#51279=EDGE_CURVE('',#39831,#39832,#25096,.T.);
#51280=EDGE_CURVE('',#39566,#39830,#21091,.T.);
#51281=EDGE_CURVE('',#39832,#39830,#21092,.T.);
#51282=EDGE_CURVE('',#39567,#39832,#21093,.T.);
#51283=EDGE_CURVE('',#39565,#39829,#21094,.T.);
#51284=EDGE_CURVE('',#39825,#39564,#21095,.T.);
#51285=EDGE_CURVE('',#39826,#38907,#21096,.T.);
#51286=EDGE_CURVE('',#39827,#38906,#21097,.T.);
#51287=EDGE_CURVE('',#39821,#38905,#21098,.T.);
#51288=EDGE_CURVE('',#39822,#38904,#21099,.T.);
#51289=EDGE_CURVE('',#39569,#39823,#21100,.T.);
#51290=EDGE_CURVE('',#39568,#39824,#21101,.T.);
#51291=EDGE_CURVE('',#39833,#39834,#29412,.T.);
#51292=EDGE_CURVE('',#39834,#39835,#25097,.T.);
#51293=EDGE_CURVE('',#39835,#39836,#744,.T.);
#51294=EDGE_CURVE('',#39836,#39837,#29413,.T.);
#51295=EDGE_CURVE('',#39837,#39833,#25098,.T.);
#51296=EDGE_CURVE('',#39838,#39839,#745,.T.);
#51297=EDGE_CURVE('',#39839,#39840,#25099,.T.);
#51298=EDGE_CURVE('',#39841,#39840,#29414,.T.);
#51299=EDGE_CURVE('',#39841,#39842,#25100,.T.);
#51300=EDGE_CURVE('',#39842,#39838,#29415,.T.);
#51301=EDGE_CURVE('',#39840,#39834,#25101,.T.);
#51302=EDGE_CURVE('',#39833,#39841,#21102,.T.);
#51303=EDGE_CURVE('',#39842,#39843,#25102,.T.);
#51304=EDGE_CURVE('',#39844,#39841,#746,.T.);
#51305=EDGE_CURVE('',#39843,#39844,#25103,.T.);
#51306=EDGE_CURVE('',#39844,#39833,#747,.T.);
#51307=EDGE_CURVE('',#39845,#39837,#25104,.T.);
#51308=EDGE_CURVE('',#39844,#39845,#25105,.T.);
#51309=EDGE_CURVE('',#39572,#39843,#21103,.T.);
#51310=EDGE_CURVE('',#39845,#39843,#21104,.T.);
#51311=EDGE_CURVE('',#39573,#39845,#21105,.T.);
#51312=EDGE_CURVE('',#39571,#39842,#21106,.T.);
#51313=EDGE_CURVE('',#39838,#39570,#21107,.T.);
#51314=EDGE_CURVE('',#39839,#38903,#21108,.T.);
#51315=EDGE_CURVE('',#39840,#38902,#21109,.T.);
#51316=EDGE_CURVE('',#39834,#38901,#21110,.T.);
#51317=EDGE_CURVE('',#39835,#38900,#21111,.T.);
#51318=EDGE_CURVE('',#39575,#39836,#21112,.T.);
#51319=EDGE_CURVE('',#39574,#39837,#21113,.T.);
#51320=EDGE_CURVE('',#39846,#39847,#29416,.T.);
#51321=EDGE_CURVE('',#39847,#39848,#25106,.T.);
#51322=EDGE_CURVE('',#39848,#39849,#748,.T.);
#51323=EDGE_CURVE('',#39849,#39850,#29417,.T.);
#51324=EDGE_CURVE('',#39850,#39846,#25107,.T.);
#51325=EDGE_CURVE('',#39851,#39852,#749,.T.);
#51326=EDGE_CURVE('',#39852,#39853,#25108,.T.);
#51327=EDGE_CURVE('',#39854,#39853,#29418,.T.);
#51328=EDGE_CURVE('',#39854,#39855,#25109,.T.);
#51329=EDGE_CURVE('',#39855,#39851,#29419,.T.);
#51330=EDGE_CURVE('',#39853,#39847,#25110,.T.);
#51331=EDGE_CURVE('',#39846,#39854,#21114,.T.);
#51332=EDGE_CURVE('',#39855,#39856,#25111,.T.);
#51333=EDGE_CURVE('',#39857,#39854,#750,.T.);
#51334=EDGE_CURVE('',#39856,#39857,#25112,.T.);
#51335=EDGE_CURVE('',#39857,#39846,#751,.T.);
#51336=EDGE_CURVE('',#39858,#39850,#25113,.T.);
#51337=EDGE_CURVE('',#39857,#39858,#25114,.T.);
#51338=EDGE_CURVE('',#39578,#39856,#21115,.T.);
#51339=EDGE_CURVE('',#39858,#39856,#21116,.T.);
#51340=EDGE_CURVE('',#39579,#39858,#21117,.T.);
#51341=EDGE_CURVE('',#39577,#39855,#21118,.T.);
#51342=EDGE_CURVE('',#39851,#39576,#21119,.T.);
#51343=EDGE_CURVE('',#39852,#38899,#21120,.T.);
#51344=EDGE_CURVE('',#39853,#38898,#21121,.T.);
#51345=EDGE_CURVE('',#39847,#38897,#21122,.T.);
#51346=EDGE_CURVE('',#39848,#38896,#21123,.T.);
#51347=EDGE_CURVE('',#39581,#39849,#21124,.T.);
#51348=EDGE_CURVE('',#39580,#39850,#21125,.T.);
#51349=EDGE_CURVE('',#39859,#39860,#29420,.T.);
#51350=EDGE_CURVE('',#39860,#39861,#25115,.T.);
#51351=EDGE_CURVE('',#39861,#39862,#752,.T.);
#51352=EDGE_CURVE('',#39862,#39863,#29421,.T.);
#51353=EDGE_CURVE('',#39863,#39859,#25116,.T.);
#51354=EDGE_CURVE('',#39864,#39865,#753,.T.);
#51355=EDGE_CURVE('',#39865,#39866,#25117,.T.);
#51356=EDGE_CURVE('',#39867,#39866,#29422,.T.);
#51357=EDGE_CURVE('',#39867,#39868,#25118,.T.);
#51358=EDGE_CURVE('',#39868,#39864,#29423,.T.);
#51359=EDGE_CURVE('',#39866,#39860,#25119,.T.);
#51360=EDGE_CURVE('',#39859,#39867,#21126,.T.);
#51361=EDGE_CURVE('',#39868,#39869,#25120,.T.);
#51362=EDGE_CURVE('',#39870,#39867,#754,.T.);
#51363=EDGE_CURVE('',#39869,#39870,#25121,.T.);
#51364=EDGE_CURVE('',#39870,#39859,#755,.T.);
#51365=EDGE_CURVE('',#39871,#39863,#25122,.T.);
#51366=EDGE_CURVE('',#39870,#39871,#25123,.T.);
#51367=EDGE_CURVE('',#39584,#39869,#21127,.T.);
#51368=EDGE_CURVE('',#39871,#39869,#21128,.T.);
#51369=EDGE_CURVE('',#39585,#39871,#21129,.T.);
#51370=EDGE_CURVE('',#39583,#39868,#21130,.T.);
#51371=EDGE_CURVE('',#39864,#39582,#21131,.T.);
#51372=EDGE_CURVE('',#39865,#38895,#21132,.T.);
#51373=EDGE_CURVE('',#39866,#38894,#21133,.T.);
#51374=EDGE_CURVE('',#39860,#38893,#21134,.T.);
#51375=EDGE_CURVE('',#39861,#38892,#21135,.T.);
#51376=EDGE_CURVE('',#39587,#39862,#21136,.T.);
#51377=EDGE_CURVE('',#39586,#39863,#21137,.T.);
#51378=EDGE_CURVE('',#39872,#39873,#29424,.T.);
#51379=EDGE_CURVE('',#39873,#39874,#25124,.T.);
#51380=EDGE_CURVE('',#39874,#39875,#756,.T.);
#51381=EDGE_CURVE('',#39875,#39876,#29425,.T.);
#51382=EDGE_CURVE('',#39876,#39872,#25125,.T.);
#51383=EDGE_CURVE('',#39877,#39878,#757,.T.);
#51384=EDGE_CURVE('',#39878,#39879,#25126,.T.);
#51385=EDGE_CURVE('',#39880,#39879,#29426,.T.);
#51386=EDGE_CURVE('',#39880,#39881,#25127,.T.);
#51387=EDGE_CURVE('',#39881,#39877,#29427,.T.);
#51388=EDGE_CURVE('',#39879,#39873,#25128,.T.);
#51389=EDGE_CURVE('',#39872,#39880,#21138,.T.);
#51390=EDGE_CURVE('',#39881,#39882,#25129,.T.);
#51391=EDGE_CURVE('',#39883,#39880,#758,.T.);
#51392=EDGE_CURVE('',#39882,#39883,#25130,.T.);
#51393=EDGE_CURVE('',#39883,#39872,#759,.T.);
#51394=EDGE_CURVE('',#39884,#39876,#25131,.T.);
#51395=EDGE_CURVE('',#39883,#39884,#25132,.T.);
#51396=EDGE_CURVE('',#39590,#39882,#21139,.T.);
#51397=EDGE_CURVE('',#39884,#39882,#21140,.T.);
#51398=EDGE_CURVE('',#39591,#39884,#21141,.T.);
#51399=EDGE_CURVE('',#39589,#39881,#21142,.T.);
#51400=EDGE_CURVE('',#39877,#39588,#21143,.T.);
#51401=EDGE_CURVE('',#39878,#38891,#21144,.T.);
#51402=EDGE_CURVE('',#39879,#38890,#21145,.T.);
#51403=EDGE_CURVE('',#39873,#38889,#21146,.T.);
#51404=EDGE_CURVE('',#39874,#38888,#21147,.T.);
#51405=EDGE_CURVE('',#39593,#39875,#21148,.T.);
#51406=EDGE_CURVE('',#39592,#39876,#21149,.T.);
#51407=EDGE_CURVE('',#39885,#39886,#29428,.T.);
#51408=EDGE_CURVE('',#39886,#39887,#25133,.T.);
#51409=EDGE_CURVE('',#39887,#39888,#760,.T.);
#51410=EDGE_CURVE('',#39888,#39889,#29429,.T.);
#51411=EDGE_CURVE('',#39889,#39885,#25134,.T.);
#51412=EDGE_CURVE('',#39890,#39891,#761,.T.);
#51413=EDGE_CURVE('',#39891,#39892,#25135,.T.);
#51414=EDGE_CURVE('',#39893,#39892,#29430,.T.);
#51415=EDGE_CURVE('',#39893,#39894,#25136,.T.);
#51416=EDGE_CURVE('',#39894,#39890,#29431,.T.);
#51417=EDGE_CURVE('',#39892,#39886,#25137,.T.);
#51418=EDGE_CURVE('',#39885,#39893,#21150,.T.);
#51419=EDGE_CURVE('',#39894,#39895,#25138,.T.);
#51420=EDGE_CURVE('',#39896,#39893,#762,.T.);
#51421=EDGE_CURVE('',#39895,#39896,#25139,.T.);
#51422=EDGE_CURVE('',#39896,#39885,#763,.T.);
#51423=EDGE_CURVE('',#39897,#39889,#25140,.T.);
#51424=EDGE_CURVE('',#39896,#39897,#25141,.T.);
#51425=EDGE_CURVE('',#39596,#39895,#21151,.T.);
#51426=EDGE_CURVE('',#39897,#39895,#21152,.T.);
#51427=EDGE_CURVE('',#39597,#39897,#21153,.T.);
#51428=EDGE_CURVE('',#39595,#39894,#21154,.T.);
#51429=EDGE_CURVE('',#39890,#39594,#21155,.T.);
#51430=EDGE_CURVE('',#39891,#38887,#21156,.T.);
#51431=EDGE_CURVE('',#39892,#38886,#21157,.T.);
#51432=EDGE_CURVE('',#39886,#38885,#21158,.T.);
#51433=EDGE_CURVE('',#39887,#38884,#21159,.T.);
#51434=EDGE_CURVE('',#39599,#39888,#21160,.T.);
#51435=EDGE_CURVE('',#39598,#39889,#21161,.T.);
#51436=EDGE_CURVE('',#39898,#39899,#29432,.T.);
#51437=EDGE_CURVE('',#39899,#39900,#25142,.T.);
#51438=EDGE_CURVE('',#39900,#39901,#764,.T.);
#51439=EDGE_CURVE('',#39901,#39902,#29433,.T.);
#51440=EDGE_CURVE('',#39902,#39898,#25143,.T.);
#51441=EDGE_CURVE('',#39903,#39904,#765,.T.);
#51442=EDGE_CURVE('',#39904,#39905,#25144,.T.);
#51443=EDGE_CURVE('',#39906,#39905,#29434,.T.);
#51444=EDGE_CURVE('',#39906,#39907,#25145,.T.);
#51445=EDGE_CURVE('',#39907,#39903,#29435,.T.);
#51446=EDGE_CURVE('',#39905,#39899,#25146,.T.);
#51447=EDGE_CURVE('',#39898,#39906,#21162,.T.);
#51448=EDGE_CURVE('',#39907,#39908,#25147,.T.);
#51449=EDGE_CURVE('',#39909,#39906,#766,.T.);
#51450=EDGE_CURVE('',#39908,#39909,#25148,.T.);
#51451=EDGE_CURVE('',#39909,#39898,#767,.T.);
#51452=EDGE_CURVE('',#39910,#39902,#25149,.T.);
#51453=EDGE_CURVE('',#39909,#39910,#25150,.T.);
#51454=EDGE_CURVE('',#39602,#39908,#21163,.T.);
#51455=EDGE_CURVE('',#39910,#39908,#21164,.T.);
#51456=EDGE_CURVE('',#39603,#39910,#21165,.T.);
#51457=EDGE_CURVE('',#39601,#39907,#21166,.T.);
#51458=EDGE_CURVE('',#39903,#39600,#21167,.T.);
#51459=EDGE_CURVE('',#39904,#38883,#21168,.T.);
#51460=EDGE_CURVE('',#39905,#38882,#21169,.T.);
#51461=EDGE_CURVE('',#39899,#38881,#21170,.T.);
#51462=EDGE_CURVE('',#39900,#38880,#21171,.T.);
#51463=EDGE_CURVE('',#39605,#39901,#21172,.T.);
#51464=EDGE_CURVE('',#39604,#39902,#21173,.T.);
#51465=EDGE_CURVE('',#39911,#39912,#29436,.T.);
#51466=EDGE_CURVE('',#39912,#39913,#25151,.T.);
#51467=EDGE_CURVE('',#39913,#39914,#768,.T.);
#51468=EDGE_CURVE('',#39914,#39915,#29437,.T.);
#51469=EDGE_CURVE('',#39915,#39911,#25152,.T.);
#51470=EDGE_CURVE('',#39916,#39917,#769,.T.);
#51471=EDGE_CURVE('',#39917,#39918,#25153,.T.);
#51472=EDGE_CURVE('',#39919,#39918,#29438,.T.);
#51473=EDGE_CURVE('',#39919,#39920,#25154,.T.);
#51474=EDGE_CURVE('',#39920,#39916,#29439,.T.);
#51475=EDGE_CURVE('',#39918,#39912,#25155,.T.);
#51476=EDGE_CURVE('',#39911,#39919,#21174,.T.);
#51477=EDGE_CURVE('',#39920,#39921,#25156,.T.);
#51478=EDGE_CURVE('',#39922,#39919,#770,.T.);
#51479=EDGE_CURVE('',#39921,#39922,#25157,.T.);
#51480=EDGE_CURVE('',#39922,#39911,#771,.T.);
#51481=EDGE_CURVE('',#39923,#39915,#25158,.T.);
#51482=EDGE_CURVE('',#39922,#39923,#25159,.T.);
#51483=EDGE_CURVE('',#39608,#39921,#21175,.T.);
#51484=EDGE_CURVE('',#39923,#39921,#21176,.T.);
#51485=EDGE_CURVE('',#39609,#39923,#21177,.T.);
#51486=EDGE_CURVE('',#39607,#39920,#21178,.T.);
#51487=EDGE_CURVE('',#39916,#39606,#21179,.T.);
#51488=EDGE_CURVE('',#39917,#38879,#21180,.T.);
#51489=EDGE_CURVE('',#39918,#38878,#21181,.T.);
#51490=EDGE_CURVE('',#39912,#38877,#21182,.T.);
#51491=EDGE_CURVE('',#39913,#38876,#21183,.T.);
#51492=EDGE_CURVE('',#39611,#39914,#21184,.T.);
#51493=EDGE_CURVE('',#39610,#39915,#21185,.T.);
#51494=EDGE_CURVE('',#39924,#39925,#29440,.T.);
#51495=EDGE_CURVE('',#39925,#39926,#25160,.T.);
#51496=EDGE_CURVE('',#39926,#39927,#772,.T.);
#51497=EDGE_CURVE('',#39927,#39928,#29441,.T.);
#51498=EDGE_CURVE('',#39928,#39924,#25161,.T.);
#51499=EDGE_CURVE('',#39929,#39930,#773,.T.);
#51500=EDGE_CURVE('',#39930,#39931,#25162,.T.);
#51501=EDGE_CURVE('',#39932,#39931,#29442,.T.);
#51502=EDGE_CURVE('',#39932,#39933,#25163,.T.);
#51503=EDGE_CURVE('',#39933,#39929,#29443,.T.);
#51504=EDGE_CURVE('',#39931,#39925,#25164,.T.);
#51505=EDGE_CURVE('',#39924,#39932,#21186,.T.);
#51506=EDGE_CURVE('',#39933,#39934,#25165,.T.);
#51507=EDGE_CURVE('',#39935,#39932,#774,.T.);
#51508=EDGE_CURVE('',#39934,#39935,#25166,.T.);
#51509=EDGE_CURVE('',#39935,#39924,#775,.T.);
#51510=EDGE_CURVE('',#39936,#39928,#25167,.T.);
#51511=EDGE_CURVE('',#39935,#39936,#25168,.T.);
#51512=EDGE_CURVE('',#39614,#39934,#21187,.T.);
#51513=EDGE_CURVE('',#39936,#39934,#21188,.T.);
#51514=EDGE_CURVE('',#39615,#39936,#21189,.T.);
#51515=EDGE_CURVE('',#39613,#39933,#21190,.T.);
#51516=EDGE_CURVE('',#39929,#39612,#21191,.T.);
#51517=EDGE_CURVE('',#39930,#38875,#21192,.T.);
#51518=EDGE_CURVE('',#39931,#38874,#21193,.T.);
#51519=EDGE_CURVE('',#39925,#38873,#21194,.T.);
#51520=EDGE_CURVE('',#39926,#38872,#21195,.T.);
#51521=EDGE_CURVE('',#39617,#39927,#21196,.T.);
#51522=EDGE_CURVE('',#39616,#39928,#21197,.T.);
#51523=EDGE_CURVE('',#39937,#39938,#29444,.T.);
#51524=EDGE_CURVE('',#39938,#39939,#25169,.T.);
#51525=EDGE_CURVE('',#39939,#39940,#776,.T.);
#51526=EDGE_CURVE('',#39940,#39941,#29445,.T.);
#51527=EDGE_CURVE('',#39941,#39937,#25170,.T.);
#51528=EDGE_CURVE('',#39942,#39943,#777,.T.);
#51529=EDGE_CURVE('',#39943,#39944,#25171,.T.);
#51530=EDGE_CURVE('',#39945,#39944,#29446,.T.);
#51531=EDGE_CURVE('',#39945,#39946,#25172,.T.);
#51532=EDGE_CURVE('',#39946,#39942,#29447,.T.);
#51533=EDGE_CURVE('',#39944,#39938,#25173,.T.);
#51534=EDGE_CURVE('',#39937,#39945,#21198,.T.);
#51535=EDGE_CURVE('',#39946,#39947,#25174,.T.);
#51536=EDGE_CURVE('',#39948,#39945,#778,.T.);
#51537=EDGE_CURVE('',#39947,#39948,#25175,.T.);
#51538=EDGE_CURVE('',#39948,#39937,#779,.T.);
#51539=EDGE_CURVE('',#39949,#39941,#25176,.T.);
#51540=EDGE_CURVE('',#39948,#39949,#25177,.T.);
#51541=EDGE_CURVE('',#39620,#39947,#21199,.T.);
#51542=EDGE_CURVE('',#39949,#39947,#21200,.T.);
#51543=EDGE_CURVE('',#39621,#39949,#21201,.T.);
#51544=EDGE_CURVE('',#39619,#39946,#21202,.T.);
#51545=EDGE_CURVE('',#39942,#39618,#21203,.T.);
#51546=EDGE_CURVE('',#39943,#38871,#21204,.T.);
#51547=EDGE_CURVE('',#39944,#38870,#21205,.T.);
#51548=EDGE_CURVE('',#39938,#38869,#21206,.T.);
#51549=EDGE_CURVE('',#39939,#38868,#21207,.T.);
#51550=EDGE_CURVE('',#39623,#39940,#21208,.T.);
#51551=EDGE_CURVE('',#39622,#39941,#21209,.T.);
#51552=EDGE_CURVE('',#39950,#39951,#29448,.T.);
#51553=EDGE_CURVE('',#39951,#39952,#25178,.T.);
#51554=EDGE_CURVE('',#39952,#39953,#780,.T.);
#51555=EDGE_CURVE('',#39953,#39954,#29449,.T.);
#51556=EDGE_CURVE('',#39954,#39950,#25179,.T.);
#51557=EDGE_CURVE('',#39955,#39956,#781,.T.);
#51558=EDGE_CURVE('',#39956,#39957,#25180,.T.);
#51559=EDGE_CURVE('',#39958,#39957,#29450,.T.);
#51560=EDGE_CURVE('',#39958,#39959,#25181,.T.);
#51561=EDGE_CURVE('',#39959,#39955,#29451,.T.);
#51562=EDGE_CURVE('',#39957,#39951,#25182,.T.);
#51563=EDGE_CURVE('',#39950,#39958,#21210,.T.);
#51564=EDGE_CURVE('',#39959,#39960,#25183,.T.);
#51565=EDGE_CURVE('',#39961,#39958,#782,.T.);
#51566=EDGE_CURVE('',#39960,#39961,#25184,.T.);
#51567=EDGE_CURVE('',#39961,#39950,#783,.T.);
#51568=EDGE_CURVE('',#39962,#39954,#25185,.T.);
#51569=EDGE_CURVE('',#39961,#39962,#25186,.T.);
#51570=EDGE_CURVE('',#39626,#39960,#21211,.T.);
#51571=EDGE_CURVE('',#39962,#39960,#21212,.T.);
#51572=EDGE_CURVE('',#39627,#39962,#21213,.T.);
#51573=EDGE_CURVE('',#39625,#39959,#21214,.T.);
#51574=EDGE_CURVE('',#39955,#39624,#21215,.T.);
#51575=EDGE_CURVE('',#39956,#38867,#21216,.T.);
#51576=EDGE_CURVE('',#39957,#38866,#21217,.T.);
#51577=EDGE_CURVE('',#39951,#38865,#21218,.T.);
#51578=EDGE_CURVE('',#39952,#38864,#21219,.T.);
#51579=EDGE_CURVE('',#39629,#39953,#21220,.T.);
#51580=EDGE_CURVE('',#39628,#39954,#21221,.T.);
#51581=EDGE_CURVE('',#39963,#39964,#29452,.T.);
#51582=EDGE_CURVE('',#39964,#39965,#25187,.T.);
#51583=EDGE_CURVE('',#39965,#39966,#784,.T.);
#51584=EDGE_CURVE('',#39966,#39967,#29453,.T.);
#51585=EDGE_CURVE('',#39967,#39963,#25188,.T.);
#51586=EDGE_CURVE('',#39968,#39969,#785,.T.);
#51587=EDGE_CURVE('',#39969,#39970,#25189,.T.);
#51588=EDGE_CURVE('',#39971,#39970,#29454,.T.);
#51589=EDGE_CURVE('',#39971,#39972,#25190,.T.);
#51590=EDGE_CURVE('',#39972,#39968,#29455,.T.);
#51591=EDGE_CURVE('',#39970,#39964,#25191,.T.);
#51592=EDGE_CURVE('',#39963,#39971,#21222,.T.);
#51593=EDGE_CURVE('',#39972,#39973,#25192,.T.);
#51594=EDGE_CURVE('',#39974,#39971,#786,.T.);
#51595=EDGE_CURVE('',#39973,#39974,#25193,.T.);
#51596=EDGE_CURVE('',#39974,#39963,#787,.T.);
#51597=EDGE_CURVE('',#39975,#39967,#25194,.T.);
#51598=EDGE_CURVE('',#39974,#39975,#25195,.T.);
#51599=EDGE_CURVE('',#39632,#39973,#21223,.T.);
#51600=EDGE_CURVE('',#39975,#39973,#21224,.T.);
#51601=EDGE_CURVE('',#39633,#39975,#21225,.T.);
#51602=EDGE_CURVE('',#39631,#39972,#21226,.T.);
#51603=EDGE_CURVE('',#39968,#39630,#21227,.T.);
#51604=EDGE_CURVE('',#39969,#38863,#21228,.T.);
#51605=EDGE_CURVE('',#39970,#38862,#21229,.T.);
#51606=EDGE_CURVE('',#39964,#38861,#21230,.T.);
#51607=EDGE_CURVE('',#39965,#38860,#21231,.T.);
#51608=EDGE_CURVE('',#39635,#39966,#21232,.T.);
#51609=EDGE_CURVE('',#39634,#39967,#21233,.T.);
#51610=EDGE_CURVE('',#39976,#39977,#29456,.T.);
#51611=EDGE_CURVE('',#39977,#39978,#25196,.T.);
#51612=EDGE_CURVE('',#39978,#39979,#788,.T.);
#51613=EDGE_CURVE('',#39979,#39980,#29457,.T.);
#51614=EDGE_CURVE('',#39980,#39976,#25197,.T.);
#51615=EDGE_CURVE('',#39981,#39982,#789,.T.);
#51616=EDGE_CURVE('',#39982,#39983,#25198,.T.);
#51617=EDGE_CURVE('',#39984,#39983,#29458,.T.);
#51618=EDGE_CURVE('',#39984,#39985,#25199,.T.);
#51619=EDGE_CURVE('',#39985,#39981,#29459,.T.);
#51620=EDGE_CURVE('',#39983,#39977,#25200,.T.);
#51621=EDGE_CURVE('',#39976,#39984,#21234,.T.);
#51622=EDGE_CURVE('',#39985,#39986,#25201,.T.);
#51623=EDGE_CURVE('',#39987,#39984,#790,.T.);
#51624=EDGE_CURVE('',#39986,#39987,#25202,.T.);
#51625=EDGE_CURVE('',#39987,#39976,#791,.T.);
#51626=EDGE_CURVE('',#39988,#39980,#25203,.T.);
#51627=EDGE_CURVE('',#39987,#39988,#25204,.T.);
#51628=EDGE_CURVE('',#39638,#39986,#21235,.T.);
#51629=EDGE_CURVE('',#39988,#39986,#21236,.T.);
#51630=EDGE_CURVE('',#39639,#39988,#21237,.T.);
#51631=EDGE_CURVE('',#39637,#39985,#21238,.T.);
#51632=EDGE_CURVE('',#39981,#39636,#21239,.T.);
#51633=EDGE_CURVE('',#39982,#38859,#21240,.T.);
#51634=EDGE_CURVE('',#39983,#38858,#21241,.T.);
#51635=EDGE_CURVE('',#39977,#38857,#21242,.T.);
#51636=EDGE_CURVE('',#39978,#38856,#21243,.T.);
#51637=EDGE_CURVE('',#39053,#39979,#21244,.T.);
#51638=EDGE_CURVE('',#39640,#39980,#21245,.T.);
#51639=EDGE_CURVE('',#39989,#39990,#29460,.T.);
#51640=EDGE_CURVE('',#39990,#39991,#25205,.T.);
#51641=EDGE_CURVE('',#39991,#39992,#792,.T.);
#51642=EDGE_CURVE('',#39992,#39993,#29461,.T.);
#51643=EDGE_CURVE('',#39993,#39989,#25206,.T.);
#51644=EDGE_CURVE('',#39994,#39995,#793,.T.);
#51645=EDGE_CURVE('',#39995,#39996,#25207,.T.);
#51646=EDGE_CURVE('',#39997,#39996,#29462,.T.);
#51647=EDGE_CURVE('',#39997,#39998,#25208,.T.);
#51648=EDGE_CURVE('',#39998,#39994,#29463,.T.);
#51649=EDGE_CURVE('',#39996,#39990,#25209,.T.);
#51650=EDGE_CURVE('',#39989,#39997,#21246,.T.);
#51651=EDGE_CURVE('',#39998,#39999,#25210,.T.);
#51652=EDGE_CURVE('',#40000,#39997,#794,.T.);
#51653=EDGE_CURVE('',#39999,#40000,#25211,.T.);
#51654=EDGE_CURVE('',#40000,#39989,#795,.T.);
#51655=EDGE_CURVE('',#40001,#39993,#25212,.T.);
#51656=EDGE_CURVE('',#40000,#40001,#25213,.T.);
#51657=EDGE_CURVE('',#39055,#39999,#21247,.T.);
#51658=EDGE_CURVE('',#40001,#39999,#21248,.T.);
#51659=EDGE_CURVE('',#39056,#40001,#21249,.T.);
#51660=EDGE_CURVE('',#39054,#39998,#21250,.T.);
#51661=EDGE_CURVE('',#39994,#39052,#21251,.T.);
#51662=EDGE_CURVE('',#39995,#38852,#21252,.T.);
#51663=EDGE_CURVE('',#39996,#38851,#21253,.T.);
#51664=EDGE_CURVE('',#39990,#38850,#21254,.T.);
#51665=EDGE_CURVE('',#39991,#38849,#21255,.T.);
#51666=EDGE_CURVE('',#39058,#39992,#21256,.T.);
#51667=EDGE_CURVE('',#39057,#39993,#21257,.T.);
#51668=EDGE_CURVE('',#40002,#40003,#29464,.T.);
#51669=EDGE_CURVE('',#40003,#40004,#25214,.T.);
#51670=EDGE_CURVE('',#40004,#40005,#796,.T.);
#51671=EDGE_CURVE('',#40005,#40006,#29465,.T.);
#51672=EDGE_CURVE('',#40006,#40002,#25215,.T.);
#51673=EDGE_CURVE('',#40007,#40008,#797,.T.);
#51674=EDGE_CURVE('',#40008,#40009,#25216,.T.);
#51675=EDGE_CURVE('',#40010,#40009,#29466,.T.);
#51676=EDGE_CURVE('',#40010,#40011,#25217,.T.);
#51677=EDGE_CURVE('',#40011,#40007,#29467,.T.);
#51678=EDGE_CURVE('',#40009,#40003,#25218,.T.);
#51679=EDGE_CURVE('',#40002,#40010,#21258,.T.);
#51680=EDGE_CURVE('',#40011,#40012,#25219,.T.);
#51681=EDGE_CURVE('',#40013,#40010,#798,.T.);
#51682=EDGE_CURVE('',#40012,#40013,#25220,.T.);
#51683=EDGE_CURVE('',#40013,#40002,#799,.T.);
#51684=EDGE_CURVE('',#40014,#40006,#25221,.T.);
#51685=EDGE_CURVE('',#40013,#40014,#25222,.T.);
#51686=EDGE_CURVE('',#39061,#40012,#21259,.T.);
#51687=EDGE_CURVE('',#40014,#40012,#21260,.T.);
#51688=EDGE_CURVE('',#39062,#40014,#21261,.T.);
#51689=EDGE_CURVE('',#39060,#40011,#21262,.T.);
#51690=EDGE_CURVE('',#40007,#39059,#21263,.T.);
#51691=EDGE_CURVE('',#40008,#38848,#21264,.T.);
#51692=EDGE_CURVE('',#40009,#38847,#21265,.T.);
#51693=EDGE_CURVE('',#40003,#38846,#21266,.T.);
#51694=EDGE_CURVE('',#40004,#38845,#21267,.T.);
#51695=EDGE_CURVE('',#39064,#40005,#21268,.T.);
#51696=EDGE_CURVE('',#39063,#40006,#21269,.T.);
#51697=EDGE_CURVE('',#40015,#40016,#29468,.T.);
#51698=EDGE_CURVE('',#40016,#40017,#25223,.T.);
#51699=EDGE_CURVE('',#40017,#40018,#800,.T.);
#51700=EDGE_CURVE('',#40018,#40019,#29469,.T.);
#51701=EDGE_CURVE('',#40019,#40015,#25224,.T.);
#51702=EDGE_CURVE('',#40020,#40021,#801,.T.);
#51703=EDGE_CURVE('',#40021,#40022,#25225,.T.);
#51704=EDGE_CURVE('',#40023,#40022,#29470,.T.);
#51705=EDGE_CURVE('',#40023,#40024,#25226,.T.);
#51706=EDGE_CURVE('',#40024,#40020,#29471,.T.);
#51707=EDGE_CURVE('',#40022,#40016,#25227,.T.);
#51708=EDGE_CURVE('',#40015,#40023,#21270,.T.);
#51709=EDGE_CURVE('',#40024,#40025,#25228,.T.);
#51710=EDGE_CURVE('',#40026,#40023,#802,.T.);
#51711=EDGE_CURVE('',#40025,#40026,#25229,.T.);
#51712=EDGE_CURVE('',#40026,#40015,#803,.T.);
#51713=EDGE_CURVE('',#40027,#40019,#25230,.T.);
#51714=EDGE_CURVE('',#40026,#40027,#25231,.T.);
#51715=EDGE_CURVE('',#39067,#40025,#21271,.T.);
#51716=EDGE_CURVE('',#40027,#40025,#21272,.T.);
#51717=EDGE_CURVE('',#39068,#40027,#21273,.T.);
#51718=EDGE_CURVE('',#39066,#40024,#21274,.T.);
#51719=EDGE_CURVE('',#40020,#39065,#21275,.T.);
#51720=EDGE_CURVE('',#40021,#38844,#21276,.T.);
#51721=EDGE_CURVE('',#40022,#38843,#21277,.T.);
#51722=EDGE_CURVE('',#40016,#38842,#21278,.T.);
#51723=EDGE_CURVE('',#40017,#38841,#21279,.T.);
#51724=EDGE_CURVE('',#39070,#40018,#21280,.T.);
#51725=EDGE_CURVE('',#39069,#40019,#21281,.T.);
#51726=EDGE_CURVE('',#40028,#40029,#29472,.T.);
#51727=EDGE_CURVE('',#40029,#40030,#25232,.T.);
#51728=EDGE_CURVE('',#40030,#40031,#804,.T.);
#51729=EDGE_CURVE('',#40031,#40032,#29473,.T.);
#51730=EDGE_CURVE('',#40032,#40028,#25233,.T.);
#51731=EDGE_CURVE('',#40033,#40034,#805,.T.);
#51732=EDGE_CURVE('',#40034,#40035,#25234,.T.);
#51733=EDGE_CURVE('',#40036,#40035,#29474,.T.);
#51734=EDGE_CURVE('',#40036,#40037,#25235,.T.);
#51735=EDGE_CURVE('',#40037,#40033,#29475,.T.);
#51736=EDGE_CURVE('',#40035,#40029,#25236,.T.);
#51737=EDGE_CURVE('',#40028,#40036,#21282,.T.);
#51738=EDGE_CURVE('',#40037,#40038,#25237,.T.);
#51739=EDGE_CURVE('',#40039,#40036,#806,.T.);
#51740=EDGE_CURVE('',#40038,#40039,#25238,.T.);
#51741=EDGE_CURVE('',#40039,#40028,#807,.T.);
#51742=EDGE_CURVE('',#40040,#40032,#25239,.T.);
#51743=EDGE_CURVE('',#40039,#40040,#25240,.T.);
#51744=EDGE_CURVE('',#39073,#40038,#21283,.T.);
#51745=EDGE_CURVE('',#40040,#40038,#21284,.T.);
#51746=EDGE_CURVE('',#39074,#40040,#21285,.T.);
#51747=EDGE_CURVE('',#39072,#40037,#21286,.T.);
#51748=EDGE_CURVE('',#40033,#39071,#21287,.T.);
#51749=EDGE_CURVE('',#40034,#38840,#21288,.T.);
#51750=EDGE_CURVE('',#40035,#38839,#21289,.T.);
#51751=EDGE_CURVE('',#40029,#38838,#21290,.T.);
#51752=EDGE_CURVE('',#40030,#38837,#21291,.T.);
#51753=EDGE_CURVE('',#39076,#40031,#21292,.T.);
#51754=EDGE_CURVE('',#39075,#40032,#21293,.T.);
#51755=EDGE_CURVE('',#40041,#40042,#29476,.T.);
#51756=EDGE_CURVE('',#40042,#40043,#25241,.T.);
#51757=EDGE_CURVE('',#40043,#40044,#808,.T.);
#51758=EDGE_CURVE('',#40044,#40045,#29477,.T.);
#51759=EDGE_CURVE('',#40045,#40041,#25242,.T.);
#51760=EDGE_CURVE('',#40046,#40047,#809,.T.);
#51761=EDGE_CURVE('',#40047,#40048,#25243,.T.);
#51762=EDGE_CURVE('',#40049,#40048,#29478,.T.);
#51763=EDGE_CURVE('',#40049,#40050,#25244,.T.);
#51764=EDGE_CURVE('',#40050,#40046,#29479,.T.);
#51765=EDGE_CURVE('',#40048,#40042,#25245,.T.);
#51766=EDGE_CURVE('',#40041,#40049,#21294,.T.);
#51767=EDGE_CURVE('',#40050,#40051,#25246,.T.);
#51768=EDGE_CURVE('',#40052,#40049,#810,.T.);
#51769=EDGE_CURVE('',#40051,#40052,#25247,.T.);
#51770=EDGE_CURVE('',#40052,#40041,#811,.T.);
#51771=EDGE_CURVE('',#40053,#40045,#25248,.T.);
#51772=EDGE_CURVE('',#40052,#40053,#25249,.T.);
#51773=EDGE_CURVE('',#39079,#40051,#21295,.T.);
#51774=EDGE_CURVE('',#40053,#40051,#21296,.T.);
#51775=EDGE_CURVE('',#39080,#40053,#21297,.T.);
#51776=EDGE_CURVE('',#39078,#40050,#21298,.T.);
#51777=EDGE_CURVE('',#40046,#39077,#21299,.T.);
#51778=EDGE_CURVE('',#40047,#38836,#21300,.T.);
#51779=EDGE_CURVE('',#40048,#38835,#21301,.T.);
#51780=EDGE_CURVE('',#40042,#38834,#21302,.T.);
#51781=EDGE_CURVE('',#40043,#38833,#21303,.T.);
#51782=EDGE_CURVE('',#39082,#40044,#21304,.T.);
#51783=EDGE_CURVE('',#39081,#40045,#21305,.T.);
#51784=EDGE_CURVE('',#40054,#40055,#29480,.T.);
#51785=EDGE_CURVE('',#40055,#40056,#25250,.T.);
#51786=EDGE_CURVE('',#40056,#40057,#812,.T.);
#51787=EDGE_CURVE('',#40057,#40058,#29481,.T.);
#51788=EDGE_CURVE('',#40058,#40054,#25251,.T.);
#51789=EDGE_CURVE('',#40059,#40060,#813,.T.);
#51790=EDGE_CURVE('',#40060,#40061,#25252,.T.);
#51791=EDGE_CURVE('',#40062,#40061,#29482,.T.);
#51792=EDGE_CURVE('',#40062,#40063,#25253,.T.);
#51793=EDGE_CURVE('',#40063,#40059,#29483,.T.);
#51794=EDGE_CURVE('',#40061,#40055,#25254,.T.);
#51795=EDGE_CURVE('',#40054,#40062,#21306,.T.);
#51796=EDGE_CURVE('',#40063,#40064,#25255,.T.);
#51797=EDGE_CURVE('',#40065,#40062,#814,.T.);
#51798=EDGE_CURVE('',#40064,#40065,#25256,.T.);
#51799=EDGE_CURVE('',#40065,#40054,#815,.T.);
#51800=EDGE_CURVE('',#40066,#40058,#25257,.T.);
#51801=EDGE_CURVE('',#40065,#40066,#25258,.T.);
#51802=EDGE_CURVE('',#39085,#40064,#21307,.T.);
#51803=EDGE_CURVE('',#40066,#40064,#21308,.T.);
#51804=EDGE_CURVE('',#39086,#40066,#21309,.T.);
#51805=EDGE_CURVE('',#39084,#40063,#21310,.T.);
#51806=EDGE_CURVE('',#40059,#39083,#21311,.T.);
#51807=EDGE_CURVE('',#40060,#38832,#21312,.T.);
#51808=EDGE_CURVE('',#40061,#38831,#21313,.T.);
#51809=EDGE_CURVE('',#40055,#38830,#21314,.T.);
#51810=EDGE_CURVE('',#40056,#38829,#21315,.T.);
#51811=EDGE_CURVE('',#39088,#40057,#21316,.T.);
#51812=EDGE_CURVE('',#39087,#40058,#21317,.T.);
#51813=EDGE_CURVE('',#40067,#40068,#29484,.T.);
#51814=EDGE_CURVE('',#40068,#40069,#25259,.T.);
#51815=EDGE_CURVE('',#40069,#40070,#816,.T.);
#51816=EDGE_CURVE('',#40070,#40071,#29485,.T.);
#51817=EDGE_CURVE('',#40071,#40067,#25260,.T.);
#51818=EDGE_CURVE('',#40072,#40073,#817,.T.);
#51819=EDGE_CURVE('',#40073,#40074,#25261,.T.);
#51820=EDGE_CURVE('',#40075,#40074,#29486,.T.);
#51821=EDGE_CURVE('',#40075,#40076,#25262,.T.);
#51822=EDGE_CURVE('',#40076,#40072,#29487,.T.);
#51823=EDGE_CURVE('',#40074,#40068,#25263,.T.);
#51824=EDGE_CURVE('',#40067,#40075,#21318,.T.);
#51825=EDGE_CURVE('',#40076,#40077,#25264,.T.);
#51826=EDGE_CURVE('',#40078,#40075,#818,.T.);
#51827=EDGE_CURVE('',#40077,#40078,#25265,.T.);
#51828=EDGE_CURVE('',#40078,#40067,#819,.T.);
#51829=EDGE_CURVE('',#40079,#40071,#25266,.T.);
#51830=EDGE_CURVE('',#40078,#40079,#25267,.T.);
#51831=EDGE_CURVE('',#39091,#40077,#21319,.T.);
#51832=EDGE_CURVE('',#40079,#40077,#21320,.T.);
#51833=EDGE_CURVE('',#39092,#40079,#21321,.T.);
#51834=EDGE_CURVE('',#39090,#40076,#21322,.T.);
#51835=EDGE_CURVE('',#40072,#39089,#21323,.T.);
#51836=EDGE_CURVE('',#40073,#38828,#21324,.T.);
#51837=EDGE_CURVE('',#40074,#38827,#21325,.T.);
#51838=EDGE_CURVE('',#40068,#38826,#21326,.T.);
#51839=EDGE_CURVE('',#40069,#38825,#21327,.T.);
#51840=EDGE_CURVE('',#39094,#40070,#21328,.T.);
#51841=EDGE_CURVE('',#39093,#40071,#21329,.T.);
#51842=EDGE_CURVE('',#40080,#40081,#29488,.T.);
#51843=EDGE_CURVE('',#40081,#40082,#25268,.T.);
#51844=EDGE_CURVE('',#40082,#40083,#820,.T.);
#51845=EDGE_CURVE('',#40083,#40084,#29489,.T.);
#51846=EDGE_CURVE('',#40084,#40080,#25269,.T.);
#51847=EDGE_CURVE('',#40085,#40086,#821,.T.);
#51848=EDGE_CURVE('',#40086,#40087,#25270,.T.);
#51849=EDGE_CURVE('',#40088,#40087,#29490,.T.);
#51850=EDGE_CURVE('',#40088,#40089,#25271,.T.);
#51851=EDGE_CURVE('',#40089,#40085,#29491,.T.);
#51852=EDGE_CURVE('',#40087,#40081,#25272,.T.);
#51853=EDGE_CURVE('',#40080,#40088,#21330,.T.);
#51854=EDGE_CURVE('',#40089,#40090,#25273,.T.);
#51855=EDGE_CURVE('',#40091,#40088,#822,.T.);
#51856=EDGE_CURVE('',#40090,#40091,#25274,.T.);
#51857=EDGE_CURVE('',#40091,#40080,#823,.T.);
#51858=EDGE_CURVE('',#40092,#40084,#25275,.T.);
#51859=EDGE_CURVE('',#40091,#40092,#25276,.T.);
#51860=EDGE_CURVE('',#39097,#40090,#21331,.T.);
#51861=EDGE_CURVE('',#40092,#40090,#21332,.T.);
#51862=EDGE_CURVE('',#39098,#40092,#21333,.T.);
#51863=EDGE_CURVE('',#39096,#40089,#21334,.T.);
#51864=EDGE_CURVE('',#40085,#39095,#21335,.T.);
#51865=EDGE_CURVE('',#40086,#38824,#21336,.T.);
#51866=EDGE_CURVE('',#40087,#38823,#21337,.T.);
#51867=EDGE_CURVE('',#40081,#38822,#21338,.T.);
#51868=EDGE_CURVE('',#40082,#38821,#21339,.T.);
#51869=EDGE_CURVE('',#39100,#40083,#21340,.T.);
#51870=EDGE_CURVE('',#39099,#40084,#21341,.T.);
#51871=EDGE_CURVE('',#40093,#40094,#29492,.T.);
#51872=EDGE_CURVE('',#40094,#40095,#25277,.T.);
#51873=EDGE_CURVE('',#40095,#40096,#824,.T.);
#51874=EDGE_CURVE('',#40096,#40097,#29493,.T.);
#51875=EDGE_CURVE('',#40097,#40093,#25278,.T.);
#51876=EDGE_CURVE('',#40098,#40099,#825,.T.);
#51877=EDGE_CURVE('',#40099,#40100,#25279,.T.);
#51878=EDGE_CURVE('',#40101,#40100,#29494,.T.);
#51879=EDGE_CURVE('',#40101,#40102,#25280,.T.);
#51880=EDGE_CURVE('',#40102,#40098,#29495,.T.);
#51881=EDGE_CURVE('',#40100,#40094,#25281,.T.);
#51882=EDGE_CURVE('',#40093,#40101,#21342,.T.);
#51883=EDGE_CURVE('',#40102,#40103,#25282,.T.);
#51884=EDGE_CURVE('',#40104,#40101,#826,.T.);
#51885=EDGE_CURVE('',#40103,#40104,#25283,.T.);
#51886=EDGE_CURVE('',#40104,#40093,#827,.T.);
#51887=EDGE_CURVE('',#40105,#40097,#25284,.T.);
#51888=EDGE_CURVE('',#40104,#40105,#25285,.T.);
#51889=EDGE_CURVE('',#39482,#40103,#21343,.T.);
#51890=EDGE_CURVE('',#40105,#40103,#21344,.T.);
#51891=EDGE_CURVE('',#39483,#40105,#21345,.T.);
#51892=EDGE_CURVE('',#39481,#40102,#21346,.T.);
#51893=EDGE_CURVE('',#40098,#39480,#21347,.T.);
#51894=EDGE_CURVE('',#40099,#38963,#21348,.T.);
#51895=EDGE_CURVE('',#40100,#38962,#21349,.T.);
#51896=EDGE_CURVE('',#40094,#38961,#21350,.T.);
#51897=EDGE_CURVE('',#40095,#38960,#21351,.T.);
#51898=EDGE_CURVE('',#39485,#40096,#21352,.T.);
#51899=EDGE_CURVE('',#39484,#40097,#21353,.T.);
#51900=EDGE_CURVE('',#40106,#40107,#29496,.T.);
#51901=EDGE_CURVE('',#40107,#40108,#25286,.T.);
#51902=EDGE_CURVE('',#40108,#40109,#828,.T.);
#51903=EDGE_CURVE('',#40109,#40110,#29497,.T.);
#51904=EDGE_CURVE('',#40110,#40106,#25287,.T.);
#51905=EDGE_CURVE('',#40111,#40112,#829,.T.);
#51906=EDGE_CURVE('',#40112,#40113,#25288,.T.);
#51907=EDGE_CURVE('',#40114,#40113,#29498,.T.);
#51908=EDGE_CURVE('',#40114,#40115,#25289,.T.);
#51909=EDGE_CURVE('',#40115,#40111,#29499,.T.);
#51910=EDGE_CURVE('',#40113,#40107,#25290,.T.);
#51911=EDGE_CURVE('',#40106,#40114,#21354,.T.);
#51912=EDGE_CURVE('',#40115,#40116,#25291,.T.);
#51913=EDGE_CURVE('',#40117,#40114,#830,.T.);
#51914=EDGE_CURVE('',#40116,#40117,#25292,.T.);
#51915=EDGE_CURVE('',#40117,#40106,#831,.T.);
#51916=EDGE_CURVE('',#40118,#40110,#25293,.T.);
#51917=EDGE_CURVE('',#40117,#40118,#25294,.T.);
#51918=EDGE_CURVE('',#39476,#40116,#21355,.T.);
#51919=EDGE_CURVE('',#40118,#40116,#21356,.T.);
#51920=EDGE_CURVE('',#39477,#40118,#21357,.T.);
#51921=EDGE_CURVE('',#39475,#40115,#21358,.T.);
#51922=EDGE_CURVE('',#40111,#39474,#21359,.T.);
#51923=EDGE_CURVE('',#40112,#38967,#21360,.T.);
#51924=EDGE_CURVE('',#40113,#38966,#21361,.T.);
#51925=EDGE_CURVE('',#40107,#38965,#21362,.T.);
#51926=EDGE_CURVE('',#40108,#38964,#21363,.T.);
#51927=EDGE_CURVE('',#39479,#40109,#21364,.T.);
#51928=EDGE_CURVE('',#39478,#40110,#21365,.T.);
#51929=EDGE_CURVE('',#40119,#40120,#29500,.T.);
#51930=EDGE_CURVE('',#40120,#40121,#25295,.T.);
#51931=EDGE_CURVE('',#40121,#40122,#832,.T.);
#51932=EDGE_CURVE('',#40122,#40123,#29501,.T.);
#51933=EDGE_CURVE('',#40123,#40119,#25296,.T.);
#51934=EDGE_CURVE('',#40124,#40125,#833,.T.);
#51935=EDGE_CURVE('',#40125,#40126,#25297,.T.);
#51936=EDGE_CURVE('',#40127,#40126,#29502,.T.);
#51937=EDGE_CURVE('',#40127,#40128,#25298,.T.);
#51938=EDGE_CURVE('',#40128,#40124,#29503,.T.);
#51939=EDGE_CURVE('',#40126,#40120,#25299,.T.);
#51940=EDGE_CURVE('',#40119,#40127,#21366,.T.);
#51941=EDGE_CURVE('',#40128,#40129,#25300,.T.);
#51942=EDGE_CURVE('',#40130,#40127,#834,.T.);
#51943=EDGE_CURVE('',#40129,#40130,#25301,.T.);
#51944=EDGE_CURVE('',#40130,#40119,#835,.T.);
#51945=EDGE_CURVE('',#40131,#40123,#25302,.T.);
#51946=EDGE_CURVE('',#40130,#40131,#25303,.T.);
#51947=EDGE_CURVE('',#39470,#40129,#21367,.T.);
#51948=EDGE_CURVE('',#40131,#40129,#21368,.T.);
#51949=EDGE_CURVE('',#39471,#40131,#21369,.T.);
#51950=EDGE_CURVE('',#39469,#40128,#21370,.T.);
#51951=EDGE_CURVE('',#40124,#39468,#21371,.T.);
#51952=EDGE_CURVE('',#40125,#38971,#21372,.T.);
#51953=EDGE_CURVE('',#40126,#38970,#21373,.T.);
#51954=EDGE_CURVE('',#40120,#38969,#21374,.T.);
#51955=EDGE_CURVE('',#40121,#38968,#21375,.T.);
#51956=EDGE_CURVE('',#39473,#40122,#21376,.T.);
#51957=EDGE_CURVE('',#39472,#40123,#21377,.T.);
#51958=EDGE_CURVE('',#40132,#40133,#29504,.T.);
#51959=EDGE_CURVE('',#40133,#40134,#25304,.T.);
#51960=EDGE_CURVE('',#40134,#40135,#836,.T.);
#51961=EDGE_CURVE('',#40135,#40136,#29505,.T.);
#51962=EDGE_CURVE('',#40136,#40132,#25305,.T.);
#51963=EDGE_CURVE('',#40137,#40138,#837,.T.);
#51964=EDGE_CURVE('',#40138,#40139,#25306,.T.);
#51965=EDGE_CURVE('',#40140,#40139,#29506,.T.);
#51966=EDGE_CURVE('',#40140,#40141,#25307,.T.);
#51967=EDGE_CURVE('',#40141,#40137,#29507,.T.);
#51968=EDGE_CURVE('',#40139,#40133,#25308,.T.);
#51969=EDGE_CURVE('',#40132,#40140,#21378,.T.);
#51970=EDGE_CURVE('',#40141,#40142,#25309,.T.);
#51971=EDGE_CURVE('',#40143,#40140,#838,.T.);
#51972=EDGE_CURVE('',#40142,#40143,#25310,.T.);
#51973=EDGE_CURVE('',#40143,#40132,#839,.T.);
#51974=EDGE_CURVE('',#40144,#40136,#25311,.T.);
#51975=EDGE_CURVE('',#40143,#40144,#25312,.T.);
#51976=EDGE_CURVE('',#39464,#40142,#21379,.T.);
#51977=EDGE_CURVE('',#40144,#40142,#21380,.T.);
#51978=EDGE_CURVE('',#39465,#40144,#21381,.T.);
#51979=EDGE_CURVE('',#39463,#40141,#21382,.T.);
#51980=EDGE_CURVE('',#40137,#39462,#21383,.T.);
#51981=EDGE_CURVE('',#40138,#38975,#21384,.T.);
#51982=EDGE_CURVE('',#40139,#38974,#21385,.T.);
#51983=EDGE_CURVE('',#40133,#38973,#21386,.T.);
#51984=EDGE_CURVE('',#40134,#38972,#21387,.T.);
#51985=EDGE_CURVE('',#39467,#40135,#21388,.T.);
#51986=EDGE_CURVE('',#39466,#40136,#21389,.T.);
#51987=EDGE_CURVE('',#40145,#40146,#29508,.T.);
#51988=EDGE_CURVE('',#40146,#40147,#25313,.T.);
#51989=EDGE_CURVE('',#40147,#40148,#840,.T.);
#51990=EDGE_CURVE('',#40148,#40149,#29509,.T.);
#51991=EDGE_CURVE('',#40149,#40145,#25314,.T.);
#51992=EDGE_CURVE('',#40150,#40151,#841,.T.);
#51993=EDGE_CURVE('',#40151,#40152,#25315,.T.);
#51994=EDGE_CURVE('',#40153,#40152,#29510,.T.);
#51995=EDGE_CURVE('',#40153,#40154,#25316,.T.);
#51996=EDGE_CURVE('',#40154,#40150,#29511,.T.);
#51997=EDGE_CURVE('',#40152,#40146,#25317,.T.);
#51998=EDGE_CURVE('',#40145,#40153,#21390,.T.);
#51999=EDGE_CURVE('',#40154,#40155,#25318,.T.);
#52000=EDGE_CURVE('',#40156,#40153,#842,.T.);
#52001=EDGE_CURVE('',#40155,#40156,#25319,.T.);
#52002=EDGE_CURVE('',#40156,#40145,#843,.T.);
#52003=EDGE_CURVE('',#40157,#40149,#25320,.T.);
#52004=EDGE_CURVE('',#40156,#40157,#25321,.T.);
#52005=EDGE_CURVE('',#39458,#40155,#21391,.T.);
#52006=EDGE_CURVE('',#40157,#40155,#21392,.T.);
#52007=EDGE_CURVE('',#39459,#40157,#21393,.T.);
#52008=EDGE_CURVE('',#39457,#40154,#21394,.T.);
#52009=EDGE_CURVE('',#40150,#39456,#21395,.T.);
#52010=EDGE_CURVE('',#40151,#38979,#21396,.T.);
#52011=EDGE_CURVE('',#40152,#38978,#21397,.T.);
#52012=EDGE_CURVE('',#40146,#38977,#21398,.T.);
#52013=EDGE_CURVE('',#40147,#38976,#21399,.T.);
#52014=EDGE_CURVE('',#39461,#40148,#21400,.T.);
#52015=EDGE_CURVE('',#39460,#40149,#21401,.T.);
#52016=EDGE_CURVE('',#40158,#40159,#29512,.T.);
#52017=EDGE_CURVE('',#40159,#40160,#25322,.T.);
#52018=EDGE_CURVE('',#40160,#40161,#844,.T.);
#52019=EDGE_CURVE('',#40161,#40162,#29513,.T.);
#52020=EDGE_CURVE('',#40162,#40158,#25323,.T.);
#52021=EDGE_CURVE('',#40163,#40164,#845,.T.);
#52022=EDGE_CURVE('',#40164,#40165,#25324,.T.);
#52023=EDGE_CURVE('',#40166,#40165,#29514,.T.);
#52024=EDGE_CURVE('',#40166,#40167,#25325,.T.);
#52025=EDGE_CURVE('',#40167,#40163,#29515,.T.);
#52026=EDGE_CURVE('',#40165,#40159,#25326,.T.);
#52027=EDGE_CURVE('',#40158,#40166,#21402,.T.);
#52028=EDGE_CURVE('',#40167,#40168,#25327,.T.);
#52029=EDGE_CURVE('',#40169,#40166,#846,.T.);
#52030=EDGE_CURVE('',#40168,#40169,#25328,.T.);
#52031=EDGE_CURVE('',#40169,#40158,#847,.T.);
#52032=EDGE_CURVE('',#40170,#40162,#25329,.T.);
#52033=EDGE_CURVE('',#40169,#40170,#25330,.T.);
#52034=EDGE_CURVE('',#39452,#40168,#21403,.T.);
#52035=EDGE_CURVE('',#40170,#40168,#21404,.T.);
#52036=EDGE_CURVE('',#39453,#40170,#21405,.T.);
#52037=EDGE_CURVE('',#39451,#40167,#21406,.T.);
#52038=EDGE_CURVE('',#40163,#39450,#21407,.T.);
#52039=EDGE_CURVE('',#40164,#38983,#21408,.T.);
#52040=EDGE_CURVE('',#40165,#38982,#21409,.T.);
#52041=EDGE_CURVE('',#40159,#38981,#21410,.T.);
#52042=EDGE_CURVE('',#40160,#38980,#21411,.T.);
#52043=EDGE_CURVE('',#39455,#40161,#21412,.T.);
#52044=EDGE_CURVE('',#39454,#40162,#21413,.T.);
#52045=EDGE_CURVE('',#40171,#40172,#29516,.T.);
#52046=EDGE_CURVE('',#40172,#40173,#25331,.T.);
#52047=EDGE_CURVE('',#40173,#40174,#848,.T.);
#52048=EDGE_CURVE('',#40174,#40175,#29517,.T.);
#52049=EDGE_CURVE('',#40175,#40171,#25332,.T.);
#52050=EDGE_CURVE('',#40176,#40177,#849,.T.);
#52051=EDGE_CURVE('',#40177,#40178,#25333,.T.);
#52052=EDGE_CURVE('',#40179,#40178,#29518,.T.);
#52053=EDGE_CURVE('',#40179,#40180,#25334,.T.);
#52054=EDGE_CURVE('',#40180,#40176,#29519,.T.);
#52055=EDGE_CURVE('',#40178,#40172,#25335,.T.);
#52056=EDGE_CURVE('',#40171,#40179,#21414,.T.);
#52057=EDGE_CURVE('',#40180,#40181,#25336,.T.);
#52058=EDGE_CURVE('',#40182,#40179,#850,.T.);
#52059=EDGE_CURVE('',#40181,#40182,#25337,.T.);
#52060=EDGE_CURVE('',#40182,#40171,#851,.T.);
#52061=EDGE_CURVE('',#40183,#40175,#25338,.T.);
#52062=EDGE_CURVE('',#40182,#40183,#25339,.T.);
#52063=EDGE_CURVE('',#39446,#40181,#21415,.T.);
#52064=EDGE_CURVE('',#40183,#40181,#21416,.T.);
#52065=EDGE_CURVE('',#39447,#40183,#21417,.T.);
#52066=EDGE_CURVE('',#39445,#40180,#21418,.T.);
#52067=EDGE_CURVE('',#40176,#39444,#21419,.T.);
#52068=EDGE_CURVE('',#40177,#38987,#21420,.T.);
#52069=EDGE_CURVE('',#40178,#38986,#21421,.T.);
#52070=EDGE_CURVE('',#40172,#38985,#21422,.T.);
#52071=EDGE_CURVE('',#40173,#38984,#21423,.T.);
#52072=EDGE_CURVE('',#39449,#40174,#21424,.T.);
#52073=EDGE_CURVE('',#39448,#40175,#21425,.T.);
#52074=EDGE_CURVE('',#40184,#40185,#29520,.T.);
#52075=EDGE_CURVE('',#40185,#40186,#25340,.T.);
#52076=EDGE_CURVE('',#40186,#40187,#852,.T.);
#52077=EDGE_CURVE('',#40187,#40188,#29521,.T.);
#52078=EDGE_CURVE('',#40188,#40184,#25341,.T.);
#52079=EDGE_CURVE('',#40189,#40190,#853,.T.);
#52080=EDGE_CURVE('',#40190,#40191,#25342,.T.);
#52081=EDGE_CURVE('',#40192,#40191,#29522,.T.);
#52082=EDGE_CURVE('',#40192,#40193,#25343,.T.);
#52083=EDGE_CURVE('',#40193,#40189,#29523,.T.);
#52084=EDGE_CURVE('',#40191,#40185,#25344,.T.);
#52085=EDGE_CURVE('',#40184,#40192,#21426,.T.);
#52086=EDGE_CURVE('',#40193,#40194,#25345,.T.);
#52087=EDGE_CURVE('',#40195,#40192,#854,.T.);
#52088=EDGE_CURVE('',#40194,#40195,#25346,.T.);
#52089=EDGE_CURVE('',#40195,#40184,#855,.T.);
#52090=EDGE_CURVE('',#40196,#40188,#25347,.T.);
#52091=EDGE_CURVE('',#40195,#40196,#25348,.T.);
#52092=EDGE_CURVE('',#39440,#40194,#21427,.T.);
#52093=EDGE_CURVE('',#40196,#40194,#21428,.T.);
#52094=EDGE_CURVE('',#39441,#40196,#21429,.T.);
#52095=EDGE_CURVE('',#39439,#40193,#21430,.T.);
#52096=EDGE_CURVE('',#40189,#39438,#21431,.T.);
#52097=EDGE_CURVE('',#40190,#38991,#21432,.T.);
#52098=EDGE_CURVE('',#40191,#38990,#21433,.T.);
#52099=EDGE_CURVE('',#40185,#38989,#21434,.T.);
#52100=EDGE_CURVE('',#40186,#38988,#21435,.T.);
#52101=EDGE_CURVE('',#39443,#40187,#21436,.T.);
#52102=EDGE_CURVE('',#39442,#40188,#21437,.T.);
#52103=EDGE_CURVE('',#40197,#40198,#29524,.T.);
#52104=EDGE_CURVE('',#40198,#40199,#25349,.T.);
#52105=EDGE_CURVE('',#40199,#40200,#856,.T.);
#52106=EDGE_CURVE('',#40200,#40201,#29525,.T.);
#52107=EDGE_CURVE('',#40201,#40197,#25350,.T.);
#52108=EDGE_CURVE('',#40202,#40203,#857,.T.);
#52109=EDGE_CURVE('',#40203,#40204,#25351,.T.);
#52110=EDGE_CURVE('',#40205,#40204,#29526,.T.);
#52111=EDGE_CURVE('',#40205,#40206,#25352,.T.);
#52112=EDGE_CURVE('',#40206,#40202,#29527,.T.);
#52113=EDGE_CURVE('',#40204,#40198,#25353,.T.);
#52114=EDGE_CURVE('',#40197,#40205,#21438,.T.);
#52115=EDGE_CURVE('',#40206,#40207,#25354,.T.);
#52116=EDGE_CURVE('',#40208,#40205,#858,.T.);
#52117=EDGE_CURVE('',#40207,#40208,#25355,.T.);
#52118=EDGE_CURVE('',#40208,#40197,#859,.T.);
#52119=EDGE_CURVE('',#40209,#40201,#25356,.T.);
#52120=EDGE_CURVE('',#40208,#40209,#25357,.T.);
#52121=EDGE_CURVE('',#39434,#40207,#21439,.T.);
#52122=EDGE_CURVE('',#40209,#40207,#21440,.T.);
#52123=EDGE_CURVE('',#39435,#40209,#21441,.T.);
#52124=EDGE_CURVE('',#39433,#40206,#21442,.T.);
#52125=EDGE_CURVE('',#40202,#39432,#21443,.T.);
#52126=EDGE_CURVE('',#40203,#38995,#21444,.T.);
#52127=EDGE_CURVE('',#40204,#38994,#21445,.T.);
#52128=EDGE_CURVE('',#40198,#38993,#21446,.T.);
#52129=EDGE_CURVE('',#40199,#38992,#21447,.T.);
#52130=EDGE_CURVE('',#39437,#40200,#21448,.T.);
#52131=EDGE_CURVE('',#39436,#40201,#21449,.T.);
#52132=EDGE_CURVE('',#40210,#40211,#29528,.T.);
#52133=EDGE_CURVE('',#40211,#40212,#25358,.T.);
#52134=EDGE_CURVE('',#40212,#40213,#860,.T.);
#52135=EDGE_CURVE('',#40213,#40214,#29529,.T.);
#52136=EDGE_CURVE('',#40214,#40210,#25359,.T.);
#52137=EDGE_CURVE('',#40215,#40216,#861,.T.);
#52138=EDGE_CURVE('',#40216,#40217,#25360,.T.);
#52139=EDGE_CURVE('',#40218,#40217,#29530,.T.);
#52140=EDGE_CURVE('',#40218,#40219,#25361,.T.);
#52141=EDGE_CURVE('',#40219,#40215,#29531,.T.);
#52142=EDGE_CURVE('',#40217,#40211,#25362,.T.);
#52143=EDGE_CURVE('',#40210,#40218,#21450,.T.);
#52144=EDGE_CURVE('',#40219,#40220,#25363,.T.);
#52145=EDGE_CURVE('',#40221,#40218,#862,.T.);
#52146=EDGE_CURVE('',#40220,#40221,#25364,.T.);
#52147=EDGE_CURVE('',#40221,#40210,#863,.T.);
#52148=EDGE_CURVE('',#40222,#40214,#25365,.T.);
#52149=EDGE_CURVE('',#40221,#40222,#25366,.T.);
#52150=EDGE_CURVE('',#39428,#40220,#21451,.T.);
#52151=EDGE_CURVE('',#40222,#40220,#21452,.T.);
#52152=EDGE_CURVE('',#39429,#40222,#21453,.T.);
#52153=EDGE_CURVE('',#39427,#40219,#21454,.T.);
#52154=EDGE_CURVE('',#40215,#39426,#21455,.T.);
#52155=EDGE_CURVE('',#40216,#38999,#21456,.T.);
#52156=EDGE_CURVE('',#40217,#38998,#21457,.T.);
#52157=EDGE_CURVE('',#40211,#38997,#21458,.T.);
#52158=EDGE_CURVE('',#40212,#38996,#21459,.T.);
#52159=EDGE_CURVE('',#39431,#40213,#21460,.T.);
#52160=EDGE_CURVE('',#39430,#40214,#21461,.T.);
#52161=EDGE_CURVE('',#40223,#40224,#29532,.T.);
#52162=EDGE_CURVE('',#40224,#40225,#25367,.T.);
#52163=EDGE_CURVE('',#40225,#40226,#864,.T.);
#52164=EDGE_CURVE('',#40226,#40227,#29533,.T.);
#52165=EDGE_CURVE('',#40227,#40223,#25368,.T.);
#52166=EDGE_CURVE('',#40228,#40229,#865,.T.);
#52167=EDGE_CURVE('',#40229,#40230,#25369,.T.);
#52168=EDGE_CURVE('',#40231,#40230,#29534,.T.);
#52169=EDGE_CURVE('',#40231,#40232,#25370,.T.);
#52170=EDGE_CURVE('',#40232,#40228,#29535,.T.);
#52171=EDGE_CURVE('',#40230,#40224,#25371,.T.);
#52172=EDGE_CURVE('',#40223,#40231,#21462,.T.);
#52173=EDGE_CURVE('',#40232,#40233,#25372,.T.);
#52174=EDGE_CURVE('',#40234,#40231,#866,.T.);
#52175=EDGE_CURVE('',#40233,#40234,#25373,.T.);
#52176=EDGE_CURVE('',#40234,#40223,#867,.T.);
#52177=EDGE_CURVE('',#40235,#40227,#25374,.T.);
#52178=EDGE_CURVE('',#40234,#40235,#25375,.T.);
#52179=EDGE_CURVE('',#39422,#40233,#21463,.T.);
#52180=EDGE_CURVE('',#40235,#40233,#21464,.T.);
#52181=EDGE_CURVE('',#39423,#40235,#21465,.T.);
#52182=EDGE_CURVE('',#39421,#40232,#21466,.T.);
#52183=EDGE_CURVE('',#40228,#39420,#21467,.T.);
#52184=EDGE_CURVE('',#40229,#39003,#21468,.T.);
#52185=EDGE_CURVE('',#40230,#39002,#21469,.T.);
#52186=EDGE_CURVE('',#40224,#39001,#21470,.T.);
#52187=EDGE_CURVE('',#40225,#39000,#21471,.T.);
#52188=EDGE_CURVE('',#39425,#40226,#21472,.T.);
#52189=EDGE_CURVE('',#39424,#40227,#21473,.T.);
#52190=EDGE_CURVE('',#40236,#40237,#29536,.T.);
#52191=EDGE_CURVE('',#40237,#40238,#25376,.T.);
#52192=EDGE_CURVE('',#40238,#40239,#868,.T.);
#52193=EDGE_CURVE('',#40239,#40240,#29537,.T.);
#52194=EDGE_CURVE('',#40240,#40236,#25377,.T.);
#52195=EDGE_CURVE('',#40241,#40242,#869,.T.);
#52196=EDGE_CURVE('',#40242,#40243,#25378,.T.);
#52197=EDGE_CURVE('',#40244,#40243,#29538,.T.);
#52198=EDGE_CURVE('',#40244,#40245,#25379,.T.);
#52199=EDGE_CURVE('',#40245,#40241,#29539,.T.);
#52200=EDGE_CURVE('',#40243,#40237,#25380,.T.);
#52201=EDGE_CURVE('',#40236,#40244,#21474,.T.);
#52202=EDGE_CURVE('',#40245,#40246,#25381,.T.);
#52203=EDGE_CURVE('',#40247,#40244,#870,.T.);
#52204=EDGE_CURVE('',#40246,#40247,#25382,.T.);
#52205=EDGE_CURVE('',#40247,#40236,#871,.T.);
#52206=EDGE_CURVE('',#40248,#40240,#25383,.T.);
#52207=EDGE_CURVE('',#40247,#40248,#25384,.T.);
#52208=EDGE_CURVE('',#39416,#40246,#21475,.T.);
#52209=EDGE_CURVE('',#40248,#40246,#21476,.T.);
#52210=EDGE_CURVE('',#39417,#40248,#21477,.T.);
#52211=EDGE_CURVE('',#39415,#40245,#21478,.T.);
#52212=EDGE_CURVE('',#40241,#39414,#21479,.T.);
#52213=EDGE_CURVE('',#40242,#39007,#21480,.T.);
#52214=EDGE_CURVE('',#40243,#39006,#21481,.T.);
#52215=EDGE_CURVE('',#40237,#39005,#21482,.T.);
#52216=EDGE_CURVE('',#40238,#39004,#21483,.T.);
#52217=EDGE_CURVE('',#39419,#40239,#21484,.T.);
#52218=EDGE_CURVE('',#39418,#40240,#21485,.T.);
#52219=EDGE_CURVE('',#40249,#40250,#29540,.T.);
#52220=EDGE_CURVE('',#40250,#40251,#25385,.T.);
#52221=EDGE_CURVE('',#40251,#40252,#872,.T.);
#52222=EDGE_CURVE('',#40252,#40253,#29541,.T.);
#52223=EDGE_CURVE('',#40253,#40249,#25386,.T.);
#52224=EDGE_CURVE('',#40254,#40255,#873,.T.);
#52225=EDGE_CURVE('',#40255,#40256,#25387,.T.);
#52226=EDGE_CURVE('',#40257,#40256,#29542,.T.);
#52227=EDGE_CURVE('',#40257,#40258,#25388,.T.);
#52228=EDGE_CURVE('',#40258,#40254,#29543,.T.);
#52229=EDGE_CURVE('',#40256,#40250,#25389,.T.);
#52230=EDGE_CURVE('',#40249,#40257,#21486,.T.);
#52231=EDGE_CURVE('',#40258,#40259,#25390,.T.);
#52232=EDGE_CURVE('',#40260,#40257,#874,.T.);
#52233=EDGE_CURVE('',#40259,#40260,#25391,.T.);
#52234=EDGE_CURVE('',#40260,#40249,#875,.T.);
#52235=EDGE_CURVE('',#40261,#40253,#25392,.T.);
#52236=EDGE_CURVE('',#40260,#40261,#25393,.T.);
#52237=EDGE_CURVE('',#39410,#40259,#21487,.T.);
#52238=EDGE_CURVE('',#40261,#40259,#21488,.T.);
#52239=EDGE_CURVE('',#39411,#40261,#21489,.T.);
#52240=EDGE_CURVE('',#39409,#40258,#21490,.T.);
#52241=EDGE_CURVE('',#40254,#39408,#21491,.T.);
#52242=EDGE_CURVE('',#40255,#39011,#21492,.T.);
#52243=EDGE_CURVE('',#40256,#39010,#21493,.T.);
#52244=EDGE_CURVE('',#40250,#39009,#21494,.T.);
#52245=EDGE_CURVE('',#40251,#39008,#21495,.T.);
#52246=EDGE_CURVE('',#39413,#40252,#21496,.T.);
#52247=EDGE_CURVE('',#39412,#40253,#21497,.T.);
#52248=EDGE_CURVE('',#40262,#40263,#29544,.T.);
#52249=EDGE_CURVE('',#40263,#40264,#25394,.T.);
#52250=EDGE_CURVE('',#40264,#40265,#876,.T.);
#52251=EDGE_CURVE('',#40265,#40266,#29545,.T.);
#52252=EDGE_CURVE('',#40266,#40262,#25395,.T.);
#52253=EDGE_CURVE('',#40267,#40268,#877,.T.);
#52254=EDGE_CURVE('',#40268,#40269,#25396,.T.);
#52255=EDGE_CURVE('',#40270,#40269,#29546,.T.);
#52256=EDGE_CURVE('',#40270,#40271,#25397,.T.);
#52257=EDGE_CURVE('',#40271,#40267,#29547,.T.);
#52258=EDGE_CURVE('',#40269,#40263,#25398,.T.);
#52259=EDGE_CURVE('',#40262,#40270,#21498,.T.);
#52260=EDGE_CURVE('',#40271,#40272,#25399,.T.);
#52261=EDGE_CURVE('',#40273,#40270,#878,.T.);
#52262=EDGE_CURVE('',#40272,#40273,#25400,.T.);
#52263=EDGE_CURVE('',#40273,#40262,#879,.T.);
#52264=EDGE_CURVE('',#40274,#40266,#25401,.T.);
#52265=EDGE_CURVE('',#40273,#40274,#25402,.T.);
#52266=EDGE_CURVE('',#39404,#40272,#21499,.T.);
#52267=EDGE_CURVE('',#40274,#40272,#21500,.T.);
#52268=EDGE_CURVE('',#39405,#40274,#21501,.T.);
#52269=EDGE_CURVE('',#39403,#40271,#21502,.T.);
#52270=EDGE_CURVE('',#40267,#39402,#21503,.T.);
#52271=EDGE_CURVE('',#40268,#39015,#21504,.T.);
#52272=EDGE_CURVE('',#40269,#39014,#21505,.T.);
#52273=EDGE_CURVE('',#40263,#39013,#21506,.T.);
#52274=EDGE_CURVE('',#40264,#39012,#21507,.T.);
#52275=EDGE_CURVE('',#39407,#40265,#21508,.T.);
#52276=EDGE_CURVE('',#39406,#40266,#21509,.T.);
#52277=EDGE_CURVE('',#40275,#40276,#29548,.T.);
#52278=EDGE_CURVE('',#40276,#40277,#25403,.T.);
#52279=EDGE_CURVE('',#40277,#40278,#880,.T.);
#52280=EDGE_CURVE('',#40278,#40279,#29549,.T.);
#52281=EDGE_CURVE('',#40279,#40275,#25404,.T.);
#52282=EDGE_CURVE('',#40280,#40281,#881,.T.);
#52283=EDGE_CURVE('',#40281,#40282,#25405,.T.);
#52284=EDGE_CURVE('',#40283,#40282,#29550,.T.);
#52285=EDGE_CURVE('',#40283,#40284,#25406,.T.);
#52286=EDGE_CURVE('',#40284,#40280,#29551,.T.);
#52287=EDGE_CURVE('',#40282,#40276,#25407,.T.);
#52288=EDGE_CURVE('',#40275,#40283,#21510,.T.);
#52289=EDGE_CURVE('',#40284,#40285,#25408,.T.);
#52290=EDGE_CURVE('',#40286,#40283,#882,.T.);
#52291=EDGE_CURVE('',#40285,#40286,#25409,.T.);
#52292=EDGE_CURVE('',#40286,#40275,#883,.T.);
#52293=EDGE_CURVE('',#40287,#40279,#25410,.T.);
#52294=EDGE_CURVE('',#40286,#40287,#25411,.T.);
#52295=EDGE_CURVE('',#39398,#40285,#21511,.T.);
#52296=EDGE_CURVE('',#40287,#40285,#21512,.T.);
#52297=EDGE_CURVE('',#39399,#40287,#21513,.T.);
#52298=EDGE_CURVE('',#39397,#40284,#21514,.T.);
#52299=EDGE_CURVE('',#40280,#39396,#21515,.T.);
#52300=EDGE_CURVE('',#40281,#39019,#21516,.T.);
#52301=EDGE_CURVE('',#40282,#39018,#21517,.T.);
#52302=EDGE_CURVE('',#40276,#39017,#21518,.T.);
#52303=EDGE_CURVE('',#40277,#39016,#21519,.T.);
#52304=EDGE_CURVE('',#39401,#40278,#21520,.T.);
#52305=EDGE_CURVE('',#39400,#40279,#21521,.T.);
#52306=EDGE_CURVE('',#40288,#40289,#29552,.T.);
#52307=EDGE_CURVE('',#40289,#40290,#25412,.T.);
#52308=EDGE_CURVE('',#40290,#40291,#884,.T.);
#52309=EDGE_CURVE('',#40291,#40292,#29553,.T.);
#52310=EDGE_CURVE('',#40292,#40288,#25413,.T.);
#52311=EDGE_CURVE('',#40293,#40294,#885,.T.);
#52312=EDGE_CURVE('',#40294,#40295,#25414,.T.);
#52313=EDGE_CURVE('',#40296,#40295,#29554,.T.);
#52314=EDGE_CURVE('',#40296,#40297,#25415,.T.);
#52315=EDGE_CURVE('',#40297,#40293,#29555,.T.);
#52316=EDGE_CURVE('',#40295,#40289,#25416,.T.);
#52317=EDGE_CURVE('',#40288,#40296,#21522,.T.);
#52318=EDGE_CURVE('',#40297,#40298,#25417,.T.);
#52319=EDGE_CURVE('',#40299,#40296,#886,.T.);
#52320=EDGE_CURVE('',#40298,#40299,#25418,.T.);
#52321=EDGE_CURVE('',#40299,#40288,#887,.T.);
#52322=EDGE_CURVE('',#40300,#40292,#25419,.T.);
#52323=EDGE_CURVE('',#40299,#40300,#25420,.T.);
#52324=EDGE_CURVE('',#39392,#40298,#21523,.T.);
#52325=EDGE_CURVE('',#40300,#40298,#21524,.T.);
#52326=EDGE_CURVE('',#39393,#40300,#21525,.T.);
#52327=EDGE_CURVE('',#39391,#40297,#21526,.T.);
#52328=EDGE_CURVE('',#40293,#39390,#21527,.T.);
#52329=EDGE_CURVE('',#40294,#39023,#21528,.T.);
#52330=EDGE_CURVE('',#40295,#39022,#21529,.T.);
#52331=EDGE_CURVE('',#40289,#39021,#21530,.T.);
#52332=EDGE_CURVE('',#40290,#39020,#21531,.T.);
#52333=EDGE_CURVE('',#39395,#40291,#21532,.T.);
#52334=EDGE_CURVE('',#39394,#40292,#21533,.T.);
#52335=EDGE_CURVE('',#40301,#40302,#29556,.T.);
#52336=EDGE_CURVE('',#40302,#40303,#25421,.T.);
#52337=EDGE_CURVE('',#40303,#40304,#888,.T.);
#52338=EDGE_CURVE('',#40304,#40305,#29557,.T.);
#52339=EDGE_CURVE('',#40305,#40301,#25422,.T.);
#52340=EDGE_CURVE('',#40306,#40307,#889,.T.);
#52341=EDGE_CURVE('',#40307,#40308,#25423,.T.);
#52342=EDGE_CURVE('',#40309,#40308,#29558,.T.);
#52343=EDGE_CURVE('',#40309,#40310,#25424,.T.);
#52344=EDGE_CURVE('',#40310,#40306,#29559,.T.);
#52345=EDGE_CURVE('',#40308,#40302,#25425,.T.);
#52346=EDGE_CURVE('',#40301,#40309,#21534,.T.);
#52347=EDGE_CURVE('',#40310,#40311,#25426,.T.);
#52348=EDGE_CURVE('',#40312,#40309,#890,.T.);
#52349=EDGE_CURVE('',#40311,#40312,#25427,.T.);
#52350=EDGE_CURVE('',#40312,#40301,#891,.T.);
#52351=EDGE_CURVE('',#40313,#40305,#25428,.T.);
#52352=EDGE_CURVE('',#40312,#40313,#25429,.T.);
#52353=EDGE_CURVE('',#39386,#40311,#21535,.T.);
#52354=EDGE_CURVE('',#40313,#40311,#21536,.T.);
#52355=EDGE_CURVE('',#39387,#40313,#21537,.T.);
#52356=EDGE_CURVE('',#39385,#40310,#21538,.T.);
#52357=EDGE_CURVE('',#40306,#39384,#21539,.T.);
#52358=EDGE_CURVE('',#40307,#39027,#21540,.T.);
#52359=EDGE_CURVE('',#40308,#39026,#21541,.T.);
#52360=EDGE_CURVE('',#40302,#39025,#21542,.T.);
#52361=EDGE_CURVE('',#40303,#39024,#21543,.T.);
#52362=EDGE_CURVE('',#39389,#40304,#21544,.T.);
#52363=EDGE_CURVE('',#39388,#40305,#21545,.T.);
#52364=EDGE_CURVE('',#40314,#40315,#29560,.T.);
#52365=EDGE_CURVE('',#40315,#40316,#25430,.T.);
#52366=EDGE_CURVE('',#40316,#40317,#892,.T.);
#52367=EDGE_CURVE('',#40317,#40318,#29561,.T.);
#52368=EDGE_CURVE('',#40318,#40314,#25431,.T.);
#52369=EDGE_CURVE('',#40319,#40320,#893,.T.);
#52370=EDGE_CURVE('',#40320,#40321,#25432,.T.);
#52371=EDGE_CURVE('',#40322,#40321,#29562,.T.);
#52372=EDGE_CURVE('',#40322,#40323,#25433,.T.);
#52373=EDGE_CURVE('',#40323,#40319,#29563,.T.);
#52374=EDGE_CURVE('',#40321,#40315,#25434,.T.);
#52375=EDGE_CURVE('',#40314,#40322,#21546,.T.);
#52376=EDGE_CURVE('',#40323,#40324,#25435,.T.);
#52377=EDGE_CURVE('',#40325,#40322,#894,.T.);
#52378=EDGE_CURVE('',#40324,#40325,#25436,.T.);
#52379=EDGE_CURVE('',#40325,#40314,#895,.T.);
#52380=EDGE_CURVE('',#40326,#40318,#25437,.T.);
#52381=EDGE_CURVE('',#40325,#40326,#25438,.T.);
#52382=EDGE_CURVE('',#39380,#40324,#21547,.T.);
#52383=EDGE_CURVE('',#40326,#40324,#21548,.T.);
#52384=EDGE_CURVE('',#39381,#40326,#21549,.T.);
#52385=EDGE_CURVE('',#39379,#40323,#21550,.T.);
#52386=EDGE_CURVE('',#40319,#39378,#21551,.T.);
#52387=EDGE_CURVE('',#40320,#39031,#21552,.T.);
#52388=EDGE_CURVE('',#40321,#39030,#21553,.T.);
#52389=EDGE_CURVE('',#40315,#39029,#21554,.T.);
#52390=EDGE_CURVE('',#40316,#39028,#21555,.T.);
#52391=EDGE_CURVE('',#39383,#40317,#21556,.T.);
#52392=EDGE_CURVE('',#39382,#40318,#21557,.T.);
#52393=EDGE_CURVE('',#40327,#40328,#29564,.T.);
#52394=EDGE_CURVE('',#40328,#40329,#25439,.T.);
#52395=EDGE_CURVE('',#40329,#40330,#896,.T.);
#52396=EDGE_CURVE('',#40330,#40331,#29565,.T.);
#52397=EDGE_CURVE('',#40331,#40327,#25440,.T.);
#52398=EDGE_CURVE('',#40332,#40333,#897,.T.);
#52399=EDGE_CURVE('',#40333,#40334,#25441,.T.);
#52400=EDGE_CURVE('',#40335,#40334,#29566,.T.);
#52401=EDGE_CURVE('',#40335,#40336,#25442,.T.);
#52402=EDGE_CURVE('',#40336,#40332,#29567,.T.);
#52403=EDGE_CURVE('',#40334,#40328,#25443,.T.);
#52404=EDGE_CURVE('',#40327,#40335,#21558,.T.);
#52405=EDGE_CURVE('',#40336,#40337,#25444,.T.);
#52406=EDGE_CURVE('',#40338,#40335,#898,.T.);
#52407=EDGE_CURVE('',#40337,#40338,#25445,.T.);
#52408=EDGE_CURVE('',#40338,#40327,#899,.T.);
#52409=EDGE_CURVE('',#40339,#40331,#25446,.T.);
#52410=EDGE_CURVE('',#40338,#40339,#25447,.T.);
#52411=EDGE_CURVE('',#39374,#40337,#21559,.T.);
#52412=EDGE_CURVE('',#40339,#40337,#21560,.T.);
#52413=EDGE_CURVE('',#39375,#40339,#21561,.T.);
#52414=EDGE_CURVE('',#39373,#40336,#21562,.T.);
#52415=EDGE_CURVE('',#40332,#39372,#21563,.T.);
#52416=EDGE_CURVE('',#40333,#39035,#21564,.T.);
#52417=EDGE_CURVE('',#40334,#39034,#21565,.T.);
#52418=EDGE_CURVE('',#40328,#39033,#21566,.T.);
#52419=EDGE_CURVE('',#40329,#39032,#21567,.T.);
#52420=EDGE_CURVE('',#39377,#40330,#21568,.T.);
#52421=EDGE_CURVE('',#39376,#40331,#21569,.T.);
#52422=EDGE_CURVE('',#40340,#40341,#29568,.T.);
#52423=EDGE_CURVE('',#40341,#40342,#25448,.T.);
#52424=EDGE_CURVE('',#40342,#40343,#900,.T.);
#52425=EDGE_CURVE('',#40343,#40344,#29569,.T.);
#52426=EDGE_CURVE('',#40344,#40340,#25449,.T.);
#52427=EDGE_CURVE('',#40345,#40346,#901,.T.);
#52428=EDGE_CURVE('',#40346,#40347,#25450,.T.);
#52429=EDGE_CURVE('',#40348,#40347,#29570,.T.);
#52430=EDGE_CURVE('',#40348,#40349,#25451,.T.);
#52431=EDGE_CURVE('',#40349,#40345,#29571,.T.);
#52432=EDGE_CURVE('',#40347,#40341,#25452,.T.);
#52433=EDGE_CURVE('',#40340,#40348,#21570,.T.);
#52434=EDGE_CURVE('',#40349,#40350,#25453,.T.);
#52435=EDGE_CURVE('',#40351,#40348,#902,.T.);
#52436=EDGE_CURVE('',#40350,#40351,#25454,.T.);
#52437=EDGE_CURVE('',#40351,#40340,#903,.T.);
#52438=EDGE_CURVE('',#40352,#40344,#25455,.T.);
#52439=EDGE_CURVE('',#40351,#40352,#25456,.T.);
#52440=EDGE_CURVE('',#39368,#40350,#21571,.T.);
#52441=EDGE_CURVE('',#40352,#40350,#21572,.T.);
#52442=EDGE_CURVE('',#39369,#40352,#21573,.T.);
#52443=EDGE_CURVE('',#39367,#40349,#21574,.T.);
#52444=EDGE_CURVE('',#40345,#39366,#21575,.T.);
#52445=EDGE_CURVE('',#40346,#39039,#21576,.T.);
#52446=EDGE_CURVE('',#40347,#39038,#21577,.T.);
#52447=EDGE_CURVE('',#40341,#39037,#21578,.T.);
#52448=EDGE_CURVE('',#40342,#39036,#21579,.T.);
#52449=EDGE_CURVE('',#39371,#40343,#21580,.T.);
#52450=EDGE_CURVE('',#39370,#40344,#21581,.T.);
#52451=EDGE_CURVE('',#40353,#40354,#29572,.T.);
#52452=EDGE_CURVE('',#40354,#40355,#25457,.T.);
#52453=EDGE_CURVE('',#40355,#40356,#904,.T.);
#52454=EDGE_CURVE('',#40356,#40357,#29573,.T.);
#52455=EDGE_CURVE('',#40357,#40353,#25458,.T.);
#52456=EDGE_CURVE('',#40358,#40359,#905,.T.);
#52457=EDGE_CURVE('',#40359,#40360,#25459,.T.);
#52458=EDGE_CURVE('',#40361,#40360,#29574,.T.);
#52459=EDGE_CURVE('',#40361,#40362,#25460,.T.);
#52460=EDGE_CURVE('',#40362,#40358,#29575,.T.);
#52461=EDGE_CURVE('',#40360,#40354,#25461,.T.);
#52462=EDGE_CURVE('',#40353,#40361,#21582,.T.);
#52463=EDGE_CURVE('',#40362,#40363,#25462,.T.);
#52464=EDGE_CURVE('',#40364,#40361,#906,.T.);
#52465=EDGE_CURVE('',#40363,#40364,#25463,.T.);
#52466=EDGE_CURVE('',#40364,#40353,#907,.T.);
#52467=EDGE_CURVE('',#40365,#40357,#25464,.T.);
#52468=EDGE_CURVE('',#40364,#40365,#25465,.T.);
#52469=EDGE_CURVE('',#39362,#40363,#21583,.T.);
#52470=EDGE_CURVE('',#40365,#40363,#21584,.T.);
#52471=EDGE_CURVE('',#39363,#40365,#21585,.T.);
#52472=EDGE_CURVE('',#39361,#40362,#21586,.T.);
#52473=EDGE_CURVE('',#40358,#39360,#21587,.T.);
#52474=EDGE_CURVE('',#40359,#39043,#21588,.T.);
#52475=EDGE_CURVE('',#40360,#39042,#21589,.T.);
#52476=EDGE_CURVE('',#40354,#39041,#21590,.T.);
#52477=EDGE_CURVE('',#40355,#39040,#21591,.T.);
#52478=EDGE_CURVE('',#39365,#40356,#21592,.T.);
#52479=EDGE_CURVE('',#39364,#40357,#21593,.T.);
#52480=EDGE_CURVE('',#40366,#40367,#29576,.T.);
#52481=EDGE_CURVE('',#40367,#40368,#25466,.T.);
#52482=EDGE_CURVE('',#40368,#40369,#908,.T.);
#52483=EDGE_CURVE('',#40369,#40370,#29577,.T.);
#52484=EDGE_CURVE('',#40370,#40366,#25467,.T.);
#52485=EDGE_CURVE('',#40371,#40372,#909,.T.);
#52486=EDGE_CURVE('',#40372,#40373,#25468,.T.);
#52487=EDGE_CURVE('',#40374,#40373,#29578,.T.);
#52488=EDGE_CURVE('',#40374,#40375,#25469,.T.);
#52489=EDGE_CURVE('',#40375,#40371,#29579,.T.);
#52490=EDGE_CURVE('',#40373,#40367,#25470,.T.);
#52491=EDGE_CURVE('',#40366,#40374,#21594,.T.);
#52492=EDGE_CURVE('',#40375,#40376,#25471,.T.);
#52493=EDGE_CURVE('',#40377,#40374,#910,.T.);
#52494=EDGE_CURVE('',#40376,#40377,#25472,.T.);
#52495=EDGE_CURVE('',#40377,#40366,#911,.T.);
#52496=EDGE_CURVE('',#40378,#40370,#25473,.T.);
#52497=EDGE_CURVE('',#40377,#40378,#25474,.T.);
#52498=EDGE_CURVE('',#39356,#40376,#21595,.T.);
#52499=EDGE_CURVE('',#40378,#40376,#21596,.T.);
#52500=EDGE_CURVE('',#39357,#40378,#21597,.T.);
#52501=EDGE_CURVE('',#39355,#40375,#21598,.T.);
#52502=EDGE_CURVE('',#40371,#39354,#21599,.T.);
#52503=EDGE_CURVE('',#40372,#39047,#21600,.T.);
#52504=EDGE_CURVE('',#40373,#39046,#21601,.T.);
#52505=EDGE_CURVE('',#40367,#39045,#21602,.T.);
#52506=EDGE_CURVE('',#40368,#39044,#21603,.T.);
#52507=EDGE_CURVE('',#39359,#40369,#21604,.T.);
#52508=EDGE_CURVE('',#39358,#40370,#21605,.T.);
#52509=EDGE_CURVE('',#40379,#40380,#29580,.T.);
#52510=EDGE_CURVE('',#40380,#40381,#25475,.T.);
#52511=EDGE_CURVE('',#40381,#40382,#912,.T.);
#52512=EDGE_CURVE('',#40382,#40383,#29581,.T.);
#52513=EDGE_CURVE('',#40383,#40379,#25476,.T.);
#52514=EDGE_CURVE('',#40384,#40385,#913,.T.);
#52515=EDGE_CURVE('',#40385,#40386,#25477,.T.);
#52516=EDGE_CURVE('',#40387,#40386,#29582,.T.);
#52517=EDGE_CURVE('',#40387,#40388,#25478,.T.);
#52518=EDGE_CURVE('',#40388,#40384,#29583,.T.);
#52519=EDGE_CURVE('',#40386,#40380,#25479,.T.);
#52520=EDGE_CURVE('',#40379,#40387,#21606,.T.);
#52521=EDGE_CURVE('',#40388,#40389,#25480,.T.);
#52522=EDGE_CURVE('',#40390,#40387,#914,.T.);
#52523=EDGE_CURVE('',#40389,#40390,#25481,.T.);
#52524=EDGE_CURVE('',#40390,#40379,#915,.T.);
#52525=EDGE_CURVE('',#40391,#40383,#25482,.T.);
#52526=EDGE_CURVE('',#40390,#40391,#25483,.T.);
#52527=EDGE_CURVE('',#39350,#40389,#21607,.T.);
#52528=EDGE_CURVE('',#40391,#40389,#21608,.T.);
#52529=EDGE_CURVE('',#39351,#40391,#21609,.T.);
#52530=EDGE_CURVE('',#39349,#40388,#21610,.T.);
#52531=EDGE_CURVE('',#40384,#39348,#21611,.T.);
#52532=EDGE_CURVE('',#40385,#38656,#21612,.T.);
#52533=EDGE_CURVE('',#40386,#39050,#21613,.T.);
#52534=EDGE_CURVE('',#40380,#39049,#21614,.T.);
#52535=EDGE_CURVE('',#40381,#39048,#21615,.T.);
#52536=EDGE_CURVE('',#39353,#40382,#21616,.T.);
#52537=EDGE_CURVE('',#39352,#40383,#21617,.T.);
#52538=EDGE_CURVE('',#40392,#40393,#29584,.T.);
#52539=EDGE_CURVE('',#40393,#40394,#25484,.T.);
#52540=EDGE_CURVE('',#40394,#40395,#916,.T.);
#52541=EDGE_CURVE('',#40395,#40396,#29585,.T.);
#52542=EDGE_CURVE('',#40396,#40392,#25485,.T.);
#52543=EDGE_CURVE('',#40397,#40398,#917,.T.);
#52544=EDGE_CURVE('',#40398,#40399,#25486,.T.);
#52545=EDGE_CURVE('',#40400,#40399,#29586,.T.);
#52546=EDGE_CURVE('',#40400,#40401,#25487,.T.);
#52547=EDGE_CURVE('',#40401,#40397,#29587,.T.);
#52548=EDGE_CURVE('',#40399,#40393,#25488,.T.);
#52549=EDGE_CURVE('',#40392,#40400,#21618,.T.);
#52550=EDGE_CURVE('',#40401,#40402,#25489,.T.);
#52551=EDGE_CURVE('',#40403,#40400,#918,.T.);
#52552=EDGE_CURVE('',#40402,#40403,#25490,.T.);
#52553=EDGE_CURVE('',#40403,#40392,#919,.T.);
#52554=EDGE_CURVE('',#40404,#40396,#25491,.T.);
#52555=EDGE_CURVE('',#40403,#40404,#25492,.T.);
#52556=EDGE_CURVE('',#39343,#40402,#21619,.T.);
#52557=EDGE_CURVE('',#40404,#40402,#21620,.T.);
#52558=EDGE_CURVE('',#39344,#40404,#21621,.T.);
#52559=EDGE_CURVE('',#39342,#40401,#21622,.T.);
#52560=EDGE_CURVE('',#40397,#39341,#21623,.T.);
#52561=EDGE_CURVE('',#40398,#38660,#21624,.T.);
#52562=EDGE_CURVE('',#40399,#38659,#21625,.T.);
#52563=EDGE_CURVE('',#40393,#38658,#21626,.T.);
#52564=EDGE_CURVE('',#40394,#38657,#21627,.T.);
#52565=EDGE_CURVE('',#39346,#40395,#21628,.T.);
#52566=EDGE_CURVE('',#39345,#40396,#21629,.T.);
#52567=EDGE_CURVE('',#40405,#40406,#29588,.T.);
#52568=EDGE_CURVE('',#40406,#40407,#25493,.T.);
#52569=EDGE_CURVE('',#40407,#40408,#920,.T.);
#52570=EDGE_CURVE('',#40408,#40409,#29589,.T.);
#52571=EDGE_CURVE('',#40409,#40405,#25494,.T.);
#52572=EDGE_CURVE('',#40410,#40411,#921,.T.);
#52573=EDGE_CURVE('',#40411,#40412,#25495,.T.);
#52574=EDGE_CURVE('',#40413,#40412,#29590,.T.);
#52575=EDGE_CURVE('',#40413,#40414,#25496,.T.);
#52576=EDGE_CURVE('',#40414,#40410,#29591,.T.);
#52577=EDGE_CURVE('',#40412,#40406,#25497,.T.);
#52578=EDGE_CURVE('',#40405,#40413,#21630,.T.);
#52579=EDGE_CURVE('',#40414,#40415,#25498,.T.);
#52580=EDGE_CURVE('',#40416,#40413,#922,.T.);
#52581=EDGE_CURVE('',#40415,#40416,#25499,.T.);
#52582=EDGE_CURVE('',#40416,#40405,#923,.T.);
#52583=EDGE_CURVE('',#40417,#40409,#25500,.T.);
#52584=EDGE_CURVE('',#40416,#40417,#25501,.T.);
#52585=EDGE_CURVE('',#39337,#40415,#21631,.T.);
#52586=EDGE_CURVE('',#40417,#40415,#21632,.T.);
#52587=EDGE_CURVE('',#39338,#40417,#21633,.T.);
#52588=EDGE_CURVE('',#39336,#40414,#21634,.T.);
#52589=EDGE_CURVE('',#40410,#39335,#21635,.T.);
#52590=EDGE_CURVE('',#40411,#38664,#21636,.T.);
#52591=EDGE_CURVE('',#40412,#38663,#21637,.T.);
#52592=EDGE_CURVE('',#40406,#38662,#21638,.T.);
#52593=EDGE_CURVE('',#40407,#38661,#21639,.T.);
#52594=EDGE_CURVE('',#39340,#40408,#21640,.T.);
#52595=EDGE_CURVE('',#39339,#40409,#21641,.T.);
#52596=EDGE_CURVE('',#40418,#40419,#29592,.T.);
#52597=EDGE_CURVE('',#40419,#40420,#25502,.T.);
#52598=EDGE_CURVE('',#40420,#40421,#924,.T.);
#52599=EDGE_CURVE('',#40421,#40422,#29593,.T.);
#52600=EDGE_CURVE('',#40422,#40418,#25503,.T.);
#52601=EDGE_CURVE('',#40423,#40424,#925,.T.);
#52602=EDGE_CURVE('',#40424,#40425,#25504,.T.);
#52603=EDGE_CURVE('',#40426,#40425,#29594,.T.);
#52604=EDGE_CURVE('',#40426,#40427,#25505,.T.);
#52605=EDGE_CURVE('',#40427,#40423,#29595,.T.);
#52606=EDGE_CURVE('',#40425,#40419,#25506,.T.);
#52607=EDGE_CURVE('',#40418,#40426,#21642,.T.);
#52608=EDGE_CURVE('',#40427,#40428,#25507,.T.);
#52609=EDGE_CURVE('',#40429,#40426,#926,.T.);
#52610=EDGE_CURVE('',#40428,#40429,#25508,.T.);
#52611=EDGE_CURVE('',#40429,#40418,#927,.T.);
#52612=EDGE_CURVE('',#40430,#40422,#25509,.T.);
#52613=EDGE_CURVE('',#40429,#40430,#25510,.T.);
#52614=EDGE_CURVE('',#39331,#40428,#21643,.T.);
#52615=EDGE_CURVE('',#40430,#40428,#21644,.T.);
#52616=EDGE_CURVE('',#39332,#40430,#21645,.T.);
#52617=EDGE_CURVE('',#39330,#40427,#21646,.T.);
#52618=EDGE_CURVE('',#40423,#39329,#21647,.T.);
#52619=EDGE_CURVE('',#40424,#38668,#21648,.T.);
#52620=EDGE_CURVE('',#40425,#38667,#21649,.T.);
#52621=EDGE_CURVE('',#40419,#38666,#21650,.T.);
#52622=EDGE_CURVE('',#40420,#38665,#21651,.T.);
#52623=EDGE_CURVE('',#39334,#40421,#21652,.T.);
#52624=EDGE_CURVE('',#39333,#40422,#21653,.T.);
#52625=EDGE_CURVE('',#40431,#40432,#29596,.T.);
#52626=EDGE_CURVE('',#40432,#40433,#25511,.T.);
#52627=EDGE_CURVE('',#40433,#40434,#928,.T.);
#52628=EDGE_CURVE('',#40434,#40435,#29597,.T.);
#52629=EDGE_CURVE('',#40435,#40431,#25512,.T.);
#52630=EDGE_CURVE('',#40436,#40437,#929,.T.);
#52631=EDGE_CURVE('',#40437,#40438,#25513,.T.);
#52632=EDGE_CURVE('',#40439,#40438,#29598,.T.);
#52633=EDGE_CURVE('',#40439,#40440,#25514,.T.);
#52634=EDGE_CURVE('',#40440,#40436,#29599,.T.);
#52635=EDGE_CURVE('',#40438,#40432,#25515,.T.);
#52636=EDGE_CURVE('',#40431,#40439,#21654,.T.);
#52637=EDGE_CURVE('',#40440,#40441,#25516,.T.);
#52638=EDGE_CURVE('',#40442,#40439,#930,.T.);
#52639=EDGE_CURVE('',#40441,#40442,#25517,.T.);
#52640=EDGE_CURVE('',#40442,#40431,#931,.T.);
#52641=EDGE_CURVE('',#40443,#40435,#25518,.T.);
#52642=EDGE_CURVE('',#40442,#40443,#25519,.T.);
#52643=EDGE_CURVE('',#39325,#40441,#21655,.T.);
#52644=EDGE_CURVE('',#40443,#40441,#21656,.T.);
#52645=EDGE_CURVE('',#39326,#40443,#21657,.T.);
#52646=EDGE_CURVE('',#39324,#40440,#21658,.T.);
#52647=EDGE_CURVE('',#40436,#39323,#21659,.T.);
#52648=EDGE_CURVE('',#40437,#38672,#21660,.T.);
#52649=EDGE_CURVE('',#40438,#38671,#21661,.T.);
#52650=EDGE_CURVE('',#40432,#38670,#21662,.T.);
#52651=EDGE_CURVE('',#40433,#38669,#21663,.T.);
#52652=EDGE_CURVE('',#39328,#40434,#21664,.T.);
#52653=EDGE_CURVE('',#39327,#40435,#21665,.T.);
#52654=EDGE_CURVE('',#40444,#40445,#29600,.T.);
#52655=EDGE_CURVE('',#40445,#40446,#25520,.T.);
#52656=EDGE_CURVE('',#40446,#40447,#932,.T.);
#52657=EDGE_CURVE('',#40447,#40448,#29601,.T.);
#52658=EDGE_CURVE('',#40448,#40444,#25521,.T.);
#52659=EDGE_CURVE('',#40449,#40450,#933,.T.);
#52660=EDGE_CURVE('',#40450,#40451,#25522,.T.);
#52661=EDGE_CURVE('',#40452,#40451,#29602,.T.);
#52662=EDGE_CURVE('',#40452,#40453,#25523,.T.);
#52663=EDGE_CURVE('',#40453,#40449,#29603,.T.);
#52664=EDGE_CURVE('',#40451,#40445,#25524,.T.);
#52665=EDGE_CURVE('',#40444,#40452,#21666,.T.);
#52666=EDGE_CURVE('',#40453,#40454,#25525,.T.);
#52667=EDGE_CURVE('',#40455,#40452,#934,.T.);
#52668=EDGE_CURVE('',#40454,#40455,#25526,.T.);
#52669=EDGE_CURVE('',#40455,#40444,#935,.T.);
#52670=EDGE_CURVE('',#40456,#40448,#25527,.T.);
#52671=EDGE_CURVE('',#40455,#40456,#25528,.T.);
#52672=EDGE_CURVE('',#39319,#40454,#21667,.T.);
#52673=EDGE_CURVE('',#40456,#40454,#21668,.T.);
#52674=EDGE_CURVE('',#39320,#40456,#21669,.T.);
#52675=EDGE_CURVE('',#39318,#40453,#21670,.T.);
#52676=EDGE_CURVE('',#40449,#39317,#21671,.T.);
#52677=EDGE_CURVE('',#40450,#38676,#21672,.T.);
#52678=EDGE_CURVE('',#40451,#38675,#21673,.T.);
#52679=EDGE_CURVE('',#40445,#38674,#21674,.T.);
#52680=EDGE_CURVE('',#40446,#38673,#21675,.T.);
#52681=EDGE_CURVE('',#39322,#40447,#21676,.T.);
#52682=EDGE_CURVE('',#39321,#40448,#21677,.T.);
#52683=EDGE_CURVE('',#40457,#40458,#29604,.T.);
#52684=EDGE_CURVE('',#40458,#40459,#25529,.T.);
#52685=EDGE_CURVE('',#40459,#40460,#936,.T.);
#52686=EDGE_CURVE('',#40460,#40461,#29605,.T.);
#52687=EDGE_CURVE('',#40461,#40457,#25530,.T.);
#52688=EDGE_CURVE('',#40462,#40463,#937,.T.);
#52689=EDGE_CURVE('',#40463,#40464,#25531,.T.);
#52690=EDGE_CURVE('',#40465,#40464,#29606,.T.);
#52691=EDGE_CURVE('',#40465,#40466,#25532,.T.);
#52692=EDGE_CURVE('',#40466,#40462,#29607,.T.);
#52693=EDGE_CURVE('',#40464,#40458,#25533,.T.);
#52694=EDGE_CURVE('',#40457,#40465,#21678,.T.);
#52695=EDGE_CURVE('',#40466,#40467,#25534,.T.);
#52696=EDGE_CURVE('',#40468,#40465,#938,.T.);
#52697=EDGE_CURVE('',#40467,#40468,#25535,.T.);
#52698=EDGE_CURVE('',#40468,#40457,#939,.T.);
#52699=EDGE_CURVE('',#40469,#40461,#25536,.T.);
#52700=EDGE_CURVE('',#40468,#40469,#25537,.T.);
#52701=EDGE_CURVE('',#39313,#40467,#21679,.T.);
#52702=EDGE_CURVE('',#40469,#40467,#21680,.T.);
#52703=EDGE_CURVE('',#39314,#40469,#21681,.T.);
#52704=EDGE_CURVE('',#39312,#40466,#21682,.T.);
#52705=EDGE_CURVE('',#40462,#39311,#21683,.T.);
#52706=EDGE_CURVE('',#40463,#38680,#21684,.T.);
#52707=EDGE_CURVE('',#40464,#38679,#21685,.T.);
#52708=EDGE_CURVE('',#40458,#38678,#21686,.T.);
#52709=EDGE_CURVE('',#40459,#38677,#21687,.T.);
#52710=EDGE_CURVE('',#39316,#40460,#21688,.T.);
#52711=EDGE_CURVE('',#39315,#40461,#21689,.T.);
#52712=EDGE_CURVE('',#40470,#40471,#29608,.T.);
#52713=EDGE_CURVE('',#40471,#40472,#25538,.T.);
#52714=EDGE_CURVE('',#40472,#40473,#940,.T.);
#52715=EDGE_CURVE('',#40473,#40474,#29609,.T.);
#52716=EDGE_CURVE('',#40474,#40470,#25539,.T.);
#52717=EDGE_CURVE('',#40475,#40476,#941,.T.);
#52718=EDGE_CURVE('',#40476,#40477,#25540,.T.);
#52719=EDGE_CURVE('',#40478,#40477,#29610,.T.);
#52720=EDGE_CURVE('',#40478,#40479,#25541,.T.);
#52721=EDGE_CURVE('',#40479,#40475,#29611,.T.);
#52722=EDGE_CURVE('',#40477,#40471,#25542,.T.);
#52723=EDGE_CURVE('',#40470,#40478,#21690,.T.);
#52724=EDGE_CURVE('',#40479,#40480,#25543,.T.);
#52725=EDGE_CURVE('',#40481,#40478,#942,.T.);
#52726=EDGE_CURVE('',#40480,#40481,#25544,.T.);
#52727=EDGE_CURVE('',#40481,#40470,#943,.T.);
#52728=EDGE_CURVE('',#40482,#40474,#25545,.T.);
#52729=EDGE_CURVE('',#40481,#40482,#25546,.T.);
#52730=EDGE_CURVE('',#39307,#40480,#21691,.T.);
#52731=EDGE_CURVE('',#40482,#40480,#21692,.T.);
#52732=EDGE_CURVE('',#39308,#40482,#21693,.T.);
#52733=EDGE_CURVE('',#39306,#40479,#21694,.T.);
#52734=EDGE_CURVE('',#40475,#39305,#21695,.T.);
#52735=EDGE_CURVE('',#40476,#38684,#21696,.T.);
#52736=EDGE_CURVE('',#40477,#38683,#21697,.T.);
#52737=EDGE_CURVE('',#40471,#38682,#21698,.T.);
#52738=EDGE_CURVE('',#40472,#38681,#21699,.T.);
#52739=EDGE_CURVE('',#39310,#40473,#21700,.T.);
#52740=EDGE_CURVE('',#39309,#40474,#21701,.T.);
#52741=EDGE_CURVE('',#40483,#40484,#29612,.T.);
#52742=EDGE_CURVE('',#40484,#40485,#25547,.T.);
#52743=EDGE_CURVE('',#40485,#40486,#944,.T.);
#52744=EDGE_CURVE('',#40486,#40487,#29613,.T.);
#52745=EDGE_CURVE('',#40487,#40483,#25548,.T.);
#52746=EDGE_CURVE('',#40488,#40489,#945,.T.);
#52747=EDGE_CURVE('',#40489,#40490,#25549,.T.);
#52748=EDGE_CURVE('',#40491,#40490,#29614,.T.);
#52749=EDGE_CURVE('',#40491,#40492,#25550,.T.);
#52750=EDGE_CURVE('',#40492,#40488,#29615,.T.);
#52751=EDGE_CURVE('',#40490,#40484,#25551,.T.);
#52752=EDGE_CURVE('',#40483,#40491,#21702,.T.);
#52753=EDGE_CURVE('',#40492,#40493,#25552,.T.);
#52754=EDGE_CURVE('',#40494,#40491,#946,.T.);
#52755=EDGE_CURVE('',#40493,#40494,#25553,.T.);
#52756=EDGE_CURVE('',#40494,#40483,#947,.T.);
#52757=EDGE_CURVE('',#40495,#40487,#25554,.T.);
#52758=EDGE_CURVE('',#40494,#40495,#25555,.T.);
#52759=EDGE_CURVE('',#39301,#40493,#21703,.T.);
#52760=EDGE_CURVE('',#40495,#40493,#21704,.T.);
#52761=EDGE_CURVE('',#39302,#40495,#21705,.T.);
#52762=EDGE_CURVE('',#39300,#40492,#21706,.T.);
#52763=EDGE_CURVE('',#40488,#39299,#21707,.T.);
#52764=EDGE_CURVE('',#40489,#38688,#21708,.T.);
#52765=EDGE_CURVE('',#40490,#38687,#21709,.T.);
#52766=EDGE_CURVE('',#40484,#38686,#21710,.T.);
#52767=EDGE_CURVE('',#40485,#38685,#21711,.T.);
#52768=EDGE_CURVE('',#39304,#40486,#21712,.T.);
#52769=EDGE_CURVE('',#39303,#40487,#21713,.T.);
#52770=EDGE_CURVE('',#40496,#40497,#29616,.T.);
#52771=EDGE_CURVE('',#40497,#40498,#25556,.T.);
#52772=EDGE_CURVE('',#40498,#40499,#948,.T.);
#52773=EDGE_CURVE('',#40499,#40500,#29617,.T.);
#52774=EDGE_CURVE('',#40500,#40496,#25557,.T.);
#52775=EDGE_CURVE('',#40501,#40502,#949,.T.);
#52776=EDGE_CURVE('',#40502,#40503,#25558,.T.);
#52777=EDGE_CURVE('',#40504,#40503,#29618,.T.);
#52778=EDGE_CURVE('',#40504,#40505,#25559,.T.);
#52779=EDGE_CURVE('',#40505,#40501,#29619,.T.);
#52780=EDGE_CURVE('',#40503,#40497,#25560,.T.);
#52781=EDGE_CURVE('',#40496,#40504,#21714,.T.);
#52782=EDGE_CURVE('',#40505,#40506,#25561,.T.);
#52783=EDGE_CURVE('',#40507,#40504,#950,.T.);
#52784=EDGE_CURVE('',#40506,#40507,#25562,.T.);
#52785=EDGE_CURVE('',#40507,#40496,#951,.T.);
#52786=EDGE_CURVE('',#40508,#40500,#25563,.T.);
#52787=EDGE_CURVE('',#40507,#40508,#25564,.T.);
#52788=EDGE_CURVE('',#39295,#40506,#21715,.T.);
#52789=EDGE_CURVE('',#40508,#40506,#21716,.T.);
#52790=EDGE_CURVE('',#39296,#40508,#21717,.T.);
#52791=EDGE_CURVE('',#39294,#40505,#21718,.T.);
#52792=EDGE_CURVE('',#40501,#39293,#21719,.T.);
#52793=EDGE_CURVE('',#40502,#38692,#21720,.T.);
#52794=EDGE_CURVE('',#40503,#38691,#21721,.T.);
#52795=EDGE_CURVE('',#40497,#38690,#21722,.T.);
#52796=EDGE_CURVE('',#40498,#38689,#21723,.T.);
#52797=EDGE_CURVE('',#39298,#40499,#21724,.T.);
#52798=EDGE_CURVE('',#39297,#40500,#21725,.T.);
#52799=EDGE_CURVE('',#40509,#40510,#29620,.T.);
#52800=EDGE_CURVE('',#40510,#40511,#25565,.T.);
#52801=EDGE_CURVE('',#40511,#40512,#952,.T.);
#52802=EDGE_CURVE('',#40512,#40513,#29621,.T.);
#52803=EDGE_CURVE('',#40513,#40509,#25566,.T.);
#52804=EDGE_CURVE('',#40514,#40515,#953,.T.);
#52805=EDGE_CURVE('',#40515,#40516,#25567,.T.);
#52806=EDGE_CURVE('',#40517,#40516,#29622,.T.);
#52807=EDGE_CURVE('',#40517,#40518,#25568,.T.);
#52808=EDGE_CURVE('',#40518,#40514,#29623,.T.);
#52809=EDGE_CURVE('',#40516,#40510,#25569,.T.);
#52810=EDGE_CURVE('',#40509,#40517,#21726,.T.);
#52811=EDGE_CURVE('',#40518,#40519,#25570,.T.);
#52812=EDGE_CURVE('',#40520,#40517,#954,.T.);
#52813=EDGE_CURVE('',#40519,#40520,#25571,.T.);
#52814=EDGE_CURVE('',#40520,#40509,#955,.T.);
#52815=EDGE_CURVE('',#40521,#40513,#25572,.T.);
#52816=EDGE_CURVE('',#40520,#40521,#25573,.T.);
#52817=EDGE_CURVE('',#39289,#40519,#21727,.T.);
#52818=EDGE_CURVE('',#40521,#40519,#21728,.T.);
#52819=EDGE_CURVE('',#39290,#40521,#21729,.T.);
#52820=EDGE_CURVE('',#39288,#40518,#21730,.T.);
#52821=EDGE_CURVE('',#40514,#39287,#21731,.T.);
#52822=EDGE_CURVE('',#40515,#38696,#21732,.T.);
#52823=EDGE_CURVE('',#40516,#38695,#21733,.T.);
#52824=EDGE_CURVE('',#40510,#38694,#21734,.T.);
#52825=EDGE_CURVE('',#40511,#38693,#21735,.T.);
#52826=EDGE_CURVE('',#39292,#40512,#21736,.T.);
#52827=EDGE_CURVE('',#39291,#40513,#21737,.T.);
#52828=EDGE_CURVE('',#40522,#40523,#29624,.T.);
#52829=EDGE_CURVE('',#40523,#40524,#25574,.T.);
#52830=EDGE_CURVE('',#40524,#40525,#956,.T.);
#52831=EDGE_CURVE('',#40525,#40526,#29625,.T.);
#52832=EDGE_CURVE('',#40526,#40522,#25575,.T.);
#52833=EDGE_CURVE('',#40527,#40528,#957,.T.);
#52834=EDGE_CURVE('',#40528,#40529,#25576,.T.);
#52835=EDGE_CURVE('',#40530,#40529,#29626,.T.);
#52836=EDGE_CURVE('',#40530,#40531,#25577,.T.);
#52837=EDGE_CURVE('',#40531,#40527,#29627,.T.);
#52838=EDGE_CURVE('',#40529,#40523,#25578,.T.);
#52839=EDGE_CURVE('',#40522,#40530,#21738,.T.);
#52840=EDGE_CURVE('',#40531,#40532,#25579,.T.);
#52841=EDGE_CURVE('',#40533,#40530,#958,.T.);
#52842=EDGE_CURVE('',#40532,#40533,#25580,.T.);
#52843=EDGE_CURVE('',#40533,#40522,#959,.T.);
#52844=EDGE_CURVE('',#40534,#40526,#25581,.T.);
#52845=EDGE_CURVE('',#40533,#40534,#25582,.T.);
#52846=EDGE_CURVE('',#39283,#40532,#21739,.T.);
#52847=EDGE_CURVE('',#40534,#40532,#21740,.T.);
#52848=EDGE_CURVE('',#39284,#40534,#21741,.T.);
#52849=EDGE_CURVE('',#39282,#40531,#21742,.T.);
#52850=EDGE_CURVE('',#40527,#39281,#21743,.T.);
#52851=EDGE_CURVE('',#40528,#38700,#21744,.T.);
#52852=EDGE_CURVE('',#40529,#38699,#21745,.T.);
#52853=EDGE_CURVE('',#40523,#38698,#21746,.T.);
#52854=EDGE_CURVE('',#40524,#38697,#21747,.T.);
#52855=EDGE_CURVE('',#39286,#40525,#21748,.T.);
#52856=EDGE_CURVE('',#39285,#40526,#21749,.T.);
#52857=EDGE_CURVE('',#40535,#40536,#29628,.T.);
#52858=EDGE_CURVE('',#40536,#40537,#25583,.T.);
#52859=EDGE_CURVE('',#40537,#40538,#960,.T.);
#52860=EDGE_CURVE('',#40538,#40539,#29629,.T.);
#52861=EDGE_CURVE('',#40539,#40535,#25584,.T.);
#52862=EDGE_CURVE('',#40540,#40541,#961,.T.);
#52863=EDGE_CURVE('',#40541,#40542,#25585,.T.);
#52864=EDGE_CURVE('',#40543,#40542,#29630,.T.);
#52865=EDGE_CURVE('',#40543,#40544,#25586,.T.);
#52866=EDGE_CURVE('',#40544,#40540,#29631,.T.);
#52867=EDGE_CURVE('',#40542,#40536,#25587,.T.);
#52868=EDGE_CURVE('',#40535,#40543,#21750,.T.);
#52869=EDGE_CURVE('',#40544,#40545,#25588,.T.);
#52870=EDGE_CURVE('',#40546,#40543,#962,.T.);
#52871=EDGE_CURVE('',#40545,#40546,#25589,.T.);
#52872=EDGE_CURVE('',#40546,#40535,#963,.T.);
#52873=EDGE_CURVE('',#40547,#40539,#25590,.T.);
#52874=EDGE_CURVE('',#40546,#40547,#25591,.T.);
#52875=EDGE_CURVE('',#39277,#40545,#21751,.T.);
#52876=EDGE_CURVE('',#40547,#40545,#21752,.T.);
#52877=EDGE_CURVE('',#39278,#40547,#21753,.T.);
#52878=EDGE_CURVE('',#39276,#40544,#21754,.T.);
#52879=EDGE_CURVE('',#40540,#39275,#21755,.T.);
#52880=EDGE_CURVE('',#40541,#38704,#21756,.T.);
#52881=EDGE_CURVE('',#40542,#38703,#21757,.T.);
#52882=EDGE_CURVE('',#40536,#38702,#21758,.T.);
#52883=EDGE_CURVE('',#40537,#38701,#21759,.T.);
#52884=EDGE_CURVE('',#39280,#40538,#21760,.T.);
#52885=EDGE_CURVE('',#39279,#40539,#21761,.T.);
#52886=EDGE_CURVE('',#40548,#40549,#29632,.T.);
#52887=EDGE_CURVE('',#40549,#40550,#25592,.T.);
#52888=EDGE_CURVE('',#40550,#40551,#964,.T.);
#52889=EDGE_CURVE('',#40551,#40552,#29633,.T.);
#52890=EDGE_CURVE('',#40552,#40548,#25593,.T.);
#52891=EDGE_CURVE('',#40553,#40554,#965,.T.);
#52892=EDGE_CURVE('',#40554,#40555,#25594,.T.);
#52893=EDGE_CURVE('',#40556,#40555,#29634,.T.);
#52894=EDGE_CURVE('',#40556,#40557,#25595,.T.);
#52895=EDGE_CURVE('',#40557,#40553,#29635,.T.);
#52896=EDGE_CURVE('',#40555,#40549,#25596,.T.);
#52897=EDGE_CURVE('',#40548,#40556,#21762,.T.);
#52898=EDGE_CURVE('',#40557,#40558,#25597,.T.);
#52899=EDGE_CURVE('',#40559,#40556,#966,.T.);
#52900=EDGE_CURVE('',#40558,#40559,#25598,.T.);
#52901=EDGE_CURVE('',#40559,#40548,#967,.T.);
#52902=EDGE_CURVE('',#40560,#40552,#25599,.T.);
#52903=EDGE_CURVE('',#40559,#40560,#25600,.T.);
#52904=EDGE_CURVE('',#39271,#40558,#21763,.T.);
#52905=EDGE_CURVE('',#40560,#40558,#21764,.T.);
#52906=EDGE_CURVE('',#39272,#40560,#21765,.T.);
#52907=EDGE_CURVE('',#39270,#40557,#21766,.T.);
#52908=EDGE_CURVE('',#40553,#39269,#21767,.T.);
#52909=EDGE_CURVE('',#40554,#38708,#21768,.T.);
#52910=EDGE_CURVE('',#40555,#38707,#21769,.T.);
#52911=EDGE_CURVE('',#40549,#38706,#21770,.T.);
#52912=EDGE_CURVE('',#40550,#38705,#21771,.T.);
#52913=EDGE_CURVE('',#39274,#40551,#21772,.T.);
#52914=EDGE_CURVE('',#39273,#40552,#21773,.T.);
#52915=EDGE_CURVE('',#40561,#40562,#29636,.T.);
#52916=EDGE_CURVE('',#40562,#40563,#25601,.T.);
#52917=EDGE_CURVE('',#40563,#40564,#968,.T.);
#52918=EDGE_CURVE('',#40564,#40565,#29637,.T.);
#52919=EDGE_CURVE('',#40565,#40561,#25602,.T.);
#52920=EDGE_CURVE('',#40566,#40567,#969,.T.);
#52921=EDGE_CURVE('',#40567,#40568,#25603,.T.);
#52922=EDGE_CURVE('',#40569,#40568,#29638,.T.);
#52923=EDGE_CURVE('',#40569,#40570,#25604,.T.);
#52924=EDGE_CURVE('',#40570,#40566,#29639,.T.);
#52925=EDGE_CURVE('',#40568,#40562,#25605,.T.);
#52926=EDGE_CURVE('',#40561,#40569,#21774,.T.);
#52927=EDGE_CURVE('',#40570,#40571,#25606,.T.);
#52928=EDGE_CURVE('',#40572,#40569,#970,.T.);
#52929=EDGE_CURVE('',#40571,#40572,#25607,.T.);
#52930=EDGE_CURVE('',#40572,#40561,#971,.T.);
#52931=EDGE_CURVE('',#40573,#40565,#25608,.T.);
#52932=EDGE_CURVE('',#40572,#40573,#25609,.T.);
#52933=EDGE_CURVE('',#39265,#40571,#21775,.T.);
#52934=EDGE_CURVE('',#40573,#40571,#21776,.T.);
#52935=EDGE_CURVE('',#39266,#40573,#21777,.T.);
#52936=EDGE_CURVE('',#39264,#40570,#21778,.T.);
#52937=EDGE_CURVE('',#40566,#39263,#21779,.T.);
#52938=EDGE_CURVE('',#40567,#38712,#21780,.T.);
#52939=EDGE_CURVE('',#40568,#38711,#21781,.T.);
#52940=EDGE_CURVE('',#40562,#38710,#21782,.T.);
#52941=EDGE_CURVE('',#40563,#38709,#21783,.T.);
#52942=EDGE_CURVE('',#39268,#40564,#21784,.T.);
#52943=EDGE_CURVE('',#39267,#40565,#21785,.T.);
#52944=EDGE_CURVE('',#40574,#40575,#29640,.T.);
#52945=EDGE_CURVE('',#40575,#40576,#25610,.T.);
#52946=EDGE_CURVE('',#40576,#40577,#972,.T.);
#52947=EDGE_CURVE('',#40577,#40578,#29641,.T.);
#52948=EDGE_CURVE('',#40578,#40574,#25611,.T.);
#52949=EDGE_CURVE('',#40579,#40580,#973,.T.);
#52950=EDGE_CURVE('',#40580,#40581,#25612,.T.);
#52951=EDGE_CURVE('',#40582,#40581,#29642,.T.);
#52952=EDGE_CURVE('',#40582,#40583,#25613,.T.);
#52953=EDGE_CURVE('',#40583,#40579,#29643,.T.);
#52954=EDGE_CURVE('',#40581,#40575,#25614,.T.);
#52955=EDGE_CURVE('',#40574,#40582,#21786,.T.);
#52956=EDGE_CURVE('',#40583,#40584,#25615,.T.);
#52957=EDGE_CURVE('',#40585,#40582,#974,.T.);
#52958=EDGE_CURVE('',#40584,#40585,#25616,.T.);
#52959=EDGE_CURVE('',#40585,#40574,#975,.T.);
#52960=EDGE_CURVE('',#40586,#40578,#25617,.T.);
#52961=EDGE_CURVE('',#40585,#40586,#25618,.T.);
#52962=EDGE_CURVE('',#39259,#40584,#21787,.T.);
#52963=EDGE_CURVE('',#40586,#40584,#21788,.T.);
#52964=EDGE_CURVE('',#39260,#40586,#21789,.T.);
#52965=EDGE_CURVE('',#39258,#40583,#21790,.T.);
#52966=EDGE_CURVE('',#40579,#39257,#21791,.T.);
#52967=EDGE_CURVE('',#40580,#38716,#21792,.T.);
#52968=EDGE_CURVE('',#40581,#38715,#21793,.T.);
#52969=EDGE_CURVE('',#40575,#38714,#21794,.T.);
#52970=EDGE_CURVE('',#40576,#38713,#21795,.T.);
#52971=EDGE_CURVE('',#39262,#40577,#21796,.T.);
#52972=EDGE_CURVE('',#39261,#40578,#21797,.T.);
#52973=EDGE_CURVE('',#40587,#40588,#29644,.T.);
#52974=EDGE_CURVE('',#40588,#40589,#25619,.T.);
#52975=EDGE_CURVE('',#40589,#40590,#976,.T.);
#52976=EDGE_CURVE('',#40590,#40591,#29645,.T.);
#52977=EDGE_CURVE('',#40591,#40587,#25620,.T.);
#52978=EDGE_CURVE('',#40592,#40593,#977,.T.);
#52979=EDGE_CURVE('',#40593,#40594,#25621,.T.);
#52980=EDGE_CURVE('',#40595,#40594,#29646,.T.);
#52981=EDGE_CURVE('',#40595,#40596,#25622,.T.);
#52982=EDGE_CURVE('',#40596,#40592,#29647,.T.);
#52983=EDGE_CURVE('',#40594,#40588,#25623,.T.);
#52984=EDGE_CURVE('',#40587,#40595,#21798,.T.);
#52985=EDGE_CURVE('',#40596,#40597,#25624,.T.);
#52986=EDGE_CURVE('',#40598,#40595,#978,.T.);
#52987=EDGE_CURVE('',#40597,#40598,#25625,.T.);
#52988=EDGE_CURVE('',#40598,#40587,#979,.T.);
#52989=EDGE_CURVE('',#40599,#40591,#25626,.T.);
#52990=EDGE_CURVE('',#40598,#40599,#25627,.T.);
#52991=EDGE_CURVE('',#39253,#40597,#21799,.T.);
#52992=EDGE_CURVE('',#40599,#40597,#21800,.T.);
#52993=EDGE_CURVE('',#39254,#40599,#21801,.T.);
#52994=EDGE_CURVE('',#39252,#40596,#21802,.T.);
#52995=EDGE_CURVE('',#40592,#39251,#21803,.T.);
#52996=EDGE_CURVE('',#40593,#38720,#21804,.T.);
#52997=EDGE_CURVE('',#40594,#38719,#21805,.T.);
#52998=EDGE_CURVE('',#40588,#38718,#21806,.T.);
#52999=EDGE_CURVE('',#40589,#38717,#21807,.T.);
#53000=EDGE_CURVE('',#39256,#40590,#21808,.T.);
#53001=EDGE_CURVE('',#39255,#40591,#21809,.T.);
#53002=EDGE_CURVE('',#40600,#40601,#29648,.T.);
#53003=EDGE_CURVE('',#40601,#40602,#25628,.T.);
#53004=EDGE_CURVE('',#40602,#40603,#980,.T.);
#53005=EDGE_CURVE('',#40603,#40604,#29649,.T.);
#53006=EDGE_CURVE('',#40604,#40600,#25629,.T.);
#53007=EDGE_CURVE('',#40605,#40606,#981,.T.);
#53008=EDGE_CURVE('',#40606,#40607,#25630,.T.);
#53009=EDGE_CURVE('',#40608,#40607,#29650,.T.);
#53010=EDGE_CURVE('',#40608,#40609,#25631,.T.);
#53011=EDGE_CURVE('',#40609,#40605,#29651,.T.);
#53012=EDGE_CURVE('',#40607,#40601,#25632,.T.);
#53013=EDGE_CURVE('',#40600,#40608,#21810,.T.);
#53014=EDGE_CURVE('',#40609,#40610,#25633,.T.);
#53015=EDGE_CURVE('',#40611,#40608,#982,.T.);
#53016=EDGE_CURVE('',#40610,#40611,#25634,.T.);
#53017=EDGE_CURVE('',#40611,#40600,#983,.T.);
#53018=EDGE_CURVE('',#40612,#40604,#25635,.T.);
#53019=EDGE_CURVE('',#40611,#40612,#25636,.T.);
#53020=EDGE_CURVE('',#39247,#40610,#21811,.T.);
#53021=EDGE_CURVE('',#40612,#40610,#21812,.T.);
#53022=EDGE_CURVE('',#39248,#40612,#21813,.T.);
#53023=EDGE_CURVE('',#39246,#40609,#21814,.T.);
#53024=EDGE_CURVE('',#40605,#39245,#21815,.T.);
#53025=EDGE_CURVE('',#40606,#38724,#21816,.T.);
#53026=EDGE_CURVE('',#40607,#38723,#21817,.T.);
#53027=EDGE_CURVE('',#40601,#38722,#21818,.T.);
#53028=EDGE_CURVE('',#40602,#38721,#21819,.T.);
#53029=EDGE_CURVE('',#39250,#40603,#21820,.T.);
#53030=EDGE_CURVE('',#39249,#40604,#21821,.T.);
#53031=EDGE_CURVE('',#40613,#40614,#29652,.T.);
#53032=EDGE_CURVE('',#40614,#40615,#25637,.T.);
#53033=EDGE_CURVE('',#40615,#40616,#984,.T.);
#53034=EDGE_CURVE('',#40616,#40617,#29653,.T.);
#53035=EDGE_CURVE('',#40617,#40613,#25638,.T.);
#53036=EDGE_CURVE('',#40618,#40619,#985,.T.);
#53037=EDGE_CURVE('',#40619,#40620,#25639,.T.);
#53038=EDGE_CURVE('',#40621,#40620,#29654,.T.);
#53039=EDGE_CURVE('',#40621,#40622,#25640,.T.);
#53040=EDGE_CURVE('',#40622,#40618,#29655,.T.);
#53041=EDGE_CURVE('',#40620,#40614,#25641,.T.);
#53042=EDGE_CURVE('',#40613,#40621,#21822,.T.);
#53043=EDGE_CURVE('',#40622,#40623,#25642,.T.);
#53044=EDGE_CURVE('',#40624,#40621,#986,.T.);
#53045=EDGE_CURVE('',#40623,#40624,#25643,.T.);
#53046=EDGE_CURVE('',#40624,#40613,#987,.T.);
#53047=EDGE_CURVE('',#40625,#40617,#25644,.T.);
#53048=EDGE_CURVE('',#40624,#40625,#25645,.T.);
#53049=EDGE_CURVE('',#39241,#40623,#21823,.T.);
#53050=EDGE_CURVE('',#40625,#40623,#21824,.T.);
#53051=EDGE_CURVE('',#39242,#40625,#21825,.T.);
#53052=EDGE_CURVE('',#39240,#40622,#21826,.T.);
#53053=EDGE_CURVE('',#40618,#39239,#21827,.T.);
#53054=EDGE_CURVE('',#40619,#38728,#21828,.T.);
#53055=EDGE_CURVE('',#40620,#38727,#21829,.T.);
#53056=EDGE_CURVE('',#40614,#38726,#21830,.T.);
#53057=EDGE_CURVE('',#40615,#38725,#21831,.T.);
#53058=EDGE_CURVE('',#39244,#40616,#21832,.T.);
#53059=EDGE_CURVE('',#39243,#40617,#21833,.T.);
#53060=EDGE_CURVE('',#40626,#40627,#29656,.T.);
#53061=EDGE_CURVE('',#40627,#40628,#25646,.T.);
#53062=EDGE_CURVE('',#40628,#40629,#988,.T.);
#53063=EDGE_CURVE('',#40629,#40630,#29657,.T.);
#53064=EDGE_CURVE('',#40630,#40626,#25647,.T.);
#53065=EDGE_CURVE('',#40631,#40632,#989,.T.);
#53066=EDGE_CURVE('',#40632,#40633,#25648,.T.);
#53067=EDGE_CURVE('',#40634,#40633,#29658,.T.);
#53068=EDGE_CURVE('',#40634,#40635,#25649,.T.);
#53069=EDGE_CURVE('',#40635,#40631,#29659,.T.);
#53070=EDGE_CURVE('',#40633,#40627,#25650,.T.);
#53071=EDGE_CURVE('',#40626,#40634,#21834,.T.);
#53072=EDGE_CURVE('',#40635,#40636,#25651,.T.);
#53073=EDGE_CURVE('',#40637,#40634,#990,.T.);
#53074=EDGE_CURVE('',#40636,#40637,#25652,.T.);
#53075=EDGE_CURVE('',#40637,#40626,#991,.T.);
#53076=EDGE_CURVE('',#40638,#40630,#25653,.T.);
#53077=EDGE_CURVE('',#40637,#40638,#25654,.T.);
#53078=EDGE_CURVE('',#39235,#40636,#21835,.T.);
#53079=EDGE_CURVE('',#40638,#40636,#21836,.T.);
#53080=EDGE_CURVE('',#39236,#40638,#21837,.T.);
#53081=EDGE_CURVE('',#39234,#40635,#21838,.T.);
#53082=EDGE_CURVE('',#40631,#39233,#21839,.T.);
#53083=EDGE_CURVE('',#40632,#38732,#21840,.T.);
#53084=EDGE_CURVE('',#40633,#38731,#21841,.T.);
#53085=EDGE_CURVE('',#40627,#38730,#21842,.T.);
#53086=EDGE_CURVE('',#40628,#38729,#21843,.T.);
#53087=EDGE_CURVE('',#39238,#40629,#21844,.T.);
#53088=EDGE_CURVE('',#39237,#40630,#21845,.T.);
#53089=EDGE_CURVE('',#40639,#40640,#29660,.T.);
#53090=EDGE_CURVE('',#40640,#40641,#25655,.T.);
#53091=EDGE_CURVE('',#40641,#40642,#992,.T.);
#53092=EDGE_CURVE('',#40642,#40643,#29661,.T.);
#53093=EDGE_CURVE('',#40643,#40639,#25656,.T.);
#53094=EDGE_CURVE('',#40644,#40645,#993,.T.);
#53095=EDGE_CURVE('',#40645,#40646,#25657,.T.);
#53096=EDGE_CURVE('',#40647,#40646,#29662,.T.);
#53097=EDGE_CURVE('',#40647,#40648,#25658,.T.);
#53098=EDGE_CURVE('',#40648,#40644,#29663,.T.);
#53099=EDGE_CURVE('',#40646,#40640,#25659,.T.);
#53100=EDGE_CURVE('',#40639,#40647,#21846,.T.);
#53101=EDGE_CURVE('',#40648,#40649,#25660,.T.);
#53102=EDGE_CURVE('',#40650,#40647,#994,.T.);
#53103=EDGE_CURVE('',#40649,#40650,#25661,.T.);
#53104=EDGE_CURVE('',#40650,#40639,#995,.T.);
#53105=EDGE_CURVE('',#40651,#40643,#25662,.T.);
#53106=EDGE_CURVE('',#40650,#40651,#25663,.T.);
#53107=EDGE_CURVE('',#39229,#40649,#21847,.T.);
#53108=EDGE_CURVE('',#40651,#40649,#21848,.T.);
#53109=EDGE_CURVE('',#39230,#40651,#21849,.T.);
#53110=EDGE_CURVE('',#39228,#40648,#21850,.T.);
#53111=EDGE_CURVE('',#40644,#39227,#21851,.T.);
#53112=EDGE_CURVE('',#40645,#38736,#21852,.T.);
#53113=EDGE_CURVE('',#40646,#38735,#21853,.T.);
#53114=EDGE_CURVE('',#40640,#38734,#21854,.T.);
#53115=EDGE_CURVE('',#40641,#38733,#21855,.T.);
#53116=EDGE_CURVE('',#39232,#40642,#21856,.T.);
#53117=EDGE_CURVE('',#39231,#40643,#21857,.T.);
#53118=EDGE_CURVE('',#40652,#40653,#29664,.T.);
#53119=EDGE_CURVE('',#40653,#40654,#25664,.T.);
#53120=EDGE_CURVE('',#40654,#40655,#996,.T.);
#53121=EDGE_CURVE('',#40655,#40656,#29665,.T.);
#53122=EDGE_CURVE('',#40656,#40652,#25665,.T.);
#53123=EDGE_CURVE('',#40657,#40658,#997,.T.);
#53124=EDGE_CURVE('',#40658,#40659,#25666,.T.);
#53125=EDGE_CURVE('',#40660,#40659,#29666,.T.);
#53126=EDGE_CURVE('',#40660,#40661,#25667,.T.);
#53127=EDGE_CURVE('',#40661,#40657,#29667,.T.);
#53128=EDGE_CURVE('',#40659,#40653,#25668,.T.);
#53129=EDGE_CURVE('',#40652,#40660,#21858,.T.);
#53130=EDGE_CURVE('',#40661,#40662,#25669,.T.);
#53131=EDGE_CURVE('',#40663,#40660,#998,.T.);
#53132=EDGE_CURVE('',#40662,#40663,#25670,.T.);
#53133=EDGE_CURVE('',#40663,#40652,#999,.T.);
#53134=EDGE_CURVE('',#40664,#40656,#25671,.T.);
#53135=EDGE_CURVE('',#40663,#40664,#25672,.T.);
#53136=EDGE_CURVE('',#39223,#40662,#21859,.T.);
#53137=EDGE_CURVE('',#40664,#40662,#21860,.T.);
#53138=EDGE_CURVE('',#39224,#40664,#21861,.T.);
#53139=EDGE_CURVE('',#39222,#40661,#21862,.T.);
#53140=EDGE_CURVE('',#40657,#39221,#21863,.T.);
#53141=EDGE_CURVE('',#40658,#38740,#21864,.T.);
#53142=EDGE_CURVE('',#40659,#38739,#21865,.T.);
#53143=EDGE_CURVE('',#40653,#38738,#21866,.T.);
#53144=EDGE_CURVE('',#40654,#38737,#21867,.T.);
#53145=EDGE_CURVE('',#39226,#40655,#21868,.T.);
#53146=EDGE_CURVE('',#39225,#40656,#21869,.T.);
#53147=EDGE_CURVE('',#40665,#40666,#29668,.T.);
#53148=EDGE_CURVE('',#40666,#40667,#25673,.T.);
#53149=EDGE_CURVE('',#40667,#40668,#1000,.T.);
#53150=EDGE_CURVE('',#40668,#40669,#29669,.T.);
#53151=EDGE_CURVE('',#40669,#40665,#25674,.T.);
#53152=EDGE_CURVE('',#40670,#40671,#1001,.T.);
#53153=EDGE_CURVE('',#40671,#40672,#25675,.T.);
#53154=EDGE_CURVE('',#40673,#40672,#29670,.T.);
#53155=EDGE_CURVE('',#40673,#40674,#25676,.T.);
#53156=EDGE_CURVE('',#40674,#40670,#29671,.T.);
#53157=EDGE_CURVE('',#40672,#40666,#25677,.T.);
#53158=EDGE_CURVE('',#40665,#40673,#21870,.T.);
#53159=EDGE_CURVE('',#40674,#40675,#25678,.T.);
#53160=EDGE_CURVE('',#40676,#40673,#1002,.T.);
#53161=EDGE_CURVE('',#40675,#40676,#25679,.T.);
#53162=EDGE_CURVE('',#40676,#40665,#1003,.T.);
#53163=EDGE_CURVE('',#40677,#40669,#25680,.T.);
#53164=EDGE_CURVE('',#40676,#40677,#25681,.T.);
#53165=EDGE_CURVE('',#39217,#40675,#21871,.T.);
#53166=EDGE_CURVE('',#40677,#40675,#21872,.T.);
#53167=EDGE_CURVE('',#39218,#40677,#21873,.T.);
#53168=EDGE_CURVE('',#39216,#40674,#21874,.T.);
#53169=EDGE_CURVE('',#40670,#39215,#21875,.T.);
#53170=EDGE_CURVE('',#40671,#38744,#21876,.T.);
#53171=EDGE_CURVE('',#40672,#38743,#21877,.T.);
#53172=EDGE_CURVE('',#40666,#38742,#21878,.T.);
#53173=EDGE_CURVE('',#40667,#38741,#21879,.T.);
#53174=EDGE_CURVE('',#39220,#40668,#21880,.T.);
#53175=EDGE_CURVE('',#39219,#40669,#21881,.T.);
#53176=EDGE_CURVE('',#40678,#40679,#29672,.T.);
#53177=EDGE_CURVE('',#40679,#40680,#25682,.T.);
#53178=EDGE_CURVE('',#40680,#40681,#1004,.T.);
#53179=EDGE_CURVE('',#40681,#40682,#29673,.T.);
#53180=EDGE_CURVE('',#40682,#40678,#25683,.T.);
#53181=EDGE_CURVE('',#40683,#40684,#1005,.T.);
#53182=EDGE_CURVE('',#40684,#40685,#25684,.T.);
#53183=EDGE_CURVE('',#40686,#40685,#29674,.T.);
#53184=EDGE_CURVE('',#40686,#40687,#25685,.T.);
#53185=EDGE_CURVE('',#40687,#40683,#29675,.T.);
#53186=EDGE_CURVE('',#40685,#40679,#25686,.T.);
#53187=EDGE_CURVE('',#40678,#40686,#21882,.T.);
#53188=EDGE_CURVE('',#40687,#40688,#25687,.T.);
#53189=EDGE_CURVE('',#40689,#40686,#1006,.T.);
#53190=EDGE_CURVE('',#40688,#40689,#25688,.T.);
#53191=EDGE_CURVE('',#40689,#40678,#1007,.T.);
#53192=EDGE_CURVE('',#40690,#40682,#25689,.T.);
#53193=EDGE_CURVE('',#40689,#40690,#25690,.T.);
#53194=EDGE_CURVE('',#39211,#40688,#21883,.T.);
#53195=EDGE_CURVE('',#40690,#40688,#21884,.T.);
#53196=EDGE_CURVE('',#39212,#40690,#21885,.T.);
#53197=EDGE_CURVE('',#39210,#40687,#21886,.T.);
#53198=EDGE_CURVE('',#40683,#39209,#21887,.T.);
#53199=EDGE_CURVE('',#40684,#38748,#21888,.T.);
#53200=EDGE_CURVE('',#40685,#38747,#21889,.T.);
#53201=EDGE_CURVE('',#40679,#38746,#21890,.T.);
#53202=EDGE_CURVE('',#40680,#38745,#21891,.T.);
#53203=EDGE_CURVE('',#39214,#40681,#21892,.T.);
#53204=EDGE_CURVE('',#39213,#40682,#21893,.T.);
#53205=EDGE_CURVE('',#40691,#40692,#29676,.T.);
#53206=EDGE_CURVE('',#40692,#40693,#25691,.T.);
#53207=EDGE_CURVE('',#40693,#40694,#1008,.T.);
#53208=EDGE_CURVE('',#40694,#40695,#29677,.T.);
#53209=EDGE_CURVE('',#40695,#40691,#25692,.T.);
#53210=EDGE_CURVE('',#40696,#40697,#1009,.T.);
#53211=EDGE_CURVE('',#40697,#40698,#25693,.T.);
#53212=EDGE_CURVE('',#40699,#40698,#29678,.T.);
#53213=EDGE_CURVE('',#40699,#40700,#25694,.T.);
#53214=EDGE_CURVE('',#40700,#40696,#29679,.T.);
#53215=EDGE_CURVE('',#40698,#40692,#25695,.T.);
#53216=EDGE_CURVE('',#40691,#40699,#21894,.T.);
#53217=EDGE_CURVE('',#40700,#40701,#25696,.T.);
#53218=EDGE_CURVE('',#40702,#40699,#1010,.T.);
#53219=EDGE_CURVE('',#40701,#40702,#25697,.T.);
#53220=EDGE_CURVE('',#40702,#40691,#1011,.T.);
#53221=EDGE_CURVE('',#40703,#40695,#25698,.T.);
#53222=EDGE_CURVE('',#40702,#40703,#25699,.T.);
#53223=EDGE_CURVE('',#39205,#40701,#21895,.T.);
#53224=EDGE_CURVE('',#40703,#40701,#21896,.T.);
#53225=EDGE_CURVE('',#39206,#40703,#21897,.T.);
#53226=EDGE_CURVE('',#39204,#40700,#21898,.T.);
#53227=EDGE_CURVE('',#40696,#39203,#21899,.T.);
#53228=EDGE_CURVE('',#40697,#38752,#21900,.T.);
#53229=EDGE_CURVE('',#40698,#38751,#21901,.T.);
#53230=EDGE_CURVE('',#40692,#38750,#21902,.T.);
#53231=EDGE_CURVE('',#40693,#38749,#21903,.T.);
#53232=EDGE_CURVE('',#39208,#40694,#21904,.T.);
#53233=EDGE_CURVE('',#39207,#40695,#21905,.T.);
#53234=EDGE_CURVE('',#40704,#40705,#29680,.T.);
#53235=EDGE_CURVE('',#40705,#40706,#25700,.T.);
#53236=EDGE_CURVE('',#40706,#40707,#1012,.T.);
#53237=EDGE_CURVE('',#40707,#40708,#29681,.T.);
#53238=EDGE_CURVE('',#40708,#40704,#25701,.T.);
#53239=EDGE_CURVE('',#40709,#40710,#1013,.T.);
#53240=EDGE_CURVE('',#40710,#40711,#25702,.T.);
#53241=EDGE_CURVE('',#40712,#40711,#29682,.T.);
#53242=EDGE_CURVE('',#40712,#40713,#25703,.T.);
#53243=EDGE_CURVE('',#40713,#40709,#29683,.T.);
#53244=EDGE_CURVE('',#40711,#40705,#25704,.T.);
#53245=EDGE_CURVE('',#40704,#40712,#21906,.T.);
#53246=EDGE_CURVE('',#40713,#40714,#25705,.T.);
#53247=EDGE_CURVE('',#40715,#40712,#1014,.T.);
#53248=EDGE_CURVE('',#40714,#40715,#25706,.T.);
#53249=EDGE_CURVE('',#40715,#40704,#1015,.T.);
#53250=EDGE_CURVE('',#40716,#40708,#25707,.T.);
#53251=EDGE_CURVE('',#40715,#40716,#25708,.T.);
#53252=EDGE_CURVE('',#39199,#40714,#21907,.T.);
#53253=EDGE_CURVE('',#40716,#40714,#21908,.T.);
#53254=EDGE_CURVE('',#39200,#40716,#21909,.T.);
#53255=EDGE_CURVE('',#39198,#40713,#21910,.T.);
#53256=EDGE_CURVE('',#40709,#39197,#21911,.T.);
#53257=EDGE_CURVE('',#40710,#38756,#21912,.T.);
#53258=EDGE_CURVE('',#40711,#38755,#21913,.T.);
#53259=EDGE_CURVE('',#40705,#38754,#21914,.T.);
#53260=EDGE_CURVE('',#40706,#38753,#21915,.T.);
#53261=EDGE_CURVE('',#39202,#40707,#21916,.T.);
#53262=EDGE_CURVE('',#39201,#40708,#21917,.T.);
#53263=EDGE_CURVE('',#40717,#40718,#29684,.T.);
#53264=EDGE_CURVE('',#40718,#40719,#25709,.T.);
#53265=EDGE_CURVE('',#40719,#40720,#1016,.T.);
#53266=EDGE_CURVE('',#40720,#40721,#29685,.T.);
#53267=EDGE_CURVE('',#40721,#40717,#25710,.T.);
#53268=EDGE_CURVE('',#40722,#40723,#1017,.T.);
#53269=EDGE_CURVE('',#40723,#40724,#25711,.T.);
#53270=EDGE_CURVE('',#40725,#40724,#29686,.T.);
#53271=EDGE_CURVE('',#40725,#40726,#25712,.T.);
#53272=EDGE_CURVE('',#40726,#40722,#29687,.T.);
#53273=EDGE_CURVE('',#40724,#40718,#25713,.T.);
#53274=EDGE_CURVE('',#40717,#40725,#21918,.T.);
#53275=EDGE_CURVE('',#40726,#40727,#25714,.T.);
#53276=EDGE_CURVE('',#40728,#40725,#1018,.T.);
#53277=EDGE_CURVE('',#40727,#40728,#25715,.T.);
#53278=EDGE_CURVE('',#40728,#40717,#1019,.T.);
#53279=EDGE_CURVE('',#40729,#40721,#25716,.T.);
#53280=EDGE_CURVE('',#40728,#40729,#25717,.T.);
#53281=EDGE_CURVE('',#39193,#40727,#21919,.T.);
#53282=EDGE_CURVE('',#40729,#40727,#21920,.T.);
#53283=EDGE_CURVE('',#39194,#40729,#21921,.T.);
#53284=EDGE_CURVE('',#39192,#40726,#21922,.T.);
#53285=EDGE_CURVE('',#40722,#39191,#21923,.T.);
#53286=EDGE_CURVE('',#40723,#38760,#21924,.T.);
#53287=EDGE_CURVE('',#40724,#38759,#21925,.T.);
#53288=EDGE_CURVE('',#40718,#38758,#21926,.T.);
#53289=EDGE_CURVE('',#40719,#38757,#21927,.T.);
#53290=EDGE_CURVE('',#39196,#40720,#21928,.T.);
#53291=EDGE_CURVE('',#39195,#40721,#21929,.T.);
#53292=EDGE_CURVE('',#40730,#40731,#29688,.T.);
#53293=EDGE_CURVE('',#40731,#40732,#25718,.T.);
#53294=EDGE_CURVE('',#40732,#40733,#1020,.T.);
#53295=EDGE_CURVE('',#40733,#40734,#29689,.T.);
#53296=EDGE_CURVE('',#40734,#40730,#25719,.T.);
#53297=EDGE_CURVE('',#40735,#40736,#1021,.T.);
#53298=EDGE_CURVE('',#40736,#40737,#25720,.T.);
#53299=EDGE_CURVE('',#40738,#40737,#29690,.T.);
#53300=EDGE_CURVE('',#40738,#40739,#25721,.T.);
#53301=EDGE_CURVE('',#40739,#40735,#29691,.T.);
#53302=EDGE_CURVE('',#40737,#40731,#25722,.T.);
#53303=EDGE_CURVE('',#40730,#40738,#21930,.T.);
#53304=EDGE_CURVE('',#40739,#40740,#25723,.T.);
#53305=EDGE_CURVE('',#40741,#40738,#1022,.T.);
#53306=EDGE_CURVE('',#40740,#40741,#25724,.T.);
#53307=EDGE_CURVE('',#40741,#40730,#1023,.T.);
#53308=EDGE_CURVE('',#40742,#40734,#25725,.T.);
#53309=EDGE_CURVE('',#40741,#40742,#25726,.T.);
#53310=EDGE_CURVE('',#39187,#40740,#21931,.T.);
#53311=EDGE_CURVE('',#40742,#40740,#21932,.T.);
#53312=EDGE_CURVE('',#39188,#40742,#21933,.T.);
#53313=EDGE_CURVE('',#39186,#40739,#21934,.T.);
#53314=EDGE_CURVE('',#40735,#39185,#21935,.T.);
#53315=EDGE_CURVE('',#40736,#38764,#21936,.T.);
#53316=EDGE_CURVE('',#40737,#38763,#21937,.T.);
#53317=EDGE_CURVE('',#40731,#38762,#21938,.T.);
#53318=EDGE_CURVE('',#40732,#38761,#21939,.T.);
#53319=EDGE_CURVE('',#39190,#40733,#21940,.T.);
#53320=EDGE_CURVE('',#39189,#40734,#21941,.T.);
#53321=EDGE_CURVE('',#40743,#40744,#29692,.T.);
#53322=EDGE_CURVE('',#40744,#40745,#25727,.T.);
#53323=EDGE_CURVE('',#40745,#40746,#1024,.T.);
#53324=EDGE_CURVE('',#40746,#40747,#29693,.T.);
#53325=EDGE_CURVE('',#40747,#40743,#25728,.T.);
#53326=EDGE_CURVE('',#40748,#40749,#1025,.T.);
#53327=EDGE_CURVE('',#40749,#40750,#25729,.T.);
#53328=EDGE_CURVE('',#40751,#40750,#29694,.T.);
#53329=EDGE_CURVE('',#40751,#40752,#25730,.T.);
#53330=EDGE_CURVE('',#40752,#40748,#29695,.T.);
#53331=EDGE_CURVE('',#40750,#40744,#25731,.T.);
#53332=EDGE_CURVE('',#40743,#40751,#21942,.T.);
#53333=EDGE_CURVE('',#40752,#40753,#25732,.T.);
#53334=EDGE_CURVE('',#40754,#40751,#1026,.T.);
#53335=EDGE_CURVE('',#40753,#40754,#25733,.T.);
#53336=EDGE_CURVE('',#40754,#40743,#1027,.T.);
#53337=EDGE_CURVE('',#40755,#40747,#25734,.T.);
#53338=EDGE_CURVE('',#40754,#40755,#25735,.T.);
#53339=EDGE_CURVE('',#39181,#40753,#21943,.T.);
#53340=EDGE_CURVE('',#40755,#40753,#21944,.T.);
#53341=EDGE_CURVE('',#39182,#40755,#21945,.T.);
#53342=EDGE_CURVE('',#39180,#40752,#21946,.T.);
#53343=EDGE_CURVE('',#40748,#39179,#21947,.T.);
#53344=EDGE_CURVE('',#40749,#38768,#21948,.T.);
#53345=EDGE_CURVE('',#40750,#38767,#21949,.T.);
#53346=EDGE_CURVE('',#40744,#38766,#21950,.T.);
#53347=EDGE_CURVE('',#40745,#38765,#21951,.T.);
#53348=EDGE_CURVE('',#39184,#40746,#21952,.T.);
#53349=EDGE_CURVE('',#39183,#40747,#21953,.T.);
#53350=EDGE_CURVE('',#40756,#40757,#29696,.T.);
#53351=EDGE_CURVE('',#40757,#40758,#25736,.T.);
#53352=EDGE_CURVE('',#40758,#40759,#1028,.T.);
#53353=EDGE_CURVE('',#40759,#40760,#29697,.T.);
#53354=EDGE_CURVE('',#40760,#40756,#25737,.T.);
#53355=EDGE_CURVE('',#40761,#40762,#1029,.T.);
#53356=EDGE_CURVE('',#40762,#40763,#25738,.T.);
#53357=EDGE_CURVE('',#40764,#40763,#29698,.T.);
#53358=EDGE_CURVE('',#40764,#40765,#25739,.T.);
#53359=EDGE_CURVE('',#40765,#40761,#29699,.T.);
#53360=EDGE_CURVE('',#40763,#40757,#25740,.T.);
#53361=EDGE_CURVE('',#40756,#40764,#21954,.T.);
#53362=EDGE_CURVE('',#40765,#40766,#25741,.T.);
#53363=EDGE_CURVE('',#40767,#40764,#1030,.T.);
#53364=EDGE_CURVE('',#40766,#40767,#25742,.T.);
#53365=EDGE_CURVE('',#40767,#40756,#1031,.T.);
#53366=EDGE_CURVE('',#40768,#40760,#25743,.T.);
#53367=EDGE_CURVE('',#40767,#40768,#25744,.T.);
#53368=EDGE_CURVE('',#39175,#40766,#21955,.T.);
#53369=EDGE_CURVE('',#40768,#40766,#21956,.T.);
#53370=EDGE_CURVE('',#39176,#40768,#21957,.T.);
#53371=EDGE_CURVE('',#39174,#40765,#21958,.T.);
#53372=EDGE_CURVE('',#40761,#39173,#21959,.T.);
#53373=EDGE_CURVE('',#40762,#38772,#21960,.T.);
#53374=EDGE_CURVE('',#40763,#38771,#21961,.T.);
#53375=EDGE_CURVE('',#40757,#38770,#21962,.T.);
#53376=EDGE_CURVE('',#40758,#38769,#21963,.T.);
#53377=EDGE_CURVE('',#39178,#40759,#21964,.T.);
#53378=EDGE_CURVE('',#39177,#40760,#21965,.T.);
#53379=EDGE_CURVE('',#40769,#40770,#29700,.T.);
#53380=EDGE_CURVE('',#40770,#40771,#25745,.T.);
#53381=EDGE_CURVE('',#40771,#40772,#1032,.T.);
#53382=EDGE_CURVE('',#40772,#40773,#29701,.T.);
#53383=EDGE_CURVE('',#40773,#40769,#25746,.T.);
#53384=EDGE_CURVE('',#40774,#40775,#1033,.T.);
#53385=EDGE_CURVE('',#40775,#40776,#25747,.T.);
#53386=EDGE_CURVE('',#40777,#40776,#29702,.T.);
#53387=EDGE_CURVE('',#40777,#40778,#25748,.T.);
#53388=EDGE_CURVE('',#40778,#40774,#29703,.T.);
#53389=EDGE_CURVE('',#40776,#40770,#25749,.T.);
#53390=EDGE_CURVE('',#40769,#40777,#21966,.T.);
#53391=EDGE_CURVE('',#40778,#40779,#25750,.T.);
#53392=EDGE_CURVE('',#40780,#40777,#1034,.T.);
#53393=EDGE_CURVE('',#40779,#40780,#25751,.T.);
#53394=EDGE_CURVE('',#40780,#40769,#1035,.T.);
#53395=EDGE_CURVE('',#40781,#40773,#25752,.T.);
#53396=EDGE_CURVE('',#40780,#40781,#25753,.T.);
#53397=EDGE_CURVE('',#39169,#40779,#21967,.T.);
#53398=EDGE_CURVE('',#40781,#40779,#21968,.T.);
#53399=EDGE_CURVE('',#39170,#40781,#21969,.T.);
#53400=EDGE_CURVE('',#39168,#40778,#21970,.T.);
#53401=EDGE_CURVE('',#40774,#39167,#21971,.T.);
#53402=EDGE_CURVE('',#40775,#38776,#21972,.T.);
#53403=EDGE_CURVE('',#40776,#38775,#21973,.T.);
#53404=EDGE_CURVE('',#40770,#38774,#21974,.T.);
#53405=EDGE_CURVE('',#40771,#38773,#21975,.T.);
#53406=EDGE_CURVE('',#39172,#40772,#21976,.T.);
#53407=EDGE_CURVE('',#39171,#40773,#21977,.T.);
#53408=EDGE_CURVE('',#40782,#40783,#29704,.T.);
#53409=EDGE_CURVE('',#40783,#40784,#25754,.T.);
#53410=EDGE_CURVE('',#40784,#40785,#1036,.T.);
#53411=EDGE_CURVE('',#40785,#40786,#29705,.T.);
#53412=EDGE_CURVE('',#40786,#40782,#25755,.T.);
#53413=EDGE_CURVE('',#40787,#40788,#1037,.T.);
#53414=EDGE_CURVE('',#40788,#40789,#25756,.T.);
#53415=EDGE_CURVE('',#40790,#40789,#29706,.T.);
#53416=EDGE_CURVE('',#40790,#40791,#25757,.T.);
#53417=EDGE_CURVE('',#40791,#40787,#29707,.T.);
#53418=EDGE_CURVE('',#40789,#40783,#25758,.T.);
#53419=EDGE_CURVE('',#40782,#40790,#21978,.T.);
#53420=EDGE_CURVE('',#40791,#40792,#25759,.T.);
#53421=EDGE_CURVE('',#40793,#40790,#1038,.T.);
#53422=EDGE_CURVE('',#40792,#40793,#25760,.T.);
#53423=EDGE_CURVE('',#40793,#40782,#1039,.T.);
#53424=EDGE_CURVE('',#40794,#40786,#25761,.T.);
#53425=EDGE_CURVE('',#40793,#40794,#25762,.T.);
#53426=EDGE_CURVE('',#39163,#40792,#21979,.T.);
#53427=EDGE_CURVE('',#40794,#40792,#21980,.T.);
#53428=EDGE_CURVE('',#39164,#40794,#21981,.T.);
#53429=EDGE_CURVE('',#39162,#40791,#21982,.T.);
#53430=EDGE_CURVE('',#40787,#39161,#21983,.T.);
#53431=EDGE_CURVE('',#40788,#38780,#21984,.T.);
#53432=EDGE_CURVE('',#40789,#38779,#21985,.T.);
#53433=EDGE_CURVE('',#40783,#38778,#21986,.T.);
#53434=EDGE_CURVE('',#40784,#38777,#21987,.T.);
#53435=EDGE_CURVE('',#39166,#40785,#21988,.T.);
#53436=EDGE_CURVE('',#39165,#40786,#21989,.T.);
#53437=EDGE_CURVE('',#40795,#40796,#29708,.T.);
#53438=EDGE_CURVE('',#40796,#40797,#25763,.T.);
#53439=EDGE_CURVE('',#40797,#40798,#1040,.T.);
#53440=EDGE_CURVE('',#40798,#40799,#29709,.T.);
#53441=EDGE_CURVE('',#40799,#40795,#25764,.T.);
#53442=EDGE_CURVE('',#40800,#40801,#1041,.T.);
#53443=EDGE_CURVE('',#40801,#40802,#25765,.T.);
#53444=EDGE_CURVE('',#40803,#40802,#29710,.T.);
#53445=EDGE_CURVE('',#40803,#40804,#25766,.T.);
#53446=EDGE_CURVE('',#40804,#40800,#29711,.T.);
#53447=EDGE_CURVE('',#40802,#40796,#25767,.T.);
#53448=EDGE_CURVE('',#40795,#40803,#21990,.T.);
#53449=EDGE_CURVE('',#40804,#40805,#25768,.T.);
#53450=EDGE_CURVE('',#40806,#40803,#1042,.T.);
#53451=EDGE_CURVE('',#40805,#40806,#25769,.T.);
#53452=EDGE_CURVE('',#40806,#40795,#1043,.T.);
#53453=EDGE_CURVE('',#40807,#40799,#25770,.T.);
#53454=EDGE_CURVE('',#40806,#40807,#25771,.T.);
#53455=EDGE_CURVE('',#39157,#40805,#21991,.T.);
#53456=EDGE_CURVE('',#40807,#40805,#21992,.T.);
#53457=EDGE_CURVE('',#39158,#40807,#21993,.T.);
#53458=EDGE_CURVE('',#39156,#40804,#21994,.T.);
#53459=EDGE_CURVE('',#40800,#39155,#21995,.T.);
#53460=EDGE_CURVE('',#40801,#38784,#21996,.T.);
#53461=EDGE_CURVE('',#40802,#38783,#21997,.T.);
#53462=EDGE_CURVE('',#40796,#38782,#21998,.T.);
#53463=EDGE_CURVE('',#40797,#38781,#21999,.T.);
#53464=EDGE_CURVE('',#39160,#40798,#22000,.T.);
#53465=EDGE_CURVE('',#39159,#40799,#22001,.T.);
#53466=EDGE_CURVE('',#40808,#40809,#29712,.T.);
#53467=EDGE_CURVE('',#40809,#40810,#25772,.T.);
#53468=EDGE_CURVE('',#40810,#40811,#1044,.T.);
#53469=EDGE_CURVE('',#40811,#40812,#29713,.T.);
#53470=EDGE_CURVE('',#40812,#40808,#25773,.T.);
#53471=EDGE_CURVE('',#40813,#40814,#1045,.T.);
#53472=EDGE_CURVE('',#40814,#40815,#25774,.T.);
#53473=EDGE_CURVE('',#40816,#40815,#29714,.T.);
#53474=EDGE_CURVE('',#40816,#40817,#25775,.T.);
#53475=EDGE_CURVE('',#40817,#40813,#29715,.T.);
#53476=EDGE_CURVE('',#40815,#40809,#25776,.T.);
#53477=EDGE_CURVE('',#40808,#40816,#22002,.T.);
#53478=EDGE_CURVE('',#40817,#40818,#25777,.T.);
#53479=EDGE_CURVE('',#40819,#40816,#1046,.T.);
#53480=EDGE_CURVE('',#40818,#40819,#25778,.T.);
#53481=EDGE_CURVE('',#40819,#40808,#1047,.T.);
#53482=EDGE_CURVE('',#40820,#40812,#25779,.T.);
#53483=EDGE_CURVE('',#40819,#40820,#25780,.T.);
#53484=EDGE_CURVE('',#39151,#40818,#22003,.T.);
#53485=EDGE_CURVE('',#40820,#40818,#22004,.T.);
#53486=EDGE_CURVE('',#39152,#40820,#22005,.T.);
#53487=EDGE_CURVE('',#39150,#40817,#22006,.T.);
#53488=EDGE_CURVE('',#40813,#39149,#22007,.T.);
#53489=EDGE_CURVE('',#40814,#38788,#22008,.T.);
#53490=EDGE_CURVE('',#40815,#38787,#22009,.T.);
#53491=EDGE_CURVE('',#40809,#38786,#22010,.T.);
#53492=EDGE_CURVE('',#40810,#38785,#22011,.T.);
#53493=EDGE_CURVE('',#39154,#40811,#22012,.T.);
#53494=EDGE_CURVE('',#39153,#40812,#22013,.T.);
#53495=EDGE_CURVE('',#40821,#40822,#29716,.T.);
#53496=EDGE_CURVE('',#40822,#40823,#25781,.T.);
#53497=EDGE_CURVE('',#40823,#40824,#1048,.T.);
#53498=EDGE_CURVE('',#40824,#40825,#29717,.T.);
#53499=EDGE_CURVE('',#40825,#40821,#25782,.T.);
#53500=EDGE_CURVE('',#40826,#40827,#1049,.T.);
#53501=EDGE_CURVE('',#40827,#40828,#25783,.T.);
#53502=EDGE_CURVE('',#40829,#40828,#29718,.T.);
#53503=EDGE_CURVE('',#40829,#40830,#25784,.T.);
#53504=EDGE_CURVE('',#40830,#40826,#29719,.T.);
#53505=EDGE_CURVE('',#40828,#40822,#25785,.T.);
#53506=EDGE_CURVE('',#40821,#40829,#22014,.T.);
#53507=EDGE_CURVE('',#40830,#40831,#25786,.T.);
#53508=EDGE_CURVE('',#40832,#40829,#1050,.T.);
#53509=EDGE_CURVE('',#40831,#40832,#25787,.T.);
#53510=EDGE_CURVE('',#40832,#40821,#1051,.T.);
#53511=EDGE_CURVE('',#40833,#40825,#25788,.T.);
#53512=EDGE_CURVE('',#40832,#40833,#25789,.T.);
#53513=EDGE_CURVE('',#39145,#40831,#22015,.T.);
#53514=EDGE_CURVE('',#40833,#40831,#22016,.T.);
#53515=EDGE_CURVE('',#39146,#40833,#22017,.T.);
#53516=EDGE_CURVE('',#39144,#40830,#22018,.T.);
#53517=EDGE_CURVE('',#40826,#39143,#22019,.T.);
#53518=EDGE_CURVE('',#40827,#38792,#22020,.T.);
#53519=EDGE_CURVE('',#40828,#38791,#22021,.T.);
#53520=EDGE_CURVE('',#40822,#38790,#22022,.T.);
#53521=EDGE_CURVE('',#40823,#38789,#22023,.T.);
#53522=EDGE_CURVE('',#39148,#40824,#22024,.T.);
#53523=EDGE_CURVE('',#39147,#40825,#22025,.T.);
#53524=EDGE_CURVE('',#40834,#40835,#29720,.T.);
#53525=EDGE_CURVE('',#40835,#40836,#25790,.T.);
#53526=EDGE_CURVE('',#40836,#40837,#1052,.T.);
#53527=EDGE_CURVE('',#40837,#40838,#29721,.T.);
#53528=EDGE_CURVE('',#40838,#40834,#25791,.T.);
#53529=EDGE_CURVE('',#40839,#40840,#1053,.T.);
#53530=EDGE_CURVE('',#40840,#40841,#25792,.T.);
#53531=EDGE_CURVE('',#40842,#40841,#29722,.T.);
#53532=EDGE_CURVE('',#40842,#40843,#25793,.T.);
#53533=EDGE_CURVE('',#40843,#40839,#29723,.T.);
#53534=EDGE_CURVE('',#40841,#40835,#25794,.T.);
#53535=EDGE_CURVE('',#40834,#40842,#22026,.T.);
#53536=EDGE_CURVE('',#40843,#40844,#25795,.T.);
#53537=EDGE_CURVE('',#40845,#40842,#1054,.T.);
#53538=EDGE_CURVE('',#40844,#40845,#25796,.T.);
#53539=EDGE_CURVE('',#40845,#40834,#1055,.T.);
#53540=EDGE_CURVE('',#40846,#40838,#25797,.T.);
#53541=EDGE_CURVE('',#40845,#40846,#25798,.T.);
#53542=EDGE_CURVE('',#39139,#40844,#22027,.T.);
#53543=EDGE_CURVE('',#40846,#40844,#22028,.T.);
#53544=EDGE_CURVE('',#39140,#40846,#22029,.T.);
#53545=EDGE_CURVE('',#39138,#40843,#22030,.T.);
#53546=EDGE_CURVE('',#40839,#39137,#22031,.T.);
#53547=EDGE_CURVE('',#40840,#38796,#22032,.T.);
#53548=EDGE_CURVE('',#40841,#38795,#22033,.T.);
#53549=EDGE_CURVE('',#40835,#38794,#22034,.T.);
#53550=EDGE_CURVE('',#40836,#38793,#22035,.T.);
#53551=EDGE_CURVE('',#39142,#40837,#22036,.T.);
#53552=EDGE_CURVE('',#39141,#40838,#22037,.T.);
#53553=EDGE_CURVE('',#40847,#40848,#29724,.T.);
#53554=EDGE_CURVE('',#40848,#40849,#25799,.T.);
#53555=EDGE_CURVE('',#40849,#40850,#1056,.T.);
#53556=EDGE_CURVE('',#40850,#40851,#29725,.T.);
#53557=EDGE_CURVE('',#40851,#40847,#25800,.T.);
#53558=EDGE_CURVE('',#40852,#40853,#1057,.T.);
#53559=EDGE_CURVE('',#40853,#40854,#25801,.T.);
#53560=EDGE_CURVE('',#40855,#40854,#29726,.T.);
#53561=EDGE_CURVE('',#40855,#40856,#25802,.T.);
#53562=EDGE_CURVE('',#40856,#40852,#29727,.T.);
#53563=EDGE_CURVE('',#40854,#40848,#25803,.T.);
#53564=EDGE_CURVE('',#40847,#40855,#22038,.T.);
#53565=EDGE_CURVE('',#40856,#40857,#25804,.T.);
#53566=EDGE_CURVE('',#40858,#40855,#1058,.T.);
#53567=EDGE_CURVE('',#40857,#40858,#25805,.T.);
#53568=EDGE_CURVE('',#40858,#40847,#1059,.T.);
#53569=EDGE_CURVE('',#40859,#40851,#25806,.T.);
#53570=EDGE_CURVE('',#40858,#40859,#25807,.T.);
#53571=EDGE_CURVE('',#39133,#40857,#22039,.T.);
#53572=EDGE_CURVE('',#40859,#40857,#22040,.T.);
#53573=EDGE_CURVE('',#39134,#40859,#22041,.T.);
#53574=EDGE_CURVE('',#39132,#40856,#22042,.T.);
#53575=EDGE_CURVE('',#40852,#39131,#22043,.T.);
#53576=EDGE_CURVE('',#40853,#38800,#22044,.T.);
#53577=EDGE_CURVE('',#40854,#38799,#22045,.T.);
#53578=EDGE_CURVE('',#40848,#38798,#22046,.T.);
#53579=EDGE_CURVE('',#40849,#38797,#22047,.T.);
#53580=EDGE_CURVE('',#39136,#40850,#22048,.T.);
#53581=EDGE_CURVE('',#39135,#40851,#22049,.T.);
#53582=EDGE_CURVE('',#40860,#40861,#29728,.T.);
#53583=EDGE_CURVE('',#40861,#40862,#25808,.T.);
#53584=EDGE_CURVE('',#40862,#40863,#1060,.T.);
#53585=EDGE_CURVE('',#40863,#40864,#29729,.T.);
#53586=EDGE_CURVE('',#40864,#40860,#25809,.T.);
#53587=EDGE_CURVE('',#40865,#40866,#1061,.T.);
#53588=EDGE_CURVE('',#40866,#40867,#25810,.T.);
#53589=EDGE_CURVE('',#40868,#40867,#29730,.T.);
#53590=EDGE_CURVE('',#40868,#40869,#25811,.T.);
#53591=EDGE_CURVE('',#40869,#40865,#29731,.T.);
#53592=EDGE_CURVE('',#40867,#40861,#25812,.T.);
#53593=EDGE_CURVE('',#40860,#40868,#22050,.T.);
#53594=EDGE_CURVE('',#40869,#40870,#25813,.T.);
#53595=EDGE_CURVE('',#40871,#40868,#1062,.T.);
#53596=EDGE_CURVE('',#40870,#40871,#25814,.T.);
#53597=EDGE_CURVE('',#40871,#40860,#1063,.T.);
#53598=EDGE_CURVE('',#40872,#40864,#25815,.T.);
#53599=EDGE_CURVE('',#40871,#40872,#25816,.T.);
#53600=EDGE_CURVE('',#39127,#40870,#22051,.T.);
#53601=EDGE_CURVE('',#40872,#40870,#22052,.T.);
#53602=EDGE_CURVE('',#39128,#40872,#22053,.T.);
#53603=EDGE_CURVE('',#39126,#40869,#22054,.T.);
#53604=EDGE_CURVE('',#40865,#39125,#22055,.T.);
#53605=EDGE_CURVE('',#40866,#38804,#22056,.T.);
#53606=EDGE_CURVE('',#40867,#38803,#22057,.T.);
#53607=EDGE_CURVE('',#40861,#38802,#22058,.T.);
#53608=EDGE_CURVE('',#40862,#38801,#22059,.T.);
#53609=EDGE_CURVE('',#39130,#40863,#22060,.T.);
#53610=EDGE_CURVE('',#39129,#40864,#22061,.T.);
#53611=EDGE_CURVE('',#40873,#40874,#29732,.T.);
#53612=EDGE_CURVE('',#40874,#40875,#25817,.T.);
#53613=EDGE_CURVE('',#40875,#40876,#1064,.T.);
#53614=EDGE_CURVE('',#40876,#40877,#29733,.T.);
#53615=EDGE_CURVE('',#40877,#40873,#25818,.T.);
#53616=EDGE_CURVE('',#40878,#40879,#1065,.T.);
#53617=EDGE_CURVE('',#40879,#40880,#25819,.T.);
#53618=EDGE_CURVE('',#40881,#40880,#29734,.T.);
#53619=EDGE_CURVE('',#40881,#40882,#25820,.T.);
#53620=EDGE_CURVE('',#40882,#40878,#29735,.T.);
#53621=EDGE_CURVE('',#40880,#40874,#25821,.T.);
#53622=EDGE_CURVE('',#40873,#40881,#22062,.T.);
#53623=EDGE_CURVE('',#40882,#40883,#25822,.T.);
#53624=EDGE_CURVE('',#40884,#40881,#1066,.T.);
#53625=EDGE_CURVE('',#40883,#40884,#25823,.T.);
#53626=EDGE_CURVE('',#40884,#40873,#1067,.T.);
#53627=EDGE_CURVE('',#40885,#40877,#25824,.T.);
#53628=EDGE_CURVE('',#40884,#40885,#25825,.T.);
#53629=EDGE_CURVE('',#39121,#40883,#22063,.T.);
#53630=EDGE_CURVE('',#40885,#40883,#22064,.T.);
#53631=EDGE_CURVE('',#39122,#40885,#22065,.T.);
#53632=EDGE_CURVE('',#39120,#40882,#22066,.T.);
#53633=EDGE_CURVE('',#40878,#39119,#22067,.T.);
#53634=EDGE_CURVE('',#40879,#38808,#22068,.T.);
#53635=EDGE_CURVE('',#40880,#38807,#22069,.T.);
#53636=EDGE_CURVE('',#40874,#38806,#22070,.T.);
#53637=EDGE_CURVE('',#40875,#38805,#22071,.T.);
#53638=EDGE_CURVE('',#39124,#40876,#22072,.T.);
#53639=EDGE_CURVE('',#39123,#40877,#22073,.T.);
#53640=EDGE_CURVE('',#40886,#40887,#29736,.T.);
#53641=EDGE_CURVE('',#40887,#40888,#25826,.T.);
#53642=EDGE_CURVE('',#40888,#40889,#1068,.T.);
#53643=EDGE_CURVE('',#40889,#40890,#29737,.T.);
#53644=EDGE_CURVE('',#40890,#40886,#25827,.T.);
#53645=EDGE_CURVE('',#40891,#40892,#1069,.T.);
#53646=EDGE_CURVE('',#40892,#40893,#25828,.T.);
#53647=EDGE_CURVE('',#40894,#40893,#29738,.T.);
#53648=EDGE_CURVE('',#40894,#40895,#25829,.T.);
#53649=EDGE_CURVE('',#40895,#40891,#29739,.T.);
#53650=EDGE_CURVE('',#40893,#40887,#25830,.T.);
#53651=EDGE_CURVE('',#40886,#40894,#22074,.T.);
#53652=EDGE_CURVE('',#40895,#40896,#25831,.T.);
#53653=EDGE_CURVE('',#40897,#40894,#1070,.T.);
#53654=EDGE_CURVE('',#40896,#40897,#25832,.T.);
#53655=EDGE_CURVE('',#40897,#40886,#1071,.T.);
#53656=EDGE_CURVE('',#40898,#40890,#25833,.T.);
#53657=EDGE_CURVE('',#40897,#40898,#25834,.T.);
#53658=EDGE_CURVE('',#39115,#40896,#22075,.T.);
#53659=EDGE_CURVE('',#40898,#40896,#22076,.T.);
#53660=EDGE_CURVE('',#39116,#40898,#22077,.T.);
#53661=EDGE_CURVE('',#39114,#40895,#22078,.T.);
#53662=EDGE_CURVE('',#40891,#39113,#22079,.T.);
#53663=EDGE_CURVE('',#40892,#38812,#22080,.T.);
#53664=EDGE_CURVE('',#40893,#38811,#22081,.T.);
#53665=EDGE_CURVE('',#40887,#38810,#22082,.T.);
#53666=EDGE_CURVE('',#40888,#38809,#22083,.T.);
#53667=EDGE_CURVE('',#39118,#40889,#22084,.T.);
#53668=EDGE_CURVE('',#39117,#40890,#22085,.T.);
#53669=EDGE_CURVE('',#40899,#40900,#29740,.T.);
#53670=EDGE_CURVE('',#40900,#40901,#25835,.T.);
#53671=EDGE_CURVE('',#40901,#40902,#1072,.T.);
#53672=EDGE_CURVE('',#40902,#40903,#29741,.T.);
#53673=EDGE_CURVE('',#40903,#40899,#25836,.T.);
#53674=EDGE_CURVE('',#40904,#40905,#1073,.T.);
#53675=EDGE_CURVE('',#40905,#40906,#25837,.T.);
#53676=EDGE_CURVE('',#40907,#40906,#29742,.T.);
#53677=EDGE_CURVE('',#40907,#40908,#25838,.T.);
#53678=EDGE_CURVE('',#40908,#40904,#29743,.T.);
#53679=EDGE_CURVE('',#40906,#40900,#25839,.T.);
#53680=EDGE_CURVE('',#40899,#40907,#22086,.T.);
#53681=EDGE_CURVE('',#40908,#40909,#25840,.T.);
#53682=EDGE_CURVE('',#40910,#40907,#1074,.T.);
#53683=EDGE_CURVE('',#40909,#40910,#25841,.T.);
#53684=EDGE_CURVE('',#40910,#40899,#1075,.T.);
#53685=EDGE_CURVE('',#40911,#40903,#25842,.T.);
#53686=EDGE_CURVE('',#40910,#40911,#25843,.T.);
#53687=EDGE_CURVE('',#39109,#40909,#22087,.T.);
#53688=EDGE_CURVE('',#40911,#40909,#22088,.T.);
#53689=EDGE_CURVE('',#39110,#40911,#22089,.T.);
#53690=EDGE_CURVE('',#39108,#40908,#22090,.T.);
#53691=EDGE_CURVE('',#40904,#39107,#22091,.T.);
#53692=EDGE_CURVE('',#40905,#38816,#22092,.T.);
#53693=EDGE_CURVE('',#40906,#38815,#22093,.T.);
#53694=EDGE_CURVE('',#40900,#38814,#22094,.T.);
#53695=EDGE_CURVE('',#40901,#38813,#22095,.T.);
#53696=EDGE_CURVE('',#39112,#40902,#22096,.T.);
#53697=EDGE_CURVE('',#39111,#40903,#22097,.T.);
#53698=EDGE_CURVE('',#40912,#40913,#29744,.T.);
#53699=EDGE_CURVE('',#40913,#40914,#25844,.T.);
#53700=EDGE_CURVE('',#40914,#40915,#1076,.T.);
#53701=EDGE_CURVE('',#40915,#40916,#29745,.T.);
#53702=EDGE_CURVE('',#40916,#40912,#25845,.T.);
#53703=EDGE_CURVE('',#40917,#40918,#1077,.T.);
#53704=EDGE_CURVE('',#40918,#40919,#25846,.T.);
#53705=EDGE_CURVE('',#40920,#40919,#29746,.T.);
#53706=EDGE_CURVE('',#40920,#40921,#25847,.T.);
#53707=EDGE_CURVE('',#40921,#40917,#29747,.T.);
#53708=EDGE_CURVE('',#40919,#40913,#25848,.T.);
#53709=EDGE_CURVE('',#40912,#40920,#22098,.T.);
#53710=EDGE_CURVE('',#40921,#40922,#25849,.T.);
#53711=EDGE_CURVE('',#40923,#40920,#1078,.T.);
#53712=EDGE_CURVE('',#40922,#40923,#25850,.T.);
#53713=EDGE_CURVE('',#40923,#40912,#1079,.T.);
#53714=EDGE_CURVE('',#40924,#40916,#25851,.T.);
#53715=EDGE_CURVE('',#40923,#40924,#25852,.T.);
#53716=EDGE_CURVE('',#39103,#40922,#22099,.T.);
#53717=EDGE_CURVE('',#40924,#40922,#22100,.T.);
#53718=EDGE_CURVE('',#39104,#40924,#22101,.T.);
#53719=EDGE_CURVE('',#39102,#40921,#22102,.T.);
#53720=EDGE_CURVE('',#40917,#39101,#22103,.T.);
#53721=EDGE_CURVE('',#40918,#38820,#22104,.T.);
#53722=EDGE_CURVE('',#40919,#38819,#22105,.T.);
#53723=EDGE_CURVE('',#40913,#38818,#22106,.T.);
#53724=EDGE_CURVE('',#40914,#38817,#22107,.T.);
#53725=EDGE_CURVE('',#39106,#40915,#22108,.T.);
#53726=EDGE_CURVE('',#39105,#40916,#22109,.T.);
#53727=EDGE_CURVE('',#40925,#40926,#29748,.T.);
#53728=EDGE_CURVE('',#40927,#40925,#4326,.T.);
#53729=EDGE_CURVE('',#40927,#40926,#22110,.T.);
#53730=EDGE_CURVE('',#40928,#40929,#29749,.T.);
#53731=EDGE_CURVE('',#40925,#40928,#4327,.T.);
#53732=EDGE_CURVE('',#40926,#40929,#4328,.T.);
#53733=EDGE_CURVE('',#40930,#40931,#29750,.T.);
#53734=EDGE_CURVE('',#40928,#40930,#4329,.T.);
#53735=EDGE_CURVE('',#40929,#40931,#4330,.T.);
#53736=EDGE_CURVE('',#40932,#40933,#29751,.T.);
#53737=EDGE_CURVE('',#40930,#40932,#4331,.T.);
#53738=EDGE_CURVE('',#40931,#40933,#4332,.T.);
#53739=EDGE_CURVE('',#40934,#40935,#29752,.T.);
#53740=EDGE_CURVE('',#40932,#40934,#4333,.T.);
#53741=EDGE_CURVE('',#40933,#40935,#4334,.T.);
#53742=EDGE_CURVE('',#40936,#40937,#29753,.T.);
#53743=EDGE_CURVE('',#40934,#40936,#4335,.T.);
#53744=EDGE_CURVE('',#40935,#40937,#4336,.T.);
#53745=EDGE_CURVE('',#40938,#40939,#29754,.T.);
#53746=EDGE_CURVE('',#40936,#40938,#4337,.T.);
#53747=EDGE_CURVE('',#40937,#40939,#4338,.T.);
#53748=EDGE_CURVE('',#40940,#40941,#29755,.T.);
#53749=EDGE_CURVE('',#40938,#40940,#4339,.T.);
#53750=EDGE_CURVE('',#40939,#40941,#4340,.T.);
#53751=EDGE_CURVE('',#40942,#40943,#29756,.T.);
#53752=EDGE_CURVE('',#40940,#40942,#4341,.T.);
#53753=EDGE_CURVE('',#40941,#40943,#4342,.T.);
#53754=EDGE_CURVE('',#40944,#40945,#29757,.T.);
#53755=EDGE_CURVE('',#40942,#40944,#4343,.T.);
#53756=EDGE_CURVE('',#40943,#40945,#4344,.T.);
#53757=EDGE_CURVE('',#40946,#40947,#29758,.T.);
#53758=EDGE_CURVE('',#40944,#40946,#4345,.T.);
#53759=EDGE_CURVE('',#40945,#40947,#4346,.T.);
#53760=EDGE_CURVE('',#40948,#40949,#29759,.T.);
#53761=EDGE_CURVE('',#40946,#40948,#4347,.T.);
#53762=EDGE_CURVE('',#40947,#40949,#4348,.T.);
#53763=EDGE_CURVE('',#40950,#40951,#29760,.T.);
#53764=EDGE_CURVE('',#40948,#40950,#4349,.T.);
#53765=EDGE_CURVE('',#40949,#40951,#4350,.T.);
#53766=EDGE_CURVE('',#40952,#40953,#29761,.T.);
#53767=EDGE_CURVE('',#40950,#40952,#4351,.T.);
#53768=EDGE_CURVE('',#40951,#40953,#4352,.T.);
#53769=EDGE_CURVE('',#40954,#40955,#29762,.T.);
#53770=EDGE_CURVE('',#40952,#40954,#4353,.T.);
#53771=EDGE_CURVE('',#40953,#40955,#4354,.T.);
#53772=EDGE_CURVE('',#40956,#40957,#29763,.T.);
#53773=EDGE_CURVE('',#40954,#40956,#4355,.T.);
#53774=EDGE_CURVE('',#40955,#40957,#4356,.T.);
#53775=EDGE_CURVE('',#40958,#40959,#29764,.T.);
#53776=EDGE_CURVE('',#40956,#40958,#4357,.T.);
#53777=EDGE_CURVE('',#40957,#40959,#4358,.T.);
#53778=EDGE_CURVE('',#40960,#40961,#29765,.T.);
#53779=EDGE_CURVE('',#40958,#40960,#4359,.T.);
#53780=EDGE_CURVE('',#40959,#40961,#4360,.T.);
#53781=EDGE_CURVE('',#40962,#40963,#29766,.T.);
#53782=EDGE_CURVE('',#40960,#40962,#4361,.T.);
#53783=EDGE_CURVE('',#40961,#40963,#4362,.T.);
#53784=EDGE_CURVE('',#40964,#40965,#29767,.T.);
#53785=EDGE_CURVE('',#40962,#40964,#4363,.T.);
#53786=EDGE_CURVE('',#40963,#40965,#4364,.T.);
#53787=EDGE_CURVE('',#40966,#40967,#29768,.T.);
#53788=EDGE_CURVE('',#40964,#40966,#4365,.T.);
#53789=EDGE_CURVE('',#40965,#40967,#4366,.T.);
#53790=EDGE_CURVE('',#40968,#40969,#29769,.T.);
#53791=EDGE_CURVE('',#40966,#40968,#4367,.T.);
#53792=EDGE_CURVE('',#40967,#40969,#4368,.T.);
#53793=EDGE_CURVE('',#40970,#40971,#29770,.T.);
#53794=EDGE_CURVE('',#40968,#40970,#4369,.T.);
#53795=EDGE_CURVE('',#40969,#40971,#4370,.T.);
#53796=EDGE_CURVE('',#40972,#40973,#29771,.T.);
#53797=EDGE_CURVE('',#40970,#40972,#4371,.T.);
#53798=EDGE_CURVE('',#40971,#40973,#4372,.T.);
#53799=EDGE_CURVE('',#40974,#40975,#29772,.T.);
#53800=EDGE_CURVE('',#40972,#40974,#4373,.T.);
#53801=EDGE_CURVE('',#40973,#40975,#4374,.T.);
#53802=EDGE_CURVE('',#40976,#40977,#29773,.T.);
#53803=EDGE_CURVE('',#40974,#40976,#4375,.T.);
#53804=EDGE_CURVE('',#40975,#40977,#4376,.T.);
#53805=EDGE_CURVE('',#40978,#40979,#29774,.T.);
#53806=EDGE_CURVE('',#40976,#40978,#4377,.T.);
#53807=EDGE_CURVE('',#40977,#40979,#4378,.T.);
#53808=EDGE_CURVE('',#40980,#40981,#29775,.T.);
#53809=EDGE_CURVE('',#40978,#40980,#4379,.T.);
#53810=EDGE_CURVE('',#40979,#40981,#4380,.T.);
#53811=EDGE_CURVE('',#40982,#40983,#29776,.T.);
#53812=EDGE_CURVE('',#40980,#40982,#4381,.T.);
#53813=EDGE_CURVE('',#40981,#40983,#4382,.T.);
#53814=EDGE_CURVE('',#40984,#40985,#29777,.T.);
#53815=EDGE_CURVE('',#40982,#40984,#4383,.T.);
#53816=EDGE_CURVE('',#40983,#40985,#4384,.T.);
#53817=EDGE_CURVE('',#40986,#40987,#29778,.T.);
#53818=EDGE_CURVE('',#40984,#40986,#4385,.T.);
#53819=EDGE_CURVE('',#40985,#40987,#4386,.T.);
#53820=EDGE_CURVE('',#40988,#40989,#29779,.T.);
#53821=EDGE_CURVE('',#40986,#40988,#4387,.T.);
#53822=EDGE_CURVE('',#40987,#40989,#4388,.T.);
#53823=EDGE_CURVE('',#40990,#40991,#29780,.T.);
#53824=EDGE_CURVE('',#40988,#40990,#4389,.T.);
#53825=EDGE_CURVE('',#40989,#40991,#4390,.T.);
#53826=EDGE_CURVE('',#40992,#40993,#29781,.T.);
#53827=EDGE_CURVE('',#40990,#40992,#4391,.T.);
#53828=EDGE_CURVE('',#40991,#40993,#4392,.T.);
#53829=EDGE_CURVE('',#40994,#40995,#29782,.T.);
#53830=EDGE_CURVE('',#40992,#40994,#4393,.T.);
#53831=EDGE_CURVE('',#40993,#40995,#4394,.T.);
#53832=EDGE_CURVE('',#40996,#40997,#29783,.T.);
#53833=EDGE_CURVE('',#40994,#40996,#4395,.T.);
#53834=EDGE_CURVE('',#40995,#40997,#4396,.T.);
#53835=EDGE_CURVE('',#40998,#40999,#29784,.T.);
#53836=EDGE_CURVE('',#40998,#41000,#25853,.T.);
#53837=EDGE_CURVE('',#41000,#41001,#22111,.T.);
#53838=EDGE_CURVE('',#41001,#40999,#25854,.T.);
#53839=EDGE_CURVE('',#41002,#41003,#29785,.T.);
#53840=EDGE_CURVE('',#40926,#41002,#25855,.F.);
#53841=EDGE_CURVE('',#40926,#41003,#22112,.T.);
#53842=EDGE_CURVE('',#41004,#41005,#29786,.T.);
#53843=EDGE_CURVE('',#41006,#41004,#25856,.F.);
#53844=EDGE_CURVE('',#41006,#41007,#22113,.T.);
#53845=EDGE_CURVE('',#41005,#41007,#25857,.F.);
#53846=EDGE_CURVE('',#41008,#41009,#29787,.T.);
#53847=EDGE_CURVE('',#41004,#41008,#25858,.F.);
#53848=EDGE_CURVE('',#41009,#41005,#25859,.F.);
#53849=EDGE_CURVE('',#41010,#41011,#29788,.T.);
#53850=EDGE_CURVE('',#41008,#41010,#25860,.F.);
#53851=EDGE_CURVE('',#41011,#41009,#25861,.F.);
#53852=EDGE_CURVE('',#41012,#41013,#29789,.T.);
#53853=EDGE_CURVE('',#41010,#41012,#25862,.F.);
#53854=EDGE_CURVE('',#41013,#41011,#25863,.F.);
#53855=EDGE_CURVE('',#41014,#41015,#29790,.T.);
#53856=EDGE_CURVE('',#41012,#41014,#25864,.F.);
#53857=EDGE_CURVE('',#41015,#41013,#25865,.F.);
#53858=EDGE_CURVE('',#41016,#41017,#29791,.T.);
#53859=EDGE_CURVE('',#41014,#41016,#25866,.F.);
#53860=EDGE_CURVE('',#41017,#41015,#25867,.F.);
#53861=EDGE_CURVE('',#41018,#41019,#29792,.T.);
#53862=EDGE_CURVE('',#41016,#41018,#25868,.F.);
#53863=EDGE_CURVE('',#41019,#41017,#25869,.F.);
#53864=EDGE_CURVE('',#41020,#41021,#29793,.T.);
#53865=EDGE_CURVE('',#41018,#41020,#25870,.F.);
#53866=EDGE_CURVE('',#41021,#41019,#25871,.F.);
#53867=EDGE_CURVE('',#41022,#41023,#29794,.T.);
#53868=EDGE_CURVE('',#41020,#41022,#25872,.F.);
#53869=EDGE_CURVE('',#41023,#41021,#25873,.F.);
#53870=EDGE_CURVE('',#41024,#41025,#29795,.T.);
#53871=EDGE_CURVE('',#41022,#41024,#25874,.F.);
#53872=EDGE_CURVE('',#41025,#41023,#25875,.F.);
#53873=EDGE_CURVE('',#41026,#41027,#29796,.T.);
#53874=EDGE_CURVE('',#41024,#41026,#25876,.F.);
#53875=EDGE_CURVE('',#41027,#41025,#25877,.F.);
#53876=EDGE_CURVE('',#41028,#41029,#29797,.T.);
#53877=EDGE_CURVE('',#41026,#41028,#25878,.F.);
#53878=EDGE_CURVE('',#41029,#41027,#25879,.F.);
#53879=EDGE_CURVE('',#41030,#41031,#29798,.T.);
#53880=EDGE_CURVE('',#41028,#41030,#25880,.F.);
#53881=EDGE_CURVE('',#41031,#41029,#25881,.F.);
#53882=EDGE_CURVE('',#41032,#41033,#29799,.T.);
#53883=EDGE_CURVE('',#41030,#41032,#25882,.F.);
#53884=EDGE_CURVE('',#41033,#41031,#25883,.F.);
#53885=EDGE_CURVE('',#41034,#41035,#29800,.T.);
#53886=EDGE_CURVE('',#41032,#41034,#25884,.F.);
#53887=EDGE_CURVE('',#41035,#41033,#25885,.F.);
#53888=EDGE_CURVE('',#41036,#41037,#29801,.T.);
#53889=EDGE_CURVE('',#41034,#41036,#25886,.F.);
#53890=EDGE_CURVE('',#41037,#41035,#25887,.F.);
#53891=EDGE_CURVE('',#41038,#41039,#29802,.T.);
#53892=EDGE_CURVE('',#41036,#41038,#25888,.F.);
#53893=EDGE_CURVE('',#41039,#41037,#25889,.F.);
#53894=EDGE_CURVE('',#41040,#41041,#29803,.T.);
#53895=EDGE_CURVE('',#41038,#41040,#25890,.F.);
#53896=EDGE_CURVE('',#41041,#41039,#25891,.F.);
#53897=EDGE_CURVE('',#41042,#41043,#29804,.T.);
#53898=EDGE_CURVE('',#41040,#41042,#25892,.F.);
#53899=EDGE_CURVE('',#41043,#41041,#25893,.F.);
#53900=EDGE_CURVE('',#41044,#41045,#29805,.T.);
#53901=EDGE_CURVE('',#41042,#41044,#25894,.F.);
#53902=EDGE_CURVE('',#41045,#41043,#25895,.F.);
#53903=EDGE_CURVE('',#41046,#41047,#29806,.T.);
#53904=EDGE_CURVE('',#41044,#41046,#25896,.F.);
#53905=EDGE_CURVE('',#41047,#41045,#25897,.F.);
#53906=EDGE_CURVE('',#41048,#41049,#29807,.T.);
#53907=EDGE_CURVE('',#41046,#41048,#25898,.F.);
#53908=EDGE_CURVE('',#41049,#41047,#25899,.F.);
#53909=EDGE_CURVE('',#41050,#41051,#29808,.T.);
#53910=EDGE_CURVE('',#41048,#41050,#25900,.F.);
#53911=EDGE_CURVE('',#41051,#41049,#25901,.F.);
#53912=EDGE_CURVE('',#41052,#41053,#29809,.T.);
#53913=EDGE_CURVE('',#41050,#41052,#25902,.F.);
#53914=EDGE_CURVE('',#41053,#41051,#25903,.F.);
#53915=EDGE_CURVE('',#41054,#41055,#29810,.T.);
#53916=EDGE_CURVE('',#41052,#41054,#25904,.F.);
#53917=EDGE_CURVE('',#41055,#41053,#25905,.F.);
#53918=EDGE_CURVE('',#41056,#41057,#29811,.T.);
#53919=EDGE_CURVE('',#41054,#41056,#25906,.F.);
#53920=EDGE_CURVE('',#41057,#41055,#25907,.F.);
#53921=EDGE_CURVE('',#41058,#41059,#29812,.T.);
#53922=EDGE_CURVE('',#41056,#41058,#25908,.F.);
#53923=EDGE_CURVE('',#41059,#41057,#25909,.F.);
#53924=EDGE_CURVE('',#41060,#41061,#29813,.T.);
#53925=EDGE_CURVE('',#41058,#41060,#25910,.F.);
#53926=EDGE_CURVE('',#41061,#41059,#25911,.F.);
#53927=EDGE_CURVE('',#41062,#41063,#29814,.T.);
#53928=EDGE_CURVE('',#41060,#41062,#25912,.F.);
#53929=EDGE_CURVE('',#41063,#41061,#25913,.F.);
#53930=EDGE_CURVE('',#41064,#41065,#29815,.T.);
#53931=EDGE_CURVE('',#41062,#41064,#25914,.F.);
#53932=EDGE_CURVE('',#41065,#41063,#25915,.F.);
#53933=EDGE_CURVE('',#41066,#41067,#29816,.T.);
#53934=EDGE_CURVE('',#41064,#41066,#25916,.F.);
#53935=EDGE_CURVE('',#41067,#41065,#25917,.F.);
#53936=EDGE_CURVE('',#41068,#41069,#29817,.T.);
#53937=EDGE_CURVE('',#41066,#41068,#25918,.F.);
#53938=EDGE_CURVE('',#41070,#41067,#25919,.F.);
#53939=EDGE_CURVE('',#41069,#41070,#25920,.F.);
#53940=EDGE_CURVE('',#41071,#41072,#29818,.T.);
#53941=EDGE_CURVE('',#41068,#41071,#25921,.F.);
#53942=EDGE_CURVE('',#41072,#41069,#25922,.F.);
#53943=EDGE_CURVE('',#41073,#41074,#29819,.T.);
#53944=EDGE_CURVE('',#41071,#41073,#25923,.F.);
#53945=EDGE_CURVE('',#41074,#41072,#25924,.F.);
#53946=EDGE_CURVE('',#41075,#41075,#22114,.T.);
#53947=EDGE_CURVE('',#41075,#40998,#29820,.T.);
#53948=EDGE_CURVE('',#41076,#40998,#22115,.T.);
#53949=EDGE_CURVE('',#41077,#41076,#25925,.F.);
#53950=EDGE_CURVE('',#41077,#41078,#29821,.T.);
#53951=EDGE_CURVE('',#40998,#41078,#25926,.F.);
#53952=EDGE_CURVE('',#41079,#41080,#22116,.T.);
#53953=EDGE_CURVE('',#41081,#41079,#22117,.T.);
#53954=EDGE_CURVE('',#41082,#41081,#22118,.T.);
#53955=EDGE_CURVE('',#41082,#41080,#22119,.T.);
#53956=EDGE_CURVE('',#41083,#41084,#22120,.T.);
#53957=EDGE_CURVE('',#41085,#41083,#22121,.T.);
#53958=EDGE_CURVE('',#41086,#41085,#22122,.T.);
#53959=EDGE_CURVE('',#41086,#41084,#22123,.T.);
#53960=EDGE_CURVE('',#41087,#41088,#22124,.T.);
#53961=EDGE_CURVE('',#41089,#41087,#22125,.T.);
#53962=EDGE_CURVE('',#41090,#41089,#22126,.T.);
#53963=EDGE_CURVE('',#41090,#41088,#22127,.T.);
#53964=EDGE_CURVE('',#41091,#41092,#22128,.T.);
#53965=EDGE_CURVE('',#41093,#41091,#22129,.T.);
#53966=EDGE_CURVE('',#41094,#41093,#22130,.T.);
#53967=EDGE_CURVE('',#41094,#41092,#22131,.T.);
#53968=EDGE_CURVE('',#41095,#41096,#22132,.T.);
#53969=EDGE_CURVE('',#41097,#41095,#22133,.T.);
#53970=EDGE_CURVE('',#41098,#41097,#22134,.T.);
#53971=EDGE_CURVE('',#41098,#41096,#22135,.T.);
#53972=EDGE_CURVE('',#41099,#41100,#22136,.T.);
#53973=EDGE_CURVE('',#41101,#41099,#22137,.T.);
#53974=EDGE_CURVE('',#41102,#41101,#22138,.T.);
#53975=EDGE_CURVE('',#41102,#41100,#22139,.T.);
#53976=EDGE_CURVE('',#41103,#41104,#22140,.T.);
#53977=EDGE_CURVE('',#41105,#41103,#22141,.T.);
#53978=EDGE_CURVE('',#41106,#41105,#22142,.T.);
#53979=EDGE_CURVE('',#41106,#41104,#22143,.T.);
#53980=EDGE_CURVE('',#41107,#41108,#22144,.T.);
#53981=EDGE_CURVE('',#41109,#41107,#22145,.T.);
#53982=EDGE_CURVE('',#41110,#41109,#22146,.T.);
#53983=EDGE_CURVE('',#41110,#41108,#22147,.T.);
#53984=EDGE_CURVE('',#41111,#41112,#22148,.T.);
#53985=EDGE_CURVE('',#41113,#41111,#22149,.T.);
#53986=EDGE_CURVE('',#41114,#41113,#22150,.T.);
#53987=EDGE_CURVE('',#41114,#41112,#22151,.T.);
#53988=EDGE_CURVE('',#41115,#41116,#22152,.T.);
#53989=EDGE_CURVE('',#41117,#41115,#22153,.T.);
#53990=EDGE_CURVE('',#41118,#41117,#22154,.T.);
#53991=EDGE_CURVE('',#41118,#41116,#22155,.T.);
#53992=EDGE_CURVE('',#41119,#41120,#22156,.T.);
#53993=EDGE_CURVE('',#41121,#41119,#22157,.T.);
#53994=EDGE_CURVE('',#41122,#41121,#22158,.T.);
#53995=EDGE_CURVE('',#41122,#41120,#22159,.T.);
#53996=EDGE_CURVE('',#41123,#41124,#22160,.T.);
#53997=EDGE_CURVE('',#41125,#41123,#22161,.T.);
#53998=EDGE_CURVE('',#41126,#41125,#22162,.T.);
#53999=EDGE_CURVE('',#41126,#41124,#22163,.T.);
#54000=EDGE_CURVE('',#41127,#41128,#22164,.T.);
#54001=EDGE_CURVE('',#41129,#41127,#22165,.T.);
#54002=EDGE_CURVE('',#41130,#41129,#22166,.T.);
#54003=EDGE_CURVE('',#41130,#41128,#22167,.T.);
#54004=EDGE_CURVE('',#41131,#41132,#22168,.T.);
#54005=EDGE_CURVE('',#41133,#41131,#22169,.T.);
#54006=EDGE_CURVE('',#41134,#41133,#22170,.T.);
#54007=EDGE_CURVE('',#41134,#41132,#22171,.T.);
#54008=EDGE_CURVE('',#41135,#41136,#22172,.T.);
#54009=EDGE_CURVE('',#41137,#41135,#22173,.T.);
#54010=EDGE_CURVE('',#41138,#41137,#22174,.T.);
#54011=EDGE_CURVE('',#41138,#41136,#22175,.T.);
#54012=EDGE_CURVE('',#41139,#41140,#22176,.T.);
#54013=EDGE_CURVE('',#41141,#41139,#22177,.T.);
#54014=EDGE_CURVE('',#41142,#41141,#22178,.T.);
#54015=EDGE_CURVE('',#41142,#41140,#22179,.T.);
#54016=EDGE_CURVE('',#41143,#41144,#22180,.T.);
#54017=EDGE_CURVE('',#41145,#41143,#22181,.T.);
#54018=EDGE_CURVE('',#41146,#41145,#22182,.T.);
#54019=EDGE_CURVE('',#41146,#41144,#22183,.T.);
#54020=EDGE_CURVE('',#41147,#41148,#22184,.T.);
#54021=EDGE_CURVE('',#41149,#41147,#22185,.T.);
#54022=EDGE_CURVE('',#41150,#41149,#22186,.T.);
#54023=EDGE_CURVE('',#41150,#41148,#22187,.T.);
#54024=EDGE_CURVE('',#41151,#41152,#22188,.T.);
#54025=EDGE_CURVE('',#41153,#41151,#22189,.T.);
#54026=EDGE_CURVE('',#41154,#41153,#22190,.T.);
#54027=EDGE_CURVE('',#41154,#41152,#22191,.T.);
#54028=EDGE_CURVE('',#41155,#41156,#22192,.T.);
#54029=EDGE_CURVE('',#41157,#41155,#22193,.T.);
#54030=EDGE_CURVE('',#41158,#41157,#22194,.T.);
#54031=EDGE_CURVE('',#41158,#41156,#22195,.T.);
#54032=EDGE_CURVE('',#41159,#41160,#22196,.T.);
#54033=EDGE_CURVE('',#41161,#41159,#22197,.T.);
#54034=EDGE_CURVE('',#41162,#41161,#22198,.T.);
#54035=EDGE_CURVE('',#41162,#41160,#22199,.T.);
#54036=EDGE_CURVE('',#41163,#41164,#22200,.T.);
#54037=EDGE_CURVE('',#41165,#41163,#22201,.T.);
#54038=EDGE_CURVE('',#41166,#41165,#22202,.T.);
#54039=EDGE_CURVE('',#41166,#41164,#22203,.T.);
#54040=EDGE_CURVE('',#41167,#41168,#22204,.T.);
#54041=EDGE_CURVE('',#41169,#41167,#22205,.T.);
#54042=EDGE_CURVE('',#41170,#41169,#22206,.T.);
#54043=EDGE_CURVE('',#41170,#41168,#22207,.T.);
#54044=EDGE_CURVE('',#41171,#41172,#22208,.T.);
#54045=EDGE_CURVE('',#41173,#41171,#22209,.T.);
#54046=EDGE_CURVE('',#41174,#41173,#22210,.T.);
#54047=EDGE_CURVE('',#41174,#41172,#22211,.T.);
#54048=EDGE_CURVE('',#41175,#41176,#22212,.T.);
#54049=EDGE_CURVE('',#41177,#41175,#22213,.T.);
#54050=EDGE_CURVE('',#41178,#41177,#22214,.T.);
#54051=EDGE_CURVE('',#41178,#41176,#22215,.T.);
#54052=EDGE_CURVE('',#41179,#41180,#22216,.T.);
#54053=EDGE_CURVE('',#41181,#41179,#22217,.T.);
#54054=EDGE_CURVE('',#41182,#41181,#22218,.T.);
#54055=EDGE_CURVE('',#41182,#41180,#22219,.T.);
#54056=EDGE_CURVE('',#41183,#41184,#22220,.T.);
#54057=EDGE_CURVE('',#41185,#41183,#22221,.T.);
#54058=EDGE_CURVE('',#41186,#41185,#22222,.T.);
#54059=EDGE_CURVE('',#41186,#41184,#22223,.T.);
#54060=EDGE_CURVE('',#41187,#41188,#22224,.T.);
#54061=EDGE_CURVE('',#41189,#41187,#22225,.T.);
#54062=EDGE_CURVE('',#41190,#41189,#22226,.T.);
#54063=EDGE_CURVE('',#41190,#41188,#22227,.T.);
#54064=EDGE_CURVE('',#41191,#41192,#22228,.T.);
#54065=EDGE_CURVE('',#41193,#41191,#22229,.T.);
#54066=EDGE_CURVE('',#41194,#41193,#22230,.T.);
#54067=EDGE_CURVE('',#41194,#41192,#22231,.T.);
#54068=EDGE_CURVE('',#41195,#41196,#22232,.T.);
#54069=EDGE_CURVE('',#41197,#41195,#22233,.T.);
#54070=EDGE_CURVE('',#41198,#41197,#22234,.T.);
#54071=EDGE_CURVE('',#41198,#41196,#22235,.T.);
#54072=EDGE_CURVE('',#41199,#41200,#22236,.T.);
#54073=EDGE_CURVE('',#41201,#41199,#22237,.T.);
#54074=EDGE_CURVE('',#41202,#41201,#22238,.T.);
#54075=EDGE_CURVE('',#41202,#41200,#22239,.T.);
#54076=EDGE_CURVE('',#41203,#41204,#22240,.T.);
#54077=EDGE_CURVE('',#41205,#41203,#22241,.T.);
#54078=EDGE_CURVE('',#41206,#41205,#22242,.T.);
#54079=EDGE_CURVE('',#41206,#41204,#22243,.T.);
#54080=EDGE_CURVE('',#41207,#41208,#22244,.T.);
#54081=EDGE_CURVE('',#41209,#41207,#22245,.T.);
#54082=EDGE_CURVE('',#41210,#41209,#22246,.T.);
#54083=EDGE_CURVE('',#41210,#41208,#22247,.T.);
#54084=EDGE_CURVE('',#41211,#41212,#22248,.T.);
#54085=EDGE_CURVE('',#41213,#41211,#22249,.T.);
#54086=EDGE_CURVE('',#41214,#41213,#22250,.T.);
#54087=EDGE_CURVE('',#41214,#41212,#22251,.T.);
#54088=EDGE_CURVE('',#41215,#41216,#22252,.T.);
#54089=EDGE_CURVE('',#41217,#41215,#22253,.T.);
#54090=EDGE_CURVE('',#41218,#41217,#22254,.T.);
#54091=EDGE_CURVE('',#41218,#41216,#22255,.T.);
#54092=EDGE_CURVE('',#41219,#41220,#22256,.T.);
#54093=EDGE_CURVE('',#41221,#41219,#22257,.T.);
#54094=EDGE_CURVE('',#41222,#41221,#22258,.T.);
#54095=EDGE_CURVE('',#41222,#41220,#22259,.T.);
#54096=EDGE_CURVE('',#41223,#41224,#22260,.T.);
#54097=EDGE_CURVE('',#41225,#41223,#22261,.T.);
#54098=EDGE_CURVE('',#41226,#41225,#22262,.T.);
#54099=EDGE_CURVE('',#41226,#41224,#22263,.T.);
#54100=EDGE_CURVE('',#41227,#41228,#22264,.T.);
#54101=EDGE_CURVE('',#41229,#41227,#22265,.T.);
#54102=EDGE_CURVE('',#41230,#41229,#22266,.T.);
#54103=EDGE_CURVE('',#41230,#41228,#22267,.T.);
#54104=EDGE_CURVE('',#41231,#41232,#22268,.T.);
#54105=EDGE_CURVE('',#41233,#41231,#22269,.T.);
#54106=EDGE_CURVE('',#41234,#41233,#22270,.T.);
#54107=EDGE_CURVE('',#41234,#41232,#22271,.T.);
#54108=EDGE_CURVE('',#41235,#41236,#22272,.T.);
#54109=EDGE_CURVE('',#41237,#41235,#22273,.T.);
#54110=EDGE_CURVE('',#41238,#41237,#22274,.T.);
#54111=EDGE_CURVE('',#41238,#41236,#22275,.T.);
#54112=EDGE_CURVE('',#41239,#41240,#22276,.T.);
#54113=EDGE_CURVE('',#41241,#41239,#22277,.T.);
#54114=EDGE_CURVE('',#41242,#41241,#22278,.T.);
#54115=EDGE_CURVE('',#41242,#41240,#22279,.T.);
#54116=EDGE_CURVE('',#41243,#41244,#22280,.T.);
#54117=EDGE_CURVE('',#41245,#41243,#22281,.T.);
#54118=EDGE_CURVE('',#41246,#41245,#22282,.T.);
#54119=EDGE_CURVE('',#41246,#41244,#22283,.T.);
#54120=EDGE_CURVE('',#41247,#41248,#22284,.T.);
#54121=EDGE_CURVE('',#41249,#41247,#22285,.T.);
#54122=EDGE_CURVE('',#41250,#41249,#22286,.T.);
#54123=EDGE_CURVE('',#41250,#41248,#22287,.T.);
#54124=EDGE_CURVE('',#41251,#41252,#22288,.T.);
#54125=EDGE_CURVE('',#41253,#41251,#22289,.T.);
#54126=EDGE_CURVE('',#41254,#41253,#22290,.T.);
#54127=EDGE_CURVE('',#41254,#41252,#22291,.T.);
#54128=EDGE_CURVE('',#41255,#41256,#22292,.T.);
#54129=EDGE_CURVE('',#41257,#41255,#22293,.T.);
#54130=EDGE_CURVE('',#41258,#41257,#22294,.T.);
#54131=EDGE_CURVE('',#41258,#41256,#22295,.T.);
#54132=EDGE_CURVE('',#41259,#41260,#22296,.T.);
#54133=EDGE_CURVE('',#41261,#41259,#22297,.T.);
#54134=EDGE_CURVE('',#41262,#41261,#22298,.T.);
#54135=EDGE_CURVE('',#41262,#41260,#22299,.T.);
#54136=EDGE_CURVE('',#41263,#41264,#22300,.T.);
#54137=EDGE_CURVE('',#41265,#41263,#22301,.T.);
#54138=EDGE_CURVE('',#41266,#41265,#22302,.T.);
#54139=EDGE_CURVE('',#41266,#41264,#22303,.T.);
#54140=EDGE_CURVE('',#41267,#41268,#22304,.T.);
#54141=EDGE_CURVE('',#41269,#41267,#22305,.T.);
#54142=EDGE_CURVE('',#41270,#41269,#22306,.T.);
#54143=EDGE_CURVE('',#41270,#41268,#22307,.T.);
#54144=EDGE_CURVE('',#41271,#41272,#22308,.T.);
#54145=EDGE_CURVE('',#41273,#41271,#22309,.T.);
#54146=EDGE_CURVE('',#41274,#41273,#22310,.T.);
#54147=EDGE_CURVE('',#41274,#41272,#22311,.T.);
#54148=EDGE_CURVE('',#41275,#41276,#22312,.T.);
#54149=EDGE_CURVE('',#41277,#41275,#22313,.T.);
#54150=EDGE_CURVE('',#41278,#41277,#22314,.T.);
#54151=EDGE_CURVE('',#41278,#41276,#22315,.T.);
#54152=EDGE_CURVE('',#41279,#41280,#22316,.T.);
#54153=EDGE_CURVE('',#41281,#41279,#22317,.T.);
#54154=EDGE_CURVE('',#41282,#41281,#22318,.T.);
#54155=EDGE_CURVE('',#41282,#41280,#22319,.T.);
#54156=EDGE_CURVE('',#41283,#41284,#22320,.T.);
#54157=EDGE_CURVE('',#41285,#41283,#22321,.T.);
#54158=EDGE_CURVE('',#41286,#41285,#22322,.T.);
#54159=EDGE_CURVE('',#41286,#41284,#22323,.T.);
#54160=EDGE_CURVE('',#41287,#41288,#22324,.T.);
#54161=EDGE_CURVE('',#41289,#41287,#22325,.T.);
#54162=EDGE_CURVE('',#41290,#41289,#22326,.T.);
#54163=EDGE_CURVE('',#41290,#41288,#22327,.T.);
#54164=EDGE_CURVE('',#41291,#41292,#22328,.T.);
#54165=EDGE_CURVE('',#41293,#41291,#22329,.T.);
#54166=EDGE_CURVE('',#41294,#41293,#22330,.T.);
#54167=EDGE_CURVE('',#41294,#41292,#22331,.T.);
#54168=EDGE_CURVE('',#41295,#41296,#22332,.T.);
#54169=EDGE_CURVE('',#41297,#41295,#22333,.T.);
#54170=EDGE_CURVE('',#41298,#41297,#22334,.T.);
#54171=EDGE_CURVE('',#41298,#41296,#22335,.T.);
#54172=EDGE_CURVE('',#41299,#41300,#22336,.T.);
#54173=EDGE_CURVE('',#41301,#41299,#22337,.T.);
#54174=EDGE_CURVE('',#41302,#41301,#22338,.T.);
#54175=EDGE_CURVE('',#41302,#41300,#22339,.T.);
#54176=EDGE_CURVE('',#41303,#41304,#22340,.T.);
#54177=EDGE_CURVE('',#41305,#41303,#22341,.T.);
#54178=EDGE_CURVE('',#41306,#41305,#22342,.T.);
#54179=EDGE_CURVE('',#41306,#41304,#22343,.T.);
#54180=EDGE_CURVE('',#41307,#41308,#22344,.T.);
#54181=EDGE_CURVE('',#41309,#41307,#22345,.T.);
#54182=EDGE_CURVE('',#41310,#41309,#22346,.T.);
#54183=EDGE_CURVE('',#41310,#41308,#22347,.T.);
#54184=EDGE_CURVE('',#41311,#41312,#22348,.T.);
#54185=EDGE_CURVE('',#41313,#41311,#22349,.T.);
#54186=EDGE_CURVE('',#41314,#41313,#22350,.T.);
#54187=EDGE_CURVE('',#41314,#41312,#22351,.T.);
#54188=EDGE_CURVE('',#41315,#41316,#22352,.T.);
#54189=EDGE_CURVE('',#41317,#41315,#22353,.T.);
#54190=EDGE_CURVE('',#41318,#41317,#22354,.T.);
#54191=EDGE_CURVE('',#41318,#41316,#22355,.T.);
#54192=EDGE_CURVE('',#41319,#41320,#22356,.T.);
#54193=EDGE_CURVE('',#41321,#41319,#22357,.T.);
#54194=EDGE_CURVE('',#41322,#41321,#22358,.T.);
#54195=EDGE_CURVE('',#41322,#41320,#22359,.T.);
#54196=EDGE_CURVE('',#41323,#41324,#22360,.T.);
#54197=EDGE_CURVE('',#41325,#41323,#22361,.T.);
#54198=EDGE_CURVE('',#41326,#41325,#22362,.T.);
#54199=EDGE_CURVE('',#41326,#41324,#22363,.T.);
#54200=EDGE_CURVE('',#41327,#41328,#22364,.T.);
#54201=EDGE_CURVE('',#41329,#41327,#22365,.T.);
#54202=EDGE_CURVE('',#41330,#41329,#22366,.T.);
#54203=EDGE_CURVE('',#41330,#41328,#22367,.T.);
#54204=EDGE_CURVE('',#41331,#41332,#22368,.T.);
#54205=EDGE_CURVE('',#41333,#41331,#22369,.T.);
#54206=EDGE_CURVE('',#41334,#41333,#22370,.T.);
#54207=EDGE_CURVE('',#41334,#41332,#22371,.T.);
#54208=EDGE_CURVE('',#41335,#41336,#22372,.T.);
#54209=EDGE_CURVE('',#41337,#41335,#22373,.T.);
#54210=EDGE_CURVE('',#41338,#41337,#22374,.T.);
#54211=EDGE_CURVE('',#41338,#41336,#22375,.T.);
#54212=EDGE_CURVE('',#41339,#41340,#22376,.T.);
#54213=EDGE_CURVE('',#41341,#41339,#22377,.T.);
#54214=EDGE_CURVE('',#41342,#41341,#22378,.T.);
#54215=EDGE_CURVE('',#41342,#41340,#22379,.T.);
#54216=EDGE_CURVE('',#41343,#41344,#22380,.T.);
#54217=EDGE_CURVE('',#41345,#41343,#22381,.T.);
#54218=EDGE_CURVE('',#41346,#41345,#22382,.T.);
#54219=EDGE_CURVE('',#41346,#41344,#22383,.T.);
#54220=EDGE_CURVE('',#41347,#41348,#22384,.T.);
#54221=EDGE_CURVE('',#41349,#41347,#22385,.T.);
#54222=EDGE_CURVE('',#41350,#41349,#22386,.T.);
#54223=EDGE_CURVE('',#41350,#41348,#22387,.T.);
#54224=EDGE_CURVE('',#41351,#41352,#22388,.T.);
#54225=EDGE_CURVE('',#41353,#41351,#22389,.T.);
#54226=EDGE_CURVE('',#41354,#41353,#22390,.T.);
#54227=EDGE_CURVE('',#41354,#41352,#22391,.T.);
#54228=EDGE_CURVE('',#41355,#41356,#22392,.T.);
#54229=EDGE_CURVE('',#41357,#41355,#22393,.T.);
#54230=EDGE_CURVE('',#41358,#41357,#22394,.T.);
#54231=EDGE_CURVE('',#41358,#41356,#22395,.T.);
#54232=EDGE_CURVE('',#41359,#41360,#22396,.T.);
#54233=EDGE_CURVE('',#41361,#41359,#22397,.T.);
#54234=EDGE_CURVE('',#41362,#41361,#22398,.T.);
#54235=EDGE_CURVE('',#41362,#41360,#22399,.T.);
#54236=EDGE_CURVE('',#41363,#41364,#22400,.T.);
#54237=EDGE_CURVE('',#41365,#41363,#22401,.T.);
#54238=EDGE_CURVE('',#41366,#41365,#22402,.T.);
#54239=EDGE_CURVE('',#41366,#41364,#22403,.T.);
#54240=EDGE_CURVE('',#41367,#41368,#22404,.T.);
#54241=EDGE_CURVE('',#41369,#41367,#22405,.T.);
#54242=EDGE_CURVE('',#41370,#41369,#22406,.T.);
#54243=EDGE_CURVE('',#41370,#41368,#22407,.T.);
#54244=EDGE_CURVE('',#41371,#41372,#22408,.T.);
#54245=EDGE_CURVE('',#41373,#41371,#22409,.T.);
#54246=EDGE_CURVE('',#41374,#41373,#22410,.T.);
#54247=EDGE_CURVE('',#41374,#41372,#22411,.T.);
#54248=EDGE_CURVE('',#41375,#41376,#22412,.T.);
#54249=EDGE_CURVE('',#41377,#41375,#22413,.T.);
#54250=EDGE_CURVE('',#41378,#41377,#22414,.T.);
#54251=EDGE_CURVE('',#41378,#41376,#22415,.T.);
#54252=EDGE_CURVE('',#41379,#41380,#22416,.T.);
#54253=EDGE_CURVE('',#41381,#41379,#22417,.T.);
#54254=EDGE_CURVE('',#41382,#41381,#22418,.T.);
#54255=EDGE_CURVE('',#41382,#41380,#22419,.T.);
#54256=EDGE_CURVE('',#41383,#41384,#22420,.T.);
#54257=EDGE_CURVE('',#41385,#41383,#22421,.T.);
#54258=EDGE_CURVE('',#41386,#41385,#22422,.T.);
#54259=EDGE_CURVE('',#41387,#41386,#22423,.T.);
#54260=EDGE_CURVE('',#41387,#41384,#22424,.T.);
#54261=EDGE_CURVE('',#41073,#41077,#25927,.F.);
#54262=EDGE_CURVE('',#41078,#41074,#25928,.F.);
#54263=EDGE_CURVE('',#41003,#40927,#22425,.T.);
#54264=EDGE_CURVE('',#41007,#40927,#25929,.F.);
#54265=EDGE_CURVE('',#41002,#41006,#25930,.F.);
#54266=EDGE_CURVE('',#41388,#41388,#22426,.T.);
#54267=EDGE_CURVE('',#41388,#41075,#29822,.T.);
#54268=EDGE_CURVE('',#40999,#41076,#25931,.T.);
#54269=EDGE_CURVE('',#41389,#41390,#29823,.T.);
#54270=EDGE_CURVE('',#41391,#41390,#22427,.T.);
#54271=EDGE_CURVE('',#41392,#41391,#22428,.T.);
#54272=EDGE_CURVE('',#41393,#41392,#22429,.T.);
#54273=EDGE_CURVE('',#41393,#41394,#22430,.T.);
#54274=EDGE_CURVE('',#41395,#41394,#22431,.T.);
#54275=EDGE_CURVE('',#41390,#41395,#22432,.T.);
#54276=EDGE_CURVE('',#41396,#41397,#4397,.T.);
#54277=EDGE_CURVE('',#41397,#41396,#22433,.T.);
#54278=EDGE_CURVE('',#41398,#41398,#22434,.T.);
#54279=EDGE_CURVE('',#41398,#41399,#22435,.T.);
#54280=EDGE_CURVE('',#41399,#41399,#22436,.T.);
#54281=EDGE_CURVE('',#41400,#41400,#22437,.T.);
#54282=EDGE_CURVE('',#41400,#41398,#29824,.T.);
#54283=EDGE_CURVE('',#41401,#41401,#22438,.T.);
#54284=EDGE_CURVE('',#41401,#41400,#22439,.T.);
#54285=EDGE_CURVE('',#41402,#41403,#25932,.T.);
#54286=EDGE_CURVE('',#41403,#41404,#29825,.T.);
#54287=EDGE_CURVE('',#41404,#41405,#22440,.T.);
#54288=EDGE_CURVE('',#41405,#41406,#29826,.T.);
#54289=EDGE_CURVE('',#41406,#41407,#25933,.T.);
#54290=EDGE_CURVE('',#41407,#41408,#29827,.T.);
#54291=EDGE_CURVE('',#41408,#41409,#22441,.T.);
#54292=EDGE_CURVE('',#41409,#41410,#29828,.T.);
#54293=EDGE_CURVE('',#41410,#41411,#25934,.T.);
#54294=EDGE_CURVE('',#41411,#41412,#29829,.T.);
#54295=EDGE_CURVE('',#41412,#41413,#22442,.T.);
#54296=EDGE_CURVE('',#41413,#41414,#29830,.T.);
#54297=EDGE_CURVE('',#41414,#41415,#25935,.T.);
#54298=EDGE_CURVE('',#41415,#41416,#29831,.T.);
#54299=EDGE_CURVE('',#41416,#41417,#22443,.T.);
#54300=EDGE_CURVE('',#41417,#41418,#29832,.T.);
#54301=EDGE_CURVE('',#41418,#41419,#25936,.T.);
#54302=EDGE_CURVE('',#41419,#41420,#29833,.T.);
#54303=EDGE_CURVE('',#41420,#41421,#22444,.T.);
#54304=EDGE_CURVE('',#41421,#41422,#29834,.T.);
#54305=EDGE_CURVE('',#41422,#41423,#25937,.T.);
#54306=EDGE_CURVE('',#41423,#41424,#29835,.T.);
#54307=EDGE_CURVE('',#41424,#41425,#22445,.T.);
#54308=EDGE_CURVE('',#41425,#41426,#29836,.T.);
#54309=EDGE_CURVE('',#41426,#41427,#25938,.T.);
#54310=EDGE_CURVE('',#41427,#41428,#29837,.T.);
#54311=EDGE_CURVE('',#41428,#41429,#22446,.T.);
#54312=EDGE_CURVE('',#41429,#41430,#29838,.T.);
#54313=EDGE_CURVE('',#41430,#41431,#25939,.T.);
#54314=EDGE_CURVE('',#41431,#41432,#29839,.T.);
#54315=EDGE_CURVE('',#41432,#41433,#22447,.T.);
#54316=EDGE_CURVE('',#41433,#41434,#29840,.T.);
#54317=EDGE_CURVE('',#41434,#41435,#25940,.T.);
#54318=EDGE_CURVE('',#41435,#41436,#29841,.T.);
#54319=EDGE_CURVE('',#41436,#41437,#22448,.T.);
#54320=EDGE_CURVE('',#41437,#41438,#29842,.T.);
#54321=EDGE_CURVE('',#41438,#41439,#25941,.T.);
#54322=EDGE_CURVE('',#41439,#41440,#29843,.T.);
#54323=EDGE_CURVE('',#41440,#41441,#22449,.T.);
#54324=EDGE_CURVE('',#41441,#41442,#29844,.T.);
#54325=EDGE_CURVE('',#41442,#41443,#25942,.T.);
#54326=EDGE_CURVE('',#41443,#41444,#29845,.T.);
#54327=EDGE_CURVE('',#41444,#41445,#22450,.T.);
#54328=EDGE_CURVE('',#41445,#41446,#29846,.T.);
#54329=EDGE_CURVE('',#41446,#41447,#25943,.T.);
#54330=EDGE_CURVE('',#41447,#41448,#29847,.T.);
#54331=EDGE_CURVE('',#41448,#41449,#22451,.T.);
#54332=EDGE_CURVE('',#41449,#41450,#29848,.T.);
#54333=EDGE_CURVE('',#41450,#41451,#25944,.T.);
#54334=EDGE_CURVE('',#41451,#41452,#29849,.T.);
#54335=EDGE_CURVE('',#41452,#41453,#22452,.T.);
#54336=EDGE_CURVE('',#41453,#41454,#29850,.T.);
#54337=EDGE_CURVE('',#41454,#41455,#25945,.T.);
#54338=EDGE_CURVE('',#41455,#41456,#29851,.T.);
#54339=EDGE_CURVE('',#41456,#41457,#22453,.T.);
#54340=EDGE_CURVE('',#41457,#41458,#29852,.T.);
#54341=EDGE_CURVE('',#41458,#41459,#25946,.T.);
#54342=EDGE_CURVE('',#41459,#41460,#29853,.T.);
#54343=EDGE_CURVE('',#41460,#41461,#22454,.T.);
#54344=EDGE_CURVE('',#41461,#41462,#29854,.T.);
#54345=EDGE_CURVE('',#41462,#41463,#25947,.T.);
#54346=EDGE_CURVE('',#41463,#41464,#29855,.T.);
#54347=EDGE_CURVE('',#41464,#41465,#22455,.T.);
#54348=EDGE_CURVE('',#41465,#41466,#29856,.T.);
#54349=EDGE_CURVE('',#41466,#41467,#25948,.T.);
#54350=EDGE_CURVE('',#41467,#41468,#29857,.T.);
#54351=EDGE_CURVE('',#41468,#41469,#22456,.T.);
#54352=EDGE_CURVE('',#41469,#41470,#29858,.T.);
#54353=EDGE_CURVE('',#41470,#41471,#25949,.T.);
#54354=EDGE_CURVE('',#41471,#41472,#29859,.T.);
#54355=EDGE_CURVE('',#41472,#41473,#22457,.T.);
#54356=EDGE_CURVE('',#41473,#41474,#29860,.T.);
#54357=EDGE_CURVE('',#41474,#41475,#25950,.T.);
#54358=EDGE_CURVE('',#41475,#41476,#29861,.T.);
#54359=EDGE_CURVE('',#41476,#41477,#22458,.T.);
#54360=EDGE_CURVE('',#41477,#41478,#29862,.T.);
#54361=EDGE_CURVE('',#41478,#41479,#25951,.T.);
#54362=EDGE_CURVE('',#41479,#41480,#29863,.T.);
#54363=EDGE_CURVE('',#41480,#41481,#22459,.T.);
#54364=EDGE_CURVE('',#41481,#41482,#29864,.T.);
#54365=EDGE_CURVE('',#41482,#41483,#25952,.T.);
#54366=EDGE_CURVE('',#41483,#41484,#29865,.T.);
#54367=EDGE_CURVE('',#41484,#41485,#22460,.T.);
#54368=EDGE_CURVE('',#41485,#41486,#29866,.T.);
#54369=EDGE_CURVE('',#41486,#41487,#25953,.T.);
#54370=EDGE_CURVE('',#41487,#41488,#29867,.T.);
#54371=EDGE_CURVE('',#41488,#41489,#22461,.T.);
#54372=EDGE_CURVE('',#41489,#41490,#29868,.T.);
#54373=EDGE_CURVE('',#41490,#41491,#25954,.T.);
#54374=EDGE_CURVE('',#41491,#41492,#29869,.T.);
#54375=EDGE_CURVE('',#41492,#41493,#22462,.T.);
#54376=EDGE_CURVE('',#41493,#41494,#29870,.T.);
#54377=EDGE_CURVE('',#41494,#41495,#25955,.T.);
#54378=EDGE_CURVE('',#41495,#41496,#29871,.T.);
#54379=EDGE_CURVE('',#41496,#41497,#22463,.T.);
#54380=EDGE_CURVE('',#41497,#41498,#29872,.T.);
#54381=EDGE_CURVE('',#41498,#41499,#25956,.T.);
#54382=EDGE_CURVE('',#41499,#41500,#29873,.T.);
#54383=EDGE_CURVE('',#41500,#41501,#22464,.T.);
#54384=EDGE_CURVE('',#41501,#41502,#29874,.T.);
#54385=EDGE_CURVE('',#41502,#41503,#25957,.T.);
#54386=EDGE_CURVE('',#41503,#41504,#29875,.T.);
#54387=EDGE_CURVE('',#41504,#41505,#22465,.T.);
#54388=EDGE_CURVE('',#41505,#41506,#29876,.T.);
#54389=EDGE_CURVE('',#41506,#41507,#25958,.T.);
#54390=EDGE_CURVE('',#41507,#41508,#29877,.T.);
#54391=EDGE_CURVE('',#41508,#41509,#22466,.T.);
#54392=EDGE_CURVE('',#41509,#41510,#29878,.T.);
#54393=EDGE_CURVE('',#41510,#41511,#25959,.T.);
#54394=EDGE_CURVE('',#41511,#41512,#29879,.T.);
#54395=EDGE_CURVE('',#41512,#41513,#22467,.T.);
#54396=EDGE_CURVE('',#41513,#41514,#29880,.T.);
#54397=EDGE_CURVE('',#41514,#41515,#25960,.T.);
#54398=EDGE_CURVE('',#41515,#41516,#29881,.T.);
#54399=EDGE_CURVE('',#41516,#41517,#22468,.T.);
#54400=EDGE_CURVE('',#41517,#41518,#29882,.T.);
#54401=EDGE_CURVE('',#41518,#41519,#25961,.T.);
#54402=EDGE_CURVE('',#41519,#41520,#29883,.T.);
#54403=EDGE_CURVE('',#41520,#41521,#22469,.T.);
#54404=EDGE_CURVE('',#41521,#41522,#29884,.T.);
#54405=EDGE_CURVE('',#41522,#41523,#25962,.T.);
#54406=EDGE_CURVE('',#41523,#41524,#29885,.T.);
#54407=EDGE_CURVE('',#41524,#41525,#22470,.T.);
#54408=EDGE_CURVE('',#41525,#41526,#29886,.T.);
#54409=EDGE_CURVE('',#41526,#41527,#25963,.T.);
#54410=EDGE_CURVE('',#41527,#41528,#29887,.T.);
#54411=EDGE_CURVE('',#41528,#41529,#22471,.T.);
#54412=EDGE_CURVE('',#41529,#41530,#29888,.T.);
#54413=EDGE_CURVE('',#41530,#41531,#25964,.T.);
#54414=EDGE_CURVE('',#41531,#41532,#29889,.T.);
#54415=EDGE_CURVE('',#41532,#41533,#22472,.T.);
#54416=EDGE_CURVE('',#41533,#41534,#29890,.T.);
#54417=EDGE_CURVE('',#41534,#41535,#25965,.T.);
#54418=EDGE_CURVE('',#41535,#41536,#29891,.T.);
#54419=EDGE_CURVE('',#41536,#41537,#22473,.T.);
#54420=EDGE_CURVE('',#41537,#41538,#29892,.T.);
#54421=EDGE_CURVE('',#41538,#41539,#25966,.T.);
#54422=EDGE_CURVE('',#41539,#41540,#29893,.T.);
#54423=EDGE_CURVE('',#41540,#41541,#22474,.T.);
#54424=EDGE_CURVE('',#41541,#41542,#29894,.T.);
#54425=EDGE_CURVE('',#41542,#41543,#25967,.T.);
#54426=EDGE_CURVE('',#41543,#41544,#29895,.T.);
#54427=EDGE_CURVE('',#41544,#41545,#22475,.T.);
#54428=EDGE_CURVE('',#41545,#41546,#29896,.T.);
#54429=EDGE_CURVE('',#41546,#41547,#25968,.T.);
#54430=EDGE_CURVE('',#41547,#41548,#29897,.T.);
#54431=EDGE_CURVE('',#41548,#41549,#22476,.T.);
#54432=EDGE_CURVE('',#41549,#41550,#29898,.T.);
#54433=EDGE_CURVE('',#41550,#41551,#25969,.T.);
#54434=EDGE_CURVE('',#41551,#41552,#29899,.T.);
#54435=EDGE_CURVE('',#41552,#41553,#22477,.T.);
#54436=EDGE_CURVE('',#41553,#41554,#29900,.T.);
#54437=EDGE_CURVE('',#41554,#41555,#25970,.T.);
#54438=EDGE_CURVE('',#41555,#41556,#29901,.T.);
#54439=EDGE_CURVE('',#41556,#41557,#22478,.T.);
#54440=EDGE_CURVE('',#41557,#41558,#29902,.T.);
#54441=EDGE_CURVE('',#41559,#41558,#22479,.T.);
#54442=EDGE_CURVE('',#41558,#41559,#22480,.T.);
#54443=EDGE_CURVE('',#41557,#41560,#22481,.T.);
#54444=EDGE_CURVE('',#41560,#41561,#29903,.T.);
#54445=EDGE_CURVE('',#41561,#41562,#25971,.T.);
#54446=EDGE_CURVE('',#41562,#41563,#29904,.T.);
#54447=EDGE_CURVE('',#41563,#41564,#22482,.T.);
#54448=EDGE_CURVE('',#41564,#41565,#29905,.T.);
#54449=EDGE_CURVE('',#41565,#41566,#25972,.T.);
#54450=EDGE_CURVE('',#41566,#41567,#29906,.T.);
#54451=EDGE_CURVE('',#41567,#41568,#22483,.T.);
#54452=EDGE_CURVE('',#41568,#41569,#29907,.T.);
#54453=EDGE_CURVE('',#41569,#41570,#25973,.T.);
#54454=EDGE_CURVE('',#41570,#41571,#29908,.T.);
#54455=EDGE_CURVE('',#41571,#41572,#22484,.T.);
#54456=EDGE_CURVE('',#41572,#41573,#29909,.T.);
#54457=EDGE_CURVE('',#41573,#41574,#25974,.T.);
#54458=EDGE_CURVE('',#41574,#41575,#29910,.T.);
#54459=EDGE_CURVE('',#41575,#41576,#22485,.T.);
#54460=EDGE_CURVE('',#41576,#41577,#29911,.T.);
#54461=EDGE_CURVE('',#41577,#41578,#25975,.T.);
#54462=EDGE_CURVE('',#41578,#41579,#29912,.T.);
#54463=EDGE_CURVE('',#41579,#41580,#22486,.T.);
#54464=EDGE_CURVE('',#41580,#41581,#29913,.T.);
#54465=EDGE_CURVE('',#41581,#41582,#25976,.T.);
#54466=EDGE_CURVE('',#41582,#41583,#29914,.T.);
#54467=EDGE_CURVE('',#41583,#41584,#22487,.T.);
#54468=EDGE_CURVE('',#41584,#41585,#29915,.T.);
#54469=EDGE_CURVE('',#41585,#41586,#25977,.T.);
#54470=EDGE_CURVE('',#41586,#41587,#29916,.T.);
#54471=EDGE_CURVE('',#41587,#41588,#22488,.T.);
#54472=EDGE_CURVE('',#41588,#41589,#29917,.T.);
#54473=EDGE_CURVE('',#41589,#41590,#25978,.T.);
#54474=EDGE_CURVE('',#41590,#41591,#29918,.T.);
#54475=EDGE_CURVE('',#41591,#41592,#22489,.T.);
#54476=EDGE_CURVE('',#41592,#41593,#29919,.T.);
#54477=EDGE_CURVE('',#41593,#41594,#25979,.T.);
#54478=EDGE_CURVE('',#41594,#41595,#29920,.T.);
#54479=EDGE_CURVE('',#41595,#41596,#22490,.T.);
#54480=EDGE_CURVE('',#41596,#41597,#29921,.T.);
#54481=EDGE_CURVE('',#41597,#41598,#25980,.T.);
#54482=EDGE_CURVE('',#41598,#41599,#29922,.T.);
#54483=EDGE_CURVE('',#41599,#41600,#22491,.T.);
#54484=EDGE_CURVE('',#41600,#41601,#29923,.T.);
#54485=EDGE_CURVE('',#41601,#41602,#25981,.T.);
#54486=EDGE_CURVE('',#41602,#41603,#29924,.T.);
#54487=EDGE_CURVE('',#41603,#41604,#22492,.T.);
#54488=EDGE_CURVE('',#41604,#41605,#29925,.T.);
#54489=EDGE_CURVE('',#41605,#41606,#25982,.T.);
#54490=EDGE_CURVE('',#41606,#41607,#29926,.T.);
#54491=EDGE_CURVE('',#41607,#41608,#22493,.T.);
#54492=EDGE_CURVE('',#41608,#41609,#29927,.T.);
#54493=EDGE_CURVE('',#41609,#41610,#25983,.T.);
#54494=EDGE_CURVE('',#41610,#41611,#29928,.T.);
#54495=EDGE_CURVE('',#41611,#41612,#22494,.T.);
#54496=EDGE_CURVE('',#41612,#41613,#29929,.T.);
#54497=EDGE_CURVE('',#41613,#41614,#25984,.T.);
#54498=EDGE_CURVE('',#41614,#41615,#29930,.T.);
#54499=EDGE_CURVE('',#41615,#41616,#22495,.T.);
#54500=EDGE_CURVE('',#41616,#41617,#29931,.T.);
#54501=EDGE_CURVE('',#41617,#41618,#25985,.T.);
#54502=EDGE_CURVE('',#41618,#41619,#29932,.T.);
#54503=EDGE_CURVE('',#41619,#41620,#22496,.T.);
#54504=EDGE_CURVE('',#41620,#41621,#29933,.T.);
#54505=EDGE_CURVE('',#41621,#41622,#25986,.T.);
#54506=EDGE_CURVE('',#41622,#41623,#29934,.T.);
#54507=EDGE_CURVE('',#41623,#41624,#22497,.T.);
#54508=EDGE_CURVE('',#41624,#41625,#29935,.T.);
#54509=EDGE_CURVE('',#41625,#41626,#25987,.T.);
#54510=EDGE_CURVE('',#41626,#41627,#29936,.T.);
#54511=EDGE_CURVE('',#41627,#41628,#22498,.T.);
#54512=EDGE_CURVE('',#41628,#41629,#29937,.T.);
#54513=EDGE_CURVE('',#41629,#41630,#25988,.T.);
#54514=EDGE_CURVE('',#41630,#41631,#29938,.T.);
#54515=EDGE_CURVE('',#41631,#41632,#22499,.T.);
#54516=EDGE_CURVE('',#41632,#41633,#29939,.T.);
#54517=EDGE_CURVE('',#41633,#41634,#25989,.T.);
#54518=EDGE_CURVE('',#41634,#41635,#29940,.T.);
#54519=EDGE_CURVE('',#41635,#41636,#22500,.T.);
#54520=EDGE_CURVE('',#41636,#41637,#29941,.T.);
#54521=EDGE_CURVE('',#41637,#41638,#25990,.T.);
#54522=EDGE_CURVE('',#41638,#41639,#29942,.T.);
#54523=EDGE_CURVE('',#41639,#41640,#22501,.T.);
#54524=EDGE_CURVE('',#41640,#41641,#29943,.T.);
#54525=EDGE_CURVE('',#41641,#41642,#25991,.T.);
#54526=EDGE_CURVE('',#41642,#41643,#29944,.T.);
#54527=EDGE_CURVE('',#41643,#41644,#22502,.T.);
#54528=EDGE_CURVE('',#41644,#41645,#29945,.T.);
#54529=EDGE_CURVE('',#41645,#41646,#25992,.T.);
#54530=EDGE_CURVE('',#41646,#41647,#29946,.T.);
#54531=EDGE_CURVE('',#41647,#41648,#22503,.T.);
#54532=EDGE_CURVE('',#41648,#41649,#29947,.T.);
#54533=EDGE_CURVE('',#41649,#41650,#25993,.T.);
#54534=EDGE_CURVE('',#41650,#41651,#29948,.T.);
#54535=EDGE_CURVE('',#41651,#41652,#22504,.T.);
#54536=EDGE_CURVE('',#41652,#41653,#29949,.T.);
#54537=EDGE_CURVE('',#41653,#41654,#25994,.T.);
#54538=EDGE_CURVE('',#41654,#41655,#29950,.T.);
#54539=EDGE_CURVE('',#41655,#41656,#22505,.T.);
#54540=EDGE_CURVE('',#41656,#41657,#29951,.T.);
#54541=EDGE_CURVE('',#41657,#41658,#25995,.T.);
#54542=EDGE_CURVE('',#41658,#41659,#29952,.T.);
#54543=EDGE_CURVE('',#41659,#41660,#22506,.T.);
#54544=EDGE_CURVE('',#41660,#41661,#29953,.T.);
#54545=EDGE_CURVE('',#41661,#41662,#25996,.T.);
#54546=EDGE_CURVE('',#41662,#41663,#29954,.T.);
#54547=EDGE_CURVE('',#41663,#41664,#22507,.T.);
#54548=EDGE_CURVE('',#41664,#41665,#29955,.T.);
#54549=EDGE_CURVE('',#41665,#41666,#25997,.T.);
#54550=EDGE_CURVE('',#41666,#41667,#29956,.T.);
#54551=EDGE_CURVE('',#41667,#41668,#22508,.T.);
#54552=EDGE_CURVE('',#41668,#41669,#29957,.T.);
#54553=EDGE_CURVE('',#41669,#41670,#25998,.T.);
#54554=EDGE_CURVE('',#41670,#41671,#29958,.T.);
#54555=EDGE_CURVE('',#41671,#41672,#22509,.T.);
#54556=EDGE_CURVE('',#41672,#41673,#29959,.T.);
#54557=EDGE_CURVE('',#41673,#41674,#25999,.T.);
#54558=EDGE_CURVE('',#41674,#41675,#29960,.T.);
#54559=EDGE_CURVE('',#41675,#41676,#22510,.T.);
#54560=EDGE_CURVE('',#41676,#41677,#29961,.T.);
#54561=EDGE_CURVE('',#41677,#41678,#26000,.T.);
#54562=EDGE_CURVE('',#41678,#41679,#29962,.T.);
#54563=EDGE_CURVE('',#41679,#41680,#22511,.T.);
#54564=EDGE_CURVE('',#41680,#41681,#29963,.T.);
#54565=EDGE_CURVE('',#41681,#41682,#26001,.T.);
#54566=EDGE_CURVE('',#41682,#41683,#29964,.T.);
#54567=EDGE_CURVE('',#41683,#41684,#22512,.T.);
#54568=EDGE_CURVE('',#41684,#41685,#29965,.T.);
#54569=EDGE_CURVE('',#41685,#41686,#26002,.T.);
#54570=EDGE_CURVE('',#41686,#41687,#29966,.T.);
#54571=EDGE_CURVE('',#41687,#41688,#22513,.T.);
#54572=EDGE_CURVE('',#41688,#41689,#29967,.T.);
#54573=EDGE_CURVE('',#41689,#41690,#26003,.T.);
#54574=EDGE_CURVE('',#41690,#41691,#29968,.T.);
#54575=EDGE_CURVE('',#41691,#41692,#22514,.T.);
#54576=EDGE_CURVE('',#41692,#41693,#29969,.T.);
#54577=EDGE_CURVE('',#41693,#41694,#26004,.T.);
#54578=EDGE_CURVE('',#41694,#41695,#29970,.T.);
#54579=EDGE_CURVE('',#41695,#41696,#22515,.T.);
#54580=EDGE_CURVE('',#41696,#41697,#29971,.T.);
#54581=EDGE_CURVE('',#41697,#41698,#26005,.T.);
#54582=EDGE_CURVE('',#41698,#41699,#29972,.T.);
#54583=EDGE_CURVE('',#41699,#41700,#22516,.T.);
#54584=EDGE_CURVE('',#41700,#41701,#29973,.T.);
#54585=EDGE_CURVE('',#41701,#41702,#26006,.T.);
#54586=EDGE_CURVE('',#41702,#41703,#29974,.T.);
#54587=EDGE_CURVE('',#41703,#41704,#22517,.T.);
#54588=EDGE_CURVE('',#41704,#41705,#29975,.T.);
#54589=EDGE_CURVE('',#41705,#41706,#26007,.T.);
#54590=EDGE_CURVE('',#41706,#41707,#29976,.T.);
#54591=EDGE_CURVE('',#41707,#41708,#22518,.T.);
#54592=EDGE_CURVE('',#41708,#41709,#29977,.T.);
#54593=EDGE_CURVE('',#41709,#41710,#26008,.T.);
#54594=EDGE_CURVE('',#41710,#41711,#29978,.T.);
#54595=EDGE_CURVE('',#41711,#41712,#22519,.T.);
#54596=EDGE_CURVE('',#41712,#41713,#29979,.T.);
#54597=EDGE_CURVE('',#41713,#41402,#26009,.T.);
#54598=EDGE_CURVE('',#41714,#41714,#22520,.T.);
#54599=EDGE_CURVE('',#41714,#41559,#22521,.T.);
#54600=EDGE_CURVE('',#41715,#41716,#22522,.T.);
#54601=EDGE_CURVE('',#41715,#41717,#29980,.T.);
#54602=EDGE_CURVE('',#41190,#41717,#26010,.T.);
#54603=EDGE_CURVE('',#41718,#41189,#26011,.T.);
#54604=EDGE_CURVE('',#41718,#41719,#29981,.T.);
#54605=EDGE_CURVE('',#41720,#41719,#22523,.T.);
#54606=EDGE_CURVE('',#41720,#41721,#29982,.T.);
#54607=EDGE_CURVE('',#41194,#41721,#26012,.T.);
#54608=EDGE_CURVE('',#41722,#41193,#26013,.T.);
#54609=EDGE_CURVE('',#41722,#41723,#29983,.T.);
#54610=EDGE_CURVE('',#41724,#41723,#22524,.T.);
#54611=EDGE_CURVE('',#41724,#41725,#29984,.T.);
#54612=EDGE_CURVE('',#41198,#41725,#26014,.T.);
#54613=EDGE_CURVE('',#41726,#41197,#26015,.T.);
#54614=EDGE_CURVE('',#41726,#41727,#29985,.T.);
#54615=EDGE_CURVE('',#41728,#41727,#22525,.T.);
#54616=EDGE_CURVE('',#41728,#41729,#29986,.T.);
#54617=EDGE_CURVE('',#41202,#41729,#26016,.T.);
#54618=EDGE_CURVE('',#41730,#41201,#26017,.T.);
#54619=EDGE_CURVE('',#41730,#41731,#29987,.T.);
#54620=EDGE_CURVE('',#41732,#41731,#22526,.T.);
#54621=EDGE_CURVE('',#41732,#41733,#29988,.T.);
#54622=EDGE_CURVE('',#41206,#41733,#26018,.T.);
#54623=EDGE_CURVE('',#41734,#41205,#26019,.T.);
#54624=EDGE_CURVE('',#41734,#41735,#29989,.T.);
#54625=EDGE_CURVE('',#41736,#41735,#22527,.T.);
#54626=EDGE_CURVE('',#41736,#41737,#29990,.T.);
#54627=EDGE_CURVE('',#41210,#41737,#26020,.T.);
#54628=EDGE_CURVE('',#41738,#41209,#26021,.T.);
#54629=EDGE_CURVE('',#41738,#41739,#29991,.T.);
#54630=EDGE_CURVE('',#41740,#41739,#22528,.T.);
#54631=EDGE_CURVE('',#41740,#41741,#29992,.T.);
#54632=EDGE_CURVE('',#41214,#41741,#26022,.T.);
#54633=EDGE_CURVE('',#41742,#41213,#26023,.T.);
#54634=EDGE_CURVE('',#41742,#41743,#29993,.T.);
#54635=EDGE_CURVE('',#41744,#41743,#22529,.T.);
#54636=EDGE_CURVE('',#41744,#41745,#29994,.T.);
#54637=EDGE_CURVE('',#41218,#41745,#26024,.T.);
#54638=EDGE_CURVE('',#41746,#41217,#26025,.T.);
#54639=EDGE_CURVE('',#41746,#41747,#29995,.T.);
#54640=EDGE_CURVE('',#41748,#41747,#22530,.T.);
#54641=EDGE_CURVE('',#41748,#41749,#29996,.T.);
#54642=EDGE_CURVE('',#41222,#41749,#26026,.T.);
#54643=EDGE_CURVE('',#41750,#41221,#26027,.T.);
#54644=EDGE_CURVE('',#41750,#41751,#29997,.T.);
#54645=EDGE_CURVE('',#41752,#41751,#22531,.T.);
#54646=EDGE_CURVE('',#41752,#41753,#29998,.T.);
#54647=EDGE_CURVE('',#41226,#41753,#26028,.T.);
#54648=EDGE_CURVE('',#41754,#41225,#26029,.T.);
#54649=EDGE_CURVE('',#41754,#41755,#29999,.T.);
#54650=EDGE_CURVE('',#41756,#41755,#22532,.T.);
#54651=EDGE_CURVE('',#41756,#41757,#30000,.T.);
#54652=EDGE_CURVE('',#41230,#41757,#26030,.T.);
#54653=EDGE_CURVE('',#41758,#41229,#26031,.T.);
#54654=EDGE_CURVE('',#41758,#41759,#30001,.T.);
#54655=EDGE_CURVE('',#41760,#41759,#22533,.T.);
#54656=EDGE_CURVE('',#41760,#41761,#30002,.T.);
#54657=EDGE_CURVE('',#41234,#41761,#26032,.T.);
#54658=EDGE_CURVE('',#41762,#41233,#26033,.T.);
#54659=EDGE_CURVE('',#41762,#41763,#30003,.T.);
#54660=EDGE_CURVE('',#41764,#41763,#22534,.T.);
#54661=EDGE_CURVE('',#41764,#41765,#30004,.T.);
#54662=EDGE_CURVE('',#41238,#41765,#26034,.T.);
#54663=EDGE_CURVE('',#41766,#41237,#26035,.T.);
#54664=EDGE_CURVE('',#41766,#41767,#30005,.T.);
#54665=EDGE_CURVE('',#41768,#41767,#22535,.T.);
#54666=EDGE_CURVE('',#41768,#41769,#30006,.T.);
#54667=EDGE_CURVE('',#41242,#41769,#26036,.T.);
#54668=EDGE_CURVE('',#41770,#41241,#26037,.T.);
#54669=EDGE_CURVE('',#41770,#41771,#30007,.T.);
#54670=EDGE_CURVE('',#41772,#41771,#22536,.T.);
#54671=EDGE_CURVE('',#41772,#41773,#30008,.T.);
#54672=EDGE_CURVE('',#41246,#41773,#26038,.T.);
#54673=EDGE_CURVE('',#41774,#41245,#26039,.T.);
#54674=EDGE_CURVE('',#41774,#41775,#30009,.T.);
#54675=EDGE_CURVE('',#41776,#41775,#22537,.T.);
#54676=EDGE_CURVE('',#41776,#41777,#30010,.T.);
#54677=EDGE_CURVE('',#41250,#41777,#26040,.T.);
#54678=EDGE_CURVE('',#41778,#41249,#26041,.T.);
#54679=EDGE_CURVE('',#41778,#41779,#30011,.T.);
#54680=EDGE_CURVE('',#41780,#41779,#22538,.T.);
#54681=EDGE_CURVE('',#41780,#41781,#30012,.T.);
#54682=EDGE_CURVE('',#41254,#41781,#26042,.T.);
#54683=EDGE_CURVE('',#41782,#41253,#26043,.T.);
#54684=EDGE_CURVE('',#41782,#41783,#30013,.T.);
#54685=EDGE_CURVE('',#41784,#41783,#22539,.T.);
#54686=EDGE_CURVE('',#41784,#41785,#30014,.T.);
#54687=EDGE_CURVE('',#41258,#41785,#26044,.T.);
#54688=EDGE_CURVE('',#41786,#41257,#26045,.T.);
#54689=EDGE_CURVE('',#41786,#41787,#30015,.T.);
#54690=EDGE_CURVE('',#41788,#41787,#22540,.T.);
#54691=EDGE_CURVE('',#41788,#41789,#30016,.T.);
#54692=EDGE_CURVE('',#41262,#41789,#26046,.T.);
#54693=EDGE_CURVE('',#41790,#41261,#26047,.T.);
#54694=EDGE_CURVE('',#41790,#41791,#30017,.T.);
#54695=EDGE_CURVE('',#41792,#41791,#22541,.T.);
#54696=EDGE_CURVE('',#41792,#41793,#30018,.T.);
#54697=EDGE_CURVE('',#41266,#41793,#26048,.T.);
#54698=EDGE_CURVE('',#41794,#41265,#26049,.T.);
#54699=EDGE_CURVE('',#41794,#41795,#30019,.T.);
#54700=EDGE_CURVE('',#41796,#41795,#22542,.T.);
#54701=EDGE_CURVE('',#41796,#41797,#30020,.T.);
#54702=EDGE_CURVE('',#41270,#41797,#26050,.T.);
#54703=EDGE_CURVE('',#41798,#41269,#26051,.T.);
#54704=EDGE_CURVE('',#41798,#41799,#30021,.T.);
#54705=EDGE_CURVE('',#41800,#41799,#22543,.T.);
#54706=EDGE_CURVE('',#41800,#41801,#30022,.T.);
#54707=EDGE_CURVE('',#41274,#41801,#26052,.T.);
#54708=EDGE_CURVE('',#41802,#41273,#26053,.T.);
#54709=EDGE_CURVE('',#41802,#41803,#30023,.T.);
#54710=EDGE_CURVE('',#41804,#41803,#22544,.T.);
#54711=EDGE_CURVE('',#41804,#41805,#30024,.T.);
#54712=EDGE_CURVE('',#41278,#41805,#26054,.T.);
#54713=EDGE_CURVE('',#41806,#41277,#26055,.T.);
#54714=EDGE_CURVE('',#41806,#41807,#30025,.T.);
#54715=EDGE_CURVE('',#41808,#41807,#22545,.T.);
#54716=EDGE_CURVE('',#41808,#41809,#30026,.T.);
#54717=EDGE_CURVE('',#41282,#41809,#26056,.T.);
#54718=EDGE_CURVE('',#41810,#41281,#26057,.T.);
#54719=EDGE_CURVE('',#41810,#41811,#30027,.T.);
#54720=EDGE_CURVE('',#41812,#41811,#22546,.T.);
#54721=EDGE_CURVE('',#41812,#41813,#30028,.T.);
#54722=EDGE_CURVE('',#41286,#41813,#26058,.T.);
#54723=EDGE_CURVE('',#41814,#41285,#26059,.T.);
#54724=EDGE_CURVE('',#41814,#41815,#30029,.T.);
#54725=EDGE_CURVE('',#41816,#41815,#22547,.T.);
#54726=EDGE_CURVE('',#41816,#41817,#30030,.T.);
#54727=EDGE_CURVE('',#41290,#41817,#26060,.T.);
#54728=EDGE_CURVE('',#41818,#41289,#26061,.T.);
#54729=EDGE_CURVE('',#41818,#41819,#30031,.T.);
#54730=EDGE_CURVE('',#41820,#41819,#22548,.T.);
#54731=EDGE_CURVE('',#41820,#41821,#30032,.T.);
#54732=EDGE_CURVE('',#41294,#41821,#26062,.T.);
#54733=EDGE_CURVE('',#41822,#41293,#26063,.T.);
#54734=EDGE_CURVE('',#41822,#41823,#30033,.T.);
#54735=EDGE_CURVE('',#41824,#41823,#22549,.T.);
#54736=EDGE_CURVE('',#41824,#41825,#30034,.T.);
#54737=EDGE_CURVE('',#41298,#41825,#26064,.T.);
#54738=EDGE_CURVE('',#41826,#41297,#26065,.T.);
#54739=EDGE_CURVE('',#41826,#41827,#30035,.T.);
#54740=EDGE_CURVE('',#41828,#41827,#22550,.T.);
#54741=EDGE_CURVE('',#41828,#41829,#30036,.T.);
#54742=EDGE_CURVE('',#41302,#41829,#26066,.T.);
#54743=EDGE_CURVE('',#41830,#41301,#26067,.T.);
#54744=EDGE_CURVE('',#41830,#41831,#30037,.T.);
#54745=EDGE_CURVE('',#41832,#41831,#22551,.T.);
#54746=EDGE_CURVE('',#41832,#41833,#30038,.T.);
#54747=EDGE_CURVE('',#41306,#41833,#26068,.T.);
#54748=EDGE_CURVE('',#41834,#41305,#26069,.T.);
#54749=EDGE_CURVE('',#41834,#41835,#30039,.T.);
#54750=EDGE_CURVE('',#41836,#41835,#22552,.T.);
#54751=EDGE_CURVE('',#41836,#41837,#30040,.T.);
#54752=EDGE_CURVE('',#41310,#41837,#26070,.T.);
#54753=EDGE_CURVE('',#41838,#41309,#26071,.T.);
#54754=EDGE_CURVE('',#41838,#41839,#30041,.T.);
#54755=EDGE_CURVE('',#41840,#41839,#22553,.T.);
#54756=EDGE_CURVE('',#41840,#41841,#30042,.T.);
#54757=EDGE_CURVE('',#41314,#41841,#26072,.T.);
#54758=EDGE_CURVE('',#41842,#41313,#26073,.T.);
#54759=EDGE_CURVE('',#41842,#41843,#30043,.T.);
#54760=EDGE_CURVE('',#41844,#41843,#22554,.T.);
#54761=EDGE_CURVE('',#41844,#41845,#30044,.T.);
#54762=EDGE_CURVE('',#41318,#41845,#26074,.T.);
#54763=EDGE_CURVE('',#41846,#41317,#26075,.T.);
#54764=EDGE_CURVE('',#41846,#41847,#30045,.T.);
#54765=EDGE_CURVE('',#41848,#41847,#22555,.T.);
#54766=EDGE_CURVE('',#41848,#41849,#30046,.T.);
#54767=EDGE_CURVE('',#41322,#41849,#26076,.T.);
#54768=EDGE_CURVE('',#41850,#41321,#26077,.T.);
#54769=EDGE_CURVE('',#41850,#41851,#30047,.T.);
#54770=EDGE_CURVE('',#41852,#41851,#22556,.T.);
#54771=EDGE_CURVE('',#41852,#41853,#30048,.T.);
#54772=EDGE_CURVE('',#41326,#41853,#26078,.T.);
#54773=EDGE_CURVE('',#41854,#41325,#26079,.T.);
#54774=EDGE_CURVE('',#41854,#41855,#30049,.T.);
#54775=EDGE_CURVE('',#41856,#41855,#22557,.T.);
#54776=EDGE_CURVE('',#41856,#41857,#30050,.T.);
#54777=EDGE_CURVE('',#41330,#41857,#26080,.T.);
#54778=EDGE_CURVE('',#41858,#41329,#26081,.T.);
#54779=EDGE_CURVE('',#41858,#41859,#30051,.T.);
#54780=EDGE_CURVE('',#41860,#41859,#22558,.T.);
#54781=EDGE_CURVE('',#41860,#41861,#30052,.T.);
#54782=EDGE_CURVE('',#41334,#41861,#26082,.T.);
#54783=EDGE_CURVE('',#41862,#41333,#26083,.T.);
#54784=EDGE_CURVE('',#41862,#41863,#30053,.T.);
#54785=EDGE_CURVE('',#41864,#41863,#22559,.T.);
#54786=EDGE_CURVE('',#41864,#41865,#30054,.T.);
#54787=EDGE_CURVE('',#41382,#41865,#26084,.T.);
#54788=EDGE_CURVE('',#41866,#41381,#26085,.T.);
#54789=EDGE_CURVE('',#41866,#41867,#30055,.T.);
#54790=EDGE_CURVE('',#41868,#41867,#22560,.T.);
#54791=EDGE_CURVE('',#41868,#41869,#30056,.T.);
#54792=EDGE_CURVE('',#41387,#41869,#26086,.T.);
#54793=EDGE_CURVE('',#41386,#41401,#30057,.T.);
#54794=EDGE_CURVE('',#41870,#41385,#26087,.T.);
#54795=EDGE_CURVE('',#41870,#41871,#30058,.T.);
#54796=EDGE_CURVE('',#41872,#41871,#22561,.T.);
#54797=EDGE_CURVE('',#41872,#41873,#30059,.T.);
#54798=EDGE_CURVE('',#41378,#41873,#26088,.T.);
#54799=EDGE_CURVE('',#41874,#41377,#26089,.T.);
#54800=EDGE_CURVE('',#41874,#41875,#30060,.T.);
#54801=EDGE_CURVE('',#41876,#41875,#22562,.T.);
#54802=EDGE_CURVE('',#41876,#41877,#30061,.T.);
#54803=EDGE_CURVE('',#41374,#41877,#26090,.T.);
#54804=EDGE_CURVE('',#41878,#41373,#26091,.T.);
#54805=EDGE_CURVE('',#41878,#41879,#30062,.T.);
#54806=EDGE_CURVE('',#41880,#41879,#22563,.T.);
#54807=EDGE_CURVE('',#41880,#41881,#30063,.T.);
#54808=EDGE_CURVE('',#41370,#41881,#26092,.T.);
#54809=EDGE_CURVE('',#41882,#41369,#26093,.T.);
#54810=EDGE_CURVE('',#41882,#41883,#30064,.T.);
#54811=EDGE_CURVE('',#41884,#41883,#22564,.T.);
#54812=EDGE_CURVE('',#41884,#41885,#30065,.T.);
#54813=EDGE_CURVE('',#41366,#41885,#26094,.T.);
#54814=EDGE_CURVE('',#41886,#41365,#26095,.T.);
#54815=EDGE_CURVE('',#41886,#41887,#30066,.T.);
#54816=EDGE_CURVE('',#41888,#41887,#22565,.T.);
#54817=EDGE_CURVE('',#41888,#41889,#30067,.T.);
#54818=EDGE_CURVE('',#41362,#41889,#26096,.T.);
#54819=EDGE_CURVE('',#41890,#41361,#26097,.T.);
#54820=EDGE_CURVE('',#41890,#41891,#30068,.T.);
#54821=EDGE_CURVE('',#41892,#41891,#22566,.T.);
#54822=EDGE_CURVE('',#41892,#41893,#30069,.T.);
#54823=EDGE_CURVE('',#41358,#41893,#26098,.T.);
#54824=EDGE_CURVE('',#41894,#41357,#26099,.T.);
#54825=EDGE_CURVE('',#41894,#41895,#30070,.T.);
#54826=EDGE_CURVE('',#41896,#41895,#22567,.T.);
#54827=EDGE_CURVE('',#41896,#41897,#30071,.T.);
#54828=EDGE_CURVE('',#41354,#41897,#26100,.T.);
#54829=EDGE_CURVE('',#41898,#41353,#26101,.T.);
#54830=EDGE_CURVE('',#41898,#41899,#30072,.T.);
#54831=EDGE_CURVE('',#41900,#41899,#22568,.T.);
#54832=EDGE_CURVE('',#41900,#41901,#30073,.T.);
#54833=EDGE_CURVE('',#41350,#41901,#26102,.T.);
#54834=EDGE_CURVE('',#41902,#41349,#26103,.T.);
#54835=EDGE_CURVE('',#41902,#41903,#30074,.T.);
#54836=EDGE_CURVE('',#41904,#41903,#22569,.T.);
#54837=EDGE_CURVE('',#41904,#41905,#30075,.T.);
#54838=EDGE_CURVE('',#41346,#41905,#26104,.T.);
#54839=EDGE_CURVE('',#41906,#41345,#26105,.T.);
#54840=EDGE_CURVE('',#41906,#41907,#30076,.T.);
#54841=EDGE_CURVE('',#41908,#41907,#22570,.T.);
#54842=EDGE_CURVE('',#41908,#41909,#30077,.T.);
#54843=EDGE_CURVE('',#41342,#41909,#26106,.T.);
#54844=EDGE_CURVE('',#41910,#41341,#26107,.T.);
#54845=EDGE_CURVE('',#41910,#41911,#30078,.T.);
#54846=EDGE_CURVE('',#41912,#41911,#22571,.T.);
#54847=EDGE_CURVE('',#41912,#41913,#30079,.T.);
#54848=EDGE_CURVE('',#41338,#41913,#26108,.T.);
#54849=EDGE_CURVE('',#41914,#41337,#26109,.T.);
#54850=EDGE_CURVE('',#41914,#41915,#30080,.T.);
#54851=EDGE_CURVE('',#41916,#41915,#22572,.T.);
#54852=EDGE_CURVE('',#41916,#41917,#30081,.T.);
#54853=EDGE_CURVE('',#41082,#41917,#26110,.T.);
#54854=EDGE_CURVE('',#41918,#41081,#26111,.T.);
#54855=EDGE_CURVE('',#41918,#41919,#30082,.T.);
#54856=EDGE_CURVE('',#41920,#41919,#22573,.T.);
#54857=EDGE_CURVE('',#41920,#41921,#30083,.T.);
#54858=EDGE_CURVE('',#41086,#41921,#26112,.T.);
#54859=EDGE_CURVE('',#41922,#41085,#26113,.T.);
#54860=EDGE_CURVE('',#41922,#41923,#30084,.T.);
#54861=EDGE_CURVE('',#41924,#41923,#22574,.T.);
#54862=EDGE_CURVE('',#41924,#41925,#30085,.T.);
#54863=EDGE_CURVE('',#41090,#41925,#26114,.T.);
#54864=EDGE_CURVE('',#41926,#41089,#26115,.T.);
#54865=EDGE_CURVE('',#41926,#41927,#30086,.T.);
#54866=EDGE_CURVE('',#41928,#41927,#22575,.T.);
#54867=EDGE_CURVE('',#41928,#41929,#30087,.T.);
#54868=EDGE_CURVE('',#41094,#41929,#26116,.T.);
#54869=EDGE_CURVE('',#41930,#41093,#26117,.T.);
#54870=EDGE_CURVE('',#41930,#41931,#30088,.T.);
#54871=EDGE_CURVE('',#41932,#41931,#22576,.T.);
#54872=EDGE_CURVE('',#41932,#41933,#30089,.T.);
#54873=EDGE_CURVE('',#41098,#41933,#26118,.T.);
#54874=EDGE_CURVE('',#41934,#41097,#26119,.T.);
#54875=EDGE_CURVE('',#41934,#41935,#30090,.T.);
#54876=EDGE_CURVE('',#41936,#41935,#22577,.T.);
#54877=EDGE_CURVE('',#41936,#41937,#30091,.T.);
#54878=EDGE_CURVE('',#41102,#41937,#26120,.T.);
#54879=EDGE_CURVE('',#41938,#41101,#26121,.T.);
#54880=EDGE_CURVE('',#41938,#41939,#30092,.T.);
#54881=EDGE_CURVE('',#41940,#41939,#22578,.T.);
#54882=EDGE_CURVE('',#41940,#41941,#30093,.T.);
#54883=EDGE_CURVE('',#41106,#41941,#26122,.T.);
#54884=EDGE_CURVE('',#41942,#41105,#26123,.T.);
#54885=EDGE_CURVE('',#41942,#41943,#30094,.T.);
#54886=EDGE_CURVE('',#41944,#41943,#22579,.T.);
#54887=EDGE_CURVE('',#41944,#41945,#30095,.T.);
#54888=EDGE_CURVE('',#41110,#41945,#26124,.T.);
#54889=EDGE_CURVE('',#41946,#41109,#26125,.T.);
#54890=EDGE_CURVE('',#41946,#41947,#30096,.T.);
#54891=EDGE_CURVE('',#41948,#41947,#22580,.T.);
#54892=EDGE_CURVE('',#41948,#41949,#30097,.T.);
#54893=EDGE_CURVE('',#41114,#41949,#26126,.T.);
#54894=EDGE_CURVE('',#41950,#41113,#26127,.T.);
#54895=EDGE_CURVE('',#41950,#41951,#30098,.T.);
#54896=EDGE_CURVE('',#41952,#41951,#22581,.T.);
#54897=EDGE_CURVE('',#41952,#41953,#30099,.T.);
#54898=EDGE_CURVE('',#41118,#41953,#26128,.T.);
#54899=EDGE_CURVE('',#41954,#41117,#26129,.T.);
#54900=EDGE_CURVE('',#41954,#41955,#30100,.T.);
#54901=EDGE_CURVE('',#41956,#41955,#22582,.T.);
#54902=EDGE_CURVE('',#41956,#41957,#30101,.T.);
#54903=EDGE_CURVE('',#41122,#41957,#26130,.T.);
#54904=EDGE_CURVE('',#41958,#41121,#26131,.T.);
#54905=EDGE_CURVE('',#41958,#41959,#30102,.T.);
#54906=EDGE_CURVE('',#41960,#41959,#22583,.T.);
#54907=EDGE_CURVE('',#41960,#41961,#30103,.T.);
#54908=EDGE_CURVE('',#41126,#41961,#26132,.T.);
#54909=EDGE_CURVE('',#41962,#41125,#26133,.T.);
#54910=EDGE_CURVE('',#41962,#41963,#30104,.T.);
#54911=EDGE_CURVE('',#41964,#41963,#22584,.T.);
#54912=EDGE_CURVE('',#41964,#41965,#30105,.T.);
#54913=EDGE_CURVE('',#41130,#41965,#26134,.T.);
#54914=EDGE_CURVE('',#41966,#41129,#26135,.T.);
#54915=EDGE_CURVE('',#41966,#41967,#30106,.T.);
#54916=EDGE_CURVE('',#41968,#41967,#22585,.T.);
#54917=EDGE_CURVE('',#41968,#41969,#30107,.T.);
#54918=EDGE_CURVE('',#41134,#41969,#26136,.T.);
#54919=EDGE_CURVE('',#41970,#41133,#26137,.T.);
#54920=EDGE_CURVE('',#41970,#41971,#30108,.T.);
#54921=EDGE_CURVE('',#41972,#41971,#22586,.T.);
#54922=EDGE_CURVE('',#41972,#41973,#30109,.T.);
#54923=EDGE_CURVE('',#41138,#41973,#26138,.T.);
#54924=EDGE_CURVE('',#41974,#41137,#26139,.T.);
#54925=EDGE_CURVE('',#41974,#41975,#30110,.T.);
#54926=EDGE_CURVE('',#41976,#41975,#22587,.T.);
#54927=EDGE_CURVE('',#41976,#41977,#30111,.T.);
#54928=EDGE_CURVE('',#41142,#41977,#26140,.T.);
#54929=EDGE_CURVE('',#41978,#41141,#26141,.T.);
#54930=EDGE_CURVE('',#41978,#41979,#30112,.T.);
#54931=EDGE_CURVE('',#41980,#41979,#22588,.T.);
#54932=EDGE_CURVE('',#41980,#41981,#30113,.T.);
#54933=EDGE_CURVE('',#41146,#41981,#26142,.T.);
#54934=EDGE_CURVE('',#41982,#41145,#26143,.T.);
#54935=EDGE_CURVE('',#41982,#41983,#30114,.T.);
#54936=EDGE_CURVE('',#41984,#41983,#22589,.T.);
#54937=EDGE_CURVE('',#41984,#41985,#30115,.T.);
#54938=EDGE_CURVE('',#41150,#41985,#26144,.T.);
#54939=EDGE_CURVE('',#41986,#41149,#26145,.T.);
#54940=EDGE_CURVE('',#41986,#41987,#30116,.T.);
#54941=EDGE_CURVE('',#41988,#41987,#22590,.T.);
#54942=EDGE_CURVE('',#41988,#41989,#30117,.T.);
#54943=EDGE_CURVE('',#41154,#41989,#26146,.T.);
#54944=EDGE_CURVE('',#41990,#41153,#26147,.T.);
#54945=EDGE_CURVE('',#41990,#41991,#30118,.T.);
#54946=EDGE_CURVE('',#41992,#41991,#22591,.T.);
#54947=EDGE_CURVE('',#41992,#41993,#30119,.T.);
#54948=EDGE_CURVE('',#41158,#41993,#26148,.T.);
#54949=EDGE_CURVE('',#41994,#41157,#26149,.T.);
#54950=EDGE_CURVE('',#41994,#41995,#30120,.T.);
#54951=EDGE_CURVE('',#41996,#41995,#22592,.T.);
#54952=EDGE_CURVE('',#41996,#41997,#30121,.T.);
#54953=EDGE_CURVE('',#41162,#41997,#26150,.T.);
#54954=EDGE_CURVE('',#41998,#41161,#26151,.T.);
#54955=EDGE_CURVE('',#41998,#41999,#30122,.T.);
#54956=EDGE_CURVE('',#42000,#41999,#22593,.T.);
#54957=EDGE_CURVE('',#42000,#42001,#30123,.T.);
#54958=EDGE_CURVE('',#41166,#42001,#26152,.T.);
#54959=EDGE_CURVE('',#42002,#41165,#26153,.T.);
#54960=EDGE_CURVE('',#42002,#42003,#30124,.T.);
#54961=EDGE_CURVE('',#42004,#42003,#22594,.T.);
#54962=EDGE_CURVE('',#42004,#42005,#30125,.T.);
#54963=EDGE_CURVE('',#41170,#42005,#26154,.T.);
#54964=EDGE_CURVE('',#42006,#41169,#26155,.T.);
#54965=EDGE_CURVE('',#42006,#42007,#30126,.T.);
#54966=EDGE_CURVE('',#42008,#42007,#22595,.T.);
#54967=EDGE_CURVE('',#42008,#42009,#30127,.T.);
#54968=EDGE_CURVE('',#41174,#42009,#26156,.T.);
#54969=EDGE_CURVE('',#42010,#41173,#26157,.T.);
#54970=EDGE_CURVE('',#42010,#42011,#30128,.T.);
#54971=EDGE_CURVE('',#42012,#42011,#22596,.T.);
#54972=EDGE_CURVE('',#42012,#42013,#30129,.T.);
#54973=EDGE_CURVE('',#41178,#42013,#26158,.T.);
#54974=EDGE_CURVE('',#42014,#41177,#26159,.T.);
#54975=EDGE_CURVE('',#42014,#42015,#30130,.T.);
#54976=EDGE_CURVE('',#42016,#42015,#22597,.T.);
#54977=EDGE_CURVE('',#42016,#42017,#30131,.T.);
#54978=EDGE_CURVE('',#41182,#42017,#26160,.T.);
#54979=EDGE_CURVE('',#42018,#41181,#26161,.T.);
#54980=EDGE_CURVE('',#42018,#42019,#30132,.T.);
#54981=EDGE_CURVE('',#42020,#42019,#22598,.T.);
#54982=EDGE_CURVE('',#42020,#42021,#30133,.T.);
#54983=EDGE_CURVE('',#41186,#42021,#26162,.T.);
#54984=EDGE_CURVE('',#42022,#41185,#26163,.T.);
#54985=EDGE_CURVE('',#42022,#41716,#30134,.T.);
#54986=EDGE_CURVE('',#41716,#41560,#1080,.T.);
#54987=EDGE_CURVE('',#41556,#41715,#1081,.T.);
#54988=EDGE_CURVE('',#41667,#41916,#1082,.T.);
#54989=EDGE_CURVE('',#41915,#41668,#1083,.T.);
#54990=EDGE_CURVE('',#41919,#41664,#1084,.T.);
#54991=EDGE_CURVE('',#41663,#41920,#1085,.T.);
#54992=EDGE_CURVE('',#41923,#41660,#1086,.T.);
#54993=EDGE_CURVE('',#41659,#41924,#1087,.T.);
#54994=EDGE_CURVE('',#41927,#41656,#1088,.T.);
#54995=EDGE_CURVE('',#41655,#41928,#1089,.T.);
#54996=EDGE_CURVE('',#41931,#41652,#1090,.T.);
#54997=EDGE_CURVE('',#41651,#41932,#1091,.T.);
#54998=EDGE_CURVE('',#41935,#41648,#1092,.T.);
#54999=EDGE_CURVE('',#41647,#41936,#1093,.T.);
#55000=EDGE_CURVE('',#41939,#41644,#1094,.T.);
#55001=EDGE_CURVE('',#41643,#41940,#1095,.T.);
#55002=EDGE_CURVE('',#41943,#41640,#1096,.T.);
#55003=EDGE_CURVE('',#41639,#41944,#1097,.T.);
#55004=EDGE_CURVE('',#41947,#41636,#1098,.T.);
#55005=EDGE_CURVE('',#41635,#41948,#1099,.T.);
#55006=EDGE_CURVE('',#41951,#41632,#1100,.T.);
#55007=EDGE_CURVE('',#41631,#41952,#1101,.T.);
#55008=EDGE_CURVE('',#41955,#41628,#1102,.T.);
#55009=EDGE_CURVE('',#41627,#41956,#1103,.T.);
#55010=EDGE_CURVE('',#41959,#41624,#1104,.T.);
#55011=EDGE_CURVE('',#41623,#41960,#1105,.T.);
#55012=EDGE_CURVE('',#41963,#41620,#1106,.T.);
#55013=EDGE_CURVE('',#41619,#41964,#1107,.T.);
#55014=EDGE_CURVE('',#41967,#41616,#1108,.T.);
#55015=EDGE_CURVE('',#41615,#41968,#1109,.T.);
#55016=EDGE_CURVE('',#41971,#41612,#1110,.T.);
#55017=EDGE_CURVE('',#41611,#41972,#1111,.T.);
#55018=EDGE_CURVE('',#41975,#41608,#1112,.T.);
#55019=EDGE_CURVE('',#41607,#41976,#1113,.T.);
#55020=EDGE_CURVE('',#41979,#41604,#1114,.T.);
#55021=EDGE_CURVE('',#41603,#41980,#1115,.T.);
#55022=EDGE_CURVE('',#41983,#41600,#1116,.T.);
#55023=EDGE_CURVE('',#41599,#41984,#1117,.T.);
#55024=EDGE_CURVE('',#41987,#41596,#1118,.T.);
#55025=EDGE_CURVE('',#41595,#41988,#1119,.T.);
#55026=EDGE_CURVE('',#41991,#41592,#1120,.T.);
#55027=EDGE_CURVE('',#41591,#41992,#1121,.T.);
#55028=EDGE_CURVE('',#41995,#41588,#1122,.T.);
#55029=EDGE_CURVE('',#41587,#41996,#1123,.T.);
#55030=EDGE_CURVE('',#41999,#41584,#1124,.T.);
#55031=EDGE_CURVE('',#41583,#42000,#1125,.T.);
#55032=EDGE_CURVE('',#42003,#41580,#1126,.T.);
#55033=EDGE_CURVE('',#41579,#42004,#1127,.T.);
#55034=EDGE_CURVE('',#42007,#41576,#1128,.T.);
#55035=EDGE_CURVE('',#41575,#42008,#1129,.T.);
#55036=EDGE_CURVE('',#42011,#41572,#1130,.T.);
#55037=EDGE_CURVE('',#41571,#42012,#1131,.T.);
#55038=EDGE_CURVE('',#42015,#41568,#1132,.T.);
#55039=EDGE_CURVE('',#41567,#42016,#1133,.T.);
#55040=EDGE_CURVE('',#42019,#41564,#1134,.T.);
#55041=EDGE_CURVE('',#41563,#42020,#1135,.T.);
#55042=EDGE_CURVE('',#41719,#41553,#1136,.T.);
#55043=EDGE_CURVE('',#41552,#41720,#1137,.T.);
#55044=EDGE_CURVE('',#41723,#41549,#1138,.T.);
#55045=EDGE_CURVE('',#41548,#41724,#1139,.T.);
#55046=EDGE_CURVE('',#41727,#41545,#1140,.T.);
#55047=EDGE_CURVE('',#41544,#41728,#1141,.T.);
#55048=EDGE_CURVE('',#41731,#41541,#1142,.T.);
#55049=EDGE_CURVE('',#41540,#41732,#1143,.T.);
#55050=EDGE_CURVE('',#41735,#41537,#1144,.T.);
#55051=EDGE_CURVE('',#41536,#41736,#1145,.T.);
#55052=EDGE_CURVE('',#41739,#41533,#1146,.T.);
#55053=EDGE_CURVE('',#41532,#41740,#1147,.T.);
#55054=EDGE_CURVE('',#41743,#41529,#1148,.T.);
#55055=EDGE_CURVE('',#41528,#41744,#1149,.T.);
#55056=EDGE_CURVE('',#41747,#41525,#1150,.T.);
#55057=EDGE_CURVE('',#41524,#41748,#1151,.T.);
#55058=EDGE_CURVE('',#41751,#41521,#1152,.T.);
#55059=EDGE_CURVE('',#41520,#41752,#1153,.T.);
#55060=EDGE_CURVE('',#41755,#41517,#1154,.T.);
#55061=EDGE_CURVE('',#41516,#41756,#1155,.T.);
#55062=EDGE_CURVE('',#41759,#41513,#1156,.T.);
#55063=EDGE_CURVE('',#41512,#41760,#1157,.T.);
#55064=EDGE_CURVE('',#41763,#41509,#1158,.T.);
#55065=EDGE_CURVE('',#41508,#41764,#1159,.T.);
#55066=EDGE_CURVE('',#41767,#41505,#1160,.T.);
#55067=EDGE_CURVE('',#41504,#41768,#1161,.T.);
#55068=EDGE_CURVE('',#41771,#41501,#1162,.T.);
#55069=EDGE_CURVE('',#41500,#41772,#1163,.T.);
#55070=EDGE_CURVE('',#41775,#41497,#1164,.T.);
#55071=EDGE_CURVE('',#41496,#41776,#1165,.T.);
#55072=EDGE_CURVE('',#41779,#41493,#1166,.T.);
#55073=EDGE_CURVE('',#41492,#41780,#1167,.T.);
#55074=EDGE_CURVE('',#41783,#41489,#1168,.T.);
#55075=EDGE_CURVE('',#41488,#41784,#1169,.T.);
#55076=EDGE_CURVE('',#41787,#41485,#1170,.T.);
#55077=EDGE_CURVE('',#41484,#41788,#1171,.T.);
#55078=EDGE_CURVE('',#41791,#41481,#1172,.T.);
#55079=EDGE_CURVE('',#41480,#41792,#1173,.T.);
#55080=EDGE_CURVE('',#41795,#41477,#1174,.T.);
#55081=EDGE_CURVE('',#41476,#41796,#1175,.T.);
#55082=EDGE_CURVE('',#41799,#41473,#1176,.T.);
#55083=EDGE_CURVE('',#41472,#41800,#1177,.T.);
#55084=EDGE_CURVE('',#41803,#41469,#1178,.T.);
#55085=EDGE_CURVE('',#41468,#41804,#1179,.T.);
#55086=EDGE_CURVE('',#41807,#41465,#1180,.T.);
#55087=EDGE_CURVE('',#41464,#41808,#1181,.T.);
#55088=EDGE_CURVE('',#41811,#41461,#1182,.T.);
#55089=EDGE_CURVE('',#41460,#41812,#1183,.T.);
#55090=EDGE_CURVE('',#41815,#41457,#1184,.T.);
#55091=EDGE_CURVE('',#41456,#41816,#1185,.T.);
#55092=EDGE_CURVE('',#41819,#41453,#1186,.T.);
#55093=EDGE_CURVE('',#41452,#41820,#1187,.T.);
#55094=EDGE_CURVE('',#41823,#41449,#1188,.T.);
#55095=EDGE_CURVE('',#41448,#41824,#1189,.T.);
#55096=EDGE_CURVE('',#41827,#41445,#1190,.T.);
#55097=EDGE_CURVE('',#41444,#41828,#1191,.T.);
#55098=EDGE_CURVE('',#41831,#41441,#1192,.T.);
#55099=EDGE_CURVE('',#41440,#41832,#1193,.T.);
#55100=EDGE_CURVE('',#41835,#41437,#1194,.T.);
#55101=EDGE_CURVE('',#41436,#41836,#1195,.T.);
#55102=EDGE_CURVE('',#41839,#41433,#1196,.T.);
#55103=EDGE_CURVE('',#41432,#41840,#1197,.T.);
#55104=EDGE_CURVE('',#41843,#41429,#1198,.T.);
#55105=EDGE_CURVE('',#41428,#41844,#1199,.T.);
#55106=EDGE_CURVE('',#41847,#41425,#1200,.T.);
#55107=EDGE_CURVE('',#41424,#41848,#1201,.T.);
#55108=EDGE_CURVE('',#41851,#41421,#1202,.T.);
#55109=EDGE_CURVE('',#41420,#41852,#1203,.T.);
#55110=EDGE_CURVE('',#41855,#41417,#1204,.T.);
#55111=EDGE_CURVE('',#41416,#41856,#1205,.T.);
#55112=EDGE_CURVE('',#41859,#41413,#1206,.T.);
#55113=EDGE_CURVE('',#41412,#41860,#1207,.T.);
#55114=EDGE_CURVE('',#41671,#41912,#1208,.T.);
#55115=EDGE_CURVE('',#41911,#41672,#1209,.T.);
#55116=EDGE_CURVE('',#41675,#41908,#1210,.T.);
#55117=EDGE_CURVE('',#41907,#41676,#1211,.T.);
#55118=EDGE_CURVE('',#41679,#41904,#1212,.T.);
#55119=EDGE_CURVE('',#41903,#41680,#1213,.T.);
#55120=EDGE_CURVE('',#41683,#41900,#1214,.T.);
#55121=EDGE_CURVE('',#41899,#41684,#1215,.T.);
#55122=EDGE_CURVE('',#41687,#41896,#1216,.T.);
#55123=EDGE_CURVE('',#41895,#41688,#1217,.T.);
#55124=EDGE_CURVE('',#41691,#41892,#1218,.T.);
#55125=EDGE_CURVE('',#41891,#41692,#1219,.T.);
#55126=EDGE_CURVE('',#41695,#41888,#1220,.T.);
#55127=EDGE_CURVE('',#41887,#41696,#1221,.T.);
#55128=EDGE_CURVE('',#41699,#41884,#1222,.T.);
#55129=EDGE_CURVE('',#41883,#41700,#1223,.T.);
#55130=EDGE_CURVE('',#41703,#41880,#1224,.T.);
#55131=EDGE_CURVE('',#41879,#41704,#1225,.T.);
#55132=EDGE_CURVE('',#41707,#41876,#1226,.T.);
#55133=EDGE_CURVE('',#41875,#41708,#1227,.T.);
#55134=EDGE_CURVE('',#41711,#41872,#1228,.T.);
#55135=EDGE_CURVE('',#41871,#41712,#1229,.T.);
#55136=EDGE_CURVE('',#41863,#41409,#1230,.T.);
#55137=EDGE_CURVE('',#41408,#41864,#1231,.T.);
#55138=EDGE_CURVE('',#42023,#42024,#30135,.T.);
#55139=EDGE_CURVE('',#42024,#42025,#26164,.T.);
#55140=EDGE_CURVE('',#42025,#42026,#26165,.T.);
#55141=EDGE_CURVE('',#42027,#42026,#30136,.T.);
#55142=EDGE_CURVE('',#42027,#42028,#1232,.T.);
#55143=EDGE_CURVE('',#42028,#42023,#1233,.T.);
#55144=EDGE_CURVE('',#42029,#42030,#1234,.T.);
#55145=EDGE_CURVE('',#42030,#42024,#30137,.T.);
#55146=EDGE_CURVE('',#42023,#42031,#26166,.T.);
#55147=EDGE_CURVE('',#42031,#42029,#30138,.T.);
#55148=EDGE_CURVE('',#42026,#42032,#30139,.T.);
#55149=EDGE_CURVE('',#42032,#42033,#1235,.T.);
#55150=EDGE_CURVE('',#42033,#42034,#30140,.T.);
#55151=EDGE_CURVE('',#42034,#42027,#26167,.T.);
#55152=EDGE_CURVE('',#42035,#41394,#30141,.T.);
#55153=EDGE_CURVE('',#41393,#42035,#30142,.T.);
#55154=EDGE_CURVE('',#42036,#41393,#30143,.T.);
#55155=EDGE_CURVE('',#41392,#42036,#30144,.T.);
#55156=EDGE_CURVE('',#42037,#41392,#30145,.T.);
#55157=EDGE_CURVE('',#41391,#42037,#30146,.T.);
#55158=EDGE_CURVE('',#42038,#41391,#30147,.T.);
#55159=EDGE_CURVE('',#41390,#42038,#30148,.T.);
#55160=EDGE_CURVE('',#42039,#41390,#30149,.T.);
#55161=EDGE_CURVE('',#41395,#42039,#30150,.T.);
#55162=EDGE_CURVE('',#42040,#42041,#22599,.T.);
#55163=EDGE_CURVE('',#41396,#42040,#22600,.T.);
#55164=EDGE_CURVE('',#42042,#41397,#22601,.T.);
#55165=EDGE_CURVE('',#42043,#42042,#22602,.T.);
#55166=EDGE_CURVE('',#42041,#42043,#22603,.T.);
#55167=EDGE_CURVE('',#41867,#41405,#1236,.T.);
#55168=EDGE_CURVE('',#41404,#41868,#1237,.T.);
#55169=EDGE_CURVE('',#42035,#41396,#30151,.T.);
#55170=EDGE_CURVE('',#42040,#41396,#4398,.T.);
#55171=EDGE_CURVE('',#42044,#42040,#30152,.T.);
#55172=EDGE_CURVE('',#41394,#42044,#30153,.T.);
#55173=EDGE_CURVE('',#42036,#41397,#30154,.T.);
#55174=EDGE_CURVE('',#42037,#42042,#30155,.T.);
#55175=EDGE_CURVE('',#41397,#42042,#4399,.T.);
#55176=EDGE_CURVE('',#42038,#42043,#30156,.T.);
#55177=EDGE_CURVE('',#42042,#42043,#4400,.T.);
#55178=EDGE_CURVE('',#42039,#42041,#30157,.T.);
#55179=EDGE_CURVE('',#42043,#42041,#4401,.T.);
#55180=EDGE_CURVE('',#42041,#42040,#4402,.T.);
#55181=EDGE_CURVE('',#42044,#41395,#30158,.T.);
#55182=EDGE_CURVE('',#40996,#41000,#4403,.T.);
#55183=EDGE_CURVE('',#40997,#41001,#4404,.T.);
#55184=EDGE_CURVE('',#42045,#42046,#26168,.T.);
#55185=EDGE_CURVE('',#42046,#41383,#1238,.T.);
#55186=EDGE_CURVE('',#41384,#42045,#26169,.T.);
#55187=EDGE_CURVE('',#42031,#41384,#26170,.T.);
#55188=EDGE_CURVE('',#42045,#42023,#22604,.T.);
#55189=EDGE_CURVE('',#42029,#41868,#22605,.T.);
#55190=EDGE_CURVE('',#41869,#42031,#22606,.T.);
#55191=EDGE_CURVE('',#42046,#42027,#22607,.T.);
#55192=EDGE_CURVE('',#42030,#41404,#22608,.T.);
#55193=EDGE_CURVE('',#41383,#42034,#26171,.T.);
#55194=EDGE_CURVE('',#42024,#41403,#22609,.T.);
#55195=EDGE_CURVE('',#41870,#42034,#22610,.T.);
#55196=EDGE_CURVE('',#42026,#41713,#22611,.T.);
#55197=EDGE_CURVE('',#41871,#42033,#22612,.T.);
#55198=EDGE_CURVE('',#42032,#41712,#22613,.T.);
#55199=EDGE_CURVE('',#42047,#42048,#30159,.T.);
#55200=EDGE_CURVE('',#42048,#42049,#30160,.T.);
#55201=EDGE_CURVE('',#42049,#42050,#1239,.T.);
#55202=EDGE_CURVE('',#42050,#42051,#30161,.T.);
#55203=EDGE_CURVE('',#42051,#42047,#26172,.T.);
#55204=EDGE_CURVE('',#42052,#42053,#1240,.T.);
#55205=EDGE_CURVE('',#42053,#42054,#30162,.T.);
#55206=EDGE_CURVE('',#42055,#42054,#30163,.T.);
#55207=EDGE_CURVE('',#42055,#42056,#26173,.T.);
#55208=EDGE_CURVE('',#42056,#42052,#30164,.T.);
#55209=EDGE_CURVE('',#42054,#42057,#26174,.T.);
#55210=EDGE_CURVE('',#42057,#42048,#26175,.T.);
#55211=EDGE_CURVE('',#42047,#42058,#1241,.T.);
#55212=EDGE_CURVE('',#42058,#42055,#1242,.T.);
#55213=EDGE_CURVE('',#42056,#41380,#26176,.T.);
#55214=EDGE_CURVE('',#42059,#42055,#22614,.T.);
#55215=EDGE_CURVE('',#41380,#42059,#26177,.T.);
#55216=EDGE_CURVE('',#42060,#42047,#22615,.T.);
#55217=EDGE_CURVE('',#42059,#42060,#26178,.T.);
#55218=EDGE_CURVE('',#41379,#42051,#26179,.T.);
#55219=EDGE_CURVE('',#42060,#41379,#1243,.T.);
#55220=EDGE_CURVE('',#41865,#42056,#22616,.T.);
#55221=EDGE_CURVE('',#42052,#41864,#22617,.T.);
#55222=EDGE_CURVE('',#42053,#41408,#22618,.T.);
#55223=EDGE_CURVE('',#42054,#41407,#22619,.T.);
#55224=EDGE_CURVE('',#42048,#41406,#22620,.T.);
#55225=EDGE_CURVE('',#42049,#41405,#22621,.T.);
#55226=EDGE_CURVE('',#41867,#42050,#22622,.T.);
#55227=EDGE_CURVE('',#41866,#42051,#22623,.T.);
#55228=EDGE_CURVE('',#42061,#42062,#30165,.T.);
#55229=EDGE_CURVE('',#42062,#42063,#30166,.T.);
#55230=EDGE_CURVE('',#42063,#42064,#1244,.T.);
#55231=EDGE_CURVE('',#42064,#42065,#30167,.T.);
#55232=EDGE_CURVE('',#42065,#42061,#26180,.T.);
#55233=EDGE_CURVE('',#42066,#42067,#1245,.T.);
#55234=EDGE_CURVE('',#42067,#42068,#30168,.T.);
#55235=EDGE_CURVE('',#42069,#42068,#30169,.T.);
#55236=EDGE_CURVE('',#42069,#42070,#26181,.T.);
#55237=EDGE_CURVE('',#42070,#42066,#30170,.T.);
#55238=EDGE_CURVE('',#42068,#42071,#26182,.T.);
#55239=EDGE_CURVE('',#42071,#42062,#26183,.T.);
#55240=EDGE_CURVE('',#42061,#42072,#1246,.T.);
#55241=EDGE_CURVE('',#42072,#42069,#1247,.T.);
#55242=EDGE_CURVE('',#42070,#41376,#26184,.T.);
#55243=EDGE_CURVE('',#42073,#42069,#22624,.T.);
#55244=EDGE_CURVE('',#41376,#42073,#26185,.T.);
#55245=EDGE_CURVE('',#42074,#42061,#22625,.T.);
#55246=EDGE_CURVE('',#42073,#42074,#26186,.T.);
#55247=EDGE_CURVE('',#41375,#42065,#26187,.T.);
#55248=EDGE_CURVE('',#42074,#41375,#1248,.T.);
#55249=EDGE_CURVE('',#41873,#42070,#22626,.T.);
#55250=EDGE_CURVE('',#42066,#41872,#22627,.T.);
#55251=EDGE_CURVE('',#42067,#41711,#22628,.T.);
#55252=EDGE_CURVE('',#42068,#41710,#22629,.T.);
#55253=EDGE_CURVE('',#42062,#41709,#22630,.T.);
#55254=EDGE_CURVE('',#42063,#41708,#22631,.T.);
#55255=EDGE_CURVE('',#41875,#42064,#22632,.T.);
#55256=EDGE_CURVE('',#41874,#42065,#22633,.T.);
#55257=EDGE_CURVE('',#42075,#42076,#30171,.T.);
#55258=EDGE_CURVE('',#42076,#42077,#30172,.T.);
#55259=EDGE_CURVE('',#42077,#42078,#1249,.T.);
#55260=EDGE_CURVE('',#42078,#42079,#30173,.T.);
#55261=EDGE_CURVE('',#42079,#42075,#26188,.T.);
#55262=EDGE_CURVE('',#42080,#42081,#1250,.T.);
#55263=EDGE_CURVE('',#42081,#42082,#30174,.T.);
#55264=EDGE_CURVE('',#42083,#42082,#30175,.T.);
#55265=EDGE_CURVE('',#42083,#42084,#26189,.T.);
#55266=EDGE_CURVE('',#42084,#42080,#30176,.T.);
#55267=EDGE_CURVE('',#42082,#42085,#26190,.T.);
#55268=EDGE_CURVE('',#42085,#42076,#26191,.T.);
#55269=EDGE_CURVE('',#42075,#42086,#1251,.T.);
#55270=EDGE_CURVE('',#42086,#42083,#1252,.T.);
#55271=EDGE_CURVE('',#42084,#41372,#26192,.T.);
#55272=EDGE_CURVE('',#42087,#42083,#22634,.T.);
#55273=EDGE_CURVE('',#41372,#42087,#26193,.T.);
#55274=EDGE_CURVE('',#42088,#42075,#22635,.T.);
#55275=EDGE_CURVE('',#42087,#42088,#26194,.T.);
#55276=EDGE_CURVE('',#41371,#42079,#26195,.T.);
#55277=EDGE_CURVE('',#42088,#41371,#1253,.T.);
#55278=EDGE_CURVE('',#41877,#42084,#22636,.T.);
#55279=EDGE_CURVE('',#42080,#41876,#22637,.T.);
#55280=EDGE_CURVE('',#42081,#41707,#22638,.T.);
#55281=EDGE_CURVE('',#42082,#41706,#22639,.T.);
#55282=EDGE_CURVE('',#42076,#41705,#22640,.T.);
#55283=EDGE_CURVE('',#42077,#41704,#22641,.T.);
#55284=EDGE_CURVE('',#41879,#42078,#22642,.T.);
#55285=EDGE_CURVE('',#41878,#42079,#22643,.T.);
#55286=EDGE_CURVE('',#42089,#42090,#30177,.T.);
#55287=EDGE_CURVE('',#42090,#42091,#30178,.T.);
#55288=EDGE_CURVE('',#42091,#42092,#1254,.T.);
#55289=EDGE_CURVE('',#42092,#42093,#30179,.T.);
#55290=EDGE_CURVE('',#42093,#42089,#26196,.T.);
#55291=EDGE_CURVE('',#42094,#42095,#1255,.T.);
#55292=EDGE_CURVE('',#42095,#42096,#30180,.T.);
#55293=EDGE_CURVE('',#42097,#42096,#30181,.T.);
#55294=EDGE_CURVE('',#42097,#42098,#26197,.T.);
#55295=EDGE_CURVE('',#42098,#42094,#30182,.T.);
#55296=EDGE_CURVE('',#42096,#42099,#26198,.T.);
#55297=EDGE_CURVE('',#42099,#42090,#26199,.T.);
#55298=EDGE_CURVE('',#42089,#42100,#1256,.T.);
#55299=EDGE_CURVE('',#42100,#42097,#1257,.T.);
#55300=EDGE_CURVE('',#42098,#41368,#26200,.T.);
#55301=EDGE_CURVE('',#42101,#42097,#22644,.T.);
#55302=EDGE_CURVE('',#41368,#42101,#26201,.T.);
#55303=EDGE_CURVE('',#42102,#42089,#22645,.T.);
#55304=EDGE_CURVE('',#42101,#42102,#26202,.T.);
#55305=EDGE_CURVE('',#41367,#42093,#26203,.T.);
#55306=EDGE_CURVE('',#42102,#41367,#1258,.T.);
#55307=EDGE_CURVE('',#41881,#42098,#22646,.T.);
#55308=EDGE_CURVE('',#42094,#41880,#22647,.T.);
#55309=EDGE_CURVE('',#42095,#41703,#22648,.T.);
#55310=EDGE_CURVE('',#42096,#41702,#22649,.T.);
#55311=EDGE_CURVE('',#42090,#41701,#22650,.T.);
#55312=EDGE_CURVE('',#42091,#41700,#22651,.T.);
#55313=EDGE_CURVE('',#41883,#42092,#22652,.T.);
#55314=EDGE_CURVE('',#41882,#42093,#22653,.T.);
#55315=EDGE_CURVE('',#42103,#42104,#30183,.T.);
#55316=EDGE_CURVE('',#42104,#42105,#30184,.T.);
#55317=EDGE_CURVE('',#42105,#42106,#1259,.T.);
#55318=EDGE_CURVE('',#42106,#42107,#30185,.T.);
#55319=EDGE_CURVE('',#42107,#42103,#26204,.T.);
#55320=EDGE_CURVE('',#42108,#42109,#1260,.T.);
#55321=EDGE_CURVE('',#42109,#42110,#30186,.T.);
#55322=EDGE_CURVE('',#42111,#42110,#30187,.T.);
#55323=EDGE_CURVE('',#42111,#42112,#26205,.T.);
#55324=EDGE_CURVE('',#42112,#42108,#30188,.T.);
#55325=EDGE_CURVE('',#42110,#42113,#26206,.T.);
#55326=EDGE_CURVE('',#42113,#42104,#26207,.T.);
#55327=EDGE_CURVE('',#42103,#42114,#1261,.T.);
#55328=EDGE_CURVE('',#42114,#42111,#1262,.T.);
#55329=EDGE_CURVE('',#42112,#41364,#26208,.T.);
#55330=EDGE_CURVE('',#42115,#42111,#22654,.T.);
#55331=EDGE_CURVE('',#41364,#42115,#26209,.T.);
#55332=EDGE_CURVE('',#42116,#42103,#22655,.T.);
#55333=EDGE_CURVE('',#42115,#42116,#26210,.T.);
#55334=EDGE_CURVE('',#41363,#42107,#26211,.T.);
#55335=EDGE_CURVE('',#42116,#41363,#1263,.T.);
#55336=EDGE_CURVE('',#41885,#42112,#22656,.T.);
#55337=EDGE_CURVE('',#42108,#41884,#22657,.T.);
#55338=EDGE_CURVE('',#42109,#41699,#22658,.T.);
#55339=EDGE_CURVE('',#42110,#41698,#22659,.T.);
#55340=EDGE_CURVE('',#42104,#41697,#22660,.T.);
#55341=EDGE_CURVE('',#42105,#41696,#22661,.T.);
#55342=EDGE_CURVE('',#41887,#42106,#22662,.T.);
#55343=EDGE_CURVE('',#41886,#42107,#22663,.T.);
#55344=EDGE_CURVE('',#42117,#42118,#30189,.T.);
#55345=EDGE_CURVE('',#42118,#42119,#30190,.T.);
#55346=EDGE_CURVE('',#42119,#42120,#1264,.T.);
#55347=EDGE_CURVE('',#42120,#42121,#30191,.T.);
#55348=EDGE_CURVE('',#42121,#42117,#26212,.T.);
#55349=EDGE_CURVE('',#42122,#42123,#1265,.T.);
#55350=EDGE_CURVE('',#42123,#42124,#30192,.T.);
#55351=EDGE_CURVE('',#42125,#42124,#30193,.T.);
#55352=EDGE_CURVE('',#42125,#42126,#26213,.T.);
#55353=EDGE_CURVE('',#42126,#42122,#30194,.T.);
#55354=EDGE_CURVE('',#42124,#42127,#26214,.T.);
#55355=EDGE_CURVE('',#42127,#42118,#26215,.T.);
#55356=EDGE_CURVE('',#42117,#42128,#1266,.T.);
#55357=EDGE_CURVE('',#42128,#42125,#1267,.T.);
#55358=EDGE_CURVE('',#42126,#41360,#26216,.T.);
#55359=EDGE_CURVE('',#42129,#42125,#22664,.T.);
#55360=EDGE_CURVE('',#41360,#42129,#26217,.T.);
#55361=EDGE_CURVE('',#42130,#42117,#22665,.T.);
#55362=EDGE_CURVE('',#42129,#42130,#26218,.T.);
#55363=EDGE_CURVE('',#41359,#42121,#26219,.T.);
#55364=EDGE_CURVE('',#42130,#41359,#1268,.T.);
#55365=EDGE_CURVE('',#41889,#42126,#22666,.T.);
#55366=EDGE_CURVE('',#42122,#41888,#22667,.T.);
#55367=EDGE_CURVE('',#42123,#41695,#22668,.T.);
#55368=EDGE_CURVE('',#42124,#41694,#22669,.T.);
#55369=EDGE_CURVE('',#42118,#41693,#22670,.T.);
#55370=EDGE_CURVE('',#42119,#41692,#22671,.T.);
#55371=EDGE_CURVE('',#41891,#42120,#22672,.T.);
#55372=EDGE_CURVE('',#41890,#42121,#22673,.T.);
#55373=EDGE_CURVE('',#42131,#42132,#30195,.T.);
#55374=EDGE_CURVE('',#42132,#42133,#30196,.T.);
#55375=EDGE_CURVE('',#42133,#42134,#1269,.T.);
#55376=EDGE_CURVE('',#42134,#42135,#30197,.T.);
#55377=EDGE_CURVE('',#42135,#42131,#26220,.T.);
#55378=EDGE_CURVE('',#42136,#42137,#1270,.T.);
#55379=EDGE_CURVE('',#42137,#42138,#30198,.T.);
#55380=EDGE_CURVE('',#42139,#42138,#30199,.T.);
#55381=EDGE_CURVE('',#42139,#42140,#26221,.T.);
#55382=EDGE_CURVE('',#42140,#42136,#30200,.T.);
#55383=EDGE_CURVE('',#42138,#42141,#26222,.T.);
#55384=EDGE_CURVE('',#42141,#42132,#26223,.T.);
#55385=EDGE_CURVE('',#42131,#42142,#1271,.T.);
#55386=EDGE_CURVE('',#42142,#42139,#1272,.T.);
#55387=EDGE_CURVE('',#42140,#41356,#26224,.T.);
#55388=EDGE_CURVE('',#42143,#42139,#22674,.T.);
#55389=EDGE_CURVE('',#41356,#42143,#26225,.T.);
#55390=EDGE_CURVE('',#42144,#42131,#22675,.T.);
#55391=EDGE_CURVE('',#42143,#42144,#26226,.T.);
#55392=EDGE_CURVE('',#41355,#42135,#26227,.T.);
#55393=EDGE_CURVE('',#42144,#41355,#1273,.T.);
#55394=EDGE_CURVE('',#41893,#42140,#22676,.T.);
#55395=EDGE_CURVE('',#42136,#41892,#22677,.T.);
#55396=EDGE_CURVE('',#42137,#41691,#22678,.T.);
#55397=EDGE_CURVE('',#42138,#41690,#22679,.T.);
#55398=EDGE_CURVE('',#42132,#41689,#22680,.T.);
#55399=EDGE_CURVE('',#42133,#41688,#22681,.T.);
#55400=EDGE_CURVE('',#41895,#42134,#22682,.T.);
#55401=EDGE_CURVE('',#41894,#42135,#22683,.T.);
#55402=EDGE_CURVE('',#42145,#42146,#30201,.T.);
#55403=EDGE_CURVE('',#42146,#42147,#30202,.T.);
#55404=EDGE_CURVE('',#42147,#42148,#1274,.T.);
#55405=EDGE_CURVE('',#42148,#42149,#30203,.T.);
#55406=EDGE_CURVE('',#42149,#42145,#26228,.T.);
#55407=EDGE_CURVE('',#42150,#42151,#1275,.T.);
#55408=EDGE_CURVE('',#42151,#42152,#30204,.T.);
#55409=EDGE_CURVE('',#42153,#42152,#30205,.T.);
#55410=EDGE_CURVE('',#42153,#42154,#26229,.T.);
#55411=EDGE_CURVE('',#42154,#42150,#30206,.T.);
#55412=EDGE_CURVE('',#42152,#42155,#26230,.T.);
#55413=EDGE_CURVE('',#42155,#42146,#26231,.T.);
#55414=EDGE_CURVE('',#42145,#42156,#1276,.T.);
#55415=EDGE_CURVE('',#42156,#42153,#1277,.T.);
#55416=EDGE_CURVE('',#42154,#41352,#26232,.T.);
#55417=EDGE_CURVE('',#42157,#42153,#22684,.T.);
#55418=EDGE_CURVE('',#41352,#42157,#26233,.T.);
#55419=EDGE_CURVE('',#42158,#42145,#22685,.T.);
#55420=EDGE_CURVE('',#42157,#42158,#26234,.T.);
#55421=EDGE_CURVE('',#41351,#42149,#26235,.T.);
#55422=EDGE_CURVE('',#42158,#41351,#1278,.T.);
#55423=EDGE_CURVE('',#41897,#42154,#22686,.T.);
#55424=EDGE_CURVE('',#42150,#41896,#22687,.T.);
#55425=EDGE_CURVE('',#42151,#41687,#22688,.T.);
#55426=EDGE_CURVE('',#42152,#41686,#22689,.T.);
#55427=EDGE_CURVE('',#42146,#41685,#22690,.T.);
#55428=EDGE_CURVE('',#42147,#41684,#22691,.T.);
#55429=EDGE_CURVE('',#41899,#42148,#22692,.T.);
#55430=EDGE_CURVE('',#41898,#42149,#22693,.T.);
#55431=EDGE_CURVE('',#42159,#42160,#30207,.T.);
#55432=EDGE_CURVE('',#42160,#42161,#30208,.T.);
#55433=EDGE_CURVE('',#42161,#42162,#1279,.T.);
#55434=EDGE_CURVE('',#42162,#42163,#30209,.T.);
#55435=EDGE_CURVE('',#42163,#42159,#26236,.T.);
#55436=EDGE_CURVE('',#42164,#42165,#1280,.T.);
#55437=EDGE_CURVE('',#42165,#42166,#30210,.T.);
#55438=EDGE_CURVE('',#42167,#42166,#30211,.T.);
#55439=EDGE_CURVE('',#42167,#42168,#26237,.T.);
#55440=EDGE_CURVE('',#42168,#42164,#30212,.T.);
#55441=EDGE_CURVE('',#42166,#42169,#26238,.T.);
#55442=EDGE_CURVE('',#42169,#42160,#26239,.T.);
#55443=EDGE_CURVE('',#42159,#42170,#1281,.T.);
#55444=EDGE_CURVE('',#42170,#42167,#1282,.T.);
#55445=EDGE_CURVE('',#42168,#41348,#26240,.T.);
#55446=EDGE_CURVE('',#42171,#42167,#22694,.T.);
#55447=EDGE_CURVE('',#41348,#42171,#26241,.T.);
#55448=EDGE_CURVE('',#42172,#42159,#22695,.T.);
#55449=EDGE_CURVE('',#42171,#42172,#26242,.T.);
#55450=EDGE_CURVE('',#41347,#42163,#26243,.T.);
#55451=EDGE_CURVE('',#42172,#41347,#1283,.T.);
#55452=EDGE_CURVE('',#41901,#42168,#22696,.T.);
#55453=EDGE_CURVE('',#42164,#41900,#22697,.T.);
#55454=EDGE_CURVE('',#42165,#41683,#22698,.T.);
#55455=EDGE_CURVE('',#42166,#41682,#22699,.T.);
#55456=EDGE_CURVE('',#42160,#41681,#22700,.T.);
#55457=EDGE_CURVE('',#42161,#41680,#22701,.T.);
#55458=EDGE_CURVE('',#41903,#42162,#22702,.T.);
#55459=EDGE_CURVE('',#41902,#42163,#22703,.T.);
#55460=EDGE_CURVE('',#42173,#42174,#30213,.T.);
#55461=EDGE_CURVE('',#42174,#42175,#30214,.T.);
#55462=EDGE_CURVE('',#42175,#42176,#1284,.T.);
#55463=EDGE_CURVE('',#42176,#42177,#30215,.T.);
#55464=EDGE_CURVE('',#42177,#42173,#26244,.T.);
#55465=EDGE_CURVE('',#42178,#42179,#1285,.T.);
#55466=EDGE_CURVE('',#42179,#42180,#30216,.T.);
#55467=EDGE_CURVE('',#42181,#42180,#30217,.T.);
#55468=EDGE_CURVE('',#42181,#42182,#26245,.T.);
#55469=EDGE_CURVE('',#42182,#42178,#30218,.T.);
#55470=EDGE_CURVE('',#42180,#42183,#26246,.T.);
#55471=EDGE_CURVE('',#42183,#42174,#26247,.T.);
#55472=EDGE_CURVE('',#42173,#42184,#1286,.T.);
#55473=EDGE_CURVE('',#42184,#42181,#1287,.T.);
#55474=EDGE_CURVE('',#42182,#41344,#26248,.T.);
#55475=EDGE_CURVE('',#42185,#42181,#22704,.T.);
#55476=EDGE_CURVE('',#41344,#42185,#26249,.T.);
#55477=EDGE_CURVE('',#42186,#42173,#22705,.T.);
#55478=EDGE_CURVE('',#42185,#42186,#26250,.T.);
#55479=EDGE_CURVE('',#41343,#42177,#26251,.T.);
#55480=EDGE_CURVE('',#42186,#41343,#1288,.T.);
#55481=EDGE_CURVE('',#41905,#42182,#22706,.T.);
#55482=EDGE_CURVE('',#42178,#41904,#22707,.T.);
#55483=EDGE_CURVE('',#42179,#41679,#22708,.T.);
#55484=EDGE_CURVE('',#42180,#41678,#22709,.T.);
#55485=EDGE_CURVE('',#42174,#41677,#22710,.T.);
#55486=EDGE_CURVE('',#42175,#41676,#22711,.T.);
#55487=EDGE_CURVE('',#41907,#42176,#22712,.T.);
#55488=EDGE_CURVE('',#41906,#42177,#22713,.T.);
#55489=EDGE_CURVE('',#42187,#42188,#30219,.T.);
#55490=EDGE_CURVE('',#42188,#42189,#30220,.T.);
#55491=EDGE_CURVE('',#42189,#42190,#1289,.T.);
#55492=EDGE_CURVE('',#42190,#42191,#30221,.T.);
#55493=EDGE_CURVE('',#42191,#42187,#26252,.T.);
#55494=EDGE_CURVE('',#42192,#42193,#1290,.T.);
#55495=EDGE_CURVE('',#42193,#42194,#30222,.T.);
#55496=EDGE_CURVE('',#42195,#42194,#30223,.T.);
#55497=EDGE_CURVE('',#42195,#42196,#26253,.T.);
#55498=EDGE_CURVE('',#42196,#42192,#30224,.T.);
#55499=EDGE_CURVE('',#42194,#42197,#26254,.T.);
#55500=EDGE_CURVE('',#42197,#42188,#26255,.T.);
#55501=EDGE_CURVE('',#42187,#42198,#1291,.T.);
#55502=EDGE_CURVE('',#42198,#42195,#1292,.T.);
#55503=EDGE_CURVE('',#42196,#41340,#26256,.T.);
#55504=EDGE_CURVE('',#42199,#42195,#22714,.T.);
#55505=EDGE_CURVE('',#41340,#42199,#26257,.T.);
#55506=EDGE_CURVE('',#42200,#42187,#22715,.T.);
#55507=EDGE_CURVE('',#42199,#42200,#26258,.T.);
#55508=EDGE_CURVE('',#41339,#42191,#26259,.T.);
#55509=EDGE_CURVE('',#42200,#41339,#1293,.T.);
#55510=EDGE_CURVE('',#41909,#42196,#22716,.T.);
#55511=EDGE_CURVE('',#42192,#41908,#22717,.T.);
#55512=EDGE_CURVE('',#42193,#41675,#22718,.T.);
#55513=EDGE_CURVE('',#42194,#41674,#22719,.T.);
#55514=EDGE_CURVE('',#42188,#41673,#22720,.T.);
#55515=EDGE_CURVE('',#42189,#41672,#22721,.T.);
#55516=EDGE_CURVE('',#41911,#42190,#22722,.T.);
#55517=EDGE_CURVE('',#41910,#42191,#22723,.T.);
#55518=EDGE_CURVE('',#42201,#42202,#30225,.T.);
#55519=EDGE_CURVE('',#42202,#42203,#30226,.T.);
#55520=EDGE_CURVE('',#42203,#42204,#1294,.T.);
#55521=EDGE_CURVE('',#42204,#42205,#30227,.T.);
#55522=EDGE_CURVE('',#42205,#42201,#26260,.T.);
#55523=EDGE_CURVE('',#42206,#42207,#1295,.T.);
#55524=EDGE_CURVE('',#42207,#42208,#30228,.T.);
#55525=EDGE_CURVE('',#42209,#42208,#30229,.T.);
#55526=EDGE_CURVE('',#42209,#42210,#26261,.T.);
#55527=EDGE_CURVE('',#42210,#42206,#30230,.T.);
#55528=EDGE_CURVE('',#42208,#42211,#26262,.T.);
#55529=EDGE_CURVE('',#42211,#42202,#26263,.T.);
#55530=EDGE_CURVE('',#42201,#42212,#1296,.T.);
#55531=EDGE_CURVE('',#42212,#42209,#1297,.T.);
#55532=EDGE_CURVE('',#42210,#41336,#26264,.T.);
#55533=EDGE_CURVE('',#42213,#42209,#22724,.T.);
#55534=EDGE_CURVE('',#41336,#42213,#26265,.T.);
#55535=EDGE_CURVE('',#42214,#42201,#22725,.T.);
#55536=EDGE_CURVE('',#42213,#42214,#26266,.T.);
#55537=EDGE_CURVE('',#41335,#42205,#26267,.T.);
#55538=EDGE_CURVE('',#42214,#41335,#1298,.T.);
#55539=EDGE_CURVE('',#41913,#42210,#22726,.T.);
#55540=EDGE_CURVE('',#42206,#41912,#22727,.T.);
#55541=EDGE_CURVE('',#42207,#41671,#22728,.T.);
#55542=EDGE_CURVE('',#42208,#41670,#22729,.T.);
#55543=EDGE_CURVE('',#42202,#41669,#22730,.T.);
#55544=EDGE_CURVE('',#42203,#41668,#22731,.T.);
#55545=EDGE_CURVE('',#41915,#42204,#22732,.T.);
#55546=EDGE_CURVE('',#41914,#42205,#22733,.T.);
#55547=EDGE_CURVE('',#42215,#42216,#30231,.T.);
#55548=EDGE_CURVE('',#42216,#42217,#30232,.T.);
#55549=EDGE_CURVE('',#42217,#42218,#1299,.T.);
#55550=EDGE_CURVE('',#42218,#42219,#30233,.T.);
#55551=EDGE_CURVE('',#42219,#42215,#26268,.T.);
#55552=EDGE_CURVE('',#42220,#42221,#1300,.T.);
#55553=EDGE_CURVE('',#42221,#42222,#30234,.T.);
#55554=EDGE_CURVE('',#42223,#42222,#30235,.T.);
#55555=EDGE_CURVE('',#42223,#42224,#26269,.T.);
#55556=EDGE_CURVE('',#42224,#42220,#30236,.T.);
#55557=EDGE_CURVE('',#42222,#42225,#26270,.T.);
#55558=EDGE_CURVE('',#42225,#42216,#26271,.T.);
#55559=EDGE_CURVE('',#42215,#42226,#1301,.T.);
#55560=EDGE_CURVE('',#42226,#42223,#1302,.T.);
#55561=EDGE_CURVE('',#42224,#41332,#26272,.T.);
#55562=EDGE_CURVE('',#42227,#42223,#22734,.T.);
#55563=EDGE_CURVE('',#41332,#42227,#26273,.T.);
#55564=EDGE_CURVE('',#42228,#42215,#22735,.T.);
#55565=EDGE_CURVE('',#42227,#42228,#26274,.T.);
#55566=EDGE_CURVE('',#41331,#42219,#26275,.T.);
#55567=EDGE_CURVE('',#42228,#41331,#1303,.T.);
#55568=EDGE_CURVE('',#41861,#42224,#22736,.T.);
#55569=EDGE_CURVE('',#42220,#41860,#22737,.T.);
#55570=EDGE_CURVE('',#42221,#41412,#22738,.T.);
#55571=EDGE_CURVE('',#42222,#41411,#22739,.T.);
#55572=EDGE_CURVE('',#42216,#41410,#22740,.T.);
#55573=EDGE_CURVE('',#42217,#41409,#22741,.T.);
#55574=EDGE_CURVE('',#41863,#42218,#22742,.T.);
#55575=EDGE_CURVE('',#41862,#42219,#22743,.T.);
#55576=EDGE_CURVE('',#42229,#42230,#30237,.T.);
#55577=EDGE_CURVE('',#42230,#42231,#30238,.T.);
#55578=EDGE_CURVE('',#42231,#42232,#1304,.T.);
#55579=EDGE_CURVE('',#42232,#42233,#30239,.T.);
#55580=EDGE_CURVE('',#42233,#42229,#26276,.T.);
#55581=EDGE_CURVE('',#42234,#42235,#1305,.T.);
#55582=EDGE_CURVE('',#42235,#42236,#30240,.T.);
#55583=EDGE_CURVE('',#42237,#42236,#30241,.T.);
#55584=EDGE_CURVE('',#42237,#42238,#26277,.T.);
#55585=EDGE_CURVE('',#42238,#42234,#30242,.T.);
#55586=EDGE_CURVE('',#42236,#42239,#26278,.T.);
#55587=EDGE_CURVE('',#42239,#42230,#26279,.T.);
#55588=EDGE_CURVE('',#42229,#42240,#1306,.T.);
#55589=EDGE_CURVE('',#42240,#42237,#1307,.T.);
#55590=EDGE_CURVE('',#42238,#41328,#26280,.T.);
#55591=EDGE_CURVE('',#42241,#42237,#22744,.T.);
#55592=EDGE_CURVE('',#41328,#42241,#26281,.T.);
#55593=EDGE_CURVE('',#42242,#42229,#22745,.T.);
#55594=EDGE_CURVE('',#42241,#42242,#26282,.T.);
#55595=EDGE_CURVE('',#41327,#42233,#26283,.T.);
#55596=EDGE_CURVE('',#42242,#41327,#1308,.T.);
#55597=EDGE_CURVE('',#41857,#42238,#22746,.T.);
#55598=EDGE_CURVE('',#42234,#41856,#22747,.T.);
#55599=EDGE_CURVE('',#42235,#41416,#22748,.T.);
#55600=EDGE_CURVE('',#42236,#41415,#22749,.T.);
#55601=EDGE_CURVE('',#42230,#41414,#22750,.T.);
#55602=EDGE_CURVE('',#42231,#41413,#22751,.T.);
#55603=EDGE_CURVE('',#41859,#42232,#22752,.T.);
#55604=EDGE_CURVE('',#41858,#42233,#22753,.T.);
#55605=EDGE_CURVE('',#42243,#42244,#30243,.T.);
#55606=EDGE_CURVE('',#42244,#42245,#30244,.T.);
#55607=EDGE_CURVE('',#42245,#42246,#1309,.T.);
#55608=EDGE_CURVE('',#42246,#42247,#30245,.T.);
#55609=EDGE_CURVE('',#42247,#42243,#26284,.T.);
#55610=EDGE_CURVE('',#42248,#42249,#1310,.T.);
#55611=EDGE_CURVE('',#42249,#42250,#30246,.T.);
#55612=EDGE_CURVE('',#42251,#42250,#30247,.T.);
#55613=EDGE_CURVE('',#42251,#42252,#26285,.T.);
#55614=EDGE_CURVE('',#42252,#42248,#30248,.T.);
#55615=EDGE_CURVE('',#42250,#42253,#26286,.T.);
#55616=EDGE_CURVE('',#42253,#42244,#26287,.T.);
#55617=EDGE_CURVE('',#42243,#42254,#1311,.T.);
#55618=EDGE_CURVE('',#42254,#42251,#1312,.T.);
#55619=EDGE_CURVE('',#42252,#41324,#26288,.T.);
#55620=EDGE_CURVE('',#42255,#42251,#22754,.T.);
#55621=EDGE_CURVE('',#41324,#42255,#26289,.T.);
#55622=EDGE_CURVE('',#42256,#42243,#22755,.T.);
#55623=EDGE_CURVE('',#42255,#42256,#26290,.T.);
#55624=EDGE_CURVE('',#41323,#42247,#26291,.T.);
#55625=EDGE_CURVE('',#42256,#41323,#1313,.T.);
#55626=EDGE_CURVE('',#41853,#42252,#22756,.T.);
#55627=EDGE_CURVE('',#42248,#41852,#22757,.T.);
#55628=EDGE_CURVE('',#42249,#41420,#22758,.T.);
#55629=EDGE_CURVE('',#42250,#41419,#22759,.T.);
#55630=EDGE_CURVE('',#42244,#41418,#22760,.T.);
#55631=EDGE_CURVE('',#42245,#41417,#22761,.T.);
#55632=EDGE_CURVE('',#41855,#42246,#22762,.T.);
#55633=EDGE_CURVE('',#41854,#42247,#22763,.T.);
#55634=EDGE_CURVE('',#42257,#42258,#30249,.T.);
#55635=EDGE_CURVE('',#42258,#42259,#30250,.T.);
#55636=EDGE_CURVE('',#42259,#42260,#1314,.T.);
#55637=EDGE_CURVE('',#42260,#42261,#30251,.T.);
#55638=EDGE_CURVE('',#42261,#42257,#26292,.T.);
#55639=EDGE_CURVE('',#42262,#42263,#1315,.T.);
#55640=EDGE_CURVE('',#42263,#42264,#30252,.T.);
#55641=EDGE_CURVE('',#42265,#42264,#30253,.T.);
#55642=EDGE_CURVE('',#42265,#42266,#26293,.T.);
#55643=EDGE_CURVE('',#42266,#42262,#30254,.T.);
#55644=EDGE_CURVE('',#42264,#42267,#26294,.T.);
#55645=EDGE_CURVE('',#42267,#42258,#26295,.T.);
#55646=EDGE_CURVE('',#42257,#42268,#1316,.T.);
#55647=EDGE_CURVE('',#42268,#42265,#1317,.T.);
#55648=EDGE_CURVE('',#42266,#41320,#26296,.T.);
#55649=EDGE_CURVE('',#42269,#42265,#22764,.T.);
#55650=EDGE_CURVE('',#41320,#42269,#26297,.T.);
#55651=EDGE_CURVE('',#42270,#42257,#22765,.T.);
#55652=EDGE_CURVE('',#42269,#42270,#26298,.T.);
#55653=EDGE_CURVE('',#41319,#42261,#26299,.T.);
#55654=EDGE_CURVE('',#42270,#41319,#1318,.T.);
#55655=EDGE_CURVE('',#41849,#42266,#22766,.T.);
#55656=EDGE_CURVE('',#42262,#41848,#22767,.T.);
#55657=EDGE_CURVE('',#42263,#41424,#22768,.T.);
#55658=EDGE_CURVE('',#42264,#41423,#22769,.T.);
#55659=EDGE_CURVE('',#42258,#41422,#22770,.T.);
#55660=EDGE_CURVE('',#42259,#41421,#22771,.T.);
#55661=EDGE_CURVE('',#41851,#42260,#22772,.T.);
#55662=EDGE_CURVE('',#41850,#42261,#22773,.T.);
#55663=EDGE_CURVE('',#42271,#42272,#30255,.T.);
#55664=EDGE_CURVE('',#42272,#42273,#30256,.T.);
#55665=EDGE_CURVE('',#42273,#42274,#1319,.T.);
#55666=EDGE_CURVE('',#42274,#42275,#30257,.T.);
#55667=EDGE_CURVE('',#42275,#42271,#26300,.T.);
#55668=EDGE_CURVE('',#42276,#42277,#1320,.T.);
#55669=EDGE_CURVE('',#42277,#42278,#30258,.T.);
#55670=EDGE_CURVE('',#42279,#42278,#30259,.T.);
#55671=EDGE_CURVE('',#42279,#42280,#26301,.T.);
#55672=EDGE_CURVE('',#42280,#42276,#30260,.T.);
#55673=EDGE_CURVE('',#42278,#42281,#26302,.T.);
#55674=EDGE_CURVE('',#42281,#42272,#26303,.T.);
#55675=EDGE_CURVE('',#42271,#42282,#1321,.T.);
#55676=EDGE_CURVE('',#42282,#42279,#1322,.T.);
#55677=EDGE_CURVE('',#42280,#41316,#26304,.T.);
#55678=EDGE_CURVE('',#42283,#42279,#22774,.T.);
#55679=EDGE_CURVE('',#41316,#42283,#26305,.T.);
#55680=EDGE_CURVE('',#42284,#42271,#22775,.T.);
#55681=EDGE_CURVE('',#42283,#42284,#26306,.T.);
#55682=EDGE_CURVE('',#41315,#42275,#26307,.T.);
#55683=EDGE_CURVE('',#42284,#41315,#1323,.T.);
#55684=EDGE_CURVE('',#41845,#42280,#22776,.T.);
#55685=EDGE_CURVE('',#42276,#41844,#22777,.T.);
#55686=EDGE_CURVE('',#42277,#41428,#22778,.T.);
#55687=EDGE_CURVE('',#42278,#41427,#22779,.T.);
#55688=EDGE_CURVE('',#42272,#41426,#22780,.T.);
#55689=EDGE_CURVE('',#42273,#41425,#22781,.T.);
#55690=EDGE_CURVE('',#41847,#42274,#22782,.T.);
#55691=EDGE_CURVE('',#41846,#42275,#22783,.T.);
#55692=EDGE_CURVE('',#42285,#42286,#30261,.T.);
#55693=EDGE_CURVE('',#42286,#42287,#30262,.T.);
#55694=EDGE_CURVE('',#42287,#42288,#1324,.T.);
#55695=EDGE_CURVE('',#42288,#42289,#30263,.T.);
#55696=EDGE_CURVE('',#42289,#42285,#26308,.T.);
#55697=EDGE_CURVE('',#42290,#42291,#1325,.T.);
#55698=EDGE_CURVE('',#42291,#42292,#30264,.T.);
#55699=EDGE_CURVE('',#42293,#42292,#30265,.T.);
#55700=EDGE_CURVE('',#42293,#42294,#26309,.T.);
#55701=EDGE_CURVE('',#42294,#42290,#30266,.T.);
#55702=EDGE_CURVE('',#42292,#42295,#26310,.T.);
#55703=EDGE_CURVE('',#42295,#42286,#26311,.T.);
#55704=EDGE_CURVE('',#42285,#42296,#1326,.T.);
#55705=EDGE_CURVE('',#42296,#42293,#1327,.T.);
#55706=EDGE_CURVE('',#42294,#41312,#26312,.T.);
#55707=EDGE_CURVE('',#42297,#42293,#22784,.T.);
#55708=EDGE_CURVE('',#41312,#42297,#26313,.T.);
#55709=EDGE_CURVE('',#42298,#42285,#22785,.T.);
#55710=EDGE_CURVE('',#42297,#42298,#26314,.T.);
#55711=EDGE_CURVE('',#41311,#42289,#26315,.T.);
#55712=EDGE_CURVE('',#42298,#41311,#1328,.T.);
#55713=EDGE_CURVE('',#41841,#42294,#22786,.T.);
#55714=EDGE_CURVE('',#42290,#41840,#22787,.T.);
#55715=EDGE_CURVE('',#42291,#41432,#22788,.T.);
#55716=EDGE_CURVE('',#42292,#41431,#22789,.T.);
#55717=EDGE_CURVE('',#42286,#41430,#22790,.T.);
#55718=EDGE_CURVE('',#42287,#41429,#22791,.T.);
#55719=EDGE_CURVE('',#41843,#42288,#22792,.T.);
#55720=EDGE_CURVE('',#41842,#42289,#22793,.T.);
#55721=EDGE_CURVE('',#42299,#42300,#30267,.T.);
#55722=EDGE_CURVE('',#42300,#42301,#30268,.T.);
#55723=EDGE_CURVE('',#42301,#42302,#1329,.T.);
#55724=EDGE_CURVE('',#42302,#42303,#30269,.T.);
#55725=EDGE_CURVE('',#42303,#42299,#26316,.T.);
#55726=EDGE_CURVE('',#42304,#42305,#1330,.T.);
#55727=EDGE_CURVE('',#42305,#42306,#30270,.T.);
#55728=EDGE_CURVE('',#42307,#42306,#30271,.T.);
#55729=EDGE_CURVE('',#42307,#42308,#26317,.T.);
#55730=EDGE_CURVE('',#42308,#42304,#30272,.T.);
#55731=EDGE_CURVE('',#42306,#42309,#26318,.T.);
#55732=EDGE_CURVE('',#42309,#42300,#26319,.T.);
#55733=EDGE_CURVE('',#42299,#42310,#1331,.T.);
#55734=EDGE_CURVE('',#42310,#42307,#1332,.T.);
#55735=EDGE_CURVE('',#42308,#41308,#26320,.T.);
#55736=EDGE_CURVE('',#42311,#42307,#22794,.T.);
#55737=EDGE_CURVE('',#41308,#42311,#26321,.T.);
#55738=EDGE_CURVE('',#42312,#42299,#22795,.T.);
#55739=EDGE_CURVE('',#42311,#42312,#26322,.T.);
#55740=EDGE_CURVE('',#41307,#42303,#26323,.T.);
#55741=EDGE_CURVE('',#42312,#41307,#1333,.T.);
#55742=EDGE_CURVE('',#41837,#42308,#22796,.T.);
#55743=EDGE_CURVE('',#42304,#41836,#22797,.T.);
#55744=EDGE_CURVE('',#42305,#41436,#22798,.T.);
#55745=EDGE_CURVE('',#42306,#41435,#22799,.T.);
#55746=EDGE_CURVE('',#42300,#41434,#22800,.T.);
#55747=EDGE_CURVE('',#42301,#41433,#22801,.T.);
#55748=EDGE_CURVE('',#41839,#42302,#22802,.T.);
#55749=EDGE_CURVE('',#41838,#42303,#22803,.T.);
#55750=EDGE_CURVE('',#42313,#42314,#30273,.T.);
#55751=EDGE_CURVE('',#42314,#42315,#30274,.T.);
#55752=EDGE_CURVE('',#42315,#42316,#1334,.T.);
#55753=EDGE_CURVE('',#42316,#42317,#30275,.T.);
#55754=EDGE_CURVE('',#42317,#42313,#26324,.T.);
#55755=EDGE_CURVE('',#42318,#42319,#1335,.T.);
#55756=EDGE_CURVE('',#42319,#42320,#30276,.T.);
#55757=EDGE_CURVE('',#42321,#42320,#30277,.T.);
#55758=EDGE_CURVE('',#42321,#42322,#26325,.T.);
#55759=EDGE_CURVE('',#42322,#42318,#30278,.T.);
#55760=EDGE_CURVE('',#42320,#42323,#26326,.T.);
#55761=EDGE_CURVE('',#42323,#42314,#26327,.T.);
#55762=EDGE_CURVE('',#42313,#42324,#1336,.T.);
#55763=EDGE_CURVE('',#42324,#42321,#1337,.T.);
#55764=EDGE_CURVE('',#42322,#41304,#26328,.T.);
#55765=EDGE_CURVE('',#42325,#42321,#22804,.T.);
#55766=EDGE_CURVE('',#41304,#42325,#26329,.T.);
#55767=EDGE_CURVE('',#42326,#42313,#22805,.T.);
#55768=EDGE_CURVE('',#42325,#42326,#26330,.T.);
#55769=EDGE_CURVE('',#41303,#42317,#26331,.T.);
#55770=EDGE_CURVE('',#42326,#41303,#1338,.T.);
#55771=EDGE_CURVE('',#41833,#42322,#22806,.T.);
#55772=EDGE_CURVE('',#42318,#41832,#22807,.T.);
#55773=EDGE_CURVE('',#42319,#41440,#22808,.T.);
#55774=EDGE_CURVE('',#42320,#41439,#22809,.T.);
#55775=EDGE_CURVE('',#42314,#41438,#22810,.T.);
#55776=EDGE_CURVE('',#42315,#41437,#22811,.T.);
#55777=EDGE_CURVE('',#41835,#42316,#22812,.T.);
#55778=EDGE_CURVE('',#41834,#42317,#22813,.T.);
#55779=EDGE_CURVE('',#42327,#42328,#30279,.T.);
#55780=EDGE_CURVE('',#42328,#42329,#30280,.T.);
#55781=EDGE_CURVE('',#42329,#42330,#1339,.T.);
#55782=EDGE_CURVE('',#42330,#42331,#30281,.T.);
#55783=EDGE_CURVE('',#42331,#42327,#26332,.T.);
#55784=EDGE_CURVE('',#42332,#42333,#1340,.T.);
#55785=EDGE_CURVE('',#42333,#42334,#30282,.T.);
#55786=EDGE_CURVE('',#42335,#42334,#30283,.T.);
#55787=EDGE_CURVE('',#42335,#42336,#26333,.T.);
#55788=EDGE_CURVE('',#42336,#42332,#30284,.T.);
#55789=EDGE_CURVE('',#42334,#42337,#26334,.T.);
#55790=EDGE_CURVE('',#42337,#42328,#26335,.T.);
#55791=EDGE_CURVE('',#42327,#42338,#1341,.T.);
#55792=EDGE_CURVE('',#42338,#42335,#1342,.T.);
#55793=EDGE_CURVE('',#42336,#41300,#26336,.T.);
#55794=EDGE_CURVE('',#42339,#42335,#22814,.T.);
#55795=EDGE_CURVE('',#41300,#42339,#26337,.T.);
#55796=EDGE_CURVE('',#42340,#42327,#22815,.T.);
#55797=EDGE_CURVE('',#42339,#42340,#26338,.T.);
#55798=EDGE_CURVE('',#41299,#42331,#26339,.T.);
#55799=EDGE_CURVE('',#42340,#41299,#1343,.T.);
#55800=EDGE_CURVE('',#41829,#42336,#22816,.T.);
#55801=EDGE_CURVE('',#42332,#41828,#22817,.T.);
#55802=EDGE_CURVE('',#42333,#41444,#22818,.T.);
#55803=EDGE_CURVE('',#42334,#41443,#22819,.T.);
#55804=EDGE_CURVE('',#42328,#41442,#22820,.T.);
#55805=EDGE_CURVE('',#42329,#41441,#22821,.T.);
#55806=EDGE_CURVE('',#41831,#42330,#22822,.T.);
#55807=EDGE_CURVE('',#41830,#42331,#22823,.T.);
#55808=EDGE_CURVE('',#42341,#42342,#30285,.T.);
#55809=EDGE_CURVE('',#42342,#42343,#30286,.T.);
#55810=EDGE_CURVE('',#42343,#42344,#1344,.T.);
#55811=EDGE_CURVE('',#42344,#42345,#30287,.T.);
#55812=EDGE_CURVE('',#42345,#42341,#26340,.T.);
#55813=EDGE_CURVE('',#42346,#42347,#1345,.T.);
#55814=EDGE_CURVE('',#42347,#42348,#30288,.T.);
#55815=EDGE_CURVE('',#42349,#42348,#30289,.T.);
#55816=EDGE_CURVE('',#42349,#42350,#26341,.T.);
#55817=EDGE_CURVE('',#42350,#42346,#30290,.T.);
#55818=EDGE_CURVE('',#42348,#42351,#26342,.T.);
#55819=EDGE_CURVE('',#42351,#42342,#26343,.T.);
#55820=EDGE_CURVE('',#42341,#42352,#1346,.T.);
#55821=EDGE_CURVE('',#42352,#42349,#1347,.T.);
#55822=EDGE_CURVE('',#42350,#41296,#26344,.T.);
#55823=EDGE_CURVE('',#42353,#42349,#22824,.T.);
#55824=EDGE_CURVE('',#41296,#42353,#26345,.T.);
#55825=EDGE_CURVE('',#42354,#42341,#22825,.T.);
#55826=EDGE_CURVE('',#42353,#42354,#26346,.T.);
#55827=EDGE_CURVE('',#41295,#42345,#26347,.T.);
#55828=EDGE_CURVE('',#42354,#41295,#1348,.T.);
#55829=EDGE_CURVE('',#41825,#42350,#22826,.T.);
#55830=EDGE_CURVE('',#42346,#41824,#22827,.T.);
#55831=EDGE_CURVE('',#42347,#41448,#22828,.T.);
#55832=EDGE_CURVE('',#42348,#41447,#22829,.T.);
#55833=EDGE_CURVE('',#42342,#41446,#22830,.T.);
#55834=EDGE_CURVE('',#42343,#41445,#22831,.T.);
#55835=EDGE_CURVE('',#41827,#42344,#22832,.T.);
#55836=EDGE_CURVE('',#41826,#42345,#22833,.T.);
#55837=EDGE_CURVE('',#42355,#42356,#30291,.T.);
#55838=EDGE_CURVE('',#42356,#42357,#30292,.T.);
#55839=EDGE_CURVE('',#42357,#42358,#1349,.T.);
#55840=EDGE_CURVE('',#42358,#42359,#30293,.T.);
#55841=EDGE_CURVE('',#42359,#42355,#26348,.T.);
#55842=EDGE_CURVE('',#42360,#42361,#1350,.T.);
#55843=EDGE_CURVE('',#42361,#42362,#30294,.T.);
#55844=EDGE_CURVE('',#42363,#42362,#30295,.T.);
#55845=EDGE_CURVE('',#42363,#42364,#26349,.T.);
#55846=EDGE_CURVE('',#42364,#42360,#30296,.T.);
#55847=EDGE_CURVE('',#42362,#42365,#26350,.T.);
#55848=EDGE_CURVE('',#42365,#42356,#26351,.T.);
#55849=EDGE_CURVE('',#42355,#42366,#1351,.T.);
#55850=EDGE_CURVE('',#42366,#42363,#1352,.T.);
#55851=EDGE_CURVE('',#42364,#41292,#26352,.T.);
#55852=EDGE_CURVE('',#42367,#42363,#22834,.T.);
#55853=EDGE_CURVE('',#41292,#42367,#26353,.T.);
#55854=EDGE_CURVE('',#42368,#42355,#22835,.T.);
#55855=EDGE_CURVE('',#42367,#42368,#26354,.T.);
#55856=EDGE_CURVE('',#41291,#42359,#26355,.T.);
#55857=EDGE_CURVE('',#42368,#41291,#1353,.T.);
#55858=EDGE_CURVE('',#41821,#42364,#22836,.T.);
#55859=EDGE_CURVE('',#42360,#41820,#22837,.T.);
#55860=EDGE_CURVE('',#42361,#41452,#22838,.T.);
#55861=EDGE_CURVE('',#42362,#41451,#22839,.T.);
#55862=EDGE_CURVE('',#42356,#41450,#22840,.T.);
#55863=EDGE_CURVE('',#42357,#41449,#22841,.T.);
#55864=EDGE_CURVE('',#41823,#42358,#22842,.T.);
#55865=EDGE_CURVE('',#41822,#42359,#22843,.T.);
#55866=EDGE_CURVE('',#42369,#42370,#30297,.T.);
#55867=EDGE_CURVE('',#42370,#42371,#30298,.T.);
#55868=EDGE_CURVE('',#42371,#42372,#1354,.T.);
#55869=EDGE_CURVE('',#42372,#42373,#30299,.T.);
#55870=EDGE_CURVE('',#42373,#42369,#26356,.T.);
#55871=EDGE_CURVE('',#42374,#42375,#1355,.T.);
#55872=EDGE_CURVE('',#42375,#42376,#30300,.T.);
#55873=EDGE_CURVE('',#42377,#42376,#30301,.T.);
#55874=EDGE_CURVE('',#42377,#42378,#26357,.T.);
#55875=EDGE_CURVE('',#42378,#42374,#30302,.T.);
#55876=EDGE_CURVE('',#42376,#42379,#26358,.T.);
#55877=EDGE_CURVE('',#42379,#42370,#26359,.T.);
#55878=EDGE_CURVE('',#42369,#42380,#1356,.T.);
#55879=EDGE_CURVE('',#42380,#42377,#1357,.T.);
#55880=EDGE_CURVE('',#42378,#41288,#26360,.T.);
#55881=EDGE_CURVE('',#42381,#42377,#22844,.T.);
#55882=EDGE_CURVE('',#41288,#42381,#26361,.T.);
#55883=EDGE_CURVE('',#42382,#42369,#22845,.T.);
#55884=EDGE_CURVE('',#42381,#42382,#26362,.T.);
#55885=EDGE_CURVE('',#41287,#42373,#26363,.T.);
#55886=EDGE_CURVE('',#42382,#41287,#1358,.T.);
#55887=EDGE_CURVE('',#41817,#42378,#22846,.T.);
#55888=EDGE_CURVE('',#42374,#41816,#22847,.T.);
#55889=EDGE_CURVE('',#42375,#41456,#22848,.T.);
#55890=EDGE_CURVE('',#42376,#41455,#22849,.T.);
#55891=EDGE_CURVE('',#42370,#41454,#22850,.T.);
#55892=EDGE_CURVE('',#42371,#41453,#22851,.T.);
#55893=EDGE_CURVE('',#41819,#42372,#22852,.T.);
#55894=EDGE_CURVE('',#41818,#42373,#22853,.T.);
#55895=EDGE_CURVE('',#42383,#42384,#30303,.T.);
#55896=EDGE_CURVE('',#42384,#42385,#30304,.T.);
#55897=EDGE_CURVE('',#42385,#42386,#1359,.T.);
#55898=EDGE_CURVE('',#42386,#42387,#30305,.T.);
#55899=EDGE_CURVE('',#42387,#42383,#26364,.T.);
#55900=EDGE_CURVE('',#42388,#42389,#1360,.T.);
#55901=EDGE_CURVE('',#42389,#42390,#30306,.T.);
#55902=EDGE_CURVE('',#42391,#42390,#30307,.T.);
#55903=EDGE_CURVE('',#42391,#42392,#26365,.T.);
#55904=EDGE_CURVE('',#42392,#42388,#30308,.T.);
#55905=EDGE_CURVE('',#42390,#42393,#26366,.T.);
#55906=EDGE_CURVE('',#42393,#42384,#26367,.T.);
#55907=EDGE_CURVE('',#42383,#42394,#1361,.T.);
#55908=EDGE_CURVE('',#42394,#42391,#1362,.T.);
#55909=EDGE_CURVE('',#42392,#41284,#26368,.T.);
#55910=EDGE_CURVE('',#42395,#42391,#22854,.T.);
#55911=EDGE_CURVE('',#41284,#42395,#26369,.T.);
#55912=EDGE_CURVE('',#42396,#42383,#22855,.T.);
#55913=EDGE_CURVE('',#42395,#42396,#26370,.T.);
#55914=EDGE_CURVE('',#41283,#42387,#26371,.T.);
#55915=EDGE_CURVE('',#42396,#41283,#1363,.T.);
#55916=EDGE_CURVE('',#41813,#42392,#22856,.T.);
#55917=EDGE_CURVE('',#42388,#41812,#22857,.T.);
#55918=EDGE_CURVE('',#42389,#41460,#22858,.T.);
#55919=EDGE_CURVE('',#42390,#41459,#22859,.T.);
#55920=EDGE_CURVE('',#42384,#41458,#22860,.T.);
#55921=EDGE_CURVE('',#42385,#41457,#22861,.T.);
#55922=EDGE_CURVE('',#41815,#42386,#22862,.T.);
#55923=EDGE_CURVE('',#41814,#42387,#22863,.T.);
#55924=EDGE_CURVE('',#42397,#42398,#30309,.T.);
#55925=EDGE_CURVE('',#42398,#42399,#30310,.T.);
#55926=EDGE_CURVE('',#42399,#42400,#1364,.T.);
#55927=EDGE_CURVE('',#42400,#42401,#30311,.T.);
#55928=EDGE_CURVE('',#42401,#42397,#26372,.T.);
#55929=EDGE_CURVE('',#42402,#42403,#1365,.T.);
#55930=EDGE_CURVE('',#42403,#42404,#30312,.T.);
#55931=EDGE_CURVE('',#42405,#42404,#30313,.T.);
#55932=EDGE_CURVE('',#42405,#42406,#26373,.T.);
#55933=EDGE_CURVE('',#42406,#42402,#30314,.T.);
#55934=EDGE_CURVE('',#42404,#42407,#26374,.T.);
#55935=EDGE_CURVE('',#42407,#42398,#26375,.T.);
#55936=EDGE_CURVE('',#42397,#42408,#1366,.T.);
#55937=EDGE_CURVE('',#42408,#42405,#1367,.T.);
#55938=EDGE_CURVE('',#42406,#41280,#26376,.T.);
#55939=EDGE_CURVE('',#42409,#42405,#22864,.T.);
#55940=EDGE_CURVE('',#41280,#42409,#26377,.T.);
#55941=EDGE_CURVE('',#42410,#42397,#22865,.T.);
#55942=EDGE_CURVE('',#42409,#42410,#26378,.T.);
#55943=EDGE_CURVE('',#41279,#42401,#26379,.T.);
#55944=EDGE_CURVE('',#42410,#41279,#1368,.T.);
#55945=EDGE_CURVE('',#41809,#42406,#22866,.T.);
#55946=EDGE_CURVE('',#42402,#41808,#22867,.T.);
#55947=EDGE_CURVE('',#42403,#41464,#22868,.T.);
#55948=EDGE_CURVE('',#42404,#41463,#22869,.T.);
#55949=EDGE_CURVE('',#42398,#41462,#22870,.T.);
#55950=EDGE_CURVE('',#42399,#41461,#22871,.T.);
#55951=EDGE_CURVE('',#41811,#42400,#22872,.T.);
#55952=EDGE_CURVE('',#41810,#42401,#22873,.T.);
#55953=EDGE_CURVE('',#42411,#42412,#30315,.T.);
#55954=EDGE_CURVE('',#42412,#42413,#30316,.T.);
#55955=EDGE_CURVE('',#42413,#42414,#1369,.T.);
#55956=EDGE_CURVE('',#42414,#42415,#30317,.T.);
#55957=EDGE_CURVE('',#42415,#42411,#26380,.T.);
#55958=EDGE_CURVE('',#42416,#42417,#1370,.T.);
#55959=EDGE_CURVE('',#42417,#42418,#30318,.T.);
#55960=EDGE_CURVE('',#42419,#42418,#30319,.T.);
#55961=EDGE_CURVE('',#42419,#42420,#26381,.T.);
#55962=EDGE_CURVE('',#42420,#42416,#30320,.T.);
#55963=EDGE_CURVE('',#42418,#42421,#26382,.T.);
#55964=EDGE_CURVE('',#42421,#42412,#26383,.T.);
#55965=EDGE_CURVE('',#42411,#42422,#1371,.T.);
#55966=EDGE_CURVE('',#42422,#42419,#1372,.T.);
#55967=EDGE_CURVE('',#42420,#41276,#26384,.T.);
#55968=EDGE_CURVE('',#42423,#42419,#22874,.T.);
#55969=EDGE_CURVE('',#41276,#42423,#26385,.T.);
#55970=EDGE_CURVE('',#42424,#42411,#22875,.T.);
#55971=EDGE_CURVE('',#42423,#42424,#26386,.T.);
#55972=EDGE_CURVE('',#41275,#42415,#26387,.T.);
#55973=EDGE_CURVE('',#42424,#41275,#1373,.T.);
#55974=EDGE_CURVE('',#41805,#42420,#22876,.T.);
#55975=EDGE_CURVE('',#42416,#41804,#22877,.T.);
#55976=EDGE_CURVE('',#42417,#41468,#22878,.T.);
#55977=EDGE_CURVE('',#42418,#41467,#22879,.T.);
#55978=EDGE_CURVE('',#42412,#41466,#22880,.T.);
#55979=EDGE_CURVE('',#42413,#41465,#22881,.T.);
#55980=EDGE_CURVE('',#41807,#42414,#22882,.T.);
#55981=EDGE_CURVE('',#41806,#42415,#22883,.T.);
#55982=EDGE_CURVE('',#42425,#42426,#30321,.T.);
#55983=EDGE_CURVE('',#42426,#42427,#30322,.T.);
#55984=EDGE_CURVE('',#42427,#42428,#1374,.T.);
#55985=EDGE_CURVE('',#42428,#42429,#30323,.T.);
#55986=EDGE_CURVE('',#42429,#42425,#26388,.T.);
#55987=EDGE_CURVE('',#42430,#42431,#1375,.T.);
#55988=EDGE_CURVE('',#42431,#42432,#30324,.T.);
#55989=EDGE_CURVE('',#42433,#42432,#30325,.T.);
#55990=EDGE_CURVE('',#42433,#42434,#26389,.T.);
#55991=EDGE_CURVE('',#42434,#42430,#30326,.T.);
#55992=EDGE_CURVE('',#42432,#42435,#26390,.T.);
#55993=EDGE_CURVE('',#42435,#42426,#26391,.T.);
#55994=EDGE_CURVE('',#42425,#42436,#1376,.T.);
#55995=EDGE_CURVE('',#42436,#42433,#1377,.T.);
#55996=EDGE_CURVE('',#42434,#41272,#26392,.T.);
#55997=EDGE_CURVE('',#42437,#42433,#22884,.T.);
#55998=EDGE_CURVE('',#41272,#42437,#26393,.T.);
#55999=EDGE_CURVE('',#42438,#42425,#22885,.T.);
#56000=EDGE_CURVE('',#42437,#42438,#26394,.T.);
#56001=EDGE_CURVE('',#41271,#42429,#26395,.T.);
#56002=EDGE_CURVE('',#42438,#41271,#1378,.T.);
#56003=EDGE_CURVE('',#41801,#42434,#22886,.T.);
#56004=EDGE_CURVE('',#42430,#41800,#22887,.T.);
#56005=EDGE_CURVE('',#42431,#41472,#22888,.T.);
#56006=EDGE_CURVE('',#42432,#41471,#22889,.T.);
#56007=EDGE_CURVE('',#42426,#41470,#22890,.T.);
#56008=EDGE_CURVE('',#42427,#41469,#22891,.T.);
#56009=EDGE_CURVE('',#41803,#42428,#22892,.T.);
#56010=EDGE_CURVE('',#41802,#42429,#22893,.T.);
#56011=EDGE_CURVE('',#42439,#42440,#30327,.T.);
#56012=EDGE_CURVE('',#42440,#42441,#30328,.T.);
#56013=EDGE_CURVE('',#42441,#42442,#1379,.T.);
#56014=EDGE_CURVE('',#42442,#42443,#30329,.T.);
#56015=EDGE_CURVE('',#42443,#42439,#26396,.T.);
#56016=EDGE_CURVE('',#42444,#42445,#1380,.T.);
#56017=EDGE_CURVE('',#42445,#42446,#30330,.T.);
#56018=EDGE_CURVE('',#42447,#42446,#30331,.T.);
#56019=EDGE_CURVE('',#42447,#42448,#26397,.T.);
#56020=EDGE_CURVE('',#42448,#42444,#30332,.T.);
#56021=EDGE_CURVE('',#42446,#42449,#26398,.T.);
#56022=EDGE_CURVE('',#42449,#42440,#26399,.T.);
#56023=EDGE_CURVE('',#42439,#42450,#1381,.T.);
#56024=EDGE_CURVE('',#42450,#42447,#1382,.T.);
#56025=EDGE_CURVE('',#42448,#41268,#26400,.T.);
#56026=EDGE_CURVE('',#42451,#42447,#22894,.T.);
#56027=EDGE_CURVE('',#41268,#42451,#26401,.T.);
#56028=EDGE_CURVE('',#42452,#42439,#22895,.T.);
#56029=EDGE_CURVE('',#42451,#42452,#26402,.T.);
#56030=EDGE_CURVE('',#41267,#42443,#26403,.T.);
#56031=EDGE_CURVE('',#42452,#41267,#1383,.T.);
#56032=EDGE_CURVE('',#41797,#42448,#22896,.T.);
#56033=EDGE_CURVE('',#42444,#41796,#22897,.T.);
#56034=EDGE_CURVE('',#42445,#41476,#22898,.T.);
#56035=EDGE_CURVE('',#42446,#41475,#22899,.T.);
#56036=EDGE_CURVE('',#42440,#41474,#22900,.T.);
#56037=EDGE_CURVE('',#42441,#41473,#22901,.T.);
#56038=EDGE_CURVE('',#41799,#42442,#22902,.T.);
#56039=EDGE_CURVE('',#41798,#42443,#22903,.T.);
#56040=EDGE_CURVE('',#42453,#42454,#30333,.T.);
#56041=EDGE_CURVE('',#42454,#42455,#30334,.T.);
#56042=EDGE_CURVE('',#42455,#42456,#1384,.T.);
#56043=EDGE_CURVE('',#42456,#42457,#30335,.T.);
#56044=EDGE_CURVE('',#42457,#42453,#26404,.T.);
#56045=EDGE_CURVE('',#42458,#42459,#1385,.T.);
#56046=EDGE_CURVE('',#42459,#42460,#30336,.T.);
#56047=EDGE_CURVE('',#42461,#42460,#30337,.T.);
#56048=EDGE_CURVE('',#42461,#42462,#26405,.T.);
#56049=EDGE_CURVE('',#42462,#42458,#30338,.T.);
#56050=EDGE_CURVE('',#42460,#42463,#26406,.T.);
#56051=EDGE_CURVE('',#42463,#42454,#26407,.T.);
#56052=EDGE_CURVE('',#42453,#42464,#1386,.T.);
#56053=EDGE_CURVE('',#42464,#42461,#1387,.T.);
#56054=EDGE_CURVE('',#42462,#41264,#26408,.T.);
#56055=EDGE_CURVE('',#42465,#42461,#22904,.T.);
#56056=EDGE_CURVE('',#41264,#42465,#26409,.T.);
#56057=EDGE_CURVE('',#42466,#42453,#22905,.T.);
#56058=EDGE_CURVE('',#42465,#42466,#26410,.T.);
#56059=EDGE_CURVE('',#41263,#42457,#26411,.T.);
#56060=EDGE_CURVE('',#42466,#41263,#1388,.T.);
#56061=EDGE_CURVE('',#41793,#42462,#22906,.T.);
#56062=EDGE_CURVE('',#42458,#41792,#22907,.T.);
#56063=EDGE_CURVE('',#42459,#41480,#22908,.T.);
#56064=EDGE_CURVE('',#42460,#41479,#22909,.T.);
#56065=EDGE_CURVE('',#42454,#41478,#22910,.T.);
#56066=EDGE_CURVE('',#42455,#41477,#22911,.T.);
#56067=EDGE_CURVE('',#41795,#42456,#22912,.T.);
#56068=EDGE_CURVE('',#41794,#42457,#22913,.T.);
#56069=EDGE_CURVE('',#42467,#42468,#30339,.T.);
#56070=EDGE_CURVE('',#42468,#42469,#30340,.T.);
#56071=EDGE_CURVE('',#42469,#42470,#1389,.T.);
#56072=EDGE_CURVE('',#42470,#42471,#30341,.T.);
#56073=EDGE_CURVE('',#42471,#42467,#26412,.T.);
#56074=EDGE_CURVE('',#42472,#42473,#1390,.T.);
#56075=EDGE_CURVE('',#42473,#42474,#30342,.T.);
#56076=EDGE_CURVE('',#42475,#42474,#30343,.T.);
#56077=EDGE_CURVE('',#42475,#42476,#26413,.T.);
#56078=EDGE_CURVE('',#42476,#42472,#30344,.T.);
#56079=EDGE_CURVE('',#42474,#42477,#26414,.T.);
#56080=EDGE_CURVE('',#42477,#42468,#26415,.T.);
#56081=EDGE_CURVE('',#42467,#42478,#1391,.T.);
#56082=EDGE_CURVE('',#42478,#42475,#1392,.T.);
#56083=EDGE_CURVE('',#42476,#41260,#26416,.T.);
#56084=EDGE_CURVE('',#42479,#42475,#22914,.T.);
#56085=EDGE_CURVE('',#41260,#42479,#26417,.T.);
#56086=EDGE_CURVE('',#42480,#42467,#22915,.T.);
#56087=EDGE_CURVE('',#42479,#42480,#26418,.T.);
#56088=EDGE_CURVE('',#41259,#42471,#26419,.T.);
#56089=EDGE_CURVE('',#42480,#41259,#1393,.T.);
#56090=EDGE_CURVE('',#41789,#42476,#22916,.T.);
#56091=EDGE_CURVE('',#42472,#41788,#22917,.T.);
#56092=EDGE_CURVE('',#42473,#41484,#22918,.T.);
#56093=EDGE_CURVE('',#42474,#41483,#22919,.T.);
#56094=EDGE_CURVE('',#42468,#41482,#22920,.T.);
#56095=EDGE_CURVE('',#42469,#41481,#22921,.T.);
#56096=EDGE_CURVE('',#41791,#42470,#22922,.T.);
#56097=EDGE_CURVE('',#41790,#42471,#22923,.T.);
#56098=EDGE_CURVE('',#42481,#42482,#30345,.T.);
#56099=EDGE_CURVE('',#42482,#42483,#30346,.T.);
#56100=EDGE_CURVE('',#42483,#42484,#1394,.T.);
#56101=EDGE_CURVE('',#42484,#42485,#30347,.T.);
#56102=EDGE_CURVE('',#42485,#42481,#26420,.T.);
#56103=EDGE_CURVE('',#42486,#42487,#1395,.T.);
#56104=EDGE_CURVE('',#42487,#42488,#30348,.T.);
#56105=EDGE_CURVE('',#42489,#42488,#30349,.T.);
#56106=EDGE_CURVE('',#42489,#42490,#26421,.T.);
#56107=EDGE_CURVE('',#42490,#42486,#30350,.T.);
#56108=EDGE_CURVE('',#42488,#42491,#26422,.T.);
#56109=EDGE_CURVE('',#42491,#42482,#26423,.T.);
#56110=EDGE_CURVE('',#42481,#42492,#1396,.T.);
#56111=EDGE_CURVE('',#42492,#42489,#1397,.T.);
#56112=EDGE_CURVE('',#42490,#41256,#26424,.T.);
#56113=EDGE_CURVE('',#42493,#42489,#22924,.T.);
#56114=EDGE_CURVE('',#41256,#42493,#26425,.T.);
#56115=EDGE_CURVE('',#42494,#42481,#22925,.T.);
#56116=EDGE_CURVE('',#42493,#42494,#26426,.T.);
#56117=EDGE_CURVE('',#41255,#42485,#26427,.T.);
#56118=EDGE_CURVE('',#42494,#41255,#1398,.T.);
#56119=EDGE_CURVE('',#41785,#42490,#22926,.T.);
#56120=EDGE_CURVE('',#42486,#41784,#22927,.T.);
#56121=EDGE_CURVE('',#42487,#41488,#22928,.T.);
#56122=EDGE_CURVE('',#42488,#41487,#22929,.T.);
#56123=EDGE_CURVE('',#42482,#41486,#22930,.T.);
#56124=EDGE_CURVE('',#42483,#41485,#22931,.T.);
#56125=EDGE_CURVE('',#41787,#42484,#22932,.T.);
#56126=EDGE_CURVE('',#41786,#42485,#22933,.T.);
#56127=EDGE_CURVE('',#42495,#42496,#30351,.T.);
#56128=EDGE_CURVE('',#42496,#42497,#30352,.T.);
#56129=EDGE_CURVE('',#42497,#42498,#1399,.T.);
#56130=EDGE_CURVE('',#42498,#42499,#30353,.T.);
#56131=EDGE_CURVE('',#42499,#42495,#26428,.T.);
#56132=EDGE_CURVE('',#42500,#42501,#1400,.T.);
#56133=EDGE_CURVE('',#42501,#42502,#30354,.T.);
#56134=EDGE_CURVE('',#42503,#42502,#30355,.T.);
#56135=EDGE_CURVE('',#42503,#42504,#26429,.T.);
#56136=EDGE_CURVE('',#42504,#42500,#30356,.T.);
#56137=EDGE_CURVE('',#42502,#42505,#26430,.T.);
#56138=EDGE_CURVE('',#42505,#42496,#26431,.T.);
#56139=EDGE_CURVE('',#42495,#42506,#1401,.T.);
#56140=EDGE_CURVE('',#42506,#42503,#1402,.T.);
#56141=EDGE_CURVE('',#42504,#41252,#26432,.T.);
#56142=EDGE_CURVE('',#42507,#42503,#22934,.T.);
#56143=EDGE_CURVE('',#41252,#42507,#26433,.T.);
#56144=EDGE_CURVE('',#42508,#42495,#22935,.T.);
#56145=EDGE_CURVE('',#42507,#42508,#26434,.T.);
#56146=EDGE_CURVE('',#41251,#42499,#26435,.T.);
#56147=EDGE_CURVE('',#42508,#41251,#1403,.T.);
#56148=EDGE_CURVE('',#41781,#42504,#22936,.T.);
#56149=EDGE_CURVE('',#42500,#41780,#22937,.T.);
#56150=EDGE_CURVE('',#42501,#41492,#22938,.T.);
#56151=EDGE_CURVE('',#42502,#41491,#22939,.T.);
#56152=EDGE_CURVE('',#42496,#41490,#22940,.T.);
#56153=EDGE_CURVE('',#42497,#41489,#22941,.T.);
#56154=EDGE_CURVE('',#41783,#42498,#22942,.T.);
#56155=EDGE_CURVE('',#41782,#42499,#22943,.T.);
#56156=EDGE_CURVE('',#42509,#42510,#30357,.T.);
#56157=EDGE_CURVE('',#42510,#42511,#30358,.T.);
#56158=EDGE_CURVE('',#42511,#42512,#1404,.T.);
#56159=EDGE_CURVE('',#42512,#42513,#30359,.T.);
#56160=EDGE_CURVE('',#42513,#42509,#26436,.T.);
#56161=EDGE_CURVE('',#42514,#42515,#1405,.T.);
#56162=EDGE_CURVE('',#42515,#42516,#30360,.T.);
#56163=EDGE_CURVE('',#42517,#42516,#30361,.T.);
#56164=EDGE_CURVE('',#42517,#42518,#26437,.T.);
#56165=EDGE_CURVE('',#42518,#42514,#30362,.T.);
#56166=EDGE_CURVE('',#42516,#42519,#26438,.T.);
#56167=EDGE_CURVE('',#42519,#42510,#26439,.T.);
#56168=EDGE_CURVE('',#42509,#42520,#1406,.T.);
#56169=EDGE_CURVE('',#42520,#42517,#1407,.T.);
#56170=EDGE_CURVE('',#42518,#41248,#26440,.T.);
#56171=EDGE_CURVE('',#42521,#42517,#22944,.T.);
#56172=EDGE_CURVE('',#41248,#42521,#26441,.T.);
#56173=EDGE_CURVE('',#42522,#42509,#22945,.T.);
#56174=EDGE_CURVE('',#42521,#42522,#26442,.T.);
#56175=EDGE_CURVE('',#41247,#42513,#26443,.T.);
#56176=EDGE_CURVE('',#42522,#41247,#1408,.T.);
#56177=EDGE_CURVE('',#41777,#42518,#22946,.T.);
#56178=EDGE_CURVE('',#42514,#41776,#22947,.T.);
#56179=EDGE_CURVE('',#42515,#41496,#22948,.T.);
#56180=EDGE_CURVE('',#42516,#41495,#22949,.T.);
#56181=EDGE_CURVE('',#42510,#41494,#22950,.T.);
#56182=EDGE_CURVE('',#42511,#41493,#22951,.T.);
#56183=EDGE_CURVE('',#41779,#42512,#22952,.T.);
#56184=EDGE_CURVE('',#41778,#42513,#22953,.T.);
#56185=EDGE_CURVE('',#42523,#42524,#30363,.T.);
#56186=EDGE_CURVE('',#42524,#42525,#30364,.T.);
#56187=EDGE_CURVE('',#42525,#42526,#1409,.T.);
#56188=EDGE_CURVE('',#42526,#42527,#30365,.T.);
#56189=EDGE_CURVE('',#42527,#42523,#26444,.T.);
#56190=EDGE_CURVE('',#42528,#42529,#1410,.T.);
#56191=EDGE_CURVE('',#42529,#42530,#30366,.T.);
#56192=EDGE_CURVE('',#42531,#42530,#30367,.T.);
#56193=EDGE_CURVE('',#42531,#42532,#26445,.T.);
#56194=EDGE_CURVE('',#42532,#42528,#30368,.T.);
#56195=EDGE_CURVE('',#42530,#42533,#26446,.T.);
#56196=EDGE_CURVE('',#42533,#42524,#26447,.T.);
#56197=EDGE_CURVE('',#42523,#42534,#1411,.T.);
#56198=EDGE_CURVE('',#42534,#42531,#1412,.T.);
#56199=EDGE_CURVE('',#42532,#41244,#26448,.T.);
#56200=EDGE_CURVE('',#42535,#42531,#22954,.T.);
#56201=EDGE_CURVE('',#41244,#42535,#26449,.T.);
#56202=EDGE_CURVE('',#42536,#42523,#22955,.T.);
#56203=EDGE_CURVE('',#42535,#42536,#26450,.T.);
#56204=EDGE_CURVE('',#41243,#42527,#26451,.T.);
#56205=EDGE_CURVE('',#42536,#41243,#1413,.T.);
#56206=EDGE_CURVE('',#41773,#42532,#22956,.T.);
#56207=EDGE_CURVE('',#42528,#41772,#22957,.T.);
#56208=EDGE_CURVE('',#42529,#41500,#22958,.T.);
#56209=EDGE_CURVE('',#42530,#41499,#22959,.T.);
#56210=EDGE_CURVE('',#42524,#41498,#22960,.T.);
#56211=EDGE_CURVE('',#42525,#41497,#22961,.T.);
#56212=EDGE_CURVE('',#41775,#42526,#22962,.T.);
#56213=EDGE_CURVE('',#41774,#42527,#22963,.T.);
#56214=EDGE_CURVE('',#42537,#42538,#30369,.T.);
#56215=EDGE_CURVE('',#42538,#42539,#30370,.T.);
#56216=EDGE_CURVE('',#42539,#42540,#1414,.T.);
#56217=EDGE_CURVE('',#42540,#42541,#30371,.T.);
#56218=EDGE_CURVE('',#42541,#42537,#26452,.T.);
#56219=EDGE_CURVE('',#42542,#42543,#1415,.T.);
#56220=EDGE_CURVE('',#42543,#42544,#30372,.T.);
#56221=EDGE_CURVE('',#42545,#42544,#30373,.T.);
#56222=EDGE_CURVE('',#42545,#42546,#26453,.T.);
#56223=EDGE_CURVE('',#42546,#42542,#30374,.T.);
#56224=EDGE_CURVE('',#42544,#42547,#26454,.T.);
#56225=EDGE_CURVE('',#42547,#42538,#26455,.T.);
#56226=EDGE_CURVE('',#42537,#42548,#1416,.T.);
#56227=EDGE_CURVE('',#42548,#42545,#1417,.T.);
#56228=EDGE_CURVE('',#42546,#41240,#26456,.T.);
#56229=EDGE_CURVE('',#42549,#42545,#22964,.T.);
#56230=EDGE_CURVE('',#41240,#42549,#26457,.T.);
#56231=EDGE_CURVE('',#42550,#42537,#22965,.T.);
#56232=EDGE_CURVE('',#42549,#42550,#26458,.T.);
#56233=EDGE_CURVE('',#41239,#42541,#26459,.T.);
#56234=EDGE_CURVE('',#42550,#41239,#1418,.T.);
#56235=EDGE_CURVE('',#41769,#42546,#22966,.T.);
#56236=EDGE_CURVE('',#42542,#41768,#22967,.T.);
#56237=EDGE_CURVE('',#42543,#41504,#22968,.T.);
#56238=EDGE_CURVE('',#42544,#41503,#22969,.T.);
#56239=EDGE_CURVE('',#42538,#41502,#22970,.T.);
#56240=EDGE_CURVE('',#42539,#41501,#22971,.T.);
#56241=EDGE_CURVE('',#41771,#42540,#22972,.T.);
#56242=EDGE_CURVE('',#41770,#42541,#22973,.T.);
#56243=EDGE_CURVE('',#42551,#42552,#30375,.T.);
#56244=EDGE_CURVE('',#42552,#42553,#30376,.T.);
#56245=EDGE_CURVE('',#42553,#42554,#1419,.T.);
#56246=EDGE_CURVE('',#42554,#42555,#30377,.T.);
#56247=EDGE_CURVE('',#42555,#42551,#26460,.T.);
#56248=EDGE_CURVE('',#42556,#42557,#1420,.T.);
#56249=EDGE_CURVE('',#42557,#42558,#30378,.T.);
#56250=EDGE_CURVE('',#42559,#42558,#30379,.T.);
#56251=EDGE_CURVE('',#42559,#42560,#26461,.T.);
#56252=EDGE_CURVE('',#42560,#42556,#30380,.T.);
#56253=EDGE_CURVE('',#42558,#42561,#26462,.T.);
#56254=EDGE_CURVE('',#42561,#42552,#26463,.T.);
#56255=EDGE_CURVE('',#42551,#42562,#1421,.T.);
#56256=EDGE_CURVE('',#42562,#42559,#1422,.T.);
#56257=EDGE_CURVE('',#42560,#41236,#26464,.T.);
#56258=EDGE_CURVE('',#42563,#42559,#22974,.T.);
#56259=EDGE_CURVE('',#41236,#42563,#26465,.T.);
#56260=EDGE_CURVE('',#42564,#42551,#22975,.T.);
#56261=EDGE_CURVE('',#42563,#42564,#26466,.T.);
#56262=EDGE_CURVE('',#41235,#42555,#26467,.T.);
#56263=EDGE_CURVE('',#42564,#41235,#1423,.T.);
#56264=EDGE_CURVE('',#41765,#42560,#22976,.T.);
#56265=EDGE_CURVE('',#42556,#41764,#22977,.T.);
#56266=EDGE_CURVE('',#42557,#41508,#22978,.T.);
#56267=EDGE_CURVE('',#42558,#41507,#22979,.T.);
#56268=EDGE_CURVE('',#42552,#41506,#22980,.T.);
#56269=EDGE_CURVE('',#42553,#41505,#22981,.T.);
#56270=EDGE_CURVE('',#41767,#42554,#22982,.T.);
#56271=EDGE_CURVE('',#41766,#42555,#22983,.T.);
#56272=EDGE_CURVE('',#42565,#42566,#30381,.T.);
#56273=EDGE_CURVE('',#42566,#42567,#30382,.T.);
#56274=EDGE_CURVE('',#42567,#42568,#1424,.T.);
#56275=EDGE_CURVE('',#42568,#42569,#30383,.T.);
#56276=EDGE_CURVE('',#42569,#42565,#26468,.T.);
#56277=EDGE_CURVE('',#42570,#42571,#1425,.T.);
#56278=EDGE_CURVE('',#42571,#42572,#30384,.T.);
#56279=EDGE_CURVE('',#42573,#42572,#30385,.T.);
#56280=EDGE_CURVE('',#42573,#42574,#26469,.T.);
#56281=EDGE_CURVE('',#42574,#42570,#30386,.T.);
#56282=EDGE_CURVE('',#42572,#42575,#26470,.T.);
#56283=EDGE_CURVE('',#42575,#42566,#26471,.T.);
#56284=EDGE_CURVE('',#42565,#42576,#1426,.T.);
#56285=EDGE_CURVE('',#42576,#42573,#1427,.T.);
#56286=EDGE_CURVE('',#42574,#41232,#26472,.T.);
#56287=EDGE_CURVE('',#42577,#42573,#22984,.T.);
#56288=EDGE_CURVE('',#41232,#42577,#26473,.T.);
#56289=EDGE_CURVE('',#42578,#42565,#22985,.T.);
#56290=EDGE_CURVE('',#42577,#42578,#26474,.T.);
#56291=EDGE_CURVE('',#41231,#42569,#26475,.T.);
#56292=EDGE_CURVE('',#42578,#41231,#1428,.T.);
#56293=EDGE_CURVE('',#41761,#42574,#22986,.T.);
#56294=EDGE_CURVE('',#42570,#41760,#22987,.T.);
#56295=EDGE_CURVE('',#42571,#41512,#22988,.T.);
#56296=EDGE_CURVE('',#42572,#41511,#22989,.T.);
#56297=EDGE_CURVE('',#42566,#41510,#22990,.T.);
#56298=EDGE_CURVE('',#42567,#41509,#22991,.T.);
#56299=EDGE_CURVE('',#41763,#42568,#22992,.T.);
#56300=EDGE_CURVE('',#41762,#42569,#22993,.T.);
#56301=EDGE_CURVE('',#42579,#42580,#30387,.T.);
#56302=EDGE_CURVE('',#42580,#42581,#30388,.T.);
#56303=EDGE_CURVE('',#42581,#42582,#1429,.T.);
#56304=EDGE_CURVE('',#42582,#42583,#30389,.T.);
#56305=EDGE_CURVE('',#42583,#42579,#26476,.T.);
#56306=EDGE_CURVE('',#42584,#42585,#1430,.T.);
#56307=EDGE_CURVE('',#42585,#42586,#30390,.T.);
#56308=EDGE_CURVE('',#42587,#42586,#30391,.T.);
#56309=EDGE_CURVE('',#42587,#42588,#26477,.T.);
#56310=EDGE_CURVE('',#42588,#42584,#30392,.T.);
#56311=EDGE_CURVE('',#42586,#42589,#26478,.T.);
#56312=EDGE_CURVE('',#42589,#42580,#26479,.T.);
#56313=EDGE_CURVE('',#42579,#42590,#1431,.T.);
#56314=EDGE_CURVE('',#42590,#42587,#1432,.T.);
#56315=EDGE_CURVE('',#42588,#41228,#26480,.T.);
#56316=EDGE_CURVE('',#42591,#42587,#22994,.T.);
#56317=EDGE_CURVE('',#41228,#42591,#26481,.T.);
#56318=EDGE_CURVE('',#42592,#42579,#22995,.T.);
#56319=EDGE_CURVE('',#42591,#42592,#26482,.T.);
#56320=EDGE_CURVE('',#41227,#42583,#26483,.T.);
#56321=EDGE_CURVE('',#42592,#41227,#1433,.T.);
#56322=EDGE_CURVE('',#41757,#42588,#22996,.T.);
#56323=EDGE_CURVE('',#42584,#41756,#22997,.T.);
#56324=EDGE_CURVE('',#42585,#41516,#22998,.T.);
#56325=EDGE_CURVE('',#42586,#41515,#22999,.T.);
#56326=EDGE_CURVE('',#42580,#41514,#23000,.T.);
#56327=EDGE_CURVE('',#42581,#41513,#23001,.T.);
#56328=EDGE_CURVE('',#41759,#42582,#23002,.T.);
#56329=EDGE_CURVE('',#41758,#42583,#23003,.T.);
#56330=EDGE_CURVE('',#42593,#42594,#30393,.T.);
#56331=EDGE_CURVE('',#42594,#42595,#30394,.T.);
#56332=EDGE_CURVE('',#42595,#42596,#1434,.T.);
#56333=EDGE_CURVE('',#42596,#42597,#30395,.T.);
#56334=EDGE_CURVE('',#42597,#42593,#26484,.T.);
#56335=EDGE_CURVE('',#42598,#42599,#1435,.T.);
#56336=EDGE_CURVE('',#42599,#42600,#30396,.T.);
#56337=EDGE_CURVE('',#42601,#42600,#30397,.T.);
#56338=EDGE_CURVE('',#42601,#42602,#26485,.T.);
#56339=EDGE_CURVE('',#42602,#42598,#30398,.T.);
#56340=EDGE_CURVE('',#42600,#42603,#26486,.T.);
#56341=EDGE_CURVE('',#42603,#42594,#26487,.T.);
#56342=EDGE_CURVE('',#42593,#42604,#1436,.T.);
#56343=EDGE_CURVE('',#42604,#42601,#1437,.T.);
#56344=EDGE_CURVE('',#42602,#41224,#26488,.T.);
#56345=EDGE_CURVE('',#42605,#42601,#23004,.T.);
#56346=EDGE_CURVE('',#41224,#42605,#26489,.T.);
#56347=EDGE_CURVE('',#42606,#42593,#23005,.T.);
#56348=EDGE_CURVE('',#42605,#42606,#26490,.T.);
#56349=EDGE_CURVE('',#41223,#42597,#26491,.T.);
#56350=EDGE_CURVE('',#42606,#41223,#1438,.T.);
#56351=EDGE_CURVE('',#41753,#42602,#23006,.T.);
#56352=EDGE_CURVE('',#42598,#41752,#23007,.T.);
#56353=EDGE_CURVE('',#42599,#41520,#23008,.T.);
#56354=EDGE_CURVE('',#42600,#41519,#23009,.T.);
#56355=EDGE_CURVE('',#42594,#41518,#23010,.T.);
#56356=EDGE_CURVE('',#42595,#41517,#23011,.T.);
#56357=EDGE_CURVE('',#41755,#42596,#23012,.T.);
#56358=EDGE_CURVE('',#41754,#42597,#23013,.T.);
#56359=EDGE_CURVE('',#42607,#42608,#30399,.T.);
#56360=EDGE_CURVE('',#42608,#42609,#30400,.T.);
#56361=EDGE_CURVE('',#42609,#42610,#1439,.T.);
#56362=EDGE_CURVE('',#42610,#42611,#30401,.T.);
#56363=EDGE_CURVE('',#42611,#42607,#26492,.T.);
#56364=EDGE_CURVE('',#42612,#42613,#1440,.T.);
#56365=EDGE_CURVE('',#42613,#42614,#30402,.T.);
#56366=EDGE_CURVE('',#42615,#42614,#30403,.T.);
#56367=EDGE_CURVE('',#42615,#42616,#26493,.T.);
#56368=EDGE_CURVE('',#42616,#42612,#30404,.T.);
#56369=EDGE_CURVE('',#42614,#42617,#26494,.T.);
#56370=EDGE_CURVE('',#42617,#42608,#26495,.T.);
#56371=EDGE_CURVE('',#42607,#42618,#1441,.T.);
#56372=EDGE_CURVE('',#42618,#42615,#1442,.T.);
#56373=EDGE_CURVE('',#42616,#41220,#26496,.T.);
#56374=EDGE_CURVE('',#42619,#42615,#23014,.T.);
#56375=EDGE_CURVE('',#41220,#42619,#26497,.T.);
#56376=EDGE_CURVE('',#42620,#42607,#23015,.T.);
#56377=EDGE_CURVE('',#42619,#42620,#26498,.T.);
#56378=EDGE_CURVE('',#41219,#42611,#26499,.T.);
#56379=EDGE_CURVE('',#42620,#41219,#1443,.T.);
#56380=EDGE_CURVE('',#41749,#42616,#23016,.T.);
#56381=EDGE_CURVE('',#42612,#41748,#23017,.T.);
#56382=EDGE_CURVE('',#42613,#41524,#23018,.T.);
#56383=EDGE_CURVE('',#42614,#41523,#23019,.T.);
#56384=EDGE_CURVE('',#42608,#41522,#23020,.T.);
#56385=EDGE_CURVE('',#42609,#41521,#23021,.T.);
#56386=EDGE_CURVE('',#41751,#42610,#23022,.T.);
#56387=EDGE_CURVE('',#41750,#42611,#23023,.T.);
#56388=EDGE_CURVE('',#42621,#42622,#30405,.T.);
#56389=EDGE_CURVE('',#42622,#42623,#30406,.T.);
#56390=EDGE_CURVE('',#42623,#42624,#1444,.T.);
#56391=EDGE_CURVE('',#42624,#42625,#30407,.T.);
#56392=EDGE_CURVE('',#42625,#42621,#26500,.T.);
#56393=EDGE_CURVE('',#42626,#42627,#1445,.T.);
#56394=EDGE_CURVE('',#42627,#42628,#30408,.T.);
#56395=EDGE_CURVE('',#42629,#42628,#30409,.T.);
#56396=EDGE_CURVE('',#42629,#42630,#26501,.T.);
#56397=EDGE_CURVE('',#42630,#42626,#30410,.T.);
#56398=EDGE_CURVE('',#42628,#42631,#26502,.T.);
#56399=EDGE_CURVE('',#42631,#42622,#26503,.T.);
#56400=EDGE_CURVE('',#42621,#42632,#1446,.T.);
#56401=EDGE_CURVE('',#42632,#42629,#1447,.T.);
#56402=EDGE_CURVE('',#42630,#41216,#26504,.T.);
#56403=EDGE_CURVE('',#42633,#42629,#23024,.T.);
#56404=EDGE_CURVE('',#41216,#42633,#26505,.T.);
#56405=EDGE_CURVE('',#42634,#42621,#23025,.T.);
#56406=EDGE_CURVE('',#42633,#42634,#26506,.T.);
#56407=EDGE_CURVE('',#41215,#42625,#26507,.T.);
#56408=EDGE_CURVE('',#42634,#41215,#1448,.T.);
#56409=EDGE_CURVE('',#41745,#42630,#23026,.T.);
#56410=EDGE_CURVE('',#42626,#41744,#23027,.T.);
#56411=EDGE_CURVE('',#42627,#41528,#23028,.T.);
#56412=EDGE_CURVE('',#42628,#41527,#23029,.T.);
#56413=EDGE_CURVE('',#42622,#41526,#23030,.T.);
#56414=EDGE_CURVE('',#42623,#41525,#23031,.T.);
#56415=EDGE_CURVE('',#41747,#42624,#23032,.T.);
#56416=EDGE_CURVE('',#41746,#42625,#23033,.T.);
#56417=EDGE_CURVE('',#42635,#42636,#30411,.T.);
#56418=EDGE_CURVE('',#42636,#42637,#30412,.T.);
#56419=EDGE_CURVE('',#42637,#42638,#1449,.T.);
#56420=EDGE_CURVE('',#42638,#42639,#30413,.T.);
#56421=EDGE_CURVE('',#42639,#42635,#26508,.T.);
#56422=EDGE_CURVE('',#42640,#42641,#1450,.T.);
#56423=EDGE_CURVE('',#42641,#42642,#30414,.T.);
#56424=EDGE_CURVE('',#42643,#42642,#30415,.T.);
#56425=EDGE_CURVE('',#42643,#42644,#26509,.T.);
#56426=EDGE_CURVE('',#42644,#42640,#30416,.T.);
#56427=EDGE_CURVE('',#42642,#42645,#26510,.T.);
#56428=EDGE_CURVE('',#42645,#42636,#26511,.T.);
#56429=EDGE_CURVE('',#42635,#42646,#1451,.T.);
#56430=EDGE_CURVE('',#42646,#42643,#1452,.T.);
#56431=EDGE_CURVE('',#42644,#41212,#26512,.T.);
#56432=EDGE_CURVE('',#42647,#42643,#23034,.T.);
#56433=EDGE_CURVE('',#41212,#42647,#26513,.T.);
#56434=EDGE_CURVE('',#42648,#42635,#23035,.T.);
#56435=EDGE_CURVE('',#42647,#42648,#26514,.T.);
#56436=EDGE_CURVE('',#41211,#42639,#26515,.T.);
#56437=EDGE_CURVE('',#42648,#41211,#1453,.T.);
#56438=EDGE_CURVE('',#41741,#42644,#23036,.T.);
#56439=EDGE_CURVE('',#42640,#41740,#23037,.T.);
#56440=EDGE_CURVE('',#42641,#41532,#23038,.T.);
#56441=EDGE_CURVE('',#42642,#41531,#23039,.T.);
#56442=EDGE_CURVE('',#42636,#41530,#23040,.T.);
#56443=EDGE_CURVE('',#42637,#41529,#23041,.T.);
#56444=EDGE_CURVE('',#41743,#42638,#23042,.T.);
#56445=EDGE_CURVE('',#41742,#42639,#23043,.T.);
#56446=EDGE_CURVE('',#42649,#42650,#30417,.T.);
#56447=EDGE_CURVE('',#42650,#42651,#30418,.T.);
#56448=EDGE_CURVE('',#42651,#42652,#1454,.T.);
#56449=EDGE_CURVE('',#42652,#42653,#30419,.T.);
#56450=EDGE_CURVE('',#42653,#42649,#26516,.T.);
#56451=EDGE_CURVE('',#42654,#42655,#1455,.T.);
#56452=EDGE_CURVE('',#42655,#42656,#30420,.T.);
#56453=EDGE_CURVE('',#42657,#42656,#30421,.T.);
#56454=EDGE_CURVE('',#42657,#42658,#26517,.T.);
#56455=EDGE_CURVE('',#42658,#42654,#30422,.T.);
#56456=EDGE_CURVE('',#42656,#42659,#26518,.T.);
#56457=EDGE_CURVE('',#42659,#42650,#26519,.T.);
#56458=EDGE_CURVE('',#42649,#42660,#1456,.T.);
#56459=EDGE_CURVE('',#42660,#42657,#1457,.T.);
#56460=EDGE_CURVE('',#42658,#41208,#26520,.T.);
#56461=EDGE_CURVE('',#42661,#42657,#23044,.T.);
#56462=EDGE_CURVE('',#41208,#42661,#26521,.T.);
#56463=EDGE_CURVE('',#42662,#42649,#23045,.T.);
#56464=EDGE_CURVE('',#42661,#42662,#26522,.T.);
#56465=EDGE_CURVE('',#41207,#42653,#26523,.T.);
#56466=EDGE_CURVE('',#42662,#41207,#1458,.T.);
#56467=EDGE_CURVE('',#41737,#42658,#23046,.T.);
#56468=EDGE_CURVE('',#42654,#41736,#23047,.T.);
#56469=EDGE_CURVE('',#42655,#41536,#23048,.T.);
#56470=EDGE_CURVE('',#42656,#41535,#23049,.T.);
#56471=EDGE_CURVE('',#42650,#41534,#23050,.T.);
#56472=EDGE_CURVE('',#42651,#41533,#23051,.T.);
#56473=EDGE_CURVE('',#41739,#42652,#23052,.T.);
#56474=EDGE_CURVE('',#41738,#42653,#23053,.T.);
#56475=EDGE_CURVE('',#42663,#42664,#30423,.T.);
#56476=EDGE_CURVE('',#42664,#42665,#30424,.T.);
#56477=EDGE_CURVE('',#42665,#42666,#1459,.T.);
#56478=EDGE_CURVE('',#42666,#42667,#30425,.T.);
#56479=EDGE_CURVE('',#42667,#42663,#26524,.T.);
#56480=EDGE_CURVE('',#42668,#42669,#1460,.T.);
#56481=EDGE_CURVE('',#42669,#42670,#30426,.T.);
#56482=EDGE_CURVE('',#42671,#42670,#30427,.T.);
#56483=EDGE_CURVE('',#42671,#42672,#26525,.T.);
#56484=EDGE_CURVE('',#42672,#42668,#30428,.T.);
#56485=EDGE_CURVE('',#42670,#42673,#26526,.T.);
#56486=EDGE_CURVE('',#42673,#42664,#26527,.T.);
#56487=EDGE_CURVE('',#42663,#42674,#1461,.T.);
#56488=EDGE_CURVE('',#42674,#42671,#1462,.T.);
#56489=EDGE_CURVE('',#42672,#41204,#26528,.T.);
#56490=EDGE_CURVE('',#42675,#42671,#23054,.T.);
#56491=EDGE_CURVE('',#41204,#42675,#26529,.T.);
#56492=EDGE_CURVE('',#42676,#42663,#23055,.T.);
#56493=EDGE_CURVE('',#42675,#42676,#26530,.T.);
#56494=EDGE_CURVE('',#41203,#42667,#26531,.T.);
#56495=EDGE_CURVE('',#42676,#41203,#1463,.T.);
#56496=EDGE_CURVE('',#41733,#42672,#23056,.T.);
#56497=EDGE_CURVE('',#42668,#41732,#23057,.T.);
#56498=EDGE_CURVE('',#42669,#41540,#23058,.T.);
#56499=EDGE_CURVE('',#42670,#41539,#23059,.T.);
#56500=EDGE_CURVE('',#42664,#41538,#23060,.T.);
#56501=EDGE_CURVE('',#42665,#41537,#23061,.T.);
#56502=EDGE_CURVE('',#41735,#42666,#23062,.T.);
#56503=EDGE_CURVE('',#41734,#42667,#23063,.T.);
#56504=EDGE_CURVE('',#42677,#42678,#30429,.T.);
#56505=EDGE_CURVE('',#42678,#42679,#30430,.T.);
#56506=EDGE_CURVE('',#42679,#42680,#1464,.T.);
#56507=EDGE_CURVE('',#42680,#42681,#30431,.T.);
#56508=EDGE_CURVE('',#42681,#42677,#26532,.T.);
#56509=EDGE_CURVE('',#42682,#42683,#1465,.T.);
#56510=EDGE_CURVE('',#42683,#42684,#30432,.T.);
#56511=EDGE_CURVE('',#42685,#42684,#30433,.T.);
#56512=EDGE_CURVE('',#42685,#42686,#26533,.T.);
#56513=EDGE_CURVE('',#42686,#42682,#30434,.T.);
#56514=EDGE_CURVE('',#42684,#42687,#26534,.T.);
#56515=EDGE_CURVE('',#42687,#42678,#26535,.T.);
#56516=EDGE_CURVE('',#42677,#42688,#1466,.T.);
#56517=EDGE_CURVE('',#42688,#42685,#1467,.T.);
#56518=EDGE_CURVE('',#42686,#41200,#26536,.T.);
#56519=EDGE_CURVE('',#42689,#42685,#23064,.T.);
#56520=EDGE_CURVE('',#41200,#42689,#26537,.T.);
#56521=EDGE_CURVE('',#42690,#42677,#23065,.T.);
#56522=EDGE_CURVE('',#42689,#42690,#26538,.T.);
#56523=EDGE_CURVE('',#41199,#42681,#26539,.T.);
#56524=EDGE_CURVE('',#42690,#41199,#1468,.T.);
#56525=EDGE_CURVE('',#41729,#42686,#23066,.T.);
#56526=EDGE_CURVE('',#42682,#41728,#23067,.T.);
#56527=EDGE_CURVE('',#42683,#41544,#23068,.T.);
#56528=EDGE_CURVE('',#42684,#41543,#23069,.T.);
#56529=EDGE_CURVE('',#42678,#41542,#23070,.T.);
#56530=EDGE_CURVE('',#42679,#41541,#23071,.T.);
#56531=EDGE_CURVE('',#41731,#42680,#23072,.T.);
#56532=EDGE_CURVE('',#41730,#42681,#23073,.T.);
#56533=EDGE_CURVE('',#42691,#42692,#30435,.T.);
#56534=EDGE_CURVE('',#42692,#42693,#30436,.T.);
#56535=EDGE_CURVE('',#42693,#42694,#1469,.T.);
#56536=EDGE_CURVE('',#42694,#42695,#30437,.T.);
#56537=EDGE_CURVE('',#42695,#42691,#26540,.T.);
#56538=EDGE_CURVE('',#42696,#42697,#1470,.T.);
#56539=EDGE_CURVE('',#42697,#42698,#30438,.T.);
#56540=EDGE_CURVE('',#42699,#42698,#30439,.T.);
#56541=EDGE_CURVE('',#42699,#42700,#26541,.T.);
#56542=EDGE_CURVE('',#42700,#42696,#30440,.T.);
#56543=EDGE_CURVE('',#42698,#42701,#26542,.T.);
#56544=EDGE_CURVE('',#42701,#42692,#26543,.T.);
#56545=EDGE_CURVE('',#42691,#42702,#1471,.T.);
#56546=EDGE_CURVE('',#42702,#42699,#1472,.T.);
#56547=EDGE_CURVE('',#42700,#41196,#26544,.T.);
#56548=EDGE_CURVE('',#42703,#42699,#23074,.T.);
#56549=EDGE_CURVE('',#41196,#42703,#26545,.T.);
#56550=EDGE_CURVE('',#42704,#42691,#23075,.T.);
#56551=EDGE_CURVE('',#42703,#42704,#26546,.T.);
#56552=EDGE_CURVE('',#41195,#42695,#26547,.T.);
#56553=EDGE_CURVE('',#42704,#41195,#1473,.T.);
#56554=EDGE_CURVE('',#41725,#42700,#23076,.T.);
#56555=EDGE_CURVE('',#42696,#41724,#23077,.T.);
#56556=EDGE_CURVE('',#42697,#41548,#23078,.T.);
#56557=EDGE_CURVE('',#42698,#41547,#23079,.T.);
#56558=EDGE_CURVE('',#42692,#41546,#23080,.T.);
#56559=EDGE_CURVE('',#42693,#41545,#23081,.T.);
#56560=EDGE_CURVE('',#41727,#42694,#23082,.T.);
#56561=EDGE_CURVE('',#41726,#42695,#23083,.T.);
#56562=EDGE_CURVE('',#42705,#42706,#30441,.T.);
#56563=EDGE_CURVE('',#42706,#42707,#30442,.T.);
#56564=EDGE_CURVE('',#42707,#42708,#1474,.T.);
#56565=EDGE_CURVE('',#42708,#42709,#30443,.T.);
#56566=EDGE_CURVE('',#42709,#42705,#26548,.T.);
#56567=EDGE_CURVE('',#42710,#42711,#1475,.T.);
#56568=EDGE_CURVE('',#42711,#42712,#30444,.T.);
#56569=EDGE_CURVE('',#42713,#42712,#30445,.T.);
#56570=EDGE_CURVE('',#42713,#42714,#26549,.T.);
#56571=EDGE_CURVE('',#42714,#42710,#30446,.T.);
#56572=EDGE_CURVE('',#42712,#42715,#26550,.T.);
#56573=EDGE_CURVE('',#42715,#42706,#26551,.T.);
#56574=EDGE_CURVE('',#42705,#42716,#1476,.T.);
#56575=EDGE_CURVE('',#42716,#42713,#1477,.T.);
#56576=EDGE_CURVE('',#42714,#41192,#26552,.T.);
#56577=EDGE_CURVE('',#42717,#42713,#23084,.T.);
#56578=EDGE_CURVE('',#41192,#42717,#26553,.T.);
#56579=EDGE_CURVE('',#42718,#42705,#23085,.T.);
#56580=EDGE_CURVE('',#42717,#42718,#26554,.T.);
#56581=EDGE_CURVE('',#41191,#42709,#26555,.T.);
#56582=EDGE_CURVE('',#42718,#41191,#1478,.T.);
#56583=EDGE_CURVE('',#41721,#42714,#23086,.T.);
#56584=EDGE_CURVE('',#42710,#41720,#23087,.T.);
#56585=EDGE_CURVE('',#42711,#41552,#23088,.T.);
#56586=EDGE_CURVE('',#42712,#41551,#23089,.T.);
#56587=EDGE_CURVE('',#42706,#41550,#23090,.T.);
#56588=EDGE_CURVE('',#42707,#41549,#23091,.T.);
#56589=EDGE_CURVE('',#41723,#42708,#23092,.T.);
#56590=EDGE_CURVE('',#41722,#42709,#23093,.T.);
#56591=EDGE_CURVE('',#42719,#42720,#30447,.T.);
#56592=EDGE_CURVE('',#42720,#42721,#30448,.T.);
#56593=EDGE_CURVE('',#42721,#42722,#1479,.T.);
#56594=EDGE_CURVE('',#42722,#42723,#30449,.T.);
#56595=EDGE_CURVE('',#42723,#42719,#26556,.T.);
#56596=EDGE_CURVE('',#42724,#42725,#1480,.T.);
#56597=EDGE_CURVE('',#42725,#42726,#30450,.T.);
#56598=EDGE_CURVE('',#42727,#42726,#30451,.T.);
#56599=EDGE_CURVE('',#42727,#42728,#26557,.T.);
#56600=EDGE_CURVE('',#42728,#42724,#30452,.T.);
#56601=EDGE_CURVE('',#42726,#42729,#26558,.T.);
#56602=EDGE_CURVE('',#42729,#42720,#26559,.T.);
#56603=EDGE_CURVE('',#42719,#42730,#1481,.T.);
#56604=EDGE_CURVE('',#42730,#42727,#1482,.T.);
#56605=EDGE_CURVE('',#42728,#41188,#26560,.T.);
#56606=EDGE_CURVE('',#42731,#42727,#23094,.T.);
#56607=EDGE_CURVE('',#41188,#42731,#26561,.T.);
#56608=EDGE_CURVE('',#42732,#42719,#23095,.T.);
#56609=EDGE_CURVE('',#42731,#42732,#26562,.T.);
#56610=EDGE_CURVE('',#41187,#42723,#26563,.T.);
#56611=EDGE_CURVE('',#42732,#41187,#1483,.T.);
#56612=EDGE_CURVE('',#41717,#42728,#23096,.T.);
#56613=EDGE_CURVE('',#42724,#41715,#23097,.T.);
#56614=EDGE_CURVE('',#42725,#41556,#23098,.T.);
#56615=EDGE_CURVE('',#42726,#41555,#23099,.T.);
#56616=EDGE_CURVE('',#42720,#41554,#23100,.T.);
#56617=EDGE_CURVE('',#42721,#41553,#23101,.T.);
#56618=EDGE_CURVE('',#41719,#42722,#23102,.T.);
#56619=EDGE_CURVE('',#41718,#42723,#23103,.T.);
#56620=EDGE_CURVE('',#42733,#42734,#30453,.T.);
#56621=EDGE_CURVE('',#42734,#42735,#30454,.T.);
#56622=EDGE_CURVE('',#42735,#42736,#1484,.T.);
#56623=EDGE_CURVE('',#42736,#42737,#30455,.T.);
#56624=EDGE_CURVE('',#42737,#42733,#26564,.T.);
#56625=EDGE_CURVE('',#42738,#42739,#1485,.T.);
#56626=EDGE_CURVE('',#42739,#42740,#30456,.T.);
#56627=EDGE_CURVE('',#42741,#42740,#30457,.T.);
#56628=EDGE_CURVE('',#42741,#42742,#26565,.T.);
#56629=EDGE_CURVE('',#42742,#42738,#30458,.T.);
#56630=EDGE_CURVE('',#42740,#42743,#26566,.T.);
#56631=EDGE_CURVE('',#42743,#42734,#26567,.T.);
#56632=EDGE_CURVE('',#42733,#42744,#1486,.T.);
#56633=EDGE_CURVE('',#42744,#42741,#1487,.T.);
#56634=EDGE_CURVE('',#42742,#41184,#26568,.T.);
#56635=EDGE_CURVE('',#42745,#42741,#23104,.T.);
#56636=EDGE_CURVE('',#41184,#42745,#26569,.T.);
#56637=EDGE_CURVE('',#42746,#42733,#23105,.T.);
#56638=EDGE_CURVE('',#42745,#42746,#26570,.T.);
#56639=EDGE_CURVE('',#41183,#42737,#26571,.T.);
#56640=EDGE_CURVE('',#42746,#41183,#1488,.T.);
#56641=EDGE_CURVE('',#42021,#42742,#23106,.T.);
#56642=EDGE_CURVE('',#42738,#42020,#23107,.T.);
#56643=EDGE_CURVE('',#42739,#41563,#23108,.T.);
#56644=EDGE_CURVE('',#42740,#41562,#23109,.T.);
#56645=EDGE_CURVE('',#42734,#41561,#23110,.T.);
#56646=EDGE_CURVE('',#42735,#41560,#23111,.T.);
#56647=EDGE_CURVE('',#41716,#42736,#23112,.T.);
#56648=EDGE_CURVE('',#42022,#42737,#23113,.T.);
#56649=EDGE_CURVE('',#42747,#42748,#30459,.T.);
#56650=EDGE_CURVE('',#42748,#42749,#30460,.T.);
#56651=EDGE_CURVE('',#42749,#42750,#1489,.T.);
#56652=EDGE_CURVE('',#42750,#42751,#30461,.T.);
#56653=EDGE_CURVE('',#42751,#42747,#26572,.T.);
#56654=EDGE_CURVE('',#42752,#42753,#1490,.T.);
#56655=EDGE_CURVE('',#42753,#42754,#30462,.T.);
#56656=EDGE_CURVE('',#42755,#42754,#30463,.T.);
#56657=EDGE_CURVE('',#42755,#42756,#26573,.T.);
#56658=EDGE_CURVE('',#42756,#42752,#30464,.T.);
#56659=EDGE_CURVE('',#42754,#42757,#26574,.T.);
#56660=EDGE_CURVE('',#42757,#42748,#26575,.T.);
#56661=EDGE_CURVE('',#42747,#42758,#1491,.T.);
#56662=EDGE_CURVE('',#42758,#42755,#1492,.T.);
#56663=EDGE_CURVE('',#42756,#41180,#26576,.T.);
#56664=EDGE_CURVE('',#42759,#42755,#23114,.T.);
#56665=EDGE_CURVE('',#41180,#42759,#26577,.T.);
#56666=EDGE_CURVE('',#42760,#42747,#23115,.T.);
#56667=EDGE_CURVE('',#42759,#42760,#26578,.T.);
#56668=EDGE_CURVE('',#41179,#42751,#26579,.T.);
#56669=EDGE_CURVE('',#42760,#41179,#1493,.T.);
#56670=EDGE_CURVE('',#42017,#42756,#23116,.T.);
#56671=EDGE_CURVE('',#42752,#42016,#23117,.T.);
#56672=EDGE_CURVE('',#42753,#41567,#23118,.T.);
#56673=EDGE_CURVE('',#42754,#41566,#23119,.T.);
#56674=EDGE_CURVE('',#42748,#41565,#23120,.T.);
#56675=EDGE_CURVE('',#42749,#41564,#23121,.T.);
#56676=EDGE_CURVE('',#42019,#42750,#23122,.T.);
#56677=EDGE_CURVE('',#42018,#42751,#23123,.T.);
#56678=EDGE_CURVE('',#42761,#42762,#30465,.T.);
#56679=EDGE_CURVE('',#42762,#42763,#30466,.T.);
#56680=EDGE_CURVE('',#42763,#42764,#1494,.T.);
#56681=EDGE_CURVE('',#42764,#42765,#30467,.T.);
#56682=EDGE_CURVE('',#42765,#42761,#26580,.T.);
#56683=EDGE_CURVE('',#42766,#42767,#1495,.T.);
#56684=EDGE_CURVE('',#42767,#42768,#30468,.T.);
#56685=EDGE_CURVE('',#42769,#42768,#30469,.T.);
#56686=EDGE_CURVE('',#42769,#42770,#26581,.T.);
#56687=EDGE_CURVE('',#42770,#42766,#30470,.T.);
#56688=EDGE_CURVE('',#42768,#42771,#26582,.T.);
#56689=EDGE_CURVE('',#42771,#42762,#26583,.T.);
#56690=EDGE_CURVE('',#42761,#42772,#1496,.T.);
#56691=EDGE_CURVE('',#42772,#42769,#1497,.T.);
#56692=EDGE_CURVE('',#42770,#41176,#26584,.T.);
#56693=EDGE_CURVE('',#42773,#42769,#23124,.T.);
#56694=EDGE_CURVE('',#41176,#42773,#26585,.T.);
#56695=EDGE_CURVE('',#42774,#42761,#23125,.T.);
#56696=EDGE_CURVE('',#42773,#42774,#26586,.T.);
#56697=EDGE_CURVE('',#41175,#42765,#26587,.T.);
#56698=EDGE_CURVE('',#42774,#41175,#1498,.T.);
#56699=EDGE_CURVE('',#42013,#42770,#23126,.T.);
#56700=EDGE_CURVE('',#42766,#42012,#23127,.T.);
#56701=EDGE_CURVE('',#42767,#41571,#23128,.T.);
#56702=EDGE_CURVE('',#42768,#41570,#23129,.T.);
#56703=EDGE_CURVE('',#42762,#41569,#23130,.T.);
#56704=EDGE_CURVE('',#42763,#41568,#23131,.T.);
#56705=EDGE_CURVE('',#42015,#42764,#23132,.T.);
#56706=EDGE_CURVE('',#42014,#42765,#23133,.T.);
#56707=EDGE_CURVE('',#42775,#42776,#30471,.T.);
#56708=EDGE_CURVE('',#42776,#42777,#30472,.T.);
#56709=EDGE_CURVE('',#42777,#42778,#1499,.T.);
#56710=EDGE_CURVE('',#42778,#42779,#30473,.T.);
#56711=EDGE_CURVE('',#42779,#42775,#26588,.T.);
#56712=EDGE_CURVE('',#42780,#42781,#1500,.T.);
#56713=EDGE_CURVE('',#42781,#42782,#30474,.T.);
#56714=EDGE_CURVE('',#42783,#42782,#30475,.T.);
#56715=EDGE_CURVE('',#42783,#42784,#26589,.T.);
#56716=EDGE_CURVE('',#42784,#42780,#30476,.T.);
#56717=EDGE_CURVE('',#42782,#42785,#26590,.T.);
#56718=EDGE_CURVE('',#42785,#42776,#26591,.T.);
#56719=EDGE_CURVE('',#42775,#42786,#1501,.T.);
#56720=EDGE_CURVE('',#42786,#42783,#1502,.T.);
#56721=EDGE_CURVE('',#42784,#41172,#26592,.T.);
#56722=EDGE_CURVE('',#42787,#42783,#23134,.T.);
#56723=EDGE_CURVE('',#41172,#42787,#26593,.T.);
#56724=EDGE_CURVE('',#42788,#42775,#23135,.T.);
#56725=EDGE_CURVE('',#42787,#42788,#26594,.T.);
#56726=EDGE_CURVE('',#41171,#42779,#26595,.T.);
#56727=EDGE_CURVE('',#42788,#41171,#1503,.T.);
#56728=EDGE_CURVE('',#42009,#42784,#23136,.T.);
#56729=EDGE_CURVE('',#42780,#42008,#23137,.T.);
#56730=EDGE_CURVE('',#42781,#41575,#23138,.T.);
#56731=EDGE_CURVE('',#42782,#41574,#23139,.T.);
#56732=EDGE_CURVE('',#42776,#41573,#23140,.T.);
#56733=EDGE_CURVE('',#42777,#41572,#23141,.T.);
#56734=EDGE_CURVE('',#42011,#42778,#23142,.T.);
#56735=EDGE_CURVE('',#42010,#42779,#23143,.T.);
#56736=EDGE_CURVE('',#42789,#42790,#30477,.T.);
#56737=EDGE_CURVE('',#42790,#42791,#30478,.T.);
#56738=EDGE_CURVE('',#42791,#42792,#1504,.T.);
#56739=EDGE_CURVE('',#42792,#42793,#30479,.T.);
#56740=EDGE_CURVE('',#42793,#42789,#26596,.T.);
#56741=EDGE_CURVE('',#42794,#42795,#1505,.T.);
#56742=EDGE_CURVE('',#42795,#42796,#30480,.T.);
#56743=EDGE_CURVE('',#42797,#42796,#30481,.T.);
#56744=EDGE_CURVE('',#42797,#42798,#26597,.T.);
#56745=EDGE_CURVE('',#42798,#42794,#30482,.T.);
#56746=EDGE_CURVE('',#42796,#42799,#26598,.T.);
#56747=EDGE_CURVE('',#42799,#42790,#26599,.T.);
#56748=EDGE_CURVE('',#42789,#42800,#1506,.T.);
#56749=EDGE_CURVE('',#42800,#42797,#1507,.T.);
#56750=EDGE_CURVE('',#42798,#41168,#26600,.T.);
#56751=EDGE_CURVE('',#42801,#42797,#23144,.T.);
#56752=EDGE_CURVE('',#41168,#42801,#26601,.T.);
#56753=EDGE_CURVE('',#42802,#42789,#23145,.T.);
#56754=EDGE_CURVE('',#42801,#42802,#26602,.T.);
#56755=EDGE_CURVE('',#41167,#42793,#26603,.T.);
#56756=EDGE_CURVE('',#42802,#41167,#1508,.T.);
#56757=EDGE_CURVE('',#42005,#42798,#23146,.T.);
#56758=EDGE_CURVE('',#42794,#42004,#23147,.T.);
#56759=EDGE_CURVE('',#42795,#41579,#23148,.T.);
#56760=EDGE_CURVE('',#42796,#41578,#23149,.T.);
#56761=EDGE_CURVE('',#42790,#41577,#23150,.T.);
#56762=EDGE_CURVE('',#42791,#41576,#23151,.T.);
#56763=EDGE_CURVE('',#42007,#42792,#23152,.T.);
#56764=EDGE_CURVE('',#42006,#42793,#23153,.T.);
#56765=EDGE_CURVE('',#42803,#42804,#30483,.T.);
#56766=EDGE_CURVE('',#42804,#42805,#30484,.T.);
#56767=EDGE_CURVE('',#42805,#42806,#1509,.T.);
#56768=EDGE_CURVE('',#42806,#42807,#30485,.T.);
#56769=EDGE_CURVE('',#42807,#42803,#26604,.T.);
#56770=EDGE_CURVE('',#42808,#42809,#1510,.T.);
#56771=EDGE_CURVE('',#42809,#42810,#30486,.T.);
#56772=EDGE_CURVE('',#42811,#42810,#30487,.T.);
#56773=EDGE_CURVE('',#42811,#42812,#26605,.T.);
#56774=EDGE_CURVE('',#42812,#42808,#30488,.T.);
#56775=EDGE_CURVE('',#42810,#42813,#26606,.T.);
#56776=EDGE_CURVE('',#42813,#42804,#26607,.T.);
#56777=EDGE_CURVE('',#42803,#42814,#1511,.T.);
#56778=EDGE_CURVE('',#42814,#42811,#1512,.T.);
#56779=EDGE_CURVE('',#42812,#41164,#26608,.T.);
#56780=EDGE_CURVE('',#42815,#42811,#23154,.T.);
#56781=EDGE_CURVE('',#41164,#42815,#26609,.T.);
#56782=EDGE_CURVE('',#42816,#42803,#23155,.T.);
#56783=EDGE_CURVE('',#42815,#42816,#26610,.T.);
#56784=EDGE_CURVE('',#41163,#42807,#26611,.T.);
#56785=EDGE_CURVE('',#42816,#41163,#1513,.T.);
#56786=EDGE_CURVE('',#42001,#42812,#23156,.T.);
#56787=EDGE_CURVE('',#42808,#42000,#23157,.T.);
#56788=EDGE_CURVE('',#42809,#41583,#23158,.T.);
#56789=EDGE_CURVE('',#42810,#41582,#23159,.T.);
#56790=EDGE_CURVE('',#42804,#41581,#23160,.T.);
#56791=EDGE_CURVE('',#42805,#41580,#23161,.T.);
#56792=EDGE_CURVE('',#42003,#42806,#23162,.T.);
#56793=EDGE_CURVE('',#42002,#42807,#23163,.T.);
#56794=EDGE_CURVE('',#42817,#42818,#30489,.T.);
#56795=EDGE_CURVE('',#42818,#42819,#30490,.T.);
#56796=EDGE_CURVE('',#42819,#42820,#1514,.T.);
#56797=EDGE_CURVE('',#42820,#42821,#30491,.T.);
#56798=EDGE_CURVE('',#42821,#42817,#26612,.T.);
#56799=EDGE_CURVE('',#42822,#42823,#1515,.T.);
#56800=EDGE_CURVE('',#42823,#42824,#30492,.T.);
#56801=EDGE_CURVE('',#42825,#42824,#30493,.T.);
#56802=EDGE_CURVE('',#42825,#42826,#26613,.T.);
#56803=EDGE_CURVE('',#42826,#42822,#30494,.T.);
#56804=EDGE_CURVE('',#42824,#42827,#26614,.T.);
#56805=EDGE_CURVE('',#42827,#42818,#26615,.T.);
#56806=EDGE_CURVE('',#42817,#42828,#1516,.T.);
#56807=EDGE_CURVE('',#42828,#42825,#1517,.T.);
#56808=EDGE_CURVE('',#42826,#41160,#26616,.T.);
#56809=EDGE_CURVE('',#42829,#42825,#23164,.T.);
#56810=EDGE_CURVE('',#41160,#42829,#26617,.T.);
#56811=EDGE_CURVE('',#42830,#42817,#23165,.T.);
#56812=EDGE_CURVE('',#42829,#42830,#26618,.T.);
#56813=EDGE_CURVE('',#41159,#42821,#26619,.T.);
#56814=EDGE_CURVE('',#42830,#41159,#1518,.T.);
#56815=EDGE_CURVE('',#41997,#42826,#23166,.T.);
#56816=EDGE_CURVE('',#42822,#41996,#23167,.T.);
#56817=EDGE_CURVE('',#42823,#41587,#23168,.T.);
#56818=EDGE_CURVE('',#42824,#41586,#23169,.T.);
#56819=EDGE_CURVE('',#42818,#41585,#23170,.T.);
#56820=EDGE_CURVE('',#42819,#41584,#23171,.T.);
#56821=EDGE_CURVE('',#41999,#42820,#23172,.T.);
#56822=EDGE_CURVE('',#41998,#42821,#23173,.T.);
#56823=EDGE_CURVE('',#42831,#42832,#30495,.T.);
#56824=EDGE_CURVE('',#42832,#42833,#30496,.T.);
#56825=EDGE_CURVE('',#42833,#42834,#1519,.T.);
#56826=EDGE_CURVE('',#42834,#42835,#30497,.T.);
#56827=EDGE_CURVE('',#42835,#42831,#26620,.T.);
#56828=EDGE_CURVE('',#42836,#42837,#1520,.T.);
#56829=EDGE_CURVE('',#42837,#42838,#30498,.T.);
#56830=EDGE_CURVE('',#42839,#42838,#30499,.T.);
#56831=EDGE_CURVE('',#42839,#42840,#26621,.T.);
#56832=EDGE_CURVE('',#42840,#42836,#30500,.T.);
#56833=EDGE_CURVE('',#42838,#42841,#26622,.T.);
#56834=EDGE_CURVE('',#42841,#42832,#26623,.T.);
#56835=EDGE_CURVE('',#42831,#42842,#1521,.T.);
#56836=EDGE_CURVE('',#42842,#42839,#1522,.T.);
#56837=EDGE_CURVE('',#42840,#41156,#26624,.T.);
#56838=EDGE_CURVE('',#42843,#42839,#23174,.T.);
#56839=EDGE_CURVE('',#41156,#42843,#26625,.T.);
#56840=EDGE_CURVE('',#42844,#42831,#23175,.T.);
#56841=EDGE_CURVE('',#42843,#42844,#26626,.T.);
#56842=EDGE_CURVE('',#41155,#42835,#26627,.T.);
#56843=EDGE_CURVE('',#42844,#41155,#1523,.T.);
#56844=EDGE_CURVE('',#41993,#42840,#23176,.T.);
#56845=EDGE_CURVE('',#42836,#41992,#23177,.T.);
#56846=EDGE_CURVE('',#42837,#41591,#23178,.T.);
#56847=EDGE_CURVE('',#42838,#41590,#23179,.T.);
#56848=EDGE_CURVE('',#42832,#41589,#23180,.T.);
#56849=EDGE_CURVE('',#42833,#41588,#23181,.T.);
#56850=EDGE_CURVE('',#41995,#42834,#23182,.T.);
#56851=EDGE_CURVE('',#41994,#42835,#23183,.T.);
#56852=EDGE_CURVE('',#42845,#42846,#30501,.T.);
#56853=EDGE_CURVE('',#42846,#42847,#30502,.T.);
#56854=EDGE_CURVE('',#42847,#42848,#1524,.T.);
#56855=EDGE_CURVE('',#42848,#42849,#30503,.T.);
#56856=EDGE_CURVE('',#42849,#42845,#26628,.T.);
#56857=EDGE_CURVE('',#42850,#42851,#1525,.T.);
#56858=EDGE_CURVE('',#42851,#42852,#30504,.T.);
#56859=EDGE_CURVE('',#42853,#42852,#30505,.T.);
#56860=EDGE_CURVE('',#42853,#42854,#26629,.T.);
#56861=EDGE_CURVE('',#42854,#42850,#30506,.T.);
#56862=EDGE_CURVE('',#42852,#42855,#26630,.T.);
#56863=EDGE_CURVE('',#42855,#42846,#26631,.T.);
#56864=EDGE_CURVE('',#42845,#42856,#1526,.T.);
#56865=EDGE_CURVE('',#42856,#42853,#1527,.T.);
#56866=EDGE_CURVE('',#42854,#41152,#26632,.T.);
#56867=EDGE_CURVE('',#42857,#42853,#23184,.T.);
#56868=EDGE_CURVE('',#41152,#42857,#26633,.T.);
#56869=EDGE_CURVE('',#42858,#42845,#23185,.T.);
#56870=EDGE_CURVE('',#42857,#42858,#26634,.T.);
#56871=EDGE_CURVE('',#41151,#42849,#26635,.T.);
#56872=EDGE_CURVE('',#42858,#41151,#1528,.T.);
#56873=EDGE_CURVE('',#41989,#42854,#23186,.T.);
#56874=EDGE_CURVE('',#42850,#41988,#23187,.T.);
#56875=EDGE_CURVE('',#42851,#41595,#23188,.T.);
#56876=EDGE_CURVE('',#42852,#41594,#23189,.T.);
#56877=EDGE_CURVE('',#42846,#41593,#23190,.T.);
#56878=EDGE_CURVE('',#42847,#41592,#23191,.T.);
#56879=EDGE_CURVE('',#41991,#42848,#23192,.T.);
#56880=EDGE_CURVE('',#41990,#42849,#23193,.T.);
#56881=EDGE_CURVE('',#42859,#42860,#30507,.T.);
#56882=EDGE_CURVE('',#42860,#42861,#30508,.T.);
#56883=EDGE_CURVE('',#42861,#42862,#1529,.T.);
#56884=EDGE_CURVE('',#42862,#42863,#30509,.T.);
#56885=EDGE_CURVE('',#42863,#42859,#26636,.T.);
#56886=EDGE_CURVE('',#42864,#42865,#1530,.T.);
#56887=EDGE_CURVE('',#42865,#42866,#30510,.T.);
#56888=EDGE_CURVE('',#42867,#42866,#30511,.T.);
#56889=EDGE_CURVE('',#42867,#42868,#26637,.T.);
#56890=EDGE_CURVE('',#42868,#42864,#30512,.T.);
#56891=EDGE_CURVE('',#42866,#42869,#26638,.T.);
#56892=EDGE_CURVE('',#42869,#42860,#26639,.T.);
#56893=EDGE_CURVE('',#42859,#42870,#1531,.T.);
#56894=EDGE_CURVE('',#42870,#42867,#1532,.T.);
#56895=EDGE_CURVE('',#42868,#41148,#26640,.T.);
#56896=EDGE_CURVE('',#42871,#42867,#23194,.T.);
#56897=EDGE_CURVE('',#41148,#42871,#26641,.T.);
#56898=EDGE_CURVE('',#42872,#42859,#23195,.T.);
#56899=EDGE_CURVE('',#42871,#42872,#26642,.T.);
#56900=EDGE_CURVE('',#41147,#42863,#26643,.T.);
#56901=EDGE_CURVE('',#42872,#41147,#1533,.T.);
#56902=EDGE_CURVE('',#41985,#42868,#23196,.T.);
#56903=EDGE_CURVE('',#42864,#41984,#23197,.T.);
#56904=EDGE_CURVE('',#42865,#41599,#23198,.T.);
#56905=EDGE_CURVE('',#42866,#41598,#23199,.T.);
#56906=EDGE_CURVE('',#42860,#41597,#23200,.T.);
#56907=EDGE_CURVE('',#42861,#41596,#23201,.T.);
#56908=EDGE_CURVE('',#41987,#42862,#23202,.T.);
#56909=EDGE_CURVE('',#41986,#42863,#23203,.T.);
#56910=EDGE_CURVE('',#42873,#42874,#30513,.T.);
#56911=EDGE_CURVE('',#42874,#42875,#30514,.T.);
#56912=EDGE_CURVE('',#42875,#42876,#1534,.T.);
#56913=EDGE_CURVE('',#42876,#42877,#30515,.T.);
#56914=EDGE_CURVE('',#42877,#42873,#26644,.T.);
#56915=EDGE_CURVE('',#42878,#42879,#1535,.T.);
#56916=EDGE_CURVE('',#42879,#42880,#30516,.T.);
#56917=EDGE_CURVE('',#42881,#42880,#30517,.T.);
#56918=EDGE_CURVE('',#42881,#42882,#26645,.T.);
#56919=EDGE_CURVE('',#42882,#42878,#30518,.T.);
#56920=EDGE_CURVE('',#42880,#42883,#26646,.T.);
#56921=EDGE_CURVE('',#42883,#42874,#26647,.T.);
#56922=EDGE_CURVE('',#42873,#42884,#1536,.T.);
#56923=EDGE_CURVE('',#42884,#42881,#1537,.T.);
#56924=EDGE_CURVE('',#42882,#41144,#26648,.T.);
#56925=EDGE_CURVE('',#42885,#42881,#23204,.T.);
#56926=EDGE_CURVE('',#41144,#42885,#26649,.T.);
#56927=EDGE_CURVE('',#42886,#42873,#23205,.T.);
#56928=EDGE_CURVE('',#42885,#42886,#26650,.T.);
#56929=EDGE_CURVE('',#41143,#42877,#26651,.T.);
#56930=EDGE_CURVE('',#42886,#41143,#1538,.T.);
#56931=EDGE_CURVE('',#41981,#42882,#23206,.T.);
#56932=EDGE_CURVE('',#42878,#41980,#23207,.T.);
#56933=EDGE_CURVE('',#42879,#41603,#23208,.T.);
#56934=EDGE_CURVE('',#42880,#41602,#23209,.T.);
#56935=EDGE_CURVE('',#42874,#41601,#23210,.T.);
#56936=EDGE_CURVE('',#42875,#41600,#23211,.T.);
#56937=EDGE_CURVE('',#41983,#42876,#23212,.T.);
#56938=EDGE_CURVE('',#41982,#42877,#23213,.T.);
#56939=EDGE_CURVE('',#42887,#42888,#30519,.T.);
#56940=EDGE_CURVE('',#42888,#42889,#30520,.T.);
#56941=EDGE_CURVE('',#42889,#42890,#1539,.T.);
#56942=EDGE_CURVE('',#42890,#42891,#30521,.T.);
#56943=EDGE_CURVE('',#42891,#42887,#26652,.T.);
#56944=EDGE_CURVE('',#42892,#42893,#1540,.T.);
#56945=EDGE_CURVE('',#42893,#42894,#30522,.T.);
#56946=EDGE_CURVE('',#42895,#42894,#30523,.T.);
#56947=EDGE_CURVE('',#42895,#42896,#26653,.T.);
#56948=EDGE_CURVE('',#42896,#42892,#30524,.T.);
#56949=EDGE_CURVE('',#42894,#42897,#26654,.T.);
#56950=EDGE_CURVE('',#42897,#42888,#26655,.T.);
#56951=EDGE_CURVE('',#42887,#42898,#1541,.T.);
#56952=EDGE_CURVE('',#42898,#42895,#1542,.T.);
#56953=EDGE_CURVE('',#42896,#41140,#26656,.T.);
#56954=EDGE_CURVE('',#42899,#42895,#23214,.T.);
#56955=EDGE_CURVE('',#41140,#42899,#26657,.T.);
#56956=EDGE_CURVE('',#42900,#42887,#23215,.T.);
#56957=EDGE_CURVE('',#42899,#42900,#26658,.T.);
#56958=EDGE_CURVE('',#41139,#42891,#26659,.T.);
#56959=EDGE_CURVE('',#42900,#41139,#1543,.T.);
#56960=EDGE_CURVE('',#41977,#42896,#23216,.T.);
#56961=EDGE_CURVE('',#42892,#41976,#23217,.T.);
#56962=EDGE_CURVE('',#42893,#41607,#23218,.T.);
#56963=EDGE_CURVE('',#42894,#41606,#23219,.T.);
#56964=EDGE_CURVE('',#42888,#41605,#23220,.T.);
#56965=EDGE_CURVE('',#42889,#41604,#23221,.T.);
#56966=EDGE_CURVE('',#41979,#42890,#23222,.T.);
#56967=EDGE_CURVE('',#41978,#42891,#23223,.T.);
#56968=EDGE_CURVE('',#42901,#42902,#30525,.T.);
#56969=EDGE_CURVE('',#42902,#42903,#30526,.T.);
#56970=EDGE_CURVE('',#42903,#42904,#1544,.T.);
#56971=EDGE_CURVE('',#42904,#42905,#30527,.T.);
#56972=EDGE_CURVE('',#42905,#42901,#26660,.T.);
#56973=EDGE_CURVE('',#42906,#42907,#1545,.T.);
#56974=EDGE_CURVE('',#42907,#42908,#30528,.T.);
#56975=EDGE_CURVE('',#42909,#42908,#30529,.T.);
#56976=EDGE_CURVE('',#42909,#42910,#26661,.T.);
#56977=EDGE_CURVE('',#42910,#42906,#30530,.T.);
#56978=EDGE_CURVE('',#42908,#42911,#26662,.T.);
#56979=EDGE_CURVE('',#42911,#42902,#26663,.T.);
#56980=EDGE_CURVE('',#42901,#42912,#1546,.T.);
#56981=EDGE_CURVE('',#42912,#42909,#1547,.T.);
#56982=EDGE_CURVE('',#42910,#41136,#26664,.T.);
#56983=EDGE_CURVE('',#42913,#42909,#23224,.T.);
#56984=EDGE_CURVE('',#41136,#42913,#26665,.T.);
#56985=EDGE_CURVE('',#42914,#42901,#23225,.T.);
#56986=EDGE_CURVE('',#42913,#42914,#26666,.T.);
#56987=EDGE_CURVE('',#41135,#42905,#26667,.T.);
#56988=EDGE_CURVE('',#42914,#41135,#1548,.T.);
#56989=EDGE_CURVE('',#41973,#42910,#23226,.T.);
#56990=EDGE_CURVE('',#42906,#41972,#23227,.T.);
#56991=EDGE_CURVE('',#42907,#41611,#23228,.T.);
#56992=EDGE_CURVE('',#42908,#41610,#23229,.T.);
#56993=EDGE_CURVE('',#42902,#41609,#23230,.T.);
#56994=EDGE_CURVE('',#42903,#41608,#23231,.T.);
#56995=EDGE_CURVE('',#41975,#42904,#23232,.T.);
#56996=EDGE_CURVE('',#41974,#42905,#23233,.T.);
#56997=EDGE_CURVE('',#42915,#42916,#30531,.T.);
#56998=EDGE_CURVE('',#42916,#42917,#30532,.T.);
#56999=EDGE_CURVE('',#42917,#42918,#1549,.T.);
#57000=EDGE_CURVE('',#42918,#42919,#30533,.T.);
#57001=EDGE_CURVE('',#42919,#42915,#26668,.T.);
#57002=EDGE_CURVE('',#42920,#42921,#1550,.T.);
#57003=EDGE_CURVE('',#42921,#42922,#30534,.T.);
#57004=EDGE_CURVE('',#42923,#42922,#30535,.T.);
#57005=EDGE_CURVE('',#42923,#42924,#26669,.T.);
#57006=EDGE_CURVE('',#42924,#42920,#30536,.T.);
#57007=EDGE_CURVE('',#42922,#42925,#26670,.T.);
#57008=EDGE_CURVE('',#42925,#42916,#26671,.T.);
#57009=EDGE_CURVE('',#42915,#42926,#1551,.T.);
#57010=EDGE_CURVE('',#42926,#42923,#1552,.T.);
#57011=EDGE_CURVE('',#42924,#41132,#26672,.T.);
#57012=EDGE_CURVE('',#42927,#42923,#23234,.T.);
#57013=EDGE_CURVE('',#41132,#42927,#26673,.T.);
#57014=EDGE_CURVE('',#42928,#42915,#23235,.T.);
#57015=EDGE_CURVE('',#42927,#42928,#26674,.T.);
#57016=EDGE_CURVE('',#41131,#42919,#26675,.T.);
#57017=EDGE_CURVE('',#42928,#41131,#1553,.T.);
#57018=EDGE_CURVE('',#41969,#42924,#23236,.T.);
#57019=EDGE_CURVE('',#42920,#41968,#23237,.T.);
#57020=EDGE_CURVE('',#42921,#41615,#23238,.T.);
#57021=EDGE_CURVE('',#42922,#41614,#23239,.T.);
#57022=EDGE_CURVE('',#42916,#41613,#23240,.T.);
#57023=EDGE_CURVE('',#42917,#41612,#23241,.T.);
#57024=EDGE_CURVE('',#41971,#42918,#23242,.T.);
#57025=EDGE_CURVE('',#41970,#42919,#23243,.T.);
#57026=EDGE_CURVE('',#42929,#42930,#30537,.T.);
#57027=EDGE_CURVE('',#42930,#42931,#30538,.T.);
#57028=EDGE_CURVE('',#42931,#42932,#1554,.T.);
#57029=EDGE_CURVE('',#42932,#42933,#30539,.T.);
#57030=EDGE_CURVE('',#42933,#42929,#26676,.T.);
#57031=EDGE_CURVE('',#42934,#42935,#1555,.T.);
#57032=EDGE_CURVE('',#42935,#42936,#30540,.T.);
#57033=EDGE_CURVE('',#42937,#42936,#30541,.T.);
#57034=EDGE_CURVE('',#42937,#42938,#26677,.T.);
#57035=EDGE_CURVE('',#42938,#42934,#30542,.T.);
#57036=EDGE_CURVE('',#42936,#42939,#26678,.T.);
#57037=EDGE_CURVE('',#42939,#42930,#26679,.T.);
#57038=EDGE_CURVE('',#42929,#42940,#1556,.T.);
#57039=EDGE_CURVE('',#42940,#42937,#1557,.T.);
#57040=EDGE_CURVE('',#42938,#41128,#26680,.T.);
#57041=EDGE_CURVE('',#42941,#42937,#23244,.T.);
#57042=EDGE_CURVE('',#41128,#42941,#26681,.T.);
#57043=EDGE_CURVE('',#42942,#42929,#23245,.T.);
#57044=EDGE_CURVE('',#42941,#42942,#26682,.T.);
#57045=EDGE_CURVE('',#41127,#42933,#26683,.T.);
#57046=EDGE_CURVE('',#42942,#41127,#1558,.T.);
#57047=EDGE_CURVE('',#41965,#42938,#23246,.T.);
#57048=EDGE_CURVE('',#42934,#41964,#23247,.T.);
#57049=EDGE_CURVE('',#42935,#41619,#23248,.T.);
#57050=EDGE_CURVE('',#42936,#41618,#23249,.T.);
#57051=EDGE_CURVE('',#42930,#41617,#23250,.T.);
#57052=EDGE_CURVE('',#42931,#41616,#23251,.T.);
#57053=EDGE_CURVE('',#41967,#42932,#23252,.T.);
#57054=EDGE_CURVE('',#41966,#42933,#23253,.T.);
#57055=EDGE_CURVE('',#42943,#42944,#30543,.T.);
#57056=EDGE_CURVE('',#42944,#42945,#30544,.T.);
#57057=EDGE_CURVE('',#42945,#42946,#1559,.T.);
#57058=EDGE_CURVE('',#42946,#42947,#30545,.T.);
#57059=EDGE_CURVE('',#42947,#42943,#26684,.T.);
#57060=EDGE_CURVE('',#42948,#42949,#1560,.T.);
#57061=EDGE_CURVE('',#42949,#42950,#30546,.T.);
#57062=EDGE_CURVE('',#42951,#42950,#30547,.T.);
#57063=EDGE_CURVE('',#42951,#42952,#26685,.T.);
#57064=EDGE_CURVE('',#42952,#42948,#30548,.T.);
#57065=EDGE_CURVE('',#42950,#42953,#26686,.T.);
#57066=EDGE_CURVE('',#42953,#42944,#26687,.T.);
#57067=EDGE_CURVE('',#42943,#42954,#1561,.T.);
#57068=EDGE_CURVE('',#42954,#42951,#1562,.T.);
#57069=EDGE_CURVE('',#42952,#41124,#26688,.T.);
#57070=EDGE_CURVE('',#42955,#42951,#23254,.T.);
#57071=EDGE_CURVE('',#41124,#42955,#26689,.T.);
#57072=EDGE_CURVE('',#42956,#42943,#23255,.T.);
#57073=EDGE_CURVE('',#42955,#42956,#26690,.T.);
#57074=EDGE_CURVE('',#41123,#42947,#26691,.T.);
#57075=EDGE_CURVE('',#42956,#41123,#1563,.T.);
#57076=EDGE_CURVE('',#41961,#42952,#23256,.T.);
#57077=EDGE_CURVE('',#42948,#41960,#23257,.T.);
#57078=EDGE_CURVE('',#42949,#41623,#23258,.T.);
#57079=EDGE_CURVE('',#42950,#41622,#23259,.T.);
#57080=EDGE_CURVE('',#42944,#41621,#23260,.T.);
#57081=EDGE_CURVE('',#42945,#41620,#23261,.T.);
#57082=EDGE_CURVE('',#41963,#42946,#23262,.T.);
#57083=EDGE_CURVE('',#41962,#42947,#23263,.T.);
#57084=EDGE_CURVE('',#42957,#42958,#30549,.T.);
#57085=EDGE_CURVE('',#42958,#42959,#30550,.T.);
#57086=EDGE_CURVE('',#42959,#42960,#1564,.T.);
#57087=EDGE_CURVE('',#42960,#42961,#30551,.T.);
#57088=EDGE_CURVE('',#42961,#42957,#26692,.T.);
#57089=EDGE_CURVE('',#42962,#42963,#1565,.T.);
#57090=EDGE_CURVE('',#42963,#42964,#30552,.T.);
#57091=EDGE_CURVE('',#42965,#42964,#30553,.T.);
#57092=EDGE_CURVE('',#42965,#42966,#26693,.T.);
#57093=EDGE_CURVE('',#42966,#42962,#30554,.T.);
#57094=EDGE_CURVE('',#42964,#42967,#26694,.T.);
#57095=EDGE_CURVE('',#42967,#42958,#26695,.T.);
#57096=EDGE_CURVE('',#42957,#42968,#1566,.T.);
#57097=EDGE_CURVE('',#42968,#42965,#1567,.T.);
#57098=EDGE_CURVE('',#42966,#41120,#26696,.T.);
#57099=EDGE_CURVE('',#42969,#42965,#23264,.T.);
#57100=EDGE_CURVE('',#41120,#42969,#26697,.T.);
#57101=EDGE_CURVE('',#42970,#42957,#23265,.T.);
#57102=EDGE_CURVE('',#42969,#42970,#26698,.T.);
#57103=EDGE_CURVE('',#41119,#42961,#26699,.T.);
#57104=EDGE_CURVE('',#42970,#41119,#1568,.T.);
#57105=EDGE_CURVE('',#41957,#42966,#23266,.T.);
#57106=EDGE_CURVE('',#42962,#41956,#23267,.T.);
#57107=EDGE_CURVE('',#42963,#41627,#23268,.T.);
#57108=EDGE_CURVE('',#42964,#41626,#23269,.T.);
#57109=EDGE_CURVE('',#42958,#41625,#23270,.T.);
#57110=EDGE_CURVE('',#42959,#41624,#23271,.T.);
#57111=EDGE_CURVE('',#41959,#42960,#23272,.T.);
#57112=EDGE_CURVE('',#41958,#42961,#23273,.T.);
#57113=EDGE_CURVE('',#42971,#42972,#30555,.T.);
#57114=EDGE_CURVE('',#42972,#42973,#30556,.T.);
#57115=EDGE_CURVE('',#42973,#42974,#1569,.T.);
#57116=EDGE_CURVE('',#42974,#42975,#30557,.T.);
#57117=EDGE_CURVE('',#42975,#42971,#26700,.T.);
#57118=EDGE_CURVE('',#42976,#42977,#1570,.T.);
#57119=EDGE_CURVE('',#42977,#42978,#30558,.T.);
#57120=EDGE_CURVE('',#42979,#42978,#30559,.T.);
#57121=EDGE_CURVE('',#42979,#42980,#26701,.T.);
#57122=EDGE_CURVE('',#42980,#42976,#30560,.T.);
#57123=EDGE_CURVE('',#42978,#42981,#26702,.T.);
#57124=EDGE_CURVE('',#42981,#42972,#26703,.T.);
#57125=EDGE_CURVE('',#42971,#42982,#1571,.T.);
#57126=EDGE_CURVE('',#42982,#42979,#1572,.T.);
#57127=EDGE_CURVE('',#42980,#41116,#26704,.T.);
#57128=EDGE_CURVE('',#42983,#42979,#23274,.T.);
#57129=EDGE_CURVE('',#41116,#42983,#26705,.T.);
#57130=EDGE_CURVE('',#42984,#42971,#23275,.T.);
#57131=EDGE_CURVE('',#42983,#42984,#26706,.T.);
#57132=EDGE_CURVE('',#41115,#42975,#26707,.T.);
#57133=EDGE_CURVE('',#42984,#41115,#1573,.T.);
#57134=EDGE_CURVE('',#41953,#42980,#23276,.T.);
#57135=EDGE_CURVE('',#42976,#41952,#23277,.T.);
#57136=EDGE_CURVE('',#42977,#41631,#23278,.T.);
#57137=EDGE_CURVE('',#42978,#41630,#23279,.T.);
#57138=EDGE_CURVE('',#42972,#41629,#23280,.T.);
#57139=EDGE_CURVE('',#42973,#41628,#23281,.T.);
#57140=EDGE_CURVE('',#41955,#42974,#23282,.T.);
#57141=EDGE_CURVE('',#41954,#42975,#23283,.T.);
#57142=EDGE_CURVE('',#42985,#42986,#30561,.T.);
#57143=EDGE_CURVE('',#42986,#42987,#30562,.T.);
#57144=EDGE_CURVE('',#42987,#42988,#1574,.T.);
#57145=EDGE_CURVE('',#42988,#42989,#30563,.T.);
#57146=EDGE_CURVE('',#42989,#42985,#26708,.T.);
#57147=EDGE_CURVE('',#42990,#42991,#1575,.T.);
#57148=EDGE_CURVE('',#42991,#42992,#30564,.T.);
#57149=EDGE_CURVE('',#42993,#42992,#30565,.T.);
#57150=EDGE_CURVE('',#42993,#42994,#26709,.T.);
#57151=EDGE_CURVE('',#42994,#42990,#30566,.T.);
#57152=EDGE_CURVE('',#42992,#42995,#26710,.T.);
#57153=EDGE_CURVE('',#42995,#42986,#26711,.T.);
#57154=EDGE_CURVE('',#42985,#42996,#1576,.T.);
#57155=EDGE_CURVE('',#42996,#42993,#1577,.T.);
#57156=EDGE_CURVE('',#42994,#41112,#26712,.T.);
#57157=EDGE_CURVE('',#42997,#42993,#23284,.T.);
#57158=EDGE_CURVE('',#41112,#42997,#26713,.T.);
#57159=EDGE_CURVE('',#42998,#42985,#23285,.T.);
#57160=EDGE_CURVE('',#42997,#42998,#26714,.T.);
#57161=EDGE_CURVE('',#41111,#42989,#26715,.T.);
#57162=EDGE_CURVE('',#42998,#41111,#1578,.T.);
#57163=EDGE_CURVE('',#41949,#42994,#23286,.T.);
#57164=EDGE_CURVE('',#42990,#41948,#23287,.T.);
#57165=EDGE_CURVE('',#42991,#41635,#23288,.T.);
#57166=EDGE_CURVE('',#42992,#41634,#23289,.T.);
#57167=EDGE_CURVE('',#42986,#41633,#23290,.T.);
#57168=EDGE_CURVE('',#42987,#41632,#23291,.T.);
#57169=EDGE_CURVE('',#41951,#42988,#23292,.T.);
#57170=EDGE_CURVE('',#41950,#42989,#23293,.T.);
#57171=EDGE_CURVE('',#42999,#43000,#30567,.T.);
#57172=EDGE_CURVE('',#43000,#43001,#30568,.T.);
#57173=EDGE_CURVE('',#43001,#43002,#1579,.T.);
#57174=EDGE_CURVE('',#43002,#43003,#30569,.T.);
#57175=EDGE_CURVE('',#43003,#42999,#26716,.T.);
#57176=EDGE_CURVE('',#43004,#43005,#1580,.T.);
#57177=EDGE_CURVE('',#43005,#43006,#30570,.T.);
#57178=EDGE_CURVE('',#43007,#43006,#30571,.T.);
#57179=EDGE_CURVE('',#43007,#43008,#26717,.T.);
#57180=EDGE_CURVE('',#43008,#43004,#30572,.T.);
#57181=EDGE_CURVE('',#43006,#43009,#26718,.T.);
#57182=EDGE_CURVE('',#43009,#43000,#26719,.T.);
#57183=EDGE_CURVE('',#42999,#43010,#1581,.T.);
#57184=EDGE_CURVE('',#43010,#43007,#1582,.T.);
#57185=EDGE_CURVE('',#43008,#41108,#26720,.T.);
#57186=EDGE_CURVE('',#43011,#43007,#23294,.T.);
#57187=EDGE_CURVE('',#41108,#43011,#26721,.T.);
#57188=EDGE_CURVE('',#43012,#42999,#23295,.T.);
#57189=EDGE_CURVE('',#43011,#43012,#26722,.T.);
#57190=EDGE_CURVE('',#41107,#43003,#26723,.T.);
#57191=EDGE_CURVE('',#43012,#41107,#1583,.T.);
#57192=EDGE_CURVE('',#41945,#43008,#23296,.T.);
#57193=EDGE_CURVE('',#43004,#41944,#23297,.T.);
#57194=EDGE_CURVE('',#43005,#41639,#23298,.T.);
#57195=EDGE_CURVE('',#43006,#41638,#23299,.T.);
#57196=EDGE_CURVE('',#43000,#41637,#23300,.T.);
#57197=EDGE_CURVE('',#43001,#41636,#23301,.T.);
#57198=EDGE_CURVE('',#41947,#43002,#23302,.T.);
#57199=EDGE_CURVE('',#41946,#43003,#23303,.T.);
#57200=EDGE_CURVE('',#43013,#43014,#30573,.T.);
#57201=EDGE_CURVE('',#43014,#43015,#30574,.T.);
#57202=EDGE_CURVE('',#43015,#43016,#1584,.T.);
#57203=EDGE_CURVE('',#43016,#43017,#30575,.T.);
#57204=EDGE_CURVE('',#43017,#43013,#26724,.T.);
#57205=EDGE_CURVE('',#43018,#43019,#1585,.T.);
#57206=EDGE_CURVE('',#43019,#43020,#30576,.T.);
#57207=EDGE_CURVE('',#43021,#43020,#30577,.T.);
#57208=EDGE_CURVE('',#43021,#43022,#26725,.T.);
#57209=EDGE_CURVE('',#43022,#43018,#30578,.T.);
#57210=EDGE_CURVE('',#43020,#43023,#26726,.T.);
#57211=EDGE_CURVE('',#43023,#43014,#26727,.T.);
#57212=EDGE_CURVE('',#43013,#43024,#1586,.T.);
#57213=EDGE_CURVE('',#43024,#43021,#1587,.T.);
#57214=EDGE_CURVE('',#43022,#41104,#26728,.T.);
#57215=EDGE_CURVE('',#43025,#43021,#23304,.T.);
#57216=EDGE_CURVE('',#41104,#43025,#26729,.T.);
#57217=EDGE_CURVE('',#43026,#43013,#23305,.T.);
#57218=EDGE_CURVE('',#43025,#43026,#26730,.T.);
#57219=EDGE_CURVE('',#41103,#43017,#26731,.T.);
#57220=EDGE_CURVE('',#43026,#41103,#1588,.T.);
#57221=EDGE_CURVE('',#41941,#43022,#23306,.T.);
#57222=EDGE_CURVE('',#43018,#41940,#23307,.T.);
#57223=EDGE_CURVE('',#43019,#41643,#23308,.T.);
#57224=EDGE_CURVE('',#43020,#41642,#23309,.T.);
#57225=EDGE_CURVE('',#43014,#41641,#23310,.T.);
#57226=EDGE_CURVE('',#43015,#41640,#23311,.T.);
#57227=EDGE_CURVE('',#41943,#43016,#23312,.T.);
#57228=EDGE_CURVE('',#41942,#43017,#23313,.T.);
#57229=EDGE_CURVE('',#43027,#43028,#30579,.T.);
#57230=EDGE_CURVE('',#43028,#43029,#30580,.T.);
#57231=EDGE_CURVE('',#43029,#43030,#1589,.T.);
#57232=EDGE_CURVE('',#43030,#43031,#30581,.T.);
#57233=EDGE_CURVE('',#43031,#43027,#26732,.T.);
#57234=EDGE_CURVE('',#43032,#43033,#1590,.T.);
#57235=EDGE_CURVE('',#43033,#43034,#30582,.T.);
#57236=EDGE_CURVE('',#43035,#43034,#30583,.T.);
#57237=EDGE_CURVE('',#43035,#43036,#26733,.T.);
#57238=EDGE_CURVE('',#43036,#43032,#30584,.T.);
#57239=EDGE_CURVE('',#43034,#43037,#26734,.T.);
#57240=EDGE_CURVE('',#43037,#43028,#26735,.T.);
#57241=EDGE_CURVE('',#43027,#43038,#1591,.T.);
#57242=EDGE_CURVE('',#43038,#43035,#1592,.T.);
#57243=EDGE_CURVE('',#43036,#41100,#26736,.T.);
#57244=EDGE_CURVE('',#43039,#43035,#23314,.T.);
#57245=EDGE_CURVE('',#41100,#43039,#26737,.T.);
#57246=EDGE_CURVE('',#43040,#43027,#23315,.T.);
#57247=EDGE_CURVE('',#43039,#43040,#26738,.T.);
#57248=EDGE_CURVE('',#41099,#43031,#26739,.T.);
#57249=EDGE_CURVE('',#43040,#41099,#1593,.T.);
#57250=EDGE_CURVE('',#41937,#43036,#23316,.T.);
#57251=EDGE_CURVE('',#43032,#41936,#23317,.T.);
#57252=EDGE_CURVE('',#43033,#41647,#23318,.T.);
#57253=EDGE_CURVE('',#43034,#41646,#23319,.T.);
#57254=EDGE_CURVE('',#43028,#41645,#23320,.T.);
#57255=EDGE_CURVE('',#43029,#41644,#23321,.T.);
#57256=EDGE_CURVE('',#41939,#43030,#23322,.T.);
#57257=EDGE_CURVE('',#41938,#43031,#23323,.T.);
#57258=EDGE_CURVE('',#43041,#43042,#30585,.T.);
#57259=EDGE_CURVE('',#43042,#43043,#30586,.T.);
#57260=EDGE_CURVE('',#43043,#43044,#1594,.T.);
#57261=EDGE_CURVE('',#43044,#43045,#30587,.T.);
#57262=EDGE_CURVE('',#43045,#43041,#26740,.T.);
#57263=EDGE_CURVE('',#43046,#43047,#1595,.T.);
#57264=EDGE_CURVE('',#43047,#43048,#30588,.T.);
#57265=EDGE_CURVE('',#43049,#43048,#30589,.T.);
#57266=EDGE_CURVE('',#43049,#43050,#26741,.T.);
#57267=EDGE_CURVE('',#43050,#43046,#30590,.T.);
#57268=EDGE_CURVE('',#43048,#43051,#26742,.T.);
#57269=EDGE_CURVE('',#43051,#43042,#26743,.T.);
#57270=EDGE_CURVE('',#43041,#43052,#1596,.T.);
#57271=EDGE_CURVE('',#43052,#43049,#1597,.T.);
#57272=EDGE_CURVE('',#43050,#41096,#26744,.T.);
#57273=EDGE_CURVE('',#43053,#43049,#23324,.T.);
#57274=EDGE_CURVE('',#41096,#43053,#26745,.T.);
#57275=EDGE_CURVE('',#43054,#43041,#23325,.T.);
#57276=EDGE_CURVE('',#43053,#43054,#26746,.T.);
#57277=EDGE_CURVE('',#41095,#43045,#26747,.T.);
#57278=EDGE_CURVE('',#43054,#41095,#1598,.T.);
#57279=EDGE_CURVE('',#41933,#43050,#23326,.T.);
#57280=EDGE_CURVE('',#43046,#41932,#23327,.T.);
#57281=EDGE_CURVE('',#43047,#41651,#23328,.T.);
#57282=EDGE_CURVE('',#43048,#41650,#23329,.T.);
#57283=EDGE_CURVE('',#43042,#41649,#23330,.T.);
#57284=EDGE_CURVE('',#43043,#41648,#23331,.T.);
#57285=EDGE_CURVE('',#41935,#43044,#23332,.T.);
#57286=EDGE_CURVE('',#41934,#43045,#23333,.T.);
#57287=EDGE_CURVE('',#43055,#43056,#30591,.T.);
#57288=EDGE_CURVE('',#43056,#43057,#30592,.T.);
#57289=EDGE_CURVE('',#43057,#43058,#1599,.T.);
#57290=EDGE_CURVE('',#43058,#43059,#30593,.T.);
#57291=EDGE_CURVE('',#43059,#43055,#26748,.T.);
#57292=EDGE_CURVE('',#43060,#43061,#1600,.T.);
#57293=EDGE_CURVE('',#43061,#43062,#30594,.T.);
#57294=EDGE_CURVE('',#43063,#43062,#30595,.T.);
#57295=EDGE_CURVE('',#43063,#43064,#26749,.T.);
#57296=EDGE_CURVE('',#43064,#43060,#30596,.T.);
#57297=EDGE_CURVE('',#43062,#43065,#26750,.T.);
#57298=EDGE_CURVE('',#43065,#43056,#26751,.T.);
#57299=EDGE_CURVE('',#43055,#43066,#1601,.T.);
#57300=EDGE_CURVE('',#43066,#43063,#1602,.T.);
#57301=EDGE_CURVE('',#43064,#41092,#26752,.T.);
#57302=EDGE_CURVE('',#43067,#43063,#23334,.T.);
#57303=EDGE_CURVE('',#41092,#43067,#26753,.T.);
#57304=EDGE_CURVE('',#43068,#43055,#23335,.T.);
#57305=EDGE_CURVE('',#43067,#43068,#26754,.T.);
#57306=EDGE_CURVE('',#41091,#43059,#26755,.T.);
#57307=EDGE_CURVE('',#43068,#41091,#1603,.T.);
#57308=EDGE_CURVE('',#41929,#43064,#23336,.T.);
#57309=EDGE_CURVE('',#43060,#41928,#23337,.T.);
#57310=EDGE_CURVE('',#43061,#41655,#23338,.T.);
#57311=EDGE_CURVE('',#43062,#41654,#23339,.T.);
#57312=EDGE_CURVE('',#43056,#41653,#23340,.T.);
#57313=EDGE_CURVE('',#43057,#41652,#23341,.T.);
#57314=EDGE_CURVE('',#41931,#43058,#23342,.T.);
#57315=EDGE_CURVE('',#41930,#43059,#23343,.T.);
#57316=EDGE_CURVE('',#43069,#43070,#30597,.T.);
#57317=EDGE_CURVE('',#43070,#43071,#30598,.T.);
#57318=EDGE_CURVE('',#43071,#43072,#1604,.T.);
#57319=EDGE_CURVE('',#43072,#43073,#30599,.T.);
#57320=EDGE_CURVE('',#43073,#43069,#26756,.T.);
#57321=EDGE_CURVE('',#43074,#43075,#1605,.T.);
#57322=EDGE_CURVE('',#43075,#43076,#30600,.T.);
#57323=EDGE_CURVE('',#43077,#43076,#30601,.T.);
#57324=EDGE_CURVE('',#43077,#43078,#26757,.T.);
#57325=EDGE_CURVE('',#43078,#43074,#30602,.T.);
#57326=EDGE_CURVE('',#43076,#43079,#26758,.T.);
#57327=EDGE_CURVE('',#43079,#43070,#26759,.T.);
#57328=EDGE_CURVE('',#43069,#43080,#1606,.T.);
#57329=EDGE_CURVE('',#43080,#43077,#1607,.T.);
#57330=EDGE_CURVE('',#43078,#41088,#26760,.T.);
#57331=EDGE_CURVE('',#43081,#43077,#23344,.T.);
#57332=EDGE_CURVE('',#41088,#43081,#26761,.T.);
#57333=EDGE_CURVE('',#43082,#43069,#23345,.T.);
#57334=EDGE_CURVE('',#43081,#43082,#26762,.T.);
#57335=EDGE_CURVE('',#41087,#43073,#26763,.T.);
#57336=EDGE_CURVE('',#43082,#41087,#1608,.T.);
#57337=EDGE_CURVE('',#41925,#43078,#23346,.T.);
#57338=EDGE_CURVE('',#43074,#41924,#23347,.T.);
#57339=EDGE_CURVE('',#43075,#41659,#23348,.T.);
#57340=EDGE_CURVE('',#43076,#41658,#23349,.T.);
#57341=EDGE_CURVE('',#43070,#41657,#23350,.T.);
#57342=EDGE_CURVE('',#43071,#41656,#23351,.T.);
#57343=EDGE_CURVE('',#41927,#43072,#23352,.T.);
#57344=EDGE_CURVE('',#41926,#43073,#23353,.T.);
#57345=EDGE_CURVE('',#43083,#43084,#30603,.T.);
#57346=EDGE_CURVE('',#43084,#43085,#30604,.T.);
#57347=EDGE_CURVE('',#43085,#43086,#1609,.T.);
#57348=EDGE_CURVE('',#43086,#43087,#30605,.T.);
#57349=EDGE_CURVE('',#43087,#43083,#26764,.T.);
#57350=EDGE_CURVE('',#43088,#43089,#1610,.T.);
#57351=EDGE_CURVE('',#43089,#43090,#30606,.T.);
#57352=EDGE_CURVE('',#43091,#43090,#30607,.T.);
#57353=EDGE_CURVE('',#43091,#43092,#26765,.T.);
#57354=EDGE_CURVE('',#43092,#43088,#30608,.T.);
#57355=EDGE_CURVE('',#43090,#43093,#26766,.T.);
#57356=EDGE_CURVE('',#43093,#43084,#26767,.T.);
#57357=EDGE_CURVE('',#43083,#43094,#1611,.T.);
#57358=EDGE_CURVE('',#43094,#43091,#1612,.T.);
#57359=EDGE_CURVE('',#43092,#41084,#26768,.T.);
#57360=EDGE_CURVE('',#43095,#43091,#23354,.T.);
#57361=EDGE_CURVE('',#41084,#43095,#26769,.T.);
#57362=EDGE_CURVE('',#43096,#43083,#23355,.T.);
#57363=EDGE_CURVE('',#43095,#43096,#26770,.T.);
#57364=EDGE_CURVE('',#41083,#43087,#26771,.T.);
#57365=EDGE_CURVE('',#43096,#41083,#1613,.T.);
#57366=EDGE_CURVE('',#41921,#43092,#23356,.T.);
#57367=EDGE_CURVE('',#43088,#41920,#23357,.T.);
#57368=EDGE_CURVE('',#43089,#41663,#23358,.T.);
#57369=EDGE_CURVE('',#43090,#41662,#23359,.T.);
#57370=EDGE_CURVE('',#43084,#41661,#23360,.T.);
#57371=EDGE_CURVE('',#43085,#41660,#23361,.T.);
#57372=EDGE_CURVE('',#41923,#43086,#23362,.T.);
#57373=EDGE_CURVE('',#41922,#43087,#23363,.T.);
#57374=EDGE_CURVE('',#43097,#43098,#30609,.T.);
#57375=EDGE_CURVE('',#43098,#43099,#30610,.T.);
#57376=EDGE_CURVE('',#43099,#43100,#1614,.T.);
#57377=EDGE_CURVE('',#43100,#43101,#30611,.T.);
#57378=EDGE_CURVE('',#43101,#43097,#26772,.T.);
#57379=EDGE_CURVE('',#43102,#43103,#1615,.T.);
#57380=EDGE_CURVE('',#43103,#43104,#30612,.T.);
#57381=EDGE_CURVE('',#43105,#43104,#30613,.T.);
#57382=EDGE_CURVE('',#43105,#43106,#26773,.T.);
#57383=EDGE_CURVE('',#43106,#43102,#30614,.T.);
#57384=EDGE_CURVE('',#43104,#43107,#26774,.T.);
#57385=EDGE_CURVE('',#43107,#43098,#26775,.T.);
#57386=EDGE_CURVE('',#43097,#43108,#1616,.T.);
#57387=EDGE_CURVE('',#43108,#43105,#1617,.T.);
#57388=EDGE_CURVE('',#43106,#41080,#26776,.T.);
#57389=EDGE_CURVE('',#43109,#43105,#23364,.T.);
#57390=EDGE_CURVE('',#41080,#43109,#26777,.T.);
#57391=EDGE_CURVE('',#43110,#43097,#23365,.T.);
#57392=EDGE_CURVE('',#43109,#43110,#26778,.T.);
#57393=EDGE_CURVE('',#41079,#43101,#26779,.T.);
#57394=EDGE_CURVE('',#43110,#41079,#1618,.T.);
#57395=EDGE_CURVE('',#41917,#43106,#23366,.T.);
#57396=EDGE_CURVE('',#43102,#41916,#23367,.T.);
#57397=EDGE_CURVE('',#43103,#41667,#23368,.T.);
#57398=EDGE_CURVE('',#43104,#41666,#23369,.T.);
#57399=EDGE_CURVE('',#43098,#41665,#23370,.T.);
#57400=EDGE_CURVE('',#43099,#41664,#23371,.T.);
#57401=EDGE_CURVE('',#41919,#43100,#23372,.T.);
#57402=EDGE_CURVE('',#41918,#43101,#23373,.T.);
#57403=EDGE_CURVE('',#43111,#43112,#30615,.T.);
#57404=EDGE_CURVE('',#43113,#43112,#23374,.T.);
#57405=EDGE_CURVE('',#43113,#43111,#26780,.T.);
#57406=EDGE_CURVE('',#43114,#43115,#30616,.T.);
#57407=EDGE_CURVE('',#43115,#43116,#26781,.T.);
#57408=EDGE_CURVE('',#43112,#43116,#23375,.T.);
#57409=EDGE_CURVE('',#43111,#43114,#26782,.T.);
#57410=EDGE_CURVE('',#43117,#43118,#30617,.T.);
#57411=EDGE_CURVE('',#43118,#43115,#26783,.T.);
#57412=EDGE_CURVE('',#43114,#43117,#26784,.T.);
#57413=EDGE_CURVE('',#43119,#43120,#30618,.T.);
#57414=EDGE_CURVE('',#43120,#43118,#26785,.T.);
#57415=EDGE_CURVE('',#43117,#43119,#26786,.T.);
#57416=EDGE_CURVE('',#43121,#43122,#30619,.T.);
#57417=EDGE_CURVE('',#43122,#43120,#26787,.T.);
#57418=EDGE_CURVE('',#43119,#43121,#26788,.T.);
#57419=EDGE_CURVE('',#43123,#43124,#30620,.T.);
#57420=EDGE_CURVE('',#43124,#43122,#26789,.T.);
#57421=EDGE_CURVE('',#43121,#43123,#26790,.T.);
#57422=EDGE_CURVE('',#43125,#43126,#30621,.T.);
#57423=EDGE_CURVE('',#43126,#43124,#26791,.T.);
#57424=EDGE_CURVE('',#43123,#43125,#26792,.T.);
#57425=EDGE_CURVE('',#43127,#43128,#30622,.T.);
#57426=EDGE_CURVE('',#43127,#43129,#26793,.T.);
#57427=EDGE_CURVE('',#43130,#43129,#23376,.T.);
#57428=EDGE_CURVE('',#43130,#43128,#26794,.T.);
#57429=EDGE_CURVE('',#43131,#43132,#30623,.T.);
#57430=EDGE_CURVE('',#43132,#43133,#26795,.T.);
#57431=EDGE_CURVE('',#43134,#43133,#23377,.T.);
#57432=EDGE_CURVE('',#43131,#43134,#26796,.T.);
#57433=EDGE_CURVE('',#43135,#43136,#30624,.T.);
#57434=EDGE_CURVE('',#43136,#43132,#26797,.T.);
#57435=EDGE_CURVE('',#43135,#43131,#26798,.T.);
#57436=EDGE_CURVE('',#43137,#43138,#30625,.T.);
#57437=EDGE_CURVE('',#43138,#43136,#26799,.T.);
#57438=EDGE_CURVE('',#43137,#43135,#26800,.T.);
#57439=EDGE_CURVE('',#43139,#43140,#30626,.T.);
#57440=EDGE_CURVE('',#43140,#43138,#26801,.T.);
#57441=EDGE_CURVE('',#43139,#43137,#26802,.T.);
#57442=EDGE_CURVE('',#43141,#43142,#30627,.T.);
#57443=EDGE_CURVE('',#43142,#43140,#26803,.T.);
#57444=EDGE_CURVE('',#43141,#43139,#26804,.T.);
#57445=EDGE_CURVE('',#43143,#43144,#30628,.T.);
#57446=EDGE_CURVE('',#43144,#43142,#26805,.T.);
#57447=EDGE_CURVE('',#43143,#43141,#26806,.T.);
#57448=EDGE_CURVE('',#43145,#43146,#30629,.T.);
#57449=EDGE_CURVE('',#43146,#43144,#26807,.T.);
#57450=EDGE_CURVE('',#43145,#43143,#26808,.T.);
#57451=EDGE_CURVE('',#43147,#43148,#30630,.T.);
#57452=EDGE_CURVE('',#43149,#43147,#26809,.T.);
#57453=EDGE_CURVE('',#43150,#43149,#23378,.T.);
#57454=EDGE_CURVE('',#43150,#43148,#26810,.T.);
#57455=EDGE_CURVE('',#43151,#43152,#30631,.T.);
#57456=EDGE_CURVE('',#43153,#43152,#23379,.T.);
#57457=EDGE_CURVE('',#43153,#43151,#26811,.T.);
#57458=EDGE_CURVE('',#43154,#43155,#30632,.T.);
#57459=EDGE_CURVE('',#43155,#43156,#26812,.T.);
#57460=EDGE_CURVE('',#43152,#43156,#23380,.T.);
#57461=EDGE_CURVE('',#43151,#43154,#26813,.T.);
#57462=EDGE_CURVE('',#43157,#43158,#30633,.T.);
#57463=EDGE_CURVE('',#43158,#43155,#26814,.T.);
#57464=EDGE_CURVE('',#43154,#43157,#26815,.T.);
#57465=EDGE_CURVE('',#43159,#43160,#30634,.T.);
#57466=EDGE_CURVE('',#43160,#43158,#26816,.T.);
#57467=EDGE_CURVE('',#43157,#43159,#26817,.T.);
#57468=EDGE_CURVE('',#43161,#43162,#30635,.T.);
#57469=EDGE_CURVE('',#43162,#43160,#26818,.T.);
#57470=EDGE_CURVE('',#43159,#43161,#26819,.T.);
#57471=EDGE_CURVE('',#43163,#43164,#30636,.T.);
#57472=EDGE_CURVE('',#43164,#43162,#26820,.T.);
#57473=EDGE_CURVE('',#43161,#43163,#26821,.T.);
#57474=EDGE_CURVE('',#43165,#43166,#30637,.T.);
#57475=EDGE_CURVE('',#43166,#43164,#26822,.T.);
#57476=EDGE_CURVE('',#43163,#43165,#26823,.T.);
#57477=EDGE_CURVE('',#43167,#43168,#30638,.T.);
#57478=EDGE_CURVE('',#43167,#43169,#26824,.T.);
#57479=EDGE_CURVE('',#43170,#43169,#23381,.T.);
#57480=EDGE_CURVE('',#43170,#43168,#26825,.T.);
#57481=EDGE_CURVE('',#43171,#43172,#30639,.T.);
#57482=EDGE_CURVE('',#43172,#43173,#26826,.T.);
#57483=EDGE_CURVE('',#43174,#43173,#23382,.T.);
#57484=EDGE_CURVE('',#43171,#43174,#26827,.T.);
#57485=EDGE_CURVE('',#43175,#43176,#30640,.T.);
#57486=EDGE_CURVE('',#43176,#43172,#26828,.T.);
#57487=EDGE_CURVE('',#43175,#43171,#26829,.T.);
#57488=EDGE_CURVE('',#43177,#43178,#30641,.T.);
#57489=EDGE_CURVE('',#43178,#43176,#26830,.T.);
#57490=EDGE_CURVE('',#43177,#43175,#26831,.T.);
#57491=EDGE_CURVE('',#43179,#43180,#30642,.T.);
#57492=EDGE_CURVE('',#43180,#43178,#26832,.T.);
#57493=EDGE_CURVE('',#43179,#43177,#26833,.T.);
#57494=EDGE_CURVE('',#43181,#43182,#30643,.T.);
#57495=EDGE_CURVE('',#43182,#43180,#26834,.T.);
#57496=EDGE_CURVE('',#43181,#43179,#26835,.T.);
#57497=EDGE_CURVE('',#43183,#43184,#30644,.T.);
#57498=EDGE_CURVE('',#43184,#43182,#26836,.T.);
#57499=EDGE_CURVE('',#43183,#43181,#26837,.T.);
#57500=EDGE_CURVE('',#43185,#43186,#30645,.T.);
#57501=EDGE_CURVE('',#43186,#43184,#26838,.T.);
#57502=EDGE_CURVE('',#43185,#43183,#26839,.T.);
#57503=EDGE_CURVE('',#43187,#43188,#30646,.T.);
#57504=EDGE_CURVE('',#43189,#43187,#26840,.T.);
#57505=EDGE_CURVE('',#43190,#43189,#23383,.T.);
#57506=EDGE_CURVE('',#43190,#43188,#26841,.T.);
#57507=EDGE_CURVE('',#43191,#43192,#30647,.T.);
#57508=EDGE_CURVE('',#43193,#43192,#23384,.T.);
#57509=EDGE_CURVE('',#43193,#43191,#26842,.T.);
#57510=EDGE_CURVE('',#43194,#43195,#30648,.T.);
#57511=EDGE_CURVE('',#43195,#43196,#26843,.T.);
#57512=EDGE_CURVE('',#43192,#43196,#23385,.T.);
#57513=EDGE_CURVE('',#43191,#43194,#26844,.T.);
#57514=EDGE_CURVE('',#43197,#43198,#30649,.T.);
#57515=EDGE_CURVE('',#43198,#43195,#26845,.T.);
#57516=EDGE_CURVE('',#43194,#43197,#26846,.T.);
#57517=EDGE_CURVE('',#43199,#43200,#30650,.T.);
#57518=EDGE_CURVE('',#43200,#43198,#26847,.T.);
#57519=EDGE_CURVE('',#43197,#43199,#26848,.T.);
#57520=EDGE_CURVE('',#43201,#43202,#30651,.T.);
#57521=EDGE_CURVE('',#43202,#43200,#26849,.T.);
#57522=EDGE_CURVE('',#43199,#43201,#26850,.T.);
#57523=EDGE_CURVE('',#43203,#43204,#30652,.T.);
#57524=EDGE_CURVE('',#43204,#43202,#26851,.T.);
#57525=EDGE_CURVE('',#43201,#43203,#26852,.T.);
#57526=EDGE_CURVE('',#43205,#43206,#30653,.T.);
#57527=EDGE_CURVE('',#43206,#43204,#26853,.T.);
#57528=EDGE_CURVE('',#43203,#43205,#26854,.T.);
#57529=EDGE_CURVE('',#43207,#43208,#30654,.T.);
#57530=EDGE_CURVE('',#43207,#43209,#26855,.T.);
#57531=EDGE_CURVE('',#43210,#43209,#23386,.T.);
#57532=EDGE_CURVE('',#43210,#43208,#26856,.T.);
#57533=EDGE_CURVE('',#43211,#43212,#30655,.T.);
#57534=EDGE_CURVE('',#43212,#43213,#26857,.T.);
#57535=EDGE_CURVE('',#43214,#43213,#23387,.T.);
#57536=EDGE_CURVE('',#43211,#43214,#26858,.T.);
#57537=EDGE_CURVE('',#43215,#43216,#30656,.T.);
#57538=EDGE_CURVE('',#43216,#43212,#26859,.T.);
#57539=EDGE_CURVE('',#43215,#43211,#26860,.T.);
#57540=EDGE_CURVE('',#43217,#43218,#30657,.T.);
#57541=EDGE_CURVE('',#43218,#43216,#26861,.T.);
#57542=EDGE_CURVE('',#43217,#43215,#26862,.T.);
#57543=EDGE_CURVE('',#43219,#43220,#30658,.T.);
#57544=EDGE_CURVE('',#43220,#43218,#26863,.T.);
#57545=EDGE_CURVE('',#43219,#43217,#26864,.T.);
#57546=EDGE_CURVE('',#43221,#43222,#30659,.T.);
#57547=EDGE_CURVE('',#43222,#43220,#26865,.T.);
#57548=EDGE_CURVE('',#43221,#43219,#26866,.T.);
#57549=EDGE_CURVE('',#43223,#43224,#30660,.T.);
#57550=EDGE_CURVE('',#43224,#43222,#26867,.T.);
#57551=EDGE_CURVE('',#43223,#43221,#26868,.T.);
#57552=EDGE_CURVE('',#43225,#43226,#30661,.T.);
#57553=EDGE_CURVE('',#43226,#43224,#26869,.T.);
#57554=EDGE_CURVE('',#43225,#43223,#26870,.T.);
#57555=EDGE_CURVE('',#43227,#43228,#30662,.T.);
#57556=EDGE_CURVE('',#43229,#43227,#26871,.T.);
#57557=EDGE_CURVE('',#43230,#43229,#23388,.T.);
#57558=EDGE_CURVE('',#43230,#43228,#26872,.T.);
#57559=EDGE_CURVE('',#43231,#43232,#30663,.T.);
#57560=EDGE_CURVE('',#43233,#43232,#23389,.T.);
#57561=EDGE_CURVE('',#43233,#43231,#26873,.T.);
#57562=EDGE_CURVE('',#43234,#43235,#30664,.T.);
#57563=EDGE_CURVE('',#43235,#43236,#26874,.T.);
#57564=EDGE_CURVE('',#43232,#43236,#23390,.T.);
#57565=EDGE_CURVE('',#43231,#43234,#26875,.T.);
#57566=EDGE_CURVE('',#43237,#43238,#30665,.T.);
#57567=EDGE_CURVE('',#43238,#43235,#26876,.T.);
#57568=EDGE_CURVE('',#43234,#43237,#26877,.T.);
#57569=EDGE_CURVE('',#43239,#43240,#30666,.T.);
#57570=EDGE_CURVE('',#43240,#43238,#26878,.T.);
#57571=EDGE_CURVE('',#43237,#43239,#26879,.T.);
#57572=EDGE_CURVE('',#43241,#43242,#30667,.T.);
#57573=EDGE_CURVE('',#43242,#43240,#26880,.T.);
#57574=EDGE_CURVE('',#43239,#43241,#26881,.T.);
#57575=EDGE_CURVE('',#43243,#43244,#30668,.T.);
#57576=EDGE_CURVE('',#43244,#43242,#26882,.T.);
#57577=EDGE_CURVE('',#43241,#43243,#26883,.T.);
#57578=EDGE_CURVE('',#43245,#43246,#30669,.T.);
#57579=EDGE_CURVE('',#43246,#43244,#26884,.T.);
#57580=EDGE_CURVE('',#43243,#43245,#26885,.T.);
#57581=EDGE_CURVE('',#43247,#43248,#30670,.T.);
#57582=EDGE_CURVE('',#43247,#43249,#26886,.T.);
#57583=EDGE_CURVE('',#43250,#43249,#23391,.T.);
#57584=EDGE_CURVE('',#43250,#43248,#26887,.T.);
#57585=EDGE_CURVE('',#43251,#43252,#30671,.T.);
#57586=EDGE_CURVE('',#43252,#43253,#26888,.T.);
#57587=EDGE_CURVE('',#43254,#43253,#23392,.T.);
#57588=EDGE_CURVE('',#43251,#43254,#26889,.T.);
#57589=EDGE_CURVE('',#43255,#43256,#30672,.T.);
#57590=EDGE_CURVE('',#43256,#43252,#26890,.T.);
#57591=EDGE_CURVE('',#43255,#43251,#26891,.T.);
#57592=EDGE_CURVE('',#43257,#43258,#30673,.T.);
#57593=EDGE_CURVE('',#43258,#43256,#26892,.T.);
#57594=EDGE_CURVE('',#43257,#43255,#26893,.T.);
#57595=EDGE_CURVE('',#43259,#43260,#30674,.T.);
#57596=EDGE_CURVE('',#43260,#43258,#26894,.T.);
#57597=EDGE_CURVE('',#43259,#43257,#26895,.T.);
#57598=EDGE_CURVE('',#43261,#43262,#30675,.T.);
#57599=EDGE_CURVE('',#43262,#43260,#26896,.T.);
#57600=EDGE_CURVE('',#43261,#43259,#26897,.T.);
#57601=EDGE_CURVE('',#43263,#43264,#30676,.T.);
#57602=EDGE_CURVE('',#43264,#43262,#26898,.T.);
#57603=EDGE_CURVE('',#43263,#43261,#26899,.T.);
#57604=EDGE_CURVE('',#43265,#43266,#30677,.T.);
#57605=EDGE_CURVE('',#43266,#43264,#26900,.T.);
#57606=EDGE_CURVE('',#43265,#43263,#26901,.T.);
#57607=EDGE_CURVE('',#43267,#43268,#30678,.T.);
#57608=EDGE_CURVE('',#43269,#43267,#26902,.T.);
#57609=EDGE_CURVE('',#43270,#43269,#23393,.T.);
#57610=EDGE_CURVE('',#43270,#43268,#26903,.T.);
#57611=EDGE_CURVE('',#43271,#43271,#23394,.T.);
#57612=EDGE_CURVE('',#43271,#43272,#30679,.T.);
#57613=EDGE_CURVE('',#43272,#43272,#23395,.T.);
#57614=EDGE_CURVE('',#43273,#43274,#23396,.T.);
#57615=EDGE_CURVE('',#43274,#43273,#23397,.T.);
#57616=EDGE_CURVE('',#43273,#43272,#30680,.T.);
#57617=EDGE_CURVE('',#43275,#43275,#23398,.T.);
#57618=EDGE_CURVE('',#43269,#43250,#26904,.T.);
#57619=EDGE_CURVE('',#43249,#43270,#26905,.T.);
#57620=EDGE_CURVE('',#43229,#43210,#26906,.T.);
#57621=EDGE_CURVE('',#43209,#43230,#26907,.T.);
#57622=EDGE_CURVE('',#43189,#43170,#26908,.T.);
#57623=EDGE_CURVE('',#43169,#43190,#26909,.T.);
#57624=EDGE_CURVE('',#43149,#43130,#26910,.T.);
#57625=EDGE_CURVE('',#43129,#43150,#26911,.T.);
#57626=EDGE_CURVE('',#43268,#43266,#26912,.T.);
#57627=EDGE_CURVE('',#43267,#43265,#26913,.T.);
#57628=EDGE_CURVE('',#43253,#43233,#26914,.T.);
#57629=EDGE_CURVE('',#43245,#43247,#26915,.T.);
#57630=EDGE_CURVE('',#43236,#43254,#26916,.T.);
#57631=EDGE_CURVE('',#43248,#43246,#26917,.T.);
#57632=EDGE_CURVE('',#43276,#43276,#23399,.F.);
#57633=EDGE_CURVE('',#43133,#43113,#26918,.T.);
#57634=EDGE_CURVE('',#43116,#43134,#26919,.T.);
#57635=EDGE_CURVE('',#43173,#43153,#26920,.T.);
#57636=EDGE_CURVE('',#43156,#43174,#26921,.T.);
#57637=EDGE_CURVE('',#43213,#43193,#26922,.T.);
#57638=EDGE_CURVE('',#43196,#43214,#26923,.T.);
#57639=EDGE_CURVE('',#43277,#43277,#23400,.T.);
#57640=EDGE_CURVE('',#43278,#43278,#23401,.T.);
#57641=EDGE_CURVE('',#43278,#43279,#30681,.T.);
#57642=EDGE_CURVE('',#43279,#43279,#23402,.T.);
#57643=EDGE_CURVE('',#43274,#43280,#30682,.T.);
#57644=EDGE_CURVE('',#43280,#43280,#23403,.T.);
#57645=EDGE_CURVE('',#43280,#43281,#30683,.T.);
#57646=EDGE_CURVE('',#43281,#43281,#23404,.T.);
#57647=EDGE_CURVE('',#43282,#43282,#23405,.F.);
#57648=EDGE_CURVE('',#43282,#43275,#30684,.T.);
#57649=EDGE_CURVE('',#43276,#43283,#30685,.T.);
#57650=EDGE_CURVE('',#43283,#43283,#23406,.T.);
#57651=EDGE_CURVE('',#43284,#43284,#23407,.T.);
#57652=EDGE_CURVE('',#43284,#43277,#30686,.T.);
#57653=EDGE_CURVE('',#43285,#43285,#23408,.F.);
#57654=EDGE_CURVE('',#43285,#43286,#30687,.T.);
#57655=EDGE_CURVE('',#43286,#43286,#23409,.T.);
#57656=EDGE_CURVE('',#43287,#43287,#23410,.T.);
#57657=EDGE_CURVE('',#43287,#43288,#30688,.T.);
#57658=EDGE_CURVE('',#43288,#43288,#23411,.T.);
#57659=EDGE_CURVE('',#43289,#43289,#23412,.F.);
#57660=EDGE_CURVE('',#43289,#43290,#30689,.T.);
#57661=EDGE_CURVE('',#43290,#43290,#23413,.T.);
#57662=EDGE_CURVE('',#43291,#43291,#23414,.T.);
#57663=EDGE_CURVE('',#43291,#43292,#30690,.T.);
#57664=EDGE_CURVE('',#43292,#43292,#23415,.T.);
#57665=EDGE_CURVE('',#43293,#43293,#23416,.F.);
#57666=EDGE_CURVE('',#43293,#43294,#30691,.T.);
#57667=EDGE_CURVE('',#43294,#43294,#23417,.T.);
#57668=EDGE_CURVE('',#43295,#43295,#23418,.T.);
#57669=EDGE_CURVE('',#43295,#43296,#30692,.T.);
#57670=EDGE_CURVE('',#43296,#43296,#23419,.T.);
#57671=EDGE_CURVE('',#43297,#43297,#23420,.F.);
#57672=EDGE_CURVE('',#43297,#43298,#30693,.T.);
#57673=EDGE_CURVE('',#43298,#43298,#23421,.T.);
#57674=EDGE_CURVE('',#43299,#43299,#23422,.T.);
#57675=EDGE_CURVE('',#43299,#43300,#30694,.T.);
#57676=EDGE_CURVE('',#43300,#43300,#23423,.T.);
#57677=EDGE_CURVE('',#43301,#43301,#23424,.F.);
#57678=EDGE_CURVE('',#43301,#43302,#30695,.T.);
#57679=EDGE_CURVE('',#43302,#43302,#23425,.T.);
#57680=EDGE_CURVE('',#43303,#43303,#23426,.T.);
#57681=EDGE_CURVE('',#43303,#43304,#30696,.T.);
#57682=EDGE_CURVE('',#43304,#43304,#23427,.T.);
#57683=EDGE_CURVE('',#43305,#43305,#23428,.F.);
#57684=EDGE_CURVE('',#43305,#43306,#30697,.T.);
#57685=EDGE_CURVE('',#43306,#43306,#23429,.T.);
#57686=EDGE_CURVE('',#43307,#43307,#23430,.T.);
#57687=EDGE_CURVE('',#43307,#43308,#30698,.T.);
#57688=EDGE_CURVE('',#43308,#43308,#23431,.T.);
#57689=EDGE_CURVE('',#43309,#43309,#23432,.F.);
#57690=EDGE_CURVE('',#43309,#43310,#30699,.T.);
#57691=EDGE_CURVE('',#43310,#43310,#23433,.T.);
#57692=EDGE_CURVE('',#43311,#43311,#23434,.T.);
#57693=EDGE_CURVE('',#43311,#43312,#30700,.T.);
#57694=EDGE_CURVE('',#43312,#43312,#23435,.T.);
#57695=EDGE_CURVE('',#43313,#43313,#23436,.F.);
#57696=EDGE_CURVE('',#43313,#43314,#30701,.T.);
#57697=EDGE_CURVE('',#43314,#43314,#23437,.T.);
#57698=EDGE_CURVE('',#43315,#43315,#23438,.T.);
#57699=EDGE_CURVE('',#43315,#43316,#30702,.T.);
#57700=EDGE_CURVE('',#43316,#43316,#23439,.T.);
#57701=EDGE_CURVE('',#43317,#43317,#23440,.F.);
#57702=EDGE_CURVE('',#43317,#43318,#30703,.T.);
#57703=EDGE_CURVE('',#43318,#43318,#23441,.T.);
#57704=EDGE_CURVE('',#43228,#43226,#26924,.T.);
#57705=EDGE_CURVE('',#43227,#43225,#26925,.T.);
#57706=EDGE_CURVE('',#43205,#43207,#26926,.T.);
#57707=EDGE_CURVE('',#43208,#43206,#26927,.T.);
#57708=EDGE_CURVE('',#43188,#43186,#26928,.T.);
#57709=EDGE_CURVE('',#43187,#43185,#26929,.T.);
#57710=EDGE_CURVE('',#43165,#43167,#26930,.T.);
#57711=EDGE_CURVE('',#43168,#43166,#26931,.T.);
#57712=EDGE_CURVE('',#43148,#43146,#26932,.T.);
#57713=EDGE_CURVE('',#43147,#43145,#26933,.T.);
#57714=EDGE_CURVE('',#43125,#43127,#26934,.T.);
#57715=EDGE_CURVE('',#43128,#43126,#26935,.T.);
#57716=EDGE_CURVE('',#43319,#43320,#30704,.T.);
#57717=EDGE_CURVE('',#43319,#43321,#26936,.T.);
#57718=EDGE_CURVE('',#43321,#43322,#23442,.F.);
#57719=EDGE_CURVE('',#43322,#43320,#26937,.T.);
#57720=EDGE_CURVE('',#43323,#43324,#30705,.T.);
#57721=EDGE_CURVE('',#43323,#43319,#26938,.T.);
#57722=EDGE_CURVE('',#43320,#43324,#26939,.T.);
#57723=EDGE_CURVE('',#43325,#43326,#30706,.T.);
#57724=EDGE_CURVE('',#43325,#43323,#26940,.T.);
#57725=EDGE_CURVE('',#43324,#43326,#26941,.T.);
#57726=EDGE_CURVE('',#43327,#43328,#30707,.T.);
#57727=EDGE_CURVE('',#43327,#43325,#26942,.T.);
#57728=EDGE_CURVE('',#43326,#43328,#26943,.T.);
#57729=EDGE_CURVE('',#43329,#43330,#30708,.T.);
#57730=EDGE_CURVE('',#43329,#43327,#26944,.T.);
#57731=EDGE_CURVE('',#43328,#43330,#26945,.T.);
#57732=EDGE_CURVE('',#43331,#43332,#30709,.T.);
#57733=EDGE_CURVE('',#43331,#43329,#26946,.T.);
#57734=EDGE_CURVE('',#43330,#43332,#26947,.T.);
#57735=EDGE_CURVE('',#43333,#43334,#30710,.T.);
#57736=EDGE_CURVE('',#43333,#43331,#26948,.T.);
#57737=EDGE_CURVE('',#43332,#43334,#26949,.T.);
#57738=EDGE_CURVE('',#43335,#43336,#30711,.T.);
#57739=EDGE_CURVE('',#43335,#43333,#26950,.T.);
#57740=EDGE_CURVE('',#43334,#43336,#26951,.T.);
#57741=EDGE_CURVE('',#43337,#43338,#30712,.T.);
#57742=EDGE_CURVE('',#43337,#43335,#26952,.T.);
#57743=EDGE_CURVE('',#43336,#43338,#26953,.T.);
#57744=EDGE_CURVE('',#43339,#43340,#30713,.T.);
#57745=EDGE_CURVE('',#43339,#43337,#26954,.T.);
#57746=EDGE_CURVE('',#43338,#43340,#26955,.T.);
#57747=EDGE_CURVE('',#43341,#43342,#30714,.T.);
#57748=EDGE_CURVE('',#43341,#43343,#26956,.T.);
#57749=EDGE_CURVE('',#43342,#43343,#23443,.T.);
#57750=EDGE_CURVE('',#43344,#43345,#30715,.T.);
#57751=EDGE_CURVE('',#43344,#43341,#26957,.T.);
#57752=EDGE_CURVE('',#43346,#43342,#23444,.T.);
#57753=EDGE_CURVE('',#43345,#43346,#26958,.T.);
#57754=EDGE_CURVE('',#43347,#43348,#30716,.T.);
#57755=EDGE_CURVE('',#43347,#43344,#26959,.T.);
#57756=EDGE_CURVE('',#43348,#43345,#26960,.T.);
#57757=EDGE_CURVE('',#43349,#43350,#30717,.T.);
#57758=EDGE_CURVE('',#43349,#43347,#26961,.T.);
#57759=EDGE_CURVE('',#43350,#43348,#26962,.T.);
#57760=EDGE_CURVE('',#43351,#43352,#30718,.T.);
#57761=EDGE_CURVE('',#43351,#43349,#26963,.T.);
#57762=EDGE_CURVE('',#43352,#43350,#26964,.T.);
#57763=EDGE_CURVE('',#43353,#43354,#30719,.T.);
#57764=EDGE_CURVE('',#43353,#43351,#26965,.T.);
#57765=EDGE_CURVE('',#43354,#43352,#26966,.T.);
#57766=EDGE_CURVE('',#43355,#43356,#30720,.T.);
#57767=EDGE_CURVE('',#43355,#43353,#26967,.T.);
#57768=EDGE_CURVE('',#43356,#43354,#26968,.T.);
#57769=EDGE_CURVE('',#43357,#43358,#30721,.T.);
#57770=EDGE_CURVE('',#43357,#43355,#26969,.T.);
#57771=EDGE_CURVE('',#43358,#43356,#26970,.T.);
#57772=EDGE_CURVE('',#43359,#43360,#30722,.T.);
#57773=EDGE_CURVE('',#43359,#43357,#26971,.T.);
#57774=EDGE_CURVE('',#43360,#43358,#26972,.T.);
#57775=EDGE_CURVE('',#43361,#43362,#30723,.T.);
#57776=EDGE_CURVE('',#43361,#43359,#26973,.T.);
#57777=EDGE_CURVE('',#43362,#43360,#26974,.T.);
#57778=EDGE_CURVE('',#43363,#43364,#30724,.T.);
#57779=EDGE_CURVE('',#43363,#43365,#26975,.T.);
#57780=EDGE_CURVE('',#43366,#43365,#23445,.T.);
#57781=EDGE_CURVE('',#43366,#43364,#26976,.T.);
#57782=EDGE_CURVE('',#43367,#43368,#30725,.T.);
#57783=EDGE_CURVE('',#43367,#43363,#26977,.T.);
#57784=EDGE_CURVE('',#43364,#43368,#26978,.T.);
#57785=EDGE_CURVE('',#43369,#43370,#30726,.T.);
#57786=EDGE_CURVE('',#43369,#43367,#26979,.T.);
#57787=EDGE_CURVE('',#43368,#43370,#26980,.T.);
#57788=EDGE_CURVE('',#43371,#43372,#30727,.T.);
#57789=EDGE_CURVE('',#43371,#43369,#26981,.T.);
#57790=EDGE_CURVE('',#43370,#43372,#26982,.T.);
#57791=EDGE_CURVE('',#43373,#43374,#30728,.T.);
#57792=EDGE_CURVE('',#43373,#43371,#26983,.T.);
#57793=EDGE_CURVE('',#43372,#43374,#26984,.T.);
#57794=EDGE_CURVE('',#43375,#43376,#30729,.T.);
#57795=EDGE_CURVE('',#43375,#43377,#26985,.T.);
#57796=EDGE_CURVE('',#43378,#43377,#23446,.T.);
#57797=EDGE_CURVE('',#43376,#43378,#26986,.T.);
#57798=EDGE_CURVE('',#43379,#43380,#30730,.T.);
#57799=EDGE_CURVE('',#43379,#43375,#26987,.T.);
#57800=EDGE_CURVE('',#43380,#43376,#26988,.T.);
#57801=EDGE_CURVE('',#43381,#43382,#30731,.T.);
#57802=EDGE_CURVE('',#43381,#43379,#26989,.T.);
#57803=EDGE_CURVE('',#43382,#43380,#26990,.T.);
#57804=EDGE_CURVE('',#43383,#43384,#30732,.T.);
#57805=EDGE_CURVE('',#43383,#43381,#26991,.T.);
#57806=EDGE_CURVE('',#43384,#43382,#26992,.T.);
#57807=EDGE_CURVE('',#43385,#43386,#30733,.T.);
#57808=EDGE_CURVE('',#43385,#43383,#26993,.T.);
#57809=EDGE_CURVE('',#43386,#43384,#26994,.T.);
#57810=EDGE_CURVE('',#43387,#43378,#26995,.T.);
#57811=EDGE_CURVE('',#43374,#43387,#26996,.T.);
#57812=EDGE_CURVE('',#43388,#43366,#26997,.T.);
#57813=EDGE_CURVE('',#43388,#43386,#26998,.T.);
#57814=EDGE_CURVE('',#43389,#43388,#23447,.T.);
#57815=EDGE_CURVE('',#43389,#43385,#26999,.T.);
#57816=EDGE_CURVE('',#43377,#43390,#27000,.T.);
#57817=EDGE_CURVE('',#43365,#43389,#27001,.T.);
#57818=EDGE_CURVE('',#43390,#43373,#27002,.T.);
#57819=EDGE_CURVE('',#43390,#43387,#23448,.T.);
#57820=EDGE_CURVE('',#43391,#43391,#23449,.T.);
#57821=EDGE_CURVE('',#43392,#43393,#23450,.T.);
#57822=EDGE_CURVE('',#43392,#43346,#27003,.T.);
#57823=EDGE_CURVE('',#43343,#43394,#27004,.T.);
#57824=EDGE_CURVE('',#43393,#43394,#23451,.T.);
#57825=EDGE_CURVE('',#43395,#43392,#27005,.T.);
#57826=EDGE_CURVE('',#43340,#43395,#27006,.T.);
#57827=EDGE_CURVE('',#43396,#43322,#27007,.T.);
#57828=EDGE_CURVE('',#43396,#43362,#27008,.T.);
#57829=EDGE_CURVE('',#43397,#43396,#23452,.T.);
#57830=EDGE_CURVE('',#43397,#43361,#27009,.T.);
#57831=EDGE_CURVE('',#43321,#43397,#27010,.T.);
#57832=EDGE_CURVE('',#43398,#43339,#27011,.T.);
#57833=EDGE_CURVE('',#43394,#43398,#27012,.T.);
#57834=EDGE_CURVE('',#43399,#43400,#23453,.T.);
#57835=EDGE_CURVE('',#43400,#43399,#23454,.T.);
#57836=EDGE_CURVE('',#43400,#43401,#30734,.T.);
#57837=EDGE_CURVE('',#43401,#43401,#23455,.T.);
#57838=EDGE_CURVE('',#43402,#43402,#23456,.T.);
#57839=EDGE_CURVE('',#43402,#43391,#30735,.T.);
#57840=EDGE_CURVE('',#43398,#43395,#23457,.T.);
#57841=EDGE_CURVE('',#43399,#43393,#30736,.T.);
#57842=EDGE_CURVE('',#43394,#43392,#23458,.T.);
#57843=EDGE_CURVE('',#43403,#43403,#23459,.T.);
#57844=EDGE_CURVE('',#43403,#43404,#30737,.T.);
#57845=EDGE_CURVE('',#43404,#43404,#23460,.T.);
#57846=EDGE_CURVE('',#43405,#43405,#23461,.T.);
#57847=EDGE_CURVE('',#43405,#43403,#30738,.T.);
#57848=EDGE_CURVE('',#43406,#43406,#23462,.T.);
#57849=EDGE_CURVE('',#43406,#43405,#30739,.T.);
#57850=EDGE_CURVE('',#43407,#43407,#23463,.T.);
#57851=EDGE_CURVE('',#43408,#43408,#23464,.T.);
#57852=EDGE_CURVE('',#43409,#43409,#23465,.T.);
#57853=EDGE_CURVE('',#43409,#43408,#30740,.T.);
#57854=EDGE_CURVE('',#43410,#43410,#23466,.T.);
#57855=EDGE_CURVE('',#43410,#43407,#30741,.T.);
#57856=EDGE_CURVE('',#43411,#43412,#30742,.T.);
#57857=EDGE_CURVE('',#43411,#43413,#27013,.T.);
#57858=EDGE_CURVE('',#43413,#43414,#23467,.F.);
#57859=EDGE_CURVE('',#43414,#43412,#27014,.T.);
#57860=EDGE_CURVE('',#43415,#43416,#30743,.T.);
#57861=EDGE_CURVE('',#43415,#43411,#27015,.T.);
#57862=EDGE_CURVE('',#43412,#43416,#27016,.T.);
#57863=EDGE_CURVE('',#43417,#43418,#30744,.T.);
#57864=EDGE_CURVE('',#43417,#43415,#27017,.T.);
#57865=EDGE_CURVE('',#43416,#43418,#27018,.T.);
#57866=EDGE_CURVE('',#43419,#43420,#30745,.T.);
#57867=EDGE_CURVE('',#43419,#43417,#27019,.T.);
#57868=EDGE_CURVE('',#43418,#43420,#27020,.T.);
#57869=EDGE_CURVE('',#43421,#43422,#30746,.T.);
#57870=EDGE_CURVE('',#43421,#43419,#27021,.T.);
#57871=EDGE_CURVE('',#43420,#43422,#27022,.T.);
#57872=EDGE_CURVE('',#43423,#43424,#30747,.T.);
#57873=EDGE_CURVE('',#43423,#43421,#27023,.T.);
#57874=EDGE_CURVE('',#43422,#43424,#27024,.T.);
#57875=EDGE_CURVE('',#43425,#43426,#30748,.T.);
#57876=EDGE_CURVE('',#43425,#43427,#27025,.T.);
#57877=EDGE_CURVE('',#43428,#43427,#23468,.T.);
#57878=EDGE_CURVE('',#43426,#43428,#27026,.T.);
#57879=EDGE_CURVE('',#43429,#43430,#30749,.T.);
#57880=EDGE_CURVE('',#43429,#43425,#27027,.T.);
#57881=EDGE_CURVE('',#43430,#43426,#27028,.T.);
#57882=EDGE_CURVE('',#43431,#43432,#30750,.T.);
#57883=EDGE_CURVE('',#43431,#43429,#27029,.T.);
#57884=EDGE_CURVE('',#43432,#43430,#27030,.T.);
#57885=EDGE_CURVE('',#43433,#43434,#30751,.T.);
#57886=EDGE_CURVE('',#43433,#43431,#27031,.T.);
#57887=EDGE_CURVE('',#43434,#43432,#27032,.T.);
#57888=EDGE_CURVE('',#43435,#43436,#30752,.T.);
#57889=EDGE_CURVE('',#43435,#43433,#27033,.T.);
#57890=EDGE_CURVE('',#43436,#43434,#27034,.T.);
#57891=EDGE_CURVE('',#43437,#43438,#30753,.T.);
#57892=EDGE_CURVE('',#43437,#43435,#27035,.T.);
#57893=EDGE_CURVE('',#43438,#43436,#27036,.T.);
#57894=EDGE_CURVE('',#43439,#43428,#27037,.T.);
#57895=EDGE_CURVE('',#43424,#43439,#27038,.T.);
#57896=EDGE_CURVE('',#43440,#43414,#27039,.T.);
#57897=EDGE_CURVE('',#43441,#43440,#27040,.T.);
#57898=EDGE_CURVE('',#43441,#43438,#27041,.T.);
#57899=EDGE_CURVE('',#43440,#43442,#23469,.T.);
#57900=EDGE_CURVE('',#43442,#43443,#27042,.T.);
#57901=EDGE_CURVE('',#43443,#43441,#23470,.T.);
#57902=EDGE_CURVE('',#43443,#43437,#27043,.T.);
#57903=EDGE_CURVE('',#43427,#43444,#27044,.T.);
#57904=EDGE_CURVE('',#43413,#43442,#27045,.T.);
#57905=EDGE_CURVE('',#43444,#43423,#27046,.T.);
#57906=EDGE_CURVE('',#43442,#43445,#23471,.T.);
#57907=EDGE_CURVE('',#43445,#43440,#23472,.T.);
#57908=EDGE_CURVE('',#43444,#43439,#23473,.T.);
#57909=EDGE_CURVE('',#43446,#43446,#23474,.T.);
#57910=EDGE_CURVE('',#43447,#43447,#23475,.T.);
#57911=EDGE_CURVE('',#43447,#43448,#30754,.T.);
#57912=EDGE_CURVE('',#43448,#43449,#23476,.T.);
#57913=EDGE_CURVE('',#43449,#43448,#23477,.T.);
#57914=EDGE_CURVE('',#43450,#43450,#23478,.T.);
#57915=EDGE_CURVE('',#43450,#43447,#30755,.T.);
#57916=EDGE_CURVE('',#43451,#43451,#23479,.T.);
#57917=EDGE_CURVE('',#43451,#43450,#30756,.T.);
#57918=EDGE_CURVE('',#43452,#43452,#23480,.T.);
#57919=EDGE_CURVE('',#43452,#43453,#30757,.T.);
#57920=EDGE_CURVE('',#43453,#43453,#23481,.T.);
#57921=EDGE_CURVE('',#43445,#43454,#30758,.T.);
#57922=EDGE_CURVE('',#43454,#43454,#23482,.T.);
#57923=EDGE_CURVE('',#43455,#43456,#23483,.T.);
#57924=EDGE_CURVE('',#43456,#43455,#23484,.T.);
#57925=EDGE_CURVE('',#43456,#43446,#30759,.T.);
#57926=EDGE_CURVE('',#43455,#43449,#30760,.T.);
#57927=EDGE_CURVE('',#43457,#43457,#23485,.T.);
#57928=EDGE_CURVE('',#43457,#43451,#30761,.T.);
#57929=EDGE_CURVE('',#43458,#43459,#30762,.T.);
#57930=EDGE_CURVE('',#43460,#43458,#30763,.T.);
#57931=EDGE_CURVE('',#43461,#43460,#30764,.T.);
#57932=EDGE_CURVE('',#43462,#43461,#30765,.T.);
#57933=EDGE_CURVE('',#43463,#43462,#30766,.T.);
#57934=EDGE_CURVE('',#43459,#43463,#30767,.T.);
#57935=EDGE_CURVE('',#43464,#43465,#30768,.T.);
#57936=EDGE_CURVE('',#43465,#43466,#30769,.T.);
#57937=EDGE_CURVE('',#43466,#43467,#30770,.T.);
#57938=EDGE_CURVE('',#43467,#43468,#30771,.T.);
#57939=EDGE_CURVE('',#43468,#43469,#30772,.T.);
#57940=EDGE_CURVE('',#43469,#43464,#30773,.T.);
#57941=EDGE_CURVE('',#43465,#43459,#30774,.T.);
#57942=EDGE_CURVE('',#43464,#43458,#30775,.T.);
#57943=EDGE_CURVE('',#43466,#43463,#30776,.T.);
#57944=EDGE_CURVE('',#43467,#43462,#30777,.T.);
#57945=EDGE_CURVE('',#43468,#43461,#30778,.T.);
#57946=EDGE_CURVE('',#43469,#43460,#30779,.T.);
#57947=EDGE_CURVE('',#43470,#43470,#23486,.T.);
#57948=EDGE_CURVE('',#43470,#43471,#30780,.T.);
#57949=EDGE_CURVE('',#43471,#43471,#23487,.T.);
#57950=EDGE_CURVE('',#43472,#43472,#23488,.T.);
#57951=EDGE_CURVE('',#43472,#43473,#30781,.T.);
#57952=EDGE_CURVE('',#43473,#43473,#23489,.T.);
#57953=EDGE_CURVE('',#43474,#43474,#23490,.T.);
#57954=EDGE_CURVE('',#43474,#43475,#30782,.T.);
#57955=EDGE_CURVE('',#43475,#43475,#23491,.T.);
#57956=EDGE_CURVE('',#43476,#43476,#23492,.T.);
#57957=EDGE_CURVE('',#43476,#43477,#30783,.T.);
#57958=EDGE_CURVE('',#43477,#43477,#23493,.T.);
#57959=EDGE_CURVE('',#43478,#43478,#23494,.T.);
#57960=EDGE_CURVE('',#43478,#43479,#30784,.T.);
#57961=EDGE_CURVE('',#43479,#43479,#23495,.T.);
#57962=EDGE_CURVE('',#43480,#43481,#23496,.T.);
#57963=EDGE_CURVE('',#43480,#43482,#30785,.T.);
#57964=EDGE_CURVE('',#43482,#43483,#23497,.T.);
#57965=EDGE_CURVE('',#43481,#43483,#30786,.T.);
#57966=EDGE_CURVE('',#43484,#43485,#30787,.T.);
#57967=EDGE_CURVE('',#43485,#43486,#30788,.T.);
#57968=EDGE_CURVE('',#43487,#43486,#30789,.T.);
#57969=EDGE_CURVE('',#43487,#43484,#30790,.T.);
#57970=EDGE_CURVE('',#43488,#43489,#30791,.T.);
#57971=EDGE_CURVE('',#43489,#43490,#30792,.T.);
#57972=EDGE_CURVE('',#43490,#43491,#30793,.T.);
#57973=EDGE_CURVE('',#43491,#43488,#30794,.T.);
#57974=EDGE_CURVE('',#43492,#43482,#30795,.T.);
#57975=EDGE_CURVE('',#43492,#43493,#30796,.T.);
#57976=EDGE_CURVE('',#43493,#43494,#30797,.T.);
#57977=EDGE_CURVE('',#43494,#43495,#30798,.T.);
#57978=EDGE_CURVE('',#43495,#43496,#30799,.T.);
#57979=EDGE_CURVE('',#43496,#43497,#30800,.T.);
#57980=EDGE_CURVE('',#43483,#43497,#30801,.T.);
#57981=EDGE_CURVE('',#43498,#43499,#30802,.T.);
#57982=EDGE_CURVE('',#43499,#43500,#30803,.T.);
#57983=EDGE_CURVE('',#43500,#43501,#30804,.T.);
#57984=EDGE_CURVE('',#43501,#43498,#30805,.T.);
#57985=EDGE_CURVE('',#43502,#43503,#30806,.T.);
#57986=EDGE_CURVE('',#43503,#43504,#30807,.T.);
#57987=EDGE_CURVE('',#43504,#43480,#30808,.T.);
#57988=EDGE_CURVE('',#43481,#43505,#30809,.T.);
#57989=EDGE_CURVE('',#43505,#43506,#30810,.T.);
#57990=EDGE_CURVE('',#43506,#43507,#30811,.T.);
#57991=EDGE_CURVE('',#43507,#43502,#30812,.T.);
#57992=EDGE_CURVE('',#43508,#43509,#30813,.T.);
#57993=EDGE_CURVE('',#43509,#43510,#30814,.T.);
#57994=EDGE_CURVE('',#43510,#43511,#30815,.T.);
#57995=EDGE_CURVE('',#43511,#43508,#30816,.T.);
#57996=EDGE_CURVE('',#43512,#43513,#30817,.T.);
#57997=EDGE_CURVE('',#43513,#43514,#30818,.T.);
#57998=EDGE_CURVE('',#43514,#43515,#30819,.T.);
#57999=EDGE_CURVE('',#43515,#43512,#30820,.T.);
#58000=EDGE_CURVE('',#43486,#43492,#30821,.T.);
#58001=EDGE_CURVE('',#43504,#43487,#30822,.T.);
#58002=EDGE_CURVE('',#43497,#43489,#30823,.T.);
#58003=EDGE_CURVE('',#43488,#43505,#30824,.T.);
#58004=EDGE_CURVE('',#43506,#43491,#30825,.T.);
#58005=EDGE_CURVE('',#43484,#43503,#30826,.T.);
#58006=EDGE_CURVE('',#43506,#43511,#30827,.T.);
#58007=EDGE_CURVE('',#43511,#43491,#30828,.T.);
#58008=EDGE_CURVE('',#43484,#43512,#30829,.T.);
#58009=EDGE_CURVE('',#43512,#43503,#30830,.T.);
#58010=EDGE_CURVE('',#43490,#43496,#30831,.T.);
#58011=EDGE_CURVE('',#43508,#43490,#30832,.T.);
#58012=EDGE_CURVE('',#43507,#43510,#30833,.T.);
#58013=EDGE_CURVE('',#43502,#43501,#30834,.T.);
#58014=EDGE_CURVE('',#43498,#43507,#30835,.T.);
#58015=EDGE_CURVE('',#43513,#43502,#30836,.T.);
#58016=EDGE_CURVE('',#43485,#43515,#30837,.T.);
#58017=EDGE_CURVE('',#43493,#43485,#30838,.T.);
#58018=EDGE_CURVE('',#43508,#43496,#30839,.T.);
#58019=EDGE_CURVE('',#43498,#43510,#30840,.T.);
#58020=EDGE_CURVE('',#43513,#43501,#30841,.T.);
#58021=EDGE_CURVE('',#43493,#43515,#30842,.T.);
#58022=EDGE_CURVE('',#43509,#43495,#30843,.T.);
#58023=EDGE_CURVE('',#43499,#43509,#30844,.T.);
#58024=EDGE_CURVE('',#43514,#43500,#30845,.T.);
#58025=EDGE_CURVE('',#43494,#43514,#30846,.T.);
#58026=EDGE_CURVE('',#43499,#43495,#30847,.T.);
#58027=EDGE_CURVE('',#43494,#43500,#30848,.T.);
#58028=ORIENTED_EDGE('',*,*,#43516,.T.);
#58029=ORIENTED_EDGE('',*,*,#43517,.T.);
#58030=ORIENTED_EDGE('',*,*,#43518,.T.);
#58031=ORIENTED_EDGE('',*,*,#43519,.F.);
#58032=ORIENTED_EDGE('',*,*,#43520,.T.);
#58033=ORIENTED_EDGE('',*,*,#43521,.T.);
#58034=ORIENTED_EDGE('',*,*,#43522,.T.);
#58035=ORIENTED_EDGE('',*,*,#43523,.T.);
#58036=ORIENTED_EDGE('',*,*,#43516,.F.);
#58037=ORIENTED_EDGE('',*,*,#43524,.T.);
#58038=ORIENTED_EDGE('',*,*,#43525,.T.);
#58039=ORIENTED_EDGE('',*,*,#43526,.T.);
#58040=ORIENTED_EDGE('',*,*,#43527,.T.);
#58041=ORIENTED_EDGE('',*,*,#43521,.F.);
#58042=ORIENTED_EDGE('',*,*,#43528,.T.);
#58043=ORIENTED_EDGE('',*,*,#43529,.F.);
#58044=ORIENTED_EDGE('',*,*,#43530,.T.);
#58045=ORIENTED_EDGE('',*,*,#43531,.T.);
#58046=ORIENTED_EDGE('',*,*,#43532,.T.);
#58047=ORIENTED_EDGE('',*,*,#43533,.T.);
#58048=ORIENTED_EDGE('',*,*,#43534,.T.);
#58049=ORIENTED_EDGE('',*,*,#43535,.T.);
#58050=ORIENTED_EDGE('',*,*,#43536,.F.);
#58051=ORIENTED_EDGE('',*,*,#43537,.T.);
#58052=ORIENTED_EDGE('',*,*,#43538,.T.);
#58053=ORIENTED_EDGE('',*,*,#43539,.T.);
#58054=ORIENTED_EDGE('',*,*,#43540,.T.);
#58055=ORIENTED_EDGE('',*,*,#43533,.F.);
#58056=ORIENTED_EDGE('',*,*,#43541,.T.);
#58057=ORIENTED_EDGE('',*,*,#43542,.T.);
#58058=ORIENTED_EDGE('',*,*,#43543,.T.);
#58059=ORIENTED_EDGE('',*,*,#43544,.T.);
#58060=ORIENTED_EDGE('',*,*,#43538,.F.);
#58061=ORIENTED_EDGE('',*,*,#43545,.T.);
#58062=ORIENTED_EDGE('',*,*,#43546,.F.);
#58063=ORIENTED_EDGE('',*,*,#43547,.T.);
#58064=ORIENTED_EDGE('',*,*,#43548,.T.);
#58065=ORIENTED_EDGE('',*,*,#43549,.T.);
#58066=ORIENTED_EDGE('',*,*,#43550,.T.);
#58067=ORIENTED_EDGE('',*,*,#43551,.T.);
#58068=ORIENTED_EDGE('',*,*,#43552,.F.);
#58069=ORIENTED_EDGE('',*,*,#43553,.F.);
#58070=ORIENTED_EDGE('',*,*,#43554,.T.);
#58071=ORIENTED_EDGE('',*,*,#43555,.T.);
#58072=ORIENTED_EDGE('',*,*,#43556,.T.);
#58073=ORIENTED_EDGE('',*,*,#43550,.F.);
#58074=ORIENTED_EDGE('',*,*,#43557,.F.);
#58075=ORIENTED_EDGE('',*,*,#43558,.F.);
#58076=ORIENTED_EDGE('',*,*,#43559,.T.);
#58077=ORIENTED_EDGE('',*,*,#43560,.T.);
#58078=ORIENTED_EDGE('',*,*,#43561,.T.);
#58079=ORIENTED_EDGE('',*,*,#43554,.F.);
#58080=ORIENTED_EDGE('',*,*,#43562,.F.);
#58081=ORIENTED_EDGE('',*,*,#43563,.F.);
#58082=ORIENTED_EDGE('',*,*,#43564,.F.);
#58083=ORIENTED_EDGE('',*,*,#43565,.F.);
#58084=ORIENTED_EDGE('',*,*,#43566,.F.);
#58085=ORIENTED_EDGE('',*,*,#43567,.F.);
#58086=ORIENTED_EDGE('',*,*,#43568,.T.);
#58087=ORIENTED_EDGE('',*,*,#43569,.T.);
#58088=ORIENTED_EDGE('',*,*,#43570,.T.);
#58089=ORIENTED_EDGE('',*,*,#43571,.F.);
#58090=ORIENTED_EDGE('',*,*,#43572,.F.);
#58091=ORIENTED_EDGE('',*,*,#43573,.T.);
#58092=ORIENTED_EDGE('',*,*,#43574,.T.);
#58093=ORIENTED_EDGE('',*,*,#43575,.T.);
#58094=ORIENTED_EDGE('',*,*,#43569,.F.);
#58095=ORIENTED_EDGE('',*,*,#43576,.F.);
#58096=ORIENTED_EDGE('',*,*,#43577,.F.);
#58097=ORIENTED_EDGE('',*,*,#43578,.T.);
#58098=ORIENTED_EDGE('',*,*,#43579,.T.);
#58099=ORIENTED_EDGE('',*,*,#43580,.T.);
#58100=ORIENTED_EDGE('',*,*,#43573,.F.);
#58101=ORIENTED_EDGE('',*,*,#43581,.F.);
#58102=ORIENTED_EDGE('',*,*,#43582,.F.);
#58103=ORIENTED_EDGE('',*,*,#43583,.F.);
#58104=ORIENTED_EDGE('',*,*,#43584,.F.);
#58105=ORIENTED_EDGE('',*,*,#43585,.F.);
#58106=ORIENTED_EDGE('',*,*,#43586,.F.);
#58107=ORIENTED_EDGE('',*,*,#43587,.T.);
#58108=ORIENTED_EDGE('',*,*,#43583,.T.);
#58109=ORIENTED_EDGE('',*,*,#43588,.T.);
#58110=ORIENTED_EDGE('',*,*,#43578,.F.);
#58111=ORIENTED_EDGE('',*,*,#43589,.F.);
#58112=ORIENTED_EDGE('',*,*,#43564,.T.);
#58113=ORIENTED_EDGE('',*,*,#43590,.T.);
#58114=ORIENTED_EDGE('',*,*,#43559,.F.);
#58115=ORIENTED_EDGE('',*,*,#43591,.F.);
#58116=ORIENTED_EDGE('',*,*,#43546,.T.);
#58117=ORIENTED_EDGE('',*,*,#43592,.T.);
#58118=ORIENTED_EDGE('',*,*,#43593,.T.);
#58119=ORIENTED_EDGE('',*,*,#43542,.F.);
#58120=ORIENTED_EDGE('',*,*,#43594,.T.);
#58121=ORIENTED_EDGE('',*,*,#43529,.T.);
#58122=ORIENTED_EDGE('',*,*,#43595,.T.);
#58123=ORIENTED_EDGE('',*,*,#43596,.T.);
#58124=ORIENTED_EDGE('',*,*,#43525,.F.);
#58125=ORIENTED_EDGE('',*,*,#43597,.T.);
#58126=ORIENTED_EDGE('',*,*,#43598,.F.);
#58127=ORIENTED_EDGE('',*,*,#43570,.F.);
#58128=ORIENTED_EDGE('',*,*,#43575,.F.);
#58129=ORIENTED_EDGE('',*,*,#43574,.F.);
#58130=ORIENTED_EDGE('',*,*,#43580,.F.);
#58131=ORIENTED_EDGE('',*,*,#43579,.F.);
#58132=ORIENTED_EDGE('',*,*,#43588,.F.);
#58133=ORIENTED_EDGE('',*,*,#43587,.F.);
#58134=ORIENTED_EDGE('',*,*,#43599,.F.);
#58135=ORIENTED_EDGE('',*,*,#43530,.F.);
#58136=ORIENTED_EDGE('',*,*,#43597,.F.);
#58137=ORIENTED_EDGE('',*,*,#43528,.F.);
#58138=ORIENTED_EDGE('',*,*,#43524,.F.);
#58139=ORIENTED_EDGE('',*,*,#43520,.F.);
#58140=ORIENTED_EDGE('',*,*,#43600,.F.);
#58141=ORIENTED_EDGE('',*,*,#43518,.F.);
#58142=ORIENTED_EDGE('',*,*,#43517,.F.);
#58143=ORIENTED_EDGE('',*,*,#43523,.F.);
#58144=ORIENTED_EDGE('',*,*,#43522,.F.);
#58145=ORIENTED_EDGE('',*,*,#43527,.F.);
#58146=ORIENTED_EDGE('',*,*,#43526,.F.);
#58147=ORIENTED_EDGE('',*,*,#43596,.F.);
#58148=ORIENTED_EDGE('',*,*,#43595,.F.);
#58149=ORIENTED_EDGE('',*,*,#43532,.F.);
#58150=ORIENTED_EDGE('',*,*,#43601,.T.);
#58151=ORIENTED_EDGE('',*,*,#43602,.F.);
#58152=ORIENTED_EDGE('',*,*,#43585,.T.);
#58153=ORIENTED_EDGE('',*,*,#43584,.T.);
#58154=ORIENTED_EDGE('',*,*,#43589,.T.);
#58155=ORIENTED_EDGE('',*,*,#43582,.T.);
#58156=ORIENTED_EDGE('',*,*,#43581,.T.);
#58157=ORIENTED_EDGE('',*,*,#43577,.T.);
#58158=ORIENTED_EDGE('',*,*,#43576,.T.);
#58159=ORIENTED_EDGE('',*,*,#43572,.T.);
#58160=ORIENTED_EDGE('',*,*,#43603,.F.);
#58161=ORIENTED_EDGE('',*,*,#43604,.F.);
#58162=ORIENTED_EDGE('',*,*,#43605,.F.);
#58163=ORIENTED_EDGE('',*,*,#43606,.F.);
#58164=ORIENTED_EDGE('',*,*,#43607,.F.);
#58165=ORIENTED_EDGE('',*,*,#43608,.F.);
#58166=ORIENTED_EDGE('',*,*,#43600,.T.);
#58167=ORIENTED_EDGE('',*,*,#43571,.T.);
#58168=ORIENTED_EDGE('',*,*,#43598,.T.);
#58169=ORIENTED_EDGE('',*,*,#43519,.T.);
#58170=ORIENTED_EDGE('',*,*,#43609,.F.);
#58171=ORIENTED_EDGE('',*,*,#43551,.F.);
#58172=ORIENTED_EDGE('',*,*,#43556,.F.);
#58173=ORIENTED_EDGE('',*,*,#43555,.F.);
#58174=ORIENTED_EDGE('',*,*,#43561,.F.);
#58175=ORIENTED_EDGE('',*,*,#43560,.F.);
#58176=ORIENTED_EDGE('',*,*,#43590,.F.);
#58177=ORIENTED_EDGE('',*,*,#43568,.F.);
#58178=ORIENTED_EDGE('',*,*,#43610,.F.);
#58179=ORIENTED_EDGE('',*,*,#43547,.F.);
#58180=ORIENTED_EDGE('',*,*,#43594,.F.);
#58181=ORIENTED_EDGE('',*,*,#43545,.F.);
#58182=ORIENTED_EDGE('',*,*,#43541,.F.);
#58183=ORIENTED_EDGE('',*,*,#43537,.F.);
#58184=ORIENTED_EDGE('',*,*,#43611,.F.);
#58185=ORIENTED_EDGE('',*,*,#43535,.F.);
#58186=ORIENTED_EDGE('',*,*,#43534,.F.);
#58187=ORIENTED_EDGE('',*,*,#43540,.F.);
#58188=ORIENTED_EDGE('',*,*,#43539,.F.);
#58189=ORIENTED_EDGE('',*,*,#43544,.F.);
#58190=ORIENTED_EDGE('',*,*,#43543,.F.);
#58191=ORIENTED_EDGE('',*,*,#43593,.F.);
#58192=ORIENTED_EDGE('',*,*,#43592,.F.);
#58193=ORIENTED_EDGE('',*,*,#43549,.F.);
#58194=ORIENTED_EDGE('',*,*,#43612,.T.);
#58195=ORIENTED_EDGE('',*,*,#43613,.F.);
#58196=ORIENTED_EDGE('',*,*,#43566,.T.);
#58197=ORIENTED_EDGE('',*,*,#43565,.T.);
#58198=ORIENTED_EDGE('',*,*,#43591,.T.);
#58199=ORIENTED_EDGE('',*,*,#43563,.T.);
#58200=ORIENTED_EDGE('',*,*,#43562,.T.);
#58201=ORIENTED_EDGE('',*,*,#43558,.T.);
#58202=ORIENTED_EDGE('',*,*,#43557,.T.);
#58203=ORIENTED_EDGE('',*,*,#43553,.T.);
#58204=ORIENTED_EDGE('',*,*,#43614,.F.);
#58205=ORIENTED_EDGE('',*,*,#43615,.F.);
#58206=ORIENTED_EDGE('',*,*,#43616,.F.);
#58207=ORIENTED_EDGE('',*,*,#43617,.F.);
#58208=ORIENTED_EDGE('',*,*,#43618,.F.);
#58209=ORIENTED_EDGE('',*,*,#43619,.F.);
#58210=ORIENTED_EDGE('',*,*,#43620,.F.);
#58211=ORIENTED_EDGE('',*,*,#43611,.T.);
#58212=ORIENTED_EDGE('',*,*,#43552,.T.);
#58213=ORIENTED_EDGE('',*,*,#43609,.T.);
#58214=ORIENTED_EDGE('',*,*,#43536,.T.);
#58215=ORIENTED_EDGE('',*,*,#43621,.T.);
#58216=ORIENTED_EDGE('',*,*,#43622,.T.);
#58217=ORIENTED_EDGE('',*,*,#43623,.T.);
#58218=ORIENTED_EDGE('',*,*,#43622,.F.);
#58219=ORIENTED_EDGE('',*,*,#43621,.F.);
#58220=ORIENTED_EDGE('',*,*,#43624,.T.);
#58221=ORIENTED_EDGE('',*,*,#43625,.F.);
#58222=ORIENTED_EDGE('',*,*,#43624,.F.);
#58223=ORIENTED_EDGE('',*,*,#43623,.F.);
#58224=ORIENTED_EDGE('',*,*,#43626,.T.);
#58225=ORIENTED_EDGE('',*,*,#43627,.T.);
#58226=ORIENTED_EDGE('',*,*,#43628,.T.);
#58227=ORIENTED_EDGE('',*,*,#43629,.T.);
#58228=ORIENTED_EDGE('',*,*,#43628,.F.);
#58229=ORIENTED_EDGE('',*,*,#43630,.T.);
#58230=ORIENTED_EDGE('',*,*,#43627,.F.);
#58231=ORIENTED_EDGE('',*,*,#43631,.T.);
#58232=ORIENTED_EDGE('',*,*,#43619,.T.);
#58233=ORIENTED_EDGE('',*,*,#43632,.F.);
#58234=ORIENTED_EDGE('',*,*,#43633,.F.);
#58235=ORIENTED_EDGE('',*,*,#43634,.F.);
#58236=ORIENTED_EDGE('',*,*,#43635,.F.);
#58237=ORIENTED_EDGE('',*,*,#43636,.F.);
#58238=ORIENTED_EDGE('',*,*,#43608,.T.);
#58239=ORIENTED_EDGE('',*,*,#43637,.F.);
#58240=ORIENTED_EDGE('',*,*,#43638,.F.);
#58241=ORIENTED_EDGE('',*,*,#43639,.F.);
#58242=ORIENTED_EDGE('',*,*,#43640,.F.);
#58243=ORIENTED_EDGE('',*,*,#43641,.F.);
#58244=ORIENTED_EDGE('',*,*,#43620,.T.);
#58245=ORIENTED_EDGE('',*,*,#43631,.F.);
#58246=ORIENTED_EDGE('',*,*,#43630,.F.);
#58247=ORIENTED_EDGE('',*,*,#43629,.F.);
#58248=ORIENTED_EDGE('',*,*,#43642,.F.);
#58249=ORIENTED_EDGE('',*,*,#43643,.T.);
#58250=ORIENTED_EDGE('',*,*,#43644,.T.);
#58251=ORIENTED_EDGE('',*,*,#43645,.T.);
#58252=ORIENTED_EDGE('',*,*,#43644,.F.);
#58253=ORIENTED_EDGE('',*,*,#43646,.T.);
#58254=ORIENTED_EDGE('',*,*,#43647,.F.);
#58255=ORIENTED_EDGE('',*,*,#43648,.T.);
#58256=ORIENTED_EDGE('',*,*,#43646,.F.);
#58257=ORIENTED_EDGE('',*,*,#43643,.F.);
#58258=ORIENTED_EDGE('',*,*,#43648,.F.);
#58259=ORIENTED_EDGE('',*,*,#43645,.F.);
#58260=ORIENTED_EDGE('',*,*,#43649,.F.);
#58261=ORIENTED_EDGE('',*,*,#43650,.T.);
#58262=ORIENTED_EDGE('',*,*,#43651,.T.);
#58263=ORIENTED_EDGE('',*,*,#43652,.T.);
#58264=ORIENTED_EDGE('',*,*,#43651,.F.);
#58265=ORIENTED_EDGE('',*,*,#43653,.F.);
#58266=ORIENTED_EDGE('',*,*,#43652,.F.);
#58267=ORIENTED_EDGE('',*,*,#43650,.F.);
#58268=ORIENTED_EDGE('',*,*,#43654,.T.);
#58269=ORIENTED_EDGE('',*,*,#43655,.T.);
#58270=ORIENTED_EDGE('',*,*,#43654,.F.);
#58271=ORIENTED_EDGE('',*,*,#43647,.T.);
#58272=ORIENTED_EDGE('',*,*,#43656,.T.);
#58273=ORIENTED_EDGE('',*,*,#43653,.T.);
#58274=ORIENTED_EDGE('',*,*,#43656,.F.);
#58275=ORIENTED_EDGE('',*,*,#43637,.T.);
#58276=ORIENTED_EDGE('',*,*,#43607,.T.);
#58277=ORIENTED_EDGE('',*,*,#43657,.T.);
#58278=ORIENTED_EDGE('',*,*,#43658,.T.);
#58279=ORIENTED_EDGE('',*,*,#43657,.F.);
#58280=ORIENTED_EDGE('',*,*,#43606,.T.);
#58281=ORIENTED_EDGE('',*,*,#43659,.T.);
#58282=ORIENTED_EDGE('',*,*,#43660,.T.);
#58283=ORIENTED_EDGE('',*,*,#43659,.F.);
#58284=ORIENTED_EDGE('',*,*,#43605,.T.);
#58285=ORIENTED_EDGE('',*,*,#43661,.T.);
#58286=ORIENTED_EDGE('',*,*,#43662,.T.);
#58287=ORIENTED_EDGE('',*,*,#43661,.F.);
#58288=ORIENTED_EDGE('',*,*,#43604,.T.);
#58289=ORIENTED_EDGE('',*,*,#43663,.T.);
#58290=ORIENTED_EDGE('',*,*,#43664,.T.);
#58291=ORIENTED_EDGE('',*,*,#43636,.T.);
#58292=ORIENTED_EDGE('',*,*,#43665,.T.);
#58293=ORIENTED_EDGE('',*,*,#43663,.F.);
#58294=ORIENTED_EDGE('',*,*,#43603,.T.);
#58295=ORIENTED_EDGE('',*,*,#43632,.T.);
#58296=ORIENTED_EDGE('',*,*,#43618,.T.);
#58297=ORIENTED_EDGE('',*,*,#43666,.T.);
#58298=ORIENTED_EDGE('',*,*,#43667,.T.);
#58299=ORIENTED_EDGE('',*,*,#43666,.F.);
#58300=ORIENTED_EDGE('',*,*,#43617,.T.);
#58301=ORIENTED_EDGE('',*,*,#43668,.T.);
#58302=ORIENTED_EDGE('',*,*,#43669,.T.);
#58303=ORIENTED_EDGE('',*,*,#43668,.F.);
#58304=ORIENTED_EDGE('',*,*,#43616,.T.);
#58305=ORIENTED_EDGE('',*,*,#43670,.T.);
#58306=ORIENTED_EDGE('',*,*,#43671,.T.);
#58307=ORIENTED_EDGE('',*,*,#43670,.F.);
#58308=ORIENTED_EDGE('',*,*,#43615,.T.);
#58309=ORIENTED_EDGE('',*,*,#43672,.T.);
#58310=ORIENTED_EDGE('',*,*,#43673,.T.);
#58311=ORIENTED_EDGE('',*,*,#43641,.T.);
#58312=ORIENTED_EDGE('',*,*,#43674,.T.);
#58313=ORIENTED_EDGE('',*,*,#43672,.F.);
#58314=ORIENTED_EDGE('',*,*,#43614,.T.);
#58315=ORIENTED_EDGE('',*,*,#43675,.T.);
#58316=ORIENTED_EDGE('',*,*,#43676,.T.);
#58317=ORIENTED_EDGE('',*,*,#43677,.T.);
#58318=ORIENTED_EDGE('',*,*,#43678,.T.);
#58319=ORIENTED_EDGE('',*,*,#43679,.T.);
#58320=ORIENTED_EDGE('',*,*,#43680,.T.);
#58321=ORIENTED_EDGE('',*,*,#43675,.F.);
#58322=ORIENTED_EDGE('',*,*,#43681,.T.);
#58323=ORIENTED_EDGE('',*,*,#43682,.T.);
#58324=ORIENTED_EDGE('',*,*,#43683,.T.);
#58325=ORIENTED_EDGE('',*,*,#43679,.F.);
#58326=ORIENTED_EDGE('',*,*,#43684,.T.);
#58327=ORIENTED_EDGE('',*,*,#43685,.T.);
#58328=ORIENTED_EDGE('',*,*,#43686,.T.);
#58329=ORIENTED_EDGE('',*,*,#43682,.F.);
#58330=ORIENTED_EDGE('',*,*,#43687,.T.);
#58331=ORIENTED_EDGE('',*,*,#43688,.T.);
#58332=ORIENTED_EDGE('',*,*,#43634,.T.);
#58333=ORIENTED_EDGE('',*,*,#43685,.F.);
#58334=ORIENTED_EDGE('',*,*,#43689,.T.);
#58335=ORIENTED_EDGE('',*,*,#43690,.T.);
#58336=ORIENTED_EDGE('',*,*,#43691,.T.);
#58337=ORIENTED_EDGE('',*,*,#43688,.F.);
#58338=ORIENTED_EDGE('',*,*,#43692,.T.);
#58339=ORIENTED_EDGE('',*,*,#43690,.F.);
#58340=ORIENTED_EDGE('',*,*,#43693,.T.);
#58341=ORIENTED_EDGE('',*,*,#43694,.T.);
#58342=ORIENTED_EDGE('',*,*,#43695,.T.);
#58343=ORIENTED_EDGE('',*,*,#43696,.T.);
#58344=ORIENTED_EDGE('',*,*,#43697,.T.);
#58345=ORIENTED_EDGE('',*,*,#43694,.F.);
#58346=ORIENTED_EDGE('',*,*,#43698,.T.);
#58347=ORIENTED_EDGE('',*,*,#43696,.F.);
#58348=ORIENTED_EDGE('',*,*,#43699,.T.);
#58349=ORIENTED_EDGE('',*,*,#43700,.T.);
#58350=ORIENTED_EDGE('',*,*,#43701,.T.);
#58351=ORIENTED_EDGE('',*,*,#43702,.T.);
#58352=ORIENTED_EDGE('',*,*,#43703,.T.);
#58353=ORIENTED_EDGE('',*,*,#43700,.F.);
#58354=ORIENTED_EDGE('',*,*,#43704,.T.);
#58355=ORIENTED_EDGE('',*,*,#43705,.T.);
#58356=ORIENTED_EDGE('',*,*,#43639,.T.);
#58357=ORIENTED_EDGE('',*,*,#43702,.F.);
#58358=ORIENTED_EDGE('',*,*,#43706,.T.);
#58359=ORIENTED_EDGE('',*,*,#43677,.F.);
#58360=ORIENTED_EDGE('',*,*,#43707,.T.);
#58361=ORIENTED_EDGE('',*,*,#43705,.F.);
#58362=ORIENTED_EDGE('',*,*,#43708,.T.);
#58363=ORIENTED_EDGE('',*,*,#43662,.F.);
#58364=ORIENTED_EDGE('',*,*,#43709,.F.);
#58365=ORIENTED_EDGE('',*,*,#43697,.F.);
#58366=ORIENTED_EDGE('',*,*,#43710,.T.);
#58367=ORIENTED_EDGE('',*,*,#43660,.F.);
#58368=ORIENTED_EDGE('',*,*,#43710,.F.);
#58369=ORIENTED_EDGE('',*,*,#43701,.F.);
#58370=ORIENTED_EDGE('',*,*,#43711,.F.);
#58371=ORIENTED_EDGE('',*,*,#43658,.F.);
#58372=ORIENTED_EDGE('',*,*,#43711,.T.);
#58373=ORIENTED_EDGE('',*,*,#43703,.F.);
#58374=ORIENTED_EDGE('',*,*,#43638,.T.);
#58375=ORIENTED_EDGE('',*,*,#43674,.F.);
#58376=ORIENTED_EDGE('',*,*,#43640,.T.);
#58377=ORIENTED_EDGE('',*,*,#43707,.F.);
#58378=ORIENTED_EDGE('',*,*,#43712,.T.);
#58379=ORIENTED_EDGE('',*,*,#43673,.F.);
#58380=ORIENTED_EDGE('',*,*,#43712,.F.);
#58381=ORIENTED_EDGE('',*,*,#43676,.F.);
#58382=ORIENTED_EDGE('',*,*,#43713,.T.);
#58383=ORIENTED_EDGE('',*,*,#43678,.F.);
#58384=ORIENTED_EDGE('',*,*,#43708,.F.);
#58385=ORIENTED_EDGE('',*,*,#43706,.F.);
#58386=ORIENTED_EDGE('',*,*,#43704,.F.);
#58387=ORIENTED_EDGE('',*,*,#43699,.F.);
#58388=ORIENTED_EDGE('',*,*,#43698,.F.);
#58389=ORIENTED_EDGE('',*,*,#43693,.F.);
#58390=ORIENTED_EDGE('',*,*,#43692,.F.);
#58391=ORIENTED_EDGE('',*,*,#43689,.F.);
#58392=ORIENTED_EDGE('',*,*,#43687,.F.);
#58393=ORIENTED_EDGE('',*,*,#43684,.F.);
#58394=ORIENTED_EDGE('',*,*,#43681,.F.);
#58395=ORIENTED_EDGE('',*,*,#43602,.T.);
#58396=ORIENTED_EDGE('',*,*,#43601,.F.);
#58397=ORIENTED_EDGE('',*,*,#43531,.F.);
#58398=ORIENTED_EDGE('',*,*,#43599,.T.);
#58399=ORIENTED_EDGE('',*,*,#43586,.T.);
#58400=ORIENTED_EDGE('',*,*,#43613,.T.);
#58401=ORIENTED_EDGE('',*,*,#43612,.F.);
#58402=ORIENTED_EDGE('',*,*,#43548,.F.);
#58403=ORIENTED_EDGE('',*,*,#43610,.T.);
#58404=ORIENTED_EDGE('',*,*,#43567,.T.);
#58405=ORIENTED_EDGE('',*,*,#43625,.T.);
#58406=ORIENTED_EDGE('',*,*,#43665,.F.);
#58407=ORIENTED_EDGE('',*,*,#43635,.T.);
#58408=ORIENTED_EDGE('',*,*,#43691,.F.);
#58409=ORIENTED_EDGE('',*,*,#43714,.T.);
#58410=ORIENTED_EDGE('',*,*,#43667,.F.);
#58411=ORIENTED_EDGE('',*,*,#43715,.T.);
#58412=ORIENTED_EDGE('',*,*,#43686,.F.);
#58413=ORIENTED_EDGE('',*,*,#43633,.T.);
#58414=ORIENTED_EDGE('',*,*,#43669,.F.);
#58415=ORIENTED_EDGE('',*,*,#43716,.F.);
#58416=ORIENTED_EDGE('',*,*,#43683,.F.);
#58417=ORIENTED_EDGE('',*,*,#43715,.F.);
#58418=ORIENTED_EDGE('',*,*,#43717,.T.);
#58419=ORIENTED_EDGE('',*,*,#43718,.T.);
#58420=ORIENTED_EDGE('',*,*,#43719,.T.);
#58421=ORIENTED_EDGE('',*,*,#43718,.F.);
#58422=ORIENTED_EDGE('',*,*,#43717,.F.);
#58423=ORIENTED_EDGE('',*,*,#43720,.T.);
#58424=ORIENTED_EDGE('',*,*,#43721,.T.);
#58425=ORIENTED_EDGE('',*,*,#43720,.F.);
#58426=ORIENTED_EDGE('',*,*,#43722,.T.);
#58427=ORIENTED_EDGE('',*,*,#43723,.T.);
#58428=ORIENTED_EDGE('',*,*,#43724,.T.);
#58429=ORIENTED_EDGE('',*,*,#43725,.F.);
#58430=ORIENTED_EDGE('',*,*,#43726,.T.);
#58431=ORIENTED_EDGE('',*,*,#43727,.T.);
#58432=ORIENTED_EDGE('',*,*,#43728,.T.);
#58433=ORIENTED_EDGE('',*,*,#43729,.T.);
#58434=ORIENTED_EDGE('',*,*,#43730,.T.);
#58435=ORIENTED_EDGE('',*,*,#43731,.F.);
#58436=ORIENTED_EDGE('',*,*,#43732,.T.);
#58437=ORIENTED_EDGE('',*,*,#43733,.T.);
#58438=ORIENTED_EDGE('',*,*,#43734,.T.);
#58439=ORIENTED_EDGE('',*,*,#43735,.T.);
#58440=ORIENTED_EDGE('',*,*,#43736,.T.);
#58441=ORIENTED_EDGE('',*,*,#43737,.F.);
#58442=ORIENTED_EDGE('',*,*,#43738,.T.);
#58443=ORIENTED_EDGE('',*,*,#43739,.T.);
#58444=ORIENTED_EDGE('',*,*,#43740,.T.);
#58445=ORIENTED_EDGE('',*,*,#43741,.T.);
#58446=ORIENTED_EDGE('',*,*,#43742,.T.);
#58447=ORIENTED_EDGE('',*,*,#43743,.F.);
#58448=ORIENTED_EDGE('',*,*,#43744,.T.);
#58449=ORIENTED_EDGE('',*,*,#43745,.T.);
#58450=ORIENTED_EDGE('',*,*,#43746,.T.);
#58451=ORIENTED_EDGE('',*,*,#43747,.T.);
#58452=ORIENTED_EDGE('',*,*,#43748,.T.);
#58453=ORIENTED_EDGE('',*,*,#43749,.F.);
#58454=ORIENTED_EDGE('',*,*,#43750,.T.);
#58455=ORIENTED_EDGE('',*,*,#43751,.T.);
#58456=ORIENTED_EDGE('',*,*,#43752,.T.);
#58457=ORIENTED_EDGE('',*,*,#43753,.T.);
#58458=ORIENTED_EDGE('',*,*,#43754,.T.);
#58459=ORIENTED_EDGE('',*,*,#43755,.F.);
#58460=ORIENTED_EDGE('',*,*,#43756,.T.);
#58461=ORIENTED_EDGE('',*,*,#43757,.T.);
#58462=ORIENTED_EDGE('',*,*,#43758,.T.);
#58463=ORIENTED_EDGE('',*,*,#43759,.T.);
#58464=ORIENTED_EDGE('',*,*,#43760,.T.);
#58465=ORIENTED_EDGE('',*,*,#43761,.F.);
#58466=ORIENTED_EDGE('',*,*,#43762,.T.);
#58467=ORIENTED_EDGE('',*,*,#43763,.T.);
#58468=ORIENTED_EDGE('',*,*,#43764,.T.);
#58469=ORIENTED_EDGE('',*,*,#43765,.T.);
#58470=ORIENTED_EDGE('',*,*,#43766,.T.);
#58471=ORIENTED_EDGE('',*,*,#43767,.F.);
#58472=ORIENTED_EDGE('',*,*,#43768,.T.);
#58473=ORIENTED_EDGE('',*,*,#43769,.T.);
#58474=ORIENTED_EDGE('',*,*,#43770,.T.);
#58475=ORIENTED_EDGE('',*,*,#43771,.T.);
#58476=ORIENTED_EDGE('',*,*,#43772,.T.);
#58477=ORIENTED_EDGE('',*,*,#43773,.F.);
#58478=ORIENTED_EDGE('',*,*,#43774,.T.);
#58479=ORIENTED_EDGE('',*,*,#43775,.T.);
#58480=ORIENTED_EDGE('',*,*,#43776,.T.);
#58481=ORIENTED_EDGE('',*,*,#43777,.T.);
#58482=ORIENTED_EDGE('',*,*,#43778,.T.);
#58483=ORIENTED_EDGE('',*,*,#43779,.F.);
#58484=ORIENTED_EDGE('',*,*,#43780,.T.);
#58485=ORIENTED_EDGE('',*,*,#43781,.T.);
#58486=ORIENTED_EDGE('',*,*,#43719,.F.);
#58487=ORIENTED_EDGE('',*,*,#43721,.F.);
#58488=ORIENTED_EDGE('',*,*,#43782,.F.);
#58489=ORIENTED_EDGE('',*,*,#43783,.F.);
#58490=ORIENTED_EDGE('',*,*,#43784,.F.);
#58491=ORIENTED_EDGE('',*,*,#43785,.F.);
#58492=ORIENTED_EDGE('',*,*,#43786,.F.);
#58493=ORIENTED_EDGE('',*,*,#43787,.F.);
#58494=ORIENTED_EDGE('',*,*,#43788,.F.);
#58495=ORIENTED_EDGE('',*,*,#43789,.F.);
#58496=ORIENTED_EDGE('',*,*,#43790,.F.);
#58497=ORIENTED_EDGE('',*,*,#43791,.F.);
#58498=ORIENTED_EDGE('',*,*,#43792,.F.);
#58499=ORIENTED_EDGE('',*,*,#43793,.F.);
#58500=ORIENTED_EDGE('',*,*,#43794,.F.);
#58501=ORIENTED_EDGE('',*,*,#43795,.F.);
#58502=ORIENTED_EDGE('',*,*,#43796,.F.);
#58503=ORIENTED_EDGE('',*,*,#43797,.F.);
#58504=ORIENTED_EDGE('',*,*,#43798,.F.);
#58505=ORIENTED_EDGE('',*,*,#43799,.F.);
#58506=ORIENTED_EDGE('',*,*,#43800,.F.);
#58507=ORIENTED_EDGE('',*,*,#43801,.F.);
#58508=ORIENTED_EDGE('',*,*,#43802,.F.);
#58509=ORIENTED_EDGE('',*,*,#43803,.F.);
#58510=ORIENTED_EDGE('',*,*,#43804,.F.);
#58511=ORIENTED_EDGE('',*,*,#43805,.F.);
#58512=ORIENTED_EDGE('',*,*,#43806,.F.);
#58513=ORIENTED_EDGE('',*,*,#43807,.F.);
#58514=ORIENTED_EDGE('',*,*,#43808,.F.);
#58515=ORIENTED_EDGE('',*,*,#43809,.F.);
#58516=ORIENTED_EDGE('',*,*,#43810,.F.);
#58517=ORIENTED_EDGE('',*,*,#43811,.F.);
#58518=ORIENTED_EDGE('',*,*,#43812,.F.);
#58519=ORIENTED_EDGE('',*,*,#43813,.F.);
#58520=ORIENTED_EDGE('',*,*,#43814,.F.);
#58521=ORIENTED_EDGE('',*,*,#43815,.F.);
#58522=ORIENTED_EDGE('',*,*,#43816,.F.);
#58523=ORIENTED_EDGE('',*,*,#43817,.F.);
#58524=ORIENTED_EDGE('',*,*,#43818,.F.);
#58525=ORIENTED_EDGE('',*,*,#43819,.F.);
#58526=ORIENTED_EDGE('',*,*,#43820,.F.);
#58527=ORIENTED_EDGE('',*,*,#43821,.F.);
#58528=ORIENTED_EDGE('',*,*,#43822,.F.);
#58529=ORIENTED_EDGE('',*,*,#43823,.F.);
#58530=ORIENTED_EDGE('',*,*,#43824,.F.);
#58531=ORIENTED_EDGE('',*,*,#43825,.F.);
#58532=ORIENTED_EDGE('',*,*,#43826,.F.);
#58533=ORIENTED_EDGE('',*,*,#43827,.F.);
#58534=ORIENTED_EDGE('',*,*,#43828,.F.);
#58535=ORIENTED_EDGE('',*,*,#43829,.F.);
#58536=ORIENTED_EDGE('',*,*,#43830,.F.);
#58537=ORIENTED_EDGE('',*,*,#43831,.F.);
#58538=ORIENTED_EDGE('',*,*,#43832,.F.);
#58539=ORIENTED_EDGE('',*,*,#43833,.F.);
#58540=ORIENTED_EDGE('',*,*,#43834,.F.);
#58541=ORIENTED_EDGE('',*,*,#43835,.F.);
#58542=ORIENTED_EDGE('',*,*,#43836,.F.);
#58543=ORIENTED_EDGE('',*,*,#43837,.F.);
#58544=ORIENTED_EDGE('',*,*,#43838,.F.);
#58545=ORIENTED_EDGE('',*,*,#43839,.F.);
#58546=ORIENTED_EDGE('',*,*,#43840,.F.);
#58547=ORIENTED_EDGE('',*,*,#43841,.F.);
#58548=ORIENTED_EDGE('',*,*,#43842,.F.);
#58549=ORIENTED_EDGE('',*,*,#43843,.F.);
#58550=ORIENTED_EDGE('',*,*,#43841,.T.);
#58551=ORIENTED_EDGE('',*,*,#43844,.T.);
#58552=ORIENTED_EDGE('',*,*,#43777,.F.);
#58553=ORIENTED_EDGE('',*,*,#43840,.T.);
#58554=ORIENTED_EDGE('',*,*,#43845,.F.);
#58555=ORIENTED_EDGE('',*,*,#43778,.F.);
#58556=ORIENTED_EDGE('',*,*,#43844,.F.);
#58557=ORIENTED_EDGE('',*,*,#43839,.T.);
#58558=ORIENTED_EDGE('',*,*,#43846,.T.);
#58559=ORIENTED_EDGE('',*,*,#43779,.T.);
#58560=ORIENTED_EDGE('',*,*,#43845,.T.);
#58561=ORIENTED_EDGE('',*,*,#43838,.T.);
#58562=ORIENTED_EDGE('',*,*,#43847,.T.);
#58563=ORIENTED_EDGE('',*,*,#43780,.F.);
#58564=ORIENTED_EDGE('',*,*,#43846,.F.);
#58565=ORIENTED_EDGE('',*,*,#43848,.F.);
#58566=ORIENTED_EDGE('',*,*,#43781,.F.);
#58567=ORIENTED_EDGE('',*,*,#43847,.F.);
#58568=ORIENTED_EDGE('',*,*,#43837,.T.);
#58569=ORIENTED_EDGE('',*,*,#43843,.T.);
#58570=ORIENTED_EDGE('',*,*,#43776,.F.);
#58571=ORIENTED_EDGE('',*,*,#43849,.T.);
#58572=ORIENTED_EDGE('',*,*,#43782,.T.);
#58573=ORIENTED_EDGE('',*,*,#43848,.T.);
#58574=ORIENTED_EDGE('',*,*,#43836,.T.);
#58575=ORIENTED_EDGE('',*,*,#43850,.T.);
#58576=ORIENTED_EDGE('',*,*,#43722,.F.);
#58577=ORIENTED_EDGE('',*,*,#43851,.F.);
#58578=ORIENTED_EDGE('',*,*,#43787,.T.);
#58579=ORIENTED_EDGE('',*,*,#43852,.T.);
#58580=ORIENTED_EDGE('',*,*,#43771,.F.);
#58581=ORIENTED_EDGE('',*,*,#43786,.T.);
#58582=ORIENTED_EDGE('',*,*,#43853,.F.);
#58583=ORIENTED_EDGE('',*,*,#43772,.F.);
#58584=ORIENTED_EDGE('',*,*,#43852,.F.);
#58585=ORIENTED_EDGE('',*,*,#43785,.T.);
#58586=ORIENTED_EDGE('',*,*,#43854,.T.);
#58587=ORIENTED_EDGE('',*,*,#43773,.T.);
#58588=ORIENTED_EDGE('',*,*,#43853,.T.);
#58589=ORIENTED_EDGE('',*,*,#43784,.T.);
#58590=ORIENTED_EDGE('',*,*,#43855,.T.);
#58591=ORIENTED_EDGE('',*,*,#43774,.F.);
#58592=ORIENTED_EDGE('',*,*,#43854,.F.);
#58593=ORIENTED_EDGE('',*,*,#43849,.F.);
#58594=ORIENTED_EDGE('',*,*,#43775,.F.);
#58595=ORIENTED_EDGE('',*,*,#43855,.F.);
#58596=ORIENTED_EDGE('',*,*,#43783,.T.);
#58597=ORIENTED_EDGE('',*,*,#43851,.T.);
#58598=ORIENTED_EDGE('',*,*,#43770,.F.);
#58599=ORIENTED_EDGE('',*,*,#43856,.T.);
#58600=ORIENTED_EDGE('',*,*,#43788,.T.);
#58601=ORIENTED_EDGE('',*,*,#43857,.F.);
#58602=ORIENTED_EDGE('',*,*,#43793,.T.);
#58603=ORIENTED_EDGE('',*,*,#43858,.T.);
#58604=ORIENTED_EDGE('',*,*,#43765,.F.);
#58605=ORIENTED_EDGE('',*,*,#43792,.T.);
#58606=ORIENTED_EDGE('',*,*,#43859,.F.);
#58607=ORIENTED_EDGE('',*,*,#43766,.F.);
#58608=ORIENTED_EDGE('',*,*,#43858,.F.);
#58609=ORIENTED_EDGE('',*,*,#43791,.T.);
#58610=ORIENTED_EDGE('',*,*,#43860,.T.);
#58611=ORIENTED_EDGE('',*,*,#43767,.T.);
#58612=ORIENTED_EDGE('',*,*,#43859,.T.);
#58613=ORIENTED_EDGE('',*,*,#43790,.T.);
#58614=ORIENTED_EDGE('',*,*,#43861,.T.);
#58615=ORIENTED_EDGE('',*,*,#43768,.F.);
#58616=ORIENTED_EDGE('',*,*,#43860,.F.);
#58617=ORIENTED_EDGE('',*,*,#43856,.F.);
#58618=ORIENTED_EDGE('',*,*,#43769,.F.);
#58619=ORIENTED_EDGE('',*,*,#43861,.F.);
#58620=ORIENTED_EDGE('',*,*,#43789,.T.);
#58621=ORIENTED_EDGE('',*,*,#43857,.T.);
#58622=ORIENTED_EDGE('',*,*,#43764,.F.);
#58623=ORIENTED_EDGE('',*,*,#43862,.T.);
#58624=ORIENTED_EDGE('',*,*,#43794,.T.);
#58625=ORIENTED_EDGE('',*,*,#43863,.F.);
#58626=ORIENTED_EDGE('',*,*,#43799,.T.);
#58627=ORIENTED_EDGE('',*,*,#43864,.T.);
#58628=ORIENTED_EDGE('',*,*,#43759,.F.);
#58629=ORIENTED_EDGE('',*,*,#43798,.T.);
#58630=ORIENTED_EDGE('',*,*,#43865,.F.);
#58631=ORIENTED_EDGE('',*,*,#43760,.F.);
#58632=ORIENTED_EDGE('',*,*,#43864,.F.);
#58633=ORIENTED_EDGE('',*,*,#43797,.T.);
#58634=ORIENTED_EDGE('',*,*,#43866,.T.);
#58635=ORIENTED_EDGE('',*,*,#43761,.T.);
#58636=ORIENTED_EDGE('',*,*,#43865,.T.);
#58637=ORIENTED_EDGE('',*,*,#43796,.T.);
#58638=ORIENTED_EDGE('',*,*,#43867,.T.);
#58639=ORIENTED_EDGE('',*,*,#43762,.F.);
#58640=ORIENTED_EDGE('',*,*,#43866,.F.);
#58641=ORIENTED_EDGE('',*,*,#43862,.F.);
#58642=ORIENTED_EDGE('',*,*,#43763,.F.);
#58643=ORIENTED_EDGE('',*,*,#43867,.F.);
#58644=ORIENTED_EDGE('',*,*,#43795,.T.);
#58645=ORIENTED_EDGE('',*,*,#43863,.T.);
#58646=ORIENTED_EDGE('',*,*,#43758,.F.);
#58647=ORIENTED_EDGE('',*,*,#43868,.T.);
#58648=ORIENTED_EDGE('',*,*,#43800,.T.);
#58649=ORIENTED_EDGE('',*,*,#43869,.F.);
#58650=ORIENTED_EDGE('',*,*,#43805,.T.);
#58651=ORIENTED_EDGE('',*,*,#43870,.T.);
#58652=ORIENTED_EDGE('',*,*,#43753,.F.);
#58653=ORIENTED_EDGE('',*,*,#43804,.T.);
#58654=ORIENTED_EDGE('',*,*,#43871,.F.);
#58655=ORIENTED_EDGE('',*,*,#43754,.F.);
#58656=ORIENTED_EDGE('',*,*,#43870,.F.);
#58657=ORIENTED_EDGE('',*,*,#43803,.T.);
#58658=ORIENTED_EDGE('',*,*,#43872,.T.);
#58659=ORIENTED_EDGE('',*,*,#43755,.T.);
#58660=ORIENTED_EDGE('',*,*,#43871,.T.);
#58661=ORIENTED_EDGE('',*,*,#43802,.T.);
#58662=ORIENTED_EDGE('',*,*,#43873,.T.);
#58663=ORIENTED_EDGE('',*,*,#43756,.F.);
#58664=ORIENTED_EDGE('',*,*,#43872,.F.);
#58665=ORIENTED_EDGE('',*,*,#43868,.F.);
#58666=ORIENTED_EDGE('',*,*,#43757,.F.);
#58667=ORIENTED_EDGE('',*,*,#43873,.F.);
#58668=ORIENTED_EDGE('',*,*,#43801,.T.);
#58669=ORIENTED_EDGE('',*,*,#43869,.T.);
#58670=ORIENTED_EDGE('',*,*,#43752,.F.);
#58671=ORIENTED_EDGE('',*,*,#43874,.T.);
#58672=ORIENTED_EDGE('',*,*,#43806,.T.);
#58673=ORIENTED_EDGE('',*,*,#43875,.F.);
#58674=ORIENTED_EDGE('',*,*,#43811,.T.);
#58675=ORIENTED_EDGE('',*,*,#43876,.T.);
#58676=ORIENTED_EDGE('',*,*,#43747,.F.);
#58677=ORIENTED_EDGE('',*,*,#43810,.T.);
#58678=ORIENTED_EDGE('',*,*,#43877,.F.);
#58679=ORIENTED_EDGE('',*,*,#43748,.F.);
#58680=ORIENTED_EDGE('',*,*,#43876,.F.);
#58681=ORIENTED_EDGE('',*,*,#43809,.T.);
#58682=ORIENTED_EDGE('',*,*,#43878,.T.);
#58683=ORIENTED_EDGE('',*,*,#43749,.T.);
#58684=ORIENTED_EDGE('',*,*,#43877,.T.);
#58685=ORIENTED_EDGE('',*,*,#43808,.T.);
#58686=ORIENTED_EDGE('',*,*,#43879,.T.);
#58687=ORIENTED_EDGE('',*,*,#43750,.F.);
#58688=ORIENTED_EDGE('',*,*,#43878,.F.);
#58689=ORIENTED_EDGE('',*,*,#43874,.F.);
#58690=ORIENTED_EDGE('',*,*,#43751,.F.);
#58691=ORIENTED_EDGE('',*,*,#43879,.F.);
#58692=ORIENTED_EDGE('',*,*,#43807,.T.);
#58693=ORIENTED_EDGE('',*,*,#43875,.T.);
#58694=ORIENTED_EDGE('',*,*,#43746,.F.);
#58695=ORIENTED_EDGE('',*,*,#43880,.T.);
#58696=ORIENTED_EDGE('',*,*,#43812,.T.);
#58697=ORIENTED_EDGE('',*,*,#43881,.F.);
#58698=ORIENTED_EDGE('',*,*,#43817,.T.);
#58699=ORIENTED_EDGE('',*,*,#43882,.T.);
#58700=ORIENTED_EDGE('',*,*,#43741,.F.);
#58701=ORIENTED_EDGE('',*,*,#43816,.T.);
#58702=ORIENTED_EDGE('',*,*,#43883,.F.);
#58703=ORIENTED_EDGE('',*,*,#43742,.F.);
#58704=ORIENTED_EDGE('',*,*,#43882,.F.);
#58705=ORIENTED_EDGE('',*,*,#43815,.T.);
#58706=ORIENTED_EDGE('',*,*,#43884,.T.);
#58707=ORIENTED_EDGE('',*,*,#43743,.T.);
#58708=ORIENTED_EDGE('',*,*,#43883,.T.);
#58709=ORIENTED_EDGE('',*,*,#43814,.T.);
#58710=ORIENTED_EDGE('',*,*,#43885,.T.);
#58711=ORIENTED_EDGE('',*,*,#43744,.F.);
#58712=ORIENTED_EDGE('',*,*,#43884,.F.);
#58713=ORIENTED_EDGE('',*,*,#43880,.F.);
#58714=ORIENTED_EDGE('',*,*,#43745,.F.);
#58715=ORIENTED_EDGE('',*,*,#43885,.F.);
#58716=ORIENTED_EDGE('',*,*,#43813,.T.);
#58717=ORIENTED_EDGE('',*,*,#43881,.T.);
#58718=ORIENTED_EDGE('',*,*,#43740,.F.);
#58719=ORIENTED_EDGE('',*,*,#43886,.T.);
#58720=ORIENTED_EDGE('',*,*,#43818,.T.);
#58721=ORIENTED_EDGE('',*,*,#43887,.F.);
#58722=ORIENTED_EDGE('',*,*,#43823,.T.);
#58723=ORIENTED_EDGE('',*,*,#43888,.T.);
#58724=ORIENTED_EDGE('',*,*,#43735,.F.);
#58725=ORIENTED_EDGE('',*,*,#43822,.T.);
#58726=ORIENTED_EDGE('',*,*,#43889,.F.);
#58727=ORIENTED_EDGE('',*,*,#43736,.F.);
#58728=ORIENTED_EDGE('',*,*,#43888,.F.);
#58729=ORIENTED_EDGE('',*,*,#43821,.T.);
#58730=ORIENTED_EDGE('',*,*,#43890,.T.);
#58731=ORIENTED_EDGE('',*,*,#43737,.T.);
#58732=ORIENTED_EDGE('',*,*,#43889,.T.);
#58733=ORIENTED_EDGE('',*,*,#43820,.T.);
#58734=ORIENTED_EDGE('',*,*,#43891,.T.);
#58735=ORIENTED_EDGE('',*,*,#43738,.F.);
#58736=ORIENTED_EDGE('',*,*,#43890,.F.);
#58737=ORIENTED_EDGE('',*,*,#43886,.F.);
#58738=ORIENTED_EDGE('',*,*,#43739,.F.);
#58739=ORIENTED_EDGE('',*,*,#43891,.F.);
#58740=ORIENTED_EDGE('',*,*,#43819,.T.);
#58741=ORIENTED_EDGE('',*,*,#43887,.T.);
#58742=ORIENTED_EDGE('',*,*,#43734,.F.);
#58743=ORIENTED_EDGE('',*,*,#43892,.T.);
#58744=ORIENTED_EDGE('',*,*,#43824,.T.);
#58745=ORIENTED_EDGE('',*,*,#43893,.F.);
#58746=ORIENTED_EDGE('',*,*,#43829,.T.);
#58747=ORIENTED_EDGE('',*,*,#43894,.T.);
#58748=ORIENTED_EDGE('',*,*,#43729,.F.);
#58749=ORIENTED_EDGE('',*,*,#43828,.T.);
#58750=ORIENTED_EDGE('',*,*,#43895,.F.);
#58751=ORIENTED_EDGE('',*,*,#43730,.F.);
#58752=ORIENTED_EDGE('',*,*,#43894,.F.);
#58753=ORIENTED_EDGE('',*,*,#43827,.T.);
#58754=ORIENTED_EDGE('',*,*,#43896,.T.);
#58755=ORIENTED_EDGE('',*,*,#43731,.T.);
#58756=ORIENTED_EDGE('',*,*,#43895,.T.);
#58757=ORIENTED_EDGE('',*,*,#43826,.T.);
#58758=ORIENTED_EDGE('',*,*,#43897,.T.);
#58759=ORIENTED_EDGE('',*,*,#43732,.F.);
#58760=ORIENTED_EDGE('',*,*,#43896,.F.);
#58761=ORIENTED_EDGE('',*,*,#43892,.F.);
#58762=ORIENTED_EDGE('',*,*,#43733,.F.);
#58763=ORIENTED_EDGE('',*,*,#43897,.F.);
#58764=ORIENTED_EDGE('',*,*,#43825,.T.);
#58765=ORIENTED_EDGE('',*,*,#43893,.T.);
#58766=ORIENTED_EDGE('',*,*,#43728,.F.);
#58767=ORIENTED_EDGE('',*,*,#43898,.T.);
#58768=ORIENTED_EDGE('',*,*,#43830,.T.);
#58769=ORIENTED_EDGE('',*,*,#43850,.F.);
#58770=ORIENTED_EDGE('',*,*,#43835,.T.);
#58771=ORIENTED_EDGE('',*,*,#43899,.T.);
#58772=ORIENTED_EDGE('',*,*,#43723,.F.);
#58773=ORIENTED_EDGE('',*,*,#43834,.T.);
#58774=ORIENTED_EDGE('',*,*,#43900,.F.);
#58775=ORIENTED_EDGE('',*,*,#43724,.F.);
#58776=ORIENTED_EDGE('',*,*,#43899,.F.);
#58777=ORIENTED_EDGE('',*,*,#43833,.T.);
#58778=ORIENTED_EDGE('',*,*,#43901,.T.);
#58779=ORIENTED_EDGE('',*,*,#43725,.T.);
#58780=ORIENTED_EDGE('',*,*,#43900,.T.);
#58781=ORIENTED_EDGE('',*,*,#43832,.T.);
#58782=ORIENTED_EDGE('',*,*,#43902,.T.);
#58783=ORIENTED_EDGE('',*,*,#43726,.F.);
#58784=ORIENTED_EDGE('',*,*,#43901,.F.);
#58785=ORIENTED_EDGE('',*,*,#43898,.F.);
#58786=ORIENTED_EDGE('',*,*,#43727,.F.);
#58787=ORIENTED_EDGE('',*,*,#43902,.F.);
#58788=ORIENTED_EDGE('',*,*,#43831,.T.);
#58789=ORIENTED_EDGE('',*,*,#43903,.T.);
#58790=ORIENTED_EDGE('',*,*,#43904,.T.);
#58791=ORIENTED_EDGE('',*,*,#43905,.F.);
#58792=ORIENTED_EDGE('',*,*,#43904,.F.);
#58793=ORIENTED_EDGE('',*,*,#43906,.T.);
#58794=ORIENTED_EDGE('',*,*,#43907,.T.);
#58795=ORIENTED_EDGE('',*,*,#43908,.T.);
#58796=ORIENTED_EDGE('',*,*,#43905,.T.);
#58797=ORIENTED_EDGE('',*,*,#43908,.F.);
#58798=ORIENTED_EDGE('',*,*,#43909,.T.);
#58799=ORIENTED_EDGE('',*,*,#43903,.F.);
#58800=ORIENTED_EDGE('',*,*,#43910,.T.);
#58801=ORIENTED_EDGE('',*,*,#43911,.F.);
#58802=ORIENTED_EDGE('',*,*,#43912,.F.);
#58803=ORIENTED_EDGE('',*,*,#43910,.F.);
#58804=ORIENTED_EDGE('',*,*,#43906,.F.);
#58805=ORIENTED_EDGE('',*,*,#43649,.T.);
#58806=ORIENTED_EDGE('',*,*,#43913,.T.);
#58807=ORIENTED_EDGE('',*,*,#43909,.F.);
#58808=ORIENTED_EDGE('',*,*,#43907,.F.);
#58809=ORIENTED_EDGE('',*,*,#43913,.F.);
#58810=ORIENTED_EDGE('',*,*,#43914,.T.);
#58811=ORIENTED_EDGE('',*,*,#43915,.T.);
#58812=ORIENTED_EDGE('',*,*,#43916,.F.);
#58813=ORIENTED_EDGE('',*,*,#43915,.F.);
#58814=ORIENTED_EDGE('',*,*,#43917,.T.);
#58815=ORIENTED_EDGE('',*,*,#43911,.T.);
#58816=ORIENTED_EDGE('',*,*,#43912,.T.);
#58817=ORIENTED_EDGE('',*,*,#43918,.T.);
#58818=ORIENTED_EDGE('',*,*,#43916,.T.);
#58819=ORIENTED_EDGE('',*,*,#43918,.F.);
#58820=ORIENTED_EDGE('',*,*,#43914,.F.);
#58821=ORIENTED_EDGE('',*,*,#43919,.T.);
#58822=ORIENTED_EDGE('',*,*,#43920,.F.);
#58823=ORIENTED_EDGE('',*,*,#43921,.F.);
#58824=ORIENTED_EDGE('',*,*,#43919,.F.);
#58825=ORIENTED_EDGE('',*,*,#43917,.F.);
#58826=ORIENTED_EDGE('',*,*,#43922,.T.);
#58827=ORIENTED_EDGE('',*,*,#43923,.T.);
#58828=ORIENTED_EDGE('',*,*,#43924,.F.);
#58829=ORIENTED_EDGE('',*,*,#43923,.F.);
#58830=ORIENTED_EDGE('',*,*,#43925,.T.);
#58831=ORIENTED_EDGE('',*,*,#43920,.T.);
#58832=ORIENTED_EDGE('',*,*,#43921,.T.);
#58833=ORIENTED_EDGE('',*,*,#43926,.T.);
#58834=ORIENTED_EDGE('',*,*,#43924,.T.);
#58835=ORIENTED_EDGE('',*,*,#43926,.F.);
#58836=ORIENTED_EDGE('',*,*,#43922,.F.);
#58837=ORIENTED_EDGE('',*,*,#43927,.T.);
#58838=ORIENTED_EDGE('',*,*,#43928,.F.);
#58839=ORIENTED_EDGE('',*,*,#43929,.F.);
#58840=ORIENTED_EDGE('',*,*,#43927,.F.);
#58841=ORIENTED_EDGE('',*,*,#43925,.F.);
#58842=ORIENTED_EDGE('',*,*,#43930,.T.);
#58843=ORIENTED_EDGE('',*,*,#43931,.T.);
#58844=ORIENTED_EDGE('',*,*,#43932,.F.);
#58845=ORIENTED_EDGE('',*,*,#43931,.F.);
#58846=ORIENTED_EDGE('',*,*,#43933,.T.);
#58847=ORIENTED_EDGE('',*,*,#43928,.T.);
#58848=ORIENTED_EDGE('',*,*,#43929,.T.);
#58849=ORIENTED_EDGE('',*,*,#43934,.T.);
#58850=ORIENTED_EDGE('',*,*,#43932,.T.);
#58851=ORIENTED_EDGE('',*,*,#43934,.F.);
#58852=ORIENTED_EDGE('',*,*,#43930,.F.);
#58853=ORIENTED_EDGE('',*,*,#43935,.T.);
#58854=ORIENTED_EDGE('',*,*,#43936,.F.);
#58855=ORIENTED_EDGE('',*,*,#43937,.F.);
#58856=ORIENTED_EDGE('',*,*,#43935,.F.);
#58857=ORIENTED_EDGE('',*,*,#43933,.F.);
#58858=ORIENTED_EDGE('',*,*,#43938,.T.);
#58859=ORIENTED_EDGE('',*,*,#43939,.T.);
#58860=ORIENTED_EDGE('',*,*,#43940,.F.);
#58861=ORIENTED_EDGE('',*,*,#43939,.F.);
#58862=ORIENTED_EDGE('',*,*,#43941,.T.);
#58863=ORIENTED_EDGE('',*,*,#43936,.T.);
#58864=ORIENTED_EDGE('',*,*,#43937,.T.);
#58865=ORIENTED_EDGE('',*,*,#43942,.T.);
#58866=ORIENTED_EDGE('',*,*,#43940,.T.);
#58867=ORIENTED_EDGE('',*,*,#43942,.F.);
#58868=ORIENTED_EDGE('',*,*,#43938,.F.);
#58869=ORIENTED_EDGE('',*,*,#43943,.T.);
#58870=ORIENTED_EDGE('',*,*,#43944,.F.);
#58871=ORIENTED_EDGE('',*,*,#43945,.F.);
#58872=ORIENTED_EDGE('',*,*,#43943,.F.);
#58873=ORIENTED_EDGE('',*,*,#43941,.F.);
#58874=ORIENTED_EDGE('',*,*,#43946,.T.);
#58875=ORIENTED_EDGE('',*,*,#43947,.T.);
#58876=ORIENTED_EDGE('',*,*,#43948,.F.);
#58877=ORIENTED_EDGE('',*,*,#43947,.F.);
#58878=ORIENTED_EDGE('',*,*,#43949,.T.);
#58879=ORIENTED_EDGE('',*,*,#43944,.T.);
#58880=ORIENTED_EDGE('',*,*,#43945,.T.);
#58881=ORIENTED_EDGE('',*,*,#43950,.T.);
#58882=ORIENTED_EDGE('',*,*,#43948,.T.);
#58883=ORIENTED_EDGE('',*,*,#43950,.F.);
#58884=ORIENTED_EDGE('',*,*,#43946,.F.);
#58885=ORIENTED_EDGE('',*,*,#43951,.T.);
#58886=ORIENTED_EDGE('',*,*,#43952,.F.);
#58887=ORIENTED_EDGE('',*,*,#43953,.F.);
#58888=ORIENTED_EDGE('',*,*,#43951,.F.);
#58889=ORIENTED_EDGE('',*,*,#43949,.F.);
#58890=ORIENTED_EDGE('',*,*,#43954,.T.);
#58891=ORIENTED_EDGE('',*,*,#43955,.T.);
#58892=ORIENTED_EDGE('',*,*,#43956,.F.);
#58893=ORIENTED_EDGE('',*,*,#43955,.F.);
#58894=ORIENTED_EDGE('',*,*,#43957,.T.);
#58895=ORIENTED_EDGE('',*,*,#43952,.T.);
#58896=ORIENTED_EDGE('',*,*,#43953,.T.);
#58897=ORIENTED_EDGE('',*,*,#43958,.T.);
#58898=ORIENTED_EDGE('',*,*,#43956,.T.);
#58899=ORIENTED_EDGE('',*,*,#43958,.F.);
#58900=ORIENTED_EDGE('',*,*,#43954,.F.);
#58901=ORIENTED_EDGE('',*,*,#43959,.T.);
#58902=ORIENTED_EDGE('',*,*,#43960,.F.);
#58903=ORIENTED_EDGE('',*,*,#43961,.F.);
#58904=ORIENTED_EDGE('',*,*,#43959,.F.);
#58905=ORIENTED_EDGE('',*,*,#43957,.F.);
#58906=ORIENTED_EDGE('',*,*,#43962,.T.);
#58907=ORIENTED_EDGE('',*,*,#43963,.T.);
#58908=ORIENTED_EDGE('',*,*,#43964,.F.);
#58909=ORIENTED_EDGE('',*,*,#43963,.F.);
#58910=ORIENTED_EDGE('',*,*,#43965,.T.);
#58911=ORIENTED_EDGE('',*,*,#43960,.T.);
#58912=ORIENTED_EDGE('',*,*,#43961,.T.);
#58913=ORIENTED_EDGE('',*,*,#43966,.T.);
#58914=ORIENTED_EDGE('',*,*,#43964,.T.);
#58915=ORIENTED_EDGE('',*,*,#43966,.F.);
#58916=ORIENTED_EDGE('',*,*,#43962,.F.);
#58917=ORIENTED_EDGE('',*,*,#43967,.T.);
#58918=ORIENTED_EDGE('',*,*,#43968,.F.);
#58919=ORIENTED_EDGE('',*,*,#43969,.F.);
#58920=ORIENTED_EDGE('',*,*,#43967,.F.);
#58921=ORIENTED_EDGE('',*,*,#43965,.F.);
#58922=ORIENTED_EDGE('',*,*,#43970,.T.);
#58923=ORIENTED_EDGE('',*,*,#43971,.T.);
#58924=ORIENTED_EDGE('',*,*,#43972,.F.);
#58925=ORIENTED_EDGE('',*,*,#43971,.F.);
#58926=ORIENTED_EDGE('',*,*,#43973,.T.);
#58927=ORIENTED_EDGE('',*,*,#43968,.T.);
#58928=ORIENTED_EDGE('',*,*,#43969,.T.);
#58929=ORIENTED_EDGE('',*,*,#43974,.T.);
#58930=ORIENTED_EDGE('',*,*,#43972,.T.);
#58931=ORIENTED_EDGE('',*,*,#43974,.F.);
#58932=ORIENTED_EDGE('',*,*,#43970,.F.);
#58933=ORIENTED_EDGE('',*,*,#43975,.T.);
#58934=ORIENTED_EDGE('',*,*,#43976,.F.);
#58935=ORIENTED_EDGE('',*,*,#43977,.F.);
#58936=ORIENTED_EDGE('',*,*,#43975,.F.);
#58937=ORIENTED_EDGE('',*,*,#43973,.F.);
#58938=ORIENTED_EDGE('',*,*,#43978,.T.);
#58939=ORIENTED_EDGE('',*,*,#43979,.T.);
#58940=ORIENTED_EDGE('',*,*,#43980,.F.);
#58941=ORIENTED_EDGE('',*,*,#43979,.F.);
#58942=ORIENTED_EDGE('',*,*,#43981,.T.);
#58943=ORIENTED_EDGE('',*,*,#43976,.T.);
#58944=ORIENTED_EDGE('',*,*,#43977,.T.);
#58945=ORIENTED_EDGE('',*,*,#43982,.T.);
#58946=ORIENTED_EDGE('',*,*,#43980,.T.);
#58947=ORIENTED_EDGE('',*,*,#43982,.F.);
#58948=ORIENTED_EDGE('',*,*,#43978,.F.);
#58949=ORIENTED_EDGE('',*,*,#43983,.T.);
#58950=ORIENTED_EDGE('',*,*,#43984,.F.);
#58951=ORIENTED_EDGE('',*,*,#43985,.F.);
#58952=ORIENTED_EDGE('',*,*,#43983,.F.);
#58953=ORIENTED_EDGE('',*,*,#43981,.F.);
#58954=ORIENTED_EDGE('',*,*,#43986,.T.);
#58955=ORIENTED_EDGE('',*,*,#43987,.T.);
#58956=ORIENTED_EDGE('',*,*,#43988,.F.);
#58957=ORIENTED_EDGE('',*,*,#43987,.F.);
#58958=ORIENTED_EDGE('',*,*,#43989,.T.);
#58959=ORIENTED_EDGE('',*,*,#43984,.T.);
#58960=ORIENTED_EDGE('',*,*,#43985,.T.);
#58961=ORIENTED_EDGE('',*,*,#43990,.T.);
#58962=ORIENTED_EDGE('',*,*,#43988,.T.);
#58963=ORIENTED_EDGE('',*,*,#43990,.F.);
#58964=ORIENTED_EDGE('',*,*,#43986,.F.);
#58965=ORIENTED_EDGE('',*,*,#43991,.T.);
#58966=ORIENTED_EDGE('',*,*,#43992,.F.);
#58967=ORIENTED_EDGE('',*,*,#43993,.F.);
#58968=ORIENTED_EDGE('',*,*,#43991,.F.);
#58969=ORIENTED_EDGE('',*,*,#43989,.F.);
#58970=ORIENTED_EDGE('',*,*,#43994,.T.);
#58971=ORIENTED_EDGE('',*,*,#43995,.T.);
#58972=ORIENTED_EDGE('',*,*,#43996,.F.);
#58973=ORIENTED_EDGE('',*,*,#43995,.F.);
#58974=ORIENTED_EDGE('',*,*,#43997,.T.);
#58975=ORIENTED_EDGE('',*,*,#43992,.T.);
#58976=ORIENTED_EDGE('',*,*,#43993,.T.);
#58977=ORIENTED_EDGE('',*,*,#43998,.T.);
#58978=ORIENTED_EDGE('',*,*,#43996,.T.);
#58979=ORIENTED_EDGE('',*,*,#43998,.F.);
#58980=ORIENTED_EDGE('',*,*,#43994,.F.);
#58981=ORIENTED_EDGE('',*,*,#43999,.T.);
#58982=ORIENTED_EDGE('',*,*,#44000,.F.);
#58983=ORIENTED_EDGE('',*,*,#44001,.F.);
#58984=ORIENTED_EDGE('',*,*,#43999,.F.);
#58985=ORIENTED_EDGE('',*,*,#43997,.F.);
#58986=ORIENTED_EDGE('',*,*,#44002,.T.);
#58987=ORIENTED_EDGE('',*,*,#44003,.T.);
#58988=ORIENTED_EDGE('',*,*,#44004,.F.);
#58989=ORIENTED_EDGE('',*,*,#44003,.F.);
#58990=ORIENTED_EDGE('',*,*,#44005,.T.);
#58991=ORIENTED_EDGE('',*,*,#44000,.T.);
#58992=ORIENTED_EDGE('',*,*,#44001,.T.);
#58993=ORIENTED_EDGE('',*,*,#44006,.T.);
#58994=ORIENTED_EDGE('',*,*,#44004,.T.);
#58995=ORIENTED_EDGE('',*,*,#44006,.F.);
#58996=ORIENTED_EDGE('',*,*,#44002,.F.);
#58997=ORIENTED_EDGE('',*,*,#44007,.T.);
#58998=ORIENTED_EDGE('',*,*,#44008,.F.);
#58999=ORIENTED_EDGE('',*,*,#44009,.F.);
#59000=ORIENTED_EDGE('',*,*,#44007,.F.);
#59001=ORIENTED_EDGE('',*,*,#44005,.F.);
#59002=ORIENTED_EDGE('',*,*,#44010,.T.);
#59003=ORIENTED_EDGE('',*,*,#44011,.T.);
#59004=ORIENTED_EDGE('',*,*,#44012,.F.);
#59005=ORIENTED_EDGE('',*,*,#44011,.F.);
#59006=ORIENTED_EDGE('',*,*,#44013,.T.);
#59007=ORIENTED_EDGE('',*,*,#44008,.T.);
#59008=ORIENTED_EDGE('',*,*,#44009,.T.);
#59009=ORIENTED_EDGE('',*,*,#44014,.T.);
#59010=ORIENTED_EDGE('',*,*,#44012,.T.);
#59011=ORIENTED_EDGE('',*,*,#44014,.F.);
#59012=ORIENTED_EDGE('',*,*,#43671,.F.);
#59013=ORIENTED_EDGE('',*,*,#43713,.F.);
#59014=ORIENTED_EDGE('',*,*,#43680,.F.);
#59015=ORIENTED_EDGE('',*,*,#43716,.T.);
#59016=ORIENTED_EDGE('',*,*,#44010,.F.);
#59017=ORIENTED_EDGE('',*,*,#44015,.T.);
#59018=ORIENTED_EDGE('',*,*,#44016,.T.);
#59019=ORIENTED_EDGE('',*,*,#44017,.T.);
#59020=ORIENTED_EDGE('',*,*,#44015,.F.);
#59021=ORIENTED_EDGE('',*,*,#44013,.F.);
#59022=ORIENTED_EDGE('',*,*,#44018,.F.);
#59023=ORIENTED_EDGE('',*,*,#44019,.F.);
#59024=ORIENTED_EDGE('',*,*,#44020,.T.);
#59025=ORIENTED_EDGE('',*,*,#44021,.F.);
#59026=ORIENTED_EDGE('',*,*,#44020,.F.);
#59027=ORIENTED_EDGE('',*,*,#44017,.F.);
#59028=ORIENTED_EDGE('',*,*,#44022,.T.);
#59029=ORIENTED_EDGE('',*,*,#44021,.T.);
#59030=ORIENTED_EDGE('',*,*,#44022,.F.);
#59031=ORIENTED_EDGE('',*,*,#44016,.F.);
#59032=ORIENTED_EDGE('',*,*,#44018,.T.);
#59033=ORIENTED_EDGE('',*,*,#44019,.T.);
#59034=ORIENTED_EDGE('',*,*,#44023,.T.);
#59035=ORIENTED_EDGE('',*,*,#43642,.T.);
#59036=ORIENTED_EDGE('',*,*,#44023,.F.);
#59037=ORIENTED_EDGE('',*,*,#43626,.F.);
#59038=ORIENTED_EDGE('',*,*,#44024,.T.);
#59039=ORIENTED_EDGE('',*,*,#43842,.T.);
#59040=ORIENTED_EDGE('',*,*,#44024,.F.);
#59041=ORIENTED_EDGE('',*,*,#43664,.F.);
#59042=ORIENTED_EDGE('',*,*,#43714,.F.);
#59043=ORIENTED_EDGE('',*,*,#43695,.F.);
#59044=ORIENTED_EDGE('',*,*,#43709,.T.);
#59045=ORIENTED_EDGE('',*,*,#43655,.F.);
#59046=ORIENTED_EDGE('',*,*,#44025,.F.);
#59047=ORIENTED_EDGE('',*,*,#44026,.T.);
#59048=ORIENTED_EDGE('',*,*,#44027,.F.);
#59049=ORIENTED_EDGE('',*,*,#44028,.F.);
#59050=ORIENTED_EDGE('',*,*,#44029,.F.);
#59051=ORIENTED_EDGE('',*,*,#44030,.F.);
#59052=ORIENTED_EDGE('',*,*,#44031,.F.);
#59053=ORIENTED_EDGE('',*,*,#44032,.T.);
#59054=ORIENTED_EDGE('',*,*,#44033,.F.);
#59055=ORIENTED_EDGE('',*,*,#44034,.F.);
#59056=ORIENTED_EDGE('',*,*,#44035,.F.);
#59057=ORIENTED_EDGE('',*,*,#44036,.T.);
#59058=ORIENTED_EDGE('',*,*,#44037,.F.);
#59059=ORIENTED_EDGE('',*,*,#44038,.T.);
#59060=ORIENTED_EDGE('',*,*,#44039,.F.);
#59061=ORIENTED_EDGE('',*,*,#44026,.F.);
#59062=ORIENTED_EDGE('',*,*,#44040,.F.);
#59063=ORIENTED_EDGE('',*,*,#44032,.F.);
#59064=ORIENTED_EDGE('',*,*,#44041,.F.);
#59065=ORIENTED_EDGE('',*,*,#44042,.T.);
#59066=ORIENTED_EDGE('',*,*,#44043,.F.);
#59067=ORIENTED_EDGE('',*,*,#44036,.F.);
#59068=ORIENTED_EDGE('',*,*,#44044,.F.);
#59069=ORIENTED_EDGE('',*,*,#44045,.T.);
#59070=ORIENTED_EDGE('',*,*,#44046,.F.);
#59071=ORIENTED_EDGE('',*,*,#44047,.T.);
#59072=ORIENTED_EDGE('',*,*,#44048,.F.);
#59073=ORIENTED_EDGE('',*,*,#44038,.F.);
#59074=ORIENTED_EDGE('',*,*,#44049,.F.);
#59075=ORIENTED_EDGE('',*,*,#44042,.F.);
#59076=ORIENTED_EDGE('',*,*,#44050,.F.);
#59077=ORIENTED_EDGE('',*,*,#44051,.T.);
#59078=ORIENTED_EDGE('',*,*,#44052,.F.);
#59079=ORIENTED_EDGE('',*,*,#44045,.F.);
#59080=ORIENTED_EDGE('',*,*,#44053,.F.);
#59081=ORIENTED_EDGE('',*,*,#44054,.T.);
#59082=ORIENTED_EDGE('',*,*,#44055,.F.);
#59083=ORIENTED_EDGE('',*,*,#44056,.T.);
#59084=ORIENTED_EDGE('',*,*,#44057,.F.);
#59085=ORIENTED_EDGE('',*,*,#44047,.F.);
#59086=ORIENTED_EDGE('',*,*,#44058,.F.);
#59087=ORIENTED_EDGE('',*,*,#44051,.F.);
#59088=ORIENTED_EDGE('',*,*,#44059,.F.);
#59089=ORIENTED_EDGE('',*,*,#44060,.T.);
#59090=ORIENTED_EDGE('',*,*,#44061,.F.);
#59091=ORIENTED_EDGE('',*,*,#44054,.F.);
#59092=ORIENTED_EDGE('',*,*,#44062,.F.);
#59093=ORIENTED_EDGE('',*,*,#44063,.T.);
#59094=ORIENTED_EDGE('',*,*,#44064,.F.);
#59095=ORIENTED_EDGE('',*,*,#44065,.T.);
#59096=ORIENTED_EDGE('',*,*,#44066,.T.);
#59097=ORIENTED_EDGE('',*,*,#44067,.T.);
#59098=ORIENTED_EDGE('',*,*,#44034,.T.);
#59099=ORIENTED_EDGE('',*,*,#44068,.F.);
#59100=ORIENTED_EDGE('',*,*,#44069,.T.);
#59101=ORIENTED_EDGE('',*,*,#44070,.T.);
#59102=ORIENTED_EDGE('',*,*,#44030,.T.);
#59103=ORIENTED_EDGE('',*,*,#44071,.F.);
#59104=ORIENTED_EDGE('',*,*,#44072,.T.);
#59105=ORIENTED_EDGE('',*,*,#44073,.T.);
#59106=ORIENTED_EDGE('',*,*,#44028,.T.);
#59107=ORIENTED_EDGE('',*,*,#44074,.F.);
#59108=ORIENTED_EDGE('',*,*,#44075,.T.);
#59109=ORIENTED_EDGE('',*,*,#44076,.T.);
#59110=ORIENTED_EDGE('',*,*,#44077,.T.);
#59111=ORIENTED_EDGE('',*,*,#44078,.F.);
#59112=ORIENTED_EDGE('',*,*,#44079,.T.);
#59113=ORIENTED_EDGE('',*,*,#44065,.F.);
#59114=ORIENTED_EDGE('',*,*,#44080,.F.);
#59115=ORIENTED_EDGE('',*,*,#44081,.T.);
#59116=ORIENTED_EDGE('',*,*,#44082,.F.);
#59117=ORIENTED_EDGE('',*,*,#44077,.F.);
#59118=ORIENTED_EDGE('',*,*,#44083,.F.);
#59119=ORIENTED_EDGE('',*,*,#44084,.T.);
#59120=ORIENTED_EDGE('',*,*,#44085,.F.);
#59121=ORIENTED_EDGE('',*,*,#44081,.F.);
#59122=ORIENTED_EDGE('',*,*,#44086,.F.);
#59123=ORIENTED_EDGE('',*,*,#44087,.T.);
#59124=ORIENTED_EDGE('',*,*,#44088,.F.);
#59125=ORIENTED_EDGE('',*,*,#44084,.F.);
#59126=ORIENTED_EDGE('',*,*,#44089,.F.);
#59127=ORIENTED_EDGE('',*,*,#44090,.T.);
#59128=ORIENTED_EDGE('',*,*,#44091,.F.);
#59129=ORIENTED_EDGE('',*,*,#44087,.F.);
#59130=ORIENTED_EDGE('',*,*,#44092,.T.);
#59131=ORIENTED_EDGE('',*,*,#44093,.T.);
#59132=ORIENTED_EDGE('',*,*,#44094,.T.);
#59133=ORIENTED_EDGE('',*,*,#44093,.F.);
#59134=ORIENTED_EDGE('',*,*,#44095,.T.);
#59135=ORIENTED_EDGE('',*,*,#44096,.F.);
#59136=ORIENTED_EDGE('',*,*,#44090,.F.);
#59137=ORIENTED_EDGE('',*,*,#44097,.F.);
#59138=ORIENTED_EDGE('',*,*,#44098,.T.);
#59139=ORIENTED_EDGE('',*,*,#44099,.F.);
#59140=ORIENTED_EDGE('',*,*,#44056,.F.);
#59141=ORIENTED_EDGE('',*,*,#44100,.F.);
#59142=ORIENTED_EDGE('',*,*,#44101,.T.);
#59143=ORIENTED_EDGE('',*,*,#44102,.F.);
#59144=ORIENTED_EDGE('',*,*,#44060,.F.);
#59145=ORIENTED_EDGE('',*,*,#44103,.F.);
#59146=ORIENTED_EDGE('',*,*,#44104,.T.);
#59147=ORIENTED_EDGE('',*,*,#44105,.F.);
#59148=ORIENTED_EDGE('',*,*,#44063,.F.);
#59149=ORIENTED_EDGE('',*,*,#44106,.F.);
#59150=ORIENTED_EDGE('',*,*,#44107,.T.);
#59151=ORIENTED_EDGE('',*,*,#44094,.F.);
#59152=ORIENTED_EDGE('',*,*,#44107,.F.);
#59153=ORIENTED_EDGE('',*,*,#44108,.T.);
#59154=ORIENTED_EDGE('',*,*,#44109,.T.);
#59155=ORIENTED_EDGE('',*,*,#44108,.F.);
#59156=ORIENTED_EDGE('',*,*,#44109,.F.);
#59157=ORIENTED_EDGE('',*,*,#44064,.T.);
#59158=ORIENTED_EDGE('',*,*,#44085,.T.);
#59159=ORIENTED_EDGE('',*,*,#44088,.T.);
#59160=ORIENTED_EDGE('',*,*,#44091,.T.);
#59161=ORIENTED_EDGE('',*,*,#44096,.T.);
#59162=ORIENTED_EDGE('',*,*,#44110,.T.);
#59163=ORIENTED_EDGE('',*,*,#44078,.T.);
#59164=ORIENTED_EDGE('',*,*,#44082,.T.);
#59165=ORIENTED_EDGE('',*,*,#44044,.T.);
#59166=ORIENTED_EDGE('',*,*,#44035,.T.);
#59167=ORIENTED_EDGE('',*,*,#44067,.F.);
#59168=ORIENTED_EDGE('',*,*,#44111,.T.);
#59169=ORIENTED_EDGE('',*,*,#44106,.T.);
#59170=ORIENTED_EDGE('',*,*,#44062,.T.);
#59171=ORIENTED_EDGE('',*,*,#44053,.T.);
#59172=ORIENTED_EDGE('',*,*,#44110,.F.);
#59173=ORIENTED_EDGE('',*,*,#44095,.F.);
#59174=ORIENTED_EDGE('',*,*,#44092,.F.);
#59175=ORIENTED_EDGE('',*,*,#44111,.F.);
#59176=ORIENTED_EDGE('',*,*,#44066,.F.);
#59177=ORIENTED_EDGE('',*,*,#44079,.F.);
#59178=ORIENTED_EDGE('',*,*,#44039,.T.);
#59179=ORIENTED_EDGE('',*,*,#44048,.T.);
#59180=ORIENTED_EDGE('',*,*,#44057,.T.);
#59181=ORIENTED_EDGE('',*,*,#44099,.T.);
#59182=ORIENTED_EDGE('',*,*,#44112,.T.);
#59183=ORIENTED_EDGE('',*,*,#44074,.T.);
#59184=ORIENTED_EDGE('',*,*,#44027,.T.);
#59185=ORIENTED_EDGE('',*,*,#44083,.T.);
#59186=ORIENTED_EDGE('',*,*,#44080,.T.);
#59187=ORIENTED_EDGE('',*,*,#44076,.F.);
#59188=ORIENTED_EDGE('',*,*,#44113,.T.);
#59189=ORIENTED_EDGE('',*,*,#44097,.T.);
#59190=ORIENTED_EDGE('',*,*,#44089,.T.);
#59191=ORIENTED_EDGE('',*,*,#44086,.T.);
#59192=ORIENTED_EDGE('',*,*,#44112,.F.);
#59193=ORIENTED_EDGE('',*,*,#44098,.F.);
#59194=ORIENTED_EDGE('',*,*,#44113,.F.);
#59195=ORIENTED_EDGE('',*,*,#44075,.F.);
#59196=ORIENTED_EDGE('',*,*,#44041,.T.);
#59197=ORIENTED_EDGE('',*,*,#44031,.T.);
#59198=ORIENTED_EDGE('',*,*,#44070,.F.);
#59199=ORIENTED_EDGE('',*,*,#44114,.T.);
#59200=ORIENTED_EDGE('',*,*,#44103,.T.);
#59201=ORIENTED_EDGE('',*,*,#44059,.T.);
#59202=ORIENTED_EDGE('',*,*,#44050,.T.);
#59203=ORIENTED_EDGE('',*,*,#44043,.T.);
#59204=ORIENTED_EDGE('',*,*,#44052,.T.);
#59205=ORIENTED_EDGE('',*,*,#44061,.T.);
#59206=ORIENTED_EDGE('',*,*,#44105,.T.);
#59207=ORIENTED_EDGE('',*,*,#44115,.T.);
#59208=ORIENTED_EDGE('',*,*,#44068,.T.);
#59209=ORIENTED_EDGE('',*,*,#44033,.T.);
#59210=ORIENTED_EDGE('',*,*,#44115,.F.);
#59211=ORIENTED_EDGE('',*,*,#44104,.F.);
#59212=ORIENTED_EDGE('',*,*,#44114,.F.);
#59213=ORIENTED_EDGE('',*,*,#44069,.F.);
#59214=ORIENTED_EDGE('',*,*,#44037,.T.);
#59215=ORIENTED_EDGE('',*,*,#44025,.T.);
#59216=ORIENTED_EDGE('',*,*,#44073,.F.);
#59217=ORIENTED_EDGE('',*,*,#44116,.T.);
#59218=ORIENTED_EDGE('',*,*,#44100,.T.);
#59219=ORIENTED_EDGE('',*,*,#44055,.T.);
#59220=ORIENTED_EDGE('',*,*,#44046,.T.);
#59221=ORIENTED_EDGE('',*,*,#44040,.T.);
#59222=ORIENTED_EDGE('',*,*,#44049,.T.);
#59223=ORIENTED_EDGE('',*,*,#44058,.T.);
#59224=ORIENTED_EDGE('',*,*,#44102,.T.);
#59225=ORIENTED_EDGE('',*,*,#44117,.T.);
#59226=ORIENTED_EDGE('',*,*,#44071,.T.);
#59227=ORIENTED_EDGE('',*,*,#44029,.T.);
#59228=ORIENTED_EDGE('',*,*,#44117,.F.);
#59229=ORIENTED_EDGE('',*,*,#44101,.F.);
#59230=ORIENTED_EDGE('',*,*,#44116,.F.);
#59231=ORIENTED_EDGE('',*,*,#44072,.F.);
#59232=ORIENTED_EDGE('',*,*,#44118,.T.);
#59233=ORIENTED_EDGE('',*,*,#44119,.T.);
#59234=ORIENTED_EDGE('',*,*,#44120,.T.);
#59235=ORIENTED_EDGE('',*,*,#44121,.T.);
#59236=ORIENTED_EDGE('',*,*,#44121,.F.);
#59237=ORIENTED_EDGE('',*,*,#44122,.T.);
#59238=ORIENTED_EDGE('',*,*,#44123,.F.);
#59239=ORIENTED_EDGE('',*,*,#44124,.F.);
#59240=ORIENTED_EDGE('',*,*,#44120,.F.);
#59241=ORIENTED_EDGE('',*,*,#44125,.T.);
#59242=ORIENTED_EDGE('',*,*,#44126,.F.);
#59243=ORIENTED_EDGE('',*,*,#44127,.T.);
#59244=ORIENTED_EDGE('',*,*,#44128,.F.);
#59245=ORIENTED_EDGE('',*,*,#44129,.F.);
#59246=ORIENTED_EDGE('',*,*,#44130,.F.);
#59247=ORIENTED_EDGE('',*,*,#44131,.T.);
#59248=ORIENTED_EDGE('',*,*,#44132,.T.);
#59249=ORIENTED_EDGE('',*,*,#44133,.F.);
#59250=ORIENTED_EDGE('',*,*,#44134,.F.);
#59251=ORIENTED_EDGE('',*,*,#44122,.F.);
#59252=ORIENTED_EDGE('',*,*,#44135,.T.);
#59253=ORIENTED_EDGE('',*,*,#44123,.T.);
#59254=ORIENTED_EDGE('',*,*,#44134,.T.);
#59255=ORIENTED_EDGE('',*,*,#44136,.T.);
#59256=ORIENTED_EDGE('',*,*,#44136,.F.);
#59257=ORIENTED_EDGE('',*,*,#44133,.T.);
#59258=ORIENTED_EDGE('',*,*,#44137,.T.);
#59259=ORIENTED_EDGE('',*,*,#44138,.F.);
#59260=ORIENTED_EDGE('',*,*,#44139,.T.);
#59261=ORIENTED_EDGE('',*,*,#44140,.T.);
#59262=ORIENTED_EDGE('',*,*,#44126,.T.);
#59263=ORIENTED_EDGE('',*,*,#44141,.T.);
#59264=ORIENTED_EDGE('',*,*,#44119,.F.);
#59265=ORIENTED_EDGE('',*,*,#44142,.F.);
#59266=ORIENTED_EDGE('',*,*,#44141,.F.);
#59267=ORIENTED_EDGE('',*,*,#44125,.F.);
#59268=ORIENTED_EDGE('',*,*,#44143,.T.);
#59269=ORIENTED_EDGE('',*,*,#44144,.T.);
#59270=ORIENTED_EDGE('',*,*,#44128,.T.);
#59271=ORIENTED_EDGE('',*,*,#44145,.T.);
#59272=ORIENTED_EDGE('',*,*,#44144,.F.);
#59273=ORIENTED_EDGE('',*,*,#44146,.F.);
#59274=ORIENTED_EDGE('',*,*,#44147,.F.);
#59275=ORIENTED_EDGE('',*,*,#44129,.T.);
#59276=ORIENTED_EDGE('',*,*,#44131,.F.);
#59277=ORIENTED_EDGE('',*,*,#44148,.T.);
#59278=ORIENTED_EDGE('',*,*,#44149,.F.);
#59279=ORIENTED_EDGE('',*,*,#44150,.F.);
#59280=ORIENTED_EDGE('',*,*,#44151,.T.);
#59281=ORIENTED_EDGE('',*,*,#44152,.T.);
#59282=ORIENTED_EDGE('',*,*,#44153,.T.);
#59283=ORIENTED_EDGE('',*,*,#44149,.T.);
#59284=ORIENTED_EDGE('',*,*,#44154,.F.);
#59285=ORIENTED_EDGE('',*,*,#44155,.F.);
#59286=ORIENTED_EDGE('',*,*,#44156,.F.);
#59287=ORIENTED_EDGE('',*,*,#44152,.F.);
#59288=ORIENTED_EDGE('',*,*,#44156,.T.);
#59289=ORIENTED_EDGE('',*,*,#44157,.F.);
#59290=ORIENTED_EDGE('',*,*,#44137,.F.);
#59291=ORIENTED_EDGE('',*,*,#44132,.F.);
#59292=ORIENTED_EDGE('',*,*,#44150,.T.);
#59293=ORIENTED_EDGE('',*,*,#44153,.F.);
#59294=ORIENTED_EDGE('',*,*,#44140,.F.);
#59295=ORIENTED_EDGE('',*,*,#44158,.F.);
#59296=ORIENTED_EDGE('',*,*,#44145,.F.);
#59297=ORIENTED_EDGE('',*,*,#44127,.F.);
#59298=ORIENTED_EDGE('',*,*,#44130,.T.);
#59299=ORIENTED_EDGE('',*,*,#44147,.T.);
#59300=ORIENTED_EDGE('',*,*,#44159,.F.);
#59301=ORIENTED_EDGE('',*,*,#44154,.T.);
#59302=ORIENTED_EDGE('',*,*,#44151,.F.);
#59303=ORIENTED_EDGE('',*,*,#44148,.F.);
#59304=ORIENTED_EDGE('',*,*,#44118,.F.);
#59305=ORIENTED_EDGE('',*,*,#44124,.T.);
#59306=ORIENTED_EDGE('',*,*,#44135,.F.);
#59307=ORIENTED_EDGE('',*,*,#44138,.T.);
#59308=ORIENTED_EDGE('',*,*,#44157,.T.);
#59309=ORIENTED_EDGE('',*,*,#44155,.T.);
#59310=ORIENTED_EDGE('',*,*,#44159,.T.);
#59311=ORIENTED_EDGE('',*,*,#44146,.T.);
#59312=ORIENTED_EDGE('',*,*,#44143,.F.);
#59313=ORIENTED_EDGE('',*,*,#44158,.T.);
#59314=ORIENTED_EDGE('',*,*,#44139,.F.);
#59315=ORIENTED_EDGE('',*,*,#44142,.T.);
#59316=ORIENTED_EDGE('',*,*,#44160,.T.);
#59317=ORIENTED_EDGE('',*,*,#44161,.T.);
#59318=ORIENTED_EDGE('',*,*,#44162,.T.);
#59319=ORIENTED_EDGE('',*,*,#44163,.T.);
#59320=ORIENTED_EDGE('',*,*,#44164,.T.);
#59321=ORIENTED_EDGE('',*,*,#44165,.T.);
#59322=ORIENTED_EDGE('',*,*,#44162,.F.);
#59323=ORIENTED_EDGE('',*,*,#44166,.T.);
#59324=ORIENTED_EDGE('',*,*,#44167,.T.);
#59325=ORIENTED_EDGE('',*,*,#44168,.T.);
#59326=ORIENTED_EDGE('',*,*,#44164,.F.);
#59327=ORIENTED_EDGE('',*,*,#44169,.T.);
#59328=ORIENTED_EDGE('',*,*,#44170,.T.);
#59329=ORIENTED_EDGE('',*,*,#44171,.T.);
#59330=ORIENTED_EDGE('',*,*,#44167,.F.);
#59331=ORIENTED_EDGE('',*,*,#44172,.T.);
#59332=ORIENTED_EDGE('',*,*,#44173,.T.);
#59333=ORIENTED_EDGE('',*,*,#44174,.T.);
#59334=ORIENTED_EDGE('',*,*,#44170,.F.);
#59335=ORIENTED_EDGE('',*,*,#44175,.T.);
#59336=ORIENTED_EDGE('',*,*,#44176,.T.);
#59337=ORIENTED_EDGE('',*,*,#44177,.T.);
#59338=ORIENTED_EDGE('',*,*,#44173,.F.);
#59339=ORIENTED_EDGE('',*,*,#44178,.T.);
#59340=ORIENTED_EDGE('',*,*,#44179,.T.);
#59341=ORIENTED_EDGE('',*,*,#44180,.T.);
#59342=ORIENTED_EDGE('',*,*,#44176,.F.);
#59343=ORIENTED_EDGE('',*,*,#44181,.T.);
#59344=ORIENTED_EDGE('',*,*,#44182,.T.);
#59345=ORIENTED_EDGE('',*,*,#44183,.T.);
#59346=ORIENTED_EDGE('',*,*,#44179,.F.);
#59347=ORIENTED_EDGE('',*,*,#44184,.T.);
#59348=ORIENTED_EDGE('',*,*,#44185,.T.);
#59349=ORIENTED_EDGE('',*,*,#44186,.T.);
#59350=ORIENTED_EDGE('',*,*,#44182,.F.);
#59351=ORIENTED_EDGE('',*,*,#44187,.T.);
#59352=ORIENTED_EDGE('',*,*,#44160,.F.);
#59353=ORIENTED_EDGE('',*,*,#44188,.T.);
#59354=ORIENTED_EDGE('',*,*,#44185,.F.);
#59355=ORIENTED_EDGE('',*,*,#44189,.T.);
#59356=ORIENTED_EDGE('',*,*,#44180,.F.);
#59357=ORIENTED_EDGE('',*,*,#44190,.F.);
#59358=ORIENTED_EDGE('',*,*,#44191,.T.);
#59359=ORIENTED_EDGE('',*,*,#44192,.F.);
#59360=ORIENTED_EDGE('',*,*,#44193,.T.);
#59361=ORIENTED_EDGE('',*,*,#44194,.F.);
#59362=ORIENTED_EDGE('',*,*,#44195,.F.);
#59363=ORIENTED_EDGE('',*,*,#44196,.F.);
#59364=ORIENTED_EDGE('',*,*,#44197,.F.);
#59365=ORIENTED_EDGE('',*,*,#44198,.F.);
#59366=ORIENTED_EDGE('',*,*,#44183,.F.);
#59367=ORIENTED_EDGE('',*,*,#44199,.T.);
#59368=ORIENTED_EDGE('',*,*,#44200,.T.);
#59369=ORIENTED_EDGE('',*,*,#44190,.T.);
#59370=ORIENTED_EDGE('',*,*,#44186,.F.);
#59371=ORIENTED_EDGE('',*,*,#44201,.F.);
#59372=ORIENTED_EDGE('',*,*,#44202,.F.);
#59373=ORIENTED_EDGE('',*,*,#44199,.F.);
#59374=ORIENTED_EDGE('',*,*,#44188,.F.);
#59375=ORIENTED_EDGE('',*,*,#44203,.T.);
#59376=ORIENTED_EDGE('',*,*,#44204,.T.);
#59377=ORIENTED_EDGE('',*,*,#44201,.T.);
#59378=ORIENTED_EDGE('',*,*,#44163,.F.);
#59379=ORIENTED_EDGE('',*,*,#44205,.F.);
#59380=ORIENTED_EDGE('',*,*,#44206,.F.);
#59381=ORIENTED_EDGE('',*,*,#44203,.F.);
#59382=ORIENTED_EDGE('',*,*,#44161,.F.);
#59383=ORIENTED_EDGE('',*,*,#44189,.F.);
#59384=ORIENTED_EDGE('',*,*,#44187,.F.);
#59385=ORIENTED_EDGE('',*,*,#44184,.F.);
#59386=ORIENTED_EDGE('',*,*,#44181,.F.);
#59387=ORIENTED_EDGE('',*,*,#44178,.F.);
#59388=ORIENTED_EDGE('',*,*,#44175,.F.);
#59389=ORIENTED_EDGE('',*,*,#44172,.F.);
#59390=ORIENTED_EDGE('',*,*,#44169,.F.);
#59391=ORIENTED_EDGE('',*,*,#44166,.F.);
#59392=ORIENTED_EDGE('',*,*,#44207,.T.);
#59393=ORIENTED_EDGE('',*,*,#44208,.T.);
#59394=ORIENTED_EDGE('',*,*,#44209,.T.);
#59395=ORIENTED_EDGE('',*,*,#44210,.T.);
#59396=ORIENTED_EDGE('',*,*,#44211,.T.);
#59397=ORIENTED_EDGE('',*,*,#44212,.T.);
#59398=ORIENTED_EDGE('',*,*,#44209,.F.);
#59399=ORIENTED_EDGE('',*,*,#44213,.T.);
#59400=ORIENTED_EDGE('',*,*,#44214,.T.);
#59401=ORIENTED_EDGE('',*,*,#44215,.T.);
#59402=ORIENTED_EDGE('',*,*,#44211,.F.);
#59403=ORIENTED_EDGE('',*,*,#44216,.T.);
#59404=ORIENTED_EDGE('',*,*,#44217,.T.);
#59405=ORIENTED_EDGE('',*,*,#44218,.T.);
#59406=ORIENTED_EDGE('',*,*,#44214,.F.);
#59407=ORIENTED_EDGE('',*,*,#44219,.T.);
#59408=ORIENTED_EDGE('',*,*,#44220,.T.);
#59409=ORIENTED_EDGE('',*,*,#44221,.T.);
#59410=ORIENTED_EDGE('',*,*,#44217,.F.);
#59411=ORIENTED_EDGE('',*,*,#44222,.T.);
#59412=ORIENTED_EDGE('',*,*,#44223,.T.);
#59413=ORIENTED_EDGE('',*,*,#44224,.T.);
#59414=ORIENTED_EDGE('',*,*,#44220,.F.);
#59415=ORIENTED_EDGE('',*,*,#44225,.T.);
#59416=ORIENTED_EDGE('',*,*,#44226,.T.);
#59417=ORIENTED_EDGE('',*,*,#44227,.T.);
#59418=ORIENTED_EDGE('',*,*,#44223,.F.);
#59419=ORIENTED_EDGE('',*,*,#44228,.T.);
#59420=ORIENTED_EDGE('',*,*,#44229,.T.);
#59421=ORIENTED_EDGE('',*,*,#44230,.T.);
#59422=ORIENTED_EDGE('',*,*,#44226,.F.);
#59423=ORIENTED_EDGE('',*,*,#44231,.T.);
#59424=ORIENTED_EDGE('',*,*,#44232,.T.);
#59425=ORIENTED_EDGE('',*,*,#44233,.T.);
#59426=ORIENTED_EDGE('',*,*,#44229,.F.);
#59427=ORIENTED_EDGE('',*,*,#44234,.T.);
#59428=ORIENTED_EDGE('',*,*,#44235,.T.);
#59429=ORIENTED_EDGE('',*,*,#44236,.T.);
#59430=ORIENTED_EDGE('',*,*,#44232,.F.);
#59431=ORIENTED_EDGE('',*,*,#44237,.T.);
#59432=ORIENTED_EDGE('',*,*,#44238,.T.);
#59433=ORIENTED_EDGE('',*,*,#44239,.T.);
#59434=ORIENTED_EDGE('',*,*,#44235,.F.);
#59435=ORIENTED_EDGE('',*,*,#44240,.T.);
#59436=ORIENTED_EDGE('',*,*,#44241,.T.);
#59437=ORIENTED_EDGE('',*,*,#44242,.T.);
#59438=ORIENTED_EDGE('',*,*,#44238,.F.);
#59439=ORIENTED_EDGE('',*,*,#44243,.T.);
#59440=ORIENTED_EDGE('',*,*,#44244,.T.);
#59441=ORIENTED_EDGE('',*,*,#44245,.T.);
#59442=ORIENTED_EDGE('',*,*,#44246,.T.);
#59443=ORIENTED_EDGE('',*,*,#44241,.F.);
#59444=ORIENTED_EDGE('',*,*,#44247,.T.);
#59445=ORIENTED_EDGE('',*,*,#44207,.F.);
#59446=ORIENTED_EDGE('',*,*,#44248,.T.);
#59447=ORIENTED_EDGE('',*,*,#44244,.F.);
#59448=ORIENTED_EDGE('',*,*,#44249,.T.);
#59449=ORIENTED_EDGE('',*,*,#44233,.F.);
#59450=ORIENTED_EDGE('',*,*,#44250,.F.);
#59451=ORIENTED_EDGE('',*,*,#44251,.T.);
#59452=ORIENTED_EDGE('',*,*,#44252,.F.);
#59453=ORIENTED_EDGE('',*,*,#44236,.F.);
#59454=ORIENTED_EDGE('',*,*,#44253,.T.);
#59455=ORIENTED_EDGE('',*,*,#44254,.F.);
#59456=ORIENTED_EDGE('',*,*,#44250,.T.);
#59457=ORIENTED_EDGE('',*,*,#44239,.F.);
#59458=ORIENTED_EDGE('',*,*,#44255,.F.);
#59459=ORIENTED_EDGE('',*,*,#44256,.T.);
#59460=ORIENTED_EDGE('',*,*,#44253,.F.);
#59461=ORIENTED_EDGE('',*,*,#44242,.F.);
#59462=ORIENTED_EDGE('',*,*,#44257,.T.);
#59463=ORIENTED_EDGE('',*,*,#44258,.T.);
#59464=ORIENTED_EDGE('',*,*,#44255,.T.);
#59465=ORIENTED_EDGE('',*,*,#44259,.F.);
#59466=ORIENTED_EDGE('',*,*,#44260,.T.);
#59467=ORIENTED_EDGE('',*,*,#44245,.F.);
#59468=ORIENTED_EDGE('',*,*,#44261,.F.);
#59469=ORIENTED_EDGE('',*,*,#44262,.T.);
#59470=ORIENTED_EDGE('',*,*,#44263,.F.);
#59471=ORIENTED_EDGE('',*,*,#44264,.F.);
#59472=ORIENTED_EDGE('',*,*,#44265,.F.);
#59473=ORIENTED_EDGE('',*,*,#44266,.T.);
#59474=ORIENTED_EDGE('',*,*,#44267,.F.);
#59475=ORIENTED_EDGE('',*,*,#44268,.F.);
#59476=ORIENTED_EDGE('',*,*,#44269,.F.);
#59477=ORIENTED_EDGE('',*,*,#44270,.T.);
#59478=ORIENTED_EDGE('',*,*,#44257,.F.);
#59479=ORIENTED_EDGE('',*,*,#44246,.F.);
#59480=ORIENTED_EDGE('',*,*,#44260,.F.);
#59481=ORIENTED_EDGE('',*,*,#44248,.F.);
#59482=ORIENTED_EDGE('',*,*,#44271,.T.);
#59483=ORIENTED_EDGE('',*,*,#44272,.T.);
#59484=ORIENTED_EDGE('',*,*,#44261,.T.);
#59485=ORIENTED_EDGE('',*,*,#44210,.F.);
#59486=ORIENTED_EDGE('',*,*,#44273,.F.);
#59487=ORIENTED_EDGE('',*,*,#44274,.T.);
#59488=ORIENTED_EDGE('',*,*,#44271,.F.);
#59489=ORIENTED_EDGE('',*,*,#44208,.F.);
#59490=ORIENTED_EDGE('',*,*,#44249,.F.);
#59491=ORIENTED_EDGE('',*,*,#44247,.F.);
#59492=ORIENTED_EDGE('',*,*,#44243,.F.);
#59493=ORIENTED_EDGE('',*,*,#44240,.F.);
#59494=ORIENTED_EDGE('',*,*,#44237,.F.);
#59495=ORIENTED_EDGE('',*,*,#44234,.F.);
#59496=ORIENTED_EDGE('',*,*,#44231,.F.);
#59497=ORIENTED_EDGE('',*,*,#44228,.F.);
#59498=ORIENTED_EDGE('',*,*,#44225,.F.);
#59499=ORIENTED_EDGE('',*,*,#44222,.F.);
#59500=ORIENTED_EDGE('',*,*,#44219,.F.);
#59501=ORIENTED_EDGE('',*,*,#44216,.F.);
#59502=ORIENTED_EDGE('',*,*,#44213,.F.);
#59503=ORIENTED_EDGE('',*,*,#44275,.T.);
#59504=ORIENTED_EDGE('',*,*,#44276,.T.);
#59505=ORIENTED_EDGE('',*,*,#44277,.T.);
#59506=ORIENTED_EDGE('',*,*,#44278,.T.);
#59507=ORIENTED_EDGE('',*,*,#44279,.T.);
#59508=ORIENTED_EDGE('',*,*,#44280,.T.);
#59509=ORIENTED_EDGE('',*,*,#44277,.F.);
#59510=ORIENTED_EDGE('',*,*,#44281,.T.);
#59511=ORIENTED_EDGE('',*,*,#44282,.T.);
#59512=ORIENTED_EDGE('',*,*,#44283,.T.);
#59513=ORIENTED_EDGE('',*,*,#44279,.F.);
#59514=ORIENTED_EDGE('',*,*,#44284,.T.);
#59515=ORIENTED_EDGE('',*,*,#44285,.T.);
#59516=ORIENTED_EDGE('',*,*,#44286,.T.);
#59517=ORIENTED_EDGE('',*,*,#44282,.F.);
#59518=ORIENTED_EDGE('',*,*,#44287,.T.);
#59519=ORIENTED_EDGE('',*,*,#44288,.T.);
#59520=ORIENTED_EDGE('',*,*,#44289,.T.);
#59521=ORIENTED_EDGE('',*,*,#44285,.F.);
#59522=ORIENTED_EDGE('',*,*,#44290,.T.);
#59523=ORIENTED_EDGE('',*,*,#44291,.T.);
#59524=ORIENTED_EDGE('',*,*,#44292,.T.);
#59525=ORIENTED_EDGE('',*,*,#44288,.F.);
#59526=ORIENTED_EDGE('',*,*,#44293,.T.);
#59527=ORIENTED_EDGE('',*,*,#44294,.T.);
#59528=ORIENTED_EDGE('',*,*,#44295,.T.);
#59529=ORIENTED_EDGE('',*,*,#44291,.F.);
#59530=ORIENTED_EDGE('',*,*,#44296,.T.);
#59531=ORIENTED_EDGE('',*,*,#44297,.T.);
#59532=ORIENTED_EDGE('',*,*,#44298,.T.);
#59533=ORIENTED_EDGE('',*,*,#44294,.F.);
#59534=ORIENTED_EDGE('',*,*,#44299,.T.);
#59535=ORIENTED_EDGE('',*,*,#44300,.T.);
#59536=ORIENTED_EDGE('',*,*,#44301,.T.);
#59537=ORIENTED_EDGE('',*,*,#44297,.F.);
#59538=ORIENTED_EDGE('',*,*,#44302,.T.);
#59539=ORIENTED_EDGE('',*,*,#44303,.T.);
#59540=ORIENTED_EDGE('',*,*,#44304,.T.);
#59541=ORIENTED_EDGE('',*,*,#44300,.F.);
#59542=ORIENTED_EDGE('',*,*,#44305,.T.);
#59543=ORIENTED_EDGE('',*,*,#44306,.T.);
#59544=ORIENTED_EDGE('',*,*,#44264,.T.);
#59545=ORIENTED_EDGE('',*,*,#44303,.F.);
#59546=ORIENTED_EDGE('',*,*,#44307,.T.);
#59547=ORIENTED_EDGE('',*,*,#44275,.F.);
#59548=ORIENTED_EDGE('',*,*,#44308,.T.);
#59549=ORIENTED_EDGE('',*,*,#44306,.F.);
#59550=ORIENTED_EDGE('',*,*,#44309,.T.);
#59551=ORIENTED_EDGE('',*,*,#44298,.F.);
#59552=ORIENTED_EDGE('',*,*,#44310,.T.);
#59553=ORIENTED_EDGE('',*,*,#44311,.T.);
#59554=ORIENTED_EDGE('',*,*,#44312,.T.);
#59555=ORIENTED_EDGE('',*,*,#44313,.T.);
#59556=ORIENTED_EDGE('',*,*,#44314,.T.);
#59557=ORIENTED_EDGE('',*,*,#44301,.F.);
#59558=ORIENTED_EDGE('',*,*,#44315,.F.);
#59559=ORIENTED_EDGE('',*,*,#44316,.T.);
#59560=ORIENTED_EDGE('',*,*,#44310,.F.);
#59561=ORIENTED_EDGE('',*,*,#44304,.F.);
#59562=ORIENTED_EDGE('',*,*,#44263,.T.);
#59563=ORIENTED_EDGE('',*,*,#44317,.T.);
#59564=ORIENTED_EDGE('',*,*,#44315,.T.);
#59565=ORIENTED_EDGE('',*,*,#44308,.F.);
#59566=ORIENTED_EDGE('',*,*,#44318,.T.);
#59567=ORIENTED_EDGE('',*,*,#44319,.T.);
#59568=ORIENTED_EDGE('',*,*,#44265,.T.);
#59569=ORIENTED_EDGE('',*,*,#44278,.F.);
#59570=ORIENTED_EDGE('',*,*,#44320,.F.);
#59571=ORIENTED_EDGE('',*,*,#44321,.T.);
#59572=ORIENTED_EDGE('',*,*,#44318,.F.);
#59573=ORIENTED_EDGE('',*,*,#44276,.F.);
#59574=ORIENTED_EDGE('',*,*,#44309,.F.);
#59575=ORIENTED_EDGE('',*,*,#44307,.F.);
#59576=ORIENTED_EDGE('',*,*,#44305,.F.);
#59577=ORIENTED_EDGE('',*,*,#44302,.F.);
#59578=ORIENTED_EDGE('',*,*,#44299,.F.);
#59579=ORIENTED_EDGE('',*,*,#44296,.F.);
#59580=ORIENTED_EDGE('',*,*,#44293,.F.);
#59581=ORIENTED_EDGE('',*,*,#44290,.F.);
#59582=ORIENTED_EDGE('',*,*,#44287,.F.);
#59583=ORIENTED_EDGE('',*,*,#44284,.F.);
#59584=ORIENTED_EDGE('',*,*,#44281,.F.);
#59585=ORIENTED_EDGE('',*,*,#44322,.T.);
#59586=ORIENTED_EDGE('',*,*,#44323,.T.);
#59587=ORIENTED_EDGE('',*,*,#44324,.T.);
#59588=ORIENTED_EDGE('',*,*,#44325,.T.);
#59589=ORIENTED_EDGE('',*,*,#44326,.T.);
#59590=ORIENTED_EDGE('',*,*,#44327,.T.);
#59591=ORIENTED_EDGE('',*,*,#44324,.F.);
#59592=ORIENTED_EDGE('',*,*,#44328,.T.);
#59593=ORIENTED_EDGE('',*,*,#44329,.T.);
#59594=ORIENTED_EDGE('',*,*,#44330,.T.);
#59595=ORIENTED_EDGE('',*,*,#44326,.F.);
#59596=ORIENTED_EDGE('',*,*,#44331,.T.);
#59597=ORIENTED_EDGE('',*,*,#44332,.T.);
#59598=ORIENTED_EDGE('',*,*,#44333,.T.);
#59599=ORIENTED_EDGE('',*,*,#44329,.F.);
#59600=ORIENTED_EDGE('',*,*,#44334,.T.);
#59601=ORIENTED_EDGE('',*,*,#44335,.T.);
#59602=ORIENTED_EDGE('',*,*,#44336,.T.);
#59603=ORIENTED_EDGE('',*,*,#44332,.F.);
#59604=ORIENTED_EDGE('',*,*,#44337,.T.);
#59605=ORIENTED_EDGE('',*,*,#44338,.T.);
#59606=ORIENTED_EDGE('',*,*,#44339,.T.);
#59607=ORIENTED_EDGE('',*,*,#44335,.F.);
#59608=ORIENTED_EDGE('',*,*,#44340,.T.);
#59609=ORIENTED_EDGE('',*,*,#44341,.T.);
#59610=ORIENTED_EDGE('',*,*,#44342,.T.);
#59611=ORIENTED_EDGE('',*,*,#44338,.F.);
#59612=ORIENTED_EDGE('',*,*,#44343,.T.);
#59613=ORIENTED_EDGE('',*,*,#44344,.T.);
#59614=ORIENTED_EDGE('',*,*,#44345,.T.);
#59615=ORIENTED_EDGE('',*,*,#44341,.F.);
#59616=ORIENTED_EDGE('',*,*,#44346,.T.);
#59617=ORIENTED_EDGE('',*,*,#44347,.T.);
#59618=ORIENTED_EDGE('',*,*,#44348,.T.);
#59619=ORIENTED_EDGE('',*,*,#44344,.F.);
#59620=ORIENTED_EDGE('',*,*,#44349,.T.);
#59621=ORIENTED_EDGE('',*,*,#44350,.T.);
#59622=ORIENTED_EDGE('',*,*,#44351,.T.);
#59623=ORIENTED_EDGE('',*,*,#44347,.F.);
#59624=ORIENTED_EDGE('',*,*,#44352,.T.);
#59625=ORIENTED_EDGE('',*,*,#44322,.F.);
#59626=ORIENTED_EDGE('',*,*,#44353,.T.);
#59627=ORIENTED_EDGE('',*,*,#44350,.F.);
#59628=ORIENTED_EDGE('',*,*,#44354,.T.);
#59629=ORIENTED_EDGE('',*,*,#44342,.F.);
#59630=ORIENTED_EDGE('',*,*,#44355,.F.);
#59631=ORIENTED_EDGE('',*,*,#44356,.F.);
#59632=ORIENTED_EDGE('',*,*,#44357,.T.);
#59633=ORIENTED_EDGE('',*,*,#44358,.T.);
#59634=ORIENTED_EDGE('',*,*,#44359,.T.);
#59635=ORIENTED_EDGE('',*,*,#44345,.F.);
#59636=ORIENTED_EDGE('',*,*,#44360,.F.);
#59637=ORIENTED_EDGE('',*,*,#44361,.F.);
#59638=ORIENTED_EDGE('',*,*,#44355,.T.);
#59639=ORIENTED_EDGE('',*,*,#44348,.F.);
#59640=ORIENTED_EDGE('',*,*,#44362,.T.);
#59641=ORIENTED_EDGE('',*,*,#44363,.T.);
#59642=ORIENTED_EDGE('',*,*,#44360,.T.);
#59643=ORIENTED_EDGE('',*,*,#44351,.F.);
#59644=ORIENTED_EDGE('',*,*,#44364,.F.);
#59645=ORIENTED_EDGE('',*,*,#44365,.F.);
#59646=ORIENTED_EDGE('',*,*,#44362,.F.);
#59647=ORIENTED_EDGE('',*,*,#44353,.F.);
#59648=ORIENTED_EDGE('',*,*,#44366,.T.);
#59649=ORIENTED_EDGE('',*,*,#44367,.T.);
#59650=ORIENTED_EDGE('',*,*,#44364,.T.);
#59651=ORIENTED_EDGE('',*,*,#44325,.F.);
#59652=ORIENTED_EDGE('',*,*,#44368,.F.);
#59653=ORIENTED_EDGE('',*,*,#44369,.T.);
#59654=ORIENTED_EDGE('',*,*,#44370,.F.);
#59655=ORIENTED_EDGE('',*,*,#44371,.F.);
#59656=ORIENTED_EDGE('',*,*,#44366,.F.);
#59657=ORIENTED_EDGE('',*,*,#44323,.F.);
#59658=ORIENTED_EDGE('',*,*,#44354,.F.);
#59659=ORIENTED_EDGE('',*,*,#44352,.F.);
#59660=ORIENTED_EDGE('',*,*,#44349,.F.);
#59661=ORIENTED_EDGE('',*,*,#44346,.F.);
#59662=ORIENTED_EDGE('',*,*,#44343,.F.);
#59663=ORIENTED_EDGE('',*,*,#44340,.F.);
#59664=ORIENTED_EDGE('',*,*,#44337,.F.);
#59665=ORIENTED_EDGE('',*,*,#44334,.F.);
#59666=ORIENTED_EDGE('',*,*,#44331,.F.);
#59667=ORIENTED_EDGE('',*,*,#44328,.F.);
#59668=ORIENTED_EDGE('',*,*,#44372,.T.);
#59669=ORIENTED_EDGE('',*,*,#44373,.T.);
#59670=ORIENTED_EDGE('',*,*,#44374,.T.);
#59671=ORIENTED_EDGE('',*,*,#44375,.T.);
#59672=ORIENTED_EDGE('',*,*,#44376,.T.);
#59673=ORIENTED_EDGE('',*,*,#44377,.T.);
#59674=ORIENTED_EDGE('',*,*,#44374,.F.);
#59675=ORIENTED_EDGE('',*,*,#44378,.T.);
#59676=ORIENTED_EDGE('',*,*,#44379,.T.);
#59677=ORIENTED_EDGE('',*,*,#44380,.T.);
#59678=ORIENTED_EDGE('',*,*,#44376,.F.);
#59679=ORIENTED_EDGE('',*,*,#44381,.T.);
#59680=ORIENTED_EDGE('',*,*,#44382,.T.);
#59681=ORIENTED_EDGE('',*,*,#44383,.T.);
#59682=ORIENTED_EDGE('',*,*,#44379,.F.);
#59683=ORIENTED_EDGE('',*,*,#44384,.T.);
#59684=ORIENTED_EDGE('',*,*,#44385,.T.);
#59685=ORIENTED_EDGE('',*,*,#44386,.T.);
#59686=ORIENTED_EDGE('',*,*,#44382,.F.);
#59687=ORIENTED_EDGE('',*,*,#44387,.T.);
#59688=ORIENTED_EDGE('',*,*,#44388,.T.);
#59689=ORIENTED_EDGE('',*,*,#44389,.T.);
#59690=ORIENTED_EDGE('',*,*,#44385,.F.);
#59691=ORIENTED_EDGE('',*,*,#44390,.T.);
#59692=ORIENTED_EDGE('',*,*,#44391,.T.);
#59693=ORIENTED_EDGE('',*,*,#44392,.T.);
#59694=ORIENTED_EDGE('',*,*,#44388,.F.);
#59695=ORIENTED_EDGE('',*,*,#44393,.T.);
#59696=ORIENTED_EDGE('',*,*,#44394,.T.);
#59697=ORIENTED_EDGE('',*,*,#44395,.T.);
#59698=ORIENTED_EDGE('',*,*,#44391,.F.);
#59699=ORIENTED_EDGE('',*,*,#44396,.T.);
#59700=ORIENTED_EDGE('',*,*,#44397,.T.);
#59701=ORIENTED_EDGE('',*,*,#44398,.T.);
#59702=ORIENTED_EDGE('',*,*,#44394,.F.);
#59703=ORIENTED_EDGE('',*,*,#44399,.T.);
#59704=ORIENTED_EDGE('',*,*,#44400,.T.);
#59705=ORIENTED_EDGE('',*,*,#44401,.T.);
#59706=ORIENTED_EDGE('',*,*,#44397,.F.);
#59707=ORIENTED_EDGE('',*,*,#44402,.T.);
#59708=ORIENTED_EDGE('',*,*,#44403,.T.);
#59709=ORIENTED_EDGE('',*,*,#44404,.T.);
#59710=ORIENTED_EDGE('',*,*,#44400,.F.);
#59711=ORIENTED_EDGE('',*,*,#44405,.T.);
#59712=ORIENTED_EDGE('',*,*,#44406,.T.);
#59713=ORIENTED_EDGE('',*,*,#44407,.T.);
#59714=ORIENTED_EDGE('',*,*,#44403,.F.);
#59715=ORIENTED_EDGE('',*,*,#44408,.T.);
#59716=ORIENTED_EDGE('',*,*,#44409,.T.);
#59717=ORIENTED_EDGE('',*,*,#44410,.T.);
#59718=ORIENTED_EDGE('',*,*,#44406,.F.);
#59719=ORIENTED_EDGE('',*,*,#44411,.T.);
#59720=ORIENTED_EDGE('',*,*,#44372,.F.);
#59721=ORIENTED_EDGE('',*,*,#44412,.T.);
#59722=ORIENTED_EDGE('',*,*,#44409,.F.);
#59723=ORIENTED_EDGE('',*,*,#44413,.T.);
#59724=ORIENTED_EDGE('',*,*,#44398,.F.);
#59725=ORIENTED_EDGE('',*,*,#44414,.T.);
#59726=ORIENTED_EDGE('',*,*,#44415,.T.);
#59727=ORIENTED_EDGE('',*,*,#44416,.T.);
#59728=ORIENTED_EDGE('',*,*,#44401,.F.);
#59729=ORIENTED_EDGE('',*,*,#44417,.F.);
#59730=ORIENTED_EDGE('',*,*,#44418,.F.);
#59731=ORIENTED_EDGE('',*,*,#44414,.F.);
#59732=ORIENTED_EDGE('',*,*,#44404,.F.);
#59733=ORIENTED_EDGE('',*,*,#44419,.T.);
#59734=ORIENTED_EDGE('',*,*,#44420,.T.);
#59735=ORIENTED_EDGE('',*,*,#44417,.T.);
#59736=ORIENTED_EDGE('',*,*,#44407,.F.);
#59737=ORIENTED_EDGE('',*,*,#44421,.F.);
#59738=ORIENTED_EDGE('',*,*,#44422,.F.);
#59739=ORIENTED_EDGE('',*,*,#44419,.F.);
#59740=ORIENTED_EDGE('',*,*,#44410,.F.);
#59741=ORIENTED_EDGE('',*,*,#44423,.T.);
#59742=ORIENTED_EDGE('',*,*,#44424,.T.);
#59743=ORIENTED_EDGE('',*,*,#44421,.T.);
#59744=ORIENTED_EDGE('',*,*,#44412,.F.);
#59745=ORIENTED_EDGE('',*,*,#44425,.F.);
#59746=ORIENTED_EDGE('',*,*,#44426,.T.);
#59747=ORIENTED_EDGE('',*,*,#44423,.F.);
#59748=ORIENTED_EDGE('',*,*,#44375,.F.);
#59749=ORIENTED_EDGE('',*,*,#44427,.F.);
#59750=ORIENTED_EDGE('',*,*,#44428,.T.);
#59751=ORIENTED_EDGE('',*,*,#44425,.T.);
#59752=ORIENTED_EDGE('',*,*,#44373,.F.);
#59753=ORIENTED_EDGE('',*,*,#44413,.F.);
#59754=ORIENTED_EDGE('',*,*,#44411,.F.);
#59755=ORIENTED_EDGE('',*,*,#44408,.F.);
#59756=ORIENTED_EDGE('',*,*,#44405,.F.);
#59757=ORIENTED_EDGE('',*,*,#44402,.F.);
#59758=ORIENTED_EDGE('',*,*,#44399,.F.);
#59759=ORIENTED_EDGE('',*,*,#44396,.F.);
#59760=ORIENTED_EDGE('',*,*,#44393,.F.);
#59761=ORIENTED_EDGE('',*,*,#44390,.F.);
#59762=ORIENTED_EDGE('',*,*,#44387,.F.);
#59763=ORIENTED_EDGE('',*,*,#44384,.F.);
#59764=ORIENTED_EDGE('',*,*,#44381,.F.);
#59765=ORIENTED_EDGE('',*,*,#44378,.F.);
#59766=ORIENTED_EDGE('',*,*,#44429,.T.);
#59767=ORIENTED_EDGE('',*,*,#44430,.T.);
#59768=ORIENTED_EDGE('',*,*,#44431,.T.);
#59769=ORIENTED_EDGE('',*,*,#44432,.T.);
#59770=ORIENTED_EDGE('',*,*,#44433,.T.);
#59771=ORIENTED_EDGE('',*,*,#44434,.T.);
#59772=ORIENTED_EDGE('',*,*,#44431,.F.);
#59773=ORIENTED_EDGE('',*,*,#44435,.T.);
#59774=ORIENTED_EDGE('',*,*,#44436,.T.);
#59775=ORIENTED_EDGE('',*,*,#44437,.T.);
#59776=ORIENTED_EDGE('',*,*,#44433,.F.);
#59777=ORIENTED_EDGE('',*,*,#44438,.T.);
#59778=ORIENTED_EDGE('',*,*,#44439,.T.);
#59779=ORIENTED_EDGE('',*,*,#44440,.T.);
#59780=ORIENTED_EDGE('',*,*,#44436,.F.);
#59781=ORIENTED_EDGE('',*,*,#44441,.T.);
#59782=ORIENTED_EDGE('',*,*,#44442,.T.);
#59783=ORIENTED_EDGE('',*,*,#44443,.T.);
#59784=ORIENTED_EDGE('',*,*,#44439,.F.);
#59785=ORIENTED_EDGE('',*,*,#44444,.T.);
#59786=ORIENTED_EDGE('',*,*,#44445,.T.);
#59787=ORIENTED_EDGE('',*,*,#44446,.T.);
#59788=ORIENTED_EDGE('',*,*,#44442,.F.);
#59789=ORIENTED_EDGE('',*,*,#44447,.T.);
#59790=ORIENTED_EDGE('',*,*,#44448,.T.);
#59791=ORIENTED_EDGE('',*,*,#44449,.T.);
#59792=ORIENTED_EDGE('',*,*,#44445,.F.);
#59793=ORIENTED_EDGE('',*,*,#44450,.T.);
#59794=ORIENTED_EDGE('',*,*,#44451,.T.);
#59795=ORIENTED_EDGE('',*,*,#44452,.T.);
#59796=ORIENTED_EDGE('',*,*,#44448,.F.);
#59797=ORIENTED_EDGE('',*,*,#44453,.T.);
#59798=ORIENTED_EDGE('',*,*,#44429,.F.);
#59799=ORIENTED_EDGE('',*,*,#44454,.T.);
#59800=ORIENTED_EDGE('',*,*,#44451,.F.);
#59801=ORIENTED_EDGE('',*,*,#44455,.T.);
#59802=ORIENTED_EDGE('',*,*,#44446,.F.);
#59803=ORIENTED_EDGE('',*,*,#44456,.F.);
#59804=ORIENTED_EDGE('',*,*,#44457,.T.);
#59805=ORIENTED_EDGE('',*,*,#44458,.F.);
#59806=ORIENTED_EDGE('',*,*,#44449,.F.);
#59807=ORIENTED_EDGE('',*,*,#44459,.T.);
#59808=ORIENTED_EDGE('',*,*,#44460,.T.);
#59809=ORIENTED_EDGE('',*,*,#44456,.T.);
#59810=ORIENTED_EDGE('',*,*,#44452,.F.);
#59811=ORIENTED_EDGE('',*,*,#44461,.F.);
#59812=ORIENTED_EDGE('',*,*,#44462,.F.);
#59813=ORIENTED_EDGE('',*,*,#44459,.F.);
#59814=ORIENTED_EDGE('',*,*,#44454,.F.);
#59815=ORIENTED_EDGE('',*,*,#44463,.T.);
#59816=ORIENTED_EDGE('',*,*,#44464,.F.);
#59817=ORIENTED_EDGE('',*,*,#44461,.T.);
#59818=ORIENTED_EDGE('',*,*,#44432,.F.);
#59819=ORIENTED_EDGE('',*,*,#44465,.F.);
#59820=ORIENTED_EDGE('',*,*,#44466,.F.);
#59821=ORIENTED_EDGE('',*,*,#44463,.F.);
#59822=ORIENTED_EDGE('',*,*,#44430,.F.);
#59823=ORIENTED_EDGE('',*,*,#44455,.F.);
#59824=ORIENTED_EDGE('',*,*,#44453,.F.);
#59825=ORIENTED_EDGE('',*,*,#44450,.F.);
#59826=ORIENTED_EDGE('',*,*,#44447,.F.);
#59827=ORIENTED_EDGE('',*,*,#44444,.F.);
#59828=ORIENTED_EDGE('',*,*,#44441,.F.);
#59829=ORIENTED_EDGE('',*,*,#44438,.F.);
#59830=ORIENTED_EDGE('',*,*,#44435,.F.);
#59831=ORIENTED_EDGE('',*,*,#44467,.T.);
#59832=ORIENTED_EDGE('',*,*,#44468,.T.);
#59833=ORIENTED_EDGE('',*,*,#44469,.T.);
#59834=ORIENTED_EDGE('',*,*,#44470,.T.);
#59835=ORIENTED_EDGE('',*,*,#44471,.T.);
#59836=ORIENTED_EDGE('',*,*,#44472,.T.);
#59837=ORIENTED_EDGE('',*,*,#44469,.F.);
#59838=ORIENTED_EDGE('',*,*,#44473,.T.);
#59839=ORIENTED_EDGE('',*,*,#44474,.T.);
#59840=ORIENTED_EDGE('',*,*,#44475,.T.);
#59841=ORIENTED_EDGE('',*,*,#44471,.F.);
#59842=ORIENTED_EDGE('',*,*,#44476,.T.);
#59843=ORIENTED_EDGE('',*,*,#44477,.T.);
#59844=ORIENTED_EDGE('',*,*,#44478,.T.);
#59845=ORIENTED_EDGE('',*,*,#44474,.F.);
#59846=ORIENTED_EDGE('',*,*,#44479,.T.);
#59847=ORIENTED_EDGE('',*,*,#44480,.T.);
#59848=ORIENTED_EDGE('',*,*,#44481,.T.);
#59849=ORIENTED_EDGE('',*,*,#44477,.F.);
#59850=ORIENTED_EDGE('',*,*,#44482,.T.);
#59851=ORIENTED_EDGE('',*,*,#44483,.T.);
#59852=ORIENTED_EDGE('',*,*,#44484,.T.);
#59853=ORIENTED_EDGE('',*,*,#44480,.F.);
#59854=ORIENTED_EDGE('',*,*,#44485,.T.);
#59855=ORIENTED_EDGE('',*,*,#44486,.T.);
#59856=ORIENTED_EDGE('',*,*,#44487,.T.);
#59857=ORIENTED_EDGE('',*,*,#44483,.F.);
#59858=ORIENTED_EDGE('',*,*,#44488,.T.);
#59859=ORIENTED_EDGE('',*,*,#44489,.T.);
#59860=ORIENTED_EDGE('',*,*,#44490,.T.);
#59861=ORIENTED_EDGE('',*,*,#44486,.F.);
#59862=ORIENTED_EDGE('',*,*,#44491,.T.);
#59863=ORIENTED_EDGE('',*,*,#44492,.T.);
#59864=ORIENTED_EDGE('',*,*,#44493,.T.);
#59865=ORIENTED_EDGE('',*,*,#44489,.F.);
#59866=ORIENTED_EDGE('',*,*,#44494,.T.);
#59867=ORIENTED_EDGE('',*,*,#44495,.T.);
#59868=ORIENTED_EDGE('',*,*,#44496,.T.);
#59869=ORIENTED_EDGE('',*,*,#44492,.F.);
#59870=ORIENTED_EDGE('',*,*,#44497,.T.);
#59871=ORIENTED_EDGE('',*,*,#44498,.T.);
#59872=ORIENTED_EDGE('',*,*,#44499,.T.);
#59873=ORIENTED_EDGE('',*,*,#44495,.F.);
#59874=ORIENTED_EDGE('',*,*,#44500,.T.);
#59875=ORIENTED_EDGE('',*,*,#44501,.T.);
#59876=ORIENTED_EDGE('',*,*,#44502,.T.);
#59877=ORIENTED_EDGE('',*,*,#44498,.F.);
#59878=ORIENTED_EDGE('',*,*,#44503,.T.);
#59879=ORIENTED_EDGE('',*,*,#44504,.T.);
#59880=ORIENTED_EDGE('',*,*,#44505,.T.);
#59881=ORIENTED_EDGE('',*,*,#44501,.F.);
#59882=ORIENTED_EDGE('',*,*,#44506,.T.);
#59883=ORIENTED_EDGE('',*,*,#44507,.T.);
#59884=ORIENTED_EDGE('',*,*,#44508,.T.);
#59885=ORIENTED_EDGE('',*,*,#44504,.F.);
#59886=ORIENTED_EDGE('',*,*,#44509,.T.);
#59887=ORIENTED_EDGE('',*,*,#44510,.T.);
#59888=ORIENTED_EDGE('',*,*,#44511,.T.);
#59889=ORIENTED_EDGE('',*,*,#44507,.F.);
#59890=ORIENTED_EDGE('',*,*,#44512,.T.);
#59891=ORIENTED_EDGE('',*,*,#44467,.F.);
#59892=ORIENTED_EDGE('',*,*,#44513,.T.);
#59893=ORIENTED_EDGE('',*,*,#44510,.F.);
#59894=ORIENTED_EDGE('',*,*,#44514,.T.);
#59895=ORIENTED_EDGE('',*,*,#44496,.F.);
#59896=ORIENTED_EDGE('',*,*,#44515,.T.);
#59897=ORIENTED_EDGE('',*,*,#44516,.T.);
#59898=ORIENTED_EDGE('',*,*,#44517,.T.);
#59899=ORIENTED_EDGE('',*,*,#44499,.F.);
#59900=ORIENTED_EDGE('',*,*,#44518,.F.);
#59901=ORIENTED_EDGE('',*,*,#44519,.F.);
#59902=ORIENTED_EDGE('',*,*,#44515,.F.);
#59903=ORIENTED_EDGE('',*,*,#44502,.F.);
#59904=ORIENTED_EDGE('',*,*,#44520,.T.);
#59905=ORIENTED_EDGE('',*,*,#44521,.T.);
#59906=ORIENTED_EDGE('',*,*,#44518,.T.);
#59907=ORIENTED_EDGE('',*,*,#44505,.F.);
#59908=ORIENTED_EDGE('',*,*,#44522,.F.);
#59909=ORIENTED_EDGE('',*,*,#44523,.F.);
#59910=ORIENTED_EDGE('',*,*,#44520,.F.);
#59911=ORIENTED_EDGE('',*,*,#44508,.F.);
#59912=ORIENTED_EDGE('',*,*,#44524,.T.);
#59913=ORIENTED_EDGE('',*,*,#44525,.T.);
#59914=ORIENTED_EDGE('',*,*,#44522,.T.);
#59915=ORIENTED_EDGE('',*,*,#44511,.F.);
#59916=ORIENTED_EDGE('',*,*,#44526,.F.);
#59917=ORIENTED_EDGE('',*,*,#44527,.T.);
#59918=ORIENTED_EDGE('',*,*,#44524,.F.);
#59919=ORIENTED_EDGE('',*,*,#44513,.F.);
#59920=ORIENTED_EDGE('',*,*,#44528,.T.);
#59921=ORIENTED_EDGE('',*,*,#44529,.T.);
#59922=ORIENTED_EDGE('',*,*,#44526,.T.);
#59923=ORIENTED_EDGE('',*,*,#44470,.F.);
#59924=ORIENTED_EDGE('',*,*,#44530,.F.);
#59925=ORIENTED_EDGE('',*,*,#44531,.F.);
#59926=ORIENTED_EDGE('',*,*,#44532,.F.);
#59927=ORIENTED_EDGE('',*,*,#44533,.T.);
#59928=ORIENTED_EDGE('',*,*,#44528,.F.);
#59929=ORIENTED_EDGE('',*,*,#44468,.F.);
#59930=ORIENTED_EDGE('',*,*,#44514,.F.);
#59931=ORIENTED_EDGE('',*,*,#44512,.F.);
#59932=ORIENTED_EDGE('',*,*,#44509,.F.);
#59933=ORIENTED_EDGE('',*,*,#44506,.F.);
#59934=ORIENTED_EDGE('',*,*,#44503,.F.);
#59935=ORIENTED_EDGE('',*,*,#44500,.F.);
#59936=ORIENTED_EDGE('',*,*,#44497,.F.);
#59937=ORIENTED_EDGE('',*,*,#44494,.F.);
#59938=ORIENTED_EDGE('',*,*,#44491,.F.);
#59939=ORIENTED_EDGE('',*,*,#44488,.F.);
#59940=ORIENTED_EDGE('',*,*,#44485,.F.);
#59941=ORIENTED_EDGE('',*,*,#44482,.F.);
#59942=ORIENTED_EDGE('',*,*,#44479,.F.);
#59943=ORIENTED_EDGE('',*,*,#44476,.F.);
#59944=ORIENTED_EDGE('',*,*,#44473,.F.);
#59945=ORIENTED_EDGE('',*,*,#44534,.T.);
#59946=ORIENTED_EDGE('',*,*,#44535,.T.);
#59947=ORIENTED_EDGE('',*,*,#44536,.T.);
#59948=ORIENTED_EDGE('',*,*,#44537,.T.);
#59949=ORIENTED_EDGE('',*,*,#44538,.T.);
#59950=ORIENTED_EDGE('',*,*,#44539,.T.);
#59951=ORIENTED_EDGE('',*,*,#44536,.F.);
#59952=ORIENTED_EDGE('',*,*,#44540,.T.);
#59953=ORIENTED_EDGE('',*,*,#44541,.T.);
#59954=ORIENTED_EDGE('',*,*,#44542,.T.);
#59955=ORIENTED_EDGE('',*,*,#44538,.F.);
#59956=ORIENTED_EDGE('',*,*,#44543,.T.);
#59957=ORIENTED_EDGE('',*,*,#44544,.T.);
#59958=ORIENTED_EDGE('',*,*,#44545,.T.);
#59959=ORIENTED_EDGE('',*,*,#44541,.F.);
#59960=ORIENTED_EDGE('',*,*,#44546,.T.);
#59961=ORIENTED_EDGE('',*,*,#44547,.T.);
#59962=ORIENTED_EDGE('',*,*,#44548,.T.);
#59963=ORIENTED_EDGE('',*,*,#44544,.F.);
#59964=ORIENTED_EDGE('',*,*,#44549,.T.);
#59965=ORIENTED_EDGE('',*,*,#44550,.T.);
#59966=ORIENTED_EDGE('',*,*,#44551,.T.);
#59967=ORIENTED_EDGE('',*,*,#44547,.F.);
#59968=ORIENTED_EDGE('',*,*,#44552,.T.);
#59969=ORIENTED_EDGE('',*,*,#44553,.T.);
#59970=ORIENTED_EDGE('',*,*,#44554,.T.);
#59971=ORIENTED_EDGE('',*,*,#44550,.F.);
#59972=ORIENTED_EDGE('',*,*,#44555,.T.);
#59973=ORIENTED_EDGE('',*,*,#44556,.T.);
#59974=ORIENTED_EDGE('',*,*,#44557,.T.);
#59975=ORIENTED_EDGE('',*,*,#44553,.F.);
#59976=ORIENTED_EDGE('',*,*,#44558,.T.);
#59977=ORIENTED_EDGE('',*,*,#44534,.F.);
#59978=ORIENTED_EDGE('',*,*,#44559,.T.);
#59979=ORIENTED_EDGE('',*,*,#44556,.F.);
#59980=ORIENTED_EDGE('',*,*,#44560,.T.);
#59981=ORIENTED_EDGE('',*,*,#44551,.F.);
#59982=ORIENTED_EDGE('',*,*,#44561,.F.);
#59983=ORIENTED_EDGE('',*,*,#44562,.F.);
#59984=ORIENTED_EDGE('',*,*,#44563,.F.);
#59985=ORIENTED_EDGE('',*,*,#44564,.F.);
#59986=ORIENTED_EDGE('',*,*,#44565,.F.);
#59987=ORIENTED_EDGE('',*,*,#44566,.F.);
#59988=ORIENTED_EDGE('',*,*,#44567,.F.);
#59989=ORIENTED_EDGE('',*,*,#44554,.F.);
#59990=ORIENTED_EDGE('',*,*,#44568,.T.);
#59991=ORIENTED_EDGE('',*,*,#44569,.T.);
#59992=ORIENTED_EDGE('',*,*,#44561,.T.);
#59993=ORIENTED_EDGE('',*,*,#44557,.F.);
#59994=ORIENTED_EDGE('',*,*,#44570,.F.);
#59995=ORIENTED_EDGE('',*,*,#44571,.F.);
#59996=ORIENTED_EDGE('',*,*,#44568,.F.);
#59997=ORIENTED_EDGE('',*,*,#44559,.F.);
#59998=ORIENTED_EDGE('',*,*,#44572,.T.);
#59999=ORIENTED_EDGE('',*,*,#44573,.T.);
#60000=ORIENTED_EDGE('',*,*,#44570,.T.);
#60001=ORIENTED_EDGE('',*,*,#44537,.F.);
#60002=ORIENTED_EDGE('',*,*,#44574,.F.);
#60003=ORIENTED_EDGE('',*,*,#44575,.F.);
#60004=ORIENTED_EDGE('',*,*,#44572,.F.);
#60005=ORIENTED_EDGE('',*,*,#44535,.F.);
#60006=ORIENTED_EDGE('',*,*,#44560,.F.);
#60007=ORIENTED_EDGE('',*,*,#44558,.F.);
#60008=ORIENTED_EDGE('',*,*,#44555,.F.);
#60009=ORIENTED_EDGE('',*,*,#44552,.F.);
#60010=ORIENTED_EDGE('',*,*,#44549,.F.);
#60011=ORIENTED_EDGE('',*,*,#44546,.F.);
#60012=ORIENTED_EDGE('',*,*,#44543,.F.);
#60013=ORIENTED_EDGE('',*,*,#44540,.F.);
#60014=ORIENTED_EDGE('',*,*,#44576,.T.);
#60015=ORIENTED_EDGE('',*,*,#44577,.T.);
#60016=ORIENTED_EDGE('',*,*,#44578,.T.);
#60017=ORIENTED_EDGE('',*,*,#44579,.T.);
#60018=ORIENTED_EDGE('',*,*,#44580,.T.);
#60019=ORIENTED_EDGE('',*,*,#44581,.T.);
#60020=ORIENTED_EDGE('',*,*,#44578,.F.);
#60021=ORIENTED_EDGE('',*,*,#44582,.T.);
#60022=ORIENTED_EDGE('',*,*,#44583,.T.);
#60023=ORIENTED_EDGE('',*,*,#44584,.T.);
#60024=ORIENTED_EDGE('',*,*,#44580,.F.);
#60025=ORIENTED_EDGE('',*,*,#44585,.T.);
#60026=ORIENTED_EDGE('',*,*,#44586,.T.);
#60027=ORIENTED_EDGE('',*,*,#44587,.T.);
#60028=ORIENTED_EDGE('',*,*,#44583,.F.);
#60029=ORIENTED_EDGE('',*,*,#44588,.T.);
#60030=ORIENTED_EDGE('',*,*,#44589,.T.);
#60031=ORIENTED_EDGE('',*,*,#44590,.T.);
#60032=ORIENTED_EDGE('',*,*,#44586,.F.);
#60033=ORIENTED_EDGE('',*,*,#44591,.T.);
#60034=ORIENTED_EDGE('',*,*,#44592,.T.);
#60035=ORIENTED_EDGE('',*,*,#44593,.T.);
#60036=ORIENTED_EDGE('',*,*,#44589,.F.);
#60037=ORIENTED_EDGE('',*,*,#44594,.T.);
#60038=ORIENTED_EDGE('',*,*,#44595,.T.);
#60039=ORIENTED_EDGE('',*,*,#44596,.T.);
#60040=ORIENTED_EDGE('',*,*,#44592,.F.);
#60041=ORIENTED_EDGE('',*,*,#44597,.T.);
#60042=ORIENTED_EDGE('',*,*,#44576,.F.);
#60043=ORIENTED_EDGE('',*,*,#44598,.T.);
#60044=ORIENTED_EDGE('',*,*,#44595,.F.);
#60045=ORIENTED_EDGE('',*,*,#44599,.T.);
#60046=ORIENTED_EDGE('',*,*,#44593,.F.);
#60047=ORIENTED_EDGE('',*,*,#44600,.T.);
#60048=ORIENTED_EDGE('',*,*,#44601,.T.);
#60049=ORIENTED_EDGE('',*,*,#44602,.T.);
#60050=ORIENTED_EDGE('',*,*,#44596,.F.);
#60051=ORIENTED_EDGE('',*,*,#44603,.F.);
#60052=ORIENTED_EDGE('',*,*,#44604,.F.);
#60053=ORIENTED_EDGE('',*,*,#44600,.F.);
#60054=ORIENTED_EDGE('',*,*,#44598,.F.);
#60055=ORIENTED_EDGE('',*,*,#44605,.T.);
#60056=ORIENTED_EDGE('',*,*,#44606,.T.);
#60057=ORIENTED_EDGE('',*,*,#44603,.T.);
#60058=ORIENTED_EDGE('',*,*,#44579,.F.);
#60059=ORIENTED_EDGE('',*,*,#44607,.F.);
#60060=ORIENTED_EDGE('',*,*,#44608,.F.);
#60061=ORIENTED_EDGE('',*,*,#44605,.F.);
#60062=ORIENTED_EDGE('',*,*,#44577,.F.);
#60063=ORIENTED_EDGE('',*,*,#44599,.F.);
#60064=ORIENTED_EDGE('',*,*,#44597,.F.);
#60065=ORIENTED_EDGE('',*,*,#44594,.F.);
#60066=ORIENTED_EDGE('',*,*,#44591,.F.);
#60067=ORIENTED_EDGE('',*,*,#44588,.F.);
#60068=ORIENTED_EDGE('',*,*,#44585,.F.);
#60069=ORIENTED_EDGE('',*,*,#44582,.F.);
#60070=ORIENTED_EDGE('',*,*,#44609,.T.);
#60071=ORIENTED_EDGE('',*,*,#44610,.T.);
#60072=ORIENTED_EDGE('',*,*,#44611,.T.);
#60073=ORIENTED_EDGE('',*,*,#44612,.T.);
#60074=ORIENTED_EDGE('',*,*,#44613,.T.);
#60075=ORIENTED_EDGE('',*,*,#44614,.T.);
#60076=ORIENTED_EDGE('',*,*,#44611,.F.);
#60077=ORIENTED_EDGE('',*,*,#44615,.T.);
#60078=ORIENTED_EDGE('',*,*,#44616,.T.);
#60079=ORIENTED_EDGE('',*,*,#44617,.T.);
#60080=ORIENTED_EDGE('',*,*,#44613,.F.);
#60081=ORIENTED_EDGE('',*,*,#44195,.T.);
#60082=ORIENTED_EDGE('',*,*,#44615,.F.);
#60083=ORIENTED_EDGE('',*,*,#44618,.T.);
#60084=ORIENTED_EDGE('',*,*,#44619,.T.);
#60085=ORIENTED_EDGE('',*,*,#44196,.T.);
#60086=ORIENTED_EDGE('',*,*,#44610,.F.);
#60087=ORIENTED_EDGE('',*,*,#44620,.F.);
#60088=ORIENTED_EDGE('',*,*,#44621,.T.);
#60089=ORIENTED_EDGE('',*,*,#44622,.F.);
#60090=ORIENTED_EDGE('',*,*,#44623,.T.);
#60091=ORIENTED_EDGE('',*,*,#44624,.T.);
#60092=ORIENTED_EDGE('',*,*,#44625,.F.);
#60093=ORIENTED_EDGE('',*,*,#44626,.F.);
#60094=ORIENTED_EDGE('',*,*,#44627,.F.);
#60095=ORIENTED_EDGE('',*,*,#44628,.F.);
#60096=ORIENTED_EDGE('',*,*,#44629,.F.);
#60097=ORIENTED_EDGE('',*,*,#44630,.F.);
#60098=ORIENTED_EDGE('',*,*,#44631,.F.);
#60099=ORIENTED_EDGE('',*,*,#44632,.T.);
#60100=ORIENTED_EDGE('',*,*,#44633,.T.);
#60101=ORIENTED_EDGE('',*,*,#44632,.F.);
#60102=ORIENTED_EDGE('',*,*,#44634,.F.);
#60103=ORIENTED_EDGE('',*,*,#44618,.F.);
#60104=ORIENTED_EDGE('',*,*,#44617,.F.);
#60105=ORIENTED_EDGE('',*,*,#44635,.T.);
#60106=ORIENTED_EDGE('',*,*,#44268,.T.);
#60107=ORIENTED_EDGE('',*,*,#44636,.F.);
#60108=ORIENTED_EDGE('',*,*,#44612,.F.);
#60109=ORIENTED_EDGE('',*,*,#44614,.F.);
#60110=ORIENTED_EDGE('',*,*,#44637,.T.);
#60111=ORIENTED_EDGE('',*,*,#44192,.T.);
#60112=ORIENTED_EDGE('',*,*,#44638,.T.);
#60113=ORIENTED_EDGE('',*,*,#44639,.T.);
#60114=ORIENTED_EDGE('',*,*,#44637,.F.);
#60115=ORIENTED_EDGE('',*,*,#44640,.T.);
#60116=ORIENTED_EDGE('',*,*,#44641,.F.);
#60117=ORIENTED_EDGE('',*,*,#44642,.F.);
#60118=ORIENTED_EDGE('',*,*,#44643,.F.);
#60119=ORIENTED_EDGE('',*,*,#44644,.F.);
#60120=ORIENTED_EDGE('',*,*,#44645,.F.);
#60121=ORIENTED_EDGE('',*,*,#44251,.F.);
#60122=ORIENTED_EDGE('',*,*,#44254,.T.);
#60123=ORIENTED_EDGE('',*,*,#44256,.F.);
#60124=ORIENTED_EDGE('',*,*,#44258,.F.);
#60125=ORIENTED_EDGE('',*,*,#44270,.F.);
#60126=ORIENTED_EDGE('',*,*,#44646,.F.);
#60127=ORIENTED_EDGE('',*,*,#44193,.F.);
#60128=ORIENTED_EDGE('',*,*,#44639,.F.);
#60129=ORIENTED_EDGE('',*,*,#44647,.F.);
#60130=ORIENTED_EDGE('',*,*,#44648,.F.);
#60131=ORIENTED_EDGE('',*,*,#44649,.F.);
#60132=ORIENTED_EDGE('',*,*,#44650,.F.);
#60133=ORIENTED_EDGE('',*,*,#44640,.F.);
#60134=ORIENTED_EDGE('',*,*,#44651,.T.);
#60135=ORIENTED_EDGE('',*,*,#44652,.T.);
#60136=ORIENTED_EDGE('',*,*,#44653,.T.);
#60137=ORIENTED_EDGE('',*,*,#44654,.T.);
#60138=ORIENTED_EDGE('',*,*,#44651,.F.);
#60139=ORIENTED_EDGE('',*,*,#44655,.T.);
#60140=ORIENTED_EDGE('',*,*,#44656,.T.);
#60141=ORIENTED_EDGE('',*,*,#44657,.T.);
#60142=ORIENTED_EDGE('',*,*,#44658,.T.);
#60143=ORIENTED_EDGE('',*,*,#44356,.T.);
#60144=ORIENTED_EDGE('',*,*,#44361,.T.);
#60145=ORIENTED_EDGE('',*,*,#44363,.F.);
#60146=ORIENTED_EDGE('',*,*,#44365,.T.);
#60147=ORIENTED_EDGE('',*,*,#44367,.F.);
#60148=ORIENTED_EDGE('',*,*,#44371,.T.);
#60149=ORIENTED_EDGE('',*,*,#44659,.T.);
#60150=ORIENTED_EDGE('',*,*,#44660,.T.);
#60151=ORIENTED_EDGE('',*,*,#44661,.F.);
#60152=ORIENTED_EDGE('',*,*,#44662,.T.);
#60153=ORIENTED_EDGE('',*,*,#44663,.F.);
#60154=ORIENTED_EDGE('',*,*,#44664,.T.);
#60155=ORIENTED_EDGE('',*,*,#44313,.F.);
#60156=ORIENTED_EDGE('',*,*,#44665,.T.);
#60157=ORIENTED_EDGE('',*,*,#44666,.T.);
#60158=ORIENTED_EDGE('',*,*,#44667,.F.);
#60159=ORIENTED_EDGE('',*,*,#44668,.T.);
#60160=ORIENTED_EDGE('',*,*,#44669,.F.);
#60161=ORIENTED_EDGE('',*,*,#44670,.T.);
#60162=ORIENTED_EDGE('',*,*,#44671,.F.);
#60163=ORIENTED_EDGE('',*,*,#44672,.T.);
#60164=ORIENTED_EDGE('',*,*,#44673,.T.);
#60165=ORIENTED_EDGE('',*,*,#44674,.T.);
#60166=ORIENTED_EDGE('',*,*,#44675,.F.);
#60167=ORIENTED_EDGE('',*,*,#44676,.T.);
#60168=ORIENTED_EDGE('',*,*,#44677,.T.);
#60169=ORIENTED_EDGE('',*,*,#44678,.T.);
#60170=ORIENTED_EDGE('',*,*,#44679,.T.);
#60171=ORIENTED_EDGE('',*,*,#44654,.F.);
#60172=ORIENTED_EDGE('',*,*,#44680,.T.);
#60173=ORIENTED_EDGE('',*,*,#44681,.F.);
#60174=ORIENTED_EDGE('',*,*,#44655,.F.);
#60175=ORIENTED_EDGE('',*,*,#44682,.F.);
#60176=ORIENTED_EDGE('',*,*,#44683,.F.);
#60177=ORIENTED_EDGE('',*,*,#44684,.F.);
#60178=ORIENTED_EDGE('',*,*,#44685,.F.);
#60179=ORIENTED_EDGE('',*,*,#44686,.T.);
#60180=ORIENTED_EDGE('',*,*,#44687,.F.);
#60181=ORIENTED_EDGE('',*,*,#44688,.T.);
#60182=ORIENTED_EDGE('',*,*,#44689,.F.);
#60183=ORIENTED_EDGE('',*,*,#44690,.F.);
#60184=ORIENTED_EDGE('',*,*,#44623,.F.);
#60185=ORIENTED_EDGE('',*,*,#44691,.F.);
#60186=ORIENTED_EDGE('',*,*,#44369,.F.);
#60187=ORIENTED_EDGE('',*,*,#44692,.F.);
#60188=ORIENTED_EDGE('',*,*,#44693,.F.);
#60189=ORIENTED_EDGE('',*,*,#44694,.F.);
#60190=ORIENTED_EDGE('',*,*,#44695,.F.);
#60191=ORIENTED_EDGE('',*,*,#44696,.F.);
#60192=ORIENTED_EDGE('',*,*,#44358,.F.);
#60193=ORIENTED_EDGE('',*,*,#44697,.F.);
#60194=ORIENTED_EDGE('',*,*,#44698,.F.);
#60195=ORIENTED_EDGE('',*,*,#44699,.F.);
#60196=ORIENTED_EDGE('',*,*,#44680,.F.);
#60197=ORIENTED_EDGE('',*,*,#44653,.F.);
#60198=ORIENTED_EDGE('',*,*,#44700,.F.);
#60199=ORIENTED_EDGE('',*,*,#44701,.T.);
#60200=ORIENTED_EDGE('',*,*,#44415,.F.);
#60201=ORIENTED_EDGE('',*,*,#44418,.T.);
#60202=ORIENTED_EDGE('',*,*,#44420,.F.);
#60203=ORIENTED_EDGE('',*,*,#44422,.T.);
#60204=ORIENTED_EDGE('',*,*,#44424,.F.);
#60205=ORIENTED_EDGE('',*,*,#44426,.F.);
#60206=ORIENTED_EDGE('',*,*,#44428,.F.);
#60207=ORIENTED_EDGE('',*,*,#44702,.F.);
#60208=ORIENTED_EDGE('',*,*,#44703,.T.);
#60209=ORIENTED_EDGE('',*,*,#44704,.T.);
#60210=ORIENTED_EDGE('',*,*,#44705,.F.);
#60211=ORIENTED_EDGE('',*,*,#44706,.T.);
#60212=ORIENTED_EDGE('',*,*,#44707,.F.);
#60213=ORIENTED_EDGE('',*,*,#44652,.F.);
#60214=ORIENTED_EDGE('',*,*,#44678,.F.);
#60215=ORIENTED_EDGE('',*,*,#44708,.F.);
#60216=ORIENTED_EDGE('',*,*,#44709,.T.);
#60217=ORIENTED_EDGE('',*,*,#44710,.F.);
#60218=ORIENTED_EDGE('',*,*,#44682,.T.);
#60219=ORIENTED_EDGE('',*,*,#44685,.T.);
#60220=ORIENTED_EDGE('',*,*,#44711,.T.);
#60221=ORIENTED_EDGE('',*,*,#44712,.T.);
#60222=ORIENTED_EDGE('',*,*,#44713,.T.);
#60223=ORIENTED_EDGE('',*,*,#44713,.F.);
#60224=ORIENTED_EDGE('',*,*,#44714,.F.);
#60225=ORIENTED_EDGE('',*,*,#44715,.F.);
#60226=ORIENTED_EDGE('',*,*,#44686,.F.);
#60227=ORIENTED_EDGE('',*,*,#44712,.F.);
#60228=ORIENTED_EDGE('',*,*,#44716,.F.);
#60229=ORIENTED_EDGE('',*,*,#44717,.F.);
#60230=ORIENTED_EDGE('',*,*,#44709,.F.);
#60231=ORIENTED_EDGE('',*,*,#44718,.F.);
#60232=ORIENTED_EDGE('',*,*,#44719,.T.);
#60233=ORIENTED_EDGE('',*,*,#44720,.F.);
#60234=ORIENTED_EDGE('',*,*,#44721,.T.);
#60235=ORIENTED_EDGE('',*,*,#44722,.F.);
#60236=ORIENTED_EDGE('',*,*,#44649,.T.);
#60237=ORIENTED_EDGE('',*,*,#44723,.F.);
#60238=ORIENTED_EDGE('',*,*,#44724,.T.);
#60239=ORIENTED_EDGE('',*,*,#44725,.F.);
#60240=ORIENTED_EDGE('',*,*,#44726,.F.);
#60241=ORIENTED_EDGE('',*,*,#44727,.F.);
#60242=ORIENTED_EDGE('',*,*,#44728,.T.);
#60243=ORIENTED_EDGE('',*,*,#44729,.T.);
#60244=ORIENTED_EDGE('',*,*,#44730,.T.);
#60245=ORIENTED_EDGE('',*,*,#44731,.F.);
#60246=ORIENTED_EDGE('',*,*,#44732,.F.);
#60247=ORIENTED_EDGE('',*,*,#44733,.F.);
#60248=ORIENTED_EDGE('',*,*,#44734,.T.);
#60249=ORIENTED_EDGE('',*,*,#44735,.F.);
#60250=ORIENTED_EDGE('',*,*,#44736,.T.);
#60251=ORIENTED_EDGE('',*,*,#44737,.F.);
#60252=ORIENTED_EDGE('',*,*,#44714,.T.);
#60253=ORIENTED_EDGE('',*,*,#44633,.F.);
#60254=ORIENTED_EDGE('',*,*,#44738,.T.);
#60255=ORIENTED_EDGE('',*,*,#44739,.T.);
#60256=ORIENTED_EDGE('',*,*,#44740,.T.);
#60257=ORIENTED_EDGE('',*,*,#44741,.T.);
#60258=ORIENTED_EDGE('',*,*,#44742,.F.);
#60259=ORIENTED_EDGE('',*,*,#44743,.F.);
#60260=ORIENTED_EDGE('',*,*,#44744,.F.);
#60261=ORIENTED_EDGE('',*,*,#44737,.T.);
#60262=ORIENTED_EDGE('',*,*,#44745,.T.);
#60263=ORIENTED_EDGE('',*,*,#44687,.T.);
#60264=ORIENTED_EDGE('',*,*,#44715,.T.);
#60265=ORIENTED_EDGE('',*,*,#44745,.F.);
#60266=ORIENTED_EDGE('',*,*,#44736,.F.);
#60267=ORIENTED_EDGE('',*,*,#44746,.F.);
#60268=ORIENTED_EDGE('',*,*,#44747,.F.);
#60269=ORIENTED_EDGE('',*,*,#44748,.F.);
#60270=ORIENTED_EDGE('',*,*,#44688,.F.);
#60271=ORIENTED_EDGE('',*,*,#44749,.T.);
#60272=ORIENTED_EDGE('',*,*,#44746,.T.);
#60273=ORIENTED_EDGE('',*,*,#44735,.T.);
#60274=ORIENTED_EDGE('',*,*,#44750,.T.);
#60275=ORIENTED_EDGE('',*,*,#44733,.T.);
#60276=ORIENTED_EDGE('',*,*,#44751,.T.);
#60277=ORIENTED_EDGE('',*,*,#44752,.T.);
#60278=ORIENTED_EDGE('',*,*,#44753,.T.);
#60279=ORIENTED_EDGE('',*,*,#44750,.F.);
#60280=ORIENTED_EDGE('',*,*,#44734,.F.);
#60281=ORIENTED_EDGE('',*,*,#44753,.F.);
#60282=ORIENTED_EDGE('',*,*,#44754,.F.);
#60283=ORIENTED_EDGE('',*,*,#44755,.F.);
#60284=ORIENTED_EDGE('',*,*,#44756,.F.);
#60285=ORIENTED_EDGE('',*,*,#44752,.F.);
#60286=ORIENTED_EDGE('',*,*,#44757,.F.);
#60287=ORIENTED_EDGE('',*,*,#44758,.F.);
#60288=ORIENTED_EDGE('',*,*,#44759,.T.);
#60289=ORIENTED_EDGE('',*,*,#44760,.F.);
#60290=ORIENTED_EDGE('',*,*,#44761,.T.);
#60291=ORIENTED_EDGE('',*,*,#44762,.T.);
#60292=ORIENTED_EDGE('',*,*,#44763,.F.);
#60293=ORIENTED_EDGE('',*,*,#44764,.T.);
#60294=ORIENTED_EDGE('',*,*,#44765,.T.);
#60295=ORIENTED_EDGE('',*,*,#44766,.F.);
#60296=ORIENTED_EDGE('',*,*,#44767,.T.);
#60297=ORIENTED_EDGE('',*,*,#44516,.F.);
#60298=ORIENTED_EDGE('',*,*,#44519,.T.);
#60299=ORIENTED_EDGE('',*,*,#44521,.F.);
#60300=ORIENTED_EDGE('',*,*,#44523,.T.);
#60301=ORIENTED_EDGE('',*,*,#44525,.F.);
#60302=ORIENTED_EDGE('',*,*,#44527,.F.);
#60303=ORIENTED_EDGE('',*,*,#44529,.F.);
#60304=ORIENTED_EDGE('',*,*,#44533,.F.);
#60305=ORIENTED_EDGE('',*,*,#44768,.T.);
#60306=ORIENTED_EDGE('',*,*,#44769,.F.);
#60307=ORIENTED_EDGE('',*,*,#44627,.T.);
#60308=ORIENTED_EDGE('',*,*,#44770,.F.);
#60309=ORIENTED_EDGE('',*,*,#44754,.T.);
#60310=ORIENTED_EDGE('',*,*,#44725,.T.);
#60311=ORIENTED_EDGE('',*,*,#44771,.T.);
#60312=ORIENTED_EDGE('',*,*,#44772,.T.);
#60313=ORIENTED_EDGE('',*,*,#44773,.T.);
#60314=ORIENTED_EDGE('',*,*,#44771,.F.);
#60315=ORIENTED_EDGE('',*,*,#44724,.F.);
#60316=ORIENTED_EDGE('',*,*,#44774,.F.);
#60317=ORIENTED_EDGE('',*,*,#44775,.F.);
#60318=ORIENTED_EDGE('',*,*,#44723,.T.);
#60319=ORIENTED_EDGE('',*,*,#44648,.T.);
#60320=ORIENTED_EDGE('',*,*,#44776,.T.);
#60321=ORIENTED_EDGE('',*,*,#44774,.T.);
#60322=ORIENTED_EDGE('',*,*,#44772,.F.);
#60323=ORIENTED_EDGE('',*,*,#44775,.T.);
#60324=ORIENTED_EDGE('',*,*,#44776,.F.);
#60325=ORIENTED_EDGE('',*,*,#44647,.T.);
#60326=ORIENTED_EDGE('',*,*,#44638,.F.);
#60327=ORIENTED_EDGE('',*,*,#44191,.F.);
#60328=ORIENTED_EDGE('',*,*,#44200,.F.);
#60329=ORIENTED_EDGE('',*,*,#44202,.T.);
#60330=ORIENTED_EDGE('',*,*,#44204,.F.);
#60331=ORIENTED_EDGE('',*,*,#44206,.T.);
#60332=ORIENTED_EDGE('',*,*,#44777,.F.);
#60333=ORIENTED_EDGE('',*,*,#44778,.T.);
#60334=ORIENTED_EDGE('',*,*,#44779,.F.);
#60335=ORIENTED_EDGE('',*,*,#44780,.T.);
#60336=ORIENTED_EDGE('',*,*,#44781,.F.);
#60337=ORIENTED_EDGE('',*,*,#44197,.T.);
#60338=ORIENTED_EDGE('',*,*,#44619,.F.);
#60339=ORIENTED_EDGE('',*,*,#44634,.T.);
#60340=ORIENTED_EDGE('',*,*,#44631,.T.);
#60341=ORIENTED_EDGE('',*,*,#44782,.F.);
#60342=ORIENTED_EDGE('',*,*,#44562,.T.);
#60343=ORIENTED_EDGE('',*,*,#44569,.F.);
#60344=ORIENTED_EDGE('',*,*,#44571,.T.);
#60345=ORIENTED_EDGE('',*,*,#44573,.F.);
#60346=ORIENTED_EDGE('',*,*,#44575,.T.);
#60347=ORIENTED_EDGE('',*,*,#44783,.T.);
#60348=ORIENTED_EDGE('',*,*,#44784,.T.);
#60349=ORIENTED_EDGE('',*,*,#44785,.T.);
#60350=ORIENTED_EDGE('',*,*,#44786,.F.);
#60351=ORIENTED_EDGE('',*,*,#44566,.T.);
#60352=ORIENTED_EDGE('',*,*,#44787,.F.);
#60353=ORIENTED_EDGE('',*,*,#44788,.T.);
#60354=ORIENTED_EDGE('',*,*,#44789,.T.);
#60355=ORIENTED_EDGE('',*,*,#44641,.T.);
#60356=ORIENTED_EDGE('',*,*,#44650,.T.);
#60357=ORIENTED_EDGE('',*,*,#44722,.T.);
#60358=ORIENTED_EDGE('',*,*,#44790,.T.);
#60359=ORIENTED_EDGE('',*,*,#44720,.T.);
#60360=ORIENTED_EDGE('',*,*,#44791,.T.);
#60361=ORIENTED_EDGE('',*,*,#44675,.T.);
#60362=ORIENTED_EDGE('',*,*,#44792,.T.);
#60363=ORIENTED_EDGE('',*,*,#44790,.F.);
#60364=ORIENTED_EDGE('',*,*,#44721,.F.);
#60365=ORIENTED_EDGE('',*,*,#44792,.F.);
#60366=ORIENTED_EDGE('',*,*,#44674,.F.);
#60367=ORIENTED_EDGE('',*,*,#44793,.T.);
#60368=ORIENTED_EDGE('',*,*,#44642,.T.);
#60369=ORIENTED_EDGE('',*,*,#44673,.F.);
#60370=ORIENTED_EDGE('',*,*,#44794,.F.);
#60371=ORIENTED_EDGE('',*,*,#44643,.T.);
#60372=ORIENTED_EDGE('',*,*,#44793,.F.);
#60373=ORIENTED_EDGE('',*,*,#44380,.F.);
#60374=ORIENTED_EDGE('',*,*,#44795,.F.);
#60375=ORIENTED_EDGE('',*,*,#44703,.F.);
#60376=ORIENTED_EDGE('',*,*,#44796,.F.);
#60377=ORIENTED_EDGE('',*,*,#44383,.F.);
#60378=ORIENTED_EDGE('',*,*,#44797,.F.);
#60379=ORIENTED_EDGE('',*,*,#44704,.F.);
#60380=ORIENTED_EDGE('',*,*,#44795,.T.);
#60381=ORIENTED_EDGE('',*,*,#44386,.F.);
#60382=ORIENTED_EDGE('',*,*,#44798,.T.);
#60383=ORIENTED_EDGE('',*,*,#44705,.T.);
#60384=ORIENTED_EDGE('',*,*,#44797,.T.);
#60385=ORIENTED_EDGE('',*,*,#44389,.F.);
#60386=ORIENTED_EDGE('',*,*,#44799,.F.);
#60387=ORIENTED_EDGE('',*,*,#44706,.F.);
#60388=ORIENTED_EDGE('',*,*,#44798,.F.);
#60389=ORIENTED_EDGE('',*,*,#44392,.F.);
#60390=ORIENTED_EDGE('',*,*,#44800,.T.);
#60391=ORIENTED_EDGE('',*,*,#44700,.T.);
#60392=ORIENTED_EDGE('',*,*,#44799,.T.);
#60393=ORIENTED_EDGE('',*,*,#44395,.F.);
#60394=ORIENTED_EDGE('',*,*,#44416,.F.);
#60395=ORIENTED_EDGE('',*,*,#44701,.F.);
#60396=ORIENTED_EDGE('',*,*,#44800,.F.);
#60397=ORIENTED_EDGE('',*,*,#44437,.F.);
#60398=ORIENTED_EDGE('',*,*,#44801,.T.);
#60399=ORIENTED_EDGE('',*,*,#44802,.T.);
#60400=ORIENTED_EDGE('',*,*,#44803,.T.);
#60401=ORIENTED_EDGE('',*,*,#44440,.F.);
#60402=ORIENTED_EDGE('',*,*,#44804,.F.);
#60403=ORIENTED_EDGE('',*,*,#44805,.F.);
#60404=ORIENTED_EDGE('',*,*,#44801,.F.);
#60405=ORIENTED_EDGE('',*,*,#44443,.F.);
#60406=ORIENTED_EDGE('',*,*,#44458,.T.);
#60407=ORIENTED_EDGE('',*,*,#44806,.T.);
#60408=ORIENTED_EDGE('',*,*,#44804,.T.);
#60409=ORIENTED_EDGE('',*,*,#44475,.F.);
#60410=ORIENTED_EDGE('',*,*,#44807,.F.);
#60411=ORIENTED_EDGE('',*,*,#44808,.F.);
#60412=ORIENTED_EDGE('',*,*,#44809,.F.);
#60413=ORIENTED_EDGE('',*,*,#44478,.F.);
#60414=ORIENTED_EDGE('',*,*,#44810,.F.);
#60415=ORIENTED_EDGE('',*,*,#44811,.F.);
#60416=ORIENTED_EDGE('',*,*,#44807,.T.);
#60417=ORIENTED_EDGE('',*,*,#44481,.F.);
#60418=ORIENTED_EDGE('',*,*,#44812,.F.);
#60419=ORIENTED_EDGE('',*,*,#44763,.T.);
#60420=ORIENTED_EDGE('',*,*,#44813,.T.);
#60421=ORIENTED_EDGE('',*,*,#44814,.T.);
#60422=ORIENTED_EDGE('',*,*,#44810,.T.);
#60423=ORIENTED_EDGE('',*,*,#44484,.F.);
#60424=ORIENTED_EDGE('',*,*,#44815,.T.);
#60425=ORIENTED_EDGE('',*,*,#44764,.F.);
#60426=ORIENTED_EDGE('',*,*,#44812,.T.);
#60427=ORIENTED_EDGE('',*,*,#44487,.F.);
#60428=ORIENTED_EDGE('',*,*,#44816,.F.);
#60429=ORIENTED_EDGE('',*,*,#44765,.F.);
#60430=ORIENTED_EDGE('',*,*,#44815,.F.);
#60431=ORIENTED_EDGE('',*,*,#44490,.F.);
#60432=ORIENTED_EDGE('',*,*,#44817,.T.);
#60433=ORIENTED_EDGE('',*,*,#44766,.T.);
#60434=ORIENTED_EDGE('',*,*,#44816,.T.);
#60435=ORIENTED_EDGE('',*,*,#44493,.F.);
#60436=ORIENTED_EDGE('',*,*,#44517,.F.);
#60437=ORIENTED_EDGE('',*,*,#44767,.F.);
#60438=ORIENTED_EDGE('',*,*,#44817,.F.);
#60439=ORIENTED_EDGE('',*,*,#44756,.T.);
#60440=ORIENTED_EDGE('',*,*,#44818,.T.);
#60441=ORIENTED_EDGE('',*,*,#44460,.F.);
#60442=ORIENTED_EDGE('',*,*,#44462,.T.);
#60443=ORIENTED_EDGE('',*,*,#44464,.T.);
#60444=ORIENTED_EDGE('',*,*,#44819,.F.);
#60445=ORIENTED_EDGE('',*,*,#44747,.T.);
#60446=ORIENTED_EDGE('',*,*,#44749,.F.);
#60447=ORIENTED_EDGE('',*,*,#44215,.F.);
#60448=ORIENTED_EDGE('',*,*,#44820,.F.);
#60449=ORIENTED_EDGE('',*,*,#44668,.F.);
#60450=ORIENTED_EDGE('',*,*,#44821,.F.);
#60451=ORIENTED_EDGE('',*,*,#44218,.F.);
#60452=ORIENTED_EDGE('',*,*,#44822,.T.);
#60453=ORIENTED_EDGE('',*,*,#44669,.T.);
#60454=ORIENTED_EDGE('',*,*,#44820,.T.);
#60455=ORIENTED_EDGE('',*,*,#44221,.F.);
#60456=ORIENTED_EDGE('',*,*,#44823,.F.);
#60457=ORIENTED_EDGE('',*,*,#44670,.F.);
#60458=ORIENTED_EDGE('',*,*,#44822,.F.);
#60459=ORIENTED_EDGE('',*,*,#44224,.F.);
#60460=ORIENTED_EDGE('',*,*,#44824,.T.);
#60461=ORIENTED_EDGE('',*,*,#44671,.T.);
#60462=ORIENTED_EDGE('',*,*,#44823,.T.);
#60463=ORIENTED_EDGE('',*,*,#44227,.F.);
#60464=ORIENTED_EDGE('',*,*,#44825,.F.);
#60465=ORIENTED_EDGE('',*,*,#44644,.T.);
#60466=ORIENTED_EDGE('',*,*,#44794,.T.);
#60467=ORIENTED_EDGE('',*,*,#44672,.F.);
#60468=ORIENTED_EDGE('',*,*,#44824,.F.);
#60469=ORIENTED_EDGE('',*,*,#44230,.F.);
#60470=ORIENTED_EDGE('',*,*,#44252,.T.);
#60471=ORIENTED_EDGE('',*,*,#44645,.T.);
#60472=ORIENTED_EDGE('',*,*,#44825,.T.);
#60473=ORIENTED_EDGE('',*,*,#44171,.F.);
#60474=ORIENTED_EDGE('',*,*,#44826,.T.);
#60475=ORIENTED_EDGE('',*,*,#44779,.T.);
#60476=ORIENTED_EDGE('',*,*,#44827,.T.);
#60477=ORIENTED_EDGE('',*,*,#44174,.F.);
#60478=ORIENTED_EDGE('',*,*,#44828,.F.);
#60479=ORIENTED_EDGE('',*,*,#44780,.F.);
#60480=ORIENTED_EDGE('',*,*,#44826,.F.);
#60481=ORIENTED_EDGE('',*,*,#44177,.F.);
#60482=ORIENTED_EDGE('',*,*,#44198,.T.);
#60483=ORIENTED_EDGE('',*,*,#44781,.T.);
#60484=ORIENTED_EDGE('',*,*,#44828,.T.);
#60485=ORIENTED_EDGE('',*,*,#44165,.F.);
#60486=ORIENTED_EDGE('',*,*,#44829,.T.);
#60487=ORIENTED_EDGE('',*,*,#44777,.T.);
#60488=ORIENTED_EDGE('',*,*,#44205,.T.);
#60489=ORIENTED_EDGE('',*,*,#44168,.F.);
#60490=ORIENTED_EDGE('',*,*,#44827,.F.);
#60491=ORIENTED_EDGE('',*,*,#44778,.F.);
#60492=ORIENTED_EDGE('',*,*,#44829,.F.);
#60493=ORIENTED_EDGE('',*,*,#44791,.F.);
#60494=ORIENTED_EDGE('',*,*,#44719,.F.);
#60495=ORIENTED_EDGE('',*,*,#44830,.T.);
#60496=ORIENTED_EDGE('',*,*,#44676,.F.);
#60497=ORIENTED_EDGE('',*,*,#44755,.T.);
#60498=ORIENTED_EDGE('',*,*,#44770,.T.);
#60499=ORIENTED_EDGE('',*,*,#44626,.T.);
#60500=ORIENTED_EDGE('',*,*,#44831,.T.);
#60501=ORIENTED_EDGE('',*,*,#44457,.F.);
#60502=ORIENTED_EDGE('',*,*,#44818,.F.);
#60503=ORIENTED_EDGE('',*,*,#44711,.F.);
#60504=ORIENTED_EDGE('',*,*,#44684,.T.);
#60505=ORIENTED_EDGE('',*,*,#44832,.F.);
#60506=ORIENTED_EDGE('',*,*,#44716,.T.);
#60507=ORIENTED_EDGE('',*,*,#44751,.F.);
#60508=ORIENTED_EDGE('',*,*,#44732,.T.);
#60509=ORIENTED_EDGE('',*,*,#44833,.F.);
#60510=ORIENTED_EDGE('',*,*,#44834,.T.);
#60511=ORIENTED_EDGE('',*,*,#44835,.F.);
#60512=ORIENTED_EDGE('',*,*,#44757,.T.);
#60513=ORIENTED_EDGE('',*,*,#44677,.F.);
#60514=ORIENTED_EDGE('',*,*,#44830,.F.);
#60515=ORIENTED_EDGE('',*,*,#44718,.T.);
#60516=ORIENTED_EDGE('',*,*,#44708,.T.);
#60517=ORIENTED_EDGE('',*,*,#44836,.F.);
#60518=ORIENTED_EDGE('',*,*,#44621,.F.);
#60519=ORIENTED_EDGE('',*,*,#44837,.F.);
#60520=ORIENTED_EDGE('',*,*,#44266,.F.);
#60521=ORIENTED_EDGE('',*,*,#44319,.F.);
#60522=ORIENTED_EDGE('',*,*,#44321,.F.);
#60523=ORIENTED_EDGE('',*,*,#44838,.F.);
#60524=ORIENTED_EDGE('',*,*,#44839,.F.);
#60525=ORIENTED_EDGE('',*,*,#44280,.F.);
#60526=ORIENTED_EDGE('',*,*,#44840,.T.);
#60527=ORIENTED_EDGE('',*,*,#44838,.T.);
#60528=ORIENTED_EDGE('',*,*,#44320,.T.);
#60529=ORIENTED_EDGE('',*,*,#44636,.T.);
#60530=ORIENTED_EDGE('',*,*,#44267,.T.);
#60531=ORIENTED_EDGE('',*,*,#44837,.T.);
#60532=ORIENTED_EDGE('',*,*,#44620,.T.);
#60533=ORIENTED_EDGE('',*,*,#44609,.F.);
#60534=ORIENTED_EDGE('',*,*,#44194,.T.);
#60535=ORIENTED_EDGE('',*,*,#44646,.T.);
#60536=ORIENTED_EDGE('',*,*,#44269,.T.);
#60537=ORIENTED_EDGE('',*,*,#44635,.F.);
#60538=ORIENTED_EDGE('',*,*,#44616,.F.);
#60539=ORIENTED_EDGE('',*,*,#44259,.T.);
#60540=ORIENTED_EDGE('',*,*,#44841,.T.);
#60541=ORIENTED_EDGE('',*,*,#44666,.F.);
#60542=ORIENTED_EDGE('',*,*,#44842,.T.);
#60543=ORIENTED_EDGE('',*,*,#44843,.T.);
#60544=ORIENTED_EDGE('',*,*,#44844,.F.);
#60545=ORIENTED_EDGE('',*,*,#44665,.F.);
#60546=ORIENTED_EDGE('',*,*,#44312,.F.);
#60547=ORIENTED_EDGE('',*,*,#44845,.T.);
#60548=ORIENTED_EDGE('',*,*,#44842,.F.);
#60549=ORIENTED_EDGE('',*,*,#44262,.F.);
#60550=ORIENTED_EDGE('',*,*,#44272,.F.);
#60551=ORIENTED_EDGE('',*,*,#44274,.F.);
#60552=ORIENTED_EDGE('',*,*,#44846,.F.);
#60553=ORIENTED_EDGE('',*,*,#44843,.F.);
#60554=ORIENTED_EDGE('',*,*,#44845,.F.);
#60555=ORIENTED_EDGE('',*,*,#44311,.F.);
#60556=ORIENTED_EDGE('',*,*,#44316,.F.);
#60557=ORIENTED_EDGE('',*,*,#44317,.F.);
#60558=ORIENTED_EDGE('',*,*,#44212,.F.);
#60559=ORIENTED_EDGE('',*,*,#44821,.T.);
#60560=ORIENTED_EDGE('',*,*,#44667,.T.);
#60561=ORIENTED_EDGE('',*,*,#44844,.T.);
#60562=ORIENTED_EDGE('',*,*,#44846,.T.);
#60563=ORIENTED_EDGE('',*,*,#44273,.T.);
#60564=ORIENTED_EDGE('',*,*,#44768,.F.);
#60565=ORIENTED_EDGE('',*,*,#44532,.T.);
#60566=ORIENTED_EDGE('',*,*,#44847,.T.);
#60567=ORIENTED_EDGE('',*,*,#44848,.T.);
#60568=ORIENTED_EDGE('',*,*,#44848,.F.);
#60569=ORIENTED_EDGE('',*,*,#44849,.T.);
#60570=ORIENTED_EDGE('',*,*,#44628,.T.);
#60571=ORIENTED_EDGE('',*,*,#44769,.T.);
#60572=ORIENTED_EDGE('',*,*,#44584,.F.);
#60573=ORIENTED_EDGE('',*,*,#44850,.F.);
#60574=ORIENTED_EDGE('',*,*,#44851,.F.);
#60575=ORIENTED_EDGE('',*,*,#44852,.F.);
#60576=ORIENTED_EDGE('',*,*,#44587,.F.);
#60577=ORIENTED_EDGE('',*,*,#44853,.T.);
#60578=ORIENTED_EDGE('',*,*,#44854,.T.);
#60579=ORIENTED_EDGE('',*,*,#44850,.T.);
#60580=ORIENTED_EDGE('',*,*,#44590,.F.);
#60581=ORIENTED_EDGE('',*,*,#44602,.F.);
#60582=ORIENTED_EDGE('',*,*,#44855,.F.);
#60583=ORIENTED_EDGE('',*,*,#44853,.F.);
#60584=ORIENTED_EDGE('',*,*,#44333,.F.);
#60585=ORIENTED_EDGE('',*,*,#44856,.T.);
#60586=ORIENTED_EDGE('',*,*,#44694,.T.);
#60587=ORIENTED_EDGE('',*,*,#44857,.T.);
#60588=ORIENTED_EDGE('',*,*,#44336,.F.);
#60589=ORIENTED_EDGE('',*,*,#44858,.F.);
#60590=ORIENTED_EDGE('',*,*,#44695,.T.);
#60591=ORIENTED_EDGE('',*,*,#44856,.F.);
#60592=ORIENTED_EDGE('',*,*,#44339,.F.);
#60593=ORIENTED_EDGE('',*,*,#44359,.F.);
#60594=ORIENTED_EDGE('',*,*,#44696,.T.);
#60595=ORIENTED_EDGE('',*,*,#44858,.T.);
#60596=ORIENTED_EDGE('',*,*,#44283,.F.);
#60597=ORIENTED_EDGE('',*,*,#44859,.F.);
#60598=ORIENTED_EDGE('',*,*,#44660,.F.);
#60599=ORIENTED_EDGE('',*,*,#44860,.T.);
#60600=ORIENTED_EDGE('',*,*,#44839,.T.);
#60601=ORIENTED_EDGE('',*,*,#44840,.F.);
#60602=ORIENTED_EDGE('',*,*,#44286,.F.);
#60603=ORIENTED_EDGE('',*,*,#44861,.T.);
#60604=ORIENTED_EDGE('',*,*,#44661,.T.);
#60605=ORIENTED_EDGE('',*,*,#44859,.T.);
#60606=ORIENTED_EDGE('',*,*,#44289,.F.);
#60607=ORIENTED_EDGE('',*,*,#44862,.F.);
#60608=ORIENTED_EDGE('',*,*,#44662,.F.);
#60609=ORIENTED_EDGE('',*,*,#44861,.F.);
#60610=ORIENTED_EDGE('',*,*,#44292,.F.);
#60611=ORIENTED_EDGE('',*,*,#44863,.T.);
#60612=ORIENTED_EDGE('',*,*,#44663,.T.);
#60613=ORIENTED_EDGE('',*,*,#44862,.T.);
#60614=ORIENTED_EDGE('',*,*,#44295,.F.);
#60615=ORIENTED_EDGE('',*,*,#44314,.F.);
#60616=ORIENTED_EDGE('',*,*,#44664,.F.);
#60617=ORIENTED_EDGE('',*,*,#44863,.F.);
#60618=ORIENTED_EDGE('',*,*,#44539,.F.);
#60619=ORIENTED_EDGE('',*,*,#44864,.T.);
#60620=ORIENTED_EDGE('',*,*,#44783,.F.);
#60621=ORIENTED_EDGE('',*,*,#44574,.T.);
#60622=ORIENTED_EDGE('',*,*,#44542,.F.);
#60623=ORIENTED_EDGE('',*,*,#44865,.F.);
#60624=ORIENTED_EDGE('',*,*,#44784,.F.);
#60625=ORIENTED_EDGE('',*,*,#44864,.F.);
#60626=ORIENTED_EDGE('',*,*,#44545,.F.);
#60627=ORIENTED_EDGE('',*,*,#44866,.F.);
#60628=ORIENTED_EDGE('',*,*,#44785,.F.);
#60629=ORIENTED_EDGE('',*,*,#44865,.T.);
#60630=ORIENTED_EDGE('',*,*,#44548,.F.);
#60631=ORIENTED_EDGE('',*,*,#44567,.T.);
#60632=ORIENTED_EDGE('',*,*,#44786,.T.);
#60633=ORIENTED_EDGE('',*,*,#44866,.T.);
#60634=ORIENTED_EDGE('',*,*,#44581,.F.);
#60635=ORIENTED_EDGE('',*,*,#44852,.T.);
#60636=ORIENTED_EDGE('',*,*,#44867,.T.);
#60637=ORIENTED_EDGE('',*,*,#44607,.T.);
#60638=ORIENTED_EDGE('',*,*,#44377,.F.);
#60639=ORIENTED_EDGE('',*,*,#44796,.T.);
#60640=ORIENTED_EDGE('',*,*,#44702,.T.);
#60641=ORIENTED_EDGE('',*,*,#44427,.T.);
#60642=ORIENTED_EDGE('',*,*,#44330,.F.);
#60643=ORIENTED_EDGE('',*,*,#44857,.F.);
#60644=ORIENTED_EDGE('',*,*,#44693,.T.);
#60645=ORIENTED_EDGE('',*,*,#44868,.F.);
#60646=ORIENTED_EDGE('',*,*,#44327,.F.);
#60647=ORIENTED_EDGE('',*,*,#44868,.T.);
#60648=ORIENTED_EDGE('',*,*,#44692,.T.);
#60649=ORIENTED_EDGE('',*,*,#44368,.T.);
#60650=ORIENTED_EDGE('',*,*,#44659,.F.);
#60651=ORIENTED_EDGE('',*,*,#44370,.T.);
#60652=ORIENTED_EDGE('',*,*,#44691,.T.);
#60653=ORIENTED_EDGE('',*,*,#44622,.T.);
#60654=ORIENTED_EDGE('',*,*,#44836,.T.);
#60655=ORIENTED_EDGE('',*,*,#44860,.F.);
#60656=ORIENTED_EDGE('',*,*,#44531,.T.);
#60657=ORIENTED_EDGE('',*,*,#44869,.F.);
#60658=ORIENTED_EDGE('',*,*,#44808,.T.);
#60659=ORIENTED_EDGE('',*,*,#44811,.T.);
#60660=ORIENTED_EDGE('',*,*,#44814,.F.);
#60661=ORIENTED_EDGE('',*,*,#44870,.T.);
#60662=ORIENTED_EDGE('',*,*,#44871,.T.);
#60663=ORIENTED_EDGE('',*,*,#44872,.F.);
#60664=ORIENTED_EDGE('',*,*,#44873,.T.);
#60665=ORIENTED_EDGE('',*,*,#44874,.F.);
#60666=ORIENTED_EDGE('',*,*,#44875,.T.);
#60667=ORIENTED_EDGE('',*,*,#44876,.F.);
#60668=ORIENTED_EDGE('',*,*,#44564,.T.);
#60669=ORIENTED_EDGE('',*,*,#44877,.F.);
#60670=ORIENTED_EDGE('',*,*,#44629,.T.);
#60671=ORIENTED_EDGE('',*,*,#44849,.F.);
#60672=ORIENTED_EDGE('',*,*,#44847,.F.);
#60673=ORIENTED_EDGE('',*,*,#44851,.T.);
#60674=ORIENTED_EDGE('',*,*,#44854,.F.);
#60675=ORIENTED_EDGE('',*,*,#44855,.T.);
#60676=ORIENTED_EDGE('',*,*,#44601,.F.);
#60677=ORIENTED_EDGE('',*,*,#44604,.T.);
#60678=ORIENTED_EDGE('',*,*,#44606,.F.);
#60679=ORIENTED_EDGE('',*,*,#44608,.T.);
#60680=ORIENTED_EDGE('',*,*,#44867,.F.);
#60681=ORIENTED_EDGE('',*,*,#44878,.F.);
#60682=ORIENTED_EDGE('',*,*,#44879,.T.);
#60683=ORIENTED_EDGE('',*,*,#44880,.T.);
#60684=ORIENTED_EDGE('',*,*,#44624,.F.);
#60685=ORIENTED_EDGE('',*,*,#44690,.T.);
#60686=ORIENTED_EDGE('',*,*,#44881,.F.);
#60687=ORIENTED_EDGE('',*,*,#44434,.F.);
#60688=ORIENTED_EDGE('',*,*,#44803,.F.);
#60689=ORIENTED_EDGE('',*,*,#44879,.F.);
#60690=ORIENTED_EDGE('',*,*,#44465,.T.);
#60691=ORIENTED_EDGE('',*,*,#44877,.T.);
#60692=ORIENTED_EDGE('',*,*,#44563,.T.);
#60693=ORIENTED_EDGE('',*,*,#44782,.T.);
#60694=ORIENTED_EDGE('',*,*,#44630,.T.);
#60695=ORIENTED_EDGE('',*,*,#44658,.F.);
#60696=ORIENTED_EDGE('',*,*,#44882,.T.);
#60697=ORIENTED_EDGE('',*,*,#44697,.T.);
#60698=ORIENTED_EDGE('',*,*,#44357,.F.);
#60699=ORIENTED_EDGE('',*,*,#44657,.F.);
#60700=ORIENTED_EDGE('',*,*,#44883,.F.);
#60701=ORIENTED_EDGE('',*,*,#44698,.T.);
#60702=ORIENTED_EDGE('',*,*,#44882,.F.);
#60703=ORIENTED_EDGE('',*,*,#44883,.T.);
#60704=ORIENTED_EDGE('',*,*,#44656,.F.);
#60705=ORIENTED_EDGE('',*,*,#44681,.T.);
#60706=ORIENTED_EDGE('',*,*,#44699,.T.);
#60707=ORIENTED_EDGE('',*,*,#44472,.F.);
#60708=ORIENTED_EDGE('',*,*,#44809,.T.);
#60709=ORIENTED_EDGE('',*,*,#44869,.T.);
#60710=ORIENTED_EDGE('',*,*,#44530,.T.);
#60711=ORIENTED_EDGE('',*,*,#44805,.T.);
#60712=ORIENTED_EDGE('',*,*,#44806,.F.);
#60713=ORIENTED_EDGE('',*,*,#44831,.F.);
#60714=ORIENTED_EDGE('',*,*,#44625,.T.);
#60715=ORIENTED_EDGE('',*,*,#44880,.F.);
#60716=ORIENTED_EDGE('',*,*,#44802,.F.);
#60717=ORIENTED_EDGE('',*,*,#44884,.F.);
#60718=ORIENTED_EDGE('',*,*,#44885,.T.);
#60719=ORIENTED_EDGE('',*,*,#44886,.T.);
#60720=ORIENTED_EDGE('',*,*,#44884,.T.);
#60721=ORIENTED_EDGE('',*,*,#44886,.F.);
#60722=ORIENTED_EDGE('',*,*,#44887,.F.);
#60723=ORIENTED_EDGE('',*,*,#44885,.F.);
#60724=ORIENTED_EDGE('',*,*,#44707,.T.);
#60725=ORIENTED_EDGE('',*,*,#44888,.T.);
#60726=ORIENTED_EDGE('',*,*,#44743,.T.);
#60727=ORIENTED_EDGE('',*,*,#44888,.F.);
#60728=ORIENTED_EDGE('',*,*,#44889,.F.);
#60729=ORIENTED_EDGE('',*,*,#44890,.F.);
#60730=ORIENTED_EDGE('',*,*,#44891,.T.);
#60731=ORIENTED_EDGE('',*,*,#44728,.F.);
#60732=ORIENTED_EDGE('',*,*,#44892,.T.);
#60733=ORIENTED_EDGE('',*,*,#44729,.F.);
#60734=ORIENTED_EDGE('',*,*,#44891,.F.);
#60735=ORIENTED_EDGE('',*,*,#44893,.F.);
#60736=ORIENTED_EDGE('',*,*,#44894,.F.);
#60737=ORIENTED_EDGE('',*,*,#44730,.F.);
#60738=ORIENTED_EDGE('',*,*,#44892,.F.);
#60739=ORIENTED_EDGE('',*,*,#44895,.F.);
#60740=ORIENTED_EDGE('',*,*,#44896,.F.);
#60741=ORIENTED_EDGE('',*,*,#44897,.T.);
#60742=ORIENTED_EDGE('',*,*,#44739,.F.);
#60743=ORIENTED_EDGE('',*,*,#44898,.F.);
#60744=ORIENTED_EDGE('',*,*,#44899,.F.);
#60745=ORIENTED_EDGE('',*,*,#44900,.T.);
#60746=ORIENTED_EDGE('',*,*,#44740,.F.);
#60747=ORIENTED_EDGE('',*,*,#44897,.F.);
#60748=ORIENTED_EDGE('',*,*,#44901,.F.);
#60749=ORIENTED_EDGE('',*,*,#44902,.T.);
#60750=ORIENTED_EDGE('',*,*,#44741,.F.);
#60751=ORIENTED_EDGE('',*,*,#44900,.F.);
#60752=ORIENTED_EDGE('',*,*,#44903,.F.);
#60753=ORIENTED_EDGE('',*,*,#44898,.T.);
#60754=ORIENTED_EDGE('',*,*,#44738,.F.);
#60755=ORIENTED_EDGE('',*,*,#44902,.F.);
#60756=ORIENTED_EDGE('',*,*,#44904,.F.);
#60757=ORIENTED_EDGE('',*,*,#44789,.F.);
#60758=ORIENTED_EDGE('',*,*,#44905,.T.);
#60759=ORIENTED_EDGE('',*,*,#44744,.T.);
#60760=ORIENTED_EDGE('',*,*,#44905,.F.);
#60761=ORIENTED_EDGE('',*,*,#44906,.F.);
#60762=ORIENTED_EDGE('',*,*,#44907,.T.);
#60763=ORIENTED_EDGE('',*,*,#44887,.T.);
#60764=ORIENTED_EDGE('',*,*,#44907,.F.);
#60765=ORIENTED_EDGE('',*,*,#44908,.F.);
#60766=ORIENTED_EDGE('',*,*,#44889,.T.);
#60767=ORIENTED_EDGE('',*,*,#44727,.T.);
#60768=ORIENTED_EDGE('',*,*,#44909,.T.);
#60769=ORIENTED_EDGE('',*,*,#44910,.F.);
#60770=ORIENTED_EDGE('',*,*,#44911,.T.);
#60771=ORIENTED_EDGE('',*,*,#44760,.T.);
#60772=ORIENTED_EDGE('',*,*,#44912,.T.);
#60773=ORIENTED_EDGE('',*,*,#44912,.F.);
#60774=ORIENTED_EDGE('',*,*,#44759,.F.);
#60775=ORIENTED_EDGE('',*,*,#44913,.F.);
#60776=ORIENTED_EDGE('',*,*,#44914,.T.);
#60777=ORIENTED_EDGE('',*,*,#44731,.T.);
#60778=ORIENTED_EDGE('',*,*,#44894,.T.);
#60779=ORIENTED_EDGE('',*,*,#44915,.T.);
#60780=ORIENTED_EDGE('',*,*,#44833,.T.);
#60781=ORIENTED_EDGE('',*,*,#44683,.T.);
#60782=ORIENTED_EDGE('',*,*,#44710,.T.);
#60783=ORIENTED_EDGE('',*,*,#44717,.T.);
#60784=ORIENTED_EDGE('',*,*,#44832,.T.);
#60785=ORIENTED_EDGE('',*,*,#44758,.T.);
#60786=ORIENTED_EDGE('',*,*,#44835,.T.);
#60787=ORIENTED_EDGE('',*,*,#44916,.T.);
#60788=ORIENTED_EDGE('',*,*,#44913,.T.);
#60789=ORIENTED_EDGE('',*,*,#44917,.T.);
#60790=ORIENTED_EDGE('',*,*,#44918,.T.);
#60791=ORIENTED_EDGE('',*,*,#44910,.T.);
#60792=ORIENTED_EDGE('',*,*,#44914,.F.);
#60793=ORIENTED_EDGE('',*,*,#44916,.F.);
#60794=ORIENTED_EDGE('',*,*,#44834,.F.);
#60795=ORIENTED_EDGE('',*,*,#44915,.F.);
#60796=ORIENTED_EDGE('',*,*,#44895,.T.);
#60797=ORIENTED_EDGE('',*,*,#44893,.T.);
#60798=ORIENTED_EDGE('',*,*,#44890,.T.);
#60799=ORIENTED_EDGE('',*,*,#44908,.T.);
#60800=ORIENTED_EDGE('',*,*,#44919,.T.);
#60801=ORIENTED_EDGE('',*,*,#44920,.T.);
#60802=ORIENTED_EDGE('',*,*,#44921,.T.);
#60803=ORIENTED_EDGE('',*,*,#44903,.T.);
#60804=ORIENTED_EDGE('',*,*,#44901,.T.);
#60805=ORIENTED_EDGE('',*,*,#44899,.T.);
#60806=ORIENTED_EDGE('',*,*,#44896,.T.);
#60807=ORIENTED_EDGE('',*,*,#44748,.T.);
#60808=ORIENTED_EDGE('',*,*,#44819,.T.);
#60809=ORIENTED_EDGE('',*,*,#44466,.T.);
#60810=ORIENTED_EDGE('',*,*,#44881,.T.);
#60811=ORIENTED_EDGE('',*,*,#44689,.T.);
#60812=ORIENTED_EDGE('',*,*,#44679,.F.);
#60813=ORIENTED_EDGE('',*,*,#44922,.T.);
#60814=ORIENTED_EDGE('',*,*,#44742,.T.);
#60815=ORIENTED_EDGE('',*,*,#44922,.F.);
#60816=ORIENTED_EDGE('',*,*,#44841,.F.);
#60817=ORIENTED_EDGE('',*,*,#44923,.T.);
#60818=ORIENTED_EDGE('',*,*,#44904,.T.);
#60819=ORIENTED_EDGE('',*,*,#44923,.F.);
#60820=ORIENTED_EDGE('',*,*,#44878,.T.);
#60821=ORIENTED_EDGE('',*,*,#44924,.T.);
#60822=ORIENTED_EDGE('',*,*,#44906,.T.);
#60823=ORIENTED_EDGE('',*,*,#44924,.F.);
#60824=ORIENTED_EDGE('',*,*,#44876,.T.);
#60825=ORIENTED_EDGE('',*,*,#44925,.T.);
#60826=ORIENTED_EDGE('',*,*,#44787,.T.);
#60827=ORIENTED_EDGE('',*,*,#44565,.T.);
#60828=ORIENTED_EDGE('',*,*,#44773,.F.);
#60829=ORIENTED_EDGE('',*,*,#44788,.F.);
#60830=ORIENTED_EDGE('',*,*,#44925,.F.);
#60831=ORIENTED_EDGE('',*,*,#44875,.F.);
#60832=ORIENTED_EDGE('',*,*,#44926,.F.);
#60833=ORIENTED_EDGE('',*,*,#44919,.F.);
#60834=ORIENTED_EDGE('',*,*,#44909,.F.);
#60835=ORIENTED_EDGE('',*,*,#44726,.T.);
#60836=ORIENTED_EDGE('',*,*,#44920,.F.);
#60837=ORIENTED_EDGE('',*,*,#44926,.T.);
#60838=ORIENTED_EDGE('',*,*,#44874,.T.);
#60839=ORIENTED_EDGE('',*,*,#44927,.T.);
#60840=ORIENTED_EDGE('',*,*,#44928,.F.);
#60841=ORIENTED_EDGE('',*,*,#44921,.F.);
#60842=ORIENTED_EDGE('',*,*,#44927,.F.);
#60843=ORIENTED_EDGE('',*,*,#44873,.F.);
#60844=ORIENTED_EDGE('',*,*,#44917,.F.);
#60845=ORIENTED_EDGE('',*,*,#44928,.T.);
#60846=ORIENTED_EDGE('',*,*,#44872,.T.);
#60847=ORIENTED_EDGE('',*,*,#44929,.T.);
#60848=ORIENTED_EDGE('',*,*,#44929,.F.);
#60849=ORIENTED_EDGE('',*,*,#44871,.F.);
#60850=ORIENTED_EDGE('',*,*,#44930,.F.);
#60851=ORIENTED_EDGE('',*,*,#44761,.F.);
#60852=ORIENTED_EDGE('',*,*,#44911,.F.);
#60853=ORIENTED_EDGE('',*,*,#44918,.F.);
#60854=ORIENTED_EDGE('',*,*,#44762,.F.);
#60855=ORIENTED_EDGE('',*,*,#44930,.T.);
#60856=ORIENTED_EDGE('',*,*,#44870,.F.);
#60857=ORIENTED_EDGE('',*,*,#44813,.F.);
#60858=ORIENTED_EDGE('',*,*,#44931,.F.);
#60859=ORIENTED_EDGE('',*,*,#44932,.F.);
#60860=ORIENTED_EDGE('',*,*,#44933,.T.);
#60861=ORIENTED_EDGE('',*,*,#44934,.F.);
#60862=ORIENTED_EDGE('',*,*,#44933,.F.);
#60863=ORIENTED_EDGE('',*,*,#44935,.F.);
#60864=ORIENTED_EDGE('',*,*,#44936,.F.);
#60865=ORIENTED_EDGE('',*,*,#44936,.T.);
#60866=ORIENTED_EDGE('',*,*,#44937,.F.);
#60867=ORIENTED_EDGE('',*,*,#44938,.F.);
#60868=ORIENTED_EDGE('',*,*,#44931,.T.);
#60869=ORIENTED_EDGE('',*,*,#44934,.T.);
#60870=ORIENTED_EDGE('',*,*,#44938,.T.);
#60871=ORIENTED_EDGE('',*,*,#44939,.T.);
#60872=ORIENTED_EDGE('',*,*,#44932,.T.);
#60873=ORIENTED_EDGE('',*,*,#44939,.F.);
#60874=ORIENTED_EDGE('',*,*,#44937,.T.);
#60875=ORIENTED_EDGE('',*,*,#44935,.T.);
#60876=ORIENTED_EDGE('',*,*,#44940,.T.);
#60877=ORIENTED_EDGE('',*,*,#44941,.T.);
#60878=ORIENTED_EDGE('',*,*,#44942,.T.);
#60879=ORIENTED_EDGE('',*,*,#44943,.T.);
#60880=ORIENTED_EDGE('',*,*,#44940,.F.);
#60881=ORIENTED_EDGE('',*,*,#44944,.T.);
#60882=ORIENTED_EDGE('',*,*,#44945,.F.);
#60883=ORIENTED_EDGE('',*,*,#44946,.T.);
#60884=ORIENTED_EDGE('',*,*,#44947,.F.);
#60885=ORIENTED_EDGE('',*,*,#44948,.T.);
#60886=ORIENTED_EDGE('',*,*,#44949,.F.);
#60887=ORIENTED_EDGE('',*,*,#44950,.T.);
#60888=ORIENTED_EDGE('',*,*,#44951,.F.);
#60889=ORIENTED_EDGE('',*,*,#44952,.T.);
#60890=ORIENTED_EDGE('',*,*,#44953,.F.);
#60891=ORIENTED_EDGE('',*,*,#44954,.T.);
#60892=ORIENTED_EDGE('',*,*,#44955,.F.);
#60893=ORIENTED_EDGE('',*,*,#44956,.T.);
#60894=ORIENTED_EDGE('',*,*,#44957,.T.);
#60895=ORIENTED_EDGE('',*,*,#44958,.T.);
#60896=ORIENTED_EDGE('',*,*,#44959,.F.);
#60897=ORIENTED_EDGE('',*,*,#44960,.T.);
#60898=ORIENTED_EDGE('',*,*,#44961,.F.);
#60899=ORIENTED_EDGE('',*,*,#44962,.T.);
#60900=ORIENTED_EDGE('',*,*,#44943,.F.);
#60901=ORIENTED_EDGE('',*,*,#44963,.F.);
#60902=ORIENTED_EDGE('',*,*,#44964,.F.);
#60903=ORIENTED_EDGE('',*,*,#44944,.F.);
#60904=ORIENTED_EDGE('',*,*,#44945,.T.);
#60905=ORIENTED_EDGE('',*,*,#44964,.T.);
#60906=ORIENTED_EDGE('',*,*,#44965,.T.);
#60907=ORIENTED_EDGE('',*,*,#44966,.T.);
#60908=ORIENTED_EDGE('',*,*,#44966,.F.);
#60909=ORIENTED_EDGE('',*,*,#44967,.F.);
#60910=ORIENTED_EDGE('',*,*,#44968,.F.);
#60911=ORIENTED_EDGE('',*,*,#44969,.F.);
#60912=ORIENTED_EDGE('',*,*,#44970,.F.);
#60913=ORIENTED_EDGE('',*,*,#44946,.F.);
#60914=ORIENTED_EDGE('',*,*,#44971,.T.);
#60915=ORIENTED_EDGE('',*,*,#44972,.T.);
#60916=ORIENTED_EDGE('',*,*,#44973,.T.);
#60917=ORIENTED_EDGE('',*,*,#44974,.T.);
#60918=ORIENTED_EDGE('',*,*,#44975,.T.);
#60919=ORIENTED_EDGE('',*,*,#44976,.T.);
#60920=ORIENTED_EDGE('',*,*,#44973,.F.);
#60921=ORIENTED_EDGE('',*,*,#44977,.T.);
#60922=ORIENTED_EDGE('',*,*,#44978,.T.);
#60923=ORIENTED_EDGE('',*,*,#44969,.T.);
#60924=ORIENTED_EDGE('',*,*,#44975,.F.);
#60925=ORIENTED_EDGE('',*,*,#44979,.T.);
#60926=ORIENTED_EDGE('',*,*,#44980,.T.);
#60927=ORIENTED_EDGE('',*,*,#44981,.T.);
#60928=ORIENTED_EDGE('',*,*,#44978,.F.);
#60929=ORIENTED_EDGE('',*,*,#44982,.T.);
#60930=ORIENTED_EDGE('',*,*,#44983,.T.);
#60931=ORIENTED_EDGE('',*,*,#44984,.T.);
#60932=ORIENTED_EDGE('',*,*,#44980,.F.);
#60933=ORIENTED_EDGE('',*,*,#44985,.T.);
#60934=ORIENTED_EDGE('',*,*,#44986,.T.);
#60935=ORIENTED_EDGE('',*,*,#44987,.T.);
#60936=ORIENTED_EDGE('',*,*,#44983,.F.);
#60937=ORIENTED_EDGE('',*,*,#44988,.T.);
#60938=ORIENTED_EDGE('',*,*,#44989,.T.);
#60939=ORIENTED_EDGE('',*,*,#44990,.T.);
#60940=ORIENTED_EDGE('',*,*,#44986,.F.);
#60941=ORIENTED_EDGE('',*,*,#44991,.T.);
#60942=ORIENTED_EDGE('',*,*,#44971,.F.);
#60943=ORIENTED_EDGE('',*,*,#44992,.T.);
#60944=ORIENTED_EDGE('',*,*,#44989,.F.);
#60945=ORIENTED_EDGE('',*,*,#44993,.T.);
#60946=ORIENTED_EDGE('',*,*,#44987,.F.);
#60947=ORIENTED_EDGE('',*,*,#44994,.T.);
#60948=ORIENTED_EDGE('',*,*,#44995,.F.);
#60949=ORIENTED_EDGE('',*,*,#44996,.T.);
#60950=ORIENTED_EDGE('',*,*,#44990,.F.);
#60951=ORIENTED_EDGE('',*,*,#44997,.F.);
#60952=ORIENTED_EDGE('',*,*,#44998,.F.);
#60953=ORIENTED_EDGE('',*,*,#44994,.F.);
#60954=ORIENTED_EDGE('',*,*,#44992,.F.);
#60955=ORIENTED_EDGE('',*,*,#44999,.T.);
#60956=ORIENTED_EDGE('',*,*,#45000,.T.);
#60957=ORIENTED_EDGE('',*,*,#44997,.T.);
#60958=ORIENTED_EDGE('',*,*,#44974,.F.);
#60959=ORIENTED_EDGE('',*,*,#45001,.F.);
#60960=ORIENTED_EDGE('',*,*,#45002,.F.);
#60961=ORIENTED_EDGE('',*,*,#45003,.F.);
#60962=ORIENTED_EDGE('',*,*,#45004,.T.);
#60963=ORIENTED_EDGE('',*,*,#44999,.F.);
#60964=ORIENTED_EDGE('',*,*,#44972,.F.);
#60965=ORIENTED_EDGE('',*,*,#44993,.F.);
#60966=ORIENTED_EDGE('',*,*,#44991,.F.);
#60967=ORIENTED_EDGE('',*,*,#44988,.F.);
#60968=ORIENTED_EDGE('',*,*,#44985,.F.);
#60969=ORIENTED_EDGE('',*,*,#44982,.F.);
#60970=ORIENTED_EDGE('',*,*,#44979,.F.);
#60971=ORIENTED_EDGE('',*,*,#44977,.F.);
#60972=ORIENTED_EDGE('',*,*,#45005,.T.);
#60973=ORIENTED_EDGE('',*,*,#45006,.T.);
#60974=ORIENTED_EDGE('',*,*,#45007,.T.);
#60975=ORIENTED_EDGE('',*,*,#45008,.T.);
#60976=ORIENTED_EDGE('',*,*,#45009,.T.);
#60977=ORIENTED_EDGE('',*,*,#45010,.T.);
#60978=ORIENTED_EDGE('',*,*,#45011,.T.);
#60979=ORIENTED_EDGE('',*,*,#45012,.T.);
#60980=ORIENTED_EDGE('',*,*,#45013,.T.);
#60981=ORIENTED_EDGE('',*,*,#45014,.T.);
#60982=ORIENTED_EDGE('',*,*,#45010,.F.);
#60983=ORIENTED_EDGE('',*,*,#45015,.T.);
#60984=ORIENTED_EDGE('',*,*,#45016,.T.);
#60985=ORIENTED_EDGE('',*,*,#45013,.F.);
#60986=ORIENTED_EDGE('',*,*,#45017,.T.);
#60987=ORIENTED_EDGE('',*,*,#45008,.F.);
#60988=ORIENTED_EDGE('',*,*,#45018,.T.);
#60989=ORIENTED_EDGE('',*,*,#45019,.T.);
#60990=ORIENTED_EDGE('',*,*,#45020,.T.);
#60991=ORIENTED_EDGE('',*,*,#45021,.T.);
#60992=ORIENTED_EDGE('',*,*,#45022,.T.);
#60993=ORIENTED_EDGE('',*,*,#45019,.F.);
#60994=ORIENTED_EDGE('',*,*,#45023,.T.);
#60995=ORIENTED_EDGE('',*,*,#45012,.F.);
#60996=ORIENTED_EDGE('',*,*,#45024,.T.);
#60997=ORIENTED_EDGE('',*,*,#45006,.F.);
#60998=ORIENTED_EDGE('',*,*,#45025,.T.);
#60999=ORIENTED_EDGE('',*,*,#45026,.T.);
#61000=ORIENTED_EDGE('',*,*,#45027,.T.);
#61001=ORIENTED_EDGE('',*,*,#45026,.F.);
#61002=ORIENTED_EDGE('',*,*,#45028,.T.);
#61003=ORIENTED_EDGE('',*,*,#45021,.F.);
#61004=ORIENTED_EDGE('',*,*,#45007,.F.);
#61005=ORIENTED_EDGE('',*,*,#45029,.F.);
#61006=ORIENTED_EDGE('',*,*,#45030,.F.);
#61007=ORIENTED_EDGE('',*,*,#45031,.F.);
#61008=ORIENTED_EDGE('',*,*,#45024,.F.);
#61009=ORIENTED_EDGE('',*,*,#45032,.T.);
#61010=ORIENTED_EDGE('',*,*,#45033,.F.);
#61011=ORIENTED_EDGE('',*,*,#45029,.T.);
#61012=ORIENTED_EDGE('',*,*,#45027,.F.);
#61013=ORIENTED_EDGE('',*,*,#45034,.F.);
#61014=ORIENTED_EDGE('',*,*,#45035,.F.);
#61015=ORIENTED_EDGE('',*,*,#45032,.F.);
#61016=ORIENTED_EDGE('',*,*,#45020,.F.);
#61017=ORIENTED_EDGE('',*,*,#45036,.F.);
#61018=ORIENTED_EDGE('',*,*,#45037,.F.);
#61019=ORIENTED_EDGE('',*,*,#45034,.T.);
#61020=ORIENTED_EDGE('',*,*,#45018,.F.);
#61021=ORIENTED_EDGE('',*,*,#45028,.F.);
#61022=ORIENTED_EDGE('',*,*,#45025,.F.);
#61023=ORIENTED_EDGE('',*,*,#45005,.F.);
#61024=ORIENTED_EDGE('',*,*,#45017,.F.);
#61025=ORIENTED_EDGE('',*,*,#45015,.F.);
#61026=ORIENTED_EDGE('',*,*,#45009,.F.);
#61027=ORIENTED_EDGE('',*,*,#45023,.F.);
#61028=ORIENTED_EDGE('',*,*,#45038,.F.);
#61029=ORIENTED_EDGE('',*,*,#45039,.T.);
#61030=ORIENTED_EDGE('',*,*,#45040,.T.);
#61031=ORIENTED_EDGE('',*,*,#45041,.T.);
#61032=ORIENTED_EDGE('',*,*,#45042,.F.);
#61033=ORIENTED_EDGE('',*,*,#45043,.T.);
#61034=ORIENTED_EDGE('',*,*,#45044,.T.);
#61035=ORIENTED_EDGE('',*,*,#45040,.F.);
#61036=ORIENTED_EDGE('',*,*,#45045,.T.);
#61037=ORIENTED_EDGE('',*,*,#45046,.F.);
#61038=ORIENTED_EDGE('',*,*,#45047,.T.);
#61039=ORIENTED_EDGE('',*,*,#45048,.F.);
#61040=ORIENTED_EDGE('',*,*,#45049,.T.);
#61041=ORIENTED_EDGE('',*,*,#45043,.F.);
#61042=ORIENTED_EDGE('',*,*,#45050,.T.);
#61043=ORIENTED_EDGE('',*,*,#45051,.F.);
#61044=ORIENTED_EDGE('',*,*,#45041,.F.);
#61045=ORIENTED_EDGE('',*,*,#45052,.F.);
#61046=ORIENTED_EDGE('',*,*,#45053,.F.);
#61047=ORIENTED_EDGE('',*,*,#45054,.F.);
#61048=ORIENTED_EDGE('',*,*,#45055,.F.);
#61049=ORIENTED_EDGE('',*,*,#45056,.F.);
#61050=ORIENTED_EDGE('',*,*,#45057,.F.);
#61051=ORIENTED_EDGE('',*,*,#45058,.F.);
#61052=ORIENTED_EDGE('',*,*,#45059,.T.);
#61053=ORIENTED_EDGE('',*,*,#45060,.T.);
#61054=ORIENTED_EDGE('',*,*,#45061,.T.);
#61055=ORIENTED_EDGE('',*,*,#45062,.T.);
#61056=ORIENTED_EDGE('',*,*,#45063,.T.);
#61057=ORIENTED_EDGE('',*,*,#45044,.F.);
#61058=ORIENTED_EDGE('',*,*,#45064,.T.);
#61059=ORIENTED_EDGE('',*,*,#45065,.F.);
#61060=ORIENTED_EDGE('',*,*,#45052,.T.);
#61061=ORIENTED_EDGE('',*,*,#45049,.F.);
#61062=ORIENTED_EDGE('',*,*,#45066,.T.);
#61063=ORIENTED_EDGE('',*,*,#45067,.F.);
#61064=ORIENTED_EDGE('',*,*,#45068,.T.);
#61065=ORIENTED_EDGE('',*,*,#45069,.T.);
#61066=ORIENTED_EDGE('',*,*,#45070,.F.);
#61067=ORIENTED_EDGE('',*,*,#45064,.F.);
#61068=ORIENTED_EDGE('',*,*,#45048,.T.);
#61069=ORIENTED_EDGE('',*,*,#45071,.T.);
#61070=ORIENTED_EDGE('',*,*,#45072,.T.);
#61071=ORIENTED_EDGE('',*,*,#45073,.T.);
#61072=ORIENTED_EDGE('',*,*,#45047,.F.);
#61073=ORIENTED_EDGE('',*,*,#45074,.F.);
#61074=ORIENTED_EDGE('',*,*,#45075,.F.);
#61075=ORIENTED_EDGE('',*,*,#45076,.F.);
#61076=ORIENTED_EDGE('',*,*,#45071,.F.);
#61077=ORIENTED_EDGE('',*,*,#45046,.T.);
#61078=ORIENTED_EDGE('',*,*,#45077,.F.);
#61079=ORIENTED_EDGE('',*,*,#45078,.T.);
#61080=ORIENTED_EDGE('',*,*,#45079,.F.);
#61081=ORIENTED_EDGE('',*,*,#45080,.T.);
#61082=ORIENTED_EDGE('',*,*,#45081,.T.);
#61083=ORIENTED_EDGE('',*,*,#45082,.T.);
#61084=ORIENTED_EDGE('',*,*,#45083,.F.);
#61085=ORIENTED_EDGE('',*,*,#45084,.T.);
#61086=ORIENTED_EDGE('',*,*,#45074,.T.);
#61087=ORIENTED_EDGE('',*,*,#45085,.T.);
#61088=ORIENTED_EDGE('',*,*,#45086,.T.);
#61089=ORIENTED_EDGE('',*,*,#45072,.F.);
#61090=ORIENTED_EDGE('',*,*,#45076,.T.);
#61091=ORIENTED_EDGE('',*,*,#45084,.F.);
#61092=ORIENTED_EDGE('',*,*,#45087,.T.);
#61093=ORIENTED_EDGE('',*,*,#45085,.F.);
#61094=ORIENTED_EDGE('',*,*,#45075,.T.);
#61095=ORIENTED_EDGE('',*,*,#45073,.F.);
#61096=ORIENTED_EDGE('',*,*,#45088,.F.);
#61097=ORIENTED_EDGE('',*,*,#45089,.T.);
#61098=ORIENTED_EDGE('',*,*,#45090,.F.);
#61099=ORIENTED_EDGE('',*,*,#45091,.F.);
#61100=ORIENTED_EDGE('',*,*,#45092,.F.);
#61101=ORIENTED_EDGE('',*,*,#45066,.F.);
#61102=ORIENTED_EDGE('',*,*,#45093,.T.);
#61103=ORIENTED_EDGE('',*,*,#45086,.F.);
#61104=ORIENTED_EDGE('',*,*,#45094,.T.);
#61105=ORIENTED_EDGE('',*,*,#45095,.T.);
#61106=ORIENTED_EDGE('',*,*,#45088,.T.);
#61107=ORIENTED_EDGE('',*,*,#45087,.F.);
#61108=ORIENTED_EDGE('',*,*,#45083,.T.);
#61109=ORIENTED_EDGE('',*,*,#45096,.F.);
#61110=ORIENTED_EDGE('',*,*,#45097,.F.);
#61111=ORIENTED_EDGE('',*,*,#45098,.T.);
#61112=ORIENTED_EDGE('',*,*,#45099,.F.);
#61113=ORIENTED_EDGE('',*,*,#45100,.F.);
#61114=ORIENTED_EDGE('',*,*,#45101,.F.);
#61115=ORIENTED_EDGE('',*,*,#44960,.F.);
#61116=ORIENTED_EDGE('',*,*,#45102,.F.);
#61117=ORIENTED_EDGE('',*,*,#45103,.F.);
#61118=ORIENTED_EDGE('',*,*,#45104,.F.);
#61119=ORIENTED_EDGE('',*,*,#45105,.F.);
#61120=ORIENTED_EDGE('',*,*,#45106,.T.);
#61121=ORIENTED_EDGE('',*,*,#45107,.F.);
#61122=ORIENTED_EDGE('',*,*,#45094,.F.);
#61123=ORIENTED_EDGE('',*,*,#45051,.T.);
#61124=ORIENTED_EDGE('',*,*,#45108,.T.);
#61125=ORIENTED_EDGE('',*,*,#45109,.T.);
#61126=ORIENTED_EDGE('',*,*,#45110,.T.);
#61127=ORIENTED_EDGE('',*,*,#45077,.T.);
#61128=ORIENTED_EDGE('',*,*,#45038,.T.);
#61129=ORIENTED_EDGE('',*,*,#45111,.T.);
#61130=ORIENTED_EDGE('',*,*,#45112,.T.);
#61131=ORIENTED_EDGE('',*,*,#45109,.F.);
#61132=ORIENTED_EDGE('',*,*,#45113,.T.);
#61133=ORIENTED_EDGE('',*,*,#45110,.F.);
#61134=ORIENTED_EDGE('',*,*,#45114,.T.);
#61135=ORIENTED_EDGE('',*,*,#45115,.F.);
#61136=ORIENTED_EDGE('',*,*,#45078,.F.);
#61137=ORIENTED_EDGE('',*,*,#45112,.F.);
#61138=ORIENTED_EDGE('',*,*,#45116,.T.);
#61139=ORIENTED_EDGE('',*,*,#45117,.F.);
#61140=ORIENTED_EDGE('',*,*,#45114,.F.);
#61141=ORIENTED_EDGE('',*,*,#45118,.T.);
#61142=ORIENTED_EDGE('',*,*,#45119,.T.);
#61143=ORIENTED_EDGE('',*,*,#45120,.T.);
#61144=ORIENTED_EDGE('',*,*,#45121,.F.);
#61145=ORIENTED_EDGE('',*,*,#45122,.T.);
#61146=ORIENTED_EDGE('',*,*,#45123,.T.);
#61147=ORIENTED_EDGE('',*,*,#45119,.F.);
#61148=ORIENTED_EDGE('',*,*,#45124,.T.);
#61149=ORIENTED_EDGE('',*,*,#45125,.T.);
#61150=ORIENTED_EDGE('',*,*,#45126,.T.);
#61151=ORIENTED_EDGE('',*,*,#45122,.F.);
#61152=ORIENTED_EDGE('',*,*,#45127,.T.);
#61153=ORIENTED_EDGE('',*,*,#45128,.T.);
#61154=ORIENTED_EDGE('',*,*,#45129,.T.);
#61155=ORIENTED_EDGE('',*,*,#45125,.F.);
#61156=ORIENTED_EDGE('',*,*,#45130,.T.);
#61157=ORIENTED_EDGE('',*,*,#45131,.T.);
#61158=ORIENTED_EDGE('',*,*,#45128,.F.);
#61159=ORIENTED_EDGE('',*,*,#45132,.T.);
#61160=ORIENTED_EDGE('',*,*,#45133,.T.);
#61161=ORIENTED_EDGE('',*,*,#45134,.T.);
#61162=ORIENTED_EDGE('',*,*,#45133,.F.);
#61163=ORIENTED_EDGE('',*,*,#45135,.T.);
#61164=ORIENTED_EDGE('',*,*,#45121,.T.);
#61165=ORIENTED_EDGE('',*,*,#45131,.F.);
#61166=ORIENTED_EDGE('',*,*,#45136,.T.);
#61167=ORIENTED_EDGE('',*,*,#45137,.F.);
#61168=ORIENTED_EDGE('',*,*,#45138,.F.);
#61169=ORIENTED_EDGE('',*,*,#45139,.F.);
#61170=ORIENTED_EDGE('',*,*,#45140,.F.);
#61171=ORIENTED_EDGE('',*,*,#45134,.F.);
#61172=ORIENTED_EDGE('',*,*,#45141,.T.);
#61173=ORIENTED_EDGE('',*,*,#45142,.F.);
#61174=ORIENTED_EDGE('',*,*,#45143,.F.);
#61175=ORIENTED_EDGE('',*,*,#45144,.F.);
#61176=ORIENTED_EDGE('',*,*,#45145,.T.);
#61177=ORIENTED_EDGE('',*,*,#45136,.F.);
#61178=ORIENTED_EDGE('',*,*,#45120,.F.);
#61179=ORIENTED_EDGE('',*,*,#45146,.F.);
#61180=ORIENTED_EDGE('',*,*,#45147,.F.);
#61181=ORIENTED_EDGE('',*,*,#45141,.F.);
#61182=ORIENTED_EDGE('',*,*,#45118,.F.);
#61183=ORIENTED_EDGE('',*,*,#45135,.F.);
#61184=ORIENTED_EDGE('',*,*,#45132,.F.);
#61185=ORIENTED_EDGE('',*,*,#45130,.F.);
#61186=ORIENTED_EDGE('',*,*,#45127,.F.);
#61187=ORIENTED_EDGE('',*,*,#45124,.F.);
#61188=ORIENTED_EDGE('',*,*,#45148,.F.);
#61189=ORIENTED_EDGE('',*,*,#45149,.T.);
#61190=ORIENTED_EDGE('',*,*,#45150,.F.);
#61191=ORIENTED_EDGE('',*,*,#45151,.F.);
#61192=ORIENTED_EDGE('',*,*,#45152,.T.);
#61193=ORIENTED_EDGE('',*,*,#45153,.F.);
#61194=ORIENTED_EDGE('',*,*,#45154,.F.);
#61195=ORIENTED_EDGE('',*,*,#45155,.F.);
#61196=ORIENTED_EDGE('',*,*,#45155,.T.);
#61197=ORIENTED_EDGE('',*,*,#45156,.T.);
#61198=ORIENTED_EDGE('',*,*,#45157,.T.);
#61199=ORIENTED_EDGE('',*,*,#45154,.T.);
#61200=ORIENTED_EDGE('',*,*,#45158,.T.);
#61201=ORIENTED_EDGE('',*,*,#45159,.T.);
#61202=ORIENTED_EDGE('',*,*,#45156,.F.);
#61203=ORIENTED_EDGE('',*,*,#45153,.T.);
#61204=ORIENTED_EDGE('',*,*,#45160,.T.);
#61205=ORIENTED_EDGE('',*,*,#45161,.T.);
#61206=ORIENTED_EDGE('',*,*,#45162,.T.);
#61207=ORIENTED_EDGE('',*,*,#45158,.F.);
#61208=ORIENTED_EDGE('',*,*,#45152,.F.);
#61209=ORIENTED_EDGE('',*,*,#45163,.F.);
#61210=ORIENTED_EDGE('',*,*,#45164,.F.);
#61211=ORIENTED_EDGE('',*,*,#45165,.F.);
#61212=ORIENTED_EDGE('',*,*,#45166,.F.);
#61213=ORIENTED_EDGE('',*,*,#45167,.F.);
#61214=ORIENTED_EDGE('',*,*,#45168,.F.);
#61215=ORIENTED_EDGE('',*,*,#45169,.F.);
#61216=ORIENTED_EDGE('',*,*,#45160,.F.);
#61217=ORIENTED_EDGE('',*,*,#45170,.T.);
#61218=ORIENTED_EDGE('',*,*,#45171,.T.);
#61219=ORIENTED_EDGE('',*,*,#45161,.F.);
#61220=ORIENTED_EDGE('',*,*,#45169,.T.);
#61221=ORIENTED_EDGE('',*,*,#45172,.T.);
#61222=ORIENTED_EDGE('',*,*,#45173,.T.);
#61223=ORIENTED_EDGE('',*,*,#45170,.F.);
#61224=ORIENTED_EDGE('',*,*,#45168,.T.);
#61225=ORIENTED_EDGE('',*,*,#45174,.T.);
#61226=ORIENTED_EDGE('',*,*,#45175,.T.);
#61227=ORIENTED_EDGE('',*,*,#45172,.F.);
#61228=ORIENTED_EDGE('',*,*,#45167,.T.);
#61229=ORIENTED_EDGE('',*,*,#45176,.T.);
#61230=ORIENTED_EDGE('',*,*,#45177,.T.);
#61231=ORIENTED_EDGE('',*,*,#45174,.F.);
#61232=ORIENTED_EDGE('',*,*,#45166,.T.);
#61233=ORIENTED_EDGE('',*,*,#45178,.T.);
#61234=ORIENTED_EDGE('',*,*,#45179,.T.);
#61235=ORIENTED_EDGE('',*,*,#45176,.F.);
#61236=ORIENTED_EDGE('',*,*,#45165,.T.);
#61237=ORIENTED_EDGE('',*,*,#45180,.T.);
#61238=ORIENTED_EDGE('',*,*,#45181,.T.);
#61239=ORIENTED_EDGE('',*,*,#45178,.F.);
#61240=ORIENTED_EDGE('',*,*,#45164,.T.);
#61241=ORIENTED_EDGE('',*,*,#45151,.T.);
#61242=ORIENTED_EDGE('',*,*,#45182,.T.);
#61243=ORIENTED_EDGE('',*,*,#45180,.F.);
#61244=ORIENTED_EDGE('',*,*,#45163,.T.);
#61245=ORIENTED_EDGE('',*,*,#45148,.T.);
#61246=ORIENTED_EDGE('',*,*,#45157,.F.);
#61247=ORIENTED_EDGE('',*,*,#45183,.T.);
#61248=ORIENTED_EDGE('',*,*,#45184,.F.);
#61249=ORIENTED_EDGE('',*,*,#45185,.T.);
#61250=ORIENTED_EDGE('',*,*,#45186,.F.);
#61251=ORIENTED_EDGE('',*,*,#45159,.F.);
#61252=ORIENTED_EDGE('',*,*,#45187,.F.);
#61253=ORIENTED_EDGE('',*,*,#45188,.F.);
#61254=ORIENTED_EDGE('',*,*,#45183,.F.);
#61255=ORIENTED_EDGE('',*,*,#45162,.F.);
#61256=ORIENTED_EDGE('',*,*,#45189,.F.);
#61257=ORIENTED_EDGE('',*,*,#45190,.F.);
#61258=ORIENTED_EDGE('',*,*,#45187,.T.);
#61259=ORIENTED_EDGE('',*,*,#45171,.F.);
#61260=ORIENTED_EDGE('',*,*,#45191,.F.);
#61261=ORIENTED_EDGE('',*,*,#45192,.F.);
#61262=ORIENTED_EDGE('',*,*,#45189,.T.);
#61263=ORIENTED_EDGE('',*,*,#45173,.F.);
#61264=ORIENTED_EDGE('',*,*,#45193,.T.);
#61265=ORIENTED_EDGE('',*,*,#45194,.T.);
#61266=ORIENTED_EDGE('',*,*,#45191,.T.);
#61267=ORIENTED_EDGE('',*,*,#45175,.F.);
#61268=ORIENTED_EDGE('',*,*,#45195,.F.);
#61269=ORIENTED_EDGE('',*,*,#45196,.F.);
#61270=ORIENTED_EDGE('',*,*,#45193,.F.);
#61271=ORIENTED_EDGE('',*,*,#45177,.F.);
#61272=ORIENTED_EDGE('',*,*,#45197,.T.);
#61273=ORIENTED_EDGE('',*,*,#45198,.T.);
#61274=ORIENTED_EDGE('',*,*,#45195,.T.);
#61275=ORIENTED_EDGE('',*,*,#45179,.F.);
#61276=ORIENTED_EDGE('',*,*,#45199,.F.);
#61277=ORIENTED_EDGE('',*,*,#45200,.F.);
#61278=ORIENTED_EDGE('',*,*,#45197,.F.);
#61279=ORIENTED_EDGE('',*,*,#45181,.F.);
#61280=ORIENTED_EDGE('',*,*,#45201,.T.);
#61281=ORIENTED_EDGE('',*,*,#45202,.T.);
#61282=ORIENTED_EDGE('',*,*,#45199,.T.);
#61283=ORIENTED_EDGE('',*,*,#45150,.T.);
#61284=ORIENTED_EDGE('',*,*,#45203,.T.);
#61285=ORIENTED_EDGE('',*,*,#45185,.F.);
#61286=ORIENTED_EDGE('',*,*,#45204,.T.);
#61287=ORIENTED_EDGE('',*,*,#45205,.T.);
#61288=ORIENTED_EDGE('',*,*,#45206,.F.);
#61289=ORIENTED_EDGE('',*,*,#45207,.F.);
#61290=ORIENTED_EDGE('',*,*,#45208,.T.);
#61291=ORIENTED_EDGE('',*,*,#45209,.F.);
#61292=ORIENTED_EDGE('',*,*,#45210,.T.);
#61293=ORIENTED_EDGE('',*,*,#45211,.F.);
#61294=ORIENTED_EDGE('',*,*,#45212,.F.);
#61295=ORIENTED_EDGE('',*,*,#45213,.T.);
#61296=ORIENTED_EDGE('',*,*,#45201,.F.);
#61297=ORIENTED_EDGE('',*,*,#45182,.F.);
#61298=ORIENTED_EDGE('',*,*,#45149,.F.);
#61299=ORIENTED_EDGE('',*,*,#45186,.T.);
#61300=ORIENTED_EDGE('',*,*,#45203,.F.);
#61301=ORIENTED_EDGE('',*,*,#45214,.T.);
#61302=ORIENTED_EDGE('',*,*,#45215,.T.);
#61303=ORIENTED_EDGE('',*,*,#45216,.T.);
#61304=ORIENTED_EDGE('',*,*,#45217,.T.);
#61305=ORIENTED_EDGE('',*,*,#45218,.T.);
#61306=ORIENTED_EDGE('',*,*,#45219,.T.);
#61307=ORIENTED_EDGE('',*,*,#45216,.F.);
#61308=ORIENTED_EDGE('',*,*,#45220,.T.);
#61309=ORIENTED_EDGE('',*,*,#45221,.T.);
#61310=ORIENTED_EDGE('',*,*,#45222,.T.);
#61311=ORIENTED_EDGE('',*,*,#45218,.F.);
#61312=ORIENTED_EDGE('',*,*,#45223,.T.);
#61313=ORIENTED_EDGE('',*,*,#45224,.T.);
#61314=ORIENTED_EDGE('',*,*,#45225,.T.);
#61315=ORIENTED_EDGE('',*,*,#45221,.F.);
#61316=ORIENTED_EDGE('',*,*,#45226,.T.);
#61317=ORIENTED_EDGE('',*,*,#45227,.T.);
#61318=ORIENTED_EDGE('',*,*,#45228,.T.);
#61319=ORIENTED_EDGE('',*,*,#45224,.F.);
#61320=ORIENTED_EDGE('',*,*,#45229,.T.);
#61321=ORIENTED_EDGE('',*,*,#45230,.T.);
#61322=ORIENTED_EDGE('',*,*,#45231,.T.);
#61323=ORIENTED_EDGE('',*,*,#45227,.F.);
#61324=ORIENTED_EDGE('',*,*,#45232,.T.);
#61325=ORIENTED_EDGE('',*,*,#45233,.T.);
#61326=ORIENTED_EDGE('',*,*,#45234,.T.);
#61327=ORIENTED_EDGE('',*,*,#45235,.T.);
#61328=ORIENTED_EDGE('',*,*,#45236,.T.);
#61329=ORIENTED_EDGE('',*,*,#45237,.T.);
#61330=ORIENTED_EDGE('',*,*,#45238,.T.);
#61331=ORIENTED_EDGE('',*,*,#45235,.F.);
#61332=ORIENTED_EDGE('',*,*,#45239,.T.);
#61333=ORIENTED_EDGE('',*,*,#45240,.T.);
#61334=ORIENTED_EDGE('',*,*,#45241,.T.);
#61335=ORIENTED_EDGE('',*,*,#45237,.F.);
#61336=ORIENTED_EDGE('',*,*,#45242,.T.);
#61337=ORIENTED_EDGE('',*,*,#45243,.T.);
#61338=ORIENTED_EDGE('',*,*,#45244,.T.);
#61339=ORIENTED_EDGE('',*,*,#45240,.F.);
#61340=ORIENTED_EDGE('',*,*,#45245,.T.);
#61341=ORIENTED_EDGE('',*,*,#45233,.F.);
#61342=ORIENTED_EDGE('',*,*,#45246,.T.);
#61343=ORIENTED_EDGE('',*,*,#45230,.F.);
#61344=ORIENTED_EDGE('',*,*,#45247,.T.);
#61345=ORIENTED_EDGE('',*,*,#45214,.F.);
#61346=ORIENTED_EDGE('',*,*,#45248,.T.);
#61347=ORIENTED_EDGE('',*,*,#45243,.F.);
#61348=ORIENTED_EDGE('',*,*,#45222,.F.);
#61349=ORIENTED_EDGE('',*,*,#45249,.F.);
#61350=ORIENTED_EDGE('',*,*,#45250,.F.);
#61351=ORIENTED_EDGE('',*,*,#45251,.F.);
#61352=ORIENTED_EDGE('',*,*,#45225,.F.);
#61353=ORIENTED_EDGE('',*,*,#45252,.T.);
#61354=ORIENTED_EDGE('',*,*,#45253,.T.);
#61355=ORIENTED_EDGE('',*,*,#45249,.T.);
#61356=ORIENTED_EDGE('',*,*,#45228,.F.);
#61357=ORIENTED_EDGE('',*,*,#45254,.F.);
#61358=ORIENTED_EDGE('',*,*,#45255,.F.);
#61359=ORIENTED_EDGE('',*,*,#45252,.F.);
#61360=ORIENTED_EDGE('',*,*,#45231,.F.);
#61361=ORIENTED_EDGE('',*,*,#45256,.T.);
#61362=ORIENTED_EDGE('',*,*,#45257,.T.);
#61363=ORIENTED_EDGE('',*,*,#45254,.T.);
#61364=ORIENTED_EDGE('',*,*,#45246,.F.);
#61365=ORIENTED_EDGE('',*,*,#45258,.F.);
#61366=ORIENTED_EDGE('',*,*,#45259,.F.);
#61367=ORIENTED_EDGE('',*,*,#45256,.F.);
#61368=ORIENTED_EDGE('',*,*,#45236,.F.);
#61369=ORIENTED_EDGE('',*,*,#45260,.F.);
#61370=ORIENTED_EDGE('',*,*,#45261,.F.);
#61371=ORIENTED_EDGE('',*,*,#45258,.T.);
#61372=ORIENTED_EDGE('',*,*,#45234,.F.);
#61373=ORIENTED_EDGE('',*,*,#45247,.F.);
#61374=ORIENTED_EDGE('',*,*,#45232,.F.);
#61375=ORIENTED_EDGE('',*,*,#45229,.F.);
#61376=ORIENTED_EDGE('',*,*,#45226,.F.);
#61377=ORIENTED_EDGE('',*,*,#45223,.F.);
#61378=ORIENTED_EDGE('',*,*,#45220,.F.);
#61379=ORIENTED_EDGE('',*,*,#45215,.F.);
#61380=ORIENTED_EDGE('',*,*,#45245,.F.);
#61381=ORIENTED_EDGE('',*,*,#45242,.F.);
#61382=ORIENTED_EDGE('',*,*,#45239,.F.);
#61383=ORIENTED_EDGE('',*,*,#45262,.T.);
#61384=ORIENTED_EDGE('',*,*,#45263,.T.);
#61385=ORIENTED_EDGE('',*,*,#45264,.T.);
#61386=ORIENTED_EDGE('',*,*,#45265,.T.);
#61387=ORIENTED_EDGE('',*,*,#45266,.T.);
#61388=ORIENTED_EDGE('',*,*,#45267,.T.);
#61389=ORIENTED_EDGE('',*,*,#45264,.F.);
#61390=ORIENTED_EDGE('',*,*,#45268,.T.);
#61391=ORIENTED_EDGE('',*,*,#45269,.T.);
#61392=ORIENTED_EDGE('',*,*,#45270,.T.);
#61393=ORIENTED_EDGE('',*,*,#45266,.F.);
#61394=ORIENTED_EDGE('',*,*,#45271,.T.);
#61395=ORIENTED_EDGE('',*,*,#45272,.T.);
#61396=ORIENTED_EDGE('',*,*,#45273,.T.);
#61397=ORIENTED_EDGE('',*,*,#45269,.F.);
#61398=ORIENTED_EDGE('',*,*,#45274,.T.);
#61399=ORIENTED_EDGE('',*,*,#45275,.T.);
#61400=ORIENTED_EDGE('',*,*,#45276,.T.);
#61401=ORIENTED_EDGE('',*,*,#45272,.F.);
#61402=ORIENTED_EDGE('',*,*,#45277,.T.);
#61403=ORIENTED_EDGE('',*,*,#45278,.T.);
#61404=ORIENTED_EDGE('',*,*,#45279,.T.);
#61405=ORIENTED_EDGE('',*,*,#45275,.F.);
#61406=ORIENTED_EDGE('',*,*,#45280,.T.);
#61407=ORIENTED_EDGE('',*,*,#45281,.T.);
#61408=ORIENTED_EDGE('',*,*,#45282,.T.);
#61409=ORIENTED_EDGE('',*,*,#45278,.F.);
#61410=ORIENTED_EDGE('',*,*,#45283,.T.);
#61411=ORIENTED_EDGE('',*,*,#45284,.T.);
#61412=ORIENTED_EDGE('',*,*,#45285,.T.);
#61413=ORIENTED_EDGE('',*,*,#45281,.F.);
#61414=ORIENTED_EDGE('',*,*,#45286,.T.);
#61415=ORIENTED_EDGE('',*,*,#45287,.T.);
#61416=ORIENTED_EDGE('',*,*,#45288,.T.);
#61417=ORIENTED_EDGE('',*,*,#45284,.F.);
#61418=ORIENTED_EDGE('',*,*,#45289,.T.);
#61419=ORIENTED_EDGE('',*,*,#45290,.T.);
#61420=ORIENTED_EDGE('',*,*,#45291,.T.);
#61421=ORIENTED_EDGE('',*,*,#45287,.F.);
#61422=ORIENTED_EDGE('',*,*,#45292,.T.);
#61423=ORIENTED_EDGE('',*,*,#45293,.T.);
#61424=ORIENTED_EDGE('',*,*,#45294,.T.);
#61425=ORIENTED_EDGE('',*,*,#45290,.F.);
#61426=ORIENTED_EDGE('',*,*,#45295,.T.);
#61427=ORIENTED_EDGE('',*,*,#45262,.F.);
#61428=ORIENTED_EDGE('',*,*,#45296,.T.);
#61429=ORIENTED_EDGE('',*,*,#45293,.F.);
#61430=ORIENTED_EDGE('',*,*,#45297,.T.);
#61431=ORIENTED_EDGE('',*,*,#45285,.F.);
#61432=ORIENTED_EDGE('',*,*,#45298,.T.);
#61433=ORIENTED_EDGE('',*,*,#45299,.T.);
#61434=ORIENTED_EDGE('',*,*,#45300,.T.);
#61435=ORIENTED_EDGE('',*,*,#45288,.F.);
#61436=ORIENTED_EDGE('',*,*,#45301,.F.);
#61437=ORIENTED_EDGE('',*,*,#45302,.F.);
#61438=ORIENTED_EDGE('',*,*,#45298,.F.);
#61439=ORIENTED_EDGE('',*,*,#45291,.F.);
#61440=ORIENTED_EDGE('',*,*,#45303,.T.);
#61441=ORIENTED_EDGE('',*,*,#45304,.T.);
#61442=ORIENTED_EDGE('',*,*,#45301,.T.);
#61443=ORIENTED_EDGE('',*,*,#45294,.F.);
#61444=ORIENTED_EDGE('',*,*,#45305,.F.);
#61445=ORIENTED_EDGE('',*,*,#45306,.F.);
#61446=ORIENTED_EDGE('',*,*,#45303,.F.);
#61447=ORIENTED_EDGE('',*,*,#45296,.F.);
#61448=ORIENTED_EDGE('',*,*,#45307,.T.);
#61449=ORIENTED_EDGE('',*,*,#45308,.T.);
#61450=ORIENTED_EDGE('',*,*,#45305,.T.);
#61451=ORIENTED_EDGE('',*,*,#45265,.F.);
#61452=ORIENTED_EDGE('',*,*,#45309,.F.);
#61453=ORIENTED_EDGE('',*,*,#45310,.F.);
#61454=ORIENTED_EDGE('',*,*,#45307,.F.);
#61455=ORIENTED_EDGE('',*,*,#45263,.F.);
#61456=ORIENTED_EDGE('',*,*,#45297,.F.);
#61457=ORIENTED_EDGE('',*,*,#45295,.F.);
#61458=ORIENTED_EDGE('',*,*,#45292,.F.);
#61459=ORIENTED_EDGE('',*,*,#45289,.F.);
#61460=ORIENTED_EDGE('',*,*,#45286,.F.);
#61461=ORIENTED_EDGE('',*,*,#45283,.F.);
#61462=ORIENTED_EDGE('',*,*,#45280,.F.);
#61463=ORIENTED_EDGE('',*,*,#45277,.F.);
#61464=ORIENTED_EDGE('',*,*,#45274,.F.);
#61465=ORIENTED_EDGE('',*,*,#45271,.F.);
#61466=ORIENTED_EDGE('',*,*,#45268,.F.);
#61467=ORIENTED_EDGE('',*,*,#45311,.T.);
#61468=ORIENTED_EDGE('',*,*,#45312,.T.);
#61469=ORIENTED_EDGE('',*,*,#45313,.T.);
#61470=ORIENTED_EDGE('',*,*,#45314,.T.);
#61471=ORIENTED_EDGE('',*,*,#45315,.T.);
#61472=ORIENTED_EDGE('',*,*,#45316,.T.);
#61473=ORIENTED_EDGE('',*,*,#45313,.F.);
#61474=ORIENTED_EDGE('',*,*,#45317,.T.);
#61475=ORIENTED_EDGE('',*,*,#45318,.T.);
#61476=ORIENTED_EDGE('',*,*,#45319,.T.);
#61477=ORIENTED_EDGE('',*,*,#45315,.F.);
#61478=ORIENTED_EDGE('',*,*,#45320,.T.);
#61479=ORIENTED_EDGE('',*,*,#45321,.T.);
#61480=ORIENTED_EDGE('',*,*,#45322,.T.);
#61481=ORIENTED_EDGE('',*,*,#45318,.F.);
#61482=ORIENTED_EDGE('',*,*,#45323,.T.);
#61483=ORIENTED_EDGE('',*,*,#45324,.T.);
#61484=ORIENTED_EDGE('',*,*,#45325,.T.);
#61485=ORIENTED_EDGE('',*,*,#45321,.F.);
#61486=ORIENTED_EDGE('',*,*,#45326,.T.);
#61487=ORIENTED_EDGE('',*,*,#45327,.T.);
#61488=ORIENTED_EDGE('',*,*,#45328,.T.);
#61489=ORIENTED_EDGE('',*,*,#45324,.F.);
#61490=ORIENTED_EDGE('',*,*,#45329,.T.);
#61491=ORIENTED_EDGE('',*,*,#45330,.T.);
#61492=ORIENTED_EDGE('',*,*,#45331,.T.);
#61493=ORIENTED_EDGE('',*,*,#45327,.F.);
#61494=ORIENTED_EDGE('',*,*,#45332,.T.);
#61495=ORIENTED_EDGE('',*,*,#45333,.T.);
#61496=ORIENTED_EDGE('',*,*,#45334,.T.);
#61497=ORIENTED_EDGE('',*,*,#45330,.F.);
#61498=ORIENTED_EDGE('',*,*,#45335,.T.);
#61499=ORIENTED_EDGE('',*,*,#45336,.T.);
#61500=ORIENTED_EDGE('',*,*,#45337,.T.);
#61501=ORIENTED_EDGE('',*,*,#45333,.F.);
#61502=ORIENTED_EDGE('',*,*,#45338,.T.);
#61503=ORIENTED_EDGE('',*,*,#45339,.T.);
#61504=ORIENTED_EDGE('',*,*,#45340,.T.);
#61505=ORIENTED_EDGE('',*,*,#45336,.F.);
#61506=ORIENTED_EDGE('',*,*,#45341,.T.);
#61507=ORIENTED_EDGE('',*,*,#45311,.F.);
#61508=ORIENTED_EDGE('',*,*,#45342,.T.);
#61509=ORIENTED_EDGE('',*,*,#45339,.F.);
#61510=ORIENTED_EDGE('',*,*,#45343,.T.);
#61511=ORIENTED_EDGE('',*,*,#45331,.F.);
#61512=ORIENTED_EDGE('',*,*,#45344,.F.);
#61513=ORIENTED_EDGE('',*,*,#45345,.F.);
#61514=ORIENTED_EDGE('',*,*,#45346,.T.);
#61515=ORIENTED_EDGE('',*,*,#45334,.F.);
#61516=ORIENTED_EDGE('',*,*,#45347,.T.);
#61517=ORIENTED_EDGE('',*,*,#45348,.T.);
#61518=ORIENTED_EDGE('',*,*,#45344,.T.);
#61519=ORIENTED_EDGE('',*,*,#45337,.F.);
#61520=ORIENTED_EDGE('',*,*,#45349,.T.);
#61521=ORIENTED_EDGE('',*,*,#45350,.F.);
#61522=ORIENTED_EDGE('',*,*,#45351,.F.);
#61523=ORIENTED_EDGE('',*,*,#45352,.T.);
#61524=ORIENTED_EDGE('',*,*,#45347,.F.);
#61525=ORIENTED_EDGE('',*,*,#45340,.F.);
#61526=ORIENTED_EDGE('',*,*,#45353,.F.);
#61527=ORIENTED_EDGE('',*,*,#45354,.T.);
#61528=ORIENTED_EDGE('',*,*,#45355,.F.);
#61529=ORIENTED_EDGE('',*,*,#45356,.F.);
#61530=ORIENTED_EDGE('',*,*,#45357,.T.);
#61531=ORIENTED_EDGE('',*,*,#45358,.F.);
#61532=ORIENTED_EDGE('',*,*,#45359,.T.);
#61533=ORIENTED_EDGE('',*,*,#45360,.F.);
#61534=ORIENTED_EDGE('',*,*,#45361,.F.);
#61535=ORIENTED_EDGE('',*,*,#45349,.F.);
#61536=ORIENTED_EDGE('',*,*,#45342,.F.);
#61537=ORIENTED_EDGE('',*,*,#45362,.T.);
#61538=ORIENTED_EDGE('',*,*,#45363,.T.);
#61539=ORIENTED_EDGE('',*,*,#45353,.T.);
#61540=ORIENTED_EDGE('',*,*,#45314,.F.);
#61541=ORIENTED_EDGE('',*,*,#45364,.F.);
#61542=ORIENTED_EDGE('',*,*,#45365,.F.);
#61543=ORIENTED_EDGE('',*,*,#45362,.F.);
#61544=ORIENTED_EDGE('',*,*,#45312,.F.);
#61545=ORIENTED_EDGE('',*,*,#45343,.F.);
#61546=ORIENTED_EDGE('',*,*,#45341,.F.);
#61547=ORIENTED_EDGE('',*,*,#45338,.F.);
#61548=ORIENTED_EDGE('',*,*,#45335,.F.);
#61549=ORIENTED_EDGE('',*,*,#45332,.F.);
#61550=ORIENTED_EDGE('',*,*,#45329,.F.);
#61551=ORIENTED_EDGE('',*,*,#45326,.F.);
#61552=ORIENTED_EDGE('',*,*,#45323,.F.);
#61553=ORIENTED_EDGE('',*,*,#45320,.F.);
#61554=ORIENTED_EDGE('',*,*,#45317,.F.);
#61555=ORIENTED_EDGE('',*,*,#45366,.T.);
#61556=ORIENTED_EDGE('',*,*,#45367,.T.);
#61557=ORIENTED_EDGE('',*,*,#45368,.T.);
#61558=ORIENTED_EDGE('',*,*,#45369,.T.);
#61559=ORIENTED_EDGE('',*,*,#45370,.T.);
#61560=ORIENTED_EDGE('',*,*,#45371,.T.);
#61561=ORIENTED_EDGE('',*,*,#45367,.F.);
#61562=ORIENTED_EDGE('',*,*,#45372,.T.);
#61563=ORIENTED_EDGE('',*,*,#45373,.T.);
#61564=ORIENTED_EDGE('',*,*,#45374,.T.);
#61565=ORIENTED_EDGE('',*,*,#45370,.F.);
#61566=ORIENTED_EDGE('',*,*,#45375,.T.);
#61567=ORIENTED_EDGE('',*,*,#45376,.T.);
#61568=ORIENTED_EDGE('',*,*,#45377,.T.);
#61569=ORIENTED_EDGE('',*,*,#45373,.F.);
#61570=ORIENTED_EDGE('',*,*,#45378,.T.);
#61571=ORIENTED_EDGE('',*,*,#45379,.T.);
#61572=ORIENTED_EDGE('',*,*,#45376,.F.);
#61573=ORIENTED_EDGE('',*,*,#45380,.T.);
#61574=ORIENTED_EDGE('',*,*,#45381,.F.);
#61575=ORIENTED_EDGE('',*,*,#45382,.T.);
#61576=ORIENTED_EDGE('',*,*,#45369,.F.);
#61577=ORIENTED_EDGE('',*,*,#45383,.F.);
#61578=ORIENTED_EDGE('',*,*,#45384,.T.);
#61579=ORIENTED_EDGE('',*,*,#45385,.F.);
#61580=ORIENTED_EDGE('',*,*,#45381,.T.);
#61581=ORIENTED_EDGE('',*,*,#45377,.F.);
#61582=ORIENTED_EDGE('',*,*,#45386,.T.);
#61583=ORIENTED_EDGE('',*,*,#45387,.T.);
#61584=ORIENTED_EDGE('',*,*,#45388,.T.);
#61585=ORIENTED_EDGE('',*,*,#45379,.F.);
#61586=ORIENTED_EDGE('',*,*,#45385,.T.);
#61587=ORIENTED_EDGE('',*,*,#45389,.T.);
#61588=ORIENTED_EDGE('',*,*,#45390,.T.);
#61589=ORIENTED_EDGE('',*,*,#45391,.T.);
#61590=ORIENTED_EDGE('',*,*,#45392,.F.);
#61591=ORIENTED_EDGE('',*,*,#45393,.F.);
#61592=ORIENTED_EDGE('',*,*,#45394,.F.);
#61593=ORIENTED_EDGE('',*,*,#45395,.F.);
#61594=ORIENTED_EDGE('',*,*,#45386,.F.);
#61595=ORIENTED_EDGE('',*,*,#45384,.F.);
#61596=ORIENTED_EDGE('',*,*,#45396,.F.);
#61597=ORIENTED_EDGE('',*,*,#45397,.F.);
#61598=ORIENTED_EDGE('',*,*,#45389,.F.);
#61599=ORIENTED_EDGE('',*,*,#45366,.F.);
#61600=ORIENTED_EDGE('',*,*,#45382,.F.);
#61601=ORIENTED_EDGE('',*,*,#45380,.F.);
#61602=ORIENTED_EDGE('',*,*,#45378,.F.);
#61603=ORIENTED_EDGE('',*,*,#45375,.F.);
#61604=ORIENTED_EDGE('',*,*,#45372,.F.);
#61605=ORIENTED_EDGE('',*,*,#45368,.F.);
#61606=ORIENTED_EDGE('',*,*,#45398,.F.);
#61607=ORIENTED_EDGE('',*,*,#45399,.F.);
#61608=ORIENTED_EDGE('',*,*,#45400,.F.);
#61609=ORIENTED_EDGE('',*,*,#45401,.T.);
#61610=ORIENTED_EDGE('',*,*,#45402,.T.);
#61611=ORIENTED_EDGE('',*,*,#45403,.T.);
#61612=ORIENTED_EDGE('',*,*,#45404,.F.);
#61613=ORIENTED_EDGE('',*,*,#45405,.F.);
#61614=ORIENTED_EDGE('',*,*,#45406,.T.);
#61615=ORIENTED_EDGE('',*,*,#45407,.F.);
#61616=ORIENTED_EDGE('',*,*,#45408,.F.);
#61617=ORIENTED_EDGE('',*,*,#45396,.T.);
#61618=ORIENTED_EDGE('',*,*,#45383,.T.);
#61619=ORIENTED_EDGE('',*,*,#45409,.T.);
#61620=ORIENTED_EDGE('',*,*,#45410,.T.);
#61621=ORIENTED_EDGE('',*,*,#45411,.T.);
#61622=ORIENTED_EDGE('',*,*,#45412,.T.);
#61623=ORIENTED_EDGE('',*,*,#45413,.T.);
#61624=ORIENTED_EDGE('',*,*,#45414,.T.);
#61625=ORIENTED_EDGE('',*,*,#45411,.F.);
#61626=ORIENTED_EDGE('',*,*,#45415,.T.);
#61627=ORIENTED_EDGE('',*,*,#45416,.T.);
#61628=ORIENTED_EDGE('',*,*,#45417,.T.);
#61629=ORIENTED_EDGE('',*,*,#45413,.F.);
#61630=ORIENTED_EDGE('',*,*,#45418,.T.);
#61631=ORIENTED_EDGE('',*,*,#45419,.T.);
#61632=ORIENTED_EDGE('',*,*,#45420,.T.);
#61633=ORIENTED_EDGE('',*,*,#45416,.F.);
#61634=ORIENTED_EDGE('',*,*,#45421,.T.);
#61635=ORIENTED_EDGE('',*,*,#45422,.T.);
#61636=ORIENTED_EDGE('',*,*,#45423,.T.);
#61637=ORIENTED_EDGE('',*,*,#45419,.F.);
#61638=ORIENTED_EDGE('',*,*,#45424,.T.);
#61639=ORIENTED_EDGE('',*,*,#45425,.T.);
#61640=ORIENTED_EDGE('',*,*,#45426,.T.);
#61641=ORIENTED_EDGE('',*,*,#45422,.F.);
#61642=ORIENTED_EDGE('',*,*,#45427,.T.);
#61643=ORIENTED_EDGE('',*,*,#45428,.T.);
#61644=ORIENTED_EDGE('',*,*,#45429,.T.);
#61645=ORIENTED_EDGE('',*,*,#45425,.F.);
#61646=ORIENTED_EDGE('',*,*,#45430,.T.);
#61647=ORIENTED_EDGE('',*,*,#45431,.T.);
#61648=ORIENTED_EDGE('',*,*,#45432,.T.);
#61649=ORIENTED_EDGE('',*,*,#45428,.F.);
#61650=ORIENTED_EDGE('',*,*,#45433,.T.);
#61651=ORIENTED_EDGE('',*,*,#45434,.T.);
#61652=ORIENTED_EDGE('',*,*,#45435,.T.);
#61653=ORIENTED_EDGE('',*,*,#45436,.T.);
#61654=ORIENTED_EDGE('',*,*,#45431,.F.);
#61655=ORIENTED_EDGE('',*,*,#45437,.T.);
#61656=ORIENTED_EDGE('',*,*,#45438,.T.);
#61657=ORIENTED_EDGE('',*,*,#45439,.T.);
#61658=ORIENTED_EDGE('',*,*,#45434,.F.);
#61659=ORIENTED_EDGE('',*,*,#45440,.T.);
#61660=ORIENTED_EDGE('',*,*,#45441,.T.);
#61661=ORIENTED_EDGE('',*,*,#45442,.T.);
#61662=ORIENTED_EDGE('',*,*,#45438,.F.);
#61663=ORIENTED_EDGE('',*,*,#45443,.T.);
#61664=ORIENTED_EDGE('',*,*,#45409,.F.);
#61665=ORIENTED_EDGE('',*,*,#45444,.T.);
#61666=ORIENTED_EDGE('',*,*,#45441,.F.);
#61667=ORIENTED_EDGE('',*,*,#45445,.T.);
#61668=ORIENTED_EDGE('',*,*,#45432,.F.);
#61669=ORIENTED_EDGE('',*,*,#45446,.T.);
#61670=ORIENTED_EDGE('',*,*,#45447,.T.);
#61671=ORIENTED_EDGE('',*,*,#45448,.T.);
#61672=ORIENTED_EDGE('',*,*,#45449,.F.);
#61673=ORIENTED_EDGE('',*,*,#45450,.T.);
#61674=ORIENTED_EDGE('',*,*,#45435,.F.);
#61675=ORIENTED_EDGE('',*,*,#45451,.F.);
#61676=ORIENTED_EDGE('',*,*,#45452,.F.);
#61677=ORIENTED_EDGE('',*,*,#45453,.F.);
#61678=ORIENTED_EDGE('',*,*,#45454,.F.);
#61679=ORIENTED_EDGE('',*,*,#45455,.F.);
#61680=ORIENTED_EDGE('',*,*,#45456,.F.);
#61681=ORIENTED_EDGE('',*,*,#45457,.F.);
#61682=ORIENTED_EDGE('',*,*,#45458,.F.);
#61683=ORIENTED_EDGE('',*,*,#45459,.F.);
#61684=ORIENTED_EDGE('',*,*,#45460,.F.);
#61685=ORIENTED_EDGE('',*,*,#45446,.F.);
#61686=ORIENTED_EDGE('',*,*,#45436,.F.);
#61687=ORIENTED_EDGE('',*,*,#45450,.F.);
#61688=ORIENTED_EDGE('',*,*,#45439,.F.);
#61689=ORIENTED_EDGE('',*,*,#45461,.T.);
#61690=ORIENTED_EDGE('',*,*,#45462,.T.);
#61691=ORIENTED_EDGE('',*,*,#45451,.T.);
#61692=ORIENTED_EDGE('',*,*,#45442,.F.);
#61693=ORIENTED_EDGE('',*,*,#45463,.F.);
#61694=ORIENTED_EDGE('',*,*,#45464,.F.);
#61695=ORIENTED_EDGE('',*,*,#45461,.F.);
#61696=ORIENTED_EDGE('',*,*,#45444,.F.);
#61697=ORIENTED_EDGE('',*,*,#45465,.T.);
#61698=ORIENTED_EDGE('',*,*,#45466,.T.);
#61699=ORIENTED_EDGE('',*,*,#45463,.T.);
#61700=ORIENTED_EDGE('',*,*,#45412,.F.);
#61701=ORIENTED_EDGE('',*,*,#45467,.T.);
#61702=ORIENTED_EDGE('',*,*,#45468,.F.);
#61703=ORIENTED_EDGE('',*,*,#45465,.F.);
#61704=ORIENTED_EDGE('',*,*,#45410,.F.);
#61705=ORIENTED_EDGE('',*,*,#45445,.F.);
#61706=ORIENTED_EDGE('',*,*,#45443,.F.);
#61707=ORIENTED_EDGE('',*,*,#45440,.F.);
#61708=ORIENTED_EDGE('',*,*,#45437,.F.);
#61709=ORIENTED_EDGE('',*,*,#45433,.F.);
#61710=ORIENTED_EDGE('',*,*,#45430,.F.);
#61711=ORIENTED_EDGE('',*,*,#45427,.F.);
#61712=ORIENTED_EDGE('',*,*,#45424,.F.);
#61713=ORIENTED_EDGE('',*,*,#45421,.F.);
#61714=ORIENTED_EDGE('',*,*,#45418,.F.);
#61715=ORIENTED_EDGE('',*,*,#45415,.F.);
#61716=ORIENTED_EDGE('',*,*,#45469,.T.);
#61717=ORIENTED_EDGE('',*,*,#45470,.T.);
#61718=ORIENTED_EDGE('',*,*,#45471,.T.);
#61719=ORIENTED_EDGE('',*,*,#45472,.F.);
#61720=ORIENTED_EDGE('',*,*,#45473,.T.);
#61721=ORIENTED_EDGE('',*,*,#45474,.T.);
#61722=ORIENTED_EDGE('',*,*,#45470,.F.);
#61723=ORIENTED_EDGE('',*,*,#45475,.T.);
#61724=ORIENTED_EDGE('',*,*,#45476,.T.);
#61725=ORIENTED_EDGE('',*,*,#45477,.T.);
#61726=ORIENTED_EDGE('',*,*,#45473,.F.);
#61727=ORIENTED_EDGE('',*,*,#45478,.T.);
#61728=ORIENTED_EDGE('',*,*,#45479,.T.);
#61729=ORIENTED_EDGE('',*,*,#45480,.T.);
#61730=ORIENTED_EDGE('',*,*,#45476,.F.);
#61731=ORIENTED_EDGE('',*,*,#45481,.T.);
#61732=ORIENTED_EDGE('',*,*,#45482,.T.);
#61733=ORIENTED_EDGE('',*,*,#45483,.T.);
#61734=ORIENTED_EDGE('',*,*,#45479,.F.);
#61735=ORIENTED_EDGE('',*,*,#45484,.T.);
#61736=ORIENTED_EDGE('',*,*,#45485,.T.);
#61737=ORIENTED_EDGE('',*,*,#45486,.T.);
#61738=ORIENTED_EDGE('',*,*,#45482,.F.);
#61739=ORIENTED_EDGE('',*,*,#45487,.T.);
#61740=ORIENTED_EDGE('',*,*,#45488,.T.);
#61741=ORIENTED_EDGE('',*,*,#45458,.T.);
#61742=ORIENTED_EDGE('',*,*,#45485,.F.);
#61743=ORIENTED_EDGE('',*,*,#45489,.T.);
#61744=ORIENTED_EDGE('',*,*,#45490,.T.);
#61745=ORIENTED_EDGE('',*,*,#45491,.T.);
#61746=ORIENTED_EDGE('',*,*,#45488,.F.);
#61747=ORIENTED_EDGE('',*,*,#45492,.T.);
#61748=ORIENTED_EDGE('',*,*,#45493,.T.);
#61749=ORIENTED_EDGE('',*,*,#45494,.T.);
#61750=ORIENTED_EDGE('',*,*,#45490,.F.);
#61751=ORIENTED_EDGE('',*,*,#45495,.T.);
#61752=ORIENTED_EDGE('',*,*,#45496,.T.);
#61753=ORIENTED_EDGE('',*,*,#45497,.T.);
#61754=ORIENTED_EDGE('',*,*,#45493,.F.);
#61755=ORIENTED_EDGE('',*,*,#45498,.T.);
#61756=ORIENTED_EDGE('',*,*,#45499,.T.);
#61757=ORIENTED_EDGE('',*,*,#45496,.F.);
#61758=ORIENTED_EDGE('',*,*,#45500,.T.);
#61759=ORIENTED_EDGE('',*,*,#45501,.T.);
#61760=ORIENTED_EDGE('',*,*,#45502,.T.);
#61761=ORIENTED_EDGE('',*,*,#45503,.F.);
#61762=ORIENTED_EDGE('',*,*,#45501,.F.);
#61763=ORIENTED_EDGE('',*,*,#45504,.T.);
#61764=ORIENTED_EDGE('',*,*,#45472,.T.);
#61765=ORIENTED_EDGE('',*,*,#45505,.F.);
#61766=ORIENTED_EDGE('',*,*,#45494,.F.);
#61767=ORIENTED_EDGE('',*,*,#45506,.F.);
#61768=ORIENTED_EDGE('',*,*,#45507,.F.);
#61769=ORIENTED_EDGE('',*,*,#45508,.F.);
#61770=ORIENTED_EDGE('',*,*,#45497,.F.);
#61771=ORIENTED_EDGE('',*,*,#45509,.T.);
#61772=ORIENTED_EDGE('',*,*,#45510,.T.);
#61773=ORIENTED_EDGE('',*,*,#45506,.T.);
#61774=ORIENTED_EDGE('',*,*,#45502,.F.);
#61775=ORIENTED_EDGE('',*,*,#45511,.F.);
#61776=ORIENTED_EDGE('',*,*,#45423,.F.);
#61777=ORIENTED_EDGE('',*,*,#45512,.F.);
#61778=ORIENTED_EDGE('',*,*,#45513,.F.);
#61779=ORIENTED_EDGE('',*,*,#45509,.F.);
#61780=ORIENTED_EDGE('',*,*,#45499,.F.);
#61781=ORIENTED_EDGE('',*,*,#45503,.T.);
#61782=ORIENTED_EDGE('',*,*,#45511,.T.);
#61783=ORIENTED_EDGE('',*,*,#45505,.T.);
#61784=ORIENTED_EDGE('',*,*,#45471,.F.);
#61785=ORIENTED_EDGE('',*,*,#45514,.F.);
#61786=ORIENTED_EDGE('',*,*,#45515,.T.);
#61787=ORIENTED_EDGE('',*,*,#45516,.F.);
#61788=ORIENTED_EDGE('',*,*,#45517,.T.);
#61789=ORIENTED_EDGE('',*,*,#45518,.F.);
#61790=ORIENTED_EDGE('',*,*,#45519,.F.);
#61791=ORIENTED_EDGE('',*,*,#45520,.F.);
#61792=ORIENTED_EDGE('',*,*,#45521,.F.);
#61793=ORIENTED_EDGE('',*,*,#45522,.T.);
#61794=ORIENTED_EDGE('',*,*,#45523,.T.);
#61795=ORIENTED_EDGE('',*,*,#45524,.F.);
#61796=ORIENTED_EDGE('',*,*,#45525,.T.);
#61797=ORIENTED_EDGE('',*,*,#45526,.F.);
#61798=ORIENTED_EDGE('',*,*,#45527,.T.);
#61799=ORIENTED_EDGE('',*,*,#45528,.F.);
#61800=ORIENTED_EDGE('',*,*,#45469,.F.);
#61801=ORIENTED_EDGE('',*,*,#45504,.F.);
#61802=ORIENTED_EDGE('',*,*,#45500,.F.);
#61803=ORIENTED_EDGE('',*,*,#45498,.F.);
#61804=ORIENTED_EDGE('',*,*,#45495,.F.);
#61805=ORIENTED_EDGE('',*,*,#45492,.F.);
#61806=ORIENTED_EDGE('',*,*,#45489,.F.);
#61807=ORIENTED_EDGE('',*,*,#45487,.F.);
#61808=ORIENTED_EDGE('',*,*,#45484,.F.);
#61809=ORIENTED_EDGE('',*,*,#45481,.F.);
#61810=ORIENTED_EDGE('',*,*,#45478,.F.);
#61811=ORIENTED_EDGE('',*,*,#45475,.F.);
#61812=ORIENTED_EDGE('',*,*,#45529,.T.);
#61813=ORIENTED_EDGE('',*,*,#45530,.T.);
#61814=ORIENTED_EDGE('',*,*,#45531,.T.);
#61815=ORIENTED_EDGE('',*,*,#45532,.T.);
#61816=ORIENTED_EDGE('',*,*,#45533,.T.);
#61817=ORIENTED_EDGE('',*,*,#45534,.T.);
#61818=ORIENTED_EDGE('',*,*,#45531,.F.);
#61819=ORIENTED_EDGE('',*,*,#45535,.T.);
#61820=ORIENTED_EDGE('',*,*,#45536,.T.);
#61821=ORIENTED_EDGE('',*,*,#45537,.T.);
#61822=ORIENTED_EDGE('',*,*,#45533,.F.);
#61823=ORIENTED_EDGE('',*,*,#45538,.T.);
#61824=ORIENTED_EDGE('',*,*,#45539,.T.);
#61825=ORIENTED_EDGE('',*,*,#45540,.T.);
#61826=ORIENTED_EDGE('',*,*,#45536,.F.);
#61827=ORIENTED_EDGE('',*,*,#45541,.T.);
#61828=ORIENTED_EDGE('',*,*,#45542,.T.);
#61829=ORIENTED_EDGE('',*,*,#45454,.T.);
#61830=ORIENTED_EDGE('',*,*,#45539,.F.);
#61831=ORIENTED_EDGE('',*,*,#45543,.T.);
#61832=ORIENTED_EDGE('',*,*,#45544,.T.);
#61833=ORIENTED_EDGE('',*,*,#45545,.T.);
#61834=ORIENTED_EDGE('',*,*,#45542,.F.);
#61835=ORIENTED_EDGE('',*,*,#45546,.T.);
#61836=ORIENTED_EDGE('',*,*,#45547,.T.);
#61837=ORIENTED_EDGE('',*,*,#45548,.T.);
#61838=ORIENTED_EDGE('',*,*,#45544,.F.);
#61839=ORIENTED_EDGE('',*,*,#45549,.T.);
#61840=ORIENTED_EDGE('',*,*,#45550,.T.);
#61841=ORIENTED_EDGE('',*,*,#45551,.T.);
#61842=ORIENTED_EDGE('',*,*,#45547,.F.);
#61843=ORIENTED_EDGE('',*,*,#45552,.T.);
#61844=ORIENTED_EDGE('',*,*,#45553,.T.);
#61845=ORIENTED_EDGE('',*,*,#45554,.T.);
#61846=ORIENTED_EDGE('',*,*,#45550,.F.);
#61847=ORIENTED_EDGE('',*,*,#45555,.T.);
#61848=ORIENTED_EDGE('',*,*,#45529,.F.);
#61849=ORIENTED_EDGE('',*,*,#45556,.T.);
#61850=ORIENTED_EDGE('',*,*,#45553,.F.);
#61851=ORIENTED_EDGE('',*,*,#45557,.T.);
#61852=ORIENTED_EDGE('',*,*,#45548,.F.);
#61853=ORIENTED_EDGE('',*,*,#45558,.F.);
#61854=ORIENTED_EDGE('',*,*,#45559,.F.);
#61855=ORIENTED_EDGE('',*,*,#45560,.F.);
#61856=ORIENTED_EDGE('',*,*,#45551,.F.);
#61857=ORIENTED_EDGE('',*,*,#45561,.T.);
#61858=ORIENTED_EDGE('',*,*,#45562,.T.);
#61859=ORIENTED_EDGE('',*,*,#45558,.T.);
#61860=ORIENTED_EDGE('',*,*,#45554,.F.);
#61861=ORIENTED_EDGE('',*,*,#45563,.F.);
#61862=ORIENTED_EDGE('',*,*,#45564,.T.);
#61863=ORIENTED_EDGE('',*,*,#45561,.F.);
#61864=ORIENTED_EDGE('',*,*,#45556,.F.);
#61865=ORIENTED_EDGE('',*,*,#45565,.T.);
#61866=ORIENTED_EDGE('',*,*,#45566,.T.);
#61867=ORIENTED_EDGE('',*,*,#45563,.T.);
#61868=ORIENTED_EDGE('',*,*,#45532,.F.);
#61869=ORIENTED_EDGE('',*,*,#45567,.F.);
#61870=ORIENTED_EDGE('',*,*,#45568,.F.);
#61871=ORIENTED_EDGE('',*,*,#45569,.F.);
#61872=ORIENTED_EDGE('',*,*,#45570,.T.);
#61873=ORIENTED_EDGE('',*,*,#45571,.F.);
#61874=ORIENTED_EDGE('',*,*,#45572,.T.);
#61875=ORIENTED_EDGE('',*,*,#45573,.F.);
#61876=ORIENTED_EDGE('',*,*,#45574,.F.);
#61877=ORIENTED_EDGE('',*,*,#45575,.F.);
#61878=ORIENTED_EDGE('',*,*,#45576,.F.);
#61879=ORIENTED_EDGE('',*,*,#45577,.T.);
#61880=ORIENTED_EDGE('',*,*,#45578,.F.);
#61881=ORIENTED_EDGE('',*,*,#45579,.T.);
#61882=ORIENTED_EDGE('',*,*,#45565,.F.);
#61883=ORIENTED_EDGE('',*,*,#45530,.F.);
#61884=ORIENTED_EDGE('',*,*,#45557,.F.);
#61885=ORIENTED_EDGE('',*,*,#45555,.F.);
#61886=ORIENTED_EDGE('',*,*,#45552,.F.);
#61887=ORIENTED_EDGE('',*,*,#45549,.F.);
#61888=ORIENTED_EDGE('',*,*,#45546,.F.);
#61889=ORIENTED_EDGE('',*,*,#45543,.F.);
#61890=ORIENTED_EDGE('',*,*,#45541,.F.);
#61891=ORIENTED_EDGE('',*,*,#45538,.F.);
#61892=ORIENTED_EDGE('',*,*,#45535,.F.);
#61893=ORIENTED_EDGE('',*,*,#45414,.F.);
#61894=ORIENTED_EDGE('',*,*,#45580,.T.);
#61895=ORIENTED_EDGE('',*,*,#45581,.T.);
#61896=ORIENTED_EDGE('',*,*,#45467,.F.);
#61897=ORIENTED_EDGE('',*,*,#45417,.F.);
#61898=ORIENTED_EDGE('',*,*,#45582,.F.);
#61899=ORIENTED_EDGE('',*,*,#45583,.F.);
#61900=ORIENTED_EDGE('',*,*,#45580,.F.);
#61901=ORIENTED_EDGE('',*,*,#45420,.F.);
#61902=ORIENTED_EDGE('',*,*,#45528,.T.);
#61903=ORIENTED_EDGE('',*,*,#45584,.T.);
#61904=ORIENTED_EDGE('',*,*,#45582,.T.);
#61905=ORIENTED_EDGE('',*,*,#45371,.F.);
#61906=ORIENTED_EDGE('',*,*,#45585,.T.);
#61907=ORIENTED_EDGE('',*,*,#45586,.T.);
#61908=ORIENTED_EDGE('',*,*,#45398,.T.);
#61909=ORIENTED_EDGE('',*,*,#45374,.F.);
#61910=ORIENTED_EDGE('',*,*,#45388,.F.);
#61911=ORIENTED_EDGE('',*,*,#45587,.F.);
#61912=ORIENTED_EDGE('',*,*,#45585,.F.);
#61913=ORIENTED_EDGE('',*,*,#45588,.T.);
#61914=ORIENTED_EDGE('',*,*,#45589,.T.);
#61915=ORIENTED_EDGE('',*,*,#45590,.T.);
#61916=ORIENTED_EDGE('',*,*,#45591,.T.);
#61917=ORIENTED_EDGE('',*,*,#45592,.F.);
#61918=ORIENTED_EDGE('',*,*,#45591,.F.);
#61919=ORIENTED_EDGE('',*,*,#45593,.F.);
#61920=ORIENTED_EDGE('',*,*,#45594,.F.);
#61921=ORIENTED_EDGE('',*,*,#45595,.F.);
#61922=ORIENTED_EDGE('',*,*,#45596,.F.);
#61923=ORIENTED_EDGE('',*,*,#45597,.F.);
#61924=ORIENTED_EDGE('',*,*,#45598,.F.);
#61925=ORIENTED_EDGE('',*,*,#45589,.F.);
#61926=ORIENTED_EDGE('',*,*,#45599,.F.);
#61927=ORIENTED_EDGE('',*,*,#45600,.F.);
#61928=ORIENTED_EDGE('',*,*,#45601,.F.);
#61929=ORIENTED_EDGE('',*,*,#45602,.T.);
#61930=ORIENTED_EDGE('',*,*,#45598,.T.);
#61931=ORIENTED_EDGE('',*,*,#45603,.T.);
#61932=ORIENTED_EDGE('',*,*,#45526,.T.);
#61933=ORIENTED_EDGE('',*,*,#45426,.F.);
#61934=ORIENTED_EDGE('',*,*,#45604,.T.);
#61935=ORIENTED_EDGE('',*,*,#45605,.T.);
#61936=ORIENTED_EDGE('',*,*,#45512,.T.);
#61937=ORIENTED_EDGE('',*,*,#45606,.T.);
#61938=ORIENTED_EDGE('',*,*,#45607,.T.);
#61939=ORIENTED_EDGE('',*,*,#45608,.T.);
#61940=ORIENTED_EDGE('',*,*,#45594,.T.);
#61941=ORIENTED_EDGE('',*,*,#45609,.F.);
#61942=ORIENTED_EDGE('',*,*,#45610,.T.);
#61943=ORIENTED_EDGE('',*,*,#45611,.T.);
#61944=ORIENTED_EDGE('',*,*,#45600,.T.);
#61945=ORIENTED_EDGE('',*,*,#45610,.F.);
#61946=ORIENTED_EDGE('',*,*,#45612,.T.);
#61947=ORIENTED_EDGE('',*,*,#45613,.F.);
#61948=ORIENTED_EDGE('',*,*,#45614,.F.);
#61949=ORIENTED_EDGE('',*,*,#45607,.F.);
#61950=ORIENTED_EDGE('',*,*,#45615,.F.);
#61951=ORIENTED_EDGE('',*,*,#45616,.F.);
#61952=ORIENTED_EDGE('',*,*,#45617,.F.);
#61953=ORIENTED_EDGE('',*,*,#45618,.F.);
#61954=ORIENTED_EDGE('',*,*,#45616,.T.);
#61955=ORIENTED_EDGE('',*,*,#45619,.F.);
#61956=ORIENTED_EDGE('',*,*,#45620,.F.);
#61957=ORIENTED_EDGE('',*,*,#45621,.F.);
#61958=ORIENTED_EDGE('',*,*,#45622,.F.);
#61959=ORIENTED_EDGE('',*,*,#45623,.F.);
#61960=ORIENTED_EDGE('',*,*,#45624,.T.);
#61961=ORIENTED_EDGE('',*,*,#45622,.T.);
#61962=ORIENTED_EDGE('',*,*,#45624,.F.);
#61963=ORIENTED_EDGE('',*,*,#45625,.F.);
#61964=ORIENTED_EDGE('',*,*,#45626,.T.);
#61965=ORIENTED_EDGE('',*,*,#45621,.T.);
#61966=ORIENTED_EDGE('',*,*,#45626,.F.);
#61967=ORIENTED_EDGE('',*,*,#45244,.F.);
#61968=ORIENTED_EDGE('',*,*,#45627,.F.);
#61969=ORIENTED_EDGE('',*,*,#45628,.T.);
#61970=ORIENTED_EDGE('',*,*,#45629,.T.);
#61971=ORIENTED_EDGE('',*,*,#45630,.F.);
#61972=ORIENTED_EDGE('',*,*,#45631,.F.);
#61973=ORIENTED_EDGE('',*,*,#45632,.F.);
#61974=ORIENTED_EDGE('',*,*,#45633,.F.);
#61975=ORIENTED_EDGE('',*,*,#45634,.T.);
#61976=ORIENTED_EDGE('',*,*,#45635,.F.);
#61977=ORIENTED_EDGE('',*,*,#45248,.F.);
#61978=ORIENTED_EDGE('',*,*,#45636,.T.);
#61979=ORIENTED_EDGE('',*,*,#45637,.F.);
#61980=ORIENTED_EDGE('',*,*,#45627,.T.);
#61981=ORIENTED_EDGE('',*,*,#45217,.F.);
#61982=ORIENTED_EDGE('',*,*,#45638,.F.);
#61983=ORIENTED_EDGE('',*,*,#45639,.F.);
#61984=ORIENTED_EDGE('',*,*,#45636,.F.);
#61985=ORIENTED_EDGE('',*,*,#45219,.F.);
#61986=ORIENTED_EDGE('',*,*,#45251,.T.);
#61987=ORIENTED_EDGE('',*,*,#45640,.T.);
#61988=ORIENTED_EDGE('',*,*,#45638,.T.);
#61989=ORIENTED_EDGE('',*,*,#45641,.T.);
#61990=ORIENTED_EDGE('',*,*,#45642,.T.);
#61991=ORIENTED_EDGE('',*,*,#45643,.T.);
#61992=ORIENTED_EDGE('',*,*,#45633,.T.);
#61993=ORIENTED_EDGE('',*,*,#45644,.T.);
#61994=ORIENTED_EDGE('',*,*,#45645,.T.);
#61995=ORIENTED_EDGE('',*,*,#45646,.T.);
#61996=ORIENTED_EDGE('',*,*,#45647,.T.);
#61997=ORIENTED_EDGE('',*,*,#45647,.F.);
#61998=ORIENTED_EDGE('',*,*,#45648,.F.);
#61999=ORIENTED_EDGE('',*,*,#45649,.F.);
#62000=ORIENTED_EDGE('',*,*,#45650,.F.);
#62001=ORIENTED_EDGE('',*,*,#45238,.F.);
#62002=ORIENTED_EDGE('',*,*,#45651,.T.);
#62003=ORIENTED_EDGE('',*,*,#45652,.T.);
#62004=ORIENTED_EDGE('',*,*,#45260,.T.);
#62005=ORIENTED_EDGE('',*,*,#45645,.F.);
#62006=ORIENTED_EDGE('',*,*,#45653,.F.);
#62007=ORIENTED_EDGE('',*,*,#45654,.F.);
#62008=ORIENTED_EDGE('',*,*,#45655,.F.);
#62009=ORIENTED_EDGE('',*,*,#45656,.F.);
#62010=ORIENTED_EDGE('',*,*,#45657,.T.);
#62011=ORIENTED_EDGE('',*,*,#45658,.T.);
#62012=ORIENTED_EDGE('',*,*,#45654,.T.);
#62013=ORIENTED_EDGE('',*,*,#45659,.T.);
#62014=ORIENTED_EDGE('',*,*,#45660,.T.);
#62015=ORIENTED_EDGE('',*,*,#45661,.T.);
#62016=ORIENTED_EDGE('',*,*,#45662,.T.);
#62017=ORIENTED_EDGE('',*,*,#45660,.F.);
#62018=ORIENTED_EDGE('',*,*,#45663,.F.);
#62019=ORIENTED_EDGE('',*,*,#45629,.F.);
#62020=ORIENTED_EDGE('',*,*,#45664,.F.);
#62021=ORIENTED_EDGE('',*,*,#45665,.F.);
#62022=ORIENTED_EDGE('',*,*,#45666,.T.);
#62023=ORIENTED_EDGE('',*,*,#45667,.F.);
#62024=ORIENTED_EDGE('',*,*,#45666,.F.);
#62025=ORIENTED_EDGE('',*,*,#45668,.T.);
#62026=ORIENTED_EDGE('',*,*,#45669,.T.);
#62027=ORIENTED_EDGE('',*,*,#45670,.T.);
#62028=ORIENTED_EDGE('',*,*,#45631,.T.);
#62029=ORIENTED_EDGE('',*,*,#45671,.T.);
#62030=ORIENTED_EDGE('',*,*,#45672,.T.);
#62031=ORIENTED_EDGE('',*,*,#45673,.T.);
#62032=ORIENTED_EDGE('',*,*,#45674,.T.);
#62033=ORIENTED_EDGE('',*,*,#45675,.F.);
#62034=ORIENTED_EDGE('',*,*,#45676,.T.);
#62035=ORIENTED_EDGE('',*,*,#45677,.F.);
#62036=ORIENTED_EDGE('',*,*,#45678,.F.);
#62037=ORIENTED_EDGE('',*,*,#45402,.F.);
#62038=ORIENTED_EDGE('',*,*,#45679,.T.);
#62039=ORIENTED_EDGE('',*,*,#45680,.F.);
#62040=ORIENTED_EDGE('',*,*,#45681,.F.);
#62041=ORIENTED_EDGE('',*,*,#45682,.F.);
#62042=ORIENTED_EDGE('',*,*,#45683,.T.);
#62043=ORIENTED_EDGE('',*,*,#45684,.F.);
#62044=ORIENTED_EDGE('',*,*,#45683,.F.);
#62045=ORIENTED_EDGE('',*,*,#45685,.T.);
#62046=ORIENTED_EDGE('',*,*,#45686,.T.);
#62047=ORIENTED_EDGE('',*,*,#45687,.F.);
#62048=ORIENTED_EDGE('',*,*,#45687,.T.);
#62049=ORIENTED_EDGE('',*,*,#45688,.T.);
#62050=ORIENTED_EDGE('',*,*,#45684,.T.);
#62051=ORIENTED_EDGE('',*,*,#45688,.F.);
#62052=ORIENTED_EDGE('',*,*,#45689,.F.);
#62053=ORIENTED_EDGE('',*,*,#45690,.T.);
#62054=ORIENTED_EDGE('',*,*,#45691,.F.);
#62055=ORIENTED_EDGE('',*,*,#45690,.F.);
#62056=ORIENTED_EDGE('',*,*,#45692,.T.);
#62057=ORIENTED_EDGE('',*,*,#45693,.T.);
#62058=ORIENTED_EDGE('',*,*,#45694,.F.);
#62059=ORIENTED_EDGE('',*,*,#45694,.T.);
#62060=ORIENTED_EDGE('',*,*,#45695,.T.);
#62061=ORIENTED_EDGE('',*,*,#45691,.T.);
#62062=ORIENTED_EDGE('',*,*,#45695,.F.);
#62063=ORIENTED_EDGE('',*,*,#45696,.T.);
#62064=ORIENTED_EDGE('',*,*,#45686,.F.);
#62065=ORIENTED_EDGE('',*,*,#45697,.T.);
#62066=ORIENTED_EDGE('',*,*,#45394,.T.);
#62067=ORIENTED_EDGE('',*,*,#45698,.T.);
#62068=ORIENTED_EDGE('',*,*,#45699,.F.);
#62069=ORIENTED_EDGE('',*,*,#45700,.F.);
#62070=ORIENTED_EDGE('',*,*,#45701,.T.);
#62071=ORIENTED_EDGE('',*,*,#45702,.F.);
#62072=ORIENTED_EDGE('',*,*,#45703,.F.);
#62073=ORIENTED_EDGE('',*,*,#45704,.T.);
#62074=ORIENTED_EDGE('',*,*,#45705,.F.);
#62075=ORIENTED_EDGE('',*,*,#45706,.F.);
#62076=ORIENTED_EDGE('',*,*,#45707,.T.);
#62077=ORIENTED_EDGE('',*,*,#45708,.F.);
#62078=ORIENTED_EDGE('',*,*,#45709,.F.);
#62079=ORIENTED_EDGE('',*,*,#45700,.T.);
#62080=ORIENTED_EDGE('',*,*,#45710,.F.);
#62081=ORIENTED_EDGE('',*,*,#45711,.T.);
#62082=ORIENTED_EDGE('',*,*,#45712,.F.);
#62083=ORIENTED_EDGE('',*,*,#45701,.F.);
#62084=ORIENTED_EDGE('',*,*,#45712,.T.);
#62085=ORIENTED_EDGE('',*,*,#45713,.T.);
#62086=ORIENTED_EDGE('',*,*,#45714,.T.);
#62087=ORIENTED_EDGE('',*,*,#45715,.F.);
#62088=ORIENTED_EDGE('',*,*,#45702,.T.);
#62089=ORIENTED_EDGE('',*,*,#45715,.T.);
#62090=ORIENTED_EDGE('',*,*,#45716,.T.);
#62091=ORIENTED_EDGE('',*,*,#45717,.F.);
#62092=ORIENTED_EDGE('',*,*,#45706,.T.);
#62093=ORIENTED_EDGE('',*,*,#45718,.F.);
#62094=ORIENTED_EDGE('',*,*,#45719,.T.);
#62095=ORIENTED_EDGE('',*,*,#45720,.F.);
#62096=ORIENTED_EDGE('',*,*,#45707,.F.);
#62097=ORIENTED_EDGE('',*,*,#45720,.T.);
#62098=ORIENTED_EDGE('',*,*,#45721,.T.);
#62099=ORIENTED_EDGE('',*,*,#45722,.T.);
#62100=ORIENTED_EDGE('',*,*,#45723,.F.);
#62101=ORIENTED_EDGE('',*,*,#45708,.T.);
#62102=ORIENTED_EDGE('',*,*,#45723,.T.);
#62103=ORIENTED_EDGE('',*,*,#45724,.T.);
#62104=ORIENTED_EDGE('',*,*,#45725,.F.);
#62105=ORIENTED_EDGE('',*,*,#45721,.F.);
#62106=ORIENTED_EDGE('',*,*,#45726,.T.);
#62107=ORIENTED_EDGE('',*,*,#45722,.F.);
#62108=ORIENTED_EDGE('',*,*,#45727,.T.);
#62109=ORIENTED_EDGE('',*,*,#45727,.F.);
#62110=ORIENTED_EDGE('',*,*,#45719,.F.);
#62111=ORIENTED_EDGE('',*,*,#45728,.F.);
#62112=ORIENTED_EDGE('',*,*,#45724,.F.);
#62113=ORIENTED_EDGE('',*,*,#45726,.F.);
#62114=ORIENTED_EDGE('',*,*,#45713,.F.);
#62115=ORIENTED_EDGE('',*,*,#45729,.T.);
#62116=ORIENTED_EDGE('',*,*,#45714,.F.);
#62117=ORIENTED_EDGE('',*,*,#45730,.T.);
#62118=ORIENTED_EDGE('',*,*,#45730,.F.);
#62119=ORIENTED_EDGE('',*,*,#45711,.F.);
#62120=ORIENTED_EDGE('',*,*,#45731,.F.);
#62121=ORIENTED_EDGE('',*,*,#45716,.F.);
#62122=ORIENTED_EDGE('',*,*,#45729,.F.);
#62123=ORIENTED_EDGE('',*,*,#45732,.T.);
#62124=ORIENTED_EDGE('',*,*,#45733,.F.);
#62125=ORIENTED_EDGE('',*,*,#45734,.F.);
#62126=ORIENTED_EDGE('',*,*,#45735,.T.);
#62127=ORIENTED_EDGE('',*,*,#45736,.T.);
#62128=ORIENTED_EDGE('',*,*,#45735,.F.);
#62129=ORIENTED_EDGE('',*,*,#45737,.F.);
#62130=ORIENTED_EDGE('',*,*,#45738,.T.);
#62131=ORIENTED_EDGE('',*,*,#45739,.T.);
#62132=ORIENTED_EDGE('',*,*,#45738,.F.);
#62133=ORIENTED_EDGE('',*,*,#45740,.F.);
#62134=ORIENTED_EDGE('',*,*,#45741,.F.);
#62135=ORIENTED_EDGE('',*,*,#45742,.F.);
#62136=ORIENTED_EDGE('',*,*,#45704,.F.);
#62137=ORIENTED_EDGE('',*,*,#45743,.F.);
#62138=ORIENTED_EDGE('',*,*,#45732,.F.);
#62139=ORIENTED_EDGE('',*,*,#45736,.F.);
#62140=ORIENTED_EDGE('',*,*,#45739,.F.);
#62141=ORIENTED_EDGE('',*,*,#45744,.T.);
#62142=ORIENTED_EDGE('',*,*,#45745,.F.);
#62143=ORIENTED_EDGE('',*,*,#45746,.F.);
#62144=ORIENTED_EDGE('',*,*,#45747,.T.);
#62145=ORIENTED_EDGE('',*,*,#45748,.T.);
#62146=ORIENTED_EDGE('',*,*,#45747,.F.);
#62147=ORIENTED_EDGE('',*,*,#45749,.F.);
#62148=ORIENTED_EDGE('',*,*,#45750,.T.);
#62149=ORIENTED_EDGE('',*,*,#45751,.T.);
#62150=ORIENTED_EDGE('',*,*,#45750,.F.);
#62151=ORIENTED_EDGE('',*,*,#45752,.F.);
#62152=ORIENTED_EDGE('',*,*,#45753,.F.);
#62153=ORIENTED_EDGE('',*,*,#45754,.F.);
#62154=ORIENTED_EDGE('',*,*,#45698,.F.);
#62155=ORIENTED_EDGE('',*,*,#45755,.F.);
#62156=ORIENTED_EDGE('',*,*,#45744,.F.);
#62157=ORIENTED_EDGE('',*,*,#45748,.F.);
#62158=ORIENTED_EDGE('',*,*,#45751,.F.);
#62159=ORIENTED_EDGE('',*,*,#45756,.F.);
#62160=ORIENTED_EDGE('',*,*,#45757,.T.);
#62161=ORIENTED_EDGE('',*,*,#45758,.T.);
#62162=ORIENTED_EDGE('',*,*,#45669,.F.);
#62163=ORIENTED_EDGE('',*,*,#45759,.F.);
#62164=ORIENTED_EDGE('',*,*,#45205,.F.);
#62165=ORIENTED_EDGE('',*,*,#45760,.T.);
#62166=ORIENTED_EDGE('',*,*,#45642,.F.);
#62167=ORIENTED_EDGE('',*,*,#45761,.T.);
#62168=ORIENTED_EDGE('',*,*,#45391,.F.);
#62169=ORIENTED_EDGE('',*,*,#45762,.F.);
#62170=ORIENTED_EDGE('',*,*,#45407,.T.);
#62171=ORIENTED_EDGE('',*,*,#45763,.T.);
#62172=ORIENTED_EDGE('',*,*,#45764,.F.);
#62173=ORIENTED_EDGE('',*,*,#45390,.F.);
#62174=ORIENTED_EDGE('',*,*,#45397,.T.);
#62175=ORIENTED_EDGE('',*,*,#45408,.T.);
#62176=ORIENTED_EDGE('',*,*,#45762,.T.);
#62177=ORIENTED_EDGE('',*,*,#45765,.F.);
#62178=ORIENTED_EDGE('',*,*,#45764,.T.);
#62179=ORIENTED_EDGE('',*,*,#45766,.F.);
#62180=ORIENTED_EDGE('',*,*,#45767,.F.);
#62181=ORIENTED_EDGE('',*,*,#45768,.T.);
#62182=ORIENTED_EDGE('',*,*,#45769,.T.);
#62183=ORIENTED_EDGE('',*,*,#45770,.F.);
#62184=ORIENTED_EDGE('',*,*,#45771,.T.);
#62185=ORIENTED_EDGE('',*,*,#45772,.F.);
#62186=ORIENTED_EDGE('',*,*,#45773,.T.);
#62187=ORIENTED_EDGE('',*,*,#45774,.T.);
#62188=ORIENTED_EDGE('',*,*,#45775,.F.);
#62189=ORIENTED_EDGE('',*,*,#45776,.F.);
#62190=ORIENTED_EDGE('',*,*,#45775,.T.);
#62191=ORIENTED_EDGE('',*,*,#45777,.T.);
#62192=ORIENTED_EDGE('',*,*,#45778,.T.);
#62193=ORIENTED_EDGE('',*,*,#45779,.T.);
#62194=ORIENTED_EDGE('',*,*,#45780,.F.);
#62195=ORIENTED_EDGE('',*,*,#45770,.T.);
#62196=ORIENTED_EDGE('',*,*,#45781,.T.);
#62197=ORIENTED_EDGE('',*,*,#45773,.F.);
#62198=ORIENTED_EDGE('',*,*,#45782,.F.);
#62199=ORIENTED_EDGE('',*,*,#45783,.F.);
#62200=ORIENTED_EDGE('',*,*,#45784,.F.);
#62201=ORIENTED_EDGE('',*,*,#45785,.F.);
#62202=ORIENTED_EDGE('',*,*,#45786,.T.);
#62203=ORIENTED_EDGE('',*,*,#45783,.T.);
#62204=ORIENTED_EDGE('',*,*,#45786,.F.);
#62205=ORIENTED_EDGE('',*,*,#45787,.T.);
#62206=ORIENTED_EDGE('',*,*,#45788,.F.);
#62207=ORIENTED_EDGE('',*,*,#45693,.F.);
#62208=ORIENTED_EDGE('',*,*,#45789,.T.);
#62209=ORIENTED_EDGE('',*,*,#45790,.T.);
#62210=ORIENTED_EDGE('',*,*,#45791,.F.);
#62211=ORIENTED_EDGE('',*,*,#45792,.F.);
#62212=ORIENTED_EDGE('',*,*,#45771,.F.);
#62213=ORIENTED_EDGE('',*,*,#45780,.T.);
#62214=ORIENTED_EDGE('',*,*,#45779,.F.);
#62215=ORIENTED_EDGE('',*,*,#45793,.T.);
#62216=ORIENTED_EDGE('',*,*,#45794,.T.);
#62217=ORIENTED_EDGE('',*,*,#45791,.T.);
#62218=ORIENTED_EDGE('',*,*,#45795,.F.);
#62219=ORIENTED_EDGE('',*,*,#45790,.F.);
#62220=ORIENTED_EDGE('',*,*,#45796,.F.);
#62221=ORIENTED_EDGE('',*,*,#45793,.F.);
#62222=ORIENTED_EDGE('',*,*,#45782,.T.);
#62223=ORIENTED_EDGE('',*,*,#45772,.T.);
#62224=ORIENTED_EDGE('',*,*,#45776,.T.);
#62225=ORIENTED_EDGE('',*,*,#45797,.T.);
#62226=ORIENTED_EDGE('',*,*,#45798,.F.);
#62227=ORIENTED_EDGE('',*,*,#45799,.T.);
#62228=ORIENTED_EDGE('',*,*,#45797,.F.);
#62229=ORIENTED_EDGE('',*,*,#45778,.F.);
#62230=ORIENTED_EDGE('',*,*,#45800,.F.);
#62231=ORIENTED_EDGE('',*,*,#45801,.F.);
#62232=ORIENTED_EDGE('',*,*,#45802,.F.);
#62233=ORIENTED_EDGE('',*,*,#45803,.T.);
#62234=ORIENTED_EDGE('',*,*,#45804,.T.);
#62235=ORIENTED_EDGE('',*,*,#45787,.F.);
#62236=ORIENTED_EDGE('',*,*,#45795,.T.);
#62237=ORIENTED_EDGE('',*,*,#45799,.F.);
#62238=ORIENTED_EDGE('',*,*,#45805,.T.);
#62239=ORIENTED_EDGE('',*,*,#45806,.F.);
#62240=ORIENTED_EDGE('',*,*,#45802,.T.);
#62241=ORIENTED_EDGE('',*,*,#45798,.T.);
#62242=ORIENTED_EDGE('',*,*,#45761,.F.);
#62243=ORIENTED_EDGE('',*,*,#45765,.T.);
#62244=ORIENTED_EDGE('',*,*,#45807,.T.);
#62245=ORIENTED_EDGE('',*,*,#45392,.T.);
#62246=ORIENTED_EDGE('',*,*,#45808,.F.);
#62247=ORIENTED_EDGE('',*,*,#45803,.F.);
#62248=ORIENTED_EDGE('',*,*,#45806,.T.);
#62249=ORIENTED_EDGE('',*,*,#45809,.F.);
#62250=ORIENTED_EDGE('',*,*,#45810,.F.);
#62251=ORIENTED_EDGE('',*,*,#45811,.F.);
#62252=ORIENTED_EDGE('',*,*,#45809,.T.);
#62253=ORIENTED_EDGE('',*,*,#45805,.F.);
#62254=ORIENTED_EDGE('',*,*,#45801,.T.);
#62255=ORIENTED_EDGE('',*,*,#45812,.T.);
#62256=ORIENTED_EDGE('',*,*,#45813,.F.);
#62257=ORIENTED_EDGE('',*,*,#45814,.F.);
#62258=ORIENTED_EDGE('',*,*,#45678,.T.);
#62259=ORIENTED_EDGE('',*,*,#45815,.F.);
#62260=ORIENTED_EDGE('',*,*,#45816,.T.);
#62261=ORIENTED_EDGE('',*,*,#45817,.T.);
#62262=ORIENTED_EDGE('',*,*,#45810,.T.);
#62263=ORIENTED_EDGE('',*,*,#45818,.T.);
#62264=ORIENTED_EDGE('',*,*,#45813,.T.);
#62265=ORIENTED_EDGE('',*,*,#45819,.F.);
#62266=ORIENTED_EDGE('',*,*,#45820,.F.);
#62267=ORIENTED_EDGE('',*,*,#45676,.F.);
#62268=ORIENTED_EDGE('',*,*,#45821,.F.);
#62269=ORIENTED_EDGE('',*,*,#45822,.F.);
#62270=ORIENTED_EDGE('',*,*,#45821,.T.);
#62271=ORIENTED_EDGE('',*,*,#45675,.T.);
#62272=ORIENTED_EDGE('',*,*,#45814,.T.);
#62273=ORIENTED_EDGE('',*,*,#45818,.F.);
#62274=ORIENTED_EDGE('',*,*,#45812,.F.);
#62275=ORIENTED_EDGE('',*,*,#45800,.T.);
#62276=ORIENTED_EDGE('',*,*,#45777,.F.);
#62277=ORIENTED_EDGE('',*,*,#45774,.F.);
#62278=ORIENTED_EDGE('',*,*,#45781,.F.);
#62279=ORIENTED_EDGE('',*,*,#45769,.F.);
#62280=ORIENTED_EDGE('',*,*,#45823,.T.);
#62281=ORIENTED_EDGE('',*,*,#45824,.T.);
#62282=ORIENTED_EDGE('',*,*,#45766,.T.);
#62283=ORIENTED_EDGE('',*,*,#45763,.F.);
#62284=ORIENTED_EDGE('',*,*,#45406,.F.);
#62285=ORIENTED_EDGE('',*,*,#45825,.F.);
#62286=ORIENTED_EDGE('',*,*,#45403,.F.);
#62287=ORIENTED_EDGE('',*,*,#45681,.T.);
#62288=ORIENTED_EDGE('',*,*,#45826,.F.);
#62289=ORIENTED_EDGE('',*,*,#45827,.T.);
#62290=ORIENTED_EDGE('',*,*,#45673,.F.);
#62291=ORIENTED_EDGE('',*,*,#45828,.F.);
#62292=ORIENTED_EDGE('',*,*,#45829,.F.);
#62293=ORIENTED_EDGE('',*,*,#45826,.T.);
#62294=ORIENTED_EDGE('',*,*,#45680,.T.);
#62295=ORIENTED_EDGE('',*,*,#45830,.T.);
#62296=ORIENTED_EDGE('',*,*,#45831,.F.);
#62297=ORIENTED_EDGE('',*,*,#45832,.F.);
#62298=ORIENTED_EDGE('',*,*,#45613,.T.);
#62299=ORIENTED_EDGE('',*,*,#45833,.F.);
#62300=ORIENTED_EDGE('',*,*,#45830,.F.);
#62301=ORIENTED_EDGE('',*,*,#45679,.F.);
#62302=ORIENTED_EDGE('',*,*,#45401,.F.);
#62303=ORIENTED_EDGE('',*,*,#45834,.F.);
#62304=ORIENTED_EDGE('',*,*,#45835,.F.);
#62305=ORIENTED_EDGE('',*,*,#45671,.F.);
#62306=ORIENTED_EDGE('',*,*,#45836,.F.);
#62307=ORIENTED_EDGE('',*,*,#45757,.F.);
#62308=ORIENTED_EDGE('',*,*,#45837,.F.);
#62309=ORIENTED_EDGE('',*,*,#45816,.F.);
#62310=ORIENTED_EDGE('',*,*,#45815,.T.);
#62311=ORIENTED_EDGE('',*,*,#45677,.T.);
#62312=ORIENTED_EDGE('',*,*,#45820,.T.);
#62313=ORIENTED_EDGE('',*,*,#45834,.T.);
#62314=ORIENTED_EDGE('',*,*,#45819,.T.);
#62315=ORIENTED_EDGE('',*,*,#45822,.T.);
#62316=ORIENTED_EDGE('',*,*,#45838,.T.);
#62317=ORIENTED_EDGE('',*,*,#45829,.T.);
#62318=ORIENTED_EDGE('',*,*,#45839,.T.);
#62319=ORIENTED_EDGE('',*,*,#45404,.T.);
#62320=ORIENTED_EDGE('',*,*,#45825,.T.);
#62321=ORIENTED_EDGE('',*,*,#45831,.T.);
#62322=ORIENTED_EDGE('',*,*,#45833,.T.);
#62323=ORIENTED_EDGE('',*,*,#45400,.T.);
#62324=ORIENTED_EDGE('',*,*,#45840,.T.);
#62325=ORIENTED_EDGE('',*,*,#45832,.T.);
#62326=ORIENTED_EDGE('',*,*,#45840,.F.);
#62327=ORIENTED_EDGE('',*,*,#45399,.T.);
#62328=ORIENTED_EDGE('',*,*,#45586,.F.);
#62329=ORIENTED_EDGE('',*,*,#45587,.T.);
#62330=ORIENTED_EDGE('',*,*,#45387,.F.);
#62331=ORIENTED_EDGE('',*,*,#45395,.T.);
#62332=ORIENTED_EDGE('',*,*,#45697,.F.);
#62333=ORIENTED_EDGE('',*,*,#45685,.F.);
#62334=ORIENTED_EDGE('',*,*,#45696,.F.);
#62335=ORIENTED_EDGE('',*,*,#45393,.T.);
#62336=ORIENTED_EDGE('',*,*,#45807,.F.);
#62337=ORIENTED_EDGE('',*,*,#45767,.T.);
#62338=ORIENTED_EDGE('',*,*,#45824,.F.);
#62339=ORIENTED_EDGE('',*,*,#45405,.T.);
#62340=ORIENTED_EDGE('',*,*,#45839,.F.);
#62341=ORIENTED_EDGE('',*,*,#45828,.T.);
#62342=ORIENTED_EDGE('',*,*,#45672,.F.);
#62343=ORIENTED_EDGE('',*,*,#45835,.T.);
#62344=ORIENTED_EDGE('',*,*,#45838,.F.);
#62345=ORIENTED_EDGE('',*,*,#45823,.F.);
#62346=ORIENTED_EDGE('',*,*,#45768,.F.);
#62347=ORIENTED_EDGE('',*,*,#45792,.T.);
#62348=ORIENTED_EDGE('',*,*,#45794,.F.);
#62349=ORIENTED_EDGE('',*,*,#45796,.T.);
#62350=ORIENTED_EDGE('',*,*,#45789,.F.);
#62351=ORIENTED_EDGE('',*,*,#45692,.F.);
#62352=ORIENTED_EDGE('',*,*,#45788,.T.);
#62353=ORIENTED_EDGE('',*,*,#45804,.F.);
#62354=ORIENTED_EDGE('',*,*,#45808,.T.);
#62355=ORIENTED_EDGE('',*,*,#45811,.T.);
#62356=ORIENTED_EDGE('',*,*,#45817,.F.);
#62357=ORIENTED_EDGE('',*,*,#45837,.T.);
#62358=ORIENTED_EDGE('',*,*,#45756,.T.);
#62359=ORIENTED_EDGE('',*,*,#45668,.F.);
#62360=ORIENTED_EDGE('',*,*,#45630,.T.);
#62361=ORIENTED_EDGE('',*,*,#45663,.T.);
#62362=ORIENTED_EDGE('',*,*,#45659,.F.);
#62363=ORIENTED_EDGE('',*,*,#45841,.T.);
#62364=ORIENTED_EDGE('',*,*,#45619,.T.);
#62365=ORIENTED_EDGE('',*,*,#45615,.T.);
#62366=ORIENTED_EDGE('',*,*,#45606,.F.);
#62367=ORIENTED_EDGE('',*,*,#45593,.T.);
#62368=ORIENTED_EDGE('',*,*,#45590,.F.);
#62369=ORIENTED_EDGE('',*,*,#45601,.T.);
#62370=ORIENTED_EDGE('',*,*,#45611,.F.);
#62371=ORIENTED_EDGE('',*,*,#45614,.T.);
#62372=ORIENTED_EDGE('',*,*,#45623,.T.);
#62373=ORIENTED_EDGE('',*,*,#45842,.T.);
#62374=ORIENTED_EDGE('',*,*,#45740,.T.);
#62375=ORIENTED_EDGE('',*,*,#45737,.T.);
#62376=ORIENTED_EDGE('',*,*,#45734,.T.);
#62377=ORIENTED_EDGE('',*,*,#45843,.T.);
#62378=ORIENTED_EDGE('',*,*,#45752,.T.);
#62379=ORIENTED_EDGE('',*,*,#45749,.T.);
#62380=ORIENTED_EDGE('',*,*,#45746,.T.);
#62381=ORIENTED_EDGE('',*,*,#45844,.F.);
#62382=ORIENTED_EDGE('',*,*,#45620,.T.);
#62383=ORIENTED_EDGE('',*,*,#45841,.F.);
#62384=ORIENTED_EDGE('',*,*,#45662,.F.);
#62385=ORIENTED_EDGE('',*,*,#45845,.F.);
#62386=ORIENTED_EDGE('',*,*,#45657,.F.);
#62387=ORIENTED_EDGE('',*,*,#45689,.T.);
#62388=ORIENTED_EDGE('',*,*,#45682,.T.);
#62389=ORIENTED_EDGE('',*,*,#45785,.T.);
#62390=ORIENTED_EDGE('',*,*,#45846,.T.);
#62391=ORIENTED_EDGE('',*,*,#45847,.T.);
#62392=ORIENTED_EDGE('',*,*,#45848,.T.);
#62393=ORIENTED_EDGE('',*,*,#45849,.T.);
#62394=ORIENTED_EDGE('',*,*,#45850,.T.);
#62395=ORIENTED_EDGE('',*,*,#45851,.T.);
#62396=ORIENTED_EDGE('',*,*,#45852,.T.);
#62397=ORIENTED_EDGE('',*,*,#45056,.T.);
#62398=ORIENTED_EDGE('',*,*,#45853,.T.);
#62399=ORIENTED_EDGE('',*,*,#45854,.T.);
#62400=ORIENTED_EDGE('',*,*,#45855,.F.);
#62401=ORIENTED_EDGE('',*,*,#45856,.T.);
#62402=ORIENTED_EDGE('',*,*,#45106,.F.);
#62403=ORIENTED_EDGE('',*,*,#45857,.F.);
#62404=ORIENTED_EDGE('',*,*,#45858,.T.);
#62405=ORIENTED_EDGE('',*,*,#45859,.F.);
#62406=ORIENTED_EDGE('',*,*,#45860,.F.);
#62407=ORIENTED_EDGE('',*,*,#45861,.F.);
#62408=ORIENTED_EDGE('',*,*,#45143,.T.);
#62409=ORIENTED_EDGE('',*,*,#45862,.F.);
#62410=ORIENTED_EDGE('',*,*,#45849,.F.);
#62411=ORIENTED_EDGE('',*,*,#45863,.F.);
#62412=ORIENTED_EDGE('',*,*,#45851,.F.);
#62413=ORIENTED_EDGE('',*,*,#45864,.F.);
#62414=ORIENTED_EDGE('',*,*,#45856,.F.);
#62415=ORIENTED_EDGE('',*,*,#45865,.T.);
#62416=ORIENTED_EDGE('',*,*,#45089,.F.);
#62417=ORIENTED_EDGE('',*,*,#45095,.F.);
#62418=ORIENTED_EDGE('',*,*,#45107,.T.);
#62419=ORIENTED_EDGE('',*,*,#45866,.F.);
#62420=ORIENTED_EDGE('',*,*,#45867,.F.);
#62421=ORIENTED_EDGE('',*,*,#45868,.F.);
#62422=ORIENTED_EDGE('',*,*,#45054,.T.);
#62423=ORIENTED_EDGE('',*,*,#45869,.F.);
#62424=ORIENTED_EDGE('',*,*,#45870,.F.);
#62425=ORIENTED_EDGE('',*,*,#45871,.T.);
#62426=ORIENTED_EDGE('',*,*,#45872,.T.);
#62427=ORIENTED_EDGE('',*,*,#45873,.T.);
#62428=ORIENTED_EDGE('',*,*,#45873,.F.);
#62429=ORIENTED_EDGE('',*,*,#45874,.F.);
#62430=ORIENTED_EDGE('',*,*,#45875,.F.);
#62431=ORIENTED_EDGE('',*,*,#45876,.T.);
#62432=ORIENTED_EDGE('',*,*,#45877,.T.);
#62433=ORIENTED_EDGE('',*,*,#45878,.T.);
#62434=ORIENTED_EDGE('',*,*,#45879,.T.);
#62435=ORIENTED_EDGE('',*,*,#45880,.F.);
#62436=ORIENTED_EDGE('',*,*,#45058,.T.);
#62437=ORIENTED_EDGE('',*,*,#45881,.T.);
#62438=ORIENTED_EDGE('',*,*,#45882,.T.);
#62439=ORIENTED_EDGE('',*,*,#45871,.F.);
#62440=ORIENTED_EDGE('',*,*,#45883,.T.);
#62441=ORIENTED_EDGE('',*,*,#45884,.T.);
#62442=ORIENTED_EDGE('',*,*,#45885,.T.);
#62443=ORIENTED_EDGE('',*,*,#45882,.F.);
#62444=ORIENTED_EDGE('',*,*,#45886,.F.);
#62445=ORIENTED_EDGE('',*,*,#45887,.T.);
#62446=ORIENTED_EDGE('',*,*,#45888,.T.);
#62447=ORIENTED_EDGE('',*,*,#45889,.T.);
#62448=ORIENTED_EDGE('',*,*,#45888,.F.);
#62449=ORIENTED_EDGE('',*,*,#45889,.F.);
#62450=ORIENTED_EDGE('',*,*,#45890,.F.);
#62451=ORIENTED_EDGE('',*,*,#45887,.F.);
#62452=ORIENTED_EDGE('',*,*,#45891,.T.);
#62453=ORIENTED_EDGE('',*,*,#45892,.T.);
#62454=ORIENTED_EDGE('',*,*,#45891,.F.);
#62455=ORIENTED_EDGE('',*,*,#45890,.T.);
#62456=ORIENTED_EDGE('',*,*,#45893,.T.);
#62457=ORIENTED_EDGE('',*,*,#45894,.T.);
#62458=ORIENTED_EDGE('',*,*,#45893,.F.);
#62459=ORIENTED_EDGE('',*,*,#45895,.F.);
#62460=ORIENTED_EDGE('',*,*,#45896,.T.);
#62461=ORIENTED_EDGE('',*,*,#45897,.T.);
#62462=ORIENTED_EDGE('',*,*,#45896,.F.);
#62463=ORIENTED_EDGE('',*,*,#45865,.F.);
#62464=ORIENTED_EDGE('',*,*,#45855,.T.);
#62465=ORIENTED_EDGE('',*,*,#45898,.T.);
#62466=ORIENTED_EDGE('',*,*,#45090,.T.);
#62467=ORIENTED_EDGE('',*,*,#45899,.T.);
#62468=ORIENTED_EDGE('',*,*,#45900,.T.);
#62469=ORIENTED_EDGE('',*,*,#45901,.F.);
#62470=ORIENTED_EDGE('',*,*,#45900,.F.);
#62471=ORIENTED_EDGE('',*,*,#45123,.F.);
#62472=ORIENTED_EDGE('',*,*,#45902,.T.);
#62473=ORIENTED_EDGE('',*,*,#45903,.T.);
#62474=ORIENTED_EDGE('',*,*,#45146,.T.);
#62475=ORIENTED_EDGE('',*,*,#45904,.T.);
#62476=ORIENTED_EDGE('',*,*,#45905,.T.);
#62477=ORIENTED_EDGE('',*,*,#45906,.T.);
#62478=ORIENTED_EDGE('',*,*,#45905,.F.);
#62479=ORIENTED_EDGE('',*,*,#45906,.F.);
#62480=ORIENTED_EDGE('',*,*,#45907,.T.);
#62481=ORIENTED_EDGE('',*,*,#45908,.T.);
#62482=ORIENTED_EDGE('',*,*,#45907,.F.);
#62483=ORIENTED_EDGE('',*,*,#45909,.T.);
#62484=ORIENTED_EDGE('',*,*,#45910,.T.);
#62485=ORIENTED_EDGE('',*,*,#45911,.T.);
#62486=ORIENTED_EDGE('',*,*,#45912,.T.);
#62487=ORIENTED_EDGE('',*,*,#45913,.F.);
#62488=ORIENTED_EDGE('',*,*,#45914,.F.);
#62489=ORIENTED_EDGE('',*,*,#45915,.F.);
#62490=ORIENTED_EDGE('',*,*,#45916,.F.);
#62491=ORIENTED_EDGE('',*,*,#45917,.T.);
#62492=ORIENTED_EDGE('',*,*,#45918,.T.);
#62493=ORIENTED_EDGE('',*,*,#45913,.T.);
#62494=ORIENTED_EDGE('',*,*,#45919,.T.);
#62495=ORIENTED_EDGE('',*,*,#45102,.T.);
#62496=ORIENTED_EDGE('',*,*,#44959,.T.);
#62497=ORIENTED_EDGE('',*,*,#45920,.T.);
#62498=ORIENTED_EDGE('',*,*,#45921,.T.);
#62499=ORIENTED_EDGE('',*,*,#45920,.F.);
#62500=ORIENTED_EDGE('',*,*,#44958,.F.);
#62501=ORIENTED_EDGE('',*,*,#45922,.F.);
#62502=ORIENTED_EDGE('',*,*,#45923,.F.);
#62503=ORIENTED_EDGE('',*,*,#45924,.F.);
#62504=ORIENTED_EDGE('',*,*,#45922,.T.);
#62505=ORIENTED_EDGE('',*,*,#44957,.F.);
#62506=ORIENTED_EDGE('',*,*,#45925,.F.);
#62507=ORIENTED_EDGE('',*,*,#45011,.F.);
#62508=ORIENTED_EDGE('',*,*,#45926,.F.);
#62509=ORIENTED_EDGE('',*,*,#45927,.T.);
#62510=ORIENTED_EDGE('',*,*,#45928,.T.);
#62511=ORIENTED_EDGE('',*,*,#45929,.F.);
#62512=ORIENTED_EDGE('',*,*,#45930,.F.);
#62513=ORIENTED_EDGE('',*,*,#45931,.T.);
#62514=ORIENTED_EDGE('',*,*,#45932,.F.);
#62515=ORIENTED_EDGE('',*,*,#45933,.T.);
#62516=ORIENTED_EDGE('',*,*,#45934,.F.);
#62517=ORIENTED_EDGE('',*,*,#45933,.F.);
#62518=ORIENTED_EDGE('',*,*,#45014,.F.);
#62519=ORIENTED_EDGE('',*,*,#45935,.F.);
#62520=ORIENTED_EDGE('',*,*,#45936,.F.);
#62521=ORIENTED_EDGE('',*,*,#45926,.T.);
#62522=ORIENTED_EDGE('',*,*,#45016,.F.);
#62523=ORIENTED_EDGE('',*,*,#45031,.T.);
#62524=ORIENTED_EDGE('',*,*,#45937,.F.);
#62525=ORIENTED_EDGE('',*,*,#45938,.T.);
#62526=ORIENTED_EDGE('',*,*,#45939,.T.);
#62527=ORIENTED_EDGE('',*,*,#45935,.T.);
#62528=ORIENTED_EDGE('',*,*,#45486,.F.);
#62529=ORIENTED_EDGE('',*,*,#45457,.T.);
#62530=ORIENTED_EDGE('',*,*,#45940,.T.);
#62531=ORIENTED_EDGE('',*,*,#45941,.T.);
#62532=ORIENTED_EDGE('',*,*,#45942,.F.);
#62533=ORIENTED_EDGE('',*,*,#45943,.T.);
#62534=ORIENTED_EDGE('',*,*,#45930,.T.);
#62535=ORIENTED_EDGE('',*,*,#45937,.T.);
#62536=ORIENTED_EDGE('',*,*,#45030,.T.);
#62537=ORIENTED_EDGE('',*,*,#45944,.T.);
#62538=ORIENTED_EDGE('',*,*,#45945,.T.);
#62539=ORIENTED_EDGE('',*,*,#45946,.F.);
#62540=ORIENTED_EDGE('',*,*,#45491,.F.);
#62541=ORIENTED_EDGE('',*,*,#45508,.T.);
#62542=ORIENTED_EDGE('',*,*,#45947,.T.);
#62543=ORIENTED_EDGE('',*,*,#45459,.T.);
#62544=ORIENTED_EDGE('',*,*,#45449,.T.);
#62545=ORIENTED_EDGE('',*,*,#45948,.T.);
#62546=ORIENTED_EDGE('',*,*,#45949,.F.);
#62547=ORIENTED_EDGE('',*,*,#45950,.T.);
#62548=ORIENTED_EDGE('',*,*,#45948,.F.);
#62549=ORIENTED_EDGE('',*,*,#45951,.T.);
#62550=ORIENTED_EDGE('',*,*,#45952,.T.);
#62551=ORIENTED_EDGE('',*,*,#45951,.F.);
#62552=ORIENTED_EDGE('',*,*,#45950,.F.);
#62553=ORIENTED_EDGE('',*,*,#45953,.T.);
#62554=ORIENTED_EDGE('',*,*,#45954,.T.);
#62555=ORIENTED_EDGE('',*,*,#45953,.F.);
#62556=ORIENTED_EDGE('',*,*,#45952,.F.);
#62557=ORIENTED_EDGE('',*,*,#45954,.F.);
#62558=ORIENTED_EDGE('',*,*,#45955,.T.);
#62559=ORIENTED_EDGE('',*,*,#45956,.T.);
#62560=ORIENTED_EDGE('',*,*,#45944,.F.);
#62561=ORIENTED_EDGE('',*,*,#45033,.T.);
#62562=ORIENTED_EDGE('',*,*,#45957,.T.);
#62563=ORIENTED_EDGE('',*,*,#45958,.F.);
#62564=ORIENTED_EDGE('',*,*,#45912,.F.);
#62565=ORIENTED_EDGE('',*,*,#45959,.T.);
#62566=ORIENTED_EDGE('',*,*,#45915,.T.);
#62567=ORIENTED_EDGE('',*,*,#45960,.F.);
#62568=ORIENTED_EDGE('',*,*,#45961,.T.);
#62569=ORIENTED_EDGE('',*,*,#45093,.F.);
#62570=ORIENTED_EDGE('',*,*,#45961,.F.);
#62571=ORIENTED_EDGE('',*,*,#45908,.F.);
#62572=ORIENTED_EDGE('',*,*,#45960,.T.);
#62573=ORIENTED_EDGE('',*,*,#45934,.T.);
#62574=ORIENTED_EDGE('',*,*,#45962,.T.);
#62575=ORIENTED_EDGE('',*,*,#45892,.F.);
#62576=ORIENTED_EDGE('',*,*,#45962,.F.);
#62577=ORIENTED_EDGE('',*,*,#45963,.F.);
#62578=ORIENTED_EDGE('',*,*,#45964,.F.);
#62579=ORIENTED_EDGE('',*,*,#45965,.T.);
#62580=ORIENTED_EDGE('',*,*,#45966,.T.);
#62581=ORIENTED_EDGE('',*,*,#45964,.T.);
#62582=ORIENTED_EDGE('',*,*,#45966,.F.);
#62583=ORIENTED_EDGE('',*,*,#45967,.T.);
#62584=ORIENTED_EDGE('',*,*,#45092,.T.);
#62585=ORIENTED_EDGE('',*,*,#45968,.T.);
#62586=ORIENTED_EDGE('',*,*,#45969,.T.);
#62587=ORIENTED_EDGE('',*,*,#45067,.T.);
#62588=ORIENTED_EDGE('',*,*,#45970,.T.);
#62589=ORIENTED_EDGE('',*,*,#45869,.T.);
#62590=ORIENTED_EDGE('',*,*,#45053,.T.);
#62591=ORIENTED_EDGE('',*,*,#45065,.T.);
#62592=ORIENTED_EDGE('',*,*,#45070,.T.);
#62593=ORIENTED_EDGE('',*,*,#45971,.T.);
#62594=ORIENTED_EDGE('',*,*,#45972,.T.);
#62595=ORIENTED_EDGE('',*,*,#45973,.T.);
#62596=ORIENTED_EDGE('',*,*,#45862,.T.);
#62597=ORIENTED_EDGE('',*,*,#45142,.T.);
#62598=ORIENTED_EDGE('',*,*,#45147,.T.);
#62599=ORIENTED_EDGE('',*,*,#45903,.F.);
#62600=ORIENTED_EDGE('',*,*,#45974,.T.);
#62601=ORIENTED_EDGE('',*,*,#45897,.F.);
#62602=ORIENTED_EDGE('',*,*,#45899,.F.);
#62603=ORIENTED_EDGE('',*,*,#45894,.F.);
#62604=ORIENTED_EDGE('',*,*,#45975,.T.);
#62605=ORIENTED_EDGE('',*,*,#45963,.T.);
#62606=ORIENTED_EDGE('',*,*,#45975,.F.);
#62607=ORIENTED_EDGE('',*,*,#45976,.F.);
#62608=ORIENTED_EDGE('',*,*,#45977,.F.);
#62609=ORIENTED_EDGE('',*,*,#45877,.F.);
#62610=ORIENTED_EDGE('',*,*,#45978,.F.);
#62611=ORIENTED_EDGE('',*,*,#45080,.F.);
#62612=ORIENTED_EDGE('',*,*,#45979,.F.);
#62613=ORIENTED_EDGE('',*,*,#45068,.F.);
#62614=ORIENTED_EDGE('',*,*,#45969,.F.);
#62615=ORIENTED_EDGE('',*,*,#45870,.T.);
#62616=ORIENTED_EDGE('',*,*,#45879,.F.);
#62617=ORIENTED_EDGE('',*,*,#45980,.F.);
#62618=ORIENTED_EDGE('',*,*,#45117,.T.);
#62619=ORIENTED_EDGE('',*,*,#45981,.F.);
#62620=ORIENTED_EDGE('',*,*,#45061,.F.);
#62621=ORIENTED_EDGE('',*,*,#45982,.F.);
#62622=ORIENTED_EDGE('',*,*,#45883,.F.);
#62623=ORIENTED_EDGE('',*,*,#45062,.F.);
#62624=ORIENTED_EDGE('',*,*,#45981,.T.);
#62625=ORIENTED_EDGE('',*,*,#45983,.T.);
#62626=ORIENTED_EDGE('',*,*,#45060,.F.);
#62627=ORIENTED_EDGE('',*,*,#45984,.T.);
#62628=ORIENTED_EDGE('',*,*,#45884,.F.);
#62629=ORIENTED_EDGE('',*,*,#45982,.T.);
#62630=ORIENTED_EDGE('',*,*,#45880,.T.);
#62631=ORIENTED_EDGE('',*,*,#45885,.F.);
#62632=ORIENTED_EDGE('',*,*,#45984,.F.);
#62633=ORIENTED_EDGE('',*,*,#45059,.F.);
#62634=ORIENTED_EDGE('',*,*,#45985,.F.);
#62635=ORIENTED_EDGE('',*,*,#45986,.T.);
#62636=ORIENTED_EDGE('',*,*,#45875,.T.);
#62637=ORIENTED_EDGE('',*,*,#45987,.F.);
#62638=ORIENTED_EDGE('',*,*,#45988,.F.);
#62639=ORIENTED_EDGE('',*,*,#45989,.F.);
#62640=ORIENTED_EDGE('',*,*,#45985,.T.);
#62641=ORIENTED_EDGE('',*,*,#45990,.F.);
#62642=ORIENTED_EDGE('',*,*,#45097,.T.);
#62643=ORIENTED_EDGE('',*,*,#45991,.F.);
#62644=ORIENTED_EDGE('',*,*,#45992,.F.);
#62645=ORIENTED_EDGE('',*,*,#45993,.T.);
#62646=ORIENTED_EDGE('',*,*,#45994,.F.);
#62647=ORIENTED_EDGE('',*,*,#45995,.F.);
#62648=ORIENTED_EDGE('',*,*,#45996,.T.);
#62649=ORIENTED_EDGE('',*,*,#45997,.F.);
#62650=ORIENTED_EDGE('',*,*,#45998,.F.);
#62651=ORIENTED_EDGE('',*,*,#45999,.F.);
#62652=ORIENTED_EDGE('',*,*,#45997,.T.);
#62653=ORIENTED_EDGE('',*,*,#46000,.T.);
#62654=ORIENTED_EDGE('',*,*,#45992,.T.);
#62655=ORIENTED_EDGE('',*,*,#46001,.F.);
#62656=ORIENTED_EDGE('',*,*,#45137,.T.);
#62657=ORIENTED_EDGE('',*,*,#45145,.F.);
#62658=ORIENTED_EDGE('',*,*,#46002,.T.);
#62659=ORIENTED_EDGE('',*,*,#46003,.F.);
#62660=ORIENTED_EDGE('',*,*,#46004,.F.);
#62661=ORIENTED_EDGE('',*,*,#46005,.F.);
#62662=ORIENTED_EDGE('',*,*,#46002,.F.);
#62663=ORIENTED_EDGE('',*,*,#45144,.T.);
#62664=ORIENTED_EDGE('',*,*,#45861,.T.);
#62665=ORIENTED_EDGE('',*,*,#46006,.T.);
#62666=ORIENTED_EDGE('',*,*,#45858,.F.);
#62667=ORIENTED_EDGE('',*,*,#46007,.F.);
#62668=ORIENTED_EDGE('',*,*,#46008,.F.);
#62669=ORIENTED_EDGE('',*,*,#46007,.T.);
#62670=ORIENTED_EDGE('',*,*,#45857,.T.);
#62671=ORIENTED_EDGE('',*,*,#45105,.T.);
#62672=ORIENTED_EDGE('',*,*,#46009,.F.);
#62673=ORIENTED_EDGE('',*,*,#46001,.T.);
#62674=ORIENTED_EDGE('',*,*,#46010,.F.);
#62675=ORIENTED_EDGE('',*,*,#46009,.T.);
#62676=ORIENTED_EDGE('',*,*,#45994,.T.);
#62677=ORIENTED_EDGE('',*,*,#46011,.T.);
#62678=ORIENTED_EDGE('',*,*,#45138,.T.);
#62679=ORIENTED_EDGE('',*,*,#46012,.F.);
#62680=ORIENTED_EDGE('',*,*,#46008,.T.);
#62681=ORIENTED_EDGE('',*,*,#46013,.F.);
#62682=ORIENTED_EDGE('',*,*,#46010,.T.);
#62683=ORIENTED_EDGE('',*,*,#46005,.T.);
#62684=ORIENTED_EDGE('',*,*,#46014,.F.);
#62685=ORIENTED_EDGE('',*,*,#45991,.T.);
#62686=ORIENTED_EDGE('',*,*,#46015,.F.);
#62687=ORIENTED_EDGE('',*,*,#45999,.T.);
#62688=ORIENTED_EDGE('',*,*,#46014,.T.);
#62689=ORIENTED_EDGE('',*,*,#46004,.T.);
#62690=ORIENTED_EDGE('',*,*,#46012,.T.);
#62691=ORIENTED_EDGE('',*,*,#45998,.T.);
#62692=ORIENTED_EDGE('',*,*,#46015,.T.);
#62693=ORIENTED_EDGE('',*,*,#46003,.T.);
#62694=ORIENTED_EDGE('',*,*,#46013,.T.);
#62695=ORIENTED_EDGE('',*,*,#45104,.T.);
#62696=ORIENTED_EDGE('',*,*,#46016,.T.);
#62697=ORIENTED_EDGE('',*,*,#45995,.T.);
#62698=ORIENTED_EDGE('',*,*,#46017,.F.);
#62699=ORIENTED_EDGE('',*,*,#45972,.F.);
#62700=ORIENTED_EDGE('',*,*,#46018,.T.);
#62701=ORIENTED_EDGE('',*,*,#45976,.T.);
#62702=ORIENTED_EDGE('',*,*,#45968,.F.);
#62703=ORIENTED_EDGE('',*,*,#45091,.T.);
#62704=ORIENTED_EDGE('',*,*,#45898,.F.);
#62705=ORIENTED_EDGE('',*,*,#45854,.F.);
#62706=ORIENTED_EDGE('',*,*,#46019,.F.);
#62707=ORIENTED_EDGE('',*,*,#46020,.F.);
#62708=ORIENTED_EDGE('',*,*,#45866,.T.);
#62709=ORIENTED_EDGE('',*,*,#45970,.F.);
#62710=ORIENTED_EDGE('',*,*,#46017,.T.);
#62711=ORIENTED_EDGE('',*,*,#45126,.F.);
#62712=ORIENTED_EDGE('',*,*,#46021,.F.);
#62713=ORIENTED_EDGE('',*,*,#46022,.F.);
#62714=ORIENTED_EDGE('',*,*,#45847,.F.);
#62715=ORIENTED_EDGE('',*,*,#46023,.F.);
#62716=ORIENTED_EDGE('',*,*,#46024,.F.);
#62717=ORIENTED_EDGE('',*,*,#45974,.F.);
#62718=ORIENTED_EDGE('',*,*,#45902,.F.);
#62719=ORIENTED_EDGE('',*,*,#46025,.T.);
#62720=ORIENTED_EDGE('',*,*,#46023,.T.);
#62721=ORIENTED_EDGE('',*,*,#45846,.F.);
#62722=ORIENTED_EDGE('',*,*,#45864,.T.);
#62723=ORIENTED_EDGE('',*,*,#45850,.F.);
#62724=ORIENTED_EDGE('',*,*,#45055,.T.);
#62725=ORIENTED_EDGE('',*,*,#45868,.T.);
#62726=ORIENTED_EDGE('',*,*,#45867,.T.);
#62727=ORIENTED_EDGE('',*,*,#46020,.T.);
#62728=ORIENTED_EDGE('',*,*,#46019,.T.);
#62729=ORIENTED_EDGE('',*,*,#45853,.F.);
#62730=ORIENTED_EDGE('',*,*,#46006,.F.);
#62731=ORIENTED_EDGE('',*,*,#45860,.T.);
#62732=ORIENTED_EDGE('',*,*,#45973,.F.);
#62733=ORIENTED_EDGE('',*,*,#46024,.T.);
#62734=ORIENTED_EDGE('',*,*,#46025,.F.);
#62735=ORIENTED_EDGE('',*,*,#45859,.T.);
#62736=ORIENTED_EDGE('',*,*,#46026,.F.);
#62737=ORIENTED_EDGE('',*,*,#45988,.T.);
#62738=ORIENTED_EDGE('',*,*,#46027,.F.);
#62739=ORIENTED_EDGE('',*,*,#46028,.T.);
#62740=ORIENTED_EDGE('',*,*,#45082,.F.);
#62741=ORIENTED_EDGE('',*,*,#46029,.T.);
#62742=ORIENTED_EDGE('',*,*,#46027,.T.);
#62743=ORIENTED_EDGE('',*,*,#45096,.T.);
#62744=ORIENTED_EDGE('',*,*,#45270,.F.);
#62745=ORIENTED_EDGE('',*,*,#46030,.F.);
#62746=ORIENTED_EDGE('',*,*,#46031,.F.);
#62747=ORIENTED_EDGE('',*,*,#46032,.F.);
#62748=ORIENTED_EDGE('',*,*,#45267,.F.);
#62749=ORIENTED_EDGE('',*,*,#46032,.T.);
#62750=ORIENTED_EDGE('',*,*,#46033,.T.);
#62751=ORIENTED_EDGE('',*,*,#45309,.T.);
#62752=ORIENTED_EDGE('',*,*,#45273,.F.);
#62753=ORIENTED_EDGE('',*,*,#46034,.F.);
#62754=ORIENTED_EDGE('',*,*,#46035,.F.);
#62755=ORIENTED_EDGE('',*,*,#46030,.T.);
#62756=ORIENTED_EDGE('',*,*,#45129,.F.);
#62757=ORIENTED_EDGE('',*,*,#45140,.T.);
#62758=ORIENTED_EDGE('',*,*,#46036,.T.);
#62759=ORIENTED_EDGE('',*,*,#46021,.T.);
#62760=ORIENTED_EDGE('',*,*,#46037,.F.);
#62761=ORIENTED_EDGE('',*,*,#46038,.F.);
#62762=ORIENTED_EDGE('',*,*,#46039,.F.);
#62763=ORIENTED_EDGE('',*,*,#46040,.T.);
#62764=ORIENTED_EDGE('',*,*,#45925,.T.);
#62765=ORIENTED_EDGE('',*,*,#44956,.F.);
#62766=ORIENTED_EDGE('',*,*,#45932,.T.);
#62767=ORIENTED_EDGE('',*,*,#46041,.F.);
#62768=ORIENTED_EDGE('',*,*,#46042,.T.);
#62769=ORIENTED_EDGE('',*,*,#46043,.T.);
#62770=ORIENTED_EDGE('',*,*,#46039,.T.);
#62771=ORIENTED_EDGE('',*,*,#46044,.F.);
#62772=ORIENTED_EDGE('',*,*,#46045,.T.);
#62773=ORIENTED_EDGE('',*,*,#46046,.T.);
#62774=ORIENTED_EDGE('',*,*,#46047,.T.);
#62775=ORIENTED_EDGE('',*,*,#46048,.F.);
#62776=ORIENTED_EDGE('',*,*,#46049,.F.);
#62777=ORIENTED_EDGE('',*,*,#46050,.F.);
#62778=ORIENTED_EDGE('',*,*,#46045,.F.);
#62779=ORIENTED_EDGE('',*,*,#46051,.F.);
#62780=ORIENTED_EDGE('',*,*,#46052,.T.);
#62781=ORIENTED_EDGE('',*,*,#46053,.T.);
#62782=ORIENTED_EDGE('',*,*,#46049,.T.);
#62783=ORIENTED_EDGE('',*,*,#46054,.T.);
#62784=ORIENTED_EDGE('',*,*,#46055,.T.);
#62785=ORIENTED_EDGE('',*,*,#45037,.T.);
#62786=ORIENTED_EDGE('',*,*,#45942,.T.);
#62787=ORIENTED_EDGE('',*,*,#45929,.T.);
#62788=ORIENTED_EDGE('',*,*,#46056,.F.);
#62789=ORIENTED_EDGE('',*,*,#46057,.T.);
#62790=ORIENTED_EDGE('',*,*,#46058,.F.);
#62791=ORIENTED_EDGE('',*,*,#45945,.F.);
#62792=ORIENTED_EDGE('',*,*,#45956,.F.);
#62793=ORIENTED_EDGE('',*,*,#46059,.T.);
#62794=ORIENTED_EDGE('',*,*,#46060,.F.);
#62795=ORIENTED_EDGE('',*,*,#45648,.T.);
#62796=ORIENTED_EDGE('',*,*,#45646,.F.);
#62797=ORIENTED_EDGE('',*,*,#45655,.T.);
#62798=ORIENTED_EDGE('',*,*,#45658,.F.);
#62799=ORIENTED_EDGE('',*,*,#45845,.T.);
#62800=ORIENTED_EDGE('',*,*,#45661,.F.);
#62801=ORIENTED_EDGE('',*,*,#45664,.T.);
#62802=ORIENTED_EDGE('',*,*,#45628,.F.);
#62803=ORIENTED_EDGE('',*,*,#45637,.T.);
#62804=ORIENTED_EDGE('',*,*,#45639,.T.);
#62805=ORIENTED_EDGE('',*,*,#45640,.F.);
#62806=ORIENTED_EDGE('',*,*,#45250,.T.);
#62807=ORIENTED_EDGE('',*,*,#45253,.F.);
#62808=ORIENTED_EDGE('',*,*,#45255,.T.);
#62809=ORIENTED_EDGE('',*,*,#45257,.F.);
#62810=ORIENTED_EDGE('',*,*,#45259,.T.);
#62811=ORIENTED_EDGE('',*,*,#45261,.T.);
#62812=ORIENTED_EDGE('',*,*,#45652,.F.);
#62813=ORIENTED_EDGE('',*,*,#45665,.T.);
#62814=ORIENTED_EDGE('',*,*,#45276,.F.);
#62815=ORIENTED_EDGE('',*,*,#46061,.T.);
#62816=ORIENTED_EDGE('',*,*,#46062,.T.);
#62817=ORIENTED_EDGE('',*,*,#46034,.T.);
#62818=ORIENTED_EDGE('',*,*,#44976,.F.);
#62819=ORIENTED_EDGE('',*,*,#44968,.T.);
#62820=ORIENTED_EDGE('',*,*,#46063,.F.);
#62821=ORIENTED_EDGE('',*,*,#45001,.T.);
#62822=ORIENTED_EDGE('',*,*,#44941,.F.);
#62823=ORIENTED_EDGE('',*,*,#44962,.F.);
#62824=ORIENTED_EDGE('',*,*,#46064,.F.);
#62825=ORIENTED_EDGE('',*,*,#46065,.F.);
#62826=ORIENTED_EDGE('',*,*,#46066,.F.);
#62827=ORIENTED_EDGE('',*,*,#46064,.T.);
#62828=ORIENTED_EDGE('',*,*,#44961,.T.);
#62829=ORIENTED_EDGE('',*,*,#45101,.T.);
#62830=ORIENTED_EDGE('',*,*,#46067,.F.);
#62831=ORIENTED_EDGE('',*,*,#46068,.F.);
#62832=ORIENTED_EDGE('',*,*,#46069,.F.);
#62833=ORIENTED_EDGE('',*,*,#46070,.T.);
#62834=ORIENTED_EDGE('',*,*,#46071,.F.);
#62835=ORIENTED_EDGE('',*,*,#45099,.T.);
#62836=ORIENTED_EDGE('',*,*,#46072,.T.);
#62837=ORIENTED_EDGE('',*,*,#46068,.T.);
#62838=ORIENTED_EDGE('',*,*,#46073,.F.);
#62839=ORIENTED_EDGE('',*,*,#46074,.F.);
#62840=ORIENTED_EDGE('',*,*,#46075,.F.);
#62841=ORIENTED_EDGE('',*,*,#46076,.F.);
#62842=ORIENTED_EDGE('',*,*,#44952,.F.);
#62843=ORIENTED_EDGE('',*,*,#46077,.F.);
#62844=ORIENTED_EDGE('',*,*,#46078,.F.);
#62845=ORIENTED_EDGE('',*,*,#46079,.F.);
#62846=ORIENTED_EDGE('',*,*,#44953,.T.);
#62847=ORIENTED_EDGE('',*,*,#46076,.T.);
#62848=ORIENTED_EDGE('',*,*,#46080,.T.);
#62849=ORIENTED_EDGE('',*,*,#46081,.T.);
#62850=ORIENTED_EDGE('',*,*,#46082,.F.);
#62851=ORIENTED_EDGE('',*,*,#44954,.F.);
#62852=ORIENTED_EDGE('',*,*,#46081,.F.);
#62853=ORIENTED_EDGE('',*,*,#46083,.F.);
#62854=ORIENTED_EDGE('',*,*,#44955,.T.);
#62855=ORIENTED_EDGE('',*,*,#46082,.T.);
#62856=ORIENTED_EDGE('',*,*,#46084,.T.);
#62857=ORIENTED_EDGE('',*,*,#46037,.T.);
#62858=ORIENTED_EDGE('',*,*,#46085,.F.);
#62859=ORIENTED_EDGE('',*,*,#46086,.T.);
#62860=ORIENTED_EDGE('',*,*,#46057,.F.);
#62861=ORIENTED_EDGE('',*,*,#46087,.F.);
#62862=ORIENTED_EDGE('',*,*,#45299,.F.);
#62863=ORIENTED_EDGE('',*,*,#45302,.T.);
#62864=ORIENTED_EDGE('',*,*,#45304,.F.);
#62865=ORIENTED_EDGE('',*,*,#45306,.T.);
#62866=ORIENTED_EDGE('',*,*,#45308,.F.);
#62867=ORIENTED_EDGE('',*,*,#45310,.T.);
#62868=ORIENTED_EDGE('',*,*,#46033,.F.);
#62869=ORIENTED_EDGE('',*,*,#46031,.T.);
#62870=ORIENTED_EDGE('',*,*,#46035,.T.);
#62871=ORIENTED_EDGE('',*,*,#46062,.F.);
#62872=ORIENTED_EDGE('',*,*,#46088,.T.);
#62873=ORIENTED_EDGE('',*,*,#46046,.F.);
#62874=ORIENTED_EDGE('',*,*,#46050,.T.);
#62875=ORIENTED_EDGE('',*,*,#46053,.F.);
#62876=ORIENTED_EDGE('',*,*,#46089,.T.);
#62877=ORIENTED_EDGE('',*,*,#46090,.F.);
#62878=ORIENTED_EDGE('',*,*,#46089,.F.);
#62879=ORIENTED_EDGE('',*,*,#46052,.F.);
#62880=ORIENTED_EDGE('',*,*,#46091,.F.);
#62881=ORIENTED_EDGE('',*,*,#46085,.T.);
#62882=ORIENTED_EDGE('',*,*,#46090,.T.);
#62883=ORIENTED_EDGE('',*,*,#46092,.T.);
#62884=ORIENTED_EDGE('',*,*,#46093,.T.);
#62885=ORIENTED_EDGE('',*,*,#46060,.T.);
#62886=ORIENTED_EDGE('',*,*,#46094,.T.);
#62887=ORIENTED_EDGE('',*,*,#46095,.T.);
#62888=ORIENTED_EDGE('',*,*,#45649,.T.);
#62889=ORIENTED_EDGE('',*,*,#46096,.F.);
#62890=ORIENTED_EDGE('',*,*,#46097,.F.);
#62891=ORIENTED_EDGE('',*,*,#46070,.F.);
#62892=ORIENTED_EDGE('',*,*,#46098,.F.);
#62893=ORIENTED_EDGE('',*,*,#46099,.F.);
#62894=ORIENTED_EDGE('',*,*,#46098,.T.);
#62895=ORIENTED_EDGE('',*,*,#46069,.T.);
#62896=ORIENTED_EDGE('',*,*,#46072,.F.);
#62897=ORIENTED_EDGE('',*,*,#45098,.F.);
#62898=ORIENTED_EDGE('',*,*,#45990,.T.);
#62899=ORIENTED_EDGE('',*,*,#45987,.T.);
#62900=ORIENTED_EDGE('',*,*,#45874,.T.);
#62901=ORIENTED_EDGE('',*,*,#45872,.F.);
#62902=ORIENTED_EDGE('',*,*,#45886,.T.);
#62903=ORIENTED_EDGE('',*,*,#45881,.F.);
#62904=ORIENTED_EDGE('',*,*,#45057,.T.);
#62905=ORIENTED_EDGE('',*,*,#45852,.F.);
#62906=ORIENTED_EDGE('',*,*,#45863,.T.);
#62907=ORIENTED_EDGE('',*,*,#45848,.F.);
#62908=ORIENTED_EDGE('',*,*,#46022,.T.);
#62909=ORIENTED_EDGE('',*,*,#46036,.F.);
#62910=ORIENTED_EDGE('',*,*,#45139,.T.);
#62911=ORIENTED_EDGE('',*,*,#46011,.F.);
#62912=ORIENTED_EDGE('',*,*,#45993,.F.);
#62913=ORIENTED_EDGE('',*,*,#46000,.F.);
#62914=ORIENTED_EDGE('',*,*,#45996,.F.);
#62915=ORIENTED_EDGE('',*,*,#46016,.F.);
#62916=ORIENTED_EDGE('',*,*,#45103,.T.);
#62917=ORIENTED_EDGE('',*,*,#45921,.F.);
#62918=ORIENTED_EDGE('',*,*,#45923,.T.);
#62919=ORIENTED_EDGE('',*,*,#45924,.T.);
#62920=ORIENTED_EDGE('',*,*,#46040,.F.);
#62921=ORIENTED_EDGE('',*,*,#46043,.F.);
#62922=ORIENTED_EDGE('',*,*,#46100,.T.);
#62923=ORIENTED_EDGE('',*,*,#46101,.F.);
#62924=ORIENTED_EDGE('',*,*,#45909,.F.);
#62925=ORIENTED_EDGE('',*,*,#45958,.T.);
#62926=ORIENTED_EDGE('',*,*,#45914,.T.);
#62927=ORIENTED_EDGE('',*,*,#45918,.F.);
#62928=ORIENTED_EDGE('',*,*,#46102,.T.);
#62929=ORIENTED_EDGE('',*,*,#45901,.T.);
#62930=ORIENTED_EDGE('',*,*,#46099,.T.);
#62931=ORIENTED_EDGE('',*,*,#46103,.T.);
#62932=ORIENTED_EDGE('',*,*,#46104,.T.);
#62933=ORIENTED_EDGE('',*,*,#46096,.T.);
#62934=ORIENTED_EDGE('',*,*,#46105,.T.);
#62935=ORIENTED_EDGE('',*,*,#46106,.F.);
#62936=ORIENTED_EDGE('',*,*,#46103,.F.);
#62937=ORIENTED_EDGE('',*,*,#46102,.F.);
#62938=ORIENTED_EDGE('',*,*,#45917,.F.);
#62939=ORIENTED_EDGE('',*,*,#46107,.T.);
#62940=ORIENTED_EDGE('',*,*,#46108,.F.);
#62941=ORIENTED_EDGE('',*,*,#46109,.F.);
#62942=ORIENTED_EDGE('',*,*,#46110,.T.);
#62943=ORIENTED_EDGE('',*,*,#46108,.T.);
#62944=ORIENTED_EDGE('',*,*,#46111,.T.);
#62945=ORIENTED_EDGE('',*,*,#45003,.T.);
#62946=ORIENTED_EDGE('',*,*,#46112,.F.);
#62947=ORIENTED_EDGE('',*,*,#46113,.F.);
#62948=ORIENTED_EDGE('',*,*,#46114,.T.);
#62949=ORIENTED_EDGE('',*,*,#45949,.T.);
#62950=ORIENTED_EDGE('',*,*,#46114,.F.);
#62951=ORIENTED_EDGE('',*,*,#46065,.T.);
#62952=ORIENTED_EDGE('',*,*,#46066,.T.);
#62953=ORIENTED_EDGE('',*,*,#45100,.T.);
#62954=ORIENTED_EDGE('',*,*,#46071,.T.);
#62955=ORIENTED_EDGE('',*,*,#46067,.T.);
#62956=ORIENTED_EDGE('',*,*,#46097,.T.);
#62957=ORIENTED_EDGE('',*,*,#46104,.F.);
#62958=ORIENTED_EDGE('',*,*,#46106,.T.);
#62959=ORIENTED_EDGE('',*,*,#46115,.F.);
#62960=ORIENTED_EDGE('',*,*,#46116,.F.);
#62961=ORIENTED_EDGE('',*,*,#46109,.T.);
#62962=ORIENTED_EDGE('',*,*,#46110,.F.);
#62963=ORIENTED_EDGE('',*,*,#45002,.T.);
#62964=ORIENTED_EDGE('',*,*,#46063,.T.);
#62965=ORIENTED_EDGE('',*,*,#44967,.T.);
#62966=ORIENTED_EDGE('',*,*,#44965,.F.);
#62967=ORIENTED_EDGE('',*,*,#44963,.T.);
#62968=ORIENTED_EDGE('',*,*,#44942,.F.);
#62969=ORIENTED_EDGE('',*,*,#46105,.F.);
#62970=ORIENTED_EDGE('',*,*,#46116,.T.);
#62971=ORIENTED_EDGE('',*,*,#46117,.T.);
#62972=ORIENTED_EDGE('',*,*,#46112,.T.);
#62973=ORIENTED_EDGE('',*,*,#46113,.T.);
#62974=ORIENTED_EDGE('',*,*,#46117,.F.);
#62975=ORIENTED_EDGE('',*,*,#46115,.T.);
#62976=ORIENTED_EDGE('',*,*,#45537,.F.);
#62977=ORIENTED_EDGE('',*,*,#46118,.F.);
#62978=ORIENTED_EDGE('',*,*,#46119,.F.);
#62979=ORIENTED_EDGE('',*,*,#46120,.F.);
#62980=ORIENTED_EDGE('',*,*,#45190,.T.);
#62981=ORIENTED_EDGE('',*,*,#45192,.T.);
#62982=ORIENTED_EDGE('',*,*,#45194,.F.);
#62983=ORIENTED_EDGE('',*,*,#45196,.T.);
#62984=ORIENTED_EDGE('',*,*,#45198,.F.);
#62985=ORIENTED_EDGE('',*,*,#45200,.T.);
#62986=ORIENTED_EDGE('',*,*,#45202,.F.);
#62987=ORIENTED_EDGE('',*,*,#45213,.F.);
#62988=ORIENTED_EDGE('',*,*,#46121,.F.);
#62989=ORIENTED_EDGE('',*,*,#46122,.F.);
#62990=ORIENTED_EDGE('',*,*,#46123,.F.);
#62991=ORIENTED_EDGE('',*,*,#45515,.F.);
#62992=ORIENTED_EDGE('',*,*,#46124,.F.);
#62993=ORIENTED_EDGE('',*,*,#46125,.F.);
#62994=ORIENTED_EDGE('',*,*,#46126,.F.);
#62995=ORIENTED_EDGE('',*,*,#46127,.T.);
#62996=ORIENTED_EDGE('',*,*,#45940,.F.);
#62997=ORIENTED_EDGE('',*,*,#45456,.T.);
#62998=ORIENTED_EDGE('',*,*,#46128,.F.);
#62999=ORIENTED_EDGE('',*,*,#45559,.T.);
#63000=ORIENTED_EDGE('',*,*,#45562,.F.);
#63001=ORIENTED_EDGE('',*,*,#45564,.F.);
#63002=ORIENTED_EDGE('',*,*,#45566,.F.);
#63003=ORIENTED_EDGE('',*,*,#45579,.F.);
#63004=ORIENTED_EDGE('',*,*,#46129,.F.);
#63005=ORIENTED_EDGE('',*,*,#46130,.F.);
#63006=ORIENTED_EDGE('',*,*,#46131,.F.);
#63007=ORIENTED_EDGE('',*,*,#45354,.F.);
#63008=ORIENTED_EDGE('',*,*,#45363,.F.);
#63009=ORIENTED_EDGE('',*,*,#45365,.T.);
#63010=ORIENTED_EDGE('',*,*,#46132,.F.);
#63011=ORIENTED_EDGE('',*,*,#46133,.T.);
#63012=ORIENTED_EDGE('',*,*,#46134,.F.);
#63013=ORIENTED_EDGE('',*,*,#46135,.T.);
#63014=ORIENTED_EDGE('',*,*,#46136,.T.);
#63015=ORIENTED_EDGE('',*,*,#45345,.T.);
#63016=ORIENTED_EDGE('',*,*,#45348,.F.);
#63017=ORIENTED_EDGE('',*,*,#45352,.F.);
#63018=ORIENTED_EDGE('',*,*,#46137,.F.);
#63019=ORIENTED_EDGE('',*,*,#46138,.F.);
#63020=ORIENTED_EDGE('',*,*,#45927,.F.);
#63021=ORIENTED_EDGE('',*,*,#45936,.T.);
#63022=ORIENTED_EDGE('',*,*,#45939,.F.);
#63023=ORIENTED_EDGE('',*,*,#46139,.F.);
#63024=ORIENTED_EDGE('',*,*,#45634,.F.);
#63025=ORIENTED_EDGE('',*,*,#45643,.F.);
#63026=ORIENTED_EDGE('',*,*,#45760,.F.);
#63027=ORIENTED_EDGE('',*,*,#45204,.F.);
#63028=ORIENTED_EDGE('',*,*,#45184,.T.);
#63029=ORIENTED_EDGE('',*,*,#45188,.T.);
#63030=ORIENTED_EDGE('',*,*,#45534,.F.);
#63031=ORIENTED_EDGE('',*,*,#46120,.T.);
#63032=ORIENTED_EDGE('',*,*,#46140,.T.);
#63033=ORIENTED_EDGE('',*,*,#45567,.T.);
#63034=ORIENTED_EDGE('',*,*,#46141,.F.);
#63035=ORIENTED_EDGE('',*,*,#45357,.F.);
#63036=ORIENTED_EDGE('',*,*,#46142,.F.);
#63037=ORIENTED_EDGE('',*,*,#45575,.T.);
#63038=ORIENTED_EDGE('',*,*,#46143,.T.);
#63039=ORIENTED_EDGE('',*,*,#45967,.F.);
#63040=ORIENTED_EDGE('',*,*,#45965,.F.);
#63041=ORIENTED_EDGE('',*,*,#46143,.F.);
#63042=ORIENTED_EDGE('',*,*,#45574,.T.);
#63043=ORIENTED_EDGE('',*,*,#46144,.F.);
#63044=ORIENTED_EDGE('',*,*,#45517,.F.);
#63045=ORIENTED_EDGE('',*,*,#46145,.F.);
#63046=ORIENTED_EDGE('',*,*,#46146,.F.);
#63047=ORIENTED_EDGE('',*,*,#46147,.F.);
#63048=ORIENTED_EDGE('',*,*,#46148,.F.);
#63049=ORIENTED_EDGE('',*,*,#46149,.F.);
#63050=ORIENTED_EDGE('',*,*,#46150,.F.);
#63051=ORIENTED_EDGE('',*,*,#46151,.T.);
#63052=ORIENTED_EDGE('',*,*,#46152,.F.);
#63053=ORIENTED_EDGE('',*,*,#46153,.F.);
#63054=ORIENTED_EDGE('',*,*,#46154,.F.);
#63055=ORIENTED_EDGE('',*,*,#46155,.F.);
#63056=ORIENTED_EDGE('',*,*,#46156,.F.);
#63057=ORIENTED_EDGE('',*,*,#45208,.F.);
#63058=ORIENTED_EDGE('',*,*,#46157,.F.);
#63059=ORIENTED_EDGE('',*,*,#46153,.T.);
#63060=ORIENTED_EDGE('',*,*,#46158,.F.);
#63061=ORIENTED_EDGE('',*,*,#45523,.F.);
#63062=ORIENTED_EDGE('',*,*,#46159,.F.);
#63063=ORIENTED_EDGE('',*,*,#46146,.T.);
#63064=ORIENTED_EDGE('',*,*,#46160,.F.);
#63065=ORIENTED_EDGE('',*,*,#46122,.T.);
#63066=ORIENTED_EDGE('',*,*,#46145,.T.);
#63067=ORIENTED_EDGE('',*,*,#45516,.T.);
#63068=ORIENTED_EDGE('',*,*,#46123,.T.);
#63069=ORIENTED_EDGE('',*,*,#46160,.T.);
#63070=ORIENTED_EDGE('',*,*,#46161,.F.);
#63071=ORIENTED_EDGE('',*,*,#46147,.T.);
#63072=ORIENTED_EDGE('',*,*,#46159,.T.);
#63073=ORIENTED_EDGE('',*,*,#46121,.T.);
#63074=ORIENTED_EDGE('',*,*,#45212,.T.);
#63075=ORIENTED_EDGE('',*,*,#46162,.T.);
#63076=ORIENTED_EDGE('',*,*,#46154,.T.);
#63077=ORIENTED_EDGE('',*,*,#46157,.T.);
#63078=ORIENTED_EDGE('',*,*,#45207,.T.);
#63079=ORIENTED_EDGE('',*,*,#46163,.T.);
#63080=ORIENTED_EDGE('',*,*,#45524,.T.);
#63081=ORIENTED_EDGE('',*,*,#46158,.T.);
#63082=ORIENTED_EDGE('',*,*,#46152,.T.);
#63083=ORIENTED_EDGE('',*,*,#46164,.T.);
#63084=ORIENTED_EDGE('',*,*,#45360,.T.);
#63085=ORIENTED_EDGE('',*,*,#46165,.T.);
#63086=ORIENTED_EDGE('',*,*,#46150,.T.);
#63087=ORIENTED_EDGE('',*,*,#46166,.T.);
#63088=ORIENTED_EDGE('',*,*,#46148,.T.);
#63089=ORIENTED_EDGE('',*,*,#46167,.T.);
#63090=ORIENTED_EDGE('',*,*,#45571,.T.);
#63091=ORIENTED_EDGE('',*,*,#46168,.F.);
#63092=ORIENTED_EDGE('',*,*,#46169,.F.);
#63093=ORIENTED_EDGE('',*,*,#46170,.F.);
#63094=ORIENTED_EDGE('',*,*,#46130,.T.);
#63095=ORIENTED_EDGE('',*,*,#46171,.T.);
#63096=ORIENTED_EDGE('',*,*,#46168,.T.);
#63097=ORIENTED_EDGE('',*,*,#46129,.T.);
#63098=ORIENTED_EDGE('',*,*,#45578,.T.);
#63099=ORIENTED_EDGE('',*,*,#46172,.F.);
#63100=ORIENTED_EDGE('',*,*,#45355,.T.);
#63101=ORIENTED_EDGE('',*,*,#46131,.T.);
#63102=ORIENTED_EDGE('',*,*,#46170,.T.);
#63103=ORIENTED_EDGE('',*,*,#46173,.T.);
#63104=ORIENTED_EDGE('',*,*,#46174,.F.);
#63105=ORIENTED_EDGE('',*,*,#46173,.F.);
#63106=ORIENTED_EDGE('',*,*,#46169,.T.);
#63107=ORIENTED_EDGE('',*,*,#46171,.F.);
#63108=ORIENTED_EDGE('',*,*,#45577,.F.);
#63109=ORIENTED_EDGE('',*,*,#45576,.T.);
#63110=ORIENTED_EDGE('',*,*,#46142,.T.);
#63111=ORIENTED_EDGE('',*,*,#45356,.T.);
#63112=ORIENTED_EDGE('',*,*,#46172,.T.);
#63113=ORIENTED_EDGE('',*,*,#46174,.T.);
#63114=ORIENTED_EDGE('',*,*,#45211,.T.);
#63115=ORIENTED_EDGE('',*,*,#46175,.T.);
#63116=ORIENTED_EDGE('',*,*,#45518,.T.);
#63117=ORIENTED_EDGE('',*,*,#46144,.T.);
#63118=ORIENTED_EDGE('',*,*,#46161,.T.);
#63119=ORIENTED_EDGE('',*,*,#45521,.T.);
#63120=ORIENTED_EDGE('',*,*,#46176,.T.);
#63121=ORIENTED_EDGE('',*,*,#46177,.F.);
#63122=ORIENTED_EDGE('',*,*,#45522,.F.);
#63123=ORIENTED_EDGE('',*,*,#46177,.T.);
#63124=ORIENTED_EDGE('',*,*,#46178,.T.);
#63125=ORIENTED_EDGE('',*,*,#45209,.T.);
#63126=ORIENTED_EDGE('',*,*,#46156,.T.);
#63127=ORIENTED_EDGE('',*,*,#46179,.F.);
#63128=ORIENTED_EDGE('',*,*,#45572,.F.);
#63129=ORIENTED_EDGE('',*,*,#46167,.F.);
#63130=ORIENTED_EDGE('',*,*,#46151,.F.);
#63131=ORIENTED_EDGE('',*,*,#46165,.F.);
#63132=ORIENTED_EDGE('',*,*,#45359,.F.);
#63133=ORIENTED_EDGE('',*,*,#45358,.T.);
#63134=ORIENTED_EDGE('',*,*,#46141,.T.);
#63135=ORIENTED_EDGE('',*,*,#45573,.T.);
#63136=ORIENTED_EDGE('',*,*,#46179,.T.);
#63137=ORIENTED_EDGE('',*,*,#46180,.T.);
#63138=ORIENTED_EDGE('',*,*,#46181,.T.);
#63139=ORIENTED_EDGE('',*,*,#46137,.T.);
#63140=ORIENTED_EDGE('',*,*,#45351,.T.);
#63141=ORIENTED_EDGE('',*,*,#45316,.F.);
#63142=ORIENTED_EDGE('',*,*,#46182,.T.);
#63143=ORIENTED_EDGE('',*,*,#46132,.T.);
#63144=ORIENTED_EDGE('',*,*,#45364,.T.);
#63145=ORIENTED_EDGE('',*,*,#45322,.F.);
#63146=ORIENTED_EDGE('',*,*,#46183,.T.);
#63147=ORIENTED_EDGE('',*,*,#46134,.T.);
#63148=ORIENTED_EDGE('',*,*,#46184,.T.);
#63149=ORIENTED_EDGE('',*,*,#45319,.F.);
#63150=ORIENTED_EDGE('',*,*,#46184,.F.);
#63151=ORIENTED_EDGE('',*,*,#46133,.F.);
#63152=ORIENTED_EDGE('',*,*,#46182,.F.);
#63153=ORIENTED_EDGE('',*,*,#45540,.F.);
#63154=ORIENTED_EDGE('',*,*,#45453,.T.);
#63155=ORIENTED_EDGE('',*,*,#46185,.T.);
#63156=ORIENTED_EDGE('',*,*,#46118,.T.);
#63157=ORIENTED_EDGE('',*,*,#44949,.T.);
#63158=ORIENTED_EDGE('',*,*,#46186,.T.);
#63159=ORIENTED_EDGE('',*,*,#46187,.T.);
#63160=ORIENTED_EDGE('',*,*,#46188,.T.);
#63161=ORIENTED_EDGE('',*,*,#46189,.F.);
#63162=ORIENTED_EDGE('',*,*,#44950,.F.);
#63163=ORIENTED_EDGE('',*,*,#46188,.F.);
#63164=ORIENTED_EDGE('',*,*,#46190,.F.);
#63165=ORIENTED_EDGE('',*,*,#44951,.T.);
#63166=ORIENTED_EDGE('',*,*,#46189,.T.);
#63167=ORIENTED_EDGE('',*,*,#46191,.T.);
#63168=ORIENTED_EDGE('',*,*,#46077,.T.);
#63169=ORIENTED_EDGE('',*,*,#46192,.F.);
#63170=ORIENTED_EDGE('',*,*,#46078,.T.);
#63171=ORIENTED_EDGE('',*,*,#46191,.F.);
#63172=ORIENTED_EDGE('',*,*,#46190,.T.);
#63173=ORIENTED_EDGE('',*,*,#46187,.F.);
#63174=ORIENTED_EDGE('',*,*,#46193,.F.);
#63175=ORIENTED_EDGE('',*,*,#44995,.T.);
#63176=ORIENTED_EDGE('',*,*,#44998,.T.);
#63177=ORIENTED_EDGE('',*,*,#45000,.F.);
#63178=ORIENTED_EDGE('',*,*,#45004,.F.);
#63179=ORIENTED_EDGE('',*,*,#46111,.F.);
#63180=ORIENTED_EDGE('',*,*,#46107,.F.);
#63181=ORIENTED_EDGE('',*,*,#45919,.F.);
#63182=ORIENTED_EDGE('',*,*,#45916,.T.);
#63183=ORIENTED_EDGE('',*,*,#45959,.F.);
#63184=ORIENTED_EDGE('',*,*,#45911,.F.);
#63185=ORIENTED_EDGE('',*,*,#46194,.F.);
#63186=ORIENTED_EDGE('',*,*,#46180,.F.);
#63187=ORIENTED_EDGE('',*,*,#45350,.T.);
#63188=ORIENTED_EDGE('',*,*,#45361,.T.);
#63189=ORIENTED_EDGE('',*,*,#46164,.F.);
#63190=ORIENTED_EDGE('',*,*,#46149,.T.);
#63191=ORIENTED_EDGE('',*,*,#46166,.F.);
#63192=ORIENTED_EDGE('',*,*,#45570,.F.);
#63193=ORIENTED_EDGE('',*,*,#46192,.T.);
#63194=ORIENTED_EDGE('',*,*,#45569,.T.);
#63195=ORIENTED_EDGE('',*,*,#46195,.T.);
#63196=ORIENTED_EDGE('',*,*,#46079,.T.);
#63197=ORIENTED_EDGE('',*,*,#45545,.F.);
#63198=ORIENTED_EDGE('',*,*,#45560,.T.);
#63199=ORIENTED_EDGE('',*,*,#46128,.T.);
#63200=ORIENTED_EDGE('',*,*,#45455,.T.);
#63201=ORIENTED_EDGE('',*,*,#45483,.F.);
#63202=ORIENTED_EDGE('',*,*,#45941,.F.);
#63203=ORIENTED_EDGE('',*,*,#46127,.F.);
#63204=ORIENTED_EDGE('',*,*,#46196,.F.);
#63205=ORIENTED_EDGE('',*,*,#45480,.F.);
#63206=ORIENTED_EDGE('',*,*,#46196,.T.);
#63207=ORIENTED_EDGE('',*,*,#46126,.T.);
#63208=ORIENTED_EDGE('',*,*,#46197,.T.);
#63209=ORIENTED_EDGE('',*,*,#45477,.F.);
#63210=ORIENTED_EDGE('',*,*,#46197,.F.);
#63211=ORIENTED_EDGE('',*,*,#46125,.T.);
#63212=ORIENTED_EDGE('',*,*,#46198,.F.);
#63213=ORIENTED_EDGE('',*,*,#45474,.F.);
#63214=ORIENTED_EDGE('',*,*,#46198,.T.);
#63215=ORIENTED_EDGE('',*,*,#46124,.T.);
#63216=ORIENTED_EDGE('',*,*,#45514,.T.);
#63217=ORIENTED_EDGE('',*,*,#45241,.F.);
#63218=ORIENTED_EDGE('',*,*,#45635,.T.);
#63219=ORIENTED_EDGE('',*,*,#46139,.T.);
#63220=ORIENTED_EDGE('',*,*,#45938,.F.);
#63221=ORIENTED_EDGE('',*,*,#45946,.T.);
#63222=ORIENTED_EDGE('',*,*,#46058,.T.);
#63223=ORIENTED_EDGE('',*,*,#45651,.F.);
#63224=ORIENTED_EDGE('',*,*,#45328,.F.);
#63225=ORIENTED_EDGE('',*,*,#45346,.F.);
#63226=ORIENTED_EDGE('',*,*,#46136,.F.);
#63227=ORIENTED_EDGE('',*,*,#46199,.T.);
#63228=ORIENTED_EDGE('',*,*,#45325,.F.);
#63229=ORIENTED_EDGE('',*,*,#46199,.F.);
#63230=ORIENTED_EDGE('',*,*,#46135,.F.);
#63231=ORIENTED_EDGE('',*,*,#46183,.F.);
#63232=ORIENTED_EDGE('',*,*,#45282,.F.);
#63233=ORIENTED_EDGE('',*,*,#45300,.F.);
#63234=ORIENTED_EDGE('',*,*,#46087,.T.);
#63235=ORIENTED_EDGE('',*,*,#46056,.T.);
#63236=ORIENTED_EDGE('',*,*,#45928,.F.);
#63237=ORIENTED_EDGE('',*,*,#46138,.T.);
#63238=ORIENTED_EDGE('',*,*,#46181,.F.);
#63239=ORIENTED_EDGE('',*,*,#46194,.T.);
#63240=ORIENTED_EDGE('',*,*,#45910,.F.);
#63241=ORIENTED_EDGE('',*,*,#46101,.T.);
#63242=ORIENTED_EDGE('',*,*,#46200,.T.);
#63243=ORIENTED_EDGE('',*,*,#45279,.F.);
#63244=ORIENTED_EDGE('',*,*,#46200,.F.);
#63245=ORIENTED_EDGE('',*,*,#46100,.F.);
#63246=ORIENTED_EDGE('',*,*,#46042,.F.);
#63247=ORIENTED_EDGE('',*,*,#46201,.F.);
#63248=ORIENTED_EDGE('',*,*,#46047,.F.);
#63249=ORIENTED_EDGE('',*,*,#46088,.F.);
#63250=ORIENTED_EDGE('',*,*,#46061,.F.);
#63251=ORIENTED_EDGE('',*,*,#45904,.F.);
#63252=ORIENTED_EDGE('',*,*,#44984,.F.);
#63253=ORIENTED_EDGE('',*,*,#44996,.F.);
#63254=ORIENTED_EDGE('',*,*,#46193,.T.);
#63255=ORIENTED_EDGE('',*,*,#46186,.F.);
#63256=ORIENTED_EDGE('',*,*,#44948,.F.);
#63257=ORIENTED_EDGE('',*,*,#46202,.F.);
#63258=ORIENTED_EDGE('',*,*,#44981,.F.);
#63259=ORIENTED_EDGE('',*,*,#46202,.T.);
#63260=ORIENTED_EDGE('',*,*,#44947,.T.);
#63261=ORIENTED_EDGE('',*,*,#44970,.T.);
#63262=ORIENTED_EDGE('',*,*,#45081,.F.);
#63263=ORIENTED_EDGE('',*,*,#45978,.T.);
#63264=ORIENTED_EDGE('',*,*,#45876,.F.);
#63265=ORIENTED_EDGE('',*,*,#45986,.F.);
#63266=ORIENTED_EDGE('',*,*,#45989,.T.);
#63267=ORIENTED_EDGE('',*,*,#46026,.T.);
#63268=ORIENTED_EDGE('',*,*,#46028,.F.);
#63269=ORIENTED_EDGE('',*,*,#46029,.F.);
#63270=ORIENTED_EDGE('',*,*,#45979,.T.);
#63271=ORIENTED_EDGE('',*,*,#45079,.T.);
#63272=ORIENTED_EDGE('',*,*,#45115,.T.);
#63273=ORIENTED_EDGE('',*,*,#45980,.T.);
#63274=ORIENTED_EDGE('',*,*,#45878,.F.);
#63275=ORIENTED_EDGE('',*,*,#45977,.T.);
#63276=ORIENTED_EDGE('',*,*,#46018,.F.);
#63277=ORIENTED_EDGE('',*,*,#45971,.F.);
#63278=ORIENTED_EDGE('',*,*,#45069,.F.);
#63279=ORIENTED_EDGE('',*,*,#45039,.F.);
#63280=ORIENTED_EDGE('',*,*,#45113,.F.);
#63281=ORIENTED_EDGE('',*,*,#45108,.F.);
#63282=ORIENTED_EDGE('',*,*,#45050,.F.);
#63283=ORIENTED_EDGE('',*,*,#45045,.F.);
#63284=ORIENTED_EDGE('',*,*,#45042,.T.);
#63285=ORIENTED_EDGE('',*,*,#45063,.F.);
#63286=ORIENTED_EDGE('',*,*,#45983,.F.);
#63287=ORIENTED_EDGE('',*,*,#45116,.F.);
#63288=ORIENTED_EDGE('',*,*,#45111,.F.);
#63289=ORIENTED_EDGE('',*,*,#46054,.F.);
#63290=ORIENTED_EDGE('',*,*,#46086,.F.);
#63291=ORIENTED_EDGE('',*,*,#46093,.F.);
#63292=ORIENTED_EDGE('',*,*,#46203,.F.);
#63293=ORIENTED_EDGE('',*,*,#46204,.F.);
#63294=ORIENTED_EDGE('',*,*,#46205,.F.);
#63295=ORIENTED_EDGE('',*,*,#46204,.T.);
#63296=ORIENTED_EDGE('',*,*,#46206,.T.);
#63297=ORIENTED_EDGE('',*,*,#46207,.T.);
#63298=ORIENTED_EDGE('',*,*,#46208,.F.);
#63299=ORIENTED_EDGE('',*,*,#46207,.F.);
#63300=ORIENTED_EDGE('',*,*,#46209,.F.);
#63301=ORIENTED_EDGE('',*,*,#46094,.F.);
#63302=ORIENTED_EDGE('',*,*,#46059,.F.);
#63303=ORIENTED_EDGE('',*,*,#45955,.F.);
#63304=ORIENTED_EDGE('',*,*,#46210,.F.);
#63305=ORIENTED_EDGE('',*,*,#45022,.F.);
#63306=ORIENTED_EDGE('',*,*,#45931,.F.);
#63307=ORIENTED_EDGE('',*,*,#45943,.F.);
#63308=ORIENTED_EDGE('',*,*,#45036,.T.);
#63309=ORIENTED_EDGE('',*,*,#46205,.T.);
#63310=ORIENTED_EDGE('',*,*,#46208,.T.);
#63311=ORIENTED_EDGE('',*,*,#46210,.T.);
#63312=ORIENTED_EDGE('',*,*,#45957,.F.);
#63313=ORIENTED_EDGE('',*,*,#45035,.T.);
#63314=ORIENTED_EDGE('',*,*,#46055,.F.);
#63315=ORIENTED_EDGE('',*,*,#45784,.T.);
#63316=ORIENTED_EDGE('',*,*,#46211,.T.);
#63317=ORIENTED_EDGE('',*,*,#45519,.T.);
#63318=ORIENTED_EDGE('',*,*,#46175,.F.);
#63319=ORIENTED_EDGE('',*,*,#45210,.F.);
#63320=ORIENTED_EDGE('',*,*,#46178,.F.);
#63321=ORIENTED_EDGE('',*,*,#46176,.F.);
#63322=ORIENTED_EDGE('',*,*,#45520,.T.);
#63323=ORIENTED_EDGE('',*,*,#46211,.F.);
#63324=ORIENTED_EDGE('',*,*,#46095,.F.);
#63325=ORIENTED_EDGE('',*,*,#46209,.T.);
#63326=ORIENTED_EDGE('',*,*,#46206,.F.);
#63327=ORIENTED_EDGE('',*,*,#46203,.T.);
#63328=ORIENTED_EDGE('',*,*,#46092,.F.);
#63329=ORIENTED_EDGE('',*,*,#46091,.T.);
#63330=ORIENTED_EDGE('',*,*,#46051,.T.);
#63331=ORIENTED_EDGE('',*,*,#46048,.T.);
#63332=ORIENTED_EDGE('',*,*,#46044,.T.);
#63333=ORIENTED_EDGE('',*,*,#46201,.T.);
#63334=ORIENTED_EDGE('',*,*,#46041,.T.);
#63335=ORIENTED_EDGE('',*,*,#46038,.T.);
#63336=ORIENTED_EDGE('',*,*,#46084,.F.);
#63337=ORIENTED_EDGE('',*,*,#46083,.T.);
#63338=ORIENTED_EDGE('',*,*,#46080,.F.);
#63339=ORIENTED_EDGE('',*,*,#46075,.T.);
#63340=ORIENTED_EDGE('',*,*,#46212,.F.);
#63341=ORIENTED_EDGE('',*,*,#45595,.T.);
#63342=ORIENTED_EDGE('',*,*,#45608,.F.);
#63343=ORIENTED_EDGE('',*,*,#45617,.T.);
#63344=ORIENTED_EDGE('',*,*,#45618,.T.);
#63345=ORIENTED_EDGE('',*,*,#45844,.T.);
#63346=ORIENTED_EDGE('',*,*,#45745,.T.);
#63347=ORIENTED_EDGE('',*,*,#45755,.T.);
#63348=ORIENTED_EDGE('',*,*,#45703,.T.);
#63349=ORIENTED_EDGE('',*,*,#45717,.T.);
#63350=ORIENTED_EDGE('',*,*,#45731,.T.);
#63351=ORIENTED_EDGE('',*,*,#45710,.T.);
#63352=ORIENTED_EDGE('',*,*,#45699,.T.);
#63353=ORIENTED_EDGE('',*,*,#45754,.T.);
#63354=ORIENTED_EDGE('',*,*,#45753,.T.);
#63355=ORIENTED_EDGE('',*,*,#45843,.F.);
#63356=ORIENTED_EDGE('',*,*,#45733,.T.);
#63357=ORIENTED_EDGE('',*,*,#45743,.T.);
#63358=ORIENTED_EDGE('',*,*,#45709,.T.);
#63359=ORIENTED_EDGE('',*,*,#45725,.T.);
#63360=ORIENTED_EDGE('',*,*,#45728,.T.);
#63361=ORIENTED_EDGE('',*,*,#45718,.T.);
#63362=ORIENTED_EDGE('',*,*,#45705,.T.);
#63363=ORIENTED_EDGE('',*,*,#45742,.T.);
#63364=ORIENTED_EDGE('',*,*,#45741,.T.);
#63365=ORIENTED_EDGE('',*,*,#45842,.F.);
#63366=ORIENTED_EDGE('',*,*,#45656,.T.);
#63367=ORIENTED_EDGE('',*,*,#45653,.T.);
#63368=ORIENTED_EDGE('',*,*,#45644,.F.);
#63369=ORIENTED_EDGE('',*,*,#45650,.T.);
#63370=ORIENTED_EDGE('',*,*,#45895,.T.);
#63371=ORIENTED_EDGE('',*,*,#45667,.T.);
#63372=ORIENTED_EDGE('',*,*,#45625,.T.);
#63373=ORIENTED_EDGE('',*,*,#46212,.T.);
#63374=ORIENTED_EDGE('',*,*,#46074,.T.);
#63375=ORIENTED_EDGE('',*,*,#46213,.T.);
#63376=ORIENTED_EDGE('',*,*,#45596,.T.);
#63377=ORIENTED_EDGE('',*,*,#46213,.F.);
#63378=ORIENTED_EDGE('',*,*,#46073,.T.);
#63379=ORIENTED_EDGE('',*,*,#46195,.F.);
#63380=ORIENTED_EDGE('',*,*,#45568,.T.);
#63381=ORIENTED_EDGE('',*,*,#46140,.F.);
#63382=ORIENTED_EDGE('',*,*,#46119,.T.);
#63383=ORIENTED_EDGE('',*,*,#46185,.F.);
#63384=ORIENTED_EDGE('',*,*,#45452,.T.);
#63385=ORIENTED_EDGE('',*,*,#45462,.F.);
#63386=ORIENTED_EDGE('',*,*,#45464,.T.);
#63387=ORIENTED_EDGE('',*,*,#45466,.F.);
#63388=ORIENTED_EDGE('',*,*,#45468,.T.);
#63389=ORIENTED_EDGE('',*,*,#45581,.F.);
#63390=ORIENTED_EDGE('',*,*,#45583,.T.);
#63391=ORIENTED_EDGE('',*,*,#45584,.F.);
#63392=ORIENTED_EDGE('',*,*,#45527,.F.);
#63393=ORIENTED_EDGE('',*,*,#45603,.F.);
#63394=ORIENTED_EDGE('',*,*,#45597,.T.);
#63395=ORIENTED_EDGE('',*,*,#45429,.F.);
#63396=ORIENTED_EDGE('',*,*,#45448,.F.);
#63397=ORIENTED_EDGE('',*,*,#46214,.F.);
#63398=ORIENTED_EDGE('',*,*,#45604,.F.);
#63399=ORIENTED_EDGE('',*,*,#46214,.T.);
#63400=ORIENTED_EDGE('',*,*,#45447,.F.);
#63401=ORIENTED_EDGE('',*,*,#45460,.T.);
#63402=ORIENTED_EDGE('',*,*,#45947,.F.);
#63403=ORIENTED_EDGE('',*,*,#45507,.T.);
#63404=ORIENTED_EDGE('',*,*,#45510,.F.);
#63405=ORIENTED_EDGE('',*,*,#45513,.T.);
#63406=ORIENTED_EDGE('',*,*,#45605,.F.);
#63407=ORIENTED_EDGE('',*,*,#45525,.F.);
#63408=ORIENTED_EDGE('',*,*,#46163,.F.);
#63409=ORIENTED_EDGE('',*,*,#46155,.T.);
#63410=ORIENTED_EDGE('',*,*,#46162,.F.);
#63411=ORIENTED_EDGE('',*,*,#45206,.T.);
#63412=ORIENTED_EDGE('',*,*,#45759,.T.);
#63413=ORIENTED_EDGE('',*,*,#45641,.F.);
#63414=ORIENTED_EDGE('',*,*,#45632,.T.);
#63415=ORIENTED_EDGE('',*,*,#45670,.F.);
#63416=ORIENTED_EDGE('',*,*,#45758,.F.);
#63417=ORIENTED_EDGE('',*,*,#45836,.T.);
#63418=ORIENTED_EDGE('',*,*,#45674,.F.);
#63419=ORIENTED_EDGE('',*,*,#45827,.F.);
#63420=ORIENTED_EDGE('',*,*,#45612,.F.);
#63421=ORIENTED_EDGE('',*,*,#45609,.T.);
#63422=ORIENTED_EDGE('',*,*,#45599,.T.);
#63423=ORIENTED_EDGE('',*,*,#45588,.F.);
#63424=ORIENTED_EDGE('',*,*,#45592,.T.);
#63425=ORIENTED_EDGE('',*,*,#45602,.F.);
#63426=ORIENTED_EDGE('',*,*,#46215,.F.);
#63427=ORIENTED_EDGE('',*,*,#46216,.F.);
#63428=ORIENTED_EDGE('',*,*,#46217,.F.);
#63429=ORIENTED_EDGE('',*,*,#46218,.F.);
#63430=ORIENTED_EDGE('',*,*,#46219,.F.);
#63431=ORIENTED_EDGE('',*,*,#46220,.F.);
#63432=ORIENTED_EDGE('',*,*,#46221,.F.);
#63433=ORIENTED_EDGE('',*,*,#46222,.F.);
#63434=ORIENTED_EDGE('',*,*,#46223,.T.);
#63435=ORIENTED_EDGE('',*,*,#46217,.T.);
#63436=ORIENTED_EDGE('',*,*,#46224,.F.);
#63437=ORIENTED_EDGE('',*,*,#46225,.T.);
#63438=ORIENTED_EDGE('',*,*,#46226,.T.);
#63439=ORIENTED_EDGE('',*,*,#46227,.T.);
#63440=ORIENTED_EDGE('',*,*,#46228,.F.);
#63441=ORIENTED_EDGE('',*,*,#46229,.T.);
#63442=ORIENTED_EDGE('',*,*,#46230,.T.);
#63443=ORIENTED_EDGE('',*,*,#46231,.T.);
#63444=ORIENTED_EDGE('',*,*,#46232,.T.);
#63445=ORIENTED_EDGE('',*,*,#46233,.F.);
#63446=ORIENTED_EDGE('',*,*,#46234,.F.);
#63447=ORIENTED_EDGE('',*,*,#46235,.F.);
#63448=ORIENTED_EDGE('',*,*,#46236,.T.);
#63449=ORIENTED_EDGE('',*,*,#46237,.F.);
#63450=ORIENTED_EDGE('',*,*,#46238,.T.);
#63451=ORIENTED_EDGE('',*,*,#46239,.T.);
#63452=ORIENTED_EDGE('',*,*,#46219,.T.);
#63453=ORIENTED_EDGE('',*,*,#46240,.T.);
#63454=ORIENTED_EDGE('',*,*,#46241,.F.);
#63455=ORIENTED_EDGE('',*,*,#46242,.F.);
#63456=ORIENTED_EDGE('',*,*,#46243,.F.);
#63457=ORIENTED_EDGE('',*,*,#46244,.F.);
#63458=ORIENTED_EDGE('',*,*,#46245,.F.);
#63459=ORIENTED_EDGE('',*,*,#46246,.F.);
#63460=ORIENTED_EDGE('',*,*,#46247,.F.);
#63461=ORIENTED_EDGE('',*,*,#46248,.F.);
#63462=ORIENTED_EDGE('',*,*,#46249,.F.);
#63463=ORIENTED_EDGE('',*,*,#46250,.T.);
#63464=ORIENTED_EDGE('',*,*,#46251,.T.);
#63465=ORIENTED_EDGE('',*,*,#46252,.T.);
#63466=ORIENTED_EDGE('',*,*,#46253,.F.);
#63467=ORIENTED_EDGE('',*,*,#46254,.F.);
#63468=ORIENTED_EDGE('',*,*,#46240,.F.);
#63469=ORIENTED_EDGE('',*,*,#46255,.F.);
#63470=ORIENTED_EDGE('',*,*,#46256,.T.);
#63471=ORIENTED_EDGE('',*,*,#46257,.T.);
#63472=ORIENTED_EDGE('',*,*,#46258,.T.);
#63473=ORIENTED_EDGE('',*,*,#46259,.F.);
#63474=ORIENTED_EDGE('',*,*,#46260,.F.);
#63475=ORIENTED_EDGE('',*,*,#46261,.T.);
#63476=ORIENTED_EDGE('',*,*,#46262,.F.);
#63477=ORIENTED_EDGE('',*,*,#46263,.T.);
#63478=ORIENTED_EDGE('',*,*,#46264,.F.);
#63479=ORIENTED_EDGE('',*,*,#46265,.F.);
#63480=ORIENTED_EDGE('',*,*,#46266,.F.);
#63481=ORIENTED_EDGE('',*,*,#46267,.F.);
#63482=ORIENTED_EDGE('',*,*,#46268,.F.);
#63483=ORIENTED_EDGE('',*,*,#46269,.F.);
#63484=ORIENTED_EDGE('',*,*,#46270,.F.);
#63485=ORIENTED_EDGE('',*,*,#46271,.F.);
#63486=ORIENTED_EDGE('',*,*,#46272,.F.);
#63487=ORIENTED_EDGE('',*,*,#46256,.F.);
#63488=ORIENTED_EDGE('',*,*,#46215,.T.);
#63489=ORIENTED_EDGE('',*,*,#46262,.T.);
#63490=ORIENTED_EDGE('',*,*,#46273,.T.);
#63491=ORIENTED_EDGE('',*,*,#46251,.F.);
#63492=ORIENTED_EDGE('',*,*,#46274,.T.);
#63493=ORIENTED_EDGE('',*,*,#46263,.F.);
#63494=ORIENTED_EDGE('',*,*,#46274,.F.);
#63495=ORIENTED_EDGE('',*,*,#46250,.F.);
#63496=ORIENTED_EDGE('',*,*,#46275,.F.);
#63497=ORIENTED_EDGE('',*,*,#46276,.F.);
#63498=ORIENTED_EDGE('',*,*,#46277,.T.);
#63499=ORIENTED_EDGE('',*,*,#46278,.T.);
#63500=ORIENTED_EDGE('',*,*,#46279,.T.);
#63501=ORIENTED_EDGE('',*,*,#46280,.T.);
#63502=ORIENTED_EDGE('',*,*,#46281,.T.);
#63503=ORIENTED_EDGE('',*,*,#46282,.T.);
#63504=ORIENTED_EDGE('',*,*,#46283,.T.);
#63505=ORIENTED_EDGE('',*,*,#46230,.F.);
#63506=ORIENTED_EDGE('',*,*,#46284,.F.);
#63507=ORIENTED_EDGE('',*,*,#46253,.T.);
#63508=ORIENTED_EDGE('',*,*,#46285,.T.);
#63509=ORIENTED_EDGE('',*,*,#46260,.T.);
#63510=ORIENTED_EDGE('',*,*,#46286,.T.);
#63511=ORIENTED_EDGE('',*,*,#46237,.T.);
#63512=ORIENTED_EDGE('',*,*,#46287,.T.);
#63513=ORIENTED_EDGE('',*,*,#46288,.F.);
#63514=ORIENTED_EDGE('',*,*,#46289,.T.);
#63515=ORIENTED_EDGE('',*,*,#46290,.F.);
#63516=ORIENTED_EDGE('',*,*,#46291,.F.);
#63517=ORIENTED_EDGE('',*,*,#46292,.F.);
#63518=ORIENTED_EDGE('',*,*,#46293,.F.);
#63519=ORIENTED_EDGE('',*,*,#46259,.T.);
#63520=ORIENTED_EDGE('',*,*,#46294,.T.);
#63521=ORIENTED_EDGE('',*,*,#46238,.F.);
#63522=ORIENTED_EDGE('',*,*,#46286,.F.);
#63523=ORIENTED_EDGE('',*,*,#46273,.F.);
#63524=ORIENTED_EDGE('',*,*,#46261,.F.);
#63525=ORIENTED_EDGE('',*,*,#46285,.F.);
#63526=ORIENTED_EDGE('',*,*,#46252,.F.);
#63527=ORIENTED_EDGE('',*,*,#46264,.T.);
#63528=ORIENTED_EDGE('',*,*,#46284,.T.);
#63529=ORIENTED_EDGE('',*,*,#46229,.F.);
#63530=ORIENTED_EDGE('',*,*,#46295,.T.);
#63531=ORIENTED_EDGE('',*,*,#46296,.F.);
#63532=ORIENTED_EDGE('',*,*,#46257,.F.);
#63533=ORIENTED_EDGE('',*,*,#46272,.T.);
#63534=ORIENTED_EDGE('',*,*,#46297,.F.);
#63535=ORIENTED_EDGE('',*,*,#46241,.T.);
#63536=ORIENTED_EDGE('',*,*,#46269,.T.);
#63537=ORIENTED_EDGE('',*,*,#46298,.F.);
#63538=ORIENTED_EDGE('',*,*,#46226,.F.);
#63539=ORIENTED_EDGE('',*,*,#46299,.T.);
#63540=ORIENTED_EDGE('',*,*,#46297,.T.);
#63541=ORIENTED_EDGE('',*,*,#46271,.T.);
#63542=ORIENTED_EDGE('',*,*,#46300,.T.);
#63543=ORIENTED_EDGE('',*,*,#46242,.T.);
#63544=ORIENTED_EDGE('',*,*,#46254,.T.);
#63545=ORIENTED_EDGE('',*,*,#46289,.F.);
#63546=ORIENTED_EDGE('',*,*,#46301,.F.);
#63547=ORIENTED_EDGE('',*,*,#46302,.T.);
#63548=ORIENTED_EDGE('',*,*,#46303,.F.);
#63549=ORIENTED_EDGE('',*,*,#46220,.T.);
#63550=ORIENTED_EDGE('',*,*,#46239,.F.);
#63551=ORIENTED_EDGE('',*,*,#46302,.F.);
#63552=ORIENTED_EDGE('',*,*,#46223,.F.);
#63553=ORIENTED_EDGE('',*,*,#46294,.F.);
#63554=ORIENTED_EDGE('',*,*,#46258,.F.);
#63555=ORIENTED_EDGE('',*,*,#46218,.T.);
#63556=ORIENTED_EDGE('',*,*,#46222,.T.);
#63557=ORIENTED_EDGE('',*,*,#46304,.F.);
#63558=ORIENTED_EDGE('',*,*,#46305,.F.);
#63559=ORIENTED_EDGE('',*,*,#46306,.F.);
#63560=ORIENTED_EDGE('',*,*,#46307,.F.);
#63561=ORIENTED_EDGE('',*,*,#46308,.T.);
#63562=ORIENTED_EDGE('',*,*,#46309,.T.);
#63563=ORIENTED_EDGE('',*,*,#46224,.T.);
#63564=ORIENTED_EDGE('',*,*,#46216,.T.);
#63565=ORIENTED_EDGE('',*,*,#46255,.T.);
#63566=ORIENTED_EDGE('',*,*,#46310,.T.);
#63567=ORIENTED_EDGE('',*,*,#46311,.T.);
#63568=ORIENTED_EDGE('',*,*,#46233,.T.);
#63569=ORIENTED_EDGE('',*,*,#46312,.T.);
#63570=ORIENTED_EDGE('',*,*,#46311,.F.);
#63571=ORIENTED_EDGE('',*,*,#46313,.T.);
#63572=ORIENTED_EDGE('',*,*,#46314,.F.);
#63573=ORIENTED_EDGE('',*,*,#46234,.T.);
#63574=ORIENTED_EDGE('',*,*,#46303,.T.);
#63575=ORIENTED_EDGE('',*,*,#46301,.T.);
#63576=ORIENTED_EDGE('',*,*,#46288,.T.);
#63577=ORIENTED_EDGE('',*,*,#46315,.T.);
#63578=ORIENTED_EDGE('',*,*,#46316,.F.);
#63579=ORIENTED_EDGE('',*,*,#46313,.F.);
#63580=ORIENTED_EDGE('',*,*,#46310,.F.);
#63581=ORIENTED_EDGE('',*,*,#46317,.T.);
#63582=ORIENTED_EDGE('',*,*,#46318,.T.);
#63583=ORIENTED_EDGE('',*,*,#46276,.T.);
#63584=ORIENTED_EDGE('',*,*,#46319,.F.);
#63585=ORIENTED_EDGE('',*,*,#46320,.F.);
#63586=ORIENTED_EDGE('',*,*,#46321,.F.);
#63587=ORIENTED_EDGE('',*,*,#46322,.T.);
#63588=ORIENTED_EDGE('',*,*,#46323,.T.);
#63589=ORIENTED_EDGE('',*,*,#46304,.T.);
#63590=ORIENTED_EDGE('',*,*,#46221,.T.);
#63591=ORIENTED_EDGE('',*,*,#46235,.T.);
#63592=ORIENTED_EDGE('',*,*,#46314,.T.);
#63593=ORIENTED_EDGE('',*,*,#46316,.T.);
#63594=ORIENTED_EDGE('',*,*,#46324,.T.);
#63595=ORIENTED_EDGE('',*,*,#46312,.F.);
#63596=ORIENTED_EDGE('',*,*,#46232,.F.);
#63597=ORIENTED_EDGE('',*,*,#46325,.F.);
#63598=ORIENTED_EDGE('',*,*,#46317,.F.);
#63599=ORIENTED_EDGE('',*,*,#46326,.F.);
#63600=ORIENTED_EDGE('',*,*,#46277,.F.);
#63601=ORIENTED_EDGE('',*,*,#46318,.F.);
#63602=ORIENTED_EDGE('',*,*,#46325,.T.);
#63603=ORIENTED_EDGE('',*,*,#46231,.F.);
#63604=ORIENTED_EDGE('',*,*,#46283,.F.);
#63605=ORIENTED_EDGE('',*,*,#46326,.T.);
#63606=ORIENTED_EDGE('',*,*,#46282,.F.);
#63607=ORIENTED_EDGE('',*,*,#46327,.F.);
#63608=ORIENTED_EDGE('',*,*,#46328,.T.);
#63609=ORIENTED_EDGE('',*,*,#46329,.T.);
#63610=ORIENTED_EDGE('',*,*,#46278,.F.);
#63611=ORIENTED_EDGE('',*,*,#46330,.T.);
#63612=ORIENTED_EDGE('',*,*,#46290,.T.);
#63613=ORIENTED_EDGE('',*,*,#46331,.T.);
#63614=ORIENTED_EDGE('',*,*,#46332,.T.);
#63615=ORIENTED_EDGE('',*,*,#46333,.T.);
#63616=ORIENTED_EDGE('',*,*,#46291,.T.);
#63617=ORIENTED_EDGE('',*,*,#46330,.F.);
#63618=ORIENTED_EDGE('',*,*,#46334,.T.);
#63619=ORIENTED_EDGE('',*,*,#46335,.T.);
#63620=ORIENTED_EDGE('',*,*,#46292,.T.);
#63621=ORIENTED_EDGE('',*,*,#46333,.F.);
#63622=ORIENTED_EDGE('',*,*,#46336,.T.);
#63623=ORIENTED_EDGE('',*,*,#46331,.F.);
#63624=ORIENTED_EDGE('',*,*,#46293,.T.);
#63625=ORIENTED_EDGE('',*,*,#46335,.F.);
#63626=ORIENTED_EDGE('',*,*,#46337,.T.);
#63627=ORIENTED_EDGE('',*,*,#46334,.F.);
#63628=ORIENTED_EDGE('',*,*,#46338,.T.);
#63629=ORIENTED_EDGE('',*,*,#46339,.T.);
#63630=ORIENTED_EDGE('',*,*,#46340,.F.);
#63631=ORIENTED_EDGE('',*,*,#46332,.F.);
#63632=ORIENTED_EDGE('',*,*,#46341,.T.);
#63633=ORIENTED_EDGE('',*,*,#46342,.T.);
#63634=ORIENTED_EDGE('',*,*,#46338,.F.);
#63635=ORIENTED_EDGE('',*,*,#46337,.F.);
#63636=ORIENTED_EDGE('',*,*,#46343,.T.);
#63637=ORIENTED_EDGE('',*,*,#46344,.T.);
#63638=ORIENTED_EDGE('',*,*,#46341,.F.);
#63639=ORIENTED_EDGE('',*,*,#46336,.F.);
#63640=ORIENTED_EDGE('',*,*,#46340,.T.);
#63641=ORIENTED_EDGE('',*,*,#46345,.T.);
#63642=ORIENTED_EDGE('',*,*,#46343,.F.);
#63643=ORIENTED_EDGE('',*,*,#46342,.F.);
#63644=ORIENTED_EDGE('',*,*,#46344,.F.);
#63645=ORIENTED_EDGE('',*,*,#46345,.F.);
#63646=ORIENTED_EDGE('',*,*,#46339,.F.);
#63647=ORIENTED_EDGE('',*,*,#46328,.F.);
#63648=ORIENTED_EDGE('',*,*,#46346,.F.);
#63649=ORIENTED_EDGE('',*,*,#46347,.F.);
#63650=ORIENTED_EDGE('',*,*,#46348,.F.);
#63651=ORIENTED_EDGE('',*,*,#46346,.T.);
#63652=ORIENTED_EDGE('',*,*,#46327,.T.);
#63653=ORIENTED_EDGE('',*,*,#46281,.F.);
#63654=ORIENTED_EDGE('',*,*,#46349,.F.);
#63655=ORIENTED_EDGE('',*,*,#46348,.T.);
#63656=ORIENTED_EDGE('',*,*,#46350,.T.);
#63657=ORIENTED_EDGE('',*,*,#46279,.F.);
#63658=ORIENTED_EDGE('',*,*,#46329,.F.);
#63659=ORIENTED_EDGE('',*,*,#46347,.T.);
#63660=ORIENTED_EDGE('',*,*,#46349,.T.);
#63661=ORIENTED_EDGE('',*,*,#46280,.F.);
#63662=ORIENTED_EDGE('',*,*,#46350,.F.);
#63663=ORIENTED_EDGE('',*,*,#46295,.F.);
#63664=ORIENTED_EDGE('',*,*,#46228,.T.);
#63665=ORIENTED_EDGE('',*,*,#46351,.T.);
#63666=ORIENTED_EDGE('',*,*,#46352,.F.);
#63667=ORIENTED_EDGE('',*,*,#46353,.F.);
#63668=ORIENTED_EDGE('',*,*,#46354,.F.);
#63669=ORIENTED_EDGE('',*,*,#46355,.F.);
#63670=ORIENTED_EDGE('',*,*,#46320,.T.);
#63671=ORIENTED_EDGE('',*,*,#46356,.T.);
#63672=ORIENTED_EDGE('',*,*,#46357,.F.);
#63673=ORIENTED_EDGE('',*,*,#46358,.F.);
#63674=ORIENTED_EDGE('',*,*,#46359,.F.);
#63675=ORIENTED_EDGE('',*,*,#46360,.T.);
#63676=ORIENTED_EDGE('',*,*,#46361,.T.);
#63677=ORIENTED_EDGE('',*,*,#46353,.T.);
#63678=ORIENTED_EDGE('',*,*,#46362,.T.);
#63679=ORIENTED_EDGE('',*,*,#46363,.T.);
#63680=ORIENTED_EDGE('',*,*,#46358,.T.);
#63681=ORIENTED_EDGE('',*,*,#46364,.T.);
#63682=ORIENTED_EDGE('',*,*,#46365,.T.);
#63683=ORIENTED_EDGE('',*,*,#46366,.T.);
#63684=ORIENTED_EDGE('',*,*,#46367,.T.);
#63685=ORIENTED_EDGE('',*,*,#46368,.T.);
#63686=ORIENTED_EDGE('',*,*,#46369,.F.);
#63687=ORIENTED_EDGE('',*,*,#46370,.T.);
#63688=ORIENTED_EDGE('',*,*,#46247,.T.);
#63689=ORIENTED_EDGE('',*,*,#46371,.T.);
#63690=ORIENTED_EDGE('',*,*,#46372,.F.);
#63691=ORIENTED_EDGE('',*,*,#46373,.T.);
#63692=ORIENTED_EDGE('',*,*,#46266,.T.);
#63693=ORIENTED_EDGE('',*,*,#46374,.T.);
#63694=ORIENTED_EDGE('',*,*,#46375,.T.);
#63695=ORIENTED_EDGE('',*,*,#46372,.T.);
#63696=ORIENTED_EDGE('',*,*,#46376,.T.);
#63697=ORIENTED_EDGE('',*,*,#46377,.T.);
#63698=ORIENTED_EDGE('',*,*,#46378,.T.);
#63699=ORIENTED_EDGE('',*,*,#46369,.T.);
#63700=ORIENTED_EDGE('',*,*,#46379,.T.);
#63701=ORIENTED_EDGE('',*,*,#46380,.T.);
#63702=ORIENTED_EDGE('',*,*,#46381,.T.);
#63703=ORIENTED_EDGE('',*,*,#46249,.T.);
#63704=ORIENTED_EDGE('',*,*,#46382,.F.);
#63705=ORIENTED_EDGE('',*,*,#46356,.F.);
#63706=ORIENTED_EDGE('',*,*,#46319,.T.);
#63707=ORIENTED_EDGE('',*,*,#46275,.T.);
#63708=ORIENTED_EDGE('',*,*,#46267,.T.);
#63709=ORIENTED_EDGE('',*,*,#46373,.F.);
#63710=ORIENTED_EDGE('',*,*,#46375,.F.);
#63711=ORIENTED_EDGE('',*,*,#46383,.T.);
#63712=ORIENTED_EDGE('',*,*,#46362,.F.);
#63713=ORIENTED_EDGE('',*,*,#46352,.T.);
#63714=ORIENTED_EDGE('',*,*,#46384,.T.);
#63715=ORIENTED_EDGE('',*,*,#46385,.F.);
#63716=ORIENTED_EDGE('',*,*,#46360,.F.);
#63717=ORIENTED_EDGE('',*,*,#46383,.F.);
#63718=ORIENTED_EDGE('',*,*,#46374,.F.);
#63719=ORIENTED_EDGE('',*,*,#46265,.T.);
#63720=ORIENTED_EDGE('',*,*,#46296,.T.);
#63721=ORIENTED_EDGE('',*,*,#46354,.T.);
#63722=ORIENTED_EDGE('',*,*,#46361,.F.);
#63723=ORIENTED_EDGE('',*,*,#46385,.T.);
#63724=ORIENTED_EDGE('',*,*,#46376,.F.);
#63725=ORIENTED_EDGE('',*,*,#46371,.F.);
#63726=ORIENTED_EDGE('',*,*,#46386,.T.);
#63727=ORIENTED_EDGE('',*,*,#46387,.T.);
#63728=ORIENTED_EDGE('',*,*,#46388,.T.);
#63729=ORIENTED_EDGE('',*,*,#46389,.T.);
#63730=ORIENTED_EDGE('',*,*,#46306,.T.);
#63731=ORIENTED_EDGE('',*,*,#46390,.T.);
#63732=ORIENTED_EDGE('',*,*,#46391,.T.);
#63733=ORIENTED_EDGE('',*,*,#46392,.T.);
#63734=ORIENTED_EDGE('',*,*,#46308,.F.);
#63735=ORIENTED_EDGE('',*,*,#46393,.T.);
#63736=ORIENTED_EDGE('',*,*,#46244,.T.);
#63737=ORIENTED_EDGE('',*,*,#46394,.T.);
#63738=ORIENTED_EDGE('',*,*,#46322,.F.);
#63739=ORIENTED_EDGE('',*,*,#46395,.F.);
#63740=ORIENTED_EDGE('',*,*,#46396,.F.);
#63741=ORIENTED_EDGE('',*,*,#46365,.F.);
#63742=ORIENTED_EDGE('',*,*,#46397,.F.);
#63743=ORIENTED_EDGE('',*,*,#46380,.F.);
#63744=ORIENTED_EDGE('',*,*,#46268,.T.);
#63745=ORIENTED_EDGE('',*,*,#46384,.F.);
#63746=ORIENTED_EDGE('',*,*,#46351,.F.);
#63747=ORIENTED_EDGE('',*,*,#46227,.F.);
#63748=ORIENTED_EDGE('',*,*,#46298,.T.);
#63749=ORIENTED_EDGE('',*,*,#46245,.T.);
#63750=ORIENTED_EDGE('',*,*,#46395,.T.);
#63751=ORIENTED_EDGE('',*,*,#46321,.T.);
#63752=ORIENTED_EDGE('',*,*,#46355,.T.);
#63753=ORIENTED_EDGE('',*,*,#46398,.T.);
#63754=ORIENTED_EDGE('',*,*,#46246,.T.);
#63755=ORIENTED_EDGE('',*,*,#46398,.F.);
#63756=ORIENTED_EDGE('',*,*,#46359,.T.);
#63757=ORIENTED_EDGE('',*,*,#46366,.F.);
#63758=ORIENTED_EDGE('',*,*,#46396,.T.);
#63759=ORIENTED_EDGE('',*,*,#46379,.F.);
#63760=ORIENTED_EDGE('',*,*,#46368,.F.);
#63761=ORIENTED_EDGE('',*,*,#46377,.F.);
#63762=ORIENTED_EDGE('',*,*,#46399,.T.);
#63763=ORIENTED_EDGE('',*,*,#46363,.F.);
#63764=ORIENTED_EDGE('',*,*,#46399,.F.);
#63765=ORIENTED_EDGE('',*,*,#46248,.T.);
#63766=ORIENTED_EDGE('',*,*,#46370,.F.);
#63767=ORIENTED_EDGE('',*,*,#46378,.F.);
#63768=ORIENTED_EDGE('',*,*,#46397,.T.);
#63769=ORIENTED_EDGE('',*,*,#46364,.F.);
#63770=ORIENTED_EDGE('',*,*,#46357,.T.);
#63771=ORIENTED_EDGE('',*,*,#46382,.T.);
#63772=ORIENTED_EDGE('',*,*,#46324,.F.);
#63773=ORIENTED_EDGE('',*,*,#46315,.F.);
#63774=ORIENTED_EDGE('',*,*,#46287,.F.);
#63775=ORIENTED_EDGE('',*,*,#46236,.F.);
#63776=ORIENTED_EDGE('',*,*,#46389,.F.);
#63777=ORIENTED_EDGE('',*,*,#46400,.F.);
#63778=ORIENTED_EDGE('',*,*,#46393,.F.);
#63779=ORIENTED_EDGE('',*,*,#46307,.T.);
#63780=ORIENTED_EDGE('',*,*,#46387,.F.);
#63781=ORIENTED_EDGE('',*,*,#46401,.T.);
#63782=ORIENTED_EDGE('',*,*,#46391,.F.);
#63783=ORIENTED_EDGE('',*,*,#46401,.F.);
#63784=ORIENTED_EDGE('',*,*,#46367,.F.);
#63785=ORIENTED_EDGE('',*,*,#46402,.T.);
#63786=ORIENTED_EDGE('',*,*,#46381,.F.);
#63787=ORIENTED_EDGE('',*,*,#46402,.F.);
#63788=ORIENTED_EDGE('',*,*,#46386,.F.);
#63789=ORIENTED_EDGE('',*,*,#46403,.T.);
#63790=ORIENTED_EDGE('',*,*,#46305,.T.);
#63791=ORIENTED_EDGE('',*,*,#46323,.F.);
#63792=ORIENTED_EDGE('',*,*,#46394,.F.);
#63793=ORIENTED_EDGE('',*,*,#46243,.T.);
#63794=ORIENTED_EDGE('',*,*,#46300,.F.);
#63795=ORIENTED_EDGE('',*,*,#46270,.T.);
#63796=ORIENTED_EDGE('',*,*,#46299,.F.);
#63797=ORIENTED_EDGE('',*,*,#46225,.F.);
#63798=ORIENTED_EDGE('',*,*,#46309,.F.);
#63799=ORIENTED_EDGE('',*,*,#46404,.T.);
#63800=ORIENTED_EDGE('',*,*,#46390,.F.);
#63801=ORIENTED_EDGE('',*,*,#46404,.F.);
#63802=ORIENTED_EDGE('',*,*,#46392,.F.);
#63803=ORIENTED_EDGE('',*,*,#46400,.T.);
#63804=ORIENTED_EDGE('',*,*,#46388,.F.);
#63805=ORIENTED_EDGE('',*,*,#46403,.F.);
#63806=ORIENTED_EDGE('',*,*,#46405,.T.);
#63807=ORIENTED_EDGE('',*,*,#46406,.T.);
#63808=ORIENTED_EDGE('',*,*,#46407,.T.);
#63809=ORIENTED_EDGE('',*,*,#46406,.F.);
#63810=ORIENTED_EDGE('',*,*,#46407,.F.);
#63811=ORIENTED_EDGE('',*,*,#46408,.T.);
#63812=ORIENTED_EDGE('',*,*,#46409,.F.);
#63813=ORIENTED_EDGE('',*,*,#46408,.F.);
#63814=ORIENTED_EDGE('',*,*,#46405,.F.);
#63815=ORIENTED_EDGE('',*,*,#46410,.T.);
#63816=ORIENTED_EDGE('',*,*,#46411,.T.);
#63817=ORIENTED_EDGE('',*,*,#46409,.T.);
#63818=ORIENTED_EDGE('',*,*,#46411,.F.);
#63819=ORIENTED_EDGE('',*,*,#46410,.F.);
#63820=ORIENTED_EDGE('',*,*,#46412,.T.);
#63821=ORIENTED_EDGE('',*,*,#46413,.T.);
#63822=ORIENTED_EDGE('',*,*,#46414,.T.);
#63823=ORIENTED_EDGE('',*,*,#46413,.F.);
#63824=ORIENTED_EDGE('',*,*,#46415,.F.);
#63825=ORIENTED_EDGE('',*,*,#46416,.T.);
#63826=ORIENTED_EDGE('',*,*,#46414,.F.);
#63827=ORIENTED_EDGE('',*,*,#46416,.F.);
#63828=ORIENTED_EDGE('',*,*,#46412,.F.);
#63829=ORIENTED_EDGE('',*,*,#46417,.T.);
#63830=ORIENTED_EDGE('',*,*,#46418,.T.);
#63831=ORIENTED_EDGE('',*,*,#46415,.T.);
#63832=ORIENTED_EDGE('',*,*,#46418,.F.);
#63833=ORIENTED_EDGE('',*,*,#46417,.F.);
#63834=ORIENTED_EDGE('',*,*,#46419,.F.);
#63835=ORIENTED_EDGE('',*,*,#46420,.T.);
#63836=ORIENTED_EDGE('',*,*,#46421,.F.);
#63837=ORIENTED_EDGE('',*,*,#46422,.F.);
#63838=ORIENTED_EDGE('',*,*,#46423,.F.);
#63839=ORIENTED_EDGE('',*,*,#46424,.T.);
#63840=ORIENTED_EDGE('',*,*,#46425,.F.);
#63841=ORIENTED_EDGE('',*,*,#46426,.F.);
#63842=ORIENTED_EDGE('',*,*,#46427,.F.);
#63843=ORIENTED_EDGE('',*,*,#46428,.T.);
#63844=ORIENTED_EDGE('',*,*,#46429,.F.);
#63845=ORIENTED_EDGE('',*,*,#46430,.F.);
#63846=ORIENTED_EDGE('',*,*,#46431,.F.);
#63847=ORIENTED_EDGE('',*,*,#46432,.T.);
#63848=ORIENTED_EDGE('',*,*,#46433,.F.);
#63849=ORIENTED_EDGE('',*,*,#46434,.F.);
#63850=ORIENTED_EDGE('',*,*,#46435,.F.);
#63851=ORIENTED_EDGE('',*,*,#46436,.T.);
#63852=ORIENTED_EDGE('',*,*,#46437,.F.);
#63853=ORIENTED_EDGE('',*,*,#46438,.F.);
#63854=ORIENTED_EDGE('',*,*,#46439,.F.);
#63855=ORIENTED_EDGE('',*,*,#46440,.T.);
#63856=ORIENTED_EDGE('',*,*,#46441,.F.);
#63857=ORIENTED_EDGE('',*,*,#46442,.F.);
#63858=ORIENTED_EDGE('',*,*,#46443,.F.);
#63859=ORIENTED_EDGE('',*,*,#46444,.T.);
#63860=ORIENTED_EDGE('',*,*,#46445,.F.);
#63861=ORIENTED_EDGE('',*,*,#46446,.F.);
#63862=ORIENTED_EDGE('',*,*,#46447,.F.);
#63863=ORIENTED_EDGE('',*,*,#46448,.T.);
#63864=ORIENTED_EDGE('',*,*,#46449,.F.);
#63865=ORIENTED_EDGE('',*,*,#46450,.F.);
#63866=ORIENTED_EDGE('',*,*,#46451,.F.);
#63867=ORIENTED_EDGE('',*,*,#46452,.T.);
#63868=ORIENTED_EDGE('',*,*,#46453,.F.);
#63869=ORIENTED_EDGE('',*,*,#46454,.F.);
#63870=ORIENTED_EDGE('',*,*,#46455,.F.);
#63871=ORIENTED_EDGE('',*,*,#46456,.T.);
#63872=ORIENTED_EDGE('',*,*,#46457,.F.);
#63873=ORIENTED_EDGE('',*,*,#46458,.F.);
#63874=ORIENTED_EDGE('',*,*,#46459,.F.);
#63875=ORIENTED_EDGE('',*,*,#46460,.T.);
#63876=ORIENTED_EDGE('',*,*,#46461,.F.);
#63877=ORIENTED_EDGE('',*,*,#46462,.F.);
#63878=ORIENTED_EDGE('',*,*,#46463,.F.);
#63879=ORIENTED_EDGE('',*,*,#46464,.T.);
#63880=ORIENTED_EDGE('',*,*,#46465,.F.);
#63881=ORIENTED_EDGE('',*,*,#46466,.F.);
#63882=ORIENTED_EDGE('',*,*,#46467,.F.);
#63883=ORIENTED_EDGE('',*,*,#46468,.T.);
#63884=ORIENTED_EDGE('',*,*,#46469,.F.);
#63885=ORIENTED_EDGE('',*,*,#46470,.F.);
#63886=ORIENTED_EDGE('',*,*,#46471,.F.);
#63887=ORIENTED_EDGE('',*,*,#46472,.T.);
#63888=ORIENTED_EDGE('',*,*,#46473,.F.);
#63889=ORIENTED_EDGE('',*,*,#46474,.F.);
#63890=ORIENTED_EDGE('',*,*,#46475,.F.);
#63891=ORIENTED_EDGE('',*,*,#46476,.T.);
#63892=ORIENTED_EDGE('',*,*,#46477,.F.);
#63893=ORIENTED_EDGE('',*,*,#46478,.F.);
#63894=ORIENTED_EDGE('',*,*,#46479,.F.);
#63895=ORIENTED_EDGE('',*,*,#46480,.T.);
#63896=ORIENTED_EDGE('',*,*,#46481,.F.);
#63897=ORIENTED_EDGE('',*,*,#46482,.F.);
#63898=ORIENTED_EDGE('',*,*,#46483,.F.);
#63899=ORIENTED_EDGE('',*,*,#46484,.T.);
#63900=ORIENTED_EDGE('',*,*,#46485,.F.);
#63901=ORIENTED_EDGE('',*,*,#46486,.F.);
#63902=ORIENTED_EDGE('',*,*,#46487,.F.);
#63903=ORIENTED_EDGE('',*,*,#46488,.T.);
#63904=ORIENTED_EDGE('',*,*,#46489,.F.);
#63905=ORIENTED_EDGE('',*,*,#46490,.F.);
#63906=ORIENTED_EDGE('',*,*,#46491,.F.);
#63907=ORIENTED_EDGE('',*,*,#46492,.T.);
#63908=ORIENTED_EDGE('',*,*,#46493,.F.);
#63909=ORIENTED_EDGE('',*,*,#46494,.F.);
#63910=ORIENTED_EDGE('',*,*,#46495,.F.);
#63911=ORIENTED_EDGE('',*,*,#46496,.T.);
#63912=ORIENTED_EDGE('',*,*,#46497,.F.);
#63913=ORIENTED_EDGE('',*,*,#46498,.F.);
#63914=ORIENTED_EDGE('',*,*,#46499,.F.);
#63915=ORIENTED_EDGE('',*,*,#46500,.T.);
#63916=ORIENTED_EDGE('',*,*,#46501,.F.);
#63917=ORIENTED_EDGE('',*,*,#46502,.F.);
#63918=ORIENTED_EDGE('',*,*,#46503,.F.);
#63919=ORIENTED_EDGE('',*,*,#46504,.T.);
#63920=ORIENTED_EDGE('',*,*,#46505,.F.);
#63921=ORIENTED_EDGE('',*,*,#46506,.F.);
#63922=ORIENTED_EDGE('',*,*,#46507,.F.);
#63923=ORIENTED_EDGE('',*,*,#46508,.T.);
#63924=ORIENTED_EDGE('',*,*,#46509,.F.);
#63925=ORIENTED_EDGE('',*,*,#46510,.F.);
#63926=ORIENTED_EDGE('',*,*,#46511,.F.);
#63927=ORIENTED_EDGE('',*,*,#46512,.T.);
#63928=ORIENTED_EDGE('',*,*,#46513,.F.);
#63929=ORIENTED_EDGE('',*,*,#46514,.F.);
#63930=ORIENTED_EDGE('',*,*,#46515,.F.);
#63931=ORIENTED_EDGE('',*,*,#46516,.T.);
#63932=ORIENTED_EDGE('',*,*,#46517,.F.);
#63933=ORIENTED_EDGE('',*,*,#46518,.F.);
#63934=ORIENTED_EDGE('',*,*,#46519,.F.);
#63935=ORIENTED_EDGE('',*,*,#46520,.T.);
#63936=ORIENTED_EDGE('',*,*,#46521,.F.);
#63937=ORIENTED_EDGE('',*,*,#46522,.F.);
#63938=ORIENTED_EDGE('',*,*,#46523,.F.);
#63939=ORIENTED_EDGE('',*,*,#46524,.T.);
#63940=ORIENTED_EDGE('',*,*,#46525,.F.);
#63941=ORIENTED_EDGE('',*,*,#46526,.F.);
#63942=ORIENTED_EDGE('',*,*,#46527,.F.);
#63943=ORIENTED_EDGE('',*,*,#46528,.T.);
#63944=ORIENTED_EDGE('',*,*,#46529,.F.);
#63945=ORIENTED_EDGE('',*,*,#46530,.F.);
#63946=ORIENTED_EDGE('',*,*,#46531,.F.);
#63947=ORIENTED_EDGE('',*,*,#46532,.T.);
#63948=ORIENTED_EDGE('',*,*,#46533,.F.);
#63949=ORIENTED_EDGE('',*,*,#46534,.F.);
#63950=ORIENTED_EDGE('',*,*,#46535,.F.);
#63951=ORIENTED_EDGE('',*,*,#46536,.T.);
#63952=ORIENTED_EDGE('',*,*,#46537,.F.);
#63953=ORIENTED_EDGE('',*,*,#46538,.F.);
#63954=ORIENTED_EDGE('',*,*,#46539,.F.);
#63955=ORIENTED_EDGE('',*,*,#46540,.T.);
#63956=ORIENTED_EDGE('',*,*,#46541,.F.);
#63957=ORIENTED_EDGE('',*,*,#46542,.F.);
#63958=ORIENTED_EDGE('',*,*,#46543,.F.);
#63959=ORIENTED_EDGE('',*,*,#46544,.T.);
#63960=ORIENTED_EDGE('',*,*,#46545,.F.);
#63961=ORIENTED_EDGE('',*,*,#46546,.F.);
#63962=ORIENTED_EDGE('',*,*,#46547,.F.);
#63963=ORIENTED_EDGE('',*,*,#46548,.T.);
#63964=ORIENTED_EDGE('',*,*,#46549,.F.);
#63965=ORIENTED_EDGE('',*,*,#46550,.F.);
#63966=ORIENTED_EDGE('',*,*,#46551,.F.);
#63967=ORIENTED_EDGE('',*,*,#46552,.T.);
#63968=ORIENTED_EDGE('',*,*,#46553,.F.);
#63969=ORIENTED_EDGE('',*,*,#46554,.F.);
#63970=ORIENTED_EDGE('',*,*,#46555,.F.);
#63971=ORIENTED_EDGE('',*,*,#46556,.T.);
#63972=ORIENTED_EDGE('',*,*,#46557,.F.);
#63973=ORIENTED_EDGE('',*,*,#46558,.F.);
#63974=ORIENTED_EDGE('',*,*,#46559,.F.);
#63975=ORIENTED_EDGE('',*,*,#46560,.T.);
#63976=ORIENTED_EDGE('',*,*,#46561,.F.);
#63977=ORIENTED_EDGE('',*,*,#46562,.F.);
#63978=ORIENTED_EDGE('',*,*,#46563,.F.);
#63979=ORIENTED_EDGE('',*,*,#46564,.T.);
#63980=ORIENTED_EDGE('',*,*,#46565,.F.);
#63981=ORIENTED_EDGE('',*,*,#46566,.F.);
#63982=ORIENTED_EDGE('',*,*,#46567,.F.);
#63983=ORIENTED_EDGE('',*,*,#46568,.T.);
#63984=ORIENTED_EDGE('',*,*,#46569,.F.);
#63985=ORIENTED_EDGE('',*,*,#46570,.F.);
#63986=ORIENTED_EDGE('',*,*,#46571,.F.);
#63987=ORIENTED_EDGE('',*,*,#46572,.T.);
#63988=ORIENTED_EDGE('',*,*,#46573,.F.);
#63989=ORIENTED_EDGE('',*,*,#46574,.F.);
#63990=ORIENTED_EDGE('',*,*,#46575,.F.);
#63991=ORIENTED_EDGE('',*,*,#46576,.T.);
#63992=ORIENTED_EDGE('',*,*,#46577,.F.);
#63993=ORIENTED_EDGE('',*,*,#46578,.F.);
#63994=ORIENTED_EDGE('',*,*,#46579,.F.);
#63995=ORIENTED_EDGE('',*,*,#46580,.T.);
#63996=ORIENTED_EDGE('',*,*,#46581,.F.);
#63997=ORIENTED_EDGE('',*,*,#46582,.F.);
#63998=ORIENTED_EDGE('',*,*,#46583,.F.);
#63999=ORIENTED_EDGE('',*,*,#46584,.T.);
#64000=ORIENTED_EDGE('',*,*,#46585,.F.);
#64001=ORIENTED_EDGE('',*,*,#46586,.F.);
#64002=ORIENTED_EDGE('',*,*,#46587,.F.);
#64003=ORIENTED_EDGE('',*,*,#46588,.T.);
#64004=ORIENTED_EDGE('',*,*,#46589,.F.);
#64005=ORIENTED_EDGE('',*,*,#46590,.F.);
#64006=ORIENTED_EDGE('',*,*,#46591,.F.);
#64007=ORIENTED_EDGE('',*,*,#46592,.T.);
#64008=ORIENTED_EDGE('',*,*,#46593,.F.);
#64009=ORIENTED_EDGE('',*,*,#46594,.F.);
#64010=ORIENTED_EDGE('',*,*,#46595,.F.);
#64011=ORIENTED_EDGE('',*,*,#46596,.T.);
#64012=ORIENTED_EDGE('',*,*,#46597,.F.);
#64013=ORIENTED_EDGE('',*,*,#46598,.F.);
#64014=ORIENTED_EDGE('',*,*,#46599,.F.);
#64015=ORIENTED_EDGE('',*,*,#46600,.T.);
#64016=ORIENTED_EDGE('',*,*,#46601,.F.);
#64017=ORIENTED_EDGE('',*,*,#46602,.F.);
#64018=ORIENTED_EDGE('',*,*,#46603,.F.);
#64019=ORIENTED_EDGE('',*,*,#46604,.T.);
#64020=ORIENTED_EDGE('',*,*,#46605,.F.);
#64021=ORIENTED_EDGE('',*,*,#46606,.F.);
#64022=ORIENTED_EDGE('',*,*,#46607,.F.);
#64023=ORIENTED_EDGE('',*,*,#46608,.T.);
#64024=ORIENTED_EDGE('',*,*,#46609,.F.);
#64025=ORIENTED_EDGE('',*,*,#46610,.F.);
#64026=ORIENTED_EDGE('',*,*,#46611,.F.);
#64027=ORIENTED_EDGE('',*,*,#46612,.T.);
#64028=ORIENTED_EDGE('',*,*,#46613,.F.);
#64029=ORIENTED_EDGE('',*,*,#46614,.F.);
#64030=ORIENTED_EDGE('',*,*,#46615,.F.);
#64031=ORIENTED_EDGE('',*,*,#46616,.T.);
#64032=ORIENTED_EDGE('',*,*,#46617,.F.);
#64033=ORIENTED_EDGE('',*,*,#46618,.F.);
#64034=ORIENTED_EDGE('',*,*,#46619,.F.);
#64035=ORIENTED_EDGE('',*,*,#46620,.T.);
#64036=ORIENTED_EDGE('',*,*,#46621,.F.);
#64037=ORIENTED_EDGE('',*,*,#46622,.F.);
#64038=ORIENTED_EDGE('',*,*,#46623,.F.);
#64039=ORIENTED_EDGE('',*,*,#46624,.T.);
#64040=ORIENTED_EDGE('',*,*,#46625,.F.);
#64041=ORIENTED_EDGE('',*,*,#46626,.F.);
#64042=ORIENTED_EDGE('',*,*,#46627,.F.);
#64043=ORIENTED_EDGE('',*,*,#46628,.T.);
#64044=ORIENTED_EDGE('',*,*,#46629,.F.);
#64045=ORIENTED_EDGE('',*,*,#46630,.F.);
#64046=ORIENTED_EDGE('',*,*,#46631,.F.);
#64047=ORIENTED_EDGE('',*,*,#46632,.T.);
#64048=ORIENTED_EDGE('',*,*,#46633,.F.);
#64049=ORIENTED_EDGE('',*,*,#46634,.F.);
#64050=ORIENTED_EDGE('',*,*,#46635,.F.);
#64051=ORIENTED_EDGE('',*,*,#46636,.T.);
#64052=ORIENTED_EDGE('',*,*,#46637,.F.);
#64053=ORIENTED_EDGE('',*,*,#46638,.F.);
#64054=ORIENTED_EDGE('',*,*,#46639,.F.);
#64055=ORIENTED_EDGE('',*,*,#46640,.T.);
#64056=ORIENTED_EDGE('',*,*,#46641,.F.);
#64057=ORIENTED_EDGE('',*,*,#46642,.F.);
#64058=ORIENTED_EDGE('',*,*,#46643,.F.);
#64059=ORIENTED_EDGE('',*,*,#46644,.T.);
#64060=ORIENTED_EDGE('',*,*,#46645,.F.);
#64061=ORIENTED_EDGE('',*,*,#46646,.F.);
#64062=ORIENTED_EDGE('',*,*,#46647,.F.);
#64063=ORIENTED_EDGE('',*,*,#46648,.T.);
#64064=ORIENTED_EDGE('',*,*,#46649,.F.);
#64065=ORIENTED_EDGE('',*,*,#46650,.F.);
#64066=ORIENTED_EDGE('',*,*,#46651,.F.);
#64067=ORIENTED_EDGE('',*,*,#46652,.T.);
#64068=ORIENTED_EDGE('',*,*,#46653,.F.);
#64069=ORIENTED_EDGE('',*,*,#46654,.F.);
#64070=ORIENTED_EDGE('',*,*,#46655,.F.);
#64071=ORIENTED_EDGE('',*,*,#46656,.T.);
#64072=ORIENTED_EDGE('',*,*,#46657,.F.);
#64073=ORIENTED_EDGE('',*,*,#46658,.F.);
#64074=ORIENTED_EDGE('',*,*,#46659,.F.);
#64075=ORIENTED_EDGE('',*,*,#46660,.T.);
#64076=ORIENTED_EDGE('',*,*,#46661,.F.);
#64077=ORIENTED_EDGE('',*,*,#46662,.F.);
#64078=ORIENTED_EDGE('',*,*,#46663,.F.);
#64079=ORIENTED_EDGE('',*,*,#46664,.T.);
#64080=ORIENTED_EDGE('',*,*,#46665,.F.);
#64081=ORIENTED_EDGE('',*,*,#46666,.F.);
#64082=ORIENTED_EDGE('',*,*,#46667,.F.);
#64083=ORIENTED_EDGE('',*,*,#46668,.T.);
#64084=ORIENTED_EDGE('',*,*,#46669,.F.);
#64085=ORIENTED_EDGE('',*,*,#46670,.F.);
#64086=ORIENTED_EDGE('',*,*,#46671,.F.);
#64087=ORIENTED_EDGE('',*,*,#46672,.T.);
#64088=ORIENTED_EDGE('',*,*,#46673,.F.);
#64089=ORIENTED_EDGE('',*,*,#46674,.F.);
#64090=ORIENTED_EDGE('',*,*,#46675,.F.);
#64091=ORIENTED_EDGE('',*,*,#46676,.T.);
#64092=ORIENTED_EDGE('',*,*,#46677,.F.);
#64093=ORIENTED_EDGE('',*,*,#46678,.F.);
#64094=ORIENTED_EDGE('',*,*,#46679,.F.);
#64095=ORIENTED_EDGE('',*,*,#46680,.T.);
#64096=ORIENTED_EDGE('',*,*,#46681,.F.);
#64097=ORIENTED_EDGE('',*,*,#46682,.F.);
#64098=ORIENTED_EDGE('',*,*,#46683,.F.);
#64099=ORIENTED_EDGE('',*,*,#46684,.T.);
#64100=ORIENTED_EDGE('',*,*,#46685,.F.);
#64101=ORIENTED_EDGE('',*,*,#46686,.F.);
#64102=ORIENTED_EDGE('',*,*,#46687,.F.);
#64103=ORIENTED_EDGE('',*,*,#46688,.T.);
#64104=ORIENTED_EDGE('',*,*,#46689,.F.);
#64105=ORIENTED_EDGE('',*,*,#46690,.F.);
#64106=ORIENTED_EDGE('',*,*,#46691,.F.);
#64107=ORIENTED_EDGE('',*,*,#46692,.T.);
#64108=ORIENTED_EDGE('',*,*,#46693,.F.);
#64109=ORIENTED_EDGE('',*,*,#46694,.F.);
#64110=ORIENTED_EDGE('',*,*,#46695,.F.);
#64111=ORIENTED_EDGE('',*,*,#46696,.T.);
#64112=ORIENTED_EDGE('',*,*,#46697,.F.);
#64113=ORIENTED_EDGE('',*,*,#46698,.F.);
#64114=ORIENTED_EDGE('',*,*,#46699,.F.);
#64115=ORIENTED_EDGE('',*,*,#46700,.T.);
#64116=ORIENTED_EDGE('',*,*,#46701,.F.);
#64117=ORIENTED_EDGE('',*,*,#46700,.F.);
#64118=ORIENTED_EDGE('',*,*,#46702,.F.);
#64119=ORIENTED_EDGE('',*,*,#46703,.F.);
#64120=ORIENTED_EDGE('',*,*,#46704,.T.);
#64121=ORIENTED_EDGE('',*,*,#46705,.F.);
#64122=ORIENTED_EDGE('',*,*,#46704,.F.);
#64123=ORIENTED_EDGE('',*,*,#46706,.F.);
#64124=ORIENTED_EDGE('',*,*,#46707,.F.);
#64125=ORIENTED_EDGE('',*,*,#46708,.T.);
#64126=ORIENTED_EDGE('',*,*,#46709,.F.);
#64127=ORIENTED_EDGE('',*,*,#46708,.F.);
#64128=ORIENTED_EDGE('',*,*,#46710,.F.);
#64129=ORIENTED_EDGE('',*,*,#46711,.F.);
#64130=ORIENTED_EDGE('',*,*,#46712,.T.);
#64131=ORIENTED_EDGE('',*,*,#46713,.F.);
#64132=ORIENTED_EDGE('',*,*,#46712,.F.);
#64133=ORIENTED_EDGE('',*,*,#46714,.F.);
#64134=ORIENTED_EDGE('',*,*,#46715,.F.);
#64135=ORIENTED_EDGE('',*,*,#46716,.T.);
#64136=ORIENTED_EDGE('',*,*,#46717,.F.);
#64137=ORIENTED_EDGE('',*,*,#46716,.F.);
#64138=ORIENTED_EDGE('',*,*,#46718,.F.);
#64139=ORIENTED_EDGE('',*,*,#46719,.T.);
#64140=ORIENTED_EDGE('',*,*,#46720,.F.);
#64141=ORIENTED_EDGE('',*,*,#46719,.F.);
#64142=ORIENTED_EDGE('',*,*,#46721,.F.);
#64143=ORIENTED_EDGE('',*,*,#46722,.T.);
#64144=ORIENTED_EDGE('',*,*,#46723,.F.);
#64145=ORIENTED_EDGE('',*,*,#46722,.F.);
#64146=ORIENTED_EDGE('',*,*,#46724,.F.);
#64147=ORIENTED_EDGE('',*,*,#46725,.F.);
#64148=ORIENTED_EDGE('',*,*,#46726,.T.);
#64149=ORIENTED_EDGE('',*,*,#46727,.F.);
#64150=ORIENTED_EDGE('',*,*,#46726,.F.);
#64151=ORIENTED_EDGE('',*,*,#46703,.T.);
#64152=ORIENTED_EDGE('',*,*,#46728,.T.);
#64153=ORIENTED_EDGE('',*,*,#46718,.T.);
#64154=ORIENTED_EDGE('',*,*,#46728,.F.);
#64155=ORIENTED_EDGE('',*,*,#46706,.T.);
#64156=ORIENTED_EDGE('',*,*,#46707,.T.);
#64157=ORIENTED_EDGE('',*,*,#46729,.T.);
#64158=ORIENTED_EDGE('',*,*,#46715,.T.);
#64159=ORIENTED_EDGE('',*,*,#46729,.F.);
#64160=ORIENTED_EDGE('',*,*,#46710,.T.);
#64161=ORIENTED_EDGE('',*,*,#46730,.F.);
#64162=ORIENTED_EDGE('',*,*,#46731,.F.);
#64163=ORIENTED_EDGE('',*,*,#46696,.F.);
#64164=ORIENTED_EDGE('',*,*,#46732,.F.);
#64165=ORIENTED_EDGE('',*,*,#46733,.F.);
#64166=ORIENTED_EDGE('',*,*,#46734,.F.);
#64167=ORIENTED_EDGE('',*,*,#46692,.F.);
#64168=ORIENTED_EDGE('',*,*,#46735,.F.);
#64169=ORIENTED_EDGE('',*,*,#46736,.F.);
#64170=ORIENTED_EDGE('',*,*,#46737,.F.);
#64171=ORIENTED_EDGE('',*,*,#46688,.F.);
#64172=ORIENTED_EDGE('',*,*,#46738,.F.);
#64173=ORIENTED_EDGE('',*,*,#46739,.F.);
#64174=ORIENTED_EDGE('',*,*,#46740,.F.);
#64175=ORIENTED_EDGE('',*,*,#46684,.F.);
#64176=ORIENTED_EDGE('',*,*,#46741,.F.);
#64177=ORIENTED_EDGE('',*,*,#46742,.F.);
#64178=ORIENTED_EDGE('',*,*,#46743,.F.);
#64179=ORIENTED_EDGE('',*,*,#46680,.F.);
#64180=ORIENTED_EDGE('',*,*,#46744,.F.);
#64181=ORIENTED_EDGE('',*,*,#46745,.F.);
#64182=ORIENTED_EDGE('',*,*,#46746,.F.);
#64183=ORIENTED_EDGE('',*,*,#46676,.F.);
#64184=ORIENTED_EDGE('',*,*,#46747,.F.);
#64185=ORIENTED_EDGE('',*,*,#46748,.F.);
#64186=ORIENTED_EDGE('',*,*,#46749,.F.);
#64187=ORIENTED_EDGE('',*,*,#46672,.F.);
#64188=ORIENTED_EDGE('',*,*,#46750,.F.);
#64189=ORIENTED_EDGE('',*,*,#46751,.F.);
#64190=ORIENTED_EDGE('',*,*,#46752,.F.);
#64191=ORIENTED_EDGE('',*,*,#46668,.F.);
#64192=ORIENTED_EDGE('',*,*,#46753,.F.);
#64193=ORIENTED_EDGE('',*,*,#46754,.F.);
#64194=ORIENTED_EDGE('',*,*,#46755,.F.);
#64195=ORIENTED_EDGE('',*,*,#46664,.F.);
#64196=ORIENTED_EDGE('',*,*,#46756,.F.);
#64197=ORIENTED_EDGE('',*,*,#46757,.F.);
#64198=ORIENTED_EDGE('',*,*,#46758,.F.);
#64199=ORIENTED_EDGE('',*,*,#46660,.F.);
#64200=ORIENTED_EDGE('',*,*,#46759,.F.);
#64201=ORIENTED_EDGE('',*,*,#46760,.F.);
#64202=ORIENTED_EDGE('',*,*,#46761,.F.);
#64203=ORIENTED_EDGE('',*,*,#46656,.F.);
#64204=ORIENTED_EDGE('',*,*,#46762,.F.);
#64205=ORIENTED_EDGE('',*,*,#46763,.F.);
#64206=ORIENTED_EDGE('',*,*,#46764,.F.);
#64207=ORIENTED_EDGE('',*,*,#46652,.F.);
#64208=ORIENTED_EDGE('',*,*,#46765,.F.);
#64209=ORIENTED_EDGE('',*,*,#46766,.F.);
#64210=ORIENTED_EDGE('',*,*,#46767,.F.);
#64211=ORIENTED_EDGE('',*,*,#46648,.F.);
#64212=ORIENTED_EDGE('',*,*,#46768,.F.);
#64213=ORIENTED_EDGE('',*,*,#46769,.F.);
#64214=ORIENTED_EDGE('',*,*,#46770,.F.);
#64215=ORIENTED_EDGE('',*,*,#46644,.F.);
#64216=ORIENTED_EDGE('',*,*,#46771,.F.);
#64217=ORIENTED_EDGE('',*,*,#46772,.F.);
#64218=ORIENTED_EDGE('',*,*,#46773,.F.);
#64219=ORIENTED_EDGE('',*,*,#46640,.F.);
#64220=ORIENTED_EDGE('',*,*,#46774,.F.);
#64221=ORIENTED_EDGE('',*,*,#46775,.F.);
#64222=ORIENTED_EDGE('',*,*,#46776,.F.);
#64223=ORIENTED_EDGE('',*,*,#46636,.F.);
#64224=ORIENTED_EDGE('',*,*,#46777,.F.);
#64225=ORIENTED_EDGE('',*,*,#46778,.F.);
#64226=ORIENTED_EDGE('',*,*,#46779,.F.);
#64227=ORIENTED_EDGE('',*,*,#46632,.F.);
#64228=ORIENTED_EDGE('',*,*,#46780,.F.);
#64229=ORIENTED_EDGE('',*,*,#46781,.F.);
#64230=ORIENTED_EDGE('',*,*,#46782,.F.);
#64231=ORIENTED_EDGE('',*,*,#46628,.F.);
#64232=ORIENTED_EDGE('',*,*,#46783,.F.);
#64233=ORIENTED_EDGE('',*,*,#46784,.F.);
#64234=ORIENTED_EDGE('',*,*,#46785,.F.);
#64235=ORIENTED_EDGE('',*,*,#46624,.F.);
#64236=ORIENTED_EDGE('',*,*,#46786,.F.);
#64237=ORIENTED_EDGE('',*,*,#46787,.F.);
#64238=ORIENTED_EDGE('',*,*,#46788,.F.);
#64239=ORIENTED_EDGE('',*,*,#46620,.F.);
#64240=ORIENTED_EDGE('',*,*,#46789,.F.);
#64241=ORIENTED_EDGE('',*,*,#46790,.F.);
#64242=ORIENTED_EDGE('',*,*,#46791,.F.);
#64243=ORIENTED_EDGE('',*,*,#46616,.F.);
#64244=ORIENTED_EDGE('',*,*,#46792,.F.);
#64245=ORIENTED_EDGE('',*,*,#46793,.F.);
#64246=ORIENTED_EDGE('',*,*,#46794,.F.);
#64247=ORIENTED_EDGE('',*,*,#46612,.F.);
#64248=ORIENTED_EDGE('',*,*,#46795,.F.);
#64249=ORIENTED_EDGE('',*,*,#46796,.F.);
#64250=ORIENTED_EDGE('',*,*,#46797,.F.);
#64251=ORIENTED_EDGE('',*,*,#46608,.F.);
#64252=ORIENTED_EDGE('',*,*,#46798,.F.);
#64253=ORIENTED_EDGE('',*,*,#46799,.F.);
#64254=ORIENTED_EDGE('',*,*,#46800,.F.);
#64255=ORIENTED_EDGE('',*,*,#46604,.F.);
#64256=ORIENTED_EDGE('',*,*,#46801,.F.);
#64257=ORIENTED_EDGE('',*,*,#46802,.F.);
#64258=ORIENTED_EDGE('',*,*,#46803,.F.);
#64259=ORIENTED_EDGE('',*,*,#46600,.F.);
#64260=ORIENTED_EDGE('',*,*,#46804,.F.);
#64261=ORIENTED_EDGE('',*,*,#46805,.F.);
#64262=ORIENTED_EDGE('',*,*,#46806,.F.);
#64263=ORIENTED_EDGE('',*,*,#46596,.F.);
#64264=ORIENTED_EDGE('',*,*,#46807,.F.);
#64265=ORIENTED_EDGE('',*,*,#46808,.F.);
#64266=ORIENTED_EDGE('',*,*,#46809,.F.);
#64267=ORIENTED_EDGE('',*,*,#46592,.F.);
#64268=ORIENTED_EDGE('',*,*,#46810,.F.);
#64269=ORIENTED_EDGE('',*,*,#46811,.F.);
#64270=ORIENTED_EDGE('',*,*,#46812,.F.);
#64271=ORIENTED_EDGE('',*,*,#46588,.F.);
#64272=ORIENTED_EDGE('',*,*,#46813,.F.);
#64273=ORIENTED_EDGE('',*,*,#46814,.F.);
#64274=ORIENTED_EDGE('',*,*,#46815,.F.);
#64275=ORIENTED_EDGE('',*,*,#46584,.F.);
#64276=ORIENTED_EDGE('',*,*,#46816,.F.);
#64277=ORIENTED_EDGE('',*,*,#46817,.F.);
#64278=ORIENTED_EDGE('',*,*,#46818,.F.);
#64279=ORIENTED_EDGE('',*,*,#46580,.F.);
#64280=ORIENTED_EDGE('',*,*,#46819,.F.);
#64281=ORIENTED_EDGE('',*,*,#46820,.F.);
#64282=ORIENTED_EDGE('',*,*,#46821,.F.);
#64283=ORIENTED_EDGE('',*,*,#46576,.F.);
#64284=ORIENTED_EDGE('',*,*,#46822,.F.);
#64285=ORIENTED_EDGE('',*,*,#46823,.F.);
#64286=ORIENTED_EDGE('',*,*,#46824,.F.);
#64287=ORIENTED_EDGE('',*,*,#46572,.F.);
#64288=ORIENTED_EDGE('',*,*,#46825,.F.);
#64289=ORIENTED_EDGE('',*,*,#46826,.F.);
#64290=ORIENTED_EDGE('',*,*,#46827,.F.);
#64291=ORIENTED_EDGE('',*,*,#46568,.F.);
#64292=ORIENTED_EDGE('',*,*,#46828,.F.);
#64293=ORIENTED_EDGE('',*,*,#46829,.F.);
#64294=ORIENTED_EDGE('',*,*,#46830,.F.);
#64295=ORIENTED_EDGE('',*,*,#46564,.F.);
#64296=ORIENTED_EDGE('',*,*,#46831,.F.);
#64297=ORIENTED_EDGE('',*,*,#46832,.F.);
#64298=ORIENTED_EDGE('',*,*,#46833,.F.);
#64299=ORIENTED_EDGE('',*,*,#46560,.F.);
#64300=ORIENTED_EDGE('',*,*,#46834,.F.);
#64301=ORIENTED_EDGE('',*,*,#46835,.F.);
#64302=ORIENTED_EDGE('',*,*,#46836,.T.);
#64303=ORIENTED_EDGE('',*,*,#46837,.T.);
#64304=ORIENTED_EDGE('',*,*,#46836,.F.);
#64305=ORIENTED_EDGE('',*,*,#46838,.F.);
#64306=ORIENTED_EDGE('',*,*,#46839,.F.);
#64307=ORIENTED_EDGE('',*,*,#46556,.F.);
#64308=ORIENTED_EDGE('',*,*,#46840,.F.);
#64309=ORIENTED_EDGE('',*,*,#46841,.F.);
#64310=ORIENTED_EDGE('',*,*,#46842,.F.);
#64311=ORIENTED_EDGE('',*,*,#46552,.F.);
#64312=ORIENTED_EDGE('',*,*,#46843,.F.);
#64313=ORIENTED_EDGE('',*,*,#46844,.F.);
#64314=ORIENTED_EDGE('',*,*,#46845,.F.);
#64315=ORIENTED_EDGE('',*,*,#46548,.F.);
#64316=ORIENTED_EDGE('',*,*,#46846,.F.);
#64317=ORIENTED_EDGE('',*,*,#46847,.F.);
#64318=ORIENTED_EDGE('',*,*,#46848,.F.);
#64319=ORIENTED_EDGE('',*,*,#46544,.F.);
#64320=ORIENTED_EDGE('',*,*,#46849,.F.);
#64321=ORIENTED_EDGE('',*,*,#46850,.F.);
#64322=ORIENTED_EDGE('',*,*,#46851,.F.);
#64323=ORIENTED_EDGE('',*,*,#46540,.F.);
#64324=ORIENTED_EDGE('',*,*,#46852,.F.);
#64325=ORIENTED_EDGE('',*,*,#46853,.F.);
#64326=ORIENTED_EDGE('',*,*,#46854,.F.);
#64327=ORIENTED_EDGE('',*,*,#46536,.F.);
#64328=ORIENTED_EDGE('',*,*,#46855,.F.);
#64329=ORIENTED_EDGE('',*,*,#46856,.F.);
#64330=ORIENTED_EDGE('',*,*,#46857,.F.);
#64331=ORIENTED_EDGE('',*,*,#46532,.F.);
#64332=ORIENTED_EDGE('',*,*,#46858,.F.);
#64333=ORIENTED_EDGE('',*,*,#46859,.F.);
#64334=ORIENTED_EDGE('',*,*,#46860,.F.);
#64335=ORIENTED_EDGE('',*,*,#46528,.F.);
#64336=ORIENTED_EDGE('',*,*,#46861,.F.);
#64337=ORIENTED_EDGE('',*,*,#46862,.F.);
#64338=ORIENTED_EDGE('',*,*,#46863,.F.);
#64339=ORIENTED_EDGE('',*,*,#46524,.F.);
#64340=ORIENTED_EDGE('',*,*,#46864,.F.);
#64341=ORIENTED_EDGE('',*,*,#46865,.F.);
#64342=ORIENTED_EDGE('',*,*,#46866,.F.);
#64343=ORIENTED_EDGE('',*,*,#46520,.F.);
#64344=ORIENTED_EDGE('',*,*,#46867,.F.);
#64345=ORIENTED_EDGE('',*,*,#46868,.F.);
#64346=ORIENTED_EDGE('',*,*,#46869,.F.);
#64347=ORIENTED_EDGE('',*,*,#46516,.F.);
#64348=ORIENTED_EDGE('',*,*,#46870,.F.);
#64349=ORIENTED_EDGE('',*,*,#46871,.F.);
#64350=ORIENTED_EDGE('',*,*,#46872,.F.);
#64351=ORIENTED_EDGE('',*,*,#46512,.F.);
#64352=ORIENTED_EDGE('',*,*,#46873,.F.);
#64353=ORIENTED_EDGE('',*,*,#46874,.F.);
#64354=ORIENTED_EDGE('',*,*,#46875,.F.);
#64355=ORIENTED_EDGE('',*,*,#46508,.F.);
#64356=ORIENTED_EDGE('',*,*,#46876,.F.);
#64357=ORIENTED_EDGE('',*,*,#46877,.F.);
#64358=ORIENTED_EDGE('',*,*,#46878,.F.);
#64359=ORIENTED_EDGE('',*,*,#46504,.F.);
#64360=ORIENTED_EDGE('',*,*,#46879,.F.);
#64361=ORIENTED_EDGE('',*,*,#46880,.F.);
#64362=ORIENTED_EDGE('',*,*,#46881,.F.);
#64363=ORIENTED_EDGE('',*,*,#46500,.F.);
#64364=ORIENTED_EDGE('',*,*,#46882,.F.);
#64365=ORIENTED_EDGE('',*,*,#46883,.F.);
#64366=ORIENTED_EDGE('',*,*,#46884,.F.);
#64367=ORIENTED_EDGE('',*,*,#46496,.F.);
#64368=ORIENTED_EDGE('',*,*,#46885,.F.);
#64369=ORIENTED_EDGE('',*,*,#46886,.F.);
#64370=ORIENTED_EDGE('',*,*,#46887,.F.);
#64371=ORIENTED_EDGE('',*,*,#46492,.F.);
#64372=ORIENTED_EDGE('',*,*,#46888,.F.);
#64373=ORIENTED_EDGE('',*,*,#46889,.F.);
#64374=ORIENTED_EDGE('',*,*,#46890,.F.);
#64375=ORIENTED_EDGE('',*,*,#46488,.F.);
#64376=ORIENTED_EDGE('',*,*,#46891,.F.);
#64377=ORIENTED_EDGE('',*,*,#46892,.F.);
#64378=ORIENTED_EDGE('',*,*,#46893,.F.);
#64379=ORIENTED_EDGE('',*,*,#46484,.F.);
#64380=ORIENTED_EDGE('',*,*,#46894,.F.);
#64381=ORIENTED_EDGE('',*,*,#46895,.F.);
#64382=ORIENTED_EDGE('',*,*,#46896,.F.);
#64383=ORIENTED_EDGE('',*,*,#46480,.F.);
#64384=ORIENTED_EDGE('',*,*,#46897,.F.);
#64385=ORIENTED_EDGE('',*,*,#46898,.F.);
#64386=ORIENTED_EDGE('',*,*,#46899,.F.);
#64387=ORIENTED_EDGE('',*,*,#46476,.F.);
#64388=ORIENTED_EDGE('',*,*,#46900,.F.);
#64389=ORIENTED_EDGE('',*,*,#46901,.F.);
#64390=ORIENTED_EDGE('',*,*,#46902,.F.);
#64391=ORIENTED_EDGE('',*,*,#46472,.F.);
#64392=ORIENTED_EDGE('',*,*,#46903,.F.);
#64393=ORIENTED_EDGE('',*,*,#46904,.F.);
#64394=ORIENTED_EDGE('',*,*,#46905,.F.);
#64395=ORIENTED_EDGE('',*,*,#46468,.F.);
#64396=ORIENTED_EDGE('',*,*,#46906,.F.);
#64397=ORIENTED_EDGE('',*,*,#46907,.F.);
#64398=ORIENTED_EDGE('',*,*,#46908,.F.);
#64399=ORIENTED_EDGE('',*,*,#46464,.F.);
#64400=ORIENTED_EDGE('',*,*,#46909,.F.);
#64401=ORIENTED_EDGE('',*,*,#46910,.F.);
#64402=ORIENTED_EDGE('',*,*,#46911,.F.);
#64403=ORIENTED_EDGE('',*,*,#46460,.F.);
#64404=ORIENTED_EDGE('',*,*,#46912,.F.);
#64405=ORIENTED_EDGE('',*,*,#46913,.F.);
#64406=ORIENTED_EDGE('',*,*,#46914,.F.);
#64407=ORIENTED_EDGE('',*,*,#46456,.F.);
#64408=ORIENTED_EDGE('',*,*,#46915,.F.);
#64409=ORIENTED_EDGE('',*,*,#46916,.F.);
#64410=ORIENTED_EDGE('',*,*,#46917,.F.);
#64411=ORIENTED_EDGE('',*,*,#46452,.F.);
#64412=ORIENTED_EDGE('',*,*,#46918,.F.);
#64413=ORIENTED_EDGE('',*,*,#46919,.F.);
#64414=ORIENTED_EDGE('',*,*,#46920,.F.);
#64415=ORIENTED_EDGE('',*,*,#46448,.F.);
#64416=ORIENTED_EDGE('',*,*,#46921,.F.);
#64417=ORIENTED_EDGE('',*,*,#46922,.F.);
#64418=ORIENTED_EDGE('',*,*,#46923,.F.);
#64419=ORIENTED_EDGE('',*,*,#46444,.F.);
#64420=ORIENTED_EDGE('',*,*,#46924,.F.);
#64421=ORIENTED_EDGE('',*,*,#46925,.F.);
#64422=ORIENTED_EDGE('',*,*,#46926,.F.);
#64423=ORIENTED_EDGE('',*,*,#46440,.F.);
#64424=ORIENTED_EDGE('',*,*,#46927,.F.);
#64425=ORIENTED_EDGE('',*,*,#46928,.F.);
#64426=ORIENTED_EDGE('',*,*,#46929,.F.);
#64427=ORIENTED_EDGE('',*,*,#46436,.F.);
#64428=ORIENTED_EDGE('',*,*,#46930,.F.);
#64429=ORIENTED_EDGE('',*,*,#46931,.F.);
#64430=ORIENTED_EDGE('',*,*,#46932,.F.);
#64431=ORIENTED_EDGE('',*,*,#46432,.F.);
#64432=ORIENTED_EDGE('',*,*,#46933,.F.);
#64433=ORIENTED_EDGE('',*,*,#46934,.F.);
#64434=ORIENTED_EDGE('',*,*,#46935,.F.);
#64435=ORIENTED_EDGE('',*,*,#46428,.F.);
#64436=ORIENTED_EDGE('',*,*,#46936,.F.);
#64437=ORIENTED_EDGE('',*,*,#46937,.F.);
#64438=ORIENTED_EDGE('',*,*,#46938,.F.);
#64439=ORIENTED_EDGE('',*,*,#46424,.F.);
#64440=ORIENTED_EDGE('',*,*,#46939,.F.);
#64441=ORIENTED_EDGE('',*,*,#46940,.F.);
#64442=ORIENTED_EDGE('',*,*,#46941,.F.);
#64443=ORIENTED_EDGE('',*,*,#46420,.F.);
#64444=ORIENTED_EDGE('',*,*,#46942,.F.);
#64445=ORIENTED_EDGE('',*,*,#46711,.T.);
#64446=ORIENTED_EDGE('',*,*,#46943,.T.);
#64447=ORIENTED_EDGE('',*,*,#46944,.F.);
#64448=ORIENTED_EDGE('',*,*,#46945,.F.);
#64449=ORIENTED_EDGE('',*,*,#46562,.T.);
#64450=ORIENTED_EDGE('',*,*,#46946,.F.);
#64451=ORIENTED_EDGE('',*,*,#46947,.F.);
#64452=ORIENTED_EDGE('',*,*,#46948,.F.);
#64453=ORIENTED_EDGE('',*,*,#46566,.T.);
#64454=ORIENTED_EDGE('',*,*,#46949,.F.);
#64455=ORIENTED_EDGE('',*,*,#46950,.F.);
#64456=ORIENTED_EDGE('',*,*,#46951,.F.);
#64457=ORIENTED_EDGE('',*,*,#46570,.T.);
#64458=ORIENTED_EDGE('',*,*,#46952,.F.);
#64459=ORIENTED_EDGE('',*,*,#46953,.F.);
#64460=ORIENTED_EDGE('',*,*,#46954,.F.);
#64461=ORIENTED_EDGE('',*,*,#46574,.T.);
#64462=ORIENTED_EDGE('',*,*,#46955,.F.);
#64463=ORIENTED_EDGE('',*,*,#46956,.F.);
#64464=ORIENTED_EDGE('',*,*,#46957,.F.);
#64465=ORIENTED_EDGE('',*,*,#46578,.T.);
#64466=ORIENTED_EDGE('',*,*,#46958,.F.);
#64467=ORIENTED_EDGE('',*,*,#46959,.F.);
#64468=ORIENTED_EDGE('',*,*,#46960,.F.);
#64469=ORIENTED_EDGE('',*,*,#46582,.T.);
#64470=ORIENTED_EDGE('',*,*,#46961,.F.);
#64471=ORIENTED_EDGE('',*,*,#46962,.F.);
#64472=ORIENTED_EDGE('',*,*,#46963,.F.);
#64473=ORIENTED_EDGE('',*,*,#46586,.T.);
#64474=ORIENTED_EDGE('',*,*,#46964,.F.);
#64475=ORIENTED_EDGE('',*,*,#46965,.F.);
#64476=ORIENTED_EDGE('',*,*,#46966,.F.);
#64477=ORIENTED_EDGE('',*,*,#46590,.T.);
#64478=ORIENTED_EDGE('',*,*,#46967,.F.);
#64479=ORIENTED_EDGE('',*,*,#46968,.F.);
#64480=ORIENTED_EDGE('',*,*,#46969,.F.);
#64481=ORIENTED_EDGE('',*,*,#46594,.T.);
#64482=ORIENTED_EDGE('',*,*,#46970,.F.);
#64483=ORIENTED_EDGE('',*,*,#46971,.F.);
#64484=ORIENTED_EDGE('',*,*,#46972,.F.);
#64485=ORIENTED_EDGE('',*,*,#46598,.T.);
#64486=ORIENTED_EDGE('',*,*,#46973,.F.);
#64487=ORIENTED_EDGE('',*,*,#46974,.F.);
#64488=ORIENTED_EDGE('',*,*,#46975,.F.);
#64489=ORIENTED_EDGE('',*,*,#46602,.T.);
#64490=ORIENTED_EDGE('',*,*,#46976,.F.);
#64491=ORIENTED_EDGE('',*,*,#46977,.F.);
#64492=ORIENTED_EDGE('',*,*,#46978,.F.);
#64493=ORIENTED_EDGE('',*,*,#46606,.T.);
#64494=ORIENTED_EDGE('',*,*,#46979,.F.);
#64495=ORIENTED_EDGE('',*,*,#46980,.F.);
#64496=ORIENTED_EDGE('',*,*,#46981,.F.);
#64497=ORIENTED_EDGE('',*,*,#46610,.T.);
#64498=ORIENTED_EDGE('',*,*,#46982,.F.);
#64499=ORIENTED_EDGE('',*,*,#46983,.F.);
#64500=ORIENTED_EDGE('',*,*,#46984,.F.);
#64501=ORIENTED_EDGE('',*,*,#46614,.T.);
#64502=ORIENTED_EDGE('',*,*,#46985,.F.);
#64503=ORIENTED_EDGE('',*,*,#46986,.F.);
#64504=ORIENTED_EDGE('',*,*,#46987,.F.);
#64505=ORIENTED_EDGE('',*,*,#46618,.T.);
#64506=ORIENTED_EDGE('',*,*,#46988,.F.);
#64507=ORIENTED_EDGE('',*,*,#46989,.F.);
#64508=ORIENTED_EDGE('',*,*,#46990,.F.);
#64509=ORIENTED_EDGE('',*,*,#46622,.T.);
#64510=ORIENTED_EDGE('',*,*,#46991,.F.);
#64511=ORIENTED_EDGE('',*,*,#46992,.F.);
#64512=ORIENTED_EDGE('',*,*,#46993,.F.);
#64513=ORIENTED_EDGE('',*,*,#46626,.T.);
#64514=ORIENTED_EDGE('',*,*,#46994,.F.);
#64515=ORIENTED_EDGE('',*,*,#46995,.F.);
#64516=ORIENTED_EDGE('',*,*,#46996,.F.);
#64517=ORIENTED_EDGE('',*,*,#46630,.T.);
#64518=ORIENTED_EDGE('',*,*,#46997,.F.);
#64519=ORIENTED_EDGE('',*,*,#46998,.F.);
#64520=ORIENTED_EDGE('',*,*,#46999,.F.);
#64521=ORIENTED_EDGE('',*,*,#46634,.T.);
#64522=ORIENTED_EDGE('',*,*,#47000,.F.);
#64523=ORIENTED_EDGE('',*,*,#47001,.F.);
#64524=ORIENTED_EDGE('',*,*,#47002,.F.);
#64525=ORIENTED_EDGE('',*,*,#46638,.T.);
#64526=ORIENTED_EDGE('',*,*,#47003,.F.);
#64527=ORIENTED_EDGE('',*,*,#47004,.F.);
#64528=ORIENTED_EDGE('',*,*,#47005,.F.);
#64529=ORIENTED_EDGE('',*,*,#46642,.T.);
#64530=ORIENTED_EDGE('',*,*,#47006,.F.);
#64531=ORIENTED_EDGE('',*,*,#47007,.F.);
#64532=ORIENTED_EDGE('',*,*,#47008,.F.);
#64533=ORIENTED_EDGE('',*,*,#46646,.T.);
#64534=ORIENTED_EDGE('',*,*,#47009,.F.);
#64535=ORIENTED_EDGE('',*,*,#47010,.F.);
#64536=ORIENTED_EDGE('',*,*,#47011,.F.);
#64537=ORIENTED_EDGE('',*,*,#46650,.T.);
#64538=ORIENTED_EDGE('',*,*,#47012,.F.);
#64539=ORIENTED_EDGE('',*,*,#47013,.F.);
#64540=ORIENTED_EDGE('',*,*,#47014,.F.);
#64541=ORIENTED_EDGE('',*,*,#46654,.T.);
#64542=ORIENTED_EDGE('',*,*,#47015,.F.);
#64543=ORIENTED_EDGE('',*,*,#47016,.F.);
#64544=ORIENTED_EDGE('',*,*,#47017,.F.);
#64545=ORIENTED_EDGE('',*,*,#46658,.T.);
#64546=ORIENTED_EDGE('',*,*,#47018,.F.);
#64547=ORIENTED_EDGE('',*,*,#47019,.F.);
#64548=ORIENTED_EDGE('',*,*,#47020,.F.);
#64549=ORIENTED_EDGE('',*,*,#46662,.T.);
#64550=ORIENTED_EDGE('',*,*,#47021,.F.);
#64551=ORIENTED_EDGE('',*,*,#47022,.F.);
#64552=ORIENTED_EDGE('',*,*,#47023,.F.);
#64553=ORIENTED_EDGE('',*,*,#46666,.T.);
#64554=ORIENTED_EDGE('',*,*,#47024,.F.);
#64555=ORIENTED_EDGE('',*,*,#47025,.F.);
#64556=ORIENTED_EDGE('',*,*,#47026,.F.);
#64557=ORIENTED_EDGE('',*,*,#46670,.T.);
#64558=ORIENTED_EDGE('',*,*,#47027,.F.);
#64559=ORIENTED_EDGE('',*,*,#47028,.F.);
#64560=ORIENTED_EDGE('',*,*,#47029,.F.);
#64561=ORIENTED_EDGE('',*,*,#46674,.T.);
#64562=ORIENTED_EDGE('',*,*,#47030,.F.);
#64563=ORIENTED_EDGE('',*,*,#47031,.F.);
#64564=ORIENTED_EDGE('',*,*,#47032,.F.);
#64565=ORIENTED_EDGE('',*,*,#46678,.T.);
#64566=ORIENTED_EDGE('',*,*,#47033,.F.);
#64567=ORIENTED_EDGE('',*,*,#47034,.F.);
#64568=ORIENTED_EDGE('',*,*,#47035,.F.);
#64569=ORIENTED_EDGE('',*,*,#46682,.T.);
#64570=ORIENTED_EDGE('',*,*,#47036,.F.);
#64571=ORIENTED_EDGE('',*,*,#47037,.F.);
#64572=ORIENTED_EDGE('',*,*,#47038,.F.);
#64573=ORIENTED_EDGE('',*,*,#46686,.T.);
#64574=ORIENTED_EDGE('',*,*,#47039,.F.);
#64575=ORIENTED_EDGE('',*,*,#47040,.F.);
#64576=ORIENTED_EDGE('',*,*,#47041,.F.);
#64577=ORIENTED_EDGE('',*,*,#46690,.T.);
#64578=ORIENTED_EDGE('',*,*,#47042,.F.);
#64579=ORIENTED_EDGE('',*,*,#47043,.F.);
#64580=ORIENTED_EDGE('',*,*,#47044,.F.);
#64581=ORIENTED_EDGE('',*,*,#46694,.T.);
#64582=ORIENTED_EDGE('',*,*,#47045,.F.);
#64583=ORIENTED_EDGE('',*,*,#47046,.F.);
#64584=ORIENTED_EDGE('',*,*,#47047,.F.);
#64585=ORIENTED_EDGE('',*,*,#46698,.T.);
#64586=ORIENTED_EDGE('',*,*,#47048,.F.);
#64587=ORIENTED_EDGE('',*,*,#47049,.F.);
#64588=ORIENTED_EDGE('',*,*,#47050,.F.);
#64589=ORIENTED_EDGE('',*,*,#46422,.T.);
#64590=ORIENTED_EDGE('',*,*,#47051,.F.);
#64591=ORIENTED_EDGE('',*,*,#47052,.F.);
#64592=ORIENTED_EDGE('',*,*,#47053,.F.);
#64593=ORIENTED_EDGE('',*,*,#46426,.T.);
#64594=ORIENTED_EDGE('',*,*,#47054,.F.);
#64595=ORIENTED_EDGE('',*,*,#47055,.F.);
#64596=ORIENTED_EDGE('',*,*,#47056,.F.);
#64597=ORIENTED_EDGE('',*,*,#46430,.T.);
#64598=ORIENTED_EDGE('',*,*,#47057,.F.);
#64599=ORIENTED_EDGE('',*,*,#47058,.F.);
#64600=ORIENTED_EDGE('',*,*,#47059,.F.);
#64601=ORIENTED_EDGE('',*,*,#46434,.T.);
#64602=ORIENTED_EDGE('',*,*,#47060,.F.);
#64603=ORIENTED_EDGE('',*,*,#47061,.F.);
#64604=ORIENTED_EDGE('',*,*,#47062,.F.);
#64605=ORIENTED_EDGE('',*,*,#46438,.T.);
#64606=ORIENTED_EDGE('',*,*,#47063,.F.);
#64607=ORIENTED_EDGE('',*,*,#47064,.F.);
#64608=ORIENTED_EDGE('',*,*,#47065,.F.);
#64609=ORIENTED_EDGE('',*,*,#46442,.T.);
#64610=ORIENTED_EDGE('',*,*,#47066,.F.);
#64611=ORIENTED_EDGE('',*,*,#47067,.F.);
#64612=ORIENTED_EDGE('',*,*,#47068,.F.);
#64613=ORIENTED_EDGE('',*,*,#46446,.T.);
#64614=ORIENTED_EDGE('',*,*,#47069,.F.);
#64615=ORIENTED_EDGE('',*,*,#47070,.F.);
#64616=ORIENTED_EDGE('',*,*,#47071,.F.);
#64617=ORIENTED_EDGE('',*,*,#46450,.T.);
#64618=ORIENTED_EDGE('',*,*,#47072,.F.);
#64619=ORIENTED_EDGE('',*,*,#47073,.F.);
#64620=ORIENTED_EDGE('',*,*,#47074,.F.);
#64621=ORIENTED_EDGE('',*,*,#46454,.T.);
#64622=ORIENTED_EDGE('',*,*,#47075,.F.);
#64623=ORIENTED_EDGE('',*,*,#47076,.F.);
#64624=ORIENTED_EDGE('',*,*,#47077,.F.);
#64625=ORIENTED_EDGE('',*,*,#46458,.T.);
#64626=ORIENTED_EDGE('',*,*,#47078,.F.);
#64627=ORIENTED_EDGE('',*,*,#47079,.F.);
#64628=ORIENTED_EDGE('',*,*,#47080,.F.);
#64629=ORIENTED_EDGE('',*,*,#46462,.T.);
#64630=ORIENTED_EDGE('',*,*,#47081,.F.);
#64631=ORIENTED_EDGE('',*,*,#47082,.F.);
#64632=ORIENTED_EDGE('',*,*,#47083,.F.);
#64633=ORIENTED_EDGE('',*,*,#46466,.T.);
#64634=ORIENTED_EDGE('',*,*,#47084,.F.);
#64635=ORIENTED_EDGE('',*,*,#47085,.F.);
#64636=ORIENTED_EDGE('',*,*,#47086,.F.);
#64637=ORIENTED_EDGE('',*,*,#46470,.T.);
#64638=ORIENTED_EDGE('',*,*,#47087,.F.);
#64639=ORIENTED_EDGE('',*,*,#47088,.F.);
#64640=ORIENTED_EDGE('',*,*,#47089,.F.);
#64641=ORIENTED_EDGE('',*,*,#46474,.T.);
#64642=ORIENTED_EDGE('',*,*,#47090,.F.);
#64643=ORIENTED_EDGE('',*,*,#47091,.F.);
#64644=ORIENTED_EDGE('',*,*,#47092,.F.);
#64645=ORIENTED_EDGE('',*,*,#46478,.T.);
#64646=ORIENTED_EDGE('',*,*,#47093,.F.);
#64647=ORIENTED_EDGE('',*,*,#47094,.F.);
#64648=ORIENTED_EDGE('',*,*,#47095,.F.);
#64649=ORIENTED_EDGE('',*,*,#46482,.T.);
#64650=ORIENTED_EDGE('',*,*,#47096,.F.);
#64651=ORIENTED_EDGE('',*,*,#47097,.F.);
#64652=ORIENTED_EDGE('',*,*,#47098,.F.);
#64653=ORIENTED_EDGE('',*,*,#46486,.T.);
#64654=ORIENTED_EDGE('',*,*,#47099,.F.);
#64655=ORIENTED_EDGE('',*,*,#47100,.F.);
#64656=ORIENTED_EDGE('',*,*,#47101,.F.);
#64657=ORIENTED_EDGE('',*,*,#46490,.T.);
#64658=ORIENTED_EDGE('',*,*,#47102,.F.);
#64659=ORIENTED_EDGE('',*,*,#47103,.F.);
#64660=ORIENTED_EDGE('',*,*,#47104,.F.);
#64661=ORIENTED_EDGE('',*,*,#46494,.T.);
#64662=ORIENTED_EDGE('',*,*,#47105,.F.);
#64663=ORIENTED_EDGE('',*,*,#47106,.F.);
#64664=ORIENTED_EDGE('',*,*,#47107,.F.);
#64665=ORIENTED_EDGE('',*,*,#46498,.T.);
#64666=ORIENTED_EDGE('',*,*,#47108,.F.);
#64667=ORIENTED_EDGE('',*,*,#47109,.F.);
#64668=ORIENTED_EDGE('',*,*,#47110,.F.);
#64669=ORIENTED_EDGE('',*,*,#46502,.T.);
#64670=ORIENTED_EDGE('',*,*,#47111,.F.);
#64671=ORIENTED_EDGE('',*,*,#47112,.F.);
#64672=ORIENTED_EDGE('',*,*,#47113,.F.);
#64673=ORIENTED_EDGE('',*,*,#46506,.T.);
#64674=ORIENTED_EDGE('',*,*,#47114,.F.);
#64675=ORIENTED_EDGE('',*,*,#47115,.F.);
#64676=ORIENTED_EDGE('',*,*,#47116,.F.);
#64677=ORIENTED_EDGE('',*,*,#46510,.T.);
#64678=ORIENTED_EDGE('',*,*,#47117,.F.);
#64679=ORIENTED_EDGE('',*,*,#47118,.F.);
#64680=ORIENTED_EDGE('',*,*,#47119,.F.);
#64681=ORIENTED_EDGE('',*,*,#46514,.T.);
#64682=ORIENTED_EDGE('',*,*,#47120,.F.);
#64683=ORIENTED_EDGE('',*,*,#47121,.F.);
#64684=ORIENTED_EDGE('',*,*,#47122,.F.);
#64685=ORIENTED_EDGE('',*,*,#46518,.T.);
#64686=ORIENTED_EDGE('',*,*,#47123,.F.);
#64687=ORIENTED_EDGE('',*,*,#47124,.F.);
#64688=ORIENTED_EDGE('',*,*,#47125,.F.);
#64689=ORIENTED_EDGE('',*,*,#46522,.T.);
#64690=ORIENTED_EDGE('',*,*,#47126,.F.);
#64691=ORIENTED_EDGE('',*,*,#47127,.F.);
#64692=ORIENTED_EDGE('',*,*,#47128,.F.);
#64693=ORIENTED_EDGE('',*,*,#46526,.T.);
#64694=ORIENTED_EDGE('',*,*,#47129,.F.);
#64695=ORIENTED_EDGE('',*,*,#47130,.F.);
#64696=ORIENTED_EDGE('',*,*,#47131,.F.);
#64697=ORIENTED_EDGE('',*,*,#46530,.T.);
#64698=ORIENTED_EDGE('',*,*,#47132,.F.);
#64699=ORIENTED_EDGE('',*,*,#47133,.F.);
#64700=ORIENTED_EDGE('',*,*,#47134,.F.);
#64701=ORIENTED_EDGE('',*,*,#46534,.T.);
#64702=ORIENTED_EDGE('',*,*,#47135,.F.);
#64703=ORIENTED_EDGE('',*,*,#47136,.F.);
#64704=ORIENTED_EDGE('',*,*,#47137,.F.);
#64705=ORIENTED_EDGE('',*,*,#46538,.T.);
#64706=ORIENTED_EDGE('',*,*,#47138,.F.);
#64707=ORIENTED_EDGE('',*,*,#47139,.F.);
#64708=ORIENTED_EDGE('',*,*,#47140,.F.);
#64709=ORIENTED_EDGE('',*,*,#46542,.T.);
#64710=ORIENTED_EDGE('',*,*,#47141,.F.);
#64711=ORIENTED_EDGE('',*,*,#47142,.F.);
#64712=ORIENTED_EDGE('',*,*,#47143,.F.);
#64713=ORIENTED_EDGE('',*,*,#46546,.T.);
#64714=ORIENTED_EDGE('',*,*,#47144,.F.);
#64715=ORIENTED_EDGE('',*,*,#47145,.F.);
#64716=ORIENTED_EDGE('',*,*,#47146,.F.);
#64717=ORIENTED_EDGE('',*,*,#46550,.T.);
#64718=ORIENTED_EDGE('',*,*,#47147,.F.);
#64719=ORIENTED_EDGE('',*,*,#47148,.F.);
#64720=ORIENTED_EDGE('',*,*,#47149,.F.);
#64721=ORIENTED_EDGE('',*,*,#46554,.T.);
#64722=ORIENTED_EDGE('',*,*,#47150,.F.);
#64723=ORIENTED_EDGE('',*,*,#47151,.F.);
#64724=ORIENTED_EDGE('',*,*,#47152,.F.);
#64725=ORIENTED_EDGE('',*,*,#46558,.T.);
#64726=ORIENTED_EDGE('',*,*,#47153,.F.);
#64727=ORIENTED_EDGE('',*,*,#47154,.F.);
#64728=ORIENTED_EDGE('',*,*,#46943,.F.);
#64729=ORIENTED_EDGE('',*,*,#46714,.T.);
#64730=ORIENTED_EDGE('',*,*,#46721,.T.);
#64731=ORIENTED_EDGE('',*,*,#47155,.T.);
#64732=ORIENTED_EDGE('',*,*,#47156,.T.);
#64733=ORIENTED_EDGE('',*,*,#47155,.F.);
#64734=ORIENTED_EDGE('',*,*,#46724,.T.);
#64735=ORIENTED_EDGE('',*,*,#46699,.T.);
#64736=ORIENTED_EDGE('',*,*,#47157,.T.);
#64737=ORIENTED_EDGE('',*,*,#46725,.T.);
#64738=ORIENTED_EDGE('',*,*,#47157,.F.);
#64739=ORIENTED_EDGE('',*,*,#46702,.T.);
#64740=ORIENTED_EDGE('',*,*,#46723,.T.);
#64741=ORIENTED_EDGE('',*,*,#46727,.T.);
#64742=ORIENTED_EDGE('',*,*,#46713,.T.);
#64743=ORIENTED_EDGE('',*,*,#47156,.F.);
#64744=ORIENTED_EDGE('',*,*,#46720,.T.);
#64745=ORIENTED_EDGE('',*,*,#46717,.T.);
#64746=ORIENTED_EDGE('',*,*,#46837,.F.);
#64747=ORIENTED_EDGE('',*,*,#46701,.T.);
#64748=ORIENTED_EDGE('',*,*,#46709,.T.);
#64749=ORIENTED_EDGE('',*,*,#46705,.T.);
#64750=ORIENTED_EDGE('',*,*,#47048,.T.);
#64751=ORIENTED_EDGE('',*,*,#46697,.T.);
#64752=ORIENTED_EDGE('',*,*,#46731,.T.);
#64753=ORIENTED_EDGE('',*,*,#47158,.T.);
#64754=ORIENTED_EDGE('',*,*,#47049,.T.);
#64755=ORIENTED_EDGE('',*,*,#47158,.F.);
#64756=ORIENTED_EDGE('',*,*,#46730,.T.);
#64757=ORIENTED_EDGE('',*,*,#47159,.T.);
#64758=ORIENTED_EDGE('',*,*,#47050,.T.);
#64759=ORIENTED_EDGE('',*,*,#47159,.F.);
#64760=ORIENTED_EDGE('',*,*,#46942,.T.);
#64761=ORIENTED_EDGE('',*,*,#46419,.T.);
#64762=ORIENTED_EDGE('',*,*,#47051,.T.);
#64763=ORIENTED_EDGE('',*,*,#46421,.T.);
#64764=ORIENTED_EDGE('',*,*,#46941,.T.);
#64765=ORIENTED_EDGE('',*,*,#47160,.T.);
#64766=ORIENTED_EDGE('',*,*,#47052,.T.);
#64767=ORIENTED_EDGE('',*,*,#47160,.F.);
#64768=ORIENTED_EDGE('',*,*,#46940,.T.);
#64769=ORIENTED_EDGE('',*,*,#47161,.T.);
#64770=ORIENTED_EDGE('',*,*,#47053,.T.);
#64771=ORIENTED_EDGE('',*,*,#47161,.F.);
#64772=ORIENTED_EDGE('',*,*,#46939,.T.);
#64773=ORIENTED_EDGE('',*,*,#46423,.T.);
#64774=ORIENTED_EDGE('',*,*,#47054,.T.);
#64775=ORIENTED_EDGE('',*,*,#46425,.T.);
#64776=ORIENTED_EDGE('',*,*,#46938,.T.);
#64777=ORIENTED_EDGE('',*,*,#47162,.T.);
#64778=ORIENTED_EDGE('',*,*,#47055,.T.);
#64779=ORIENTED_EDGE('',*,*,#47162,.F.);
#64780=ORIENTED_EDGE('',*,*,#46937,.T.);
#64781=ORIENTED_EDGE('',*,*,#47163,.T.);
#64782=ORIENTED_EDGE('',*,*,#47056,.T.);
#64783=ORIENTED_EDGE('',*,*,#47163,.F.);
#64784=ORIENTED_EDGE('',*,*,#46936,.T.);
#64785=ORIENTED_EDGE('',*,*,#46427,.T.);
#64786=ORIENTED_EDGE('',*,*,#47057,.T.);
#64787=ORIENTED_EDGE('',*,*,#46429,.T.);
#64788=ORIENTED_EDGE('',*,*,#46935,.T.);
#64789=ORIENTED_EDGE('',*,*,#47164,.T.);
#64790=ORIENTED_EDGE('',*,*,#47058,.T.);
#64791=ORIENTED_EDGE('',*,*,#47164,.F.);
#64792=ORIENTED_EDGE('',*,*,#46934,.T.);
#64793=ORIENTED_EDGE('',*,*,#47165,.T.);
#64794=ORIENTED_EDGE('',*,*,#47059,.T.);
#64795=ORIENTED_EDGE('',*,*,#47165,.F.);
#64796=ORIENTED_EDGE('',*,*,#46933,.T.);
#64797=ORIENTED_EDGE('',*,*,#46431,.T.);
#64798=ORIENTED_EDGE('',*,*,#47060,.T.);
#64799=ORIENTED_EDGE('',*,*,#46433,.T.);
#64800=ORIENTED_EDGE('',*,*,#46932,.T.);
#64801=ORIENTED_EDGE('',*,*,#47166,.T.);
#64802=ORIENTED_EDGE('',*,*,#47061,.T.);
#64803=ORIENTED_EDGE('',*,*,#47166,.F.);
#64804=ORIENTED_EDGE('',*,*,#46931,.T.);
#64805=ORIENTED_EDGE('',*,*,#47167,.T.);
#64806=ORIENTED_EDGE('',*,*,#47062,.T.);
#64807=ORIENTED_EDGE('',*,*,#47167,.F.);
#64808=ORIENTED_EDGE('',*,*,#46930,.T.);
#64809=ORIENTED_EDGE('',*,*,#46435,.T.);
#64810=ORIENTED_EDGE('',*,*,#47063,.T.);
#64811=ORIENTED_EDGE('',*,*,#46437,.T.);
#64812=ORIENTED_EDGE('',*,*,#46929,.T.);
#64813=ORIENTED_EDGE('',*,*,#47168,.T.);
#64814=ORIENTED_EDGE('',*,*,#47064,.T.);
#64815=ORIENTED_EDGE('',*,*,#47168,.F.);
#64816=ORIENTED_EDGE('',*,*,#46928,.T.);
#64817=ORIENTED_EDGE('',*,*,#47169,.T.);
#64818=ORIENTED_EDGE('',*,*,#47065,.T.);
#64819=ORIENTED_EDGE('',*,*,#47169,.F.);
#64820=ORIENTED_EDGE('',*,*,#46927,.T.);
#64821=ORIENTED_EDGE('',*,*,#46439,.T.);
#64822=ORIENTED_EDGE('',*,*,#47066,.T.);
#64823=ORIENTED_EDGE('',*,*,#46441,.T.);
#64824=ORIENTED_EDGE('',*,*,#46926,.T.);
#64825=ORIENTED_EDGE('',*,*,#47170,.T.);
#64826=ORIENTED_EDGE('',*,*,#47067,.T.);
#64827=ORIENTED_EDGE('',*,*,#47170,.F.);
#64828=ORIENTED_EDGE('',*,*,#46925,.T.);
#64829=ORIENTED_EDGE('',*,*,#47171,.T.);
#64830=ORIENTED_EDGE('',*,*,#47068,.T.);
#64831=ORIENTED_EDGE('',*,*,#47171,.F.);
#64832=ORIENTED_EDGE('',*,*,#46924,.T.);
#64833=ORIENTED_EDGE('',*,*,#46443,.T.);
#64834=ORIENTED_EDGE('',*,*,#47069,.T.);
#64835=ORIENTED_EDGE('',*,*,#46445,.T.);
#64836=ORIENTED_EDGE('',*,*,#46923,.T.);
#64837=ORIENTED_EDGE('',*,*,#47172,.T.);
#64838=ORIENTED_EDGE('',*,*,#47070,.T.);
#64839=ORIENTED_EDGE('',*,*,#47172,.F.);
#64840=ORIENTED_EDGE('',*,*,#46922,.T.);
#64841=ORIENTED_EDGE('',*,*,#47173,.T.);
#64842=ORIENTED_EDGE('',*,*,#47071,.T.);
#64843=ORIENTED_EDGE('',*,*,#47173,.F.);
#64844=ORIENTED_EDGE('',*,*,#46921,.T.);
#64845=ORIENTED_EDGE('',*,*,#46447,.T.);
#64846=ORIENTED_EDGE('',*,*,#47072,.T.);
#64847=ORIENTED_EDGE('',*,*,#46449,.T.);
#64848=ORIENTED_EDGE('',*,*,#46920,.T.);
#64849=ORIENTED_EDGE('',*,*,#47174,.T.);
#64850=ORIENTED_EDGE('',*,*,#47073,.T.);
#64851=ORIENTED_EDGE('',*,*,#47174,.F.);
#64852=ORIENTED_EDGE('',*,*,#46919,.T.);
#64853=ORIENTED_EDGE('',*,*,#47175,.T.);
#64854=ORIENTED_EDGE('',*,*,#47074,.T.);
#64855=ORIENTED_EDGE('',*,*,#47175,.F.);
#64856=ORIENTED_EDGE('',*,*,#46918,.T.);
#64857=ORIENTED_EDGE('',*,*,#46451,.T.);
#64858=ORIENTED_EDGE('',*,*,#47075,.T.);
#64859=ORIENTED_EDGE('',*,*,#46453,.T.);
#64860=ORIENTED_EDGE('',*,*,#46917,.T.);
#64861=ORIENTED_EDGE('',*,*,#47176,.T.);
#64862=ORIENTED_EDGE('',*,*,#47076,.T.);
#64863=ORIENTED_EDGE('',*,*,#47176,.F.);
#64864=ORIENTED_EDGE('',*,*,#46916,.T.);
#64865=ORIENTED_EDGE('',*,*,#47177,.T.);
#64866=ORIENTED_EDGE('',*,*,#47077,.T.);
#64867=ORIENTED_EDGE('',*,*,#47177,.F.);
#64868=ORIENTED_EDGE('',*,*,#46915,.T.);
#64869=ORIENTED_EDGE('',*,*,#46455,.T.);
#64870=ORIENTED_EDGE('',*,*,#47078,.T.);
#64871=ORIENTED_EDGE('',*,*,#46457,.T.);
#64872=ORIENTED_EDGE('',*,*,#46914,.T.);
#64873=ORIENTED_EDGE('',*,*,#47178,.T.);
#64874=ORIENTED_EDGE('',*,*,#47079,.T.);
#64875=ORIENTED_EDGE('',*,*,#47178,.F.);
#64876=ORIENTED_EDGE('',*,*,#46913,.T.);
#64877=ORIENTED_EDGE('',*,*,#47179,.T.);
#64878=ORIENTED_EDGE('',*,*,#47080,.T.);
#64879=ORIENTED_EDGE('',*,*,#47179,.F.);
#64880=ORIENTED_EDGE('',*,*,#46912,.T.);
#64881=ORIENTED_EDGE('',*,*,#46459,.T.);
#64882=ORIENTED_EDGE('',*,*,#47081,.T.);
#64883=ORIENTED_EDGE('',*,*,#46461,.T.);
#64884=ORIENTED_EDGE('',*,*,#46911,.T.);
#64885=ORIENTED_EDGE('',*,*,#47180,.T.);
#64886=ORIENTED_EDGE('',*,*,#47082,.T.);
#64887=ORIENTED_EDGE('',*,*,#47180,.F.);
#64888=ORIENTED_EDGE('',*,*,#46910,.T.);
#64889=ORIENTED_EDGE('',*,*,#47181,.T.);
#64890=ORIENTED_EDGE('',*,*,#47083,.T.);
#64891=ORIENTED_EDGE('',*,*,#47181,.F.);
#64892=ORIENTED_EDGE('',*,*,#46909,.T.);
#64893=ORIENTED_EDGE('',*,*,#46463,.T.);
#64894=ORIENTED_EDGE('',*,*,#47084,.T.);
#64895=ORIENTED_EDGE('',*,*,#46465,.T.);
#64896=ORIENTED_EDGE('',*,*,#46908,.T.);
#64897=ORIENTED_EDGE('',*,*,#47182,.T.);
#64898=ORIENTED_EDGE('',*,*,#47085,.T.);
#64899=ORIENTED_EDGE('',*,*,#47182,.F.);
#64900=ORIENTED_EDGE('',*,*,#46907,.T.);
#64901=ORIENTED_EDGE('',*,*,#47183,.T.);
#64902=ORIENTED_EDGE('',*,*,#47086,.T.);
#64903=ORIENTED_EDGE('',*,*,#47183,.F.);
#64904=ORIENTED_EDGE('',*,*,#46906,.T.);
#64905=ORIENTED_EDGE('',*,*,#46467,.T.);
#64906=ORIENTED_EDGE('',*,*,#47087,.T.);
#64907=ORIENTED_EDGE('',*,*,#46469,.T.);
#64908=ORIENTED_EDGE('',*,*,#46905,.T.);
#64909=ORIENTED_EDGE('',*,*,#47184,.T.);
#64910=ORIENTED_EDGE('',*,*,#47088,.T.);
#64911=ORIENTED_EDGE('',*,*,#47184,.F.);
#64912=ORIENTED_EDGE('',*,*,#46904,.T.);
#64913=ORIENTED_EDGE('',*,*,#47185,.T.);
#64914=ORIENTED_EDGE('',*,*,#47089,.T.);
#64915=ORIENTED_EDGE('',*,*,#47185,.F.);
#64916=ORIENTED_EDGE('',*,*,#46903,.T.);
#64917=ORIENTED_EDGE('',*,*,#46471,.T.);
#64918=ORIENTED_EDGE('',*,*,#47090,.T.);
#64919=ORIENTED_EDGE('',*,*,#46473,.T.);
#64920=ORIENTED_EDGE('',*,*,#46902,.T.);
#64921=ORIENTED_EDGE('',*,*,#47186,.T.);
#64922=ORIENTED_EDGE('',*,*,#47091,.T.);
#64923=ORIENTED_EDGE('',*,*,#47186,.F.);
#64924=ORIENTED_EDGE('',*,*,#46901,.T.);
#64925=ORIENTED_EDGE('',*,*,#47187,.T.);
#64926=ORIENTED_EDGE('',*,*,#47092,.T.);
#64927=ORIENTED_EDGE('',*,*,#47187,.F.);
#64928=ORIENTED_EDGE('',*,*,#46900,.T.);
#64929=ORIENTED_EDGE('',*,*,#46475,.T.);
#64930=ORIENTED_EDGE('',*,*,#47093,.T.);
#64931=ORIENTED_EDGE('',*,*,#46477,.T.);
#64932=ORIENTED_EDGE('',*,*,#46899,.T.);
#64933=ORIENTED_EDGE('',*,*,#47188,.T.);
#64934=ORIENTED_EDGE('',*,*,#47094,.T.);
#64935=ORIENTED_EDGE('',*,*,#47188,.F.);
#64936=ORIENTED_EDGE('',*,*,#46898,.T.);
#64937=ORIENTED_EDGE('',*,*,#47189,.T.);
#64938=ORIENTED_EDGE('',*,*,#47095,.T.);
#64939=ORIENTED_EDGE('',*,*,#47189,.F.);
#64940=ORIENTED_EDGE('',*,*,#46897,.T.);
#64941=ORIENTED_EDGE('',*,*,#46479,.T.);
#64942=ORIENTED_EDGE('',*,*,#47096,.T.);
#64943=ORIENTED_EDGE('',*,*,#46481,.T.);
#64944=ORIENTED_EDGE('',*,*,#46896,.T.);
#64945=ORIENTED_EDGE('',*,*,#47190,.T.);
#64946=ORIENTED_EDGE('',*,*,#47097,.T.);
#64947=ORIENTED_EDGE('',*,*,#47190,.F.);
#64948=ORIENTED_EDGE('',*,*,#46895,.T.);
#64949=ORIENTED_EDGE('',*,*,#47191,.T.);
#64950=ORIENTED_EDGE('',*,*,#47098,.T.);
#64951=ORIENTED_EDGE('',*,*,#47191,.F.);
#64952=ORIENTED_EDGE('',*,*,#46894,.T.);
#64953=ORIENTED_EDGE('',*,*,#46483,.T.);
#64954=ORIENTED_EDGE('',*,*,#47099,.T.);
#64955=ORIENTED_EDGE('',*,*,#46485,.T.);
#64956=ORIENTED_EDGE('',*,*,#46893,.T.);
#64957=ORIENTED_EDGE('',*,*,#47192,.T.);
#64958=ORIENTED_EDGE('',*,*,#47100,.T.);
#64959=ORIENTED_EDGE('',*,*,#47192,.F.);
#64960=ORIENTED_EDGE('',*,*,#46892,.T.);
#64961=ORIENTED_EDGE('',*,*,#47193,.T.);
#64962=ORIENTED_EDGE('',*,*,#47101,.T.);
#64963=ORIENTED_EDGE('',*,*,#47193,.F.);
#64964=ORIENTED_EDGE('',*,*,#46891,.T.);
#64965=ORIENTED_EDGE('',*,*,#46487,.T.);
#64966=ORIENTED_EDGE('',*,*,#47102,.T.);
#64967=ORIENTED_EDGE('',*,*,#46489,.T.);
#64968=ORIENTED_EDGE('',*,*,#46890,.T.);
#64969=ORIENTED_EDGE('',*,*,#47194,.T.);
#64970=ORIENTED_EDGE('',*,*,#47103,.T.);
#64971=ORIENTED_EDGE('',*,*,#47194,.F.);
#64972=ORIENTED_EDGE('',*,*,#46889,.T.);
#64973=ORIENTED_EDGE('',*,*,#47195,.T.);
#64974=ORIENTED_EDGE('',*,*,#47104,.T.);
#64975=ORIENTED_EDGE('',*,*,#47195,.F.);
#64976=ORIENTED_EDGE('',*,*,#46888,.T.);
#64977=ORIENTED_EDGE('',*,*,#46491,.T.);
#64978=ORIENTED_EDGE('',*,*,#47105,.T.);
#64979=ORIENTED_EDGE('',*,*,#46493,.T.);
#64980=ORIENTED_EDGE('',*,*,#46887,.T.);
#64981=ORIENTED_EDGE('',*,*,#47196,.T.);
#64982=ORIENTED_EDGE('',*,*,#47106,.T.);
#64983=ORIENTED_EDGE('',*,*,#47196,.F.);
#64984=ORIENTED_EDGE('',*,*,#46886,.T.);
#64985=ORIENTED_EDGE('',*,*,#47197,.T.);
#64986=ORIENTED_EDGE('',*,*,#47107,.T.);
#64987=ORIENTED_EDGE('',*,*,#47197,.F.);
#64988=ORIENTED_EDGE('',*,*,#46885,.T.);
#64989=ORIENTED_EDGE('',*,*,#46495,.T.);
#64990=ORIENTED_EDGE('',*,*,#47108,.T.);
#64991=ORIENTED_EDGE('',*,*,#46497,.T.);
#64992=ORIENTED_EDGE('',*,*,#46884,.T.);
#64993=ORIENTED_EDGE('',*,*,#47198,.T.);
#64994=ORIENTED_EDGE('',*,*,#47109,.T.);
#64995=ORIENTED_EDGE('',*,*,#47198,.F.);
#64996=ORIENTED_EDGE('',*,*,#46883,.T.);
#64997=ORIENTED_EDGE('',*,*,#47199,.T.);
#64998=ORIENTED_EDGE('',*,*,#47110,.T.);
#64999=ORIENTED_EDGE('',*,*,#47199,.F.);
#65000=ORIENTED_EDGE('',*,*,#46882,.T.);
#65001=ORIENTED_EDGE('',*,*,#46499,.T.);
#65002=ORIENTED_EDGE('',*,*,#47111,.T.);
#65003=ORIENTED_EDGE('',*,*,#46501,.T.);
#65004=ORIENTED_EDGE('',*,*,#46881,.T.);
#65005=ORIENTED_EDGE('',*,*,#47200,.T.);
#65006=ORIENTED_EDGE('',*,*,#47112,.T.);
#65007=ORIENTED_EDGE('',*,*,#47200,.F.);
#65008=ORIENTED_EDGE('',*,*,#46880,.T.);
#65009=ORIENTED_EDGE('',*,*,#47201,.T.);
#65010=ORIENTED_EDGE('',*,*,#47113,.T.);
#65011=ORIENTED_EDGE('',*,*,#47201,.F.);
#65012=ORIENTED_EDGE('',*,*,#46879,.T.);
#65013=ORIENTED_EDGE('',*,*,#46503,.T.);
#65014=ORIENTED_EDGE('',*,*,#47114,.T.);
#65015=ORIENTED_EDGE('',*,*,#46505,.T.);
#65016=ORIENTED_EDGE('',*,*,#46878,.T.);
#65017=ORIENTED_EDGE('',*,*,#47202,.T.);
#65018=ORIENTED_EDGE('',*,*,#47115,.T.);
#65019=ORIENTED_EDGE('',*,*,#47202,.F.);
#65020=ORIENTED_EDGE('',*,*,#46877,.T.);
#65021=ORIENTED_EDGE('',*,*,#47203,.T.);
#65022=ORIENTED_EDGE('',*,*,#47116,.T.);
#65023=ORIENTED_EDGE('',*,*,#47203,.F.);
#65024=ORIENTED_EDGE('',*,*,#46876,.T.);
#65025=ORIENTED_EDGE('',*,*,#46507,.T.);
#65026=ORIENTED_EDGE('',*,*,#47117,.T.);
#65027=ORIENTED_EDGE('',*,*,#46509,.T.);
#65028=ORIENTED_EDGE('',*,*,#46875,.T.);
#65029=ORIENTED_EDGE('',*,*,#47204,.T.);
#65030=ORIENTED_EDGE('',*,*,#47118,.T.);
#65031=ORIENTED_EDGE('',*,*,#47204,.F.);
#65032=ORIENTED_EDGE('',*,*,#46874,.T.);
#65033=ORIENTED_EDGE('',*,*,#47205,.T.);
#65034=ORIENTED_EDGE('',*,*,#47119,.T.);
#65035=ORIENTED_EDGE('',*,*,#47205,.F.);
#65036=ORIENTED_EDGE('',*,*,#46873,.T.);
#65037=ORIENTED_EDGE('',*,*,#46511,.T.);
#65038=ORIENTED_EDGE('',*,*,#47120,.T.);
#65039=ORIENTED_EDGE('',*,*,#46513,.T.);
#65040=ORIENTED_EDGE('',*,*,#46872,.T.);
#65041=ORIENTED_EDGE('',*,*,#47206,.T.);
#65042=ORIENTED_EDGE('',*,*,#47121,.T.);
#65043=ORIENTED_EDGE('',*,*,#47206,.F.);
#65044=ORIENTED_EDGE('',*,*,#46871,.T.);
#65045=ORIENTED_EDGE('',*,*,#47207,.T.);
#65046=ORIENTED_EDGE('',*,*,#47122,.T.);
#65047=ORIENTED_EDGE('',*,*,#47207,.F.);
#65048=ORIENTED_EDGE('',*,*,#46870,.T.);
#65049=ORIENTED_EDGE('',*,*,#46515,.T.);
#65050=ORIENTED_EDGE('',*,*,#47123,.T.);
#65051=ORIENTED_EDGE('',*,*,#46517,.T.);
#65052=ORIENTED_EDGE('',*,*,#46869,.T.);
#65053=ORIENTED_EDGE('',*,*,#47208,.T.);
#65054=ORIENTED_EDGE('',*,*,#47124,.T.);
#65055=ORIENTED_EDGE('',*,*,#47208,.F.);
#65056=ORIENTED_EDGE('',*,*,#46868,.T.);
#65057=ORIENTED_EDGE('',*,*,#47209,.T.);
#65058=ORIENTED_EDGE('',*,*,#47125,.T.);
#65059=ORIENTED_EDGE('',*,*,#47209,.F.);
#65060=ORIENTED_EDGE('',*,*,#46867,.T.);
#65061=ORIENTED_EDGE('',*,*,#46519,.T.);
#65062=ORIENTED_EDGE('',*,*,#47126,.T.);
#65063=ORIENTED_EDGE('',*,*,#46521,.T.);
#65064=ORIENTED_EDGE('',*,*,#46866,.T.);
#65065=ORIENTED_EDGE('',*,*,#47210,.T.);
#65066=ORIENTED_EDGE('',*,*,#47127,.T.);
#65067=ORIENTED_EDGE('',*,*,#47210,.F.);
#65068=ORIENTED_EDGE('',*,*,#46865,.T.);
#65069=ORIENTED_EDGE('',*,*,#47211,.T.);
#65070=ORIENTED_EDGE('',*,*,#47128,.T.);
#65071=ORIENTED_EDGE('',*,*,#47211,.F.);
#65072=ORIENTED_EDGE('',*,*,#46864,.T.);
#65073=ORIENTED_EDGE('',*,*,#46523,.T.);
#65074=ORIENTED_EDGE('',*,*,#47129,.T.);
#65075=ORIENTED_EDGE('',*,*,#46525,.T.);
#65076=ORIENTED_EDGE('',*,*,#46863,.T.);
#65077=ORIENTED_EDGE('',*,*,#47212,.T.);
#65078=ORIENTED_EDGE('',*,*,#47130,.T.);
#65079=ORIENTED_EDGE('',*,*,#47212,.F.);
#65080=ORIENTED_EDGE('',*,*,#46862,.T.);
#65081=ORIENTED_EDGE('',*,*,#47213,.T.);
#65082=ORIENTED_EDGE('',*,*,#47131,.T.);
#65083=ORIENTED_EDGE('',*,*,#47213,.F.);
#65084=ORIENTED_EDGE('',*,*,#46861,.T.);
#65085=ORIENTED_EDGE('',*,*,#46527,.T.);
#65086=ORIENTED_EDGE('',*,*,#47132,.T.);
#65087=ORIENTED_EDGE('',*,*,#46529,.T.);
#65088=ORIENTED_EDGE('',*,*,#46860,.T.);
#65089=ORIENTED_EDGE('',*,*,#47214,.T.);
#65090=ORIENTED_EDGE('',*,*,#47133,.T.);
#65091=ORIENTED_EDGE('',*,*,#47214,.F.);
#65092=ORIENTED_EDGE('',*,*,#46859,.T.);
#65093=ORIENTED_EDGE('',*,*,#47215,.T.);
#65094=ORIENTED_EDGE('',*,*,#47134,.T.);
#65095=ORIENTED_EDGE('',*,*,#47215,.F.);
#65096=ORIENTED_EDGE('',*,*,#46858,.T.);
#65097=ORIENTED_EDGE('',*,*,#46531,.T.);
#65098=ORIENTED_EDGE('',*,*,#47135,.T.);
#65099=ORIENTED_EDGE('',*,*,#46533,.T.);
#65100=ORIENTED_EDGE('',*,*,#46857,.T.);
#65101=ORIENTED_EDGE('',*,*,#47216,.T.);
#65102=ORIENTED_EDGE('',*,*,#47136,.T.);
#65103=ORIENTED_EDGE('',*,*,#47216,.F.);
#65104=ORIENTED_EDGE('',*,*,#46856,.T.);
#65105=ORIENTED_EDGE('',*,*,#47217,.T.);
#65106=ORIENTED_EDGE('',*,*,#47137,.T.);
#65107=ORIENTED_EDGE('',*,*,#47217,.F.);
#65108=ORIENTED_EDGE('',*,*,#46855,.T.);
#65109=ORIENTED_EDGE('',*,*,#46535,.T.);
#65110=ORIENTED_EDGE('',*,*,#47138,.T.);
#65111=ORIENTED_EDGE('',*,*,#46537,.T.);
#65112=ORIENTED_EDGE('',*,*,#46854,.T.);
#65113=ORIENTED_EDGE('',*,*,#47218,.T.);
#65114=ORIENTED_EDGE('',*,*,#47139,.T.);
#65115=ORIENTED_EDGE('',*,*,#47218,.F.);
#65116=ORIENTED_EDGE('',*,*,#46853,.T.);
#65117=ORIENTED_EDGE('',*,*,#47219,.T.);
#65118=ORIENTED_EDGE('',*,*,#47140,.T.);
#65119=ORIENTED_EDGE('',*,*,#47219,.F.);
#65120=ORIENTED_EDGE('',*,*,#46852,.T.);
#65121=ORIENTED_EDGE('',*,*,#46539,.T.);
#65122=ORIENTED_EDGE('',*,*,#47141,.T.);
#65123=ORIENTED_EDGE('',*,*,#46541,.T.);
#65124=ORIENTED_EDGE('',*,*,#46851,.T.);
#65125=ORIENTED_EDGE('',*,*,#47220,.T.);
#65126=ORIENTED_EDGE('',*,*,#47142,.T.);
#65127=ORIENTED_EDGE('',*,*,#47220,.F.);
#65128=ORIENTED_EDGE('',*,*,#46850,.T.);
#65129=ORIENTED_EDGE('',*,*,#47221,.T.);
#65130=ORIENTED_EDGE('',*,*,#47143,.T.);
#65131=ORIENTED_EDGE('',*,*,#47221,.F.);
#65132=ORIENTED_EDGE('',*,*,#46849,.T.);
#65133=ORIENTED_EDGE('',*,*,#46543,.T.);
#65134=ORIENTED_EDGE('',*,*,#47144,.T.);
#65135=ORIENTED_EDGE('',*,*,#46545,.T.);
#65136=ORIENTED_EDGE('',*,*,#46848,.T.);
#65137=ORIENTED_EDGE('',*,*,#47222,.T.);
#65138=ORIENTED_EDGE('',*,*,#47145,.T.);
#65139=ORIENTED_EDGE('',*,*,#47222,.F.);
#65140=ORIENTED_EDGE('',*,*,#46847,.T.);
#65141=ORIENTED_EDGE('',*,*,#47223,.T.);
#65142=ORIENTED_EDGE('',*,*,#47146,.T.);
#65143=ORIENTED_EDGE('',*,*,#47223,.F.);
#65144=ORIENTED_EDGE('',*,*,#46846,.T.);
#65145=ORIENTED_EDGE('',*,*,#46547,.T.);
#65146=ORIENTED_EDGE('',*,*,#47147,.T.);
#65147=ORIENTED_EDGE('',*,*,#46549,.T.);
#65148=ORIENTED_EDGE('',*,*,#46845,.T.);
#65149=ORIENTED_EDGE('',*,*,#47224,.T.);
#65150=ORIENTED_EDGE('',*,*,#47148,.T.);
#65151=ORIENTED_EDGE('',*,*,#47224,.F.);
#65152=ORIENTED_EDGE('',*,*,#46844,.T.);
#65153=ORIENTED_EDGE('',*,*,#47225,.T.);
#65154=ORIENTED_EDGE('',*,*,#47149,.T.);
#65155=ORIENTED_EDGE('',*,*,#47225,.F.);
#65156=ORIENTED_EDGE('',*,*,#46843,.T.);
#65157=ORIENTED_EDGE('',*,*,#46551,.T.);
#65158=ORIENTED_EDGE('',*,*,#47150,.T.);
#65159=ORIENTED_EDGE('',*,*,#46553,.T.);
#65160=ORIENTED_EDGE('',*,*,#46842,.T.);
#65161=ORIENTED_EDGE('',*,*,#47226,.T.);
#65162=ORIENTED_EDGE('',*,*,#47151,.T.);
#65163=ORIENTED_EDGE('',*,*,#47226,.F.);
#65164=ORIENTED_EDGE('',*,*,#46841,.T.);
#65165=ORIENTED_EDGE('',*,*,#47227,.T.);
#65166=ORIENTED_EDGE('',*,*,#47152,.T.);
#65167=ORIENTED_EDGE('',*,*,#47227,.F.);
#65168=ORIENTED_EDGE('',*,*,#46840,.T.);
#65169=ORIENTED_EDGE('',*,*,#46555,.T.);
#65170=ORIENTED_EDGE('',*,*,#47153,.T.);
#65171=ORIENTED_EDGE('',*,*,#46557,.T.);
#65172=ORIENTED_EDGE('',*,*,#46839,.T.);
#65173=ORIENTED_EDGE('',*,*,#47228,.T.);
#65174=ORIENTED_EDGE('',*,*,#46944,.T.);
#65175=ORIENTED_EDGE('',*,*,#47154,.T.);
#65176=ORIENTED_EDGE('',*,*,#47228,.F.);
#65177=ORIENTED_EDGE('',*,*,#46838,.T.);
#65178=ORIENTED_EDGE('',*,*,#46835,.T.);
#65179=ORIENTED_EDGE('',*,*,#47229,.T.);
#65180=ORIENTED_EDGE('',*,*,#46945,.T.);
#65181=ORIENTED_EDGE('',*,*,#47229,.F.);
#65182=ORIENTED_EDGE('',*,*,#46834,.T.);
#65183=ORIENTED_EDGE('',*,*,#46559,.T.);
#65184=ORIENTED_EDGE('',*,*,#46946,.T.);
#65185=ORIENTED_EDGE('',*,*,#46561,.T.);
#65186=ORIENTED_EDGE('',*,*,#46833,.T.);
#65187=ORIENTED_EDGE('',*,*,#47230,.T.);
#65188=ORIENTED_EDGE('',*,*,#46947,.T.);
#65189=ORIENTED_EDGE('',*,*,#47230,.F.);
#65190=ORIENTED_EDGE('',*,*,#46832,.T.);
#65191=ORIENTED_EDGE('',*,*,#47231,.T.);
#65192=ORIENTED_EDGE('',*,*,#46948,.T.);
#65193=ORIENTED_EDGE('',*,*,#47231,.F.);
#65194=ORIENTED_EDGE('',*,*,#46831,.T.);
#65195=ORIENTED_EDGE('',*,*,#46563,.T.);
#65196=ORIENTED_EDGE('',*,*,#46949,.T.);
#65197=ORIENTED_EDGE('',*,*,#46565,.T.);
#65198=ORIENTED_EDGE('',*,*,#46830,.T.);
#65199=ORIENTED_EDGE('',*,*,#47232,.T.);
#65200=ORIENTED_EDGE('',*,*,#46950,.T.);
#65201=ORIENTED_EDGE('',*,*,#47232,.F.);
#65202=ORIENTED_EDGE('',*,*,#46829,.T.);
#65203=ORIENTED_EDGE('',*,*,#47233,.T.);
#65204=ORIENTED_EDGE('',*,*,#46951,.T.);
#65205=ORIENTED_EDGE('',*,*,#47233,.F.);
#65206=ORIENTED_EDGE('',*,*,#46828,.T.);
#65207=ORIENTED_EDGE('',*,*,#46567,.T.);
#65208=ORIENTED_EDGE('',*,*,#46952,.T.);
#65209=ORIENTED_EDGE('',*,*,#46569,.T.);
#65210=ORIENTED_EDGE('',*,*,#46827,.T.);
#65211=ORIENTED_EDGE('',*,*,#47234,.T.);
#65212=ORIENTED_EDGE('',*,*,#46953,.T.);
#65213=ORIENTED_EDGE('',*,*,#47234,.F.);
#65214=ORIENTED_EDGE('',*,*,#46826,.T.);
#65215=ORIENTED_EDGE('',*,*,#47235,.T.);
#65216=ORIENTED_EDGE('',*,*,#46954,.T.);
#65217=ORIENTED_EDGE('',*,*,#47235,.F.);
#65218=ORIENTED_EDGE('',*,*,#46825,.T.);
#65219=ORIENTED_EDGE('',*,*,#46571,.T.);
#65220=ORIENTED_EDGE('',*,*,#46955,.T.);
#65221=ORIENTED_EDGE('',*,*,#46573,.T.);
#65222=ORIENTED_EDGE('',*,*,#46824,.T.);
#65223=ORIENTED_EDGE('',*,*,#47236,.T.);
#65224=ORIENTED_EDGE('',*,*,#46956,.T.);
#65225=ORIENTED_EDGE('',*,*,#47236,.F.);
#65226=ORIENTED_EDGE('',*,*,#46823,.T.);
#65227=ORIENTED_EDGE('',*,*,#47237,.T.);
#65228=ORIENTED_EDGE('',*,*,#46957,.T.);
#65229=ORIENTED_EDGE('',*,*,#47237,.F.);
#65230=ORIENTED_EDGE('',*,*,#46822,.T.);
#65231=ORIENTED_EDGE('',*,*,#46575,.T.);
#65232=ORIENTED_EDGE('',*,*,#46958,.T.);
#65233=ORIENTED_EDGE('',*,*,#46577,.T.);
#65234=ORIENTED_EDGE('',*,*,#46821,.T.);
#65235=ORIENTED_EDGE('',*,*,#47238,.T.);
#65236=ORIENTED_EDGE('',*,*,#46959,.T.);
#65237=ORIENTED_EDGE('',*,*,#47238,.F.);
#65238=ORIENTED_EDGE('',*,*,#46820,.T.);
#65239=ORIENTED_EDGE('',*,*,#47239,.T.);
#65240=ORIENTED_EDGE('',*,*,#46960,.T.);
#65241=ORIENTED_EDGE('',*,*,#47239,.F.);
#65242=ORIENTED_EDGE('',*,*,#46819,.T.);
#65243=ORIENTED_EDGE('',*,*,#46579,.T.);
#65244=ORIENTED_EDGE('',*,*,#46961,.T.);
#65245=ORIENTED_EDGE('',*,*,#46581,.T.);
#65246=ORIENTED_EDGE('',*,*,#46818,.T.);
#65247=ORIENTED_EDGE('',*,*,#47240,.T.);
#65248=ORIENTED_EDGE('',*,*,#46962,.T.);
#65249=ORIENTED_EDGE('',*,*,#47240,.F.);
#65250=ORIENTED_EDGE('',*,*,#46817,.T.);
#65251=ORIENTED_EDGE('',*,*,#47241,.T.);
#65252=ORIENTED_EDGE('',*,*,#46963,.T.);
#65253=ORIENTED_EDGE('',*,*,#47241,.F.);
#65254=ORIENTED_EDGE('',*,*,#46816,.T.);
#65255=ORIENTED_EDGE('',*,*,#46583,.T.);
#65256=ORIENTED_EDGE('',*,*,#46964,.T.);
#65257=ORIENTED_EDGE('',*,*,#46585,.T.);
#65258=ORIENTED_EDGE('',*,*,#46815,.T.);
#65259=ORIENTED_EDGE('',*,*,#47242,.T.);
#65260=ORIENTED_EDGE('',*,*,#46965,.T.);
#65261=ORIENTED_EDGE('',*,*,#47242,.F.);
#65262=ORIENTED_EDGE('',*,*,#46814,.T.);
#65263=ORIENTED_EDGE('',*,*,#47243,.T.);
#65264=ORIENTED_EDGE('',*,*,#46966,.T.);
#65265=ORIENTED_EDGE('',*,*,#47243,.F.);
#65266=ORIENTED_EDGE('',*,*,#46813,.T.);
#65267=ORIENTED_EDGE('',*,*,#46587,.T.);
#65268=ORIENTED_EDGE('',*,*,#46967,.T.);
#65269=ORIENTED_EDGE('',*,*,#46589,.T.);
#65270=ORIENTED_EDGE('',*,*,#46812,.T.);
#65271=ORIENTED_EDGE('',*,*,#47244,.T.);
#65272=ORIENTED_EDGE('',*,*,#46968,.T.);
#65273=ORIENTED_EDGE('',*,*,#47244,.F.);
#65274=ORIENTED_EDGE('',*,*,#46811,.T.);
#65275=ORIENTED_EDGE('',*,*,#47245,.T.);
#65276=ORIENTED_EDGE('',*,*,#46969,.T.);
#65277=ORIENTED_EDGE('',*,*,#47245,.F.);
#65278=ORIENTED_EDGE('',*,*,#46810,.T.);
#65279=ORIENTED_EDGE('',*,*,#46591,.T.);
#65280=ORIENTED_EDGE('',*,*,#46970,.T.);
#65281=ORIENTED_EDGE('',*,*,#46593,.T.);
#65282=ORIENTED_EDGE('',*,*,#46809,.T.);
#65283=ORIENTED_EDGE('',*,*,#47246,.T.);
#65284=ORIENTED_EDGE('',*,*,#46971,.T.);
#65285=ORIENTED_EDGE('',*,*,#47246,.F.);
#65286=ORIENTED_EDGE('',*,*,#46808,.T.);
#65287=ORIENTED_EDGE('',*,*,#47247,.T.);
#65288=ORIENTED_EDGE('',*,*,#46972,.T.);
#65289=ORIENTED_EDGE('',*,*,#47247,.F.);
#65290=ORIENTED_EDGE('',*,*,#46807,.T.);
#65291=ORIENTED_EDGE('',*,*,#46595,.T.);
#65292=ORIENTED_EDGE('',*,*,#46973,.T.);
#65293=ORIENTED_EDGE('',*,*,#46597,.T.);
#65294=ORIENTED_EDGE('',*,*,#46806,.T.);
#65295=ORIENTED_EDGE('',*,*,#47248,.T.);
#65296=ORIENTED_EDGE('',*,*,#46974,.T.);
#65297=ORIENTED_EDGE('',*,*,#47248,.F.);
#65298=ORIENTED_EDGE('',*,*,#46805,.T.);
#65299=ORIENTED_EDGE('',*,*,#47249,.T.);
#65300=ORIENTED_EDGE('',*,*,#46975,.T.);
#65301=ORIENTED_EDGE('',*,*,#47249,.F.);
#65302=ORIENTED_EDGE('',*,*,#46804,.T.);
#65303=ORIENTED_EDGE('',*,*,#46599,.T.);
#65304=ORIENTED_EDGE('',*,*,#46976,.T.);
#65305=ORIENTED_EDGE('',*,*,#46601,.T.);
#65306=ORIENTED_EDGE('',*,*,#46803,.T.);
#65307=ORIENTED_EDGE('',*,*,#47250,.T.);
#65308=ORIENTED_EDGE('',*,*,#46977,.T.);
#65309=ORIENTED_EDGE('',*,*,#47250,.F.);
#65310=ORIENTED_EDGE('',*,*,#46802,.T.);
#65311=ORIENTED_EDGE('',*,*,#47251,.T.);
#65312=ORIENTED_EDGE('',*,*,#46978,.T.);
#65313=ORIENTED_EDGE('',*,*,#47251,.F.);
#65314=ORIENTED_EDGE('',*,*,#46801,.T.);
#65315=ORIENTED_EDGE('',*,*,#46603,.T.);
#65316=ORIENTED_EDGE('',*,*,#46979,.T.);
#65317=ORIENTED_EDGE('',*,*,#46605,.T.);
#65318=ORIENTED_EDGE('',*,*,#46800,.T.);
#65319=ORIENTED_EDGE('',*,*,#47252,.T.);
#65320=ORIENTED_EDGE('',*,*,#46980,.T.);
#65321=ORIENTED_EDGE('',*,*,#47252,.F.);
#65322=ORIENTED_EDGE('',*,*,#46799,.T.);
#65323=ORIENTED_EDGE('',*,*,#47253,.T.);
#65324=ORIENTED_EDGE('',*,*,#46981,.T.);
#65325=ORIENTED_EDGE('',*,*,#47253,.F.);
#65326=ORIENTED_EDGE('',*,*,#46798,.T.);
#65327=ORIENTED_EDGE('',*,*,#46607,.T.);
#65328=ORIENTED_EDGE('',*,*,#46982,.T.);
#65329=ORIENTED_EDGE('',*,*,#46609,.T.);
#65330=ORIENTED_EDGE('',*,*,#46797,.T.);
#65331=ORIENTED_EDGE('',*,*,#47254,.T.);
#65332=ORIENTED_EDGE('',*,*,#46983,.T.);
#65333=ORIENTED_EDGE('',*,*,#47254,.F.);
#65334=ORIENTED_EDGE('',*,*,#46796,.T.);
#65335=ORIENTED_EDGE('',*,*,#47255,.T.);
#65336=ORIENTED_EDGE('',*,*,#46984,.T.);
#65337=ORIENTED_EDGE('',*,*,#47255,.F.);
#65338=ORIENTED_EDGE('',*,*,#46795,.T.);
#65339=ORIENTED_EDGE('',*,*,#46611,.T.);
#65340=ORIENTED_EDGE('',*,*,#46985,.T.);
#65341=ORIENTED_EDGE('',*,*,#46613,.T.);
#65342=ORIENTED_EDGE('',*,*,#46794,.T.);
#65343=ORIENTED_EDGE('',*,*,#47256,.T.);
#65344=ORIENTED_EDGE('',*,*,#46986,.T.);
#65345=ORIENTED_EDGE('',*,*,#47256,.F.);
#65346=ORIENTED_EDGE('',*,*,#46793,.T.);
#65347=ORIENTED_EDGE('',*,*,#47257,.T.);
#65348=ORIENTED_EDGE('',*,*,#46987,.T.);
#65349=ORIENTED_EDGE('',*,*,#47257,.F.);
#65350=ORIENTED_EDGE('',*,*,#46792,.T.);
#65351=ORIENTED_EDGE('',*,*,#46615,.T.);
#65352=ORIENTED_EDGE('',*,*,#46988,.T.);
#65353=ORIENTED_EDGE('',*,*,#46617,.T.);
#65354=ORIENTED_EDGE('',*,*,#46791,.T.);
#65355=ORIENTED_EDGE('',*,*,#47258,.T.);
#65356=ORIENTED_EDGE('',*,*,#46989,.T.);
#65357=ORIENTED_EDGE('',*,*,#47258,.F.);
#65358=ORIENTED_EDGE('',*,*,#46790,.T.);
#65359=ORIENTED_EDGE('',*,*,#47259,.T.);
#65360=ORIENTED_EDGE('',*,*,#46990,.T.);
#65361=ORIENTED_EDGE('',*,*,#47259,.F.);
#65362=ORIENTED_EDGE('',*,*,#46789,.T.);
#65363=ORIENTED_EDGE('',*,*,#46619,.T.);
#65364=ORIENTED_EDGE('',*,*,#46991,.T.);
#65365=ORIENTED_EDGE('',*,*,#46621,.T.);
#65366=ORIENTED_EDGE('',*,*,#46788,.T.);
#65367=ORIENTED_EDGE('',*,*,#47260,.T.);
#65368=ORIENTED_EDGE('',*,*,#46992,.T.);
#65369=ORIENTED_EDGE('',*,*,#47260,.F.);
#65370=ORIENTED_EDGE('',*,*,#46787,.T.);
#65371=ORIENTED_EDGE('',*,*,#47261,.T.);
#65372=ORIENTED_EDGE('',*,*,#46993,.T.);
#65373=ORIENTED_EDGE('',*,*,#47261,.F.);
#65374=ORIENTED_EDGE('',*,*,#46786,.T.);
#65375=ORIENTED_EDGE('',*,*,#46623,.T.);
#65376=ORIENTED_EDGE('',*,*,#46994,.T.);
#65377=ORIENTED_EDGE('',*,*,#46625,.T.);
#65378=ORIENTED_EDGE('',*,*,#46785,.T.);
#65379=ORIENTED_EDGE('',*,*,#47262,.T.);
#65380=ORIENTED_EDGE('',*,*,#46995,.T.);
#65381=ORIENTED_EDGE('',*,*,#47262,.F.);
#65382=ORIENTED_EDGE('',*,*,#46784,.T.);
#65383=ORIENTED_EDGE('',*,*,#47263,.T.);
#65384=ORIENTED_EDGE('',*,*,#46996,.T.);
#65385=ORIENTED_EDGE('',*,*,#47263,.F.);
#65386=ORIENTED_EDGE('',*,*,#46783,.T.);
#65387=ORIENTED_EDGE('',*,*,#46627,.T.);
#65388=ORIENTED_EDGE('',*,*,#46997,.T.);
#65389=ORIENTED_EDGE('',*,*,#46629,.T.);
#65390=ORIENTED_EDGE('',*,*,#46782,.T.);
#65391=ORIENTED_EDGE('',*,*,#47264,.T.);
#65392=ORIENTED_EDGE('',*,*,#46998,.T.);
#65393=ORIENTED_EDGE('',*,*,#47264,.F.);
#65394=ORIENTED_EDGE('',*,*,#46781,.T.);
#65395=ORIENTED_EDGE('',*,*,#47265,.T.);
#65396=ORIENTED_EDGE('',*,*,#46999,.T.);
#65397=ORIENTED_EDGE('',*,*,#47265,.F.);
#65398=ORIENTED_EDGE('',*,*,#46780,.T.);
#65399=ORIENTED_EDGE('',*,*,#46631,.T.);
#65400=ORIENTED_EDGE('',*,*,#47000,.T.);
#65401=ORIENTED_EDGE('',*,*,#46633,.T.);
#65402=ORIENTED_EDGE('',*,*,#46779,.T.);
#65403=ORIENTED_EDGE('',*,*,#47266,.T.);
#65404=ORIENTED_EDGE('',*,*,#47001,.T.);
#65405=ORIENTED_EDGE('',*,*,#47266,.F.);
#65406=ORIENTED_EDGE('',*,*,#46778,.T.);
#65407=ORIENTED_EDGE('',*,*,#47267,.T.);
#65408=ORIENTED_EDGE('',*,*,#47002,.T.);
#65409=ORIENTED_EDGE('',*,*,#47267,.F.);
#65410=ORIENTED_EDGE('',*,*,#46777,.T.);
#65411=ORIENTED_EDGE('',*,*,#46635,.T.);
#65412=ORIENTED_EDGE('',*,*,#47003,.T.);
#65413=ORIENTED_EDGE('',*,*,#46637,.T.);
#65414=ORIENTED_EDGE('',*,*,#46776,.T.);
#65415=ORIENTED_EDGE('',*,*,#47268,.T.);
#65416=ORIENTED_EDGE('',*,*,#47004,.T.);
#65417=ORIENTED_EDGE('',*,*,#47268,.F.);
#65418=ORIENTED_EDGE('',*,*,#46775,.T.);
#65419=ORIENTED_EDGE('',*,*,#47269,.T.);
#65420=ORIENTED_EDGE('',*,*,#47005,.T.);
#65421=ORIENTED_EDGE('',*,*,#47269,.F.);
#65422=ORIENTED_EDGE('',*,*,#46774,.T.);
#65423=ORIENTED_EDGE('',*,*,#46639,.T.);
#65424=ORIENTED_EDGE('',*,*,#47006,.T.);
#65425=ORIENTED_EDGE('',*,*,#46641,.T.);
#65426=ORIENTED_EDGE('',*,*,#46773,.T.);
#65427=ORIENTED_EDGE('',*,*,#47270,.T.);
#65428=ORIENTED_EDGE('',*,*,#47007,.T.);
#65429=ORIENTED_EDGE('',*,*,#47270,.F.);
#65430=ORIENTED_EDGE('',*,*,#46772,.T.);
#65431=ORIENTED_EDGE('',*,*,#47271,.T.);
#65432=ORIENTED_EDGE('',*,*,#47008,.T.);
#65433=ORIENTED_EDGE('',*,*,#47271,.F.);
#65434=ORIENTED_EDGE('',*,*,#46771,.T.);
#65435=ORIENTED_EDGE('',*,*,#46643,.T.);
#65436=ORIENTED_EDGE('',*,*,#47009,.T.);
#65437=ORIENTED_EDGE('',*,*,#46645,.T.);
#65438=ORIENTED_EDGE('',*,*,#46770,.T.);
#65439=ORIENTED_EDGE('',*,*,#47272,.T.);
#65440=ORIENTED_EDGE('',*,*,#47010,.T.);
#65441=ORIENTED_EDGE('',*,*,#47272,.F.);
#65442=ORIENTED_EDGE('',*,*,#46769,.T.);
#65443=ORIENTED_EDGE('',*,*,#47273,.T.);
#65444=ORIENTED_EDGE('',*,*,#47011,.T.);
#65445=ORIENTED_EDGE('',*,*,#47273,.F.);
#65446=ORIENTED_EDGE('',*,*,#46768,.T.);
#65447=ORIENTED_EDGE('',*,*,#46647,.T.);
#65448=ORIENTED_EDGE('',*,*,#47012,.T.);
#65449=ORIENTED_EDGE('',*,*,#46649,.T.);
#65450=ORIENTED_EDGE('',*,*,#46767,.T.);
#65451=ORIENTED_EDGE('',*,*,#47274,.T.);
#65452=ORIENTED_EDGE('',*,*,#47013,.T.);
#65453=ORIENTED_EDGE('',*,*,#47274,.F.);
#65454=ORIENTED_EDGE('',*,*,#46766,.T.);
#65455=ORIENTED_EDGE('',*,*,#47275,.T.);
#65456=ORIENTED_EDGE('',*,*,#47014,.T.);
#65457=ORIENTED_EDGE('',*,*,#47275,.F.);
#65458=ORIENTED_EDGE('',*,*,#46765,.T.);
#65459=ORIENTED_EDGE('',*,*,#46651,.T.);
#65460=ORIENTED_EDGE('',*,*,#47015,.T.);
#65461=ORIENTED_EDGE('',*,*,#46653,.T.);
#65462=ORIENTED_EDGE('',*,*,#46764,.T.);
#65463=ORIENTED_EDGE('',*,*,#47276,.T.);
#65464=ORIENTED_EDGE('',*,*,#47016,.T.);
#65465=ORIENTED_EDGE('',*,*,#47276,.F.);
#65466=ORIENTED_EDGE('',*,*,#46763,.T.);
#65467=ORIENTED_EDGE('',*,*,#47277,.T.);
#65468=ORIENTED_EDGE('',*,*,#47017,.T.);
#65469=ORIENTED_EDGE('',*,*,#47277,.F.);
#65470=ORIENTED_EDGE('',*,*,#46762,.T.);
#65471=ORIENTED_EDGE('',*,*,#46655,.T.);
#65472=ORIENTED_EDGE('',*,*,#47018,.T.);
#65473=ORIENTED_EDGE('',*,*,#46657,.T.);
#65474=ORIENTED_EDGE('',*,*,#46761,.T.);
#65475=ORIENTED_EDGE('',*,*,#47278,.T.);
#65476=ORIENTED_EDGE('',*,*,#47019,.T.);
#65477=ORIENTED_EDGE('',*,*,#47278,.F.);
#65478=ORIENTED_EDGE('',*,*,#46760,.T.);
#65479=ORIENTED_EDGE('',*,*,#47279,.T.);
#65480=ORIENTED_EDGE('',*,*,#47020,.T.);
#65481=ORIENTED_EDGE('',*,*,#47279,.F.);
#65482=ORIENTED_EDGE('',*,*,#46759,.T.);
#65483=ORIENTED_EDGE('',*,*,#46659,.T.);
#65484=ORIENTED_EDGE('',*,*,#47021,.T.);
#65485=ORIENTED_EDGE('',*,*,#46661,.T.);
#65486=ORIENTED_EDGE('',*,*,#46758,.T.);
#65487=ORIENTED_EDGE('',*,*,#47280,.T.);
#65488=ORIENTED_EDGE('',*,*,#47022,.T.);
#65489=ORIENTED_EDGE('',*,*,#47280,.F.);
#65490=ORIENTED_EDGE('',*,*,#46757,.T.);
#65491=ORIENTED_EDGE('',*,*,#47281,.T.);
#65492=ORIENTED_EDGE('',*,*,#47023,.T.);
#65493=ORIENTED_EDGE('',*,*,#47281,.F.);
#65494=ORIENTED_EDGE('',*,*,#46756,.T.);
#65495=ORIENTED_EDGE('',*,*,#46663,.T.);
#65496=ORIENTED_EDGE('',*,*,#47024,.T.);
#65497=ORIENTED_EDGE('',*,*,#46665,.T.);
#65498=ORIENTED_EDGE('',*,*,#46755,.T.);
#65499=ORIENTED_EDGE('',*,*,#47282,.T.);
#65500=ORIENTED_EDGE('',*,*,#47025,.T.);
#65501=ORIENTED_EDGE('',*,*,#47282,.F.);
#65502=ORIENTED_EDGE('',*,*,#46754,.T.);
#65503=ORIENTED_EDGE('',*,*,#47283,.T.);
#65504=ORIENTED_EDGE('',*,*,#47026,.T.);
#65505=ORIENTED_EDGE('',*,*,#47283,.F.);
#65506=ORIENTED_EDGE('',*,*,#46753,.T.);
#65507=ORIENTED_EDGE('',*,*,#46667,.T.);
#65508=ORIENTED_EDGE('',*,*,#47027,.T.);
#65509=ORIENTED_EDGE('',*,*,#46669,.T.);
#65510=ORIENTED_EDGE('',*,*,#46752,.T.);
#65511=ORIENTED_EDGE('',*,*,#47284,.T.);
#65512=ORIENTED_EDGE('',*,*,#47028,.T.);
#65513=ORIENTED_EDGE('',*,*,#47284,.F.);
#65514=ORIENTED_EDGE('',*,*,#46751,.T.);
#65515=ORIENTED_EDGE('',*,*,#47285,.T.);
#65516=ORIENTED_EDGE('',*,*,#47029,.T.);
#65517=ORIENTED_EDGE('',*,*,#47285,.F.);
#65518=ORIENTED_EDGE('',*,*,#46750,.T.);
#65519=ORIENTED_EDGE('',*,*,#46671,.T.);
#65520=ORIENTED_EDGE('',*,*,#47030,.T.);
#65521=ORIENTED_EDGE('',*,*,#46673,.T.);
#65522=ORIENTED_EDGE('',*,*,#46749,.T.);
#65523=ORIENTED_EDGE('',*,*,#47286,.T.);
#65524=ORIENTED_EDGE('',*,*,#47031,.T.);
#65525=ORIENTED_EDGE('',*,*,#47286,.F.);
#65526=ORIENTED_EDGE('',*,*,#46748,.T.);
#65527=ORIENTED_EDGE('',*,*,#47287,.T.);
#65528=ORIENTED_EDGE('',*,*,#47032,.T.);
#65529=ORIENTED_EDGE('',*,*,#47287,.F.);
#65530=ORIENTED_EDGE('',*,*,#46747,.T.);
#65531=ORIENTED_EDGE('',*,*,#46675,.T.);
#65532=ORIENTED_EDGE('',*,*,#47033,.T.);
#65533=ORIENTED_EDGE('',*,*,#46677,.T.);
#65534=ORIENTED_EDGE('',*,*,#46746,.T.);
#65535=ORIENTED_EDGE('',*,*,#47288,.T.);
#65536=ORIENTED_EDGE('',*,*,#47034,.T.);
#65537=ORIENTED_EDGE('',*,*,#47288,.F.);
#65538=ORIENTED_EDGE('',*,*,#46745,.T.);
#65539=ORIENTED_EDGE('',*,*,#47289,.T.);
#65540=ORIENTED_EDGE('',*,*,#47035,.T.);
#65541=ORIENTED_EDGE('',*,*,#47289,.F.);
#65542=ORIENTED_EDGE('',*,*,#46744,.T.);
#65543=ORIENTED_EDGE('',*,*,#46679,.T.);
#65544=ORIENTED_EDGE('',*,*,#47036,.T.);
#65545=ORIENTED_EDGE('',*,*,#46681,.T.);
#65546=ORIENTED_EDGE('',*,*,#46743,.T.);
#65547=ORIENTED_EDGE('',*,*,#47290,.T.);
#65548=ORIENTED_EDGE('',*,*,#47037,.T.);
#65549=ORIENTED_EDGE('',*,*,#47290,.F.);
#65550=ORIENTED_EDGE('',*,*,#46742,.T.);
#65551=ORIENTED_EDGE('',*,*,#47291,.T.);
#65552=ORIENTED_EDGE('',*,*,#47038,.T.);
#65553=ORIENTED_EDGE('',*,*,#47291,.F.);
#65554=ORIENTED_EDGE('',*,*,#46741,.T.);
#65555=ORIENTED_EDGE('',*,*,#46683,.T.);
#65556=ORIENTED_EDGE('',*,*,#47039,.T.);
#65557=ORIENTED_EDGE('',*,*,#46685,.T.);
#65558=ORIENTED_EDGE('',*,*,#46740,.T.);
#65559=ORIENTED_EDGE('',*,*,#47292,.T.);
#65560=ORIENTED_EDGE('',*,*,#47040,.T.);
#65561=ORIENTED_EDGE('',*,*,#47292,.F.);
#65562=ORIENTED_EDGE('',*,*,#46739,.T.);
#65563=ORIENTED_EDGE('',*,*,#47293,.T.);
#65564=ORIENTED_EDGE('',*,*,#47041,.T.);
#65565=ORIENTED_EDGE('',*,*,#47293,.F.);
#65566=ORIENTED_EDGE('',*,*,#46738,.T.);
#65567=ORIENTED_EDGE('',*,*,#46687,.T.);
#65568=ORIENTED_EDGE('',*,*,#47042,.T.);
#65569=ORIENTED_EDGE('',*,*,#46689,.T.);
#65570=ORIENTED_EDGE('',*,*,#46737,.T.);
#65571=ORIENTED_EDGE('',*,*,#47294,.T.);
#65572=ORIENTED_EDGE('',*,*,#47043,.T.);
#65573=ORIENTED_EDGE('',*,*,#47294,.F.);
#65574=ORIENTED_EDGE('',*,*,#46736,.T.);
#65575=ORIENTED_EDGE('',*,*,#47295,.T.);
#65576=ORIENTED_EDGE('',*,*,#47044,.T.);
#65577=ORIENTED_EDGE('',*,*,#47295,.F.);
#65578=ORIENTED_EDGE('',*,*,#46735,.T.);
#65579=ORIENTED_EDGE('',*,*,#46691,.T.);
#65580=ORIENTED_EDGE('',*,*,#47045,.T.);
#65581=ORIENTED_EDGE('',*,*,#46693,.T.);
#65582=ORIENTED_EDGE('',*,*,#46734,.T.);
#65583=ORIENTED_EDGE('',*,*,#47296,.T.);
#65584=ORIENTED_EDGE('',*,*,#47046,.T.);
#65585=ORIENTED_EDGE('',*,*,#47296,.F.);
#65586=ORIENTED_EDGE('',*,*,#46733,.T.);
#65587=ORIENTED_EDGE('',*,*,#47297,.T.);
#65588=ORIENTED_EDGE('',*,*,#47047,.T.);
#65589=ORIENTED_EDGE('',*,*,#47297,.F.);
#65590=ORIENTED_EDGE('',*,*,#46732,.T.);
#65591=ORIENTED_EDGE('',*,*,#46695,.T.);
#65592=ORIENTED_EDGE('',*,*,#47298,.F.);
#65593=ORIENTED_EDGE('',*,*,#47299,.T.);
#65594=ORIENTED_EDGE('',*,*,#47300,.T.);
#65595=ORIENTED_EDGE('',*,*,#47299,.F.);
#65596=ORIENTED_EDGE('',*,*,#47301,.F.);
#65597=ORIENTED_EDGE('',*,*,#47302,.T.);
#65598=ORIENTED_EDGE('',*,*,#47303,.T.);
#65599=ORIENTED_EDGE('',*,*,#47302,.F.);
#65600=ORIENTED_EDGE('',*,*,#47304,.F.);
#65601=ORIENTED_EDGE('',*,*,#47305,.T.);
#65602=ORIENTED_EDGE('',*,*,#47306,.F.);
#65603=ORIENTED_EDGE('',*,*,#47305,.F.);
#65604=ORIENTED_EDGE('',*,*,#47307,.F.);
#65605=ORIENTED_EDGE('',*,*,#47308,.T.);
#65606=ORIENTED_EDGE('',*,*,#47309,.F.);
#65607=ORIENTED_EDGE('',*,*,#47308,.F.);
#65608=ORIENTED_EDGE('',*,*,#47310,.F.);
#65609=ORIENTED_EDGE('',*,*,#47311,.T.);
#65610=ORIENTED_EDGE('',*,*,#47312,.F.);
#65611=ORIENTED_EDGE('',*,*,#47311,.F.);
#65612=ORIENTED_EDGE('',*,*,#47313,.F.);
#65613=ORIENTED_EDGE('',*,*,#47314,.F.);
#65614=ORIENTED_EDGE('',*,*,#47315,.T.);
#65615=ORIENTED_EDGE('',*,*,#47316,.F.);
#65616=ORIENTED_EDGE('',*,*,#47315,.F.);
#65617=ORIENTED_EDGE('',*,*,#47317,.F.);
#65618=ORIENTED_EDGE('',*,*,#47318,.T.);
#65619=ORIENTED_EDGE('',*,*,#47319,.F.);
#65620=ORIENTED_EDGE('',*,*,#47320,.F.);
#65621=ORIENTED_EDGE('',*,*,#47318,.F.);
#65622=ORIENTED_EDGE('',*,*,#47321,.F.);
#65623=ORIENTED_EDGE('',*,*,#47322,.T.);
#65624=ORIENTED_EDGE('',*,*,#47323,.F.);
#65625=ORIENTED_EDGE('',*,*,#47324,.F.);
#65626=ORIENTED_EDGE('',*,*,#47325,.F.);
#65627=ORIENTED_EDGE('',*,*,#47326,.T.);
#65628=ORIENTED_EDGE('',*,*,#47327,.F.);
#65629=ORIENTED_EDGE('',*,*,#47328,.F.);
#65630=ORIENTED_EDGE('',*,*,#47329,.F.);
#65631=ORIENTED_EDGE('',*,*,#47330,.T.);
#65632=ORIENTED_EDGE('',*,*,#47331,.F.);
#65633=ORIENTED_EDGE('',*,*,#47332,.F.);
#65634=ORIENTED_EDGE('',*,*,#47330,.F.);
#65635=ORIENTED_EDGE('',*,*,#47333,.F.);
#65636=ORIENTED_EDGE('',*,*,#47334,.T.);
#65637=ORIENTED_EDGE('',*,*,#47335,.F.);
#65638=ORIENTED_EDGE('',*,*,#47336,.F.);
#65639=ORIENTED_EDGE('',*,*,#47334,.F.);
#65640=ORIENTED_EDGE('',*,*,#47337,.F.);
#65641=ORIENTED_EDGE('',*,*,#47338,.T.);
#65642=ORIENTED_EDGE('',*,*,#47339,.F.);
#65643=ORIENTED_EDGE('',*,*,#47340,.F.);
#65644=ORIENTED_EDGE('',*,*,#47338,.F.);
#65645=ORIENTED_EDGE('',*,*,#47341,.T.);
#65646=ORIENTED_EDGE('',*,*,#47342,.F.);
#65647=ORIENTED_EDGE('',*,*,#47343,.T.);
#65648=ORIENTED_EDGE('',*,*,#47344,.T.);
#65649=ORIENTED_EDGE('',*,*,#47345,.T.);
#65650=ORIENTED_EDGE('',*,*,#47346,.F.);
#65651=ORIENTED_EDGE('',*,*,#47347,.T.);
#65652=ORIENTED_EDGE('',*,*,#47348,.T.);
#65653=ORIENTED_EDGE('',*,*,#47349,.F.);
#65654=ORIENTED_EDGE('',*,*,#47350,.T.);
#65655=ORIENTED_EDGE('',*,*,#47331,.T.);
#65656=ORIENTED_EDGE('',*,*,#47332,.T.);
#65657=ORIENTED_EDGE('',*,*,#47350,.F.);
#65658=ORIENTED_EDGE('',*,*,#47306,.T.);
#65659=ORIENTED_EDGE('',*,*,#47351,.T.);
#65660=ORIENTED_EDGE('',*,*,#47335,.T.);
#65661=ORIENTED_EDGE('',*,*,#47336,.T.);
#65662=ORIENTED_EDGE('',*,*,#47351,.F.);
#65663=ORIENTED_EDGE('',*,*,#47309,.T.);
#65664=ORIENTED_EDGE('',*,*,#47352,.T.);
#65665=ORIENTED_EDGE('',*,*,#47339,.T.);
#65666=ORIENTED_EDGE('',*,*,#47340,.T.);
#65667=ORIENTED_EDGE('',*,*,#47352,.F.);
#65668=ORIENTED_EDGE('',*,*,#47353,.T.);
#65669=ORIENTED_EDGE('',*,*,#47354,.T.);
#65670=ORIENTED_EDGE('',*,*,#47319,.T.);
#65671=ORIENTED_EDGE('',*,*,#47320,.T.);
#65672=ORIENTED_EDGE('',*,*,#47354,.F.);
#65673=ORIENTED_EDGE('',*,*,#47355,.T.);
#65674=ORIENTED_EDGE('',*,*,#47356,.T.);
#65675=ORIENTED_EDGE('',*,*,#47357,.F.);
#65676=ORIENTED_EDGE('',*,*,#47358,.F.);
#65677=ORIENTED_EDGE('',*,*,#47359,.T.);
#65678=ORIENTED_EDGE('',*,*,#47360,.T.);
#65679=ORIENTED_EDGE('',*,*,#47361,.F.);
#65680=ORIENTED_EDGE('',*,*,#47362,.F.);
#65681=ORIENTED_EDGE('',*,*,#47363,.T.);
#65682=ORIENTED_EDGE('',*,*,#47364,.T.);
#65683=ORIENTED_EDGE('',*,*,#47365,.T.);
#65684=ORIENTED_EDGE('',*,*,#47366,.T.);
#65685=ORIENTED_EDGE('',*,*,#47367,.T.);
#65686=ORIENTED_EDGE('',*,*,#47368,.T.);
#65687=ORIENTED_EDGE('',*,*,#47369,.T.);
#65688=ORIENTED_EDGE('',*,*,#47370,.T.);
#65689=ORIENTED_EDGE('',*,*,#47310,.T.);
#65690=ORIENTED_EDGE('',*,*,#47371,.T.);
#65691=ORIENTED_EDGE('',*,*,#47314,.T.);
#65692=ORIENTED_EDGE('',*,*,#47371,.F.);
#65693=ORIENTED_EDGE('',*,*,#47313,.T.);
#65694=ORIENTED_EDGE('',*,*,#47372,.F.);
#65695=ORIENTED_EDGE('',*,*,#47373,.F.);
#65696=ORIENTED_EDGE('',*,*,#47374,.F.);
#65697=ORIENTED_EDGE('',*,*,#47375,.F.);
#65698=ORIENTED_EDGE('',*,*,#47376,.F.);
#65699=ORIENTED_EDGE('',*,*,#47377,.F.);
#65700=ORIENTED_EDGE('',*,*,#47378,.F.);
#65701=ORIENTED_EDGE('',*,*,#47379,.F.);
#65702=ORIENTED_EDGE('',*,*,#47380,.F.);
#65703=ORIENTED_EDGE('',*,*,#47381,.F.);
#65704=ORIENTED_EDGE('',*,*,#47382,.F.);
#65705=ORIENTED_EDGE('',*,*,#47383,.F.);
#65706=ORIENTED_EDGE('',*,*,#47384,.F.);
#65707=ORIENTED_EDGE('',*,*,#47385,.F.);
#65708=ORIENTED_EDGE('',*,*,#47386,.F.);
#65709=ORIENTED_EDGE('',*,*,#47387,.F.);
#65710=ORIENTED_EDGE('',*,*,#47388,.F.);
#65711=ORIENTED_EDGE('',*,*,#47389,.F.);
#65712=ORIENTED_EDGE('',*,*,#47390,.F.);
#65713=ORIENTED_EDGE('',*,*,#47391,.F.);
#65714=ORIENTED_EDGE('',*,*,#47392,.F.);
#65715=ORIENTED_EDGE('',*,*,#47393,.F.);
#65716=ORIENTED_EDGE('',*,*,#47394,.F.);
#65717=ORIENTED_EDGE('',*,*,#47395,.F.);
#65718=ORIENTED_EDGE('',*,*,#47396,.F.);
#65719=ORIENTED_EDGE('',*,*,#47397,.F.);
#65720=ORIENTED_EDGE('',*,*,#47398,.F.);
#65721=ORIENTED_EDGE('',*,*,#47399,.F.);
#65722=ORIENTED_EDGE('',*,*,#47400,.F.);
#65723=ORIENTED_EDGE('',*,*,#47401,.F.);
#65724=ORIENTED_EDGE('',*,*,#47363,.F.);
#65725=ORIENTED_EDGE('',*,*,#47402,.F.);
#65726=ORIENTED_EDGE('',*,*,#47403,.F.);
#65727=ORIENTED_EDGE('',*,*,#47404,.F.);
#65728=ORIENTED_EDGE('',*,*,#47367,.F.);
#65729=ORIENTED_EDGE('',*,*,#47405,.F.);
#65730=ORIENTED_EDGE('',*,*,#47406,.F.);
#65731=ORIENTED_EDGE('',*,*,#47407,.F.);
#65732=ORIENTED_EDGE('',*,*,#47408,.F.);
#65733=ORIENTED_EDGE('',*,*,#47409,.F.);
#65734=ORIENTED_EDGE('',*,*,#47410,.F.);
#65735=ORIENTED_EDGE('',*,*,#47411,.F.);
#65736=ORIENTED_EDGE('',*,*,#47412,.F.);
#65737=ORIENTED_EDGE('',*,*,#47413,.F.);
#65738=ORIENTED_EDGE('',*,*,#47414,.F.);
#65739=ORIENTED_EDGE('',*,*,#47415,.F.);
#65740=ORIENTED_EDGE('',*,*,#47416,.F.);
#65741=ORIENTED_EDGE('',*,*,#47417,.F.);
#65742=ORIENTED_EDGE('',*,*,#47418,.F.);
#65743=ORIENTED_EDGE('',*,*,#47419,.F.);
#65744=ORIENTED_EDGE('',*,*,#47420,.F.);
#65745=ORIENTED_EDGE('',*,*,#47421,.F.);
#65746=ORIENTED_EDGE('',*,*,#47422,.F.);
#65747=ORIENTED_EDGE('',*,*,#47423,.F.);
#65748=ORIENTED_EDGE('',*,*,#47424,.F.);
#65749=ORIENTED_EDGE('',*,*,#47425,.F.);
#65750=ORIENTED_EDGE('',*,*,#47426,.F.);
#65751=ORIENTED_EDGE('',*,*,#47427,.F.);
#65752=ORIENTED_EDGE('',*,*,#47428,.F.);
#65753=ORIENTED_EDGE('',*,*,#47429,.F.);
#65754=ORIENTED_EDGE('',*,*,#47430,.F.);
#65755=ORIENTED_EDGE('',*,*,#47431,.F.);
#65756=ORIENTED_EDGE('',*,*,#47432,.F.);
#65757=ORIENTED_EDGE('',*,*,#47433,.F.);
#65758=ORIENTED_EDGE('',*,*,#47434,.F.);
#65759=ORIENTED_EDGE('',*,*,#47435,.F.);
#65760=ORIENTED_EDGE('',*,*,#47436,.F.);
#65761=ORIENTED_EDGE('',*,*,#47437,.F.);
#65762=ORIENTED_EDGE('',*,*,#47438,.F.);
#65763=ORIENTED_EDGE('',*,*,#47439,.F.);
#65764=ORIENTED_EDGE('',*,*,#47440,.F.);
#65765=ORIENTED_EDGE('',*,*,#47441,.F.);
#65766=ORIENTED_EDGE('',*,*,#47442,.F.);
#65767=ORIENTED_EDGE('',*,*,#47443,.F.);
#65768=ORIENTED_EDGE('',*,*,#47444,.F.);
#65769=ORIENTED_EDGE('',*,*,#47445,.F.);
#65770=ORIENTED_EDGE('',*,*,#47446,.F.);
#65771=ORIENTED_EDGE('',*,*,#47447,.F.);
#65772=ORIENTED_EDGE('',*,*,#47448,.F.);
#65773=ORIENTED_EDGE('',*,*,#47449,.F.);
#65774=ORIENTED_EDGE('',*,*,#47450,.F.);
#65775=ORIENTED_EDGE('',*,*,#47451,.F.);
#65776=ORIENTED_EDGE('',*,*,#47452,.F.);
#65777=ORIENTED_EDGE('',*,*,#47453,.F.);
#65778=ORIENTED_EDGE('',*,*,#47454,.F.);
#65779=ORIENTED_EDGE('',*,*,#47455,.F.);
#65780=ORIENTED_EDGE('',*,*,#47456,.F.);
#65781=ORIENTED_EDGE('',*,*,#47457,.F.);
#65782=ORIENTED_EDGE('',*,*,#47458,.F.);
#65783=ORIENTED_EDGE('',*,*,#47459,.F.);
#65784=ORIENTED_EDGE('',*,*,#47460,.F.);
#65785=ORIENTED_EDGE('',*,*,#47461,.F.);
#65786=ORIENTED_EDGE('',*,*,#47462,.F.);
#65787=ORIENTED_EDGE('',*,*,#47463,.F.);
#65788=ORIENTED_EDGE('',*,*,#47464,.F.);
#65789=ORIENTED_EDGE('',*,*,#47465,.F.);
#65790=ORIENTED_EDGE('',*,*,#47466,.F.);
#65791=ORIENTED_EDGE('',*,*,#47467,.F.);
#65792=ORIENTED_EDGE('',*,*,#47468,.F.);
#65793=ORIENTED_EDGE('',*,*,#47469,.F.);
#65794=ORIENTED_EDGE('',*,*,#47470,.F.);
#65795=ORIENTED_EDGE('',*,*,#47471,.F.);
#65796=ORIENTED_EDGE('',*,*,#47472,.F.);
#65797=ORIENTED_EDGE('',*,*,#47473,.F.);
#65798=ORIENTED_EDGE('',*,*,#47474,.F.);
#65799=ORIENTED_EDGE('',*,*,#47475,.F.);
#65800=ORIENTED_EDGE('',*,*,#47476,.F.);
#65801=ORIENTED_EDGE('',*,*,#47477,.F.);
#65802=ORIENTED_EDGE('',*,*,#47478,.F.);
#65803=ORIENTED_EDGE('',*,*,#47479,.F.);
#65804=ORIENTED_EDGE('',*,*,#47480,.F.);
#65805=ORIENTED_EDGE('',*,*,#47481,.F.);
#65806=ORIENTED_EDGE('',*,*,#47482,.F.);
#65807=ORIENTED_EDGE('',*,*,#47483,.F.);
#65808=ORIENTED_EDGE('',*,*,#47484,.F.);
#65809=ORIENTED_EDGE('',*,*,#47485,.F.);
#65810=ORIENTED_EDGE('',*,*,#47486,.F.);
#65811=ORIENTED_EDGE('',*,*,#47487,.F.);
#65812=ORIENTED_EDGE('',*,*,#47488,.F.);
#65813=ORIENTED_EDGE('',*,*,#47489,.F.);
#65814=ORIENTED_EDGE('',*,*,#47355,.F.);
#65815=ORIENTED_EDGE('',*,*,#47490,.F.);
#65816=ORIENTED_EDGE('',*,*,#47491,.F.);
#65817=ORIENTED_EDGE('',*,*,#47492,.F.);
#65818=ORIENTED_EDGE('',*,*,#47359,.F.);
#65819=ORIENTED_EDGE('',*,*,#47493,.F.);
#65820=ORIENTED_EDGE('',*,*,#47494,.F.);
#65821=ORIENTED_EDGE('',*,*,#47495,.F.);
#65822=ORIENTED_EDGE('',*,*,#47496,.F.);
#65823=ORIENTED_EDGE('',*,*,#47497,.F.);
#65824=ORIENTED_EDGE('',*,*,#47498,.F.);
#65825=ORIENTED_EDGE('',*,*,#47499,.F.);
#65826=ORIENTED_EDGE('',*,*,#47500,.F.);
#65827=ORIENTED_EDGE('',*,*,#47501,.F.);
#65828=ORIENTED_EDGE('',*,*,#47502,.F.);
#65829=ORIENTED_EDGE('',*,*,#47503,.F.);
#65830=ORIENTED_EDGE('',*,*,#47504,.F.);
#65831=ORIENTED_EDGE('',*,*,#47505,.F.);
#65832=ORIENTED_EDGE('',*,*,#47506,.F.);
#65833=ORIENTED_EDGE('',*,*,#47507,.F.);
#65834=ORIENTED_EDGE('',*,*,#47508,.F.);
#65835=ORIENTED_EDGE('',*,*,#47509,.F.);
#65836=ORIENTED_EDGE('',*,*,#47510,.F.);
#65837=ORIENTED_EDGE('',*,*,#47511,.F.);
#65838=ORIENTED_EDGE('',*,*,#47512,.F.);
#65839=ORIENTED_EDGE('',*,*,#47513,.F.);
#65840=ORIENTED_EDGE('',*,*,#47514,.F.);
#65841=ORIENTED_EDGE('',*,*,#47515,.F.);
#65842=ORIENTED_EDGE('',*,*,#47307,.T.);
#65843=ORIENTED_EDGE('',*,*,#47304,.T.);
#65844=ORIENTED_EDGE('',*,*,#47516,.T.);
#65845=ORIENTED_EDGE('',*,*,#47517,.T.);
#65846=ORIENTED_EDGE('',*,*,#47518,.T.);
#65847=ORIENTED_EDGE('',*,*,#47327,.T.);
#65848=ORIENTED_EDGE('',*,*,#47519,.T.);
#65849=ORIENTED_EDGE('',*,*,#47520,.T.);
#65850=ORIENTED_EDGE('',*,*,#47521,.T.);
#65851=ORIENTED_EDGE('',*,*,#47522,.T.);
#65852=ORIENTED_EDGE('',*,*,#47523,.T.);
#65853=ORIENTED_EDGE('',*,*,#47524,.T.);
#65854=ORIENTED_EDGE('',*,*,#47525,.T.);
#65855=ORIENTED_EDGE('',*,*,#47323,.T.);
#65856=ORIENTED_EDGE('',*,*,#47526,.T.);
#65857=ORIENTED_EDGE('',*,*,#47527,.T.);
#65858=ORIENTED_EDGE('',*,*,#47528,.T.);
#65859=ORIENTED_EDGE('',*,*,#47529,.T.);
#65860=ORIENTED_EDGE('',*,*,#47329,.T.);
#65861=ORIENTED_EDGE('',*,*,#47530,.F.);
#65862=ORIENTED_EDGE('',*,*,#47515,.T.);
#65863=ORIENTED_EDGE('',*,*,#47531,.F.);
#65864=ORIENTED_EDGE('',*,*,#47532,.F.);
#65865=ORIENTED_EDGE('',*,*,#47533,.F.);
#65866=ORIENTED_EDGE('',*,*,#47534,.F.);
#65867=ORIENTED_EDGE('',*,*,#47535,.F.);
#65868=ORIENTED_EDGE('',*,*,#47375,.T.);
#65869=ORIENTED_EDGE('',*,*,#47536,.F.);
#65870=ORIENTED_EDGE('',*,*,#47511,.T.);
#65871=ORIENTED_EDGE('',*,*,#47537,.F.);
#65872=ORIENTED_EDGE('',*,*,#47538,.F.);
#65873=ORIENTED_EDGE('',*,*,#47539,.F.);
#65874=ORIENTED_EDGE('',*,*,#47507,.T.);
#65875=ORIENTED_EDGE('',*,*,#47540,.F.);
#65876=ORIENTED_EDGE('',*,*,#47541,.F.);
#65877=ORIENTED_EDGE('',*,*,#47542,.F.);
#65878=ORIENTED_EDGE('',*,*,#47503,.T.);
#65879=ORIENTED_EDGE('',*,*,#47543,.F.);
#65880=ORIENTED_EDGE('',*,*,#47544,.F.);
#65881=ORIENTED_EDGE('',*,*,#47356,.F.);
#65882=ORIENTED_EDGE('',*,*,#47489,.T.);
#65883=ORIENTED_EDGE('',*,*,#47545,.F.);
#65884=ORIENTED_EDGE('',*,*,#47546,.F.);
#65885=ORIENTED_EDGE('',*,*,#47547,.F.);
#65886=ORIENTED_EDGE('',*,*,#47548,.F.);
#65887=ORIENTED_EDGE('',*,*,#47360,.F.);
#65888=ORIENTED_EDGE('',*,*,#47492,.T.);
#65889=ORIENTED_EDGE('',*,*,#47549,.F.);
#65890=ORIENTED_EDGE('',*,*,#47550,.F.);
#65891=ORIENTED_EDGE('',*,*,#47551,.F.);
#65892=ORIENTED_EDGE('',*,*,#47495,.T.);
#65893=ORIENTED_EDGE('',*,*,#47552,.F.);
#65894=ORIENTED_EDGE('',*,*,#47499,.T.);
#65895=ORIENTED_EDGE('',*,*,#47553,.F.);
#65896=ORIENTED_EDGE('',*,*,#47554,.F.);
#65897=ORIENTED_EDGE('',*,*,#47555,.F.);
#65898=ORIENTED_EDGE('',*,*,#47395,.T.);
#65899=ORIENTED_EDGE('',*,*,#47556,.F.);
#65900=ORIENTED_EDGE('',*,*,#47557,.F.);
#65901=ORIENTED_EDGE('',*,*,#47558,.F.);
#65902=ORIENTED_EDGE('',*,*,#47559,.F.);
#65903=ORIENTED_EDGE('',*,*,#47560,.F.);
#65904=ORIENTED_EDGE('',*,*,#47399,.T.);
#65905=ORIENTED_EDGE('',*,*,#47561,.F.);
#65906=ORIENTED_EDGE('',*,*,#47391,.T.);
#65907=ORIENTED_EDGE('',*,*,#47562,.F.);
#65908=ORIENTED_EDGE('',*,*,#47563,.F.);
#65909=ORIENTED_EDGE('',*,*,#47366,.F.);
#65910=ORIENTED_EDGE('',*,*,#47564,.F.);
#65911=ORIENTED_EDGE('',*,*,#47565,.F.);
#65912=ORIENTED_EDGE('',*,*,#47402,.T.);
#65913=ORIENTED_EDGE('',*,*,#47370,.F.);
#65914=ORIENTED_EDGE('',*,*,#47566,.F.);
#65915=ORIENTED_EDGE('',*,*,#47567,.F.);
#65916=ORIENTED_EDGE('',*,*,#47405,.T.);
#65917=ORIENTED_EDGE('',*,*,#47568,.F.);
#65918=ORIENTED_EDGE('',*,*,#47569,.F.);
#65919=ORIENTED_EDGE('',*,*,#47570,.F.);
#65920=ORIENTED_EDGE('',*,*,#47409,.T.);
#65921=ORIENTED_EDGE('',*,*,#47571,.F.);
#65922=ORIENTED_EDGE('',*,*,#47383,.T.);
#65923=ORIENTED_EDGE('',*,*,#47572,.F.);
#65924=ORIENTED_EDGE('',*,*,#47573,.F.);
#65925=ORIENTED_EDGE('',*,*,#47574,.F.);
#65926=ORIENTED_EDGE('',*,*,#47575,.F.);
#65927=ORIENTED_EDGE('',*,*,#47576,.F.);
#65928=ORIENTED_EDGE('',*,*,#47387,.T.);
#65929=ORIENTED_EDGE('',*,*,#47577,.F.);
#65930=ORIENTED_EDGE('',*,*,#47379,.T.);
#65931=ORIENTED_EDGE('',*,*,#47578,.F.);
#65932=ORIENTED_EDGE('',*,*,#47579,.F.);
#65933=ORIENTED_EDGE('',*,*,#47580,.F.);
#65934=ORIENTED_EDGE('',*,*,#47429,.T.);
#65935=ORIENTED_EDGE('',*,*,#47581,.F.);
#65936=ORIENTED_EDGE('',*,*,#47582,.F.);
#65937=ORIENTED_EDGE('',*,*,#47583,.F.);
#65938=ORIENTED_EDGE('',*,*,#47584,.F.);
#65939=ORIENTED_EDGE('',*,*,#47585,.F.);
#65940=ORIENTED_EDGE('',*,*,#47433,.T.);
#65941=ORIENTED_EDGE('',*,*,#47586,.F.);
#65942=ORIENTED_EDGE('',*,*,#47425,.T.);
#65943=ORIENTED_EDGE('',*,*,#47587,.F.);
#65944=ORIENTED_EDGE('',*,*,#47588,.F.);
#65945=ORIENTED_EDGE('',*,*,#47589,.F.);
#65946=ORIENTED_EDGE('',*,*,#47590,.F.);
#65947=ORIENTED_EDGE('',*,*,#47591,.F.);
#65948=ORIENTED_EDGE('',*,*,#47437,.T.);
#65949=ORIENTED_EDGE('',*,*,#47592,.F.);
#65950=ORIENTED_EDGE('',*,*,#47593,.F.);
#65951=ORIENTED_EDGE('',*,*,#47594,.F.);
#65952=ORIENTED_EDGE('',*,*,#47441,.T.);
#65953=ORIENTED_EDGE('',*,*,#47595,.F.);
#65954=ORIENTED_EDGE('',*,*,#47596,.F.);
#65955=ORIENTED_EDGE('',*,*,#47597,.F.);
#65956=ORIENTED_EDGE('',*,*,#47445,.T.);
#65957=ORIENTED_EDGE('',*,*,#47598,.F.);
#65958=ORIENTED_EDGE('',*,*,#47417,.T.);
#65959=ORIENTED_EDGE('',*,*,#47599,.F.);
#65960=ORIENTED_EDGE('',*,*,#47600,.F.);
#65961=ORIENTED_EDGE('',*,*,#47601,.F.);
#65962=ORIENTED_EDGE('',*,*,#47602,.F.);
#65963=ORIENTED_EDGE('',*,*,#47603,.F.);
#65964=ORIENTED_EDGE('',*,*,#47421,.T.);
#65965=ORIENTED_EDGE('',*,*,#47604,.F.);
#65966=ORIENTED_EDGE('',*,*,#47413,.T.);
#65967=ORIENTED_EDGE('',*,*,#47605,.F.);
#65968=ORIENTED_EDGE('',*,*,#47606,.F.);
#65969=ORIENTED_EDGE('',*,*,#47607,.F.);
#65970=ORIENTED_EDGE('',*,*,#47465,.T.);
#65971=ORIENTED_EDGE('',*,*,#47608,.F.);
#65972=ORIENTED_EDGE('',*,*,#47609,.F.);
#65973=ORIENTED_EDGE('',*,*,#47610,.F.);
#65974=ORIENTED_EDGE('',*,*,#47611,.F.);
#65975=ORIENTED_EDGE('',*,*,#47612,.F.);
#65976=ORIENTED_EDGE('',*,*,#47469,.T.);
#65977=ORIENTED_EDGE('',*,*,#47613,.F.);
#65978=ORIENTED_EDGE('',*,*,#47461,.T.);
#65979=ORIENTED_EDGE('',*,*,#47614,.F.);
#65980=ORIENTED_EDGE('',*,*,#47615,.F.);
#65981=ORIENTED_EDGE('',*,*,#47616,.F.);
#65982=ORIENTED_EDGE('',*,*,#47617,.F.);
#65983=ORIENTED_EDGE('',*,*,#47618,.F.);
#65984=ORIENTED_EDGE('',*,*,#47473,.T.);
#65985=ORIENTED_EDGE('',*,*,#47619,.F.);
#65986=ORIENTED_EDGE('',*,*,#47620,.F.);
#65987=ORIENTED_EDGE('',*,*,#47621,.F.);
#65988=ORIENTED_EDGE('',*,*,#47477,.T.);
#65989=ORIENTED_EDGE('',*,*,#47622,.F.);
#65990=ORIENTED_EDGE('',*,*,#47623,.F.);
#65991=ORIENTED_EDGE('',*,*,#47624,.F.);
#65992=ORIENTED_EDGE('',*,*,#47481,.T.);
#65993=ORIENTED_EDGE('',*,*,#47625,.F.);
#65994=ORIENTED_EDGE('',*,*,#47457,.T.);
#65995=ORIENTED_EDGE('',*,*,#47626,.F.);
#65996=ORIENTED_EDGE('',*,*,#47627,.F.);
#65997=ORIENTED_EDGE('',*,*,#47628,.F.);
#65998=ORIENTED_EDGE('',*,*,#47453,.T.);
#65999=ORIENTED_EDGE('',*,*,#47629,.F.);
#66000=ORIENTED_EDGE('',*,*,#47630,.F.);
#66001=ORIENTED_EDGE('',*,*,#47631,.F.);
#66002=ORIENTED_EDGE('',*,*,#47449,.T.);
#66003=ORIENTED_EDGE('',*,*,#47632,.F.);
#66004=ORIENTED_EDGE('',*,*,#47633,.F.);
#66005=ORIENTED_EDGE('',*,*,#47634,.T.);
#66006=ORIENTED_EDGE('',*,*,#47532,.T.);
#66007=ORIENTED_EDGE('',*,*,#47635,.F.);
#66008=ORIENTED_EDGE('',*,*,#47636,.T.);
#66009=ORIENTED_EDGE('',*,*,#47637,.T.);
#66010=ORIENTED_EDGE('',*,*,#47538,.T.);
#66011=ORIENTED_EDGE('',*,*,#47638,.F.);
#66012=ORIENTED_EDGE('',*,*,#47639,.T.);
#66013=ORIENTED_EDGE('',*,*,#47640,.T.);
#66014=ORIENTED_EDGE('',*,*,#47541,.T.);
#66015=ORIENTED_EDGE('',*,*,#47641,.F.);
#66016=ORIENTED_EDGE('',*,*,#47642,.T.);
#66017=ORIENTED_EDGE('',*,*,#47643,.T.);
#66018=ORIENTED_EDGE('',*,*,#47544,.T.);
#66019=ORIENTED_EDGE('',*,*,#47644,.F.);
#66020=ORIENTED_EDGE('',*,*,#47645,.T.);
#66021=ORIENTED_EDGE('',*,*,#47646,.T.);
#66022=ORIENTED_EDGE('',*,*,#47554,.T.);
#66023=ORIENTED_EDGE('',*,*,#47647,.F.);
#66024=ORIENTED_EDGE('',*,*,#47648,.T.);
#66025=ORIENTED_EDGE('',*,*,#47649,.T.);
#66026=ORIENTED_EDGE('',*,*,#47550,.T.);
#66027=ORIENTED_EDGE('',*,*,#47650,.F.);
#66028=ORIENTED_EDGE('',*,*,#47651,.T.);
#66029=ORIENTED_EDGE('',*,*,#47361,.T.);
#66030=ORIENTED_EDGE('',*,*,#47548,.T.);
#66031=ORIENTED_EDGE('',*,*,#47652,.F.);
#66032=ORIENTED_EDGE('',*,*,#47653,.T.);
#66033=ORIENTED_EDGE('',*,*,#47357,.T.);
#66034=ORIENTED_EDGE('',*,*,#47546,.T.);
#66035=ORIENTED_EDGE('',*,*,#47654,.F.);
#66036=ORIENTED_EDGE('',*,*,#47655,.T.);
#66037=ORIENTED_EDGE('',*,*,#47656,.T.);
#66038=ORIENTED_EDGE('',*,*,#47657,.T.);
#66039=ORIENTED_EDGE('',*,*,#47658,.F.);
#66040=ORIENTED_EDGE('',*,*,#47659,.T.);
#66041=ORIENTED_EDGE('',*,*,#47660,.T.);
#66042=ORIENTED_EDGE('',*,*,#47623,.T.);
#66043=ORIENTED_EDGE('',*,*,#47661,.F.);
#66044=ORIENTED_EDGE('',*,*,#47662,.T.);
#66045=ORIENTED_EDGE('',*,*,#47663,.T.);
#66046=ORIENTED_EDGE('',*,*,#47620,.T.);
#66047=ORIENTED_EDGE('',*,*,#47664,.F.);
#66048=ORIENTED_EDGE('',*,*,#47665,.T.);
#66049=ORIENTED_EDGE('',*,*,#47666,.T.);
#66050=ORIENTED_EDGE('',*,*,#47617,.T.);
#66051=ORIENTED_EDGE('',*,*,#47667,.F.);
#66052=ORIENTED_EDGE('',*,*,#47668,.T.);
#66053=ORIENTED_EDGE('',*,*,#47669,.T.);
#66054=ORIENTED_EDGE('',*,*,#47611,.T.);
#66055=ORIENTED_EDGE('',*,*,#47670,.F.);
#66056=ORIENTED_EDGE('',*,*,#47671,.T.);
#66057=ORIENTED_EDGE('',*,*,#47672,.T.);
#66058=ORIENTED_EDGE('',*,*,#47609,.T.);
#66059=ORIENTED_EDGE('',*,*,#47673,.F.);
#66060=ORIENTED_EDGE('',*,*,#47674,.T.);
#66061=ORIENTED_EDGE('',*,*,#47675,.T.);
#66062=ORIENTED_EDGE('',*,*,#47615,.T.);
#66063=ORIENTED_EDGE('',*,*,#47676,.F.);
#66064=ORIENTED_EDGE('',*,*,#47677,.T.);
#66065=ORIENTED_EDGE('',*,*,#47678,.T.);
#66066=ORIENTED_EDGE('',*,*,#47627,.T.);
#66067=ORIENTED_EDGE('',*,*,#47679,.F.);
#66068=ORIENTED_EDGE('',*,*,#47680,.T.);
#66069=ORIENTED_EDGE('',*,*,#47681,.T.);
#66070=ORIENTED_EDGE('',*,*,#47630,.T.);
#66071=ORIENTED_EDGE('',*,*,#47682,.F.);
#66072=ORIENTED_EDGE('',*,*,#47683,.T.);
#66073=ORIENTED_EDGE('',*,*,#47684,.T.);
#66074=ORIENTED_EDGE('',*,*,#47633,.T.);
#66075=ORIENTED_EDGE('',*,*,#47685,.F.);
#66076=ORIENTED_EDGE('',*,*,#47686,.T.);
#66077=ORIENTED_EDGE('',*,*,#47687,.T.);
#66078=ORIENTED_EDGE('',*,*,#47596,.T.);
#66079=ORIENTED_EDGE('',*,*,#47688,.F.);
#66080=ORIENTED_EDGE('',*,*,#47689,.T.);
#66081=ORIENTED_EDGE('',*,*,#47690,.T.);
#66082=ORIENTED_EDGE('',*,*,#47593,.T.);
#66083=ORIENTED_EDGE('',*,*,#47691,.F.);
#66084=ORIENTED_EDGE('',*,*,#47692,.T.);
#66085=ORIENTED_EDGE('',*,*,#47693,.T.);
#66086=ORIENTED_EDGE('',*,*,#47590,.T.);
#66087=ORIENTED_EDGE('',*,*,#47694,.F.);
#66088=ORIENTED_EDGE('',*,*,#47695,.T.);
#66089=ORIENTED_EDGE('',*,*,#47696,.T.);
#66090=ORIENTED_EDGE('',*,*,#47584,.T.);
#66091=ORIENTED_EDGE('',*,*,#47697,.F.);
#66092=ORIENTED_EDGE('',*,*,#47698,.T.);
#66093=ORIENTED_EDGE('',*,*,#47699,.T.);
#66094=ORIENTED_EDGE('',*,*,#47582,.T.);
#66095=ORIENTED_EDGE('',*,*,#47700,.F.);
#66096=ORIENTED_EDGE('',*,*,#47701,.T.);
#66097=ORIENTED_EDGE('',*,*,#47702,.T.);
#66098=ORIENTED_EDGE('',*,*,#47588,.T.);
#66099=ORIENTED_EDGE('',*,*,#47703,.F.);
#66100=ORIENTED_EDGE('',*,*,#47704,.T.);
#66101=ORIENTED_EDGE('',*,*,#47705,.T.);
#66102=ORIENTED_EDGE('',*,*,#47602,.T.);
#66103=ORIENTED_EDGE('',*,*,#47706,.F.);
#66104=ORIENTED_EDGE('',*,*,#47707,.T.);
#66105=ORIENTED_EDGE('',*,*,#47708,.T.);
#66106=ORIENTED_EDGE('',*,*,#47600,.T.);
#66107=ORIENTED_EDGE('',*,*,#47709,.F.);
#66108=ORIENTED_EDGE('',*,*,#47710,.T.);
#66109=ORIENTED_EDGE('',*,*,#47711,.T.);
#66110=ORIENTED_EDGE('',*,*,#47606,.T.);
#66111=ORIENTED_EDGE('',*,*,#47712,.F.);
#66112=ORIENTED_EDGE('',*,*,#47713,.T.);
#66113=ORIENTED_EDGE('',*,*,#47714,.T.);
#66114=ORIENTED_EDGE('',*,*,#47569,.T.);
#66115=ORIENTED_EDGE('',*,*,#47715,.F.);
#66116=ORIENTED_EDGE('',*,*,#47716,.T.);
#66117=ORIENTED_EDGE('',*,*,#47717,.T.);
#66118=ORIENTED_EDGE('',*,*,#47566,.T.);
#66119=ORIENTED_EDGE('',*,*,#47369,.F.);
#66120=ORIENTED_EDGE('',*,*,#47718,.T.);
#66121=ORIENTED_EDGE('',*,*,#47719,.T.);
#66122=ORIENTED_EDGE('',*,*,#47564,.T.);
#66123=ORIENTED_EDGE('',*,*,#47365,.F.);
#66124=ORIENTED_EDGE('',*,*,#47720,.T.);
#66125=ORIENTED_EDGE('',*,*,#47721,.T.);
#66126=ORIENTED_EDGE('',*,*,#47559,.T.);
#66127=ORIENTED_EDGE('',*,*,#47722,.F.);
#66128=ORIENTED_EDGE('',*,*,#47723,.T.);
#66129=ORIENTED_EDGE('',*,*,#47724,.T.);
#66130=ORIENTED_EDGE('',*,*,#47557,.T.);
#66131=ORIENTED_EDGE('',*,*,#47725,.F.);
#66132=ORIENTED_EDGE('',*,*,#47726,.T.);
#66133=ORIENTED_EDGE('',*,*,#47727,.T.);
#66134=ORIENTED_EDGE('',*,*,#47563,.T.);
#66135=ORIENTED_EDGE('',*,*,#47728,.F.);
#66136=ORIENTED_EDGE('',*,*,#47729,.T.);
#66137=ORIENTED_EDGE('',*,*,#47730,.T.);
#66138=ORIENTED_EDGE('',*,*,#47575,.T.);
#66139=ORIENTED_EDGE('',*,*,#47731,.F.);
#66140=ORIENTED_EDGE('',*,*,#47732,.T.);
#66141=ORIENTED_EDGE('',*,*,#47733,.T.);
#66142=ORIENTED_EDGE('',*,*,#47573,.T.);
#66143=ORIENTED_EDGE('',*,*,#47734,.F.);
#66144=ORIENTED_EDGE('',*,*,#47735,.T.);
#66145=ORIENTED_EDGE('',*,*,#47736,.T.);
#66146=ORIENTED_EDGE('',*,*,#47579,.T.);
#66147=ORIENTED_EDGE('',*,*,#47737,.F.);
#66148=ORIENTED_EDGE('',*,*,#47738,.T.);
#66149=ORIENTED_EDGE('',*,*,#47739,.T.);
#66150=ORIENTED_EDGE('',*,*,#47534,.T.);
#66151=ORIENTED_EDGE('',*,*,#47740,.F.);
#66152=ORIENTED_EDGE('',*,*,#47741,.T.);
#66153=ORIENTED_EDGE('',*,*,#47300,.F.);
#66154=ORIENTED_EDGE('',*,*,#47303,.F.);
#66155=ORIENTED_EDGE('',*,*,#47353,.F.);
#66156=ORIENTED_EDGE('',*,*,#47742,.F.);
#66157=ORIENTED_EDGE('',*,*,#47485,.T.);
#66158=ORIENTED_EDGE('',*,*,#47743,.F.);
#66159=ORIENTED_EDGE('',*,*,#47657,.F.);
#66160=ORIENTED_EDGE('',*,*,#47624,.T.);
#66161=ORIENTED_EDGE('',*,*,#47660,.F.);
#66162=ORIENTED_EDGE('',*,*,#47744,.F.);
#66163=ORIENTED_EDGE('',*,*,#47482,.T.);
#66164=ORIENTED_EDGE('',*,*,#47743,.T.);
#66165=ORIENTED_EDGE('',*,*,#47484,.T.);
#66166=ORIENTED_EDGE('',*,*,#47745,.T.);
#66167=ORIENTED_EDGE('',*,*,#47658,.T.);
#66168=ORIENTED_EDGE('',*,*,#47659,.F.);
#66169=ORIENTED_EDGE('',*,*,#47745,.F.);
#66170=ORIENTED_EDGE('',*,*,#47483,.T.);
#66171=ORIENTED_EDGE('',*,*,#47744,.T.);
#66172=ORIENTED_EDGE('',*,*,#47742,.T.);
#66173=ORIENTED_EDGE('',*,*,#47656,.F.);
#66174=ORIENTED_EDGE('',*,*,#47746,.F.);
#66175=ORIENTED_EDGE('',*,*,#47486,.T.);
#66176=ORIENTED_EDGE('',*,*,#47545,.T.);
#66177=ORIENTED_EDGE('',*,*,#47488,.T.);
#66178=ORIENTED_EDGE('',*,*,#47747,.T.);
#66179=ORIENTED_EDGE('',*,*,#47654,.T.);
#66180=ORIENTED_EDGE('',*,*,#47655,.F.);
#66181=ORIENTED_EDGE('',*,*,#47747,.F.);
#66182=ORIENTED_EDGE('',*,*,#47487,.T.);
#66183=ORIENTED_EDGE('',*,*,#47746,.T.);
#66184=ORIENTED_EDGE('',*,*,#47597,.T.);
#66185=ORIENTED_EDGE('',*,*,#47687,.F.);
#66186=ORIENTED_EDGE('',*,*,#47748,.F.);
#66187=ORIENTED_EDGE('',*,*,#47446,.T.);
#66188=ORIENTED_EDGE('',*,*,#47632,.T.);
#66189=ORIENTED_EDGE('',*,*,#47448,.T.);
#66190=ORIENTED_EDGE('',*,*,#47749,.T.);
#66191=ORIENTED_EDGE('',*,*,#47685,.T.);
#66192=ORIENTED_EDGE('',*,*,#47686,.F.);
#66193=ORIENTED_EDGE('',*,*,#47749,.F.);
#66194=ORIENTED_EDGE('',*,*,#47447,.T.);
#66195=ORIENTED_EDGE('',*,*,#47748,.T.);
#66196=ORIENTED_EDGE('',*,*,#47631,.T.);
#66197=ORIENTED_EDGE('',*,*,#47684,.F.);
#66198=ORIENTED_EDGE('',*,*,#47750,.F.);
#66199=ORIENTED_EDGE('',*,*,#47450,.T.);
#66200=ORIENTED_EDGE('',*,*,#47629,.T.);
#66201=ORIENTED_EDGE('',*,*,#47452,.T.);
#66202=ORIENTED_EDGE('',*,*,#47751,.T.);
#66203=ORIENTED_EDGE('',*,*,#47682,.T.);
#66204=ORIENTED_EDGE('',*,*,#47683,.F.);
#66205=ORIENTED_EDGE('',*,*,#47751,.F.);
#66206=ORIENTED_EDGE('',*,*,#47451,.T.);
#66207=ORIENTED_EDGE('',*,*,#47750,.T.);
#66208=ORIENTED_EDGE('',*,*,#47628,.T.);
#66209=ORIENTED_EDGE('',*,*,#47681,.F.);
#66210=ORIENTED_EDGE('',*,*,#47752,.F.);
#66211=ORIENTED_EDGE('',*,*,#47454,.T.);
#66212=ORIENTED_EDGE('',*,*,#47626,.T.);
#66213=ORIENTED_EDGE('',*,*,#47456,.T.);
#66214=ORIENTED_EDGE('',*,*,#47753,.T.);
#66215=ORIENTED_EDGE('',*,*,#47679,.T.);
#66216=ORIENTED_EDGE('',*,*,#47680,.F.);
#66217=ORIENTED_EDGE('',*,*,#47753,.F.);
#66218=ORIENTED_EDGE('',*,*,#47455,.T.);
#66219=ORIENTED_EDGE('',*,*,#47752,.T.);
#66220=ORIENTED_EDGE('',*,*,#47625,.T.);
#66221=ORIENTED_EDGE('',*,*,#47678,.F.);
#66222=ORIENTED_EDGE('',*,*,#47754,.F.);
#66223=ORIENTED_EDGE('',*,*,#47458,.T.);
#66224=ORIENTED_EDGE('',*,*,#47614,.T.);
#66225=ORIENTED_EDGE('',*,*,#47460,.T.);
#66226=ORIENTED_EDGE('',*,*,#47755,.T.);
#66227=ORIENTED_EDGE('',*,*,#47676,.T.);
#66228=ORIENTED_EDGE('',*,*,#47677,.F.);
#66229=ORIENTED_EDGE('',*,*,#47755,.F.);
#66230=ORIENTED_EDGE('',*,*,#47459,.T.);
#66231=ORIENTED_EDGE('',*,*,#47754,.T.);
#66232=ORIENTED_EDGE('',*,*,#47621,.T.);
#66233=ORIENTED_EDGE('',*,*,#47663,.F.);
#66234=ORIENTED_EDGE('',*,*,#47756,.F.);
#66235=ORIENTED_EDGE('',*,*,#47478,.T.);
#66236=ORIENTED_EDGE('',*,*,#47622,.T.);
#66237=ORIENTED_EDGE('',*,*,#47480,.T.);
#66238=ORIENTED_EDGE('',*,*,#47757,.T.);
#66239=ORIENTED_EDGE('',*,*,#47661,.T.);
#66240=ORIENTED_EDGE('',*,*,#47662,.F.);
#66241=ORIENTED_EDGE('',*,*,#47757,.F.);
#66242=ORIENTED_EDGE('',*,*,#47479,.T.);
#66243=ORIENTED_EDGE('',*,*,#47756,.T.);
#66244=ORIENTED_EDGE('',*,*,#47618,.T.);
#66245=ORIENTED_EDGE('',*,*,#47666,.F.);
#66246=ORIENTED_EDGE('',*,*,#47758,.F.);
#66247=ORIENTED_EDGE('',*,*,#47474,.T.);
#66248=ORIENTED_EDGE('',*,*,#47619,.T.);
#66249=ORIENTED_EDGE('',*,*,#47476,.T.);
#66250=ORIENTED_EDGE('',*,*,#47759,.T.);
#66251=ORIENTED_EDGE('',*,*,#47664,.T.);
#66252=ORIENTED_EDGE('',*,*,#47665,.F.);
#66253=ORIENTED_EDGE('',*,*,#47759,.F.);
#66254=ORIENTED_EDGE('',*,*,#47475,.T.);
#66255=ORIENTED_EDGE('',*,*,#47758,.T.);
#66256=ORIENTED_EDGE('',*,*,#47612,.T.);
#66257=ORIENTED_EDGE('',*,*,#47669,.F.);
#66258=ORIENTED_EDGE('',*,*,#47760,.F.);
#66259=ORIENTED_EDGE('',*,*,#47470,.T.);
#66260=ORIENTED_EDGE('',*,*,#47616,.T.);
#66261=ORIENTED_EDGE('',*,*,#47472,.T.);
#66262=ORIENTED_EDGE('',*,*,#47761,.T.);
#66263=ORIENTED_EDGE('',*,*,#47667,.T.);
#66264=ORIENTED_EDGE('',*,*,#47668,.F.);
#66265=ORIENTED_EDGE('',*,*,#47761,.F.);
#66266=ORIENTED_EDGE('',*,*,#47471,.T.);
#66267=ORIENTED_EDGE('',*,*,#47760,.T.);
#66268=ORIENTED_EDGE('',*,*,#47613,.T.);
#66269=ORIENTED_EDGE('',*,*,#47675,.F.);
#66270=ORIENTED_EDGE('',*,*,#47762,.F.);
#66271=ORIENTED_EDGE('',*,*,#47462,.T.);
#66272=ORIENTED_EDGE('',*,*,#47608,.T.);
#66273=ORIENTED_EDGE('',*,*,#47464,.T.);
#66274=ORIENTED_EDGE('',*,*,#47763,.T.);
#66275=ORIENTED_EDGE('',*,*,#47673,.T.);
#66276=ORIENTED_EDGE('',*,*,#47674,.F.);
#66277=ORIENTED_EDGE('',*,*,#47763,.F.);
#66278=ORIENTED_EDGE('',*,*,#47463,.T.);
#66279=ORIENTED_EDGE('',*,*,#47762,.T.);
#66280=ORIENTED_EDGE('',*,*,#47607,.T.);
#66281=ORIENTED_EDGE('',*,*,#47672,.F.);
#66282=ORIENTED_EDGE('',*,*,#47764,.F.);
#66283=ORIENTED_EDGE('',*,*,#47466,.T.);
#66284=ORIENTED_EDGE('',*,*,#47610,.T.);
#66285=ORIENTED_EDGE('',*,*,#47468,.T.);
#66286=ORIENTED_EDGE('',*,*,#47765,.T.);
#66287=ORIENTED_EDGE('',*,*,#47670,.T.);
#66288=ORIENTED_EDGE('',*,*,#47671,.F.);
#66289=ORIENTED_EDGE('',*,*,#47765,.F.);
#66290=ORIENTED_EDGE('',*,*,#47467,.T.);
#66291=ORIENTED_EDGE('',*,*,#47764,.T.);
#66292=ORIENTED_EDGE('',*,*,#47570,.T.);
#66293=ORIENTED_EDGE('',*,*,#47714,.F.);
#66294=ORIENTED_EDGE('',*,*,#47766,.F.);
#66295=ORIENTED_EDGE('',*,*,#47410,.T.);
#66296=ORIENTED_EDGE('',*,*,#47605,.T.);
#66297=ORIENTED_EDGE('',*,*,#47412,.T.);
#66298=ORIENTED_EDGE('',*,*,#47767,.T.);
#66299=ORIENTED_EDGE('',*,*,#47712,.T.);
#66300=ORIENTED_EDGE('',*,*,#47713,.F.);
#66301=ORIENTED_EDGE('',*,*,#47767,.F.);
#66302=ORIENTED_EDGE('',*,*,#47411,.T.);
#66303=ORIENTED_EDGE('',*,*,#47766,.T.);
#66304=ORIENTED_EDGE('',*,*,#47604,.T.);
#66305=ORIENTED_EDGE('',*,*,#47711,.F.);
#66306=ORIENTED_EDGE('',*,*,#47768,.F.);
#66307=ORIENTED_EDGE('',*,*,#47414,.T.);
#66308=ORIENTED_EDGE('',*,*,#47599,.T.);
#66309=ORIENTED_EDGE('',*,*,#47416,.T.);
#66310=ORIENTED_EDGE('',*,*,#47769,.T.);
#66311=ORIENTED_EDGE('',*,*,#47709,.T.);
#66312=ORIENTED_EDGE('',*,*,#47710,.F.);
#66313=ORIENTED_EDGE('',*,*,#47769,.F.);
#66314=ORIENTED_EDGE('',*,*,#47415,.T.);
#66315=ORIENTED_EDGE('',*,*,#47768,.T.);
#66316=ORIENTED_EDGE('',*,*,#47603,.T.);
#66317=ORIENTED_EDGE('',*,*,#47705,.F.);
#66318=ORIENTED_EDGE('',*,*,#47770,.F.);
#66319=ORIENTED_EDGE('',*,*,#47422,.T.);
#66320=ORIENTED_EDGE('',*,*,#47587,.T.);
#66321=ORIENTED_EDGE('',*,*,#47424,.T.);
#66322=ORIENTED_EDGE('',*,*,#47771,.T.);
#66323=ORIENTED_EDGE('',*,*,#47703,.T.);
#66324=ORIENTED_EDGE('',*,*,#47704,.F.);
#66325=ORIENTED_EDGE('',*,*,#47771,.F.);
#66326=ORIENTED_EDGE('',*,*,#47423,.T.);
#66327=ORIENTED_EDGE('',*,*,#47770,.T.);
#66328=ORIENTED_EDGE('',*,*,#47598,.T.);
#66329=ORIENTED_EDGE('',*,*,#47708,.F.);
#66330=ORIENTED_EDGE('',*,*,#47772,.F.);
#66331=ORIENTED_EDGE('',*,*,#47418,.T.);
#66332=ORIENTED_EDGE('',*,*,#47601,.T.);
#66333=ORIENTED_EDGE('',*,*,#47420,.T.);
#66334=ORIENTED_EDGE('',*,*,#47773,.T.);
#66335=ORIENTED_EDGE('',*,*,#47706,.T.);
#66336=ORIENTED_EDGE('',*,*,#47707,.F.);
#66337=ORIENTED_EDGE('',*,*,#47773,.F.);
#66338=ORIENTED_EDGE('',*,*,#47419,.T.);
#66339=ORIENTED_EDGE('',*,*,#47772,.T.);
#66340=ORIENTED_EDGE('',*,*,#47594,.T.);
#66341=ORIENTED_EDGE('',*,*,#47690,.F.);
#66342=ORIENTED_EDGE('',*,*,#47774,.F.);
#66343=ORIENTED_EDGE('',*,*,#47442,.T.);
#66344=ORIENTED_EDGE('',*,*,#47595,.T.);
#66345=ORIENTED_EDGE('',*,*,#47444,.T.);
#66346=ORIENTED_EDGE('',*,*,#47775,.T.);
#66347=ORIENTED_EDGE('',*,*,#47688,.T.);
#66348=ORIENTED_EDGE('',*,*,#47689,.F.);
#66349=ORIENTED_EDGE('',*,*,#47775,.F.);
#66350=ORIENTED_EDGE('',*,*,#47443,.T.);
#66351=ORIENTED_EDGE('',*,*,#47774,.T.);
#66352=ORIENTED_EDGE('',*,*,#47591,.T.);
#66353=ORIENTED_EDGE('',*,*,#47693,.F.);
#66354=ORIENTED_EDGE('',*,*,#47776,.F.);
#66355=ORIENTED_EDGE('',*,*,#47438,.T.);
#66356=ORIENTED_EDGE('',*,*,#47592,.T.);
#66357=ORIENTED_EDGE('',*,*,#47440,.T.);
#66358=ORIENTED_EDGE('',*,*,#47777,.T.);
#66359=ORIENTED_EDGE('',*,*,#47691,.T.);
#66360=ORIENTED_EDGE('',*,*,#47692,.F.);
#66361=ORIENTED_EDGE('',*,*,#47777,.F.);
#66362=ORIENTED_EDGE('',*,*,#47439,.T.);
#66363=ORIENTED_EDGE('',*,*,#47776,.T.);
#66364=ORIENTED_EDGE('',*,*,#47585,.T.);
#66365=ORIENTED_EDGE('',*,*,#47696,.F.);
#66366=ORIENTED_EDGE('',*,*,#47778,.F.);
#66367=ORIENTED_EDGE('',*,*,#47434,.T.);
#66368=ORIENTED_EDGE('',*,*,#47589,.T.);
#66369=ORIENTED_EDGE('',*,*,#47436,.T.);
#66370=ORIENTED_EDGE('',*,*,#47779,.T.);
#66371=ORIENTED_EDGE('',*,*,#47694,.T.);
#66372=ORIENTED_EDGE('',*,*,#47695,.F.);
#66373=ORIENTED_EDGE('',*,*,#47779,.F.);
#66374=ORIENTED_EDGE('',*,*,#47435,.T.);
#66375=ORIENTED_EDGE('',*,*,#47778,.T.);
#66376=ORIENTED_EDGE('',*,*,#47586,.T.);
#66377=ORIENTED_EDGE('',*,*,#47702,.F.);
#66378=ORIENTED_EDGE('',*,*,#47780,.F.);
#66379=ORIENTED_EDGE('',*,*,#47426,.T.);
#66380=ORIENTED_EDGE('',*,*,#47581,.T.);
#66381=ORIENTED_EDGE('',*,*,#47428,.T.);
#66382=ORIENTED_EDGE('',*,*,#47781,.T.);
#66383=ORIENTED_EDGE('',*,*,#47700,.T.);
#66384=ORIENTED_EDGE('',*,*,#47701,.F.);
#66385=ORIENTED_EDGE('',*,*,#47781,.F.);
#66386=ORIENTED_EDGE('',*,*,#47427,.T.);
#66387=ORIENTED_EDGE('',*,*,#47780,.T.);
#66388=ORIENTED_EDGE('',*,*,#47580,.T.);
#66389=ORIENTED_EDGE('',*,*,#47699,.F.);
#66390=ORIENTED_EDGE('',*,*,#47782,.F.);
#66391=ORIENTED_EDGE('',*,*,#47430,.T.);
#66392=ORIENTED_EDGE('',*,*,#47583,.T.);
#66393=ORIENTED_EDGE('',*,*,#47432,.T.);
#66394=ORIENTED_EDGE('',*,*,#47783,.T.);
#66395=ORIENTED_EDGE('',*,*,#47697,.T.);
#66396=ORIENTED_EDGE('',*,*,#47698,.F.);
#66397=ORIENTED_EDGE('',*,*,#47783,.F.);
#66398=ORIENTED_EDGE('',*,*,#47431,.T.);
#66399=ORIENTED_EDGE('',*,*,#47782,.T.);
#66400=ORIENTED_EDGE('',*,*,#47535,.T.);
#66401=ORIENTED_EDGE('',*,*,#47739,.F.);
#66402=ORIENTED_EDGE('',*,*,#47784,.F.);
#66403=ORIENTED_EDGE('',*,*,#47376,.T.);
#66404=ORIENTED_EDGE('',*,*,#47578,.T.);
#66405=ORIENTED_EDGE('',*,*,#47378,.T.);
#66406=ORIENTED_EDGE('',*,*,#47785,.T.);
#66407=ORIENTED_EDGE('',*,*,#47737,.T.);
#66408=ORIENTED_EDGE('',*,*,#47738,.F.);
#66409=ORIENTED_EDGE('',*,*,#47785,.F.);
#66410=ORIENTED_EDGE('',*,*,#47377,.T.);
#66411=ORIENTED_EDGE('',*,*,#47784,.T.);
#66412=ORIENTED_EDGE('',*,*,#47577,.T.);
#66413=ORIENTED_EDGE('',*,*,#47736,.F.);
#66414=ORIENTED_EDGE('',*,*,#47786,.F.);
#66415=ORIENTED_EDGE('',*,*,#47380,.T.);
#66416=ORIENTED_EDGE('',*,*,#47572,.T.);
#66417=ORIENTED_EDGE('',*,*,#47382,.T.);
#66418=ORIENTED_EDGE('',*,*,#47787,.T.);
#66419=ORIENTED_EDGE('',*,*,#47734,.T.);
#66420=ORIENTED_EDGE('',*,*,#47735,.F.);
#66421=ORIENTED_EDGE('',*,*,#47787,.F.);
#66422=ORIENTED_EDGE('',*,*,#47381,.T.);
#66423=ORIENTED_EDGE('',*,*,#47786,.T.);
#66424=ORIENTED_EDGE('',*,*,#47576,.T.);
#66425=ORIENTED_EDGE('',*,*,#47730,.F.);
#66426=ORIENTED_EDGE('',*,*,#47788,.F.);
#66427=ORIENTED_EDGE('',*,*,#47388,.T.);
#66428=ORIENTED_EDGE('',*,*,#47562,.T.);
#66429=ORIENTED_EDGE('',*,*,#47390,.T.);
#66430=ORIENTED_EDGE('',*,*,#47789,.T.);
#66431=ORIENTED_EDGE('',*,*,#47728,.T.);
#66432=ORIENTED_EDGE('',*,*,#47729,.F.);
#66433=ORIENTED_EDGE('',*,*,#47789,.F.);
#66434=ORIENTED_EDGE('',*,*,#47389,.T.);
#66435=ORIENTED_EDGE('',*,*,#47788,.T.);
#66436=ORIENTED_EDGE('',*,*,#47571,.T.);
#66437=ORIENTED_EDGE('',*,*,#47733,.F.);
#66438=ORIENTED_EDGE('',*,*,#47790,.F.);
#66439=ORIENTED_EDGE('',*,*,#47384,.T.);
#66440=ORIENTED_EDGE('',*,*,#47574,.T.);
#66441=ORIENTED_EDGE('',*,*,#47386,.T.);
#66442=ORIENTED_EDGE('',*,*,#47791,.T.);
#66443=ORIENTED_EDGE('',*,*,#47731,.T.);
#66444=ORIENTED_EDGE('',*,*,#47732,.F.);
#66445=ORIENTED_EDGE('',*,*,#47791,.F.);
#66446=ORIENTED_EDGE('',*,*,#47385,.T.);
#66447=ORIENTED_EDGE('',*,*,#47790,.T.);
#66448=ORIENTED_EDGE('',*,*,#47567,.T.);
#66449=ORIENTED_EDGE('',*,*,#47717,.F.);
#66450=ORIENTED_EDGE('',*,*,#47792,.F.);
#66451=ORIENTED_EDGE('',*,*,#47406,.T.);
#66452=ORIENTED_EDGE('',*,*,#47568,.T.);
#66453=ORIENTED_EDGE('',*,*,#47408,.T.);
#66454=ORIENTED_EDGE('',*,*,#47793,.T.);
#66455=ORIENTED_EDGE('',*,*,#47715,.T.);
#66456=ORIENTED_EDGE('',*,*,#47716,.F.);
#66457=ORIENTED_EDGE('',*,*,#47793,.F.);
#66458=ORIENTED_EDGE('',*,*,#47407,.T.);
#66459=ORIENTED_EDGE('',*,*,#47792,.T.);
#66460=ORIENTED_EDGE('',*,*,#47565,.T.);
#66461=ORIENTED_EDGE('',*,*,#47719,.F.);
#66462=ORIENTED_EDGE('',*,*,#47794,.F.);
#66463=ORIENTED_EDGE('',*,*,#47403,.T.);
#66464=ORIENTED_EDGE('',*,*,#47718,.F.);
#66465=ORIENTED_EDGE('',*,*,#47368,.F.);
#66466=ORIENTED_EDGE('',*,*,#47404,.T.);
#66467=ORIENTED_EDGE('',*,*,#47794,.T.);
#66468=ORIENTED_EDGE('',*,*,#47560,.T.);
#66469=ORIENTED_EDGE('',*,*,#47721,.F.);
#66470=ORIENTED_EDGE('',*,*,#47795,.F.);
#66471=ORIENTED_EDGE('',*,*,#47400,.T.);
#66472=ORIENTED_EDGE('',*,*,#47720,.F.);
#66473=ORIENTED_EDGE('',*,*,#47364,.F.);
#66474=ORIENTED_EDGE('',*,*,#47401,.T.);
#66475=ORIENTED_EDGE('',*,*,#47795,.T.);
#66476=ORIENTED_EDGE('',*,*,#47561,.T.);
#66477=ORIENTED_EDGE('',*,*,#47727,.F.);
#66478=ORIENTED_EDGE('',*,*,#47796,.F.);
#66479=ORIENTED_EDGE('',*,*,#47392,.T.);
#66480=ORIENTED_EDGE('',*,*,#47556,.T.);
#66481=ORIENTED_EDGE('',*,*,#47394,.T.);
#66482=ORIENTED_EDGE('',*,*,#47797,.T.);
#66483=ORIENTED_EDGE('',*,*,#47725,.T.);
#66484=ORIENTED_EDGE('',*,*,#47726,.F.);
#66485=ORIENTED_EDGE('',*,*,#47797,.F.);
#66486=ORIENTED_EDGE('',*,*,#47393,.T.);
#66487=ORIENTED_EDGE('',*,*,#47796,.T.);
#66488=ORIENTED_EDGE('',*,*,#47555,.T.);
#66489=ORIENTED_EDGE('',*,*,#47724,.F.);
#66490=ORIENTED_EDGE('',*,*,#47798,.F.);
#66491=ORIENTED_EDGE('',*,*,#47396,.T.);
#66492=ORIENTED_EDGE('',*,*,#47558,.T.);
#66493=ORIENTED_EDGE('',*,*,#47398,.T.);
#66494=ORIENTED_EDGE('',*,*,#47799,.T.);
#66495=ORIENTED_EDGE('',*,*,#47722,.T.);
#66496=ORIENTED_EDGE('',*,*,#47723,.F.);
#66497=ORIENTED_EDGE('',*,*,#47799,.F.);
#66498=ORIENTED_EDGE('',*,*,#47397,.T.);
#66499=ORIENTED_EDGE('',*,*,#47798,.T.);
#66500=ORIENTED_EDGE('',*,*,#47551,.T.);
#66501=ORIENTED_EDGE('',*,*,#47649,.F.);
#66502=ORIENTED_EDGE('',*,*,#47800,.F.);
#66503=ORIENTED_EDGE('',*,*,#47496,.T.);
#66504=ORIENTED_EDGE('',*,*,#47553,.T.);
#66505=ORIENTED_EDGE('',*,*,#47498,.T.);
#66506=ORIENTED_EDGE('',*,*,#47801,.T.);
#66507=ORIENTED_EDGE('',*,*,#47647,.T.);
#66508=ORIENTED_EDGE('',*,*,#47648,.F.);
#66509=ORIENTED_EDGE('',*,*,#47801,.F.);
#66510=ORIENTED_EDGE('',*,*,#47497,.T.);
#66511=ORIENTED_EDGE('',*,*,#47800,.T.);
#66512=ORIENTED_EDGE('',*,*,#47552,.T.);
#66513=ORIENTED_EDGE('',*,*,#47646,.F.);
#66514=ORIENTED_EDGE('',*,*,#47802,.F.);
#66515=ORIENTED_EDGE('',*,*,#47500,.T.);
#66516=ORIENTED_EDGE('',*,*,#47543,.T.);
#66517=ORIENTED_EDGE('',*,*,#47502,.T.);
#66518=ORIENTED_EDGE('',*,*,#47803,.T.);
#66519=ORIENTED_EDGE('',*,*,#47644,.T.);
#66520=ORIENTED_EDGE('',*,*,#47645,.F.);
#66521=ORIENTED_EDGE('',*,*,#47803,.F.);
#66522=ORIENTED_EDGE('',*,*,#47501,.T.);
#66523=ORIENTED_EDGE('',*,*,#47802,.T.);
#66524=ORIENTED_EDGE('',*,*,#47549,.T.);
#66525=ORIENTED_EDGE('',*,*,#47494,.T.);
#66526=ORIENTED_EDGE('',*,*,#47804,.T.);
#66527=ORIENTED_EDGE('',*,*,#47650,.T.);
#66528=ORIENTED_EDGE('',*,*,#47651,.F.);
#66529=ORIENTED_EDGE('',*,*,#47804,.F.);
#66530=ORIENTED_EDGE('',*,*,#47493,.T.);
#66531=ORIENTED_EDGE('',*,*,#47362,.T.);
#66532=ORIENTED_EDGE('',*,*,#47547,.T.);
#66533=ORIENTED_EDGE('',*,*,#47491,.T.);
#66534=ORIENTED_EDGE('',*,*,#47805,.T.);
#66535=ORIENTED_EDGE('',*,*,#47652,.T.);
#66536=ORIENTED_EDGE('',*,*,#47653,.F.);
#66537=ORIENTED_EDGE('',*,*,#47805,.F.);
#66538=ORIENTED_EDGE('',*,*,#47490,.T.);
#66539=ORIENTED_EDGE('',*,*,#47358,.T.);
#66540=ORIENTED_EDGE('',*,*,#47542,.T.);
#66541=ORIENTED_EDGE('',*,*,#47643,.F.);
#66542=ORIENTED_EDGE('',*,*,#47806,.F.);
#66543=ORIENTED_EDGE('',*,*,#47504,.T.);
#66544=ORIENTED_EDGE('',*,*,#47540,.T.);
#66545=ORIENTED_EDGE('',*,*,#47506,.T.);
#66546=ORIENTED_EDGE('',*,*,#47807,.T.);
#66547=ORIENTED_EDGE('',*,*,#47641,.T.);
#66548=ORIENTED_EDGE('',*,*,#47642,.F.);
#66549=ORIENTED_EDGE('',*,*,#47807,.F.);
#66550=ORIENTED_EDGE('',*,*,#47505,.T.);
#66551=ORIENTED_EDGE('',*,*,#47806,.T.);
#66552=ORIENTED_EDGE('',*,*,#47539,.T.);
#66553=ORIENTED_EDGE('',*,*,#47640,.F.);
#66554=ORIENTED_EDGE('',*,*,#47808,.F.);
#66555=ORIENTED_EDGE('',*,*,#47508,.T.);
#66556=ORIENTED_EDGE('',*,*,#47537,.T.);
#66557=ORIENTED_EDGE('',*,*,#47510,.T.);
#66558=ORIENTED_EDGE('',*,*,#47809,.T.);
#66559=ORIENTED_EDGE('',*,*,#47638,.T.);
#66560=ORIENTED_EDGE('',*,*,#47639,.F.);
#66561=ORIENTED_EDGE('',*,*,#47809,.F.);
#66562=ORIENTED_EDGE('',*,*,#47509,.T.);
#66563=ORIENTED_EDGE('',*,*,#47808,.T.);
#66564=ORIENTED_EDGE('',*,*,#47536,.T.);
#66565=ORIENTED_EDGE('',*,*,#47637,.F.);
#66566=ORIENTED_EDGE('',*,*,#47810,.F.);
#66567=ORIENTED_EDGE('',*,*,#47512,.T.);
#66568=ORIENTED_EDGE('',*,*,#47531,.T.);
#66569=ORIENTED_EDGE('',*,*,#47514,.T.);
#66570=ORIENTED_EDGE('',*,*,#47811,.T.);
#66571=ORIENTED_EDGE('',*,*,#47635,.T.);
#66572=ORIENTED_EDGE('',*,*,#47636,.F.);
#66573=ORIENTED_EDGE('',*,*,#47811,.F.);
#66574=ORIENTED_EDGE('',*,*,#47513,.T.);
#66575=ORIENTED_EDGE('',*,*,#47810,.T.);
#66576=ORIENTED_EDGE('',*,*,#47530,.T.);
#66577=ORIENTED_EDGE('',*,*,#47634,.F.);
#66578=ORIENTED_EDGE('',*,*,#47812,.F.);
#66579=ORIENTED_EDGE('',*,*,#47372,.T.);
#66580=ORIENTED_EDGE('',*,*,#47533,.T.);
#66581=ORIENTED_EDGE('',*,*,#47374,.T.);
#66582=ORIENTED_EDGE('',*,*,#47813,.T.);
#66583=ORIENTED_EDGE('',*,*,#47740,.T.);
#66584=ORIENTED_EDGE('',*,*,#47741,.F.);
#66585=ORIENTED_EDGE('',*,*,#47813,.F.);
#66586=ORIENTED_EDGE('',*,*,#47373,.T.);
#66587=ORIENTED_EDGE('',*,*,#47812,.T.);
#66588=ORIENTED_EDGE('',*,*,#47317,.T.);
#66589=ORIENTED_EDGE('',*,*,#47316,.T.);
#66590=ORIENTED_EDGE('',*,*,#47337,.T.);
#66591=ORIENTED_EDGE('',*,*,#47333,.T.);
#66592=ORIENTED_EDGE('',*,*,#47349,.T.);
#66593=ORIENTED_EDGE('',*,*,#47312,.T.);
#66594=ORIENTED_EDGE('',*,*,#47814,.T.);
#66595=ORIENTED_EDGE('',*,*,#47815,.T.);
#66596=ORIENTED_EDGE('',*,*,#47348,.F.);
#66597=ORIENTED_EDGE('',*,*,#47816,.T.);
#66598=ORIENTED_EDGE('',*,*,#47817,.T.);
#66599=ORIENTED_EDGE('',*,*,#47818,.T.);
#66600=ORIENTED_EDGE('',*,*,#47814,.F.);
#66601=ORIENTED_EDGE('',*,*,#47819,.T.);
#66602=ORIENTED_EDGE('',*,*,#47820,.T.);
#66603=ORIENTED_EDGE('',*,*,#47821,.T.);
#66604=ORIENTED_EDGE('',*,*,#47817,.F.);
#66605=ORIENTED_EDGE('',*,*,#47822,.T.);
#66606=ORIENTED_EDGE('',*,*,#47823,.T.);
#66607=ORIENTED_EDGE('',*,*,#47824,.T.);
#66608=ORIENTED_EDGE('',*,*,#47820,.F.);
#66609=ORIENTED_EDGE('',*,*,#47825,.T.);
#66610=ORIENTED_EDGE('',*,*,#47826,.T.);
#66611=ORIENTED_EDGE('',*,*,#47827,.T.);
#66612=ORIENTED_EDGE('',*,*,#47823,.F.);
#66613=ORIENTED_EDGE('',*,*,#47828,.T.);
#66614=ORIENTED_EDGE('',*,*,#47829,.T.);
#66615=ORIENTED_EDGE('',*,*,#47325,.T.);
#66616=ORIENTED_EDGE('',*,*,#47826,.F.);
#66617=ORIENTED_EDGE('',*,*,#47830,.T.);
#66618=ORIENTED_EDGE('',*,*,#47346,.T.);
#66619=ORIENTED_EDGE('',*,*,#47831,.T.);
#66620=ORIENTED_EDGE('',*,*,#47829,.F.);
#66621=ORIENTED_EDGE('',*,*,#47832,.T.);
#66622=ORIENTED_EDGE('',*,*,#47816,.F.);
#66623=ORIENTED_EDGE('',*,*,#47347,.F.);
#66624=ORIENTED_EDGE('',*,*,#47832,.F.);
#66625=ORIENTED_EDGE('',*,*,#47830,.F.);
#66626=ORIENTED_EDGE('',*,*,#47828,.F.);
#66627=ORIENTED_EDGE('',*,*,#47825,.F.);
#66628=ORIENTED_EDGE('',*,*,#47822,.F.);
#66629=ORIENTED_EDGE('',*,*,#47819,.F.);
#66630=ORIENTED_EDGE('',*,*,#47833,.T.);
#66631=ORIENTED_EDGE('',*,*,#47834,.T.);
#66632=ORIENTED_EDGE('',*,*,#47835,.F.);
#66633=ORIENTED_EDGE('',*,*,#47836,.T.);
#66634=ORIENTED_EDGE('',*,*,#47342,.T.);
#66635=ORIENTED_EDGE('',*,*,#47837,.T.);
#66636=ORIENTED_EDGE('',*,*,#47833,.F.);
#66637=ORIENTED_EDGE('',*,*,#47838,.T.);
#66638=ORIENTED_EDGE('',*,*,#47839,.T.);
#66639=ORIENTED_EDGE('',*,*,#47840,.T.);
#66640=ORIENTED_EDGE('',*,*,#47344,.F.);
#66641=ORIENTED_EDGE('',*,*,#47841,.T.);
#66642=ORIENTED_EDGE('',*,*,#47842,.T.);
#66643=ORIENTED_EDGE('',*,*,#47321,.T.);
#66644=ORIENTED_EDGE('',*,*,#47839,.F.);
#66645=ORIENTED_EDGE('',*,*,#47843,.T.);
#66646=ORIENTED_EDGE('',*,*,#47844,.T.);
#66647=ORIENTED_EDGE('',*,*,#47845,.T.);
#66648=ORIENTED_EDGE('',*,*,#47842,.F.);
#66649=ORIENTED_EDGE('',*,*,#47846,.T.);
#66650=ORIENTED_EDGE('',*,*,#47847,.T.);
#66651=ORIENTED_EDGE('',*,*,#47848,.T.);
#66652=ORIENTED_EDGE('',*,*,#47844,.F.);
#66653=ORIENTED_EDGE('',*,*,#47849,.T.);
#66654=ORIENTED_EDGE('',*,*,#47835,.T.);
#66655=ORIENTED_EDGE('',*,*,#47850,.T.);
#66656=ORIENTED_EDGE('',*,*,#47847,.F.);
#66657=ORIENTED_EDGE('',*,*,#47851,.T.);
#66658=ORIENTED_EDGE('',*,*,#47836,.F.);
#66659=ORIENTED_EDGE('',*,*,#47851,.F.);
#66660=ORIENTED_EDGE('',*,*,#47849,.F.);
#66661=ORIENTED_EDGE('',*,*,#47846,.F.);
#66662=ORIENTED_EDGE('',*,*,#47843,.F.);
#66663=ORIENTED_EDGE('',*,*,#47841,.F.);
#66664=ORIENTED_EDGE('',*,*,#47343,.F.);
#66665=ORIENTED_EDGE('',*,*,#47838,.F.);
#66666=ORIENTED_EDGE('',*,*,#47852,.F.);
#66667=ORIENTED_EDGE('',*,*,#47345,.F.);
#66668=ORIENTED_EDGE('',*,*,#47853,.F.);
#66669=ORIENTED_EDGE('',*,*,#47520,.F.);
#66670=ORIENTED_EDGE('',*,*,#47853,.T.);
#66671=ORIENTED_EDGE('',*,*,#47815,.F.);
#66672=ORIENTED_EDGE('',*,*,#47854,.F.);
#66673=ORIENTED_EDGE('',*,*,#47521,.F.);
#66674=ORIENTED_EDGE('',*,*,#47852,.T.);
#66675=ORIENTED_EDGE('',*,*,#47519,.F.);
#66676=ORIENTED_EDGE('',*,*,#47326,.F.);
#66677=ORIENTED_EDGE('',*,*,#47831,.F.);
#66678=ORIENTED_EDGE('',*,*,#47854,.T.);
#66679=ORIENTED_EDGE('',*,*,#47818,.F.);
#66680=ORIENTED_EDGE('',*,*,#47855,.F.);
#66681=ORIENTED_EDGE('',*,*,#47522,.F.);
#66682=ORIENTED_EDGE('',*,*,#47855,.T.);
#66683=ORIENTED_EDGE('',*,*,#47821,.F.);
#66684=ORIENTED_EDGE('',*,*,#47856,.F.);
#66685=ORIENTED_EDGE('',*,*,#47516,.F.);
#66686=ORIENTED_EDGE('',*,*,#47328,.T.);
#66687=ORIENTED_EDGE('',*,*,#47518,.F.);
#66688=ORIENTED_EDGE('',*,*,#47857,.F.);
#66689=ORIENTED_EDGE('',*,*,#47827,.F.);
#66690=ORIENTED_EDGE('',*,*,#47856,.T.);
#66691=ORIENTED_EDGE('',*,*,#47824,.F.);
#66692=ORIENTED_EDGE('',*,*,#47857,.T.);
#66693=ORIENTED_EDGE('',*,*,#47517,.F.);
#66694=ORIENTED_EDGE('',*,*,#47858,.F.);
#66695=ORIENTED_EDGE('',*,*,#47848,.F.);
#66696=ORIENTED_EDGE('',*,*,#47859,.F.);
#66697=ORIENTED_EDGE('',*,*,#47527,.F.);
#66698=ORIENTED_EDGE('',*,*,#47859,.T.);
#66699=ORIENTED_EDGE('',*,*,#47850,.F.);
#66700=ORIENTED_EDGE('',*,*,#47860,.F.);
#66701=ORIENTED_EDGE('',*,*,#47528,.F.);
#66702=ORIENTED_EDGE('',*,*,#47858,.T.);
#66703=ORIENTED_EDGE('',*,*,#47526,.F.);
#66704=ORIENTED_EDGE('',*,*,#47322,.F.);
#66705=ORIENTED_EDGE('',*,*,#47845,.F.);
#66706=ORIENTED_EDGE('',*,*,#47860,.T.);
#66707=ORIENTED_EDGE('',*,*,#47834,.F.);
#66708=ORIENTED_EDGE('',*,*,#47861,.F.);
#66709=ORIENTED_EDGE('',*,*,#47529,.F.);
#66710=ORIENTED_EDGE('',*,*,#47861,.T.);
#66711=ORIENTED_EDGE('',*,*,#47837,.F.);
#66712=ORIENTED_EDGE('',*,*,#47862,.F.);
#66713=ORIENTED_EDGE('',*,*,#47523,.F.);
#66714=ORIENTED_EDGE('',*,*,#47324,.T.);
#66715=ORIENTED_EDGE('',*,*,#47525,.F.);
#66716=ORIENTED_EDGE('',*,*,#47863,.F.);
#66717=ORIENTED_EDGE('',*,*,#47840,.F.);
#66718=ORIENTED_EDGE('',*,*,#47862,.T.);
#66719=ORIENTED_EDGE('',*,*,#47341,.F.);
#66720=ORIENTED_EDGE('',*,*,#47863,.T.);
#66721=ORIENTED_EDGE('',*,*,#47524,.F.);
#66722=ORIENTED_EDGE('',*,*,#47301,.T.);
#66723=ORIENTED_EDGE('',*,*,#47298,.T.);
#66724=ORIENTED_EDGE('',*,*,#47864,.T.);
#66725=ORIENTED_EDGE('',*,*,#47865,.T.);
#66726=ORIENTED_EDGE('',*,*,#47866,.F.);
#66727=ORIENTED_EDGE('',*,*,#47867,.F.);
#66728=ORIENTED_EDGE('',*,*,#47868,.F.);
#66729=ORIENTED_EDGE('',*,*,#47869,.T.);
#66730=ORIENTED_EDGE('',*,*,#47867,.T.);
#66731=ORIENTED_EDGE('',*,*,#47870,.F.);
#66732=ORIENTED_EDGE('',*,*,#47871,.F.);
#66733=ORIENTED_EDGE('',*,*,#47872,.F.);
#66734=ORIENTED_EDGE('',*,*,#47865,.F.);
#66735=ORIENTED_EDGE('',*,*,#47873,.F.);
#66736=ORIENTED_EDGE('',*,*,#47874,.T.);
#66737=ORIENTED_EDGE('',*,*,#47875,.F.);
#66738=ORIENTED_EDGE('',*,*,#47871,.T.);
#66739=ORIENTED_EDGE('',*,*,#47876,.T.);
#66740=ORIENTED_EDGE('',*,*,#47877,.T.);
#66741=ORIENTED_EDGE('',*,*,#47878,.T.);
#66742=ORIENTED_EDGE('',*,*,#47879,.F.);
#66743=ORIENTED_EDGE('',*,*,#47880,.F.);
#66744=ORIENTED_EDGE('',*,*,#47881,.F.);
#66745=ORIENTED_EDGE('',*,*,#47882,.F.);
#66746=ORIENTED_EDGE('',*,*,#47878,.F.);
#66747=ORIENTED_EDGE('',*,*,#47883,.F.);
#66748=ORIENTED_EDGE('',*,*,#47874,.F.);
#66749=ORIENTED_EDGE('',*,*,#47884,.T.);
#66750=ORIENTED_EDGE('',*,*,#47880,.T.);
#66751=ORIENTED_EDGE('',*,*,#47885,.F.);
#66752=ORIENTED_EDGE('',*,*,#47886,.T.);
#66753=ORIENTED_EDGE('',*,*,#47887,.F.);
#66754=ORIENTED_EDGE('',*,*,#47881,.T.);
#66755=ORIENTED_EDGE('',*,*,#47888,.T.);
#66756=ORIENTED_EDGE('',*,*,#47889,.T.);
#66757=ORIENTED_EDGE('',*,*,#47890,.T.);
#66758=ORIENTED_EDGE('',*,*,#47891,.F.);
#66759=ORIENTED_EDGE('',*,*,#47892,.F.);
#66760=ORIENTED_EDGE('',*,*,#47886,.F.);
#66761=ORIENTED_EDGE('',*,*,#47893,.T.);
#66762=ORIENTED_EDGE('',*,*,#47892,.T.);
#66763=ORIENTED_EDGE('',*,*,#47894,.F.);
#66764=ORIENTED_EDGE('',*,*,#47895,.F.);
#66765=ORIENTED_EDGE('',*,*,#47896,.F.);
#66766=ORIENTED_EDGE('',*,*,#47890,.F.);
#66767=ORIENTED_EDGE('',*,*,#47897,.F.);
#66768=ORIENTED_EDGE('',*,*,#47898,.T.);
#66769=ORIENTED_EDGE('',*,*,#47899,.F.);
#66770=ORIENTED_EDGE('',*,*,#47895,.T.);
#66771=ORIENTED_EDGE('',*,*,#47900,.T.);
#66772=ORIENTED_EDGE('',*,*,#47901,.T.);
#66773=ORIENTED_EDGE('',*,*,#47902,.T.);
#66774=ORIENTED_EDGE('',*,*,#47903,.F.);
#66775=ORIENTED_EDGE('',*,*,#47904,.F.);
#66776=ORIENTED_EDGE('',*,*,#47905,.F.);
#66777=ORIENTED_EDGE('',*,*,#47906,.F.);
#66778=ORIENTED_EDGE('',*,*,#47902,.F.);
#66779=ORIENTED_EDGE('',*,*,#47907,.F.);
#66780=ORIENTED_EDGE('',*,*,#47898,.F.);
#66781=ORIENTED_EDGE('',*,*,#47908,.T.);
#66782=ORIENTED_EDGE('',*,*,#47904,.T.);
#66783=ORIENTED_EDGE('',*,*,#47909,.F.);
#66784=ORIENTED_EDGE('',*,*,#47910,.T.);
#66785=ORIENTED_EDGE('',*,*,#47911,.F.);
#66786=ORIENTED_EDGE('',*,*,#47905,.T.);
#66787=ORIENTED_EDGE('',*,*,#47912,.T.);
#66788=ORIENTED_EDGE('',*,*,#47913,.T.);
#66789=ORIENTED_EDGE('',*,*,#47914,.T.);
#66790=ORIENTED_EDGE('',*,*,#47915,.F.);
#66791=ORIENTED_EDGE('',*,*,#47916,.F.);
#66792=ORIENTED_EDGE('',*,*,#47910,.F.);
#66793=ORIENTED_EDGE('',*,*,#47917,.T.);
#66794=ORIENTED_EDGE('',*,*,#47916,.T.);
#66795=ORIENTED_EDGE('',*,*,#47918,.F.);
#66796=ORIENTED_EDGE('',*,*,#47919,.F.);
#66797=ORIENTED_EDGE('',*,*,#47920,.F.);
#66798=ORIENTED_EDGE('',*,*,#47914,.F.);
#66799=ORIENTED_EDGE('',*,*,#47921,.F.);
#66800=ORIENTED_EDGE('',*,*,#47922,.T.);
#66801=ORIENTED_EDGE('',*,*,#47923,.F.);
#66802=ORIENTED_EDGE('',*,*,#47919,.T.);
#66803=ORIENTED_EDGE('',*,*,#47924,.T.);
#66804=ORIENTED_EDGE('',*,*,#47925,.T.);
#66805=ORIENTED_EDGE('',*,*,#47926,.T.);
#66806=ORIENTED_EDGE('',*,*,#47927,.F.);
#66807=ORIENTED_EDGE('',*,*,#47928,.F.);
#66808=ORIENTED_EDGE('',*,*,#47929,.F.);
#66809=ORIENTED_EDGE('',*,*,#47930,.F.);
#66810=ORIENTED_EDGE('',*,*,#47926,.F.);
#66811=ORIENTED_EDGE('',*,*,#47931,.F.);
#66812=ORIENTED_EDGE('',*,*,#47922,.F.);
#66813=ORIENTED_EDGE('',*,*,#47932,.T.);
#66814=ORIENTED_EDGE('',*,*,#47928,.T.);
#66815=ORIENTED_EDGE('',*,*,#47933,.F.);
#66816=ORIENTED_EDGE('',*,*,#47934,.T.);
#66817=ORIENTED_EDGE('',*,*,#47935,.F.);
#66818=ORIENTED_EDGE('',*,*,#47929,.T.);
#66819=ORIENTED_EDGE('',*,*,#47936,.T.);
#66820=ORIENTED_EDGE('',*,*,#47937,.T.);
#66821=ORIENTED_EDGE('',*,*,#47938,.T.);
#66822=ORIENTED_EDGE('',*,*,#47939,.F.);
#66823=ORIENTED_EDGE('',*,*,#47940,.F.);
#66824=ORIENTED_EDGE('',*,*,#47934,.F.);
#66825=ORIENTED_EDGE('',*,*,#47941,.T.);
#66826=ORIENTED_EDGE('',*,*,#47940,.T.);
#66827=ORIENTED_EDGE('',*,*,#47942,.F.);
#66828=ORIENTED_EDGE('',*,*,#47943,.F.);
#66829=ORIENTED_EDGE('',*,*,#47944,.F.);
#66830=ORIENTED_EDGE('',*,*,#47938,.F.);
#66831=ORIENTED_EDGE('',*,*,#47945,.F.);
#66832=ORIENTED_EDGE('',*,*,#47946,.T.);
#66833=ORIENTED_EDGE('',*,*,#47947,.F.);
#66834=ORIENTED_EDGE('',*,*,#47943,.T.);
#66835=ORIENTED_EDGE('',*,*,#47948,.T.);
#66836=ORIENTED_EDGE('',*,*,#47949,.T.);
#66837=ORIENTED_EDGE('',*,*,#47950,.T.);
#66838=ORIENTED_EDGE('',*,*,#47951,.F.);
#66839=ORIENTED_EDGE('',*,*,#47952,.F.);
#66840=ORIENTED_EDGE('',*,*,#47953,.F.);
#66841=ORIENTED_EDGE('',*,*,#47954,.F.);
#66842=ORIENTED_EDGE('',*,*,#47950,.F.);
#66843=ORIENTED_EDGE('',*,*,#47955,.F.);
#66844=ORIENTED_EDGE('',*,*,#47946,.F.);
#66845=ORIENTED_EDGE('',*,*,#47956,.T.);
#66846=ORIENTED_EDGE('',*,*,#47952,.T.);
#66847=ORIENTED_EDGE('',*,*,#47957,.F.);
#66848=ORIENTED_EDGE('',*,*,#47958,.T.);
#66849=ORIENTED_EDGE('',*,*,#47959,.F.);
#66850=ORIENTED_EDGE('',*,*,#47953,.T.);
#66851=ORIENTED_EDGE('',*,*,#47960,.T.);
#66852=ORIENTED_EDGE('',*,*,#47961,.T.);
#66853=ORIENTED_EDGE('',*,*,#47962,.T.);
#66854=ORIENTED_EDGE('',*,*,#47963,.F.);
#66855=ORIENTED_EDGE('',*,*,#47964,.F.);
#66856=ORIENTED_EDGE('',*,*,#47958,.F.);
#66857=ORIENTED_EDGE('',*,*,#47965,.T.);
#66858=ORIENTED_EDGE('',*,*,#47964,.T.);
#66859=ORIENTED_EDGE('',*,*,#47966,.F.);
#66860=ORIENTED_EDGE('',*,*,#47967,.F.);
#66861=ORIENTED_EDGE('',*,*,#47968,.F.);
#66862=ORIENTED_EDGE('',*,*,#47962,.F.);
#66863=ORIENTED_EDGE('',*,*,#47969,.F.);
#66864=ORIENTED_EDGE('',*,*,#47970,.T.);
#66865=ORIENTED_EDGE('',*,*,#47971,.F.);
#66866=ORIENTED_EDGE('',*,*,#47967,.T.);
#66867=ORIENTED_EDGE('',*,*,#47972,.T.);
#66868=ORIENTED_EDGE('',*,*,#47973,.T.);
#66869=ORIENTED_EDGE('',*,*,#47974,.T.);
#66870=ORIENTED_EDGE('',*,*,#47975,.F.);
#66871=ORIENTED_EDGE('',*,*,#47976,.F.);
#66872=ORIENTED_EDGE('',*,*,#47977,.F.);
#66873=ORIENTED_EDGE('',*,*,#47978,.F.);
#66874=ORIENTED_EDGE('',*,*,#47974,.F.);
#66875=ORIENTED_EDGE('',*,*,#47979,.F.);
#66876=ORIENTED_EDGE('',*,*,#47970,.F.);
#66877=ORIENTED_EDGE('',*,*,#47980,.T.);
#66878=ORIENTED_EDGE('',*,*,#47976,.T.);
#66879=ORIENTED_EDGE('',*,*,#47981,.F.);
#66880=ORIENTED_EDGE('',*,*,#47982,.T.);
#66881=ORIENTED_EDGE('',*,*,#47983,.F.);
#66882=ORIENTED_EDGE('',*,*,#47977,.T.);
#66883=ORIENTED_EDGE('',*,*,#47984,.T.);
#66884=ORIENTED_EDGE('',*,*,#47985,.T.);
#66885=ORIENTED_EDGE('',*,*,#47986,.T.);
#66886=ORIENTED_EDGE('',*,*,#47987,.F.);
#66887=ORIENTED_EDGE('',*,*,#47988,.F.);
#66888=ORIENTED_EDGE('',*,*,#47982,.F.);
#66889=ORIENTED_EDGE('',*,*,#47989,.T.);
#66890=ORIENTED_EDGE('',*,*,#47988,.T.);
#66891=ORIENTED_EDGE('',*,*,#47990,.F.);
#66892=ORIENTED_EDGE('',*,*,#47991,.F.);
#66893=ORIENTED_EDGE('',*,*,#47992,.F.);
#66894=ORIENTED_EDGE('',*,*,#47986,.F.);
#66895=ORIENTED_EDGE('',*,*,#47993,.F.);
#66896=ORIENTED_EDGE('',*,*,#47994,.T.);
#66897=ORIENTED_EDGE('',*,*,#47995,.F.);
#66898=ORIENTED_EDGE('',*,*,#47991,.T.);
#66899=ORIENTED_EDGE('',*,*,#47996,.T.);
#66900=ORIENTED_EDGE('',*,*,#47997,.T.);
#66901=ORIENTED_EDGE('',*,*,#47998,.T.);
#66902=ORIENTED_EDGE('',*,*,#47999,.F.);
#66903=ORIENTED_EDGE('',*,*,#48000,.F.);
#66904=ORIENTED_EDGE('',*,*,#48001,.F.);
#66905=ORIENTED_EDGE('',*,*,#48002,.F.);
#66906=ORIENTED_EDGE('',*,*,#47998,.F.);
#66907=ORIENTED_EDGE('',*,*,#48003,.F.);
#66908=ORIENTED_EDGE('',*,*,#47994,.F.);
#66909=ORIENTED_EDGE('',*,*,#48004,.T.);
#66910=ORIENTED_EDGE('',*,*,#48000,.T.);
#66911=ORIENTED_EDGE('',*,*,#48005,.F.);
#66912=ORIENTED_EDGE('',*,*,#48006,.T.);
#66913=ORIENTED_EDGE('',*,*,#48007,.F.);
#66914=ORIENTED_EDGE('',*,*,#48001,.T.);
#66915=ORIENTED_EDGE('',*,*,#48008,.T.);
#66916=ORIENTED_EDGE('',*,*,#48009,.T.);
#66917=ORIENTED_EDGE('',*,*,#48010,.T.);
#66918=ORIENTED_EDGE('',*,*,#48011,.F.);
#66919=ORIENTED_EDGE('',*,*,#48012,.F.);
#66920=ORIENTED_EDGE('',*,*,#48006,.F.);
#66921=ORIENTED_EDGE('',*,*,#48013,.T.);
#66922=ORIENTED_EDGE('',*,*,#48012,.T.);
#66923=ORIENTED_EDGE('',*,*,#48014,.F.);
#66924=ORIENTED_EDGE('',*,*,#48015,.F.);
#66925=ORIENTED_EDGE('',*,*,#48016,.F.);
#66926=ORIENTED_EDGE('',*,*,#48010,.F.);
#66927=ORIENTED_EDGE('',*,*,#48017,.F.);
#66928=ORIENTED_EDGE('',*,*,#48018,.T.);
#66929=ORIENTED_EDGE('',*,*,#48019,.F.);
#66930=ORIENTED_EDGE('',*,*,#48015,.T.);
#66931=ORIENTED_EDGE('',*,*,#48020,.T.);
#66932=ORIENTED_EDGE('',*,*,#48021,.T.);
#66933=ORIENTED_EDGE('',*,*,#48022,.T.);
#66934=ORIENTED_EDGE('',*,*,#48023,.F.);
#66935=ORIENTED_EDGE('',*,*,#48024,.F.);
#66936=ORIENTED_EDGE('',*,*,#48025,.F.);
#66937=ORIENTED_EDGE('',*,*,#48026,.F.);
#66938=ORIENTED_EDGE('',*,*,#48022,.F.);
#66939=ORIENTED_EDGE('',*,*,#48027,.F.);
#66940=ORIENTED_EDGE('',*,*,#48018,.F.);
#66941=ORIENTED_EDGE('',*,*,#48028,.T.);
#66942=ORIENTED_EDGE('',*,*,#48024,.T.);
#66943=ORIENTED_EDGE('',*,*,#48029,.F.);
#66944=ORIENTED_EDGE('',*,*,#48030,.T.);
#66945=ORIENTED_EDGE('',*,*,#48031,.F.);
#66946=ORIENTED_EDGE('',*,*,#48025,.T.);
#66947=ORIENTED_EDGE('',*,*,#48032,.T.);
#66948=ORIENTED_EDGE('',*,*,#48033,.T.);
#66949=ORIENTED_EDGE('',*,*,#48034,.T.);
#66950=ORIENTED_EDGE('',*,*,#48035,.F.);
#66951=ORIENTED_EDGE('',*,*,#48036,.F.);
#66952=ORIENTED_EDGE('',*,*,#48030,.F.);
#66953=ORIENTED_EDGE('',*,*,#48037,.T.);
#66954=ORIENTED_EDGE('',*,*,#48036,.T.);
#66955=ORIENTED_EDGE('',*,*,#48038,.F.);
#66956=ORIENTED_EDGE('',*,*,#48039,.F.);
#66957=ORIENTED_EDGE('',*,*,#48040,.F.);
#66958=ORIENTED_EDGE('',*,*,#48034,.F.);
#66959=ORIENTED_EDGE('',*,*,#48041,.F.);
#66960=ORIENTED_EDGE('',*,*,#48042,.T.);
#66961=ORIENTED_EDGE('',*,*,#48043,.F.);
#66962=ORIENTED_EDGE('',*,*,#48039,.T.);
#66963=ORIENTED_EDGE('',*,*,#48044,.T.);
#66964=ORIENTED_EDGE('',*,*,#48045,.T.);
#66965=ORIENTED_EDGE('',*,*,#48046,.T.);
#66966=ORIENTED_EDGE('',*,*,#48047,.F.);
#66967=ORIENTED_EDGE('',*,*,#48048,.F.);
#66968=ORIENTED_EDGE('',*,*,#48049,.F.);
#66969=ORIENTED_EDGE('',*,*,#48050,.F.);
#66970=ORIENTED_EDGE('',*,*,#48046,.F.);
#66971=ORIENTED_EDGE('',*,*,#48051,.F.);
#66972=ORIENTED_EDGE('',*,*,#48042,.F.);
#66973=ORIENTED_EDGE('',*,*,#48052,.T.);
#66974=ORIENTED_EDGE('',*,*,#48048,.T.);
#66975=ORIENTED_EDGE('',*,*,#48053,.F.);
#66976=ORIENTED_EDGE('',*,*,#48054,.T.);
#66977=ORIENTED_EDGE('',*,*,#48055,.F.);
#66978=ORIENTED_EDGE('',*,*,#48049,.T.);
#66979=ORIENTED_EDGE('',*,*,#48056,.T.);
#66980=ORIENTED_EDGE('',*,*,#48057,.T.);
#66981=ORIENTED_EDGE('',*,*,#48058,.T.);
#66982=ORIENTED_EDGE('',*,*,#48059,.F.);
#66983=ORIENTED_EDGE('',*,*,#48060,.F.);
#66984=ORIENTED_EDGE('',*,*,#48054,.F.);
#66985=ORIENTED_EDGE('',*,*,#48061,.T.);
#66986=ORIENTED_EDGE('',*,*,#48060,.T.);
#66987=ORIENTED_EDGE('',*,*,#48062,.F.);
#66988=ORIENTED_EDGE('',*,*,#48063,.F.);
#66989=ORIENTED_EDGE('',*,*,#48064,.F.);
#66990=ORIENTED_EDGE('',*,*,#48058,.F.);
#66991=ORIENTED_EDGE('',*,*,#48065,.F.);
#66992=ORIENTED_EDGE('',*,*,#48066,.T.);
#66993=ORIENTED_EDGE('',*,*,#48067,.F.);
#66994=ORIENTED_EDGE('',*,*,#48063,.T.);
#66995=ORIENTED_EDGE('',*,*,#48068,.T.);
#66996=ORIENTED_EDGE('',*,*,#48069,.T.);
#66997=ORIENTED_EDGE('',*,*,#48070,.T.);
#66998=ORIENTED_EDGE('',*,*,#48071,.F.);
#66999=ORIENTED_EDGE('',*,*,#48072,.F.);
#67000=ORIENTED_EDGE('',*,*,#48073,.F.);
#67001=ORIENTED_EDGE('',*,*,#48074,.F.);
#67002=ORIENTED_EDGE('',*,*,#48070,.F.);
#67003=ORIENTED_EDGE('',*,*,#48075,.F.);
#67004=ORIENTED_EDGE('',*,*,#48066,.F.);
#67005=ORIENTED_EDGE('',*,*,#48076,.T.);
#67006=ORIENTED_EDGE('',*,*,#48072,.T.);
#67007=ORIENTED_EDGE('',*,*,#48077,.F.);
#67008=ORIENTED_EDGE('',*,*,#48078,.T.);
#67009=ORIENTED_EDGE('',*,*,#48079,.F.);
#67010=ORIENTED_EDGE('',*,*,#48073,.T.);
#67011=ORIENTED_EDGE('',*,*,#48080,.T.);
#67012=ORIENTED_EDGE('',*,*,#48081,.T.);
#67013=ORIENTED_EDGE('',*,*,#48082,.T.);
#67014=ORIENTED_EDGE('',*,*,#48083,.F.);
#67015=ORIENTED_EDGE('',*,*,#48084,.F.);
#67016=ORIENTED_EDGE('',*,*,#48078,.F.);
#67017=ORIENTED_EDGE('',*,*,#48085,.T.);
#67018=ORIENTED_EDGE('',*,*,#48084,.T.);
#67019=ORIENTED_EDGE('',*,*,#48086,.F.);
#67020=ORIENTED_EDGE('',*,*,#48087,.F.);
#67021=ORIENTED_EDGE('',*,*,#48088,.F.);
#67022=ORIENTED_EDGE('',*,*,#48082,.F.);
#67023=ORIENTED_EDGE('',*,*,#48089,.F.);
#67024=ORIENTED_EDGE('',*,*,#48090,.T.);
#67025=ORIENTED_EDGE('',*,*,#48091,.F.);
#67026=ORIENTED_EDGE('',*,*,#48087,.T.);
#67027=ORIENTED_EDGE('',*,*,#48092,.T.);
#67028=ORIENTED_EDGE('',*,*,#48093,.T.);
#67029=ORIENTED_EDGE('',*,*,#48094,.T.);
#67030=ORIENTED_EDGE('',*,*,#48095,.F.);
#67031=ORIENTED_EDGE('',*,*,#48096,.F.);
#67032=ORIENTED_EDGE('',*,*,#48097,.F.);
#67033=ORIENTED_EDGE('',*,*,#48098,.F.);
#67034=ORIENTED_EDGE('',*,*,#48094,.F.);
#67035=ORIENTED_EDGE('',*,*,#48099,.F.);
#67036=ORIENTED_EDGE('',*,*,#48090,.F.);
#67037=ORIENTED_EDGE('',*,*,#48100,.T.);
#67038=ORIENTED_EDGE('',*,*,#48096,.T.);
#67039=ORIENTED_EDGE('',*,*,#48101,.F.);
#67040=ORIENTED_EDGE('',*,*,#48102,.T.);
#67041=ORIENTED_EDGE('',*,*,#48103,.F.);
#67042=ORIENTED_EDGE('',*,*,#48097,.T.);
#67043=ORIENTED_EDGE('',*,*,#48104,.T.);
#67044=ORIENTED_EDGE('',*,*,#48105,.T.);
#67045=ORIENTED_EDGE('',*,*,#48106,.T.);
#67046=ORIENTED_EDGE('',*,*,#48107,.F.);
#67047=ORIENTED_EDGE('',*,*,#48108,.F.);
#67048=ORIENTED_EDGE('',*,*,#48102,.F.);
#67049=ORIENTED_EDGE('',*,*,#48109,.T.);
#67050=ORIENTED_EDGE('',*,*,#48108,.T.);
#67051=ORIENTED_EDGE('',*,*,#48110,.F.);
#67052=ORIENTED_EDGE('',*,*,#48111,.F.);
#67053=ORIENTED_EDGE('',*,*,#48112,.F.);
#67054=ORIENTED_EDGE('',*,*,#48106,.F.);
#67055=ORIENTED_EDGE('',*,*,#48113,.F.);
#67056=ORIENTED_EDGE('',*,*,#48114,.T.);
#67057=ORIENTED_EDGE('',*,*,#48115,.F.);
#67058=ORIENTED_EDGE('',*,*,#48111,.T.);
#67059=ORIENTED_EDGE('',*,*,#48116,.T.);
#67060=ORIENTED_EDGE('',*,*,#48117,.T.);
#67061=ORIENTED_EDGE('',*,*,#48118,.T.);
#67062=ORIENTED_EDGE('',*,*,#48119,.F.);
#67063=ORIENTED_EDGE('',*,*,#48120,.F.);
#67064=ORIENTED_EDGE('',*,*,#48121,.F.);
#67065=ORIENTED_EDGE('',*,*,#48122,.F.);
#67066=ORIENTED_EDGE('',*,*,#48118,.F.);
#67067=ORIENTED_EDGE('',*,*,#48123,.F.);
#67068=ORIENTED_EDGE('',*,*,#48114,.F.);
#67069=ORIENTED_EDGE('',*,*,#48124,.T.);
#67070=ORIENTED_EDGE('',*,*,#48120,.T.);
#67071=ORIENTED_EDGE('',*,*,#48125,.F.);
#67072=ORIENTED_EDGE('',*,*,#48126,.T.);
#67073=ORIENTED_EDGE('',*,*,#48127,.F.);
#67074=ORIENTED_EDGE('',*,*,#48121,.T.);
#67075=ORIENTED_EDGE('',*,*,#48128,.T.);
#67076=ORIENTED_EDGE('',*,*,#48129,.T.);
#67077=ORIENTED_EDGE('',*,*,#48130,.T.);
#67078=ORIENTED_EDGE('',*,*,#48131,.F.);
#67079=ORIENTED_EDGE('',*,*,#48132,.F.);
#67080=ORIENTED_EDGE('',*,*,#48126,.F.);
#67081=ORIENTED_EDGE('',*,*,#48133,.T.);
#67082=ORIENTED_EDGE('',*,*,#48132,.T.);
#67083=ORIENTED_EDGE('',*,*,#48134,.F.);
#67084=ORIENTED_EDGE('',*,*,#48135,.F.);
#67085=ORIENTED_EDGE('',*,*,#48136,.F.);
#67086=ORIENTED_EDGE('',*,*,#48130,.F.);
#67087=ORIENTED_EDGE('',*,*,#48137,.F.);
#67088=ORIENTED_EDGE('',*,*,#48138,.T.);
#67089=ORIENTED_EDGE('',*,*,#48139,.F.);
#67090=ORIENTED_EDGE('',*,*,#48135,.T.);
#67091=ORIENTED_EDGE('',*,*,#48140,.T.);
#67092=ORIENTED_EDGE('',*,*,#48141,.T.);
#67093=ORIENTED_EDGE('',*,*,#48142,.T.);
#67094=ORIENTED_EDGE('',*,*,#48143,.F.);
#67095=ORIENTED_EDGE('',*,*,#48144,.F.);
#67096=ORIENTED_EDGE('',*,*,#48145,.F.);
#67097=ORIENTED_EDGE('',*,*,#48146,.F.);
#67098=ORIENTED_EDGE('',*,*,#48142,.F.);
#67099=ORIENTED_EDGE('',*,*,#48147,.F.);
#67100=ORIENTED_EDGE('',*,*,#48138,.F.);
#67101=ORIENTED_EDGE('',*,*,#48148,.T.);
#67102=ORIENTED_EDGE('',*,*,#48144,.T.);
#67103=ORIENTED_EDGE('',*,*,#48149,.F.);
#67104=ORIENTED_EDGE('',*,*,#48150,.T.);
#67105=ORIENTED_EDGE('',*,*,#48151,.F.);
#67106=ORIENTED_EDGE('',*,*,#48145,.T.);
#67107=ORIENTED_EDGE('',*,*,#48152,.T.);
#67108=ORIENTED_EDGE('',*,*,#48153,.T.);
#67109=ORIENTED_EDGE('',*,*,#48154,.T.);
#67110=ORIENTED_EDGE('',*,*,#48155,.F.);
#67111=ORIENTED_EDGE('',*,*,#48156,.F.);
#67112=ORIENTED_EDGE('',*,*,#48150,.F.);
#67113=ORIENTED_EDGE('',*,*,#48157,.T.);
#67114=ORIENTED_EDGE('',*,*,#48156,.T.);
#67115=ORIENTED_EDGE('',*,*,#48158,.F.);
#67116=ORIENTED_EDGE('',*,*,#48159,.F.);
#67117=ORIENTED_EDGE('',*,*,#48160,.F.);
#67118=ORIENTED_EDGE('',*,*,#48154,.F.);
#67119=ORIENTED_EDGE('',*,*,#48161,.F.);
#67120=ORIENTED_EDGE('',*,*,#48162,.T.);
#67121=ORIENTED_EDGE('',*,*,#48163,.F.);
#67122=ORIENTED_EDGE('',*,*,#48159,.T.);
#67123=ORIENTED_EDGE('',*,*,#48164,.T.);
#67124=ORIENTED_EDGE('',*,*,#48165,.T.);
#67125=ORIENTED_EDGE('',*,*,#48166,.T.);
#67126=ORIENTED_EDGE('',*,*,#48167,.F.);
#67127=ORIENTED_EDGE('',*,*,#48168,.F.);
#67128=ORIENTED_EDGE('',*,*,#48169,.F.);
#67129=ORIENTED_EDGE('',*,*,#48170,.F.);
#67130=ORIENTED_EDGE('',*,*,#48166,.F.);
#67131=ORIENTED_EDGE('',*,*,#48171,.F.);
#67132=ORIENTED_EDGE('',*,*,#48162,.F.);
#67133=ORIENTED_EDGE('',*,*,#48172,.T.);
#67134=ORIENTED_EDGE('',*,*,#48168,.T.);
#67135=ORIENTED_EDGE('',*,*,#48173,.F.);
#67136=ORIENTED_EDGE('',*,*,#48174,.T.);
#67137=ORIENTED_EDGE('',*,*,#48175,.F.);
#67138=ORIENTED_EDGE('',*,*,#48169,.T.);
#67139=ORIENTED_EDGE('',*,*,#48176,.T.);
#67140=ORIENTED_EDGE('',*,*,#48177,.T.);
#67141=ORIENTED_EDGE('',*,*,#48178,.T.);
#67142=ORIENTED_EDGE('',*,*,#48179,.F.);
#67143=ORIENTED_EDGE('',*,*,#48180,.F.);
#67144=ORIENTED_EDGE('',*,*,#48174,.F.);
#67145=ORIENTED_EDGE('',*,*,#48181,.T.);
#67146=ORIENTED_EDGE('',*,*,#48180,.T.);
#67147=ORIENTED_EDGE('',*,*,#48182,.F.);
#67148=ORIENTED_EDGE('',*,*,#48183,.F.);
#67149=ORIENTED_EDGE('',*,*,#48184,.F.);
#67150=ORIENTED_EDGE('',*,*,#48178,.F.);
#67151=ORIENTED_EDGE('',*,*,#48185,.F.);
#67152=ORIENTED_EDGE('',*,*,#48186,.T.);
#67153=ORIENTED_EDGE('',*,*,#48187,.F.);
#67154=ORIENTED_EDGE('',*,*,#48183,.T.);
#67155=ORIENTED_EDGE('',*,*,#48188,.T.);
#67156=ORIENTED_EDGE('',*,*,#48189,.T.);
#67157=ORIENTED_EDGE('',*,*,#48190,.T.);
#67158=ORIENTED_EDGE('',*,*,#48191,.F.);
#67159=ORIENTED_EDGE('',*,*,#48192,.F.);
#67160=ORIENTED_EDGE('',*,*,#48193,.F.);
#67161=ORIENTED_EDGE('',*,*,#48194,.F.);
#67162=ORIENTED_EDGE('',*,*,#48190,.F.);
#67163=ORIENTED_EDGE('',*,*,#48195,.F.);
#67164=ORIENTED_EDGE('',*,*,#48186,.F.);
#67165=ORIENTED_EDGE('',*,*,#48196,.T.);
#67166=ORIENTED_EDGE('',*,*,#48192,.T.);
#67167=ORIENTED_EDGE('',*,*,#48197,.F.);
#67168=ORIENTED_EDGE('',*,*,#48198,.T.);
#67169=ORIENTED_EDGE('',*,*,#48199,.F.);
#67170=ORIENTED_EDGE('',*,*,#48193,.T.);
#67171=ORIENTED_EDGE('',*,*,#48200,.T.);
#67172=ORIENTED_EDGE('',*,*,#48201,.T.);
#67173=ORIENTED_EDGE('',*,*,#48202,.T.);
#67174=ORIENTED_EDGE('',*,*,#48203,.F.);
#67175=ORIENTED_EDGE('',*,*,#48204,.F.);
#67176=ORIENTED_EDGE('',*,*,#48198,.F.);
#67177=ORIENTED_EDGE('',*,*,#48205,.T.);
#67178=ORIENTED_EDGE('',*,*,#48204,.T.);
#67179=ORIENTED_EDGE('',*,*,#48206,.F.);
#67180=ORIENTED_EDGE('',*,*,#48207,.F.);
#67181=ORIENTED_EDGE('',*,*,#48208,.F.);
#67182=ORIENTED_EDGE('',*,*,#48202,.F.);
#67183=ORIENTED_EDGE('',*,*,#48209,.F.);
#67184=ORIENTED_EDGE('',*,*,#48210,.T.);
#67185=ORIENTED_EDGE('',*,*,#48211,.F.);
#67186=ORIENTED_EDGE('',*,*,#48207,.T.);
#67187=ORIENTED_EDGE('',*,*,#48212,.T.);
#67188=ORIENTED_EDGE('',*,*,#48213,.T.);
#67189=ORIENTED_EDGE('',*,*,#48214,.T.);
#67190=ORIENTED_EDGE('',*,*,#48215,.F.);
#67191=ORIENTED_EDGE('',*,*,#48216,.F.);
#67192=ORIENTED_EDGE('',*,*,#48217,.F.);
#67193=ORIENTED_EDGE('',*,*,#48218,.F.);
#67194=ORIENTED_EDGE('',*,*,#48214,.F.);
#67195=ORIENTED_EDGE('',*,*,#48219,.F.);
#67196=ORIENTED_EDGE('',*,*,#48210,.F.);
#67197=ORIENTED_EDGE('',*,*,#48220,.T.);
#67198=ORIENTED_EDGE('',*,*,#48216,.T.);
#67199=ORIENTED_EDGE('',*,*,#48221,.F.);
#67200=ORIENTED_EDGE('',*,*,#48222,.T.);
#67201=ORIENTED_EDGE('',*,*,#48223,.F.);
#67202=ORIENTED_EDGE('',*,*,#48217,.T.);
#67203=ORIENTED_EDGE('',*,*,#48224,.T.);
#67204=ORIENTED_EDGE('',*,*,#48225,.T.);
#67205=ORIENTED_EDGE('',*,*,#48226,.T.);
#67206=ORIENTED_EDGE('',*,*,#48227,.F.);
#67207=ORIENTED_EDGE('',*,*,#48228,.F.);
#67208=ORIENTED_EDGE('',*,*,#48222,.F.);
#67209=ORIENTED_EDGE('',*,*,#48229,.T.);
#67210=ORIENTED_EDGE('',*,*,#48228,.T.);
#67211=ORIENTED_EDGE('',*,*,#48230,.F.);
#67212=ORIENTED_EDGE('',*,*,#48231,.F.);
#67213=ORIENTED_EDGE('',*,*,#48232,.F.);
#67214=ORIENTED_EDGE('',*,*,#48226,.F.);
#67215=ORIENTED_EDGE('',*,*,#48233,.F.);
#67216=ORIENTED_EDGE('',*,*,#48234,.T.);
#67217=ORIENTED_EDGE('',*,*,#48235,.F.);
#67218=ORIENTED_EDGE('',*,*,#48231,.T.);
#67219=ORIENTED_EDGE('',*,*,#48236,.T.);
#67220=ORIENTED_EDGE('',*,*,#48237,.T.);
#67221=ORIENTED_EDGE('',*,*,#48238,.T.);
#67222=ORIENTED_EDGE('',*,*,#48239,.F.);
#67223=ORIENTED_EDGE('',*,*,#48240,.F.);
#67224=ORIENTED_EDGE('',*,*,#48241,.F.);
#67225=ORIENTED_EDGE('',*,*,#48242,.F.);
#67226=ORIENTED_EDGE('',*,*,#48238,.F.);
#67227=ORIENTED_EDGE('',*,*,#48243,.F.);
#67228=ORIENTED_EDGE('',*,*,#48234,.F.);
#67229=ORIENTED_EDGE('',*,*,#48244,.T.);
#67230=ORIENTED_EDGE('',*,*,#48240,.T.);
#67231=ORIENTED_EDGE('',*,*,#48245,.F.);
#67232=ORIENTED_EDGE('',*,*,#48246,.T.);
#67233=ORIENTED_EDGE('',*,*,#48247,.F.);
#67234=ORIENTED_EDGE('',*,*,#48241,.T.);
#67235=ORIENTED_EDGE('',*,*,#48248,.T.);
#67236=ORIENTED_EDGE('',*,*,#48249,.T.);
#67237=ORIENTED_EDGE('',*,*,#48250,.T.);
#67238=ORIENTED_EDGE('',*,*,#48251,.F.);
#67239=ORIENTED_EDGE('',*,*,#48252,.F.);
#67240=ORIENTED_EDGE('',*,*,#48246,.F.);
#67241=ORIENTED_EDGE('',*,*,#48253,.T.);
#67242=ORIENTED_EDGE('',*,*,#48252,.T.);
#67243=ORIENTED_EDGE('',*,*,#48254,.F.);
#67244=ORIENTED_EDGE('',*,*,#48255,.F.);
#67245=ORIENTED_EDGE('',*,*,#48256,.F.);
#67246=ORIENTED_EDGE('',*,*,#48250,.F.);
#67247=ORIENTED_EDGE('',*,*,#48257,.F.);
#67248=ORIENTED_EDGE('',*,*,#48258,.T.);
#67249=ORIENTED_EDGE('',*,*,#48259,.F.);
#67250=ORIENTED_EDGE('',*,*,#48255,.T.);
#67251=ORIENTED_EDGE('',*,*,#48260,.T.);
#67252=ORIENTED_EDGE('',*,*,#48261,.T.);
#67253=ORIENTED_EDGE('',*,*,#48262,.T.);
#67254=ORIENTED_EDGE('',*,*,#48263,.F.);
#67255=ORIENTED_EDGE('',*,*,#48264,.F.);
#67256=ORIENTED_EDGE('',*,*,#48265,.F.);
#67257=ORIENTED_EDGE('',*,*,#48266,.F.);
#67258=ORIENTED_EDGE('',*,*,#48262,.F.);
#67259=ORIENTED_EDGE('',*,*,#48267,.F.);
#67260=ORIENTED_EDGE('',*,*,#48258,.F.);
#67261=ORIENTED_EDGE('',*,*,#48268,.T.);
#67262=ORIENTED_EDGE('',*,*,#48264,.T.);
#67263=ORIENTED_EDGE('',*,*,#48269,.F.);
#67264=ORIENTED_EDGE('',*,*,#48270,.T.);
#67265=ORIENTED_EDGE('',*,*,#48271,.F.);
#67266=ORIENTED_EDGE('',*,*,#48265,.T.);
#67267=ORIENTED_EDGE('',*,*,#48272,.T.);
#67268=ORIENTED_EDGE('',*,*,#48273,.T.);
#67269=ORIENTED_EDGE('',*,*,#48274,.T.);
#67270=ORIENTED_EDGE('',*,*,#48275,.F.);
#67271=ORIENTED_EDGE('',*,*,#48276,.F.);
#67272=ORIENTED_EDGE('',*,*,#48270,.F.);
#67273=ORIENTED_EDGE('',*,*,#48277,.T.);
#67274=ORIENTED_EDGE('',*,*,#48276,.T.);
#67275=ORIENTED_EDGE('',*,*,#48278,.F.);
#67276=ORIENTED_EDGE('',*,*,#48279,.F.);
#67277=ORIENTED_EDGE('',*,*,#48280,.F.);
#67278=ORIENTED_EDGE('',*,*,#48274,.F.);
#67279=ORIENTED_EDGE('',*,*,#48281,.F.);
#67280=ORIENTED_EDGE('',*,*,#48282,.T.);
#67281=ORIENTED_EDGE('',*,*,#48283,.F.);
#67282=ORIENTED_EDGE('',*,*,#48279,.T.);
#67283=ORIENTED_EDGE('',*,*,#48284,.T.);
#67284=ORIENTED_EDGE('',*,*,#48285,.T.);
#67285=ORIENTED_EDGE('',*,*,#48286,.T.);
#67286=ORIENTED_EDGE('',*,*,#48287,.F.);
#67287=ORIENTED_EDGE('',*,*,#48288,.F.);
#67288=ORIENTED_EDGE('',*,*,#48289,.F.);
#67289=ORIENTED_EDGE('',*,*,#48290,.F.);
#67290=ORIENTED_EDGE('',*,*,#48286,.F.);
#67291=ORIENTED_EDGE('',*,*,#48291,.F.);
#67292=ORIENTED_EDGE('',*,*,#48282,.F.);
#67293=ORIENTED_EDGE('',*,*,#48292,.T.);
#67294=ORIENTED_EDGE('',*,*,#48288,.T.);
#67295=ORIENTED_EDGE('',*,*,#48293,.F.);
#67296=ORIENTED_EDGE('',*,*,#48294,.T.);
#67297=ORIENTED_EDGE('',*,*,#48295,.F.);
#67298=ORIENTED_EDGE('',*,*,#48289,.T.);
#67299=ORIENTED_EDGE('',*,*,#48296,.T.);
#67300=ORIENTED_EDGE('',*,*,#48297,.T.);
#67301=ORIENTED_EDGE('',*,*,#48298,.T.);
#67302=ORIENTED_EDGE('',*,*,#48299,.F.);
#67303=ORIENTED_EDGE('',*,*,#48300,.F.);
#67304=ORIENTED_EDGE('',*,*,#48294,.F.);
#67305=ORIENTED_EDGE('',*,*,#48301,.T.);
#67306=ORIENTED_EDGE('',*,*,#48300,.T.);
#67307=ORIENTED_EDGE('',*,*,#48302,.F.);
#67308=ORIENTED_EDGE('',*,*,#48303,.F.);
#67309=ORIENTED_EDGE('',*,*,#48304,.F.);
#67310=ORIENTED_EDGE('',*,*,#48298,.F.);
#67311=ORIENTED_EDGE('',*,*,#48305,.F.);
#67312=ORIENTED_EDGE('',*,*,#48306,.T.);
#67313=ORIENTED_EDGE('',*,*,#48307,.F.);
#67314=ORIENTED_EDGE('',*,*,#48303,.T.);
#67315=ORIENTED_EDGE('',*,*,#48308,.T.);
#67316=ORIENTED_EDGE('',*,*,#48309,.T.);
#67317=ORIENTED_EDGE('',*,*,#48310,.T.);
#67318=ORIENTED_EDGE('',*,*,#48311,.F.);
#67319=ORIENTED_EDGE('',*,*,#48312,.F.);
#67320=ORIENTED_EDGE('',*,*,#48313,.F.);
#67321=ORIENTED_EDGE('',*,*,#48314,.F.);
#67322=ORIENTED_EDGE('',*,*,#48310,.F.);
#67323=ORIENTED_EDGE('',*,*,#48315,.F.);
#67324=ORIENTED_EDGE('',*,*,#48306,.F.);
#67325=ORIENTED_EDGE('',*,*,#48316,.T.);
#67326=ORIENTED_EDGE('',*,*,#48312,.T.);
#67327=ORIENTED_EDGE('',*,*,#48317,.F.);
#67328=ORIENTED_EDGE('',*,*,#48318,.T.);
#67329=ORIENTED_EDGE('',*,*,#48319,.F.);
#67330=ORIENTED_EDGE('',*,*,#48313,.T.);
#67331=ORIENTED_EDGE('',*,*,#48320,.T.);
#67332=ORIENTED_EDGE('',*,*,#48321,.T.);
#67333=ORIENTED_EDGE('',*,*,#48322,.T.);
#67334=ORIENTED_EDGE('',*,*,#48323,.F.);
#67335=ORIENTED_EDGE('',*,*,#48324,.F.);
#67336=ORIENTED_EDGE('',*,*,#48318,.F.);
#67337=ORIENTED_EDGE('',*,*,#48325,.T.);
#67338=ORIENTED_EDGE('',*,*,#48324,.T.);
#67339=ORIENTED_EDGE('',*,*,#48326,.F.);
#67340=ORIENTED_EDGE('',*,*,#48327,.F.);
#67341=ORIENTED_EDGE('',*,*,#48328,.F.);
#67342=ORIENTED_EDGE('',*,*,#48322,.F.);
#67343=ORIENTED_EDGE('',*,*,#48329,.F.);
#67344=ORIENTED_EDGE('',*,*,#48330,.T.);
#67345=ORIENTED_EDGE('',*,*,#48331,.F.);
#67346=ORIENTED_EDGE('',*,*,#48327,.T.);
#67347=ORIENTED_EDGE('',*,*,#48332,.T.);
#67348=ORIENTED_EDGE('',*,*,#48333,.T.);
#67349=ORIENTED_EDGE('',*,*,#48334,.T.);
#67350=ORIENTED_EDGE('',*,*,#48335,.F.);
#67351=ORIENTED_EDGE('',*,*,#48336,.F.);
#67352=ORIENTED_EDGE('',*,*,#48337,.F.);
#67353=ORIENTED_EDGE('',*,*,#48338,.F.);
#67354=ORIENTED_EDGE('',*,*,#48334,.F.);
#67355=ORIENTED_EDGE('',*,*,#48339,.F.);
#67356=ORIENTED_EDGE('',*,*,#48330,.F.);
#67357=ORIENTED_EDGE('',*,*,#48340,.T.);
#67358=ORIENTED_EDGE('',*,*,#48336,.T.);
#67359=ORIENTED_EDGE('',*,*,#48341,.F.);
#67360=ORIENTED_EDGE('',*,*,#48342,.T.);
#67361=ORIENTED_EDGE('',*,*,#48343,.F.);
#67362=ORIENTED_EDGE('',*,*,#48337,.T.);
#67363=ORIENTED_EDGE('',*,*,#48344,.T.);
#67364=ORIENTED_EDGE('',*,*,#48345,.T.);
#67365=ORIENTED_EDGE('',*,*,#48346,.T.);
#67366=ORIENTED_EDGE('',*,*,#48347,.F.);
#67367=ORIENTED_EDGE('',*,*,#48348,.F.);
#67368=ORIENTED_EDGE('',*,*,#48342,.F.);
#67369=ORIENTED_EDGE('',*,*,#48349,.T.);
#67370=ORIENTED_EDGE('',*,*,#48348,.T.);
#67371=ORIENTED_EDGE('',*,*,#48350,.F.);
#67372=ORIENTED_EDGE('',*,*,#48351,.F.);
#67373=ORIENTED_EDGE('',*,*,#48352,.F.);
#67374=ORIENTED_EDGE('',*,*,#48346,.F.);
#67375=ORIENTED_EDGE('',*,*,#48353,.F.);
#67376=ORIENTED_EDGE('',*,*,#48354,.T.);
#67377=ORIENTED_EDGE('',*,*,#48355,.F.);
#67378=ORIENTED_EDGE('',*,*,#48351,.T.);
#67379=ORIENTED_EDGE('',*,*,#48356,.T.);
#67380=ORIENTED_EDGE('',*,*,#48357,.T.);
#67381=ORIENTED_EDGE('',*,*,#48358,.T.);
#67382=ORIENTED_EDGE('',*,*,#48359,.F.);
#67383=ORIENTED_EDGE('',*,*,#48360,.F.);
#67384=ORIENTED_EDGE('',*,*,#48361,.F.);
#67385=ORIENTED_EDGE('',*,*,#48362,.F.);
#67386=ORIENTED_EDGE('',*,*,#48358,.F.);
#67387=ORIENTED_EDGE('',*,*,#48363,.F.);
#67388=ORIENTED_EDGE('',*,*,#48354,.F.);
#67389=ORIENTED_EDGE('',*,*,#48364,.T.);
#67390=ORIENTED_EDGE('',*,*,#48360,.T.);
#67391=ORIENTED_EDGE('',*,*,#48365,.F.);
#67392=ORIENTED_EDGE('',*,*,#48366,.T.);
#67393=ORIENTED_EDGE('',*,*,#48367,.F.);
#67394=ORIENTED_EDGE('',*,*,#48361,.T.);
#67395=ORIENTED_EDGE('',*,*,#48368,.T.);
#67396=ORIENTED_EDGE('',*,*,#48369,.T.);
#67397=ORIENTED_EDGE('',*,*,#48370,.T.);
#67398=ORIENTED_EDGE('',*,*,#48371,.F.);
#67399=ORIENTED_EDGE('',*,*,#48372,.F.);
#67400=ORIENTED_EDGE('',*,*,#48366,.F.);
#67401=ORIENTED_EDGE('',*,*,#48373,.T.);
#67402=ORIENTED_EDGE('',*,*,#48372,.T.);
#67403=ORIENTED_EDGE('',*,*,#48374,.F.);
#67404=ORIENTED_EDGE('',*,*,#48375,.F.);
#67405=ORIENTED_EDGE('',*,*,#48376,.F.);
#67406=ORIENTED_EDGE('',*,*,#48370,.F.);
#67407=ORIENTED_EDGE('',*,*,#48377,.F.);
#67408=ORIENTED_EDGE('',*,*,#48378,.F.);
#67409=ORIENTED_EDGE('',*,*,#48377,.T.);
#67410=ORIENTED_EDGE('',*,*,#48369,.F.);
#67411=ORIENTED_EDGE('',*,*,#48373,.F.);
#67412=ORIENTED_EDGE('',*,*,#48368,.F.);
#67413=ORIENTED_EDGE('',*,*,#48363,.T.);
#67414=ORIENTED_EDGE('',*,*,#48357,.F.);
#67415=ORIENTED_EDGE('',*,*,#48364,.F.);
#67416=ORIENTED_EDGE('',*,*,#48356,.F.);
#67417=ORIENTED_EDGE('',*,*,#48353,.T.);
#67418=ORIENTED_EDGE('',*,*,#48345,.F.);
#67419=ORIENTED_EDGE('',*,*,#48349,.F.);
#67420=ORIENTED_EDGE('',*,*,#48344,.F.);
#67421=ORIENTED_EDGE('',*,*,#48339,.T.);
#67422=ORIENTED_EDGE('',*,*,#48333,.F.);
#67423=ORIENTED_EDGE('',*,*,#48340,.F.);
#67424=ORIENTED_EDGE('',*,*,#48332,.F.);
#67425=ORIENTED_EDGE('',*,*,#48329,.T.);
#67426=ORIENTED_EDGE('',*,*,#48321,.F.);
#67427=ORIENTED_EDGE('',*,*,#48325,.F.);
#67428=ORIENTED_EDGE('',*,*,#48320,.F.);
#67429=ORIENTED_EDGE('',*,*,#48315,.T.);
#67430=ORIENTED_EDGE('',*,*,#48309,.F.);
#67431=ORIENTED_EDGE('',*,*,#48316,.F.);
#67432=ORIENTED_EDGE('',*,*,#48308,.F.);
#67433=ORIENTED_EDGE('',*,*,#48305,.T.);
#67434=ORIENTED_EDGE('',*,*,#48297,.F.);
#67435=ORIENTED_EDGE('',*,*,#48301,.F.);
#67436=ORIENTED_EDGE('',*,*,#48296,.F.);
#67437=ORIENTED_EDGE('',*,*,#48291,.T.);
#67438=ORIENTED_EDGE('',*,*,#48285,.F.);
#67439=ORIENTED_EDGE('',*,*,#48292,.F.);
#67440=ORIENTED_EDGE('',*,*,#48284,.F.);
#67441=ORIENTED_EDGE('',*,*,#48281,.T.);
#67442=ORIENTED_EDGE('',*,*,#48273,.F.);
#67443=ORIENTED_EDGE('',*,*,#48277,.F.);
#67444=ORIENTED_EDGE('',*,*,#48272,.F.);
#67445=ORIENTED_EDGE('',*,*,#48267,.T.);
#67446=ORIENTED_EDGE('',*,*,#48261,.F.);
#67447=ORIENTED_EDGE('',*,*,#48268,.F.);
#67448=ORIENTED_EDGE('',*,*,#48260,.F.);
#67449=ORIENTED_EDGE('',*,*,#48257,.T.);
#67450=ORIENTED_EDGE('',*,*,#48249,.F.);
#67451=ORIENTED_EDGE('',*,*,#48253,.F.);
#67452=ORIENTED_EDGE('',*,*,#48248,.F.);
#67453=ORIENTED_EDGE('',*,*,#48243,.T.);
#67454=ORIENTED_EDGE('',*,*,#48237,.F.);
#67455=ORIENTED_EDGE('',*,*,#48244,.F.);
#67456=ORIENTED_EDGE('',*,*,#48236,.F.);
#67457=ORIENTED_EDGE('',*,*,#48233,.T.);
#67458=ORIENTED_EDGE('',*,*,#48225,.F.);
#67459=ORIENTED_EDGE('',*,*,#48229,.F.);
#67460=ORIENTED_EDGE('',*,*,#48224,.F.);
#67461=ORIENTED_EDGE('',*,*,#48219,.T.);
#67462=ORIENTED_EDGE('',*,*,#48213,.F.);
#67463=ORIENTED_EDGE('',*,*,#48220,.F.);
#67464=ORIENTED_EDGE('',*,*,#48212,.F.);
#67465=ORIENTED_EDGE('',*,*,#48209,.T.);
#67466=ORIENTED_EDGE('',*,*,#48201,.F.);
#67467=ORIENTED_EDGE('',*,*,#48205,.F.);
#67468=ORIENTED_EDGE('',*,*,#48200,.F.);
#67469=ORIENTED_EDGE('',*,*,#48195,.T.);
#67470=ORIENTED_EDGE('',*,*,#48189,.F.);
#67471=ORIENTED_EDGE('',*,*,#48196,.F.);
#67472=ORIENTED_EDGE('',*,*,#48188,.F.);
#67473=ORIENTED_EDGE('',*,*,#48185,.T.);
#67474=ORIENTED_EDGE('',*,*,#48177,.F.);
#67475=ORIENTED_EDGE('',*,*,#48181,.F.);
#67476=ORIENTED_EDGE('',*,*,#48176,.F.);
#67477=ORIENTED_EDGE('',*,*,#48171,.T.);
#67478=ORIENTED_EDGE('',*,*,#48165,.F.);
#67479=ORIENTED_EDGE('',*,*,#48172,.F.);
#67480=ORIENTED_EDGE('',*,*,#48164,.F.);
#67481=ORIENTED_EDGE('',*,*,#48161,.T.);
#67482=ORIENTED_EDGE('',*,*,#48153,.F.);
#67483=ORIENTED_EDGE('',*,*,#48157,.F.);
#67484=ORIENTED_EDGE('',*,*,#48152,.F.);
#67485=ORIENTED_EDGE('',*,*,#48147,.T.);
#67486=ORIENTED_EDGE('',*,*,#48141,.F.);
#67487=ORIENTED_EDGE('',*,*,#48148,.F.);
#67488=ORIENTED_EDGE('',*,*,#48140,.F.);
#67489=ORIENTED_EDGE('',*,*,#48137,.T.);
#67490=ORIENTED_EDGE('',*,*,#48129,.F.);
#67491=ORIENTED_EDGE('',*,*,#48133,.F.);
#67492=ORIENTED_EDGE('',*,*,#48128,.F.);
#67493=ORIENTED_EDGE('',*,*,#48123,.T.);
#67494=ORIENTED_EDGE('',*,*,#48117,.F.);
#67495=ORIENTED_EDGE('',*,*,#48124,.F.);
#67496=ORIENTED_EDGE('',*,*,#48116,.F.);
#67497=ORIENTED_EDGE('',*,*,#48113,.T.);
#67498=ORIENTED_EDGE('',*,*,#48105,.F.);
#67499=ORIENTED_EDGE('',*,*,#48109,.F.);
#67500=ORIENTED_EDGE('',*,*,#48104,.F.);
#67501=ORIENTED_EDGE('',*,*,#48099,.T.);
#67502=ORIENTED_EDGE('',*,*,#48093,.F.);
#67503=ORIENTED_EDGE('',*,*,#48100,.F.);
#67504=ORIENTED_EDGE('',*,*,#48092,.F.);
#67505=ORIENTED_EDGE('',*,*,#48089,.T.);
#67506=ORIENTED_EDGE('',*,*,#48081,.F.);
#67507=ORIENTED_EDGE('',*,*,#48085,.F.);
#67508=ORIENTED_EDGE('',*,*,#48080,.F.);
#67509=ORIENTED_EDGE('',*,*,#48075,.T.);
#67510=ORIENTED_EDGE('',*,*,#48069,.F.);
#67511=ORIENTED_EDGE('',*,*,#48076,.F.);
#67512=ORIENTED_EDGE('',*,*,#48068,.F.);
#67513=ORIENTED_EDGE('',*,*,#48065,.T.);
#67514=ORIENTED_EDGE('',*,*,#48057,.F.);
#67515=ORIENTED_EDGE('',*,*,#48061,.F.);
#67516=ORIENTED_EDGE('',*,*,#48056,.F.);
#67517=ORIENTED_EDGE('',*,*,#48051,.T.);
#67518=ORIENTED_EDGE('',*,*,#48045,.F.);
#67519=ORIENTED_EDGE('',*,*,#48052,.F.);
#67520=ORIENTED_EDGE('',*,*,#48044,.F.);
#67521=ORIENTED_EDGE('',*,*,#48041,.T.);
#67522=ORIENTED_EDGE('',*,*,#48033,.F.);
#67523=ORIENTED_EDGE('',*,*,#48037,.F.);
#67524=ORIENTED_EDGE('',*,*,#48032,.F.);
#67525=ORIENTED_EDGE('',*,*,#48027,.T.);
#67526=ORIENTED_EDGE('',*,*,#48021,.F.);
#67527=ORIENTED_EDGE('',*,*,#48028,.F.);
#67528=ORIENTED_EDGE('',*,*,#48020,.F.);
#67529=ORIENTED_EDGE('',*,*,#48017,.T.);
#67530=ORIENTED_EDGE('',*,*,#48009,.F.);
#67531=ORIENTED_EDGE('',*,*,#48013,.F.);
#67532=ORIENTED_EDGE('',*,*,#48008,.F.);
#67533=ORIENTED_EDGE('',*,*,#48003,.T.);
#67534=ORIENTED_EDGE('',*,*,#47997,.F.);
#67535=ORIENTED_EDGE('',*,*,#48004,.F.);
#67536=ORIENTED_EDGE('',*,*,#47996,.F.);
#67537=ORIENTED_EDGE('',*,*,#47993,.T.);
#67538=ORIENTED_EDGE('',*,*,#47985,.F.);
#67539=ORIENTED_EDGE('',*,*,#47989,.F.);
#67540=ORIENTED_EDGE('',*,*,#47984,.F.);
#67541=ORIENTED_EDGE('',*,*,#47979,.T.);
#67542=ORIENTED_EDGE('',*,*,#47973,.F.);
#67543=ORIENTED_EDGE('',*,*,#47980,.F.);
#67544=ORIENTED_EDGE('',*,*,#47972,.F.);
#67545=ORIENTED_EDGE('',*,*,#47969,.T.);
#67546=ORIENTED_EDGE('',*,*,#47961,.F.);
#67547=ORIENTED_EDGE('',*,*,#47965,.F.);
#67548=ORIENTED_EDGE('',*,*,#47960,.F.);
#67549=ORIENTED_EDGE('',*,*,#47955,.T.);
#67550=ORIENTED_EDGE('',*,*,#47949,.F.);
#67551=ORIENTED_EDGE('',*,*,#47956,.F.);
#67552=ORIENTED_EDGE('',*,*,#47948,.F.);
#67553=ORIENTED_EDGE('',*,*,#47945,.T.);
#67554=ORIENTED_EDGE('',*,*,#47937,.F.);
#67555=ORIENTED_EDGE('',*,*,#47941,.F.);
#67556=ORIENTED_EDGE('',*,*,#47936,.F.);
#67557=ORIENTED_EDGE('',*,*,#47931,.T.);
#67558=ORIENTED_EDGE('',*,*,#47925,.F.);
#67559=ORIENTED_EDGE('',*,*,#47932,.F.);
#67560=ORIENTED_EDGE('',*,*,#47924,.F.);
#67561=ORIENTED_EDGE('',*,*,#47921,.T.);
#67562=ORIENTED_EDGE('',*,*,#47913,.F.);
#67563=ORIENTED_EDGE('',*,*,#47917,.F.);
#67564=ORIENTED_EDGE('',*,*,#47912,.F.);
#67565=ORIENTED_EDGE('',*,*,#47907,.T.);
#67566=ORIENTED_EDGE('',*,*,#47901,.F.);
#67567=ORIENTED_EDGE('',*,*,#47908,.F.);
#67568=ORIENTED_EDGE('',*,*,#47900,.F.);
#67569=ORIENTED_EDGE('',*,*,#47897,.T.);
#67570=ORIENTED_EDGE('',*,*,#47889,.F.);
#67571=ORIENTED_EDGE('',*,*,#47893,.F.);
#67572=ORIENTED_EDGE('',*,*,#47888,.F.);
#67573=ORIENTED_EDGE('',*,*,#47883,.T.);
#67574=ORIENTED_EDGE('',*,*,#47877,.F.);
#67575=ORIENTED_EDGE('',*,*,#47884,.F.);
#67576=ORIENTED_EDGE('',*,*,#47876,.F.);
#67577=ORIENTED_EDGE('',*,*,#47873,.T.);
#67578=ORIENTED_EDGE('',*,*,#47864,.F.);
#67579=ORIENTED_EDGE('',*,*,#47869,.F.);
#67580=ORIENTED_EDGE('',*,*,#48379,.F.);
#67581=ORIENTED_EDGE('',*,*,#48380,.T.);
#67582=ORIENTED_EDGE('',*,*,#48381,.F.);
#67583=ORIENTED_EDGE('',*,*,#48382,.F.);
#67584=ORIENTED_EDGE('',*,*,#48383,.T.);
#67585=ORIENTED_EDGE('',*,*,#48384,.T.);
#67586=ORIENTED_EDGE('',*,*,#48379,.T.);
#67587=ORIENTED_EDGE('',*,*,#47868,.T.);
#67588=ORIENTED_EDGE('',*,*,#48385,.F.);
#67589=ORIENTED_EDGE('',*,*,#48386,.T.);
#67590=ORIENTED_EDGE('',*,*,#48387,.F.);
#67591=ORIENTED_EDGE('',*,*,#48375,.T.);
#67592=ORIENTED_EDGE('',*,*,#48378,.T.);
#67593=ORIENTED_EDGE('',*,*,#48381,.T.);
#67594=ORIENTED_EDGE('',*,*,#48388,.T.);
#67595=ORIENTED_EDGE('',*,*,#48389,.F.);
#67596=ORIENTED_EDGE('',*,*,#48390,.F.);
#67597=ORIENTED_EDGE('',*,*,#48384,.F.);
#67598=ORIENTED_EDGE('',*,*,#48391,.F.);
#67599=ORIENTED_EDGE('',*,*,#48388,.F.);
#67600=ORIENTED_EDGE('',*,*,#48380,.F.);
#67601=ORIENTED_EDGE('',*,*,#48386,.F.);
#67602=ORIENTED_EDGE('',*,*,#48382,.T.);
#67603=ORIENTED_EDGE('',*,*,#48390,.T.);
#67604=ORIENTED_EDGE('',*,*,#48392,.F.);
#67605=ORIENTED_EDGE('',*,*,#48383,.F.);
#67606=ORIENTED_EDGE('',*,*,#48393,.T.);
#67607=ORIENTED_EDGE('',*,*,#48394,.T.);
#67608=ORIENTED_EDGE('',*,*,#48393,.F.);
#67609=ORIENTED_EDGE('',*,*,#48385,.T.);
#67610=ORIENTED_EDGE('',*,*,#47870,.T.);
#67611=ORIENTED_EDGE('',*,*,#47866,.T.);
#67612=ORIENTED_EDGE('',*,*,#47872,.T.);
#67613=ORIENTED_EDGE('',*,*,#47875,.T.);
#67614=ORIENTED_EDGE('',*,*,#47885,.T.);
#67615=ORIENTED_EDGE('',*,*,#47879,.T.);
#67616=ORIENTED_EDGE('',*,*,#47882,.T.);
#67617=ORIENTED_EDGE('',*,*,#47887,.T.);
#67618=ORIENTED_EDGE('',*,*,#47894,.T.);
#67619=ORIENTED_EDGE('',*,*,#47891,.T.);
#67620=ORIENTED_EDGE('',*,*,#47896,.T.);
#67621=ORIENTED_EDGE('',*,*,#47899,.T.);
#67622=ORIENTED_EDGE('',*,*,#47909,.T.);
#67623=ORIENTED_EDGE('',*,*,#47903,.T.);
#67624=ORIENTED_EDGE('',*,*,#47906,.T.);
#67625=ORIENTED_EDGE('',*,*,#47911,.T.);
#67626=ORIENTED_EDGE('',*,*,#47918,.T.);
#67627=ORIENTED_EDGE('',*,*,#47915,.T.);
#67628=ORIENTED_EDGE('',*,*,#47920,.T.);
#67629=ORIENTED_EDGE('',*,*,#47923,.T.);
#67630=ORIENTED_EDGE('',*,*,#47933,.T.);
#67631=ORIENTED_EDGE('',*,*,#47927,.T.);
#67632=ORIENTED_EDGE('',*,*,#47930,.T.);
#67633=ORIENTED_EDGE('',*,*,#47935,.T.);
#67634=ORIENTED_EDGE('',*,*,#47942,.T.);
#67635=ORIENTED_EDGE('',*,*,#47939,.T.);
#67636=ORIENTED_EDGE('',*,*,#47944,.T.);
#67637=ORIENTED_EDGE('',*,*,#47947,.T.);
#67638=ORIENTED_EDGE('',*,*,#47957,.T.);
#67639=ORIENTED_EDGE('',*,*,#47951,.T.);
#67640=ORIENTED_EDGE('',*,*,#47954,.T.);
#67641=ORIENTED_EDGE('',*,*,#47959,.T.);
#67642=ORIENTED_EDGE('',*,*,#47966,.T.);
#67643=ORIENTED_EDGE('',*,*,#47963,.T.);
#67644=ORIENTED_EDGE('',*,*,#47968,.T.);
#67645=ORIENTED_EDGE('',*,*,#47971,.T.);
#67646=ORIENTED_EDGE('',*,*,#47981,.T.);
#67647=ORIENTED_EDGE('',*,*,#47975,.T.);
#67648=ORIENTED_EDGE('',*,*,#47978,.T.);
#67649=ORIENTED_EDGE('',*,*,#47983,.T.);
#67650=ORIENTED_EDGE('',*,*,#47990,.T.);
#67651=ORIENTED_EDGE('',*,*,#47987,.T.);
#67652=ORIENTED_EDGE('',*,*,#47992,.T.);
#67653=ORIENTED_EDGE('',*,*,#47995,.T.);
#67654=ORIENTED_EDGE('',*,*,#48005,.T.);
#67655=ORIENTED_EDGE('',*,*,#47999,.T.);
#67656=ORIENTED_EDGE('',*,*,#48002,.T.);
#67657=ORIENTED_EDGE('',*,*,#48007,.T.);
#67658=ORIENTED_EDGE('',*,*,#48014,.T.);
#67659=ORIENTED_EDGE('',*,*,#48011,.T.);
#67660=ORIENTED_EDGE('',*,*,#48016,.T.);
#67661=ORIENTED_EDGE('',*,*,#48019,.T.);
#67662=ORIENTED_EDGE('',*,*,#48029,.T.);
#67663=ORIENTED_EDGE('',*,*,#48023,.T.);
#67664=ORIENTED_EDGE('',*,*,#48026,.T.);
#67665=ORIENTED_EDGE('',*,*,#48031,.T.);
#67666=ORIENTED_EDGE('',*,*,#48038,.T.);
#67667=ORIENTED_EDGE('',*,*,#48035,.T.);
#67668=ORIENTED_EDGE('',*,*,#48040,.T.);
#67669=ORIENTED_EDGE('',*,*,#48043,.T.);
#67670=ORIENTED_EDGE('',*,*,#48053,.T.);
#67671=ORIENTED_EDGE('',*,*,#48047,.T.);
#67672=ORIENTED_EDGE('',*,*,#48050,.T.);
#67673=ORIENTED_EDGE('',*,*,#48055,.T.);
#67674=ORIENTED_EDGE('',*,*,#48062,.T.);
#67675=ORIENTED_EDGE('',*,*,#48059,.T.);
#67676=ORIENTED_EDGE('',*,*,#48064,.T.);
#67677=ORIENTED_EDGE('',*,*,#48067,.T.);
#67678=ORIENTED_EDGE('',*,*,#48077,.T.);
#67679=ORIENTED_EDGE('',*,*,#48071,.T.);
#67680=ORIENTED_EDGE('',*,*,#48074,.T.);
#67681=ORIENTED_EDGE('',*,*,#48079,.T.);
#67682=ORIENTED_EDGE('',*,*,#48086,.T.);
#67683=ORIENTED_EDGE('',*,*,#48083,.T.);
#67684=ORIENTED_EDGE('',*,*,#48088,.T.);
#67685=ORIENTED_EDGE('',*,*,#48091,.T.);
#67686=ORIENTED_EDGE('',*,*,#48101,.T.);
#67687=ORIENTED_EDGE('',*,*,#48095,.T.);
#67688=ORIENTED_EDGE('',*,*,#48098,.T.);
#67689=ORIENTED_EDGE('',*,*,#48103,.T.);
#67690=ORIENTED_EDGE('',*,*,#48110,.T.);
#67691=ORIENTED_EDGE('',*,*,#48107,.T.);
#67692=ORIENTED_EDGE('',*,*,#48112,.T.);
#67693=ORIENTED_EDGE('',*,*,#48115,.T.);
#67694=ORIENTED_EDGE('',*,*,#48125,.T.);
#67695=ORIENTED_EDGE('',*,*,#48119,.T.);
#67696=ORIENTED_EDGE('',*,*,#48122,.T.);
#67697=ORIENTED_EDGE('',*,*,#48127,.T.);
#67698=ORIENTED_EDGE('',*,*,#48134,.T.);
#67699=ORIENTED_EDGE('',*,*,#48131,.T.);
#67700=ORIENTED_EDGE('',*,*,#48136,.T.);
#67701=ORIENTED_EDGE('',*,*,#48139,.T.);
#67702=ORIENTED_EDGE('',*,*,#48149,.T.);
#67703=ORIENTED_EDGE('',*,*,#48143,.T.);
#67704=ORIENTED_EDGE('',*,*,#48146,.T.);
#67705=ORIENTED_EDGE('',*,*,#48151,.T.);
#67706=ORIENTED_EDGE('',*,*,#48158,.T.);
#67707=ORIENTED_EDGE('',*,*,#48155,.T.);
#67708=ORIENTED_EDGE('',*,*,#48160,.T.);
#67709=ORIENTED_EDGE('',*,*,#48163,.T.);
#67710=ORIENTED_EDGE('',*,*,#48173,.T.);
#67711=ORIENTED_EDGE('',*,*,#48167,.T.);
#67712=ORIENTED_EDGE('',*,*,#48170,.T.);
#67713=ORIENTED_EDGE('',*,*,#48175,.T.);
#67714=ORIENTED_EDGE('',*,*,#48182,.T.);
#67715=ORIENTED_EDGE('',*,*,#48179,.T.);
#67716=ORIENTED_EDGE('',*,*,#48184,.T.);
#67717=ORIENTED_EDGE('',*,*,#48187,.T.);
#67718=ORIENTED_EDGE('',*,*,#48197,.T.);
#67719=ORIENTED_EDGE('',*,*,#48191,.T.);
#67720=ORIENTED_EDGE('',*,*,#48194,.T.);
#67721=ORIENTED_EDGE('',*,*,#48199,.T.);
#67722=ORIENTED_EDGE('',*,*,#48206,.T.);
#67723=ORIENTED_EDGE('',*,*,#48203,.T.);
#67724=ORIENTED_EDGE('',*,*,#48208,.T.);
#67725=ORIENTED_EDGE('',*,*,#48211,.T.);
#67726=ORIENTED_EDGE('',*,*,#48221,.T.);
#67727=ORIENTED_EDGE('',*,*,#48215,.T.);
#67728=ORIENTED_EDGE('',*,*,#48218,.T.);
#67729=ORIENTED_EDGE('',*,*,#48223,.T.);
#67730=ORIENTED_EDGE('',*,*,#48230,.T.);
#67731=ORIENTED_EDGE('',*,*,#48227,.T.);
#67732=ORIENTED_EDGE('',*,*,#48232,.T.);
#67733=ORIENTED_EDGE('',*,*,#48235,.T.);
#67734=ORIENTED_EDGE('',*,*,#48245,.T.);
#67735=ORIENTED_EDGE('',*,*,#48239,.T.);
#67736=ORIENTED_EDGE('',*,*,#48242,.T.);
#67737=ORIENTED_EDGE('',*,*,#48247,.T.);
#67738=ORIENTED_EDGE('',*,*,#48254,.T.);
#67739=ORIENTED_EDGE('',*,*,#48251,.T.);
#67740=ORIENTED_EDGE('',*,*,#48256,.T.);
#67741=ORIENTED_EDGE('',*,*,#48259,.T.);
#67742=ORIENTED_EDGE('',*,*,#48269,.T.);
#67743=ORIENTED_EDGE('',*,*,#48263,.T.);
#67744=ORIENTED_EDGE('',*,*,#48266,.T.);
#67745=ORIENTED_EDGE('',*,*,#48271,.T.);
#67746=ORIENTED_EDGE('',*,*,#48278,.T.);
#67747=ORIENTED_EDGE('',*,*,#48275,.T.);
#67748=ORIENTED_EDGE('',*,*,#48280,.T.);
#67749=ORIENTED_EDGE('',*,*,#48283,.T.);
#67750=ORIENTED_EDGE('',*,*,#48293,.T.);
#67751=ORIENTED_EDGE('',*,*,#48287,.T.);
#67752=ORIENTED_EDGE('',*,*,#48290,.T.);
#67753=ORIENTED_EDGE('',*,*,#48295,.T.);
#67754=ORIENTED_EDGE('',*,*,#48302,.T.);
#67755=ORIENTED_EDGE('',*,*,#48299,.T.);
#67756=ORIENTED_EDGE('',*,*,#48304,.T.);
#67757=ORIENTED_EDGE('',*,*,#48307,.T.);
#67758=ORIENTED_EDGE('',*,*,#48317,.T.);
#67759=ORIENTED_EDGE('',*,*,#48311,.T.);
#67760=ORIENTED_EDGE('',*,*,#48314,.T.);
#67761=ORIENTED_EDGE('',*,*,#48319,.T.);
#67762=ORIENTED_EDGE('',*,*,#48326,.T.);
#67763=ORIENTED_EDGE('',*,*,#48323,.T.);
#67764=ORIENTED_EDGE('',*,*,#48328,.T.);
#67765=ORIENTED_EDGE('',*,*,#48331,.T.);
#67766=ORIENTED_EDGE('',*,*,#48341,.T.);
#67767=ORIENTED_EDGE('',*,*,#48335,.T.);
#67768=ORIENTED_EDGE('',*,*,#48338,.T.);
#67769=ORIENTED_EDGE('',*,*,#48343,.T.);
#67770=ORIENTED_EDGE('',*,*,#48350,.T.);
#67771=ORIENTED_EDGE('',*,*,#48347,.T.);
#67772=ORIENTED_EDGE('',*,*,#48352,.T.);
#67773=ORIENTED_EDGE('',*,*,#48355,.T.);
#67774=ORIENTED_EDGE('',*,*,#48365,.T.);
#67775=ORIENTED_EDGE('',*,*,#48359,.T.);
#67776=ORIENTED_EDGE('',*,*,#48362,.T.);
#67777=ORIENTED_EDGE('',*,*,#48367,.T.);
#67778=ORIENTED_EDGE('',*,*,#48374,.T.);
#67779=ORIENTED_EDGE('',*,*,#48371,.T.);
#67780=ORIENTED_EDGE('',*,*,#48376,.T.);
#67781=ORIENTED_EDGE('',*,*,#48387,.T.);
#67782=ORIENTED_EDGE('',*,*,#48392,.T.);
#67783=ORIENTED_EDGE('',*,*,#48389,.T.);
#67784=ORIENTED_EDGE('',*,*,#48391,.T.);
#67785=ORIENTED_EDGE('',*,*,#48394,.F.);
#67786=ORIENTED_EDGE('',*,*,#48395,.F.);
#67787=ORIENTED_EDGE('',*,*,#48396,.T.);
#67788=ORIENTED_EDGE('',*,*,#48397,.F.);
#67789=ORIENTED_EDGE('',*,*,#48396,.F.);
#67790=ORIENTED_EDGE('',*,*,#48398,.F.);
#67791=ORIENTED_EDGE('',*,*,#48399,.T.);
#67792=ORIENTED_EDGE('',*,*,#48400,.F.);
#67793=ORIENTED_EDGE('',*,*,#48399,.F.);
#67794=ORIENTED_EDGE('',*,*,#48400,.T.);
#67795=ORIENTED_EDGE('',*,*,#48395,.T.);
#67796=ORIENTED_EDGE('',*,*,#48401,.T.);
#67797=ORIENTED_EDGE('',*,*,#48402,.T.);
#67798=ORIENTED_EDGE('',*,*,#48403,.T.);
#67799=ORIENTED_EDGE('',*,*,#48404,.T.);
#67800=ORIENTED_EDGE('',*,*,#48405,.T.);
#67801=ORIENTED_EDGE('',*,*,#48406,.T.);
#67802=ORIENTED_EDGE('',*,*,#48407,.T.);
#67803=ORIENTED_EDGE('',*,*,#48408,.T.);
#67804=ORIENTED_EDGE('',*,*,#48409,.T.);
#67805=ORIENTED_EDGE('',*,*,#48410,.T.);
#67806=ORIENTED_EDGE('',*,*,#48411,.T.);
#67807=ORIENTED_EDGE('',*,*,#48412,.T.);
#67808=ORIENTED_EDGE('',*,*,#48413,.T.);
#67809=ORIENTED_EDGE('',*,*,#48414,.T.);
#67810=ORIENTED_EDGE('',*,*,#48415,.T.);
#67811=ORIENTED_EDGE('',*,*,#48416,.T.);
#67812=ORIENTED_EDGE('',*,*,#48417,.T.);
#67813=ORIENTED_EDGE('',*,*,#48418,.T.);
#67814=ORIENTED_EDGE('',*,*,#48419,.T.);
#67815=ORIENTED_EDGE('',*,*,#48420,.T.);
#67816=ORIENTED_EDGE('',*,*,#48421,.T.);
#67817=ORIENTED_EDGE('',*,*,#48422,.T.);
#67818=ORIENTED_EDGE('',*,*,#48423,.T.);
#67819=ORIENTED_EDGE('',*,*,#48424,.T.);
#67820=ORIENTED_EDGE('',*,*,#48425,.T.);
#67821=ORIENTED_EDGE('',*,*,#48426,.T.);
#67822=ORIENTED_EDGE('',*,*,#48427,.T.);
#67823=ORIENTED_EDGE('',*,*,#48428,.T.);
#67824=ORIENTED_EDGE('',*,*,#48429,.T.);
#67825=ORIENTED_EDGE('',*,*,#48430,.T.);
#67826=ORIENTED_EDGE('',*,*,#48431,.T.);
#67827=ORIENTED_EDGE('',*,*,#48432,.T.);
#67828=ORIENTED_EDGE('',*,*,#48433,.T.);
#67829=ORIENTED_EDGE('',*,*,#48434,.T.);
#67830=ORIENTED_EDGE('',*,*,#48435,.T.);
#67831=ORIENTED_EDGE('',*,*,#48436,.T.);
#67832=ORIENTED_EDGE('',*,*,#48437,.T.);
#67833=ORIENTED_EDGE('',*,*,#48438,.T.);
#67834=ORIENTED_EDGE('',*,*,#48439,.T.);
#67835=ORIENTED_EDGE('',*,*,#48440,.T.);
#67836=ORIENTED_EDGE('',*,*,#48441,.T.);
#67837=ORIENTED_EDGE('',*,*,#48442,.T.);
#67838=ORIENTED_EDGE('',*,*,#48443,.T.);
#67839=ORIENTED_EDGE('',*,*,#48444,.T.);
#67840=ORIENTED_EDGE('',*,*,#48445,.T.);
#67841=ORIENTED_EDGE('',*,*,#48446,.T.);
#67842=ORIENTED_EDGE('',*,*,#48447,.T.);
#67843=ORIENTED_EDGE('',*,*,#48448,.T.);
#67844=ORIENTED_EDGE('',*,*,#48449,.T.);
#67845=ORIENTED_EDGE('',*,*,#48450,.T.);
#67846=ORIENTED_EDGE('',*,*,#48451,.T.);
#67847=ORIENTED_EDGE('',*,*,#48452,.T.);
#67848=ORIENTED_EDGE('',*,*,#48453,.T.);
#67849=ORIENTED_EDGE('',*,*,#48454,.T.);
#67850=ORIENTED_EDGE('',*,*,#48455,.T.);
#67851=ORIENTED_EDGE('',*,*,#48456,.T.);
#67852=ORIENTED_EDGE('',*,*,#48457,.T.);
#67853=ORIENTED_EDGE('',*,*,#48458,.T.);
#67854=ORIENTED_EDGE('',*,*,#48459,.T.);
#67855=ORIENTED_EDGE('',*,*,#48460,.T.);
#67856=ORIENTED_EDGE('',*,*,#48461,.T.);
#67857=ORIENTED_EDGE('',*,*,#48462,.T.);
#67858=ORIENTED_EDGE('',*,*,#48463,.T.);
#67859=ORIENTED_EDGE('',*,*,#48464,.T.);
#67860=ORIENTED_EDGE('',*,*,#48465,.T.);
#67861=ORIENTED_EDGE('',*,*,#48466,.T.);
#67862=ORIENTED_EDGE('',*,*,#48467,.T.);
#67863=ORIENTED_EDGE('',*,*,#48468,.T.);
#67864=ORIENTED_EDGE('',*,*,#48469,.T.);
#67865=ORIENTED_EDGE('',*,*,#48470,.T.);
#67866=ORIENTED_EDGE('',*,*,#48471,.T.);
#67867=ORIENTED_EDGE('',*,*,#48472,.T.);
#67868=ORIENTED_EDGE('',*,*,#48473,.T.);
#67869=ORIENTED_EDGE('',*,*,#48474,.T.);
#67870=ORIENTED_EDGE('',*,*,#48475,.T.);
#67871=ORIENTED_EDGE('',*,*,#48476,.T.);
#67872=ORIENTED_EDGE('',*,*,#48477,.T.);
#67873=ORIENTED_EDGE('',*,*,#48478,.T.);
#67874=ORIENTED_EDGE('',*,*,#48479,.T.);
#67875=ORIENTED_EDGE('',*,*,#48480,.T.);
#67876=ORIENTED_EDGE('',*,*,#48481,.T.);
#67877=ORIENTED_EDGE('',*,*,#48482,.T.);
#67878=ORIENTED_EDGE('',*,*,#48483,.T.);
#67879=ORIENTED_EDGE('',*,*,#48484,.T.);
#67880=ORIENTED_EDGE('',*,*,#48485,.T.);
#67881=ORIENTED_EDGE('',*,*,#48486,.T.);
#67882=ORIENTED_EDGE('',*,*,#48487,.T.);
#67883=ORIENTED_EDGE('',*,*,#48488,.T.);
#67884=ORIENTED_EDGE('',*,*,#48489,.T.);
#67885=ORIENTED_EDGE('',*,*,#48490,.T.);
#67886=ORIENTED_EDGE('',*,*,#48491,.T.);
#67887=ORIENTED_EDGE('',*,*,#48492,.T.);
#67888=ORIENTED_EDGE('',*,*,#48493,.T.);
#67889=ORIENTED_EDGE('',*,*,#48494,.T.);
#67890=ORIENTED_EDGE('',*,*,#48495,.T.);
#67891=ORIENTED_EDGE('',*,*,#48496,.T.);
#67892=ORIENTED_EDGE('',*,*,#48497,.T.);
#67893=ORIENTED_EDGE('',*,*,#48498,.T.);
#67894=ORIENTED_EDGE('',*,*,#48499,.T.);
#67895=ORIENTED_EDGE('',*,*,#48500,.T.);
#67896=ORIENTED_EDGE('',*,*,#48501,.T.);
#67897=ORIENTED_EDGE('',*,*,#48502,.T.);
#67898=ORIENTED_EDGE('',*,*,#48503,.T.);
#67899=ORIENTED_EDGE('',*,*,#48504,.F.);
#67900=ORIENTED_EDGE('',*,*,#48505,.T.);
#67901=ORIENTED_EDGE('',*,*,#48506,.F.);
#67902=ORIENTED_EDGE('',*,*,#48505,.F.);
#67903=ORIENTED_EDGE('',*,*,#48504,.T.);
#67904=ORIENTED_EDGE('',*,*,#48398,.T.);
#67905=ORIENTED_EDGE('',*,*,#48453,.F.);
#67906=ORIENTED_EDGE('',*,*,#48507,.T.);
#67907=ORIENTED_EDGE('',*,*,#48508,.F.);
#67908=ORIENTED_EDGE('',*,*,#48509,.F.);
#67909=ORIENTED_EDGE('',*,*,#48452,.F.);
#67910=ORIENTED_EDGE('',*,*,#48510,.T.);
#67911=ORIENTED_EDGE('',*,*,#48511,.F.);
#67912=ORIENTED_EDGE('',*,*,#48507,.F.);
#67913=ORIENTED_EDGE('',*,*,#48451,.F.);
#67914=ORIENTED_EDGE('',*,*,#48512,.F.);
#67915=ORIENTED_EDGE('',*,*,#48513,.F.);
#67916=ORIENTED_EDGE('',*,*,#48510,.F.);
#67917=ORIENTED_EDGE('',*,*,#48450,.F.);
#67918=ORIENTED_EDGE('',*,*,#48514,.T.);
#67919=ORIENTED_EDGE('',*,*,#48515,.F.);
#67920=ORIENTED_EDGE('',*,*,#48512,.T.);
#67921=ORIENTED_EDGE('',*,*,#48449,.F.);
#67922=ORIENTED_EDGE('',*,*,#48516,.T.);
#67923=ORIENTED_EDGE('',*,*,#48517,.F.);
#67924=ORIENTED_EDGE('',*,*,#48514,.F.);
#67925=ORIENTED_EDGE('',*,*,#48448,.F.);
#67926=ORIENTED_EDGE('',*,*,#48518,.T.);
#67927=ORIENTED_EDGE('',*,*,#48519,.F.);
#67928=ORIENTED_EDGE('',*,*,#48516,.F.);
#67929=ORIENTED_EDGE('',*,*,#48447,.F.);
#67930=ORIENTED_EDGE('',*,*,#48520,.T.);
#67931=ORIENTED_EDGE('',*,*,#48521,.F.);
#67932=ORIENTED_EDGE('',*,*,#48518,.F.);
#67933=ORIENTED_EDGE('',*,*,#48446,.F.);
#67934=ORIENTED_EDGE('',*,*,#48522,.T.);
#67935=ORIENTED_EDGE('',*,*,#48523,.F.);
#67936=ORIENTED_EDGE('',*,*,#48520,.F.);
#67937=ORIENTED_EDGE('',*,*,#48445,.F.);
#67938=ORIENTED_EDGE('',*,*,#48524,.F.);
#67939=ORIENTED_EDGE('',*,*,#48525,.F.);
#67940=ORIENTED_EDGE('',*,*,#48522,.F.);
#67941=ORIENTED_EDGE('',*,*,#48444,.F.);
#67942=ORIENTED_EDGE('',*,*,#48526,.T.);
#67943=ORIENTED_EDGE('',*,*,#48527,.F.);
#67944=ORIENTED_EDGE('',*,*,#48524,.T.);
#67945=ORIENTED_EDGE('',*,*,#48443,.F.);
#67946=ORIENTED_EDGE('',*,*,#48528,.T.);
#67947=ORIENTED_EDGE('',*,*,#48529,.F.);
#67948=ORIENTED_EDGE('',*,*,#48526,.F.);
#67949=ORIENTED_EDGE('',*,*,#48442,.F.);
#67950=ORIENTED_EDGE('',*,*,#48530,.T.);
#67951=ORIENTED_EDGE('',*,*,#48531,.F.);
#67952=ORIENTED_EDGE('',*,*,#48528,.F.);
#67953=ORIENTED_EDGE('',*,*,#48441,.F.);
#67954=ORIENTED_EDGE('',*,*,#48532,.T.);
#67955=ORIENTED_EDGE('',*,*,#48533,.F.);
#67956=ORIENTED_EDGE('',*,*,#48530,.F.);
#67957=ORIENTED_EDGE('',*,*,#48440,.F.);
#67958=ORIENTED_EDGE('',*,*,#48534,.T.);
#67959=ORIENTED_EDGE('',*,*,#48535,.F.);
#67960=ORIENTED_EDGE('',*,*,#48532,.F.);
#67961=ORIENTED_EDGE('',*,*,#48439,.F.);
#67962=ORIENTED_EDGE('',*,*,#48536,.F.);
#67963=ORIENTED_EDGE('',*,*,#48537,.F.);
#67964=ORIENTED_EDGE('',*,*,#48534,.F.);
#67965=ORIENTED_EDGE('',*,*,#48438,.F.);
#67966=ORIENTED_EDGE('',*,*,#48538,.T.);
#67967=ORIENTED_EDGE('',*,*,#48539,.F.);
#67968=ORIENTED_EDGE('',*,*,#48536,.T.);
#67969=ORIENTED_EDGE('',*,*,#48437,.F.);
#67970=ORIENTED_EDGE('',*,*,#48540,.T.);
#67971=ORIENTED_EDGE('',*,*,#48541,.F.);
#67972=ORIENTED_EDGE('',*,*,#48538,.F.);
#67973=ORIENTED_EDGE('',*,*,#48540,.F.);
#67974=ORIENTED_EDGE('',*,*,#48436,.F.);
#67975=ORIENTED_EDGE('',*,*,#48542,.T.);
#67976=ORIENTED_EDGE('',*,*,#48543,.F.);
#67977=ORIENTED_EDGE('',*,*,#48435,.F.);
#67978=ORIENTED_EDGE('',*,*,#48544,.T.);
#67979=ORIENTED_EDGE('',*,*,#48545,.F.);
#67980=ORIENTED_EDGE('',*,*,#48542,.F.);
#67981=ORIENTED_EDGE('',*,*,#48434,.F.);
#67982=ORIENTED_EDGE('',*,*,#48546,.T.);
#67983=ORIENTED_EDGE('',*,*,#48547,.F.);
#67984=ORIENTED_EDGE('',*,*,#48544,.F.);
#67985=ORIENTED_EDGE('',*,*,#48433,.F.);
#67986=ORIENTED_EDGE('',*,*,#48548,.F.);
#67987=ORIENTED_EDGE('',*,*,#48549,.F.);
#67988=ORIENTED_EDGE('',*,*,#48546,.F.);
#67989=ORIENTED_EDGE('',*,*,#48432,.F.);
#67990=ORIENTED_EDGE('',*,*,#48550,.T.);
#67991=ORIENTED_EDGE('',*,*,#48551,.F.);
#67992=ORIENTED_EDGE('',*,*,#48548,.T.);
#67993=ORIENTED_EDGE('',*,*,#48431,.F.);
#67994=ORIENTED_EDGE('',*,*,#48552,.T.);
#67995=ORIENTED_EDGE('',*,*,#48553,.F.);
#67996=ORIENTED_EDGE('',*,*,#48550,.F.);
#67997=ORIENTED_EDGE('',*,*,#48430,.F.);
#67998=ORIENTED_EDGE('',*,*,#48554,.T.);
#67999=ORIENTED_EDGE('',*,*,#48555,.F.);
#68000=ORIENTED_EDGE('',*,*,#48552,.F.);
#68001=ORIENTED_EDGE('',*,*,#48429,.F.);
#68002=ORIENTED_EDGE('',*,*,#48556,.T.);
#68003=ORIENTED_EDGE('',*,*,#48557,.F.);
#68004=ORIENTED_EDGE('',*,*,#48554,.F.);
#68005=ORIENTED_EDGE('',*,*,#48428,.F.);
#68006=ORIENTED_EDGE('',*,*,#48558,.T.);
#68007=ORIENTED_EDGE('',*,*,#48559,.F.);
#68008=ORIENTED_EDGE('',*,*,#48556,.F.);
#68009=ORIENTED_EDGE('',*,*,#48427,.F.);
#68010=ORIENTED_EDGE('',*,*,#48560,.F.);
#68011=ORIENTED_EDGE('',*,*,#48561,.F.);
#68012=ORIENTED_EDGE('',*,*,#48558,.F.);
#68013=ORIENTED_EDGE('',*,*,#48426,.F.);
#68014=ORIENTED_EDGE('',*,*,#48562,.T.);
#68015=ORIENTED_EDGE('',*,*,#48563,.F.);
#68016=ORIENTED_EDGE('',*,*,#48560,.T.);
#68017=ORIENTED_EDGE('',*,*,#48425,.F.);
#68018=ORIENTED_EDGE('',*,*,#48564,.T.);
#68019=ORIENTED_EDGE('',*,*,#48565,.F.);
#68020=ORIENTED_EDGE('',*,*,#48562,.F.);
#68021=ORIENTED_EDGE('',*,*,#48424,.F.);
#68022=ORIENTED_EDGE('',*,*,#48566,.T.);
#68023=ORIENTED_EDGE('',*,*,#48567,.F.);
#68024=ORIENTED_EDGE('',*,*,#48564,.F.);
#68025=ORIENTED_EDGE('',*,*,#48423,.F.);
#68026=ORIENTED_EDGE('',*,*,#48568,.T.);
#68027=ORIENTED_EDGE('',*,*,#48569,.F.);
#68028=ORIENTED_EDGE('',*,*,#48566,.F.);
#68029=ORIENTED_EDGE('',*,*,#48422,.F.);
#68030=ORIENTED_EDGE('',*,*,#48570,.T.);
#68031=ORIENTED_EDGE('',*,*,#48571,.F.);
#68032=ORIENTED_EDGE('',*,*,#48568,.F.);
#68033=ORIENTED_EDGE('',*,*,#48421,.F.);
#68034=ORIENTED_EDGE('',*,*,#48572,.F.);
#68035=ORIENTED_EDGE('',*,*,#48573,.F.);
#68036=ORIENTED_EDGE('',*,*,#48570,.F.);
#68037=ORIENTED_EDGE('',*,*,#48420,.F.);
#68038=ORIENTED_EDGE('',*,*,#48574,.T.);
#68039=ORIENTED_EDGE('',*,*,#48575,.F.);
#68040=ORIENTED_EDGE('',*,*,#48572,.T.);
#68041=ORIENTED_EDGE('',*,*,#48419,.F.);
#68042=ORIENTED_EDGE('',*,*,#48576,.T.);
#68043=ORIENTED_EDGE('',*,*,#48577,.F.);
#68044=ORIENTED_EDGE('',*,*,#48574,.F.);
#68045=ORIENTED_EDGE('',*,*,#48418,.F.);
#68046=ORIENTED_EDGE('',*,*,#48578,.T.);
#68047=ORIENTED_EDGE('',*,*,#48579,.F.);
#68048=ORIENTED_EDGE('',*,*,#48576,.F.);
#68049=ORIENTED_EDGE('',*,*,#48417,.F.);
#68050=ORIENTED_EDGE('',*,*,#48580,.T.);
#68051=ORIENTED_EDGE('',*,*,#48581,.F.);
#68052=ORIENTED_EDGE('',*,*,#48578,.F.);
#68053=ORIENTED_EDGE('',*,*,#48416,.F.);
#68054=ORIENTED_EDGE('',*,*,#48582,.T.);
#68055=ORIENTED_EDGE('',*,*,#48583,.F.);
#68056=ORIENTED_EDGE('',*,*,#48580,.F.);
#68057=ORIENTED_EDGE('',*,*,#48415,.F.);
#68058=ORIENTED_EDGE('',*,*,#48584,.F.);
#68059=ORIENTED_EDGE('',*,*,#48585,.F.);
#68060=ORIENTED_EDGE('',*,*,#48582,.F.);
#68061=ORIENTED_EDGE('',*,*,#48414,.F.);
#68062=ORIENTED_EDGE('',*,*,#48586,.T.);
#68063=ORIENTED_EDGE('',*,*,#48587,.F.);
#68064=ORIENTED_EDGE('',*,*,#48584,.T.);
#68065=ORIENTED_EDGE('',*,*,#48413,.F.);
#68066=ORIENTED_EDGE('',*,*,#48588,.T.);
#68067=ORIENTED_EDGE('',*,*,#48589,.F.);
#68068=ORIENTED_EDGE('',*,*,#48586,.F.);
#68069=ORIENTED_EDGE('',*,*,#48412,.F.);
#68070=ORIENTED_EDGE('',*,*,#48590,.T.);
#68071=ORIENTED_EDGE('',*,*,#48591,.F.);
#68072=ORIENTED_EDGE('',*,*,#48588,.F.);
#68073=ORIENTED_EDGE('',*,*,#48411,.F.);
#68074=ORIENTED_EDGE('',*,*,#48592,.T.);
#68075=ORIENTED_EDGE('',*,*,#48593,.F.);
#68076=ORIENTED_EDGE('',*,*,#48590,.F.);
#68077=ORIENTED_EDGE('',*,*,#48410,.F.);
#68078=ORIENTED_EDGE('',*,*,#48594,.T.);
#68079=ORIENTED_EDGE('',*,*,#48595,.F.);
#68080=ORIENTED_EDGE('',*,*,#48592,.F.);
#68081=ORIENTED_EDGE('',*,*,#48409,.F.);
#68082=ORIENTED_EDGE('',*,*,#48596,.F.);
#68083=ORIENTED_EDGE('',*,*,#48597,.F.);
#68084=ORIENTED_EDGE('',*,*,#48594,.F.);
#68085=ORIENTED_EDGE('',*,*,#48408,.F.);
#68086=ORIENTED_EDGE('',*,*,#48598,.T.);
#68087=ORIENTED_EDGE('',*,*,#48599,.F.);
#68088=ORIENTED_EDGE('',*,*,#48596,.T.);
#68089=ORIENTED_EDGE('',*,*,#48407,.F.);
#68090=ORIENTED_EDGE('',*,*,#48600,.T.);
#68091=ORIENTED_EDGE('',*,*,#48601,.F.);
#68092=ORIENTED_EDGE('',*,*,#48598,.F.);
#68093=ORIENTED_EDGE('',*,*,#48406,.F.);
#68094=ORIENTED_EDGE('',*,*,#48602,.T.);
#68095=ORIENTED_EDGE('',*,*,#48603,.F.);
#68096=ORIENTED_EDGE('',*,*,#48600,.F.);
#68097=ORIENTED_EDGE('',*,*,#48405,.F.);
#68098=ORIENTED_EDGE('',*,*,#48604,.T.);
#68099=ORIENTED_EDGE('',*,*,#48605,.F.);
#68100=ORIENTED_EDGE('',*,*,#48602,.F.);
#68101=ORIENTED_EDGE('',*,*,#48404,.F.);
#68102=ORIENTED_EDGE('',*,*,#48606,.T.);
#68103=ORIENTED_EDGE('',*,*,#48607,.F.);
#68104=ORIENTED_EDGE('',*,*,#48604,.F.);
#68105=ORIENTED_EDGE('',*,*,#48403,.F.);
#68106=ORIENTED_EDGE('',*,*,#48608,.F.);
#68107=ORIENTED_EDGE('',*,*,#48609,.F.);
#68108=ORIENTED_EDGE('',*,*,#48606,.F.);
#68109=ORIENTED_EDGE('',*,*,#48543,.T.);
#68110=ORIENTED_EDGE('',*,*,#48545,.T.);
#68111=ORIENTED_EDGE('',*,*,#48547,.T.);
#68112=ORIENTED_EDGE('',*,*,#48549,.T.);
#68113=ORIENTED_EDGE('',*,*,#48551,.T.);
#68114=ORIENTED_EDGE('',*,*,#48553,.T.);
#68115=ORIENTED_EDGE('',*,*,#48555,.T.);
#68116=ORIENTED_EDGE('',*,*,#48557,.T.);
#68117=ORIENTED_EDGE('',*,*,#48559,.T.);
#68118=ORIENTED_EDGE('',*,*,#48561,.T.);
#68119=ORIENTED_EDGE('',*,*,#48563,.T.);
#68120=ORIENTED_EDGE('',*,*,#48565,.T.);
#68121=ORIENTED_EDGE('',*,*,#48567,.T.);
#68122=ORIENTED_EDGE('',*,*,#48569,.T.);
#68123=ORIENTED_EDGE('',*,*,#48571,.T.);
#68124=ORIENTED_EDGE('',*,*,#48573,.T.);
#68125=ORIENTED_EDGE('',*,*,#48575,.T.);
#68126=ORIENTED_EDGE('',*,*,#48577,.T.);
#68127=ORIENTED_EDGE('',*,*,#48579,.T.);
#68128=ORIENTED_EDGE('',*,*,#48581,.T.);
#68129=ORIENTED_EDGE('',*,*,#48583,.T.);
#68130=ORIENTED_EDGE('',*,*,#48585,.T.);
#68131=ORIENTED_EDGE('',*,*,#48587,.T.);
#68132=ORIENTED_EDGE('',*,*,#48589,.T.);
#68133=ORIENTED_EDGE('',*,*,#48591,.T.);
#68134=ORIENTED_EDGE('',*,*,#48593,.T.);
#68135=ORIENTED_EDGE('',*,*,#48595,.T.);
#68136=ORIENTED_EDGE('',*,*,#48597,.T.);
#68137=ORIENTED_EDGE('',*,*,#48599,.T.);
#68138=ORIENTED_EDGE('',*,*,#48601,.T.);
#68139=ORIENTED_EDGE('',*,*,#48603,.T.);
#68140=ORIENTED_EDGE('',*,*,#48605,.T.);
#68141=ORIENTED_EDGE('',*,*,#48607,.T.);
#68142=ORIENTED_EDGE('',*,*,#48609,.T.);
#68143=ORIENTED_EDGE('',*,*,#48610,.T.);
#68144=ORIENTED_EDGE('',*,*,#48611,.T.);
#68145=ORIENTED_EDGE('',*,*,#48612,.T.);
#68146=ORIENTED_EDGE('',*,*,#48613,.T.);
#68147=ORIENTED_EDGE('',*,*,#48614,.T.);
#68148=ORIENTED_EDGE('',*,*,#48615,.T.);
#68149=ORIENTED_EDGE('',*,*,#48616,.T.);
#68150=ORIENTED_EDGE('',*,*,#48617,.T.);
#68151=ORIENTED_EDGE('',*,*,#48618,.T.);
#68152=ORIENTED_EDGE('',*,*,#48619,.T.);
#68153=ORIENTED_EDGE('',*,*,#48620,.T.);
#68154=ORIENTED_EDGE('',*,*,#48621,.T.);
#68155=ORIENTED_EDGE('',*,*,#48622,.T.);
#68156=ORIENTED_EDGE('',*,*,#48623,.T.);
#68157=ORIENTED_EDGE('',*,*,#48624,.T.);
#68158=ORIENTED_EDGE('',*,*,#48625,.T.);
#68159=ORIENTED_EDGE('',*,*,#48626,.T.);
#68160=ORIENTED_EDGE('',*,*,#48627,.T.);
#68161=ORIENTED_EDGE('',*,*,#48628,.T.);
#68162=ORIENTED_EDGE('',*,*,#48629,.T.);
#68163=ORIENTED_EDGE('',*,*,#48630,.T.);
#68164=ORIENTED_EDGE('',*,*,#48631,.T.);
#68165=ORIENTED_EDGE('',*,*,#48632,.T.);
#68166=ORIENTED_EDGE('',*,*,#48633,.T.);
#68167=ORIENTED_EDGE('',*,*,#48634,.T.);
#68168=ORIENTED_EDGE('',*,*,#48635,.T.);
#68169=ORIENTED_EDGE('',*,*,#48636,.T.);
#68170=ORIENTED_EDGE('',*,*,#48637,.T.);
#68171=ORIENTED_EDGE('',*,*,#48638,.T.);
#68172=ORIENTED_EDGE('',*,*,#48639,.T.);
#68173=ORIENTED_EDGE('',*,*,#48640,.T.);
#68174=ORIENTED_EDGE('',*,*,#48641,.T.);
#68175=ORIENTED_EDGE('',*,*,#48642,.T.);
#68176=ORIENTED_EDGE('',*,*,#48643,.T.);
#68177=ORIENTED_EDGE('',*,*,#48644,.T.);
#68178=ORIENTED_EDGE('',*,*,#48645,.T.);
#68179=ORIENTED_EDGE('',*,*,#48646,.T.);
#68180=ORIENTED_EDGE('',*,*,#48647,.T.);
#68181=ORIENTED_EDGE('',*,*,#48648,.T.);
#68182=ORIENTED_EDGE('',*,*,#48649,.T.);
#68183=ORIENTED_EDGE('',*,*,#48650,.T.);
#68184=ORIENTED_EDGE('',*,*,#48651,.T.);
#68185=ORIENTED_EDGE('',*,*,#48652,.T.);
#68186=ORIENTED_EDGE('',*,*,#48653,.T.);
#68187=ORIENTED_EDGE('',*,*,#48654,.T.);
#68188=ORIENTED_EDGE('',*,*,#48655,.T.);
#68189=ORIENTED_EDGE('',*,*,#48656,.T.);
#68190=ORIENTED_EDGE('',*,*,#48657,.T.);
#68191=ORIENTED_EDGE('',*,*,#48658,.T.);
#68192=ORIENTED_EDGE('',*,*,#48659,.T.);
#68193=ORIENTED_EDGE('',*,*,#48660,.T.);
#68194=ORIENTED_EDGE('',*,*,#48508,.T.);
#68195=ORIENTED_EDGE('',*,*,#48511,.T.);
#68196=ORIENTED_EDGE('',*,*,#48513,.T.);
#68197=ORIENTED_EDGE('',*,*,#48515,.T.);
#68198=ORIENTED_EDGE('',*,*,#48517,.T.);
#68199=ORIENTED_EDGE('',*,*,#48519,.T.);
#68200=ORIENTED_EDGE('',*,*,#48521,.T.);
#68201=ORIENTED_EDGE('',*,*,#48523,.T.);
#68202=ORIENTED_EDGE('',*,*,#48525,.T.);
#68203=ORIENTED_EDGE('',*,*,#48527,.T.);
#68204=ORIENTED_EDGE('',*,*,#48529,.T.);
#68205=ORIENTED_EDGE('',*,*,#48531,.T.);
#68206=ORIENTED_EDGE('',*,*,#48533,.T.);
#68207=ORIENTED_EDGE('',*,*,#48535,.T.);
#68208=ORIENTED_EDGE('',*,*,#48537,.T.);
#68209=ORIENTED_EDGE('',*,*,#48539,.T.);
#68210=ORIENTED_EDGE('',*,*,#48541,.T.);
#68211=ORIENTED_EDGE('',*,*,#48506,.T.);
#68212=ORIENTED_EDGE('',*,*,#48455,.F.);
#68213=ORIENTED_EDGE('',*,*,#48661,.T.);
#68214=ORIENTED_EDGE('',*,*,#48659,.F.);
#68215=ORIENTED_EDGE('',*,*,#48662,.F.);
#68216=ORIENTED_EDGE('',*,*,#48454,.F.);
#68217=ORIENTED_EDGE('',*,*,#48509,.T.);
#68218=ORIENTED_EDGE('',*,*,#48660,.F.);
#68219=ORIENTED_EDGE('',*,*,#48661,.F.);
#68220=ORIENTED_EDGE('',*,*,#48456,.F.);
#68221=ORIENTED_EDGE('',*,*,#48662,.T.);
#68222=ORIENTED_EDGE('',*,*,#48658,.F.);
#68223=ORIENTED_EDGE('',*,*,#48663,.T.);
#68224=ORIENTED_EDGE('',*,*,#48457,.F.);
#68225=ORIENTED_EDGE('',*,*,#48663,.F.);
#68226=ORIENTED_EDGE('',*,*,#48657,.F.);
#68227=ORIENTED_EDGE('',*,*,#48664,.F.);
#68228=ORIENTED_EDGE('',*,*,#48458,.F.);
#68229=ORIENTED_EDGE('',*,*,#48664,.T.);
#68230=ORIENTED_EDGE('',*,*,#48656,.F.);
#68231=ORIENTED_EDGE('',*,*,#48665,.F.);
#68232=ORIENTED_EDGE('',*,*,#48459,.F.);
#68233=ORIENTED_EDGE('',*,*,#48665,.T.);
#68234=ORIENTED_EDGE('',*,*,#48655,.F.);
#68235=ORIENTED_EDGE('',*,*,#48666,.F.);
#68236=ORIENTED_EDGE('',*,*,#48460,.F.);
#68237=ORIENTED_EDGE('',*,*,#48666,.T.);
#68238=ORIENTED_EDGE('',*,*,#48654,.F.);
#68239=ORIENTED_EDGE('',*,*,#48667,.F.);
#68240=ORIENTED_EDGE('',*,*,#48461,.F.);
#68241=ORIENTED_EDGE('',*,*,#48667,.T.);
#68242=ORIENTED_EDGE('',*,*,#48653,.F.);
#68243=ORIENTED_EDGE('',*,*,#48668,.F.);
#68244=ORIENTED_EDGE('',*,*,#48462,.F.);
#68245=ORIENTED_EDGE('',*,*,#48668,.T.);
#68246=ORIENTED_EDGE('',*,*,#48652,.F.);
#68247=ORIENTED_EDGE('',*,*,#48669,.T.);
#68248=ORIENTED_EDGE('',*,*,#48467,.F.);
#68249=ORIENTED_EDGE('',*,*,#48670,.T.);
#68250=ORIENTED_EDGE('',*,*,#48647,.F.);
#68251=ORIENTED_EDGE('',*,*,#48671,.F.);
#68252=ORIENTED_EDGE('',*,*,#48463,.F.);
#68253=ORIENTED_EDGE('',*,*,#48669,.F.);
#68254=ORIENTED_EDGE('',*,*,#48651,.F.);
#68255=ORIENTED_EDGE('',*,*,#48672,.F.);
#68256=ORIENTED_EDGE('',*,*,#48464,.F.);
#68257=ORIENTED_EDGE('',*,*,#48672,.T.);
#68258=ORIENTED_EDGE('',*,*,#48650,.F.);
#68259=ORIENTED_EDGE('',*,*,#48673,.F.);
#68260=ORIENTED_EDGE('',*,*,#48465,.F.);
#68261=ORIENTED_EDGE('',*,*,#48673,.T.);
#68262=ORIENTED_EDGE('',*,*,#48649,.F.);
#68263=ORIENTED_EDGE('',*,*,#48674,.F.);
#68264=ORIENTED_EDGE('',*,*,#48466,.F.);
#68265=ORIENTED_EDGE('',*,*,#48674,.T.);
#68266=ORIENTED_EDGE('',*,*,#48648,.F.);
#68267=ORIENTED_EDGE('',*,*,#48670,.F.);
#68268=ORIENTED_EDGE('',*,*,#48469,.F.);
#68269=ORIENTED_EDGE('',*,*,#48675,.F.);
#68270=ORIENTED_EDGE('',*,*,#48645,.F.);
#68271=ORIENTED_EDGE('',*,*,#48676,.F.);
#68272=ORIENTED_EDGE('',*,*,#48473,.F.);
#68273=ORIENTED_EDGE('',*,*,#48677,.T.);
#68274=ORIENTED_EDGE('',*,*,#48641,.F.);
#68275=ORIENTED_EDGE('',*,*,#48678,.F.);
#68276=ORIENTED_EDGE('',*,*,#48470,.F.);
#68277=ORIENTED_EDGE('',*,*,#48676,.T.);
#68278=ORIENTED_EDGE('',*,*,#48644,.F.);
#68279=ORIENTED_EDGE('',*,*,#48679,.F.);
#68280=ORIENTED_EDGE('',*,*,#48471,.F.);
#68281=ORIENTED_EDGE('',*,*,#48679,.T.);
#68282=ORIENTED_EDGE('',*,*,#48643,.F.);
#68283=ORIENTED_EDGE('',*,*,#48680,.F.);
#68284=ORIENTED_EDGE('',*,*,#48472,.F.);
#68285=ORIENTED_EDGE('',*,*,#48680,.T.);
#68286=ORIENTED_EDGE('',*,*,#48642,.F.);
#68287=ORIENTED_EDGE('',*,*,#48677,.F.);
#68288=ORIENTED_EDGE('',*,*,#48474,.F.);
#68289=ORIENTED_EDGE('',*,*,#48678,.T.);
#68290=ORIENTED_EDGE('',*,*,#48640,.F.);
#68291=ORIENTED_EDGE('',*,*,#48681,.T.);
#68292=ORIENTED_EDGE('',*,*,#48475,.F.);
#68293=ORIENTED_EDGE('',*,*,#48681,.F.);
#68294=ORIENTED_EDGE('',*,*,#48639,.F.);
#68295=ORIENTED_EDGE('',*,*,#48682,.F.);
#68296=ORIENTED_EDGE('',*,*,#48476,.F.);
#68297=ORIENTED_EDGE('',*,*,#48682,.T.);
#68298=ORIENTED_EDGE('',*,*,#48638,.F.);
#68299=ORIENTED_EDGE('',*,*,#48683,.F.);
#68300=ORIENTED_EDGE('',*,*,#48477,.F.);
#68301=ORIENTED_EDGE('',*,*,#48683,.T.);
#68302=ORIENTED_EDGE('',*,*,#48637,.F.);
#68303=ORIENTED_EDGE('',*,*,#48684,.F.);
#68304=ORIENTED_EDGE('',*,*,#48478,.F.);
#68305=ORIENTED_EDGE('',*,*,#48684,.T.);
#68306=ORIENTED_EDGE('',*,*,#48636,.F.);
#68307=ORIENTED_EDGE('',*,*,#48685,.F.);
#68308=ORIENTED_EDGE('',*,*,#48479,.F.);
#68309=ORIENTED_EDGE('',*,*,#48685,.T.);
#68310=ORIENTED_EDGE('',*,*,#48635,.F.);
#68311=ORIENTED_EDGE('',*,*,#48686,.F.);
#68312=ORIENTED_EDGE('',*,*,#48468,.F.);
#68313=ORIENTED_EDGE('',*,*,#48671,.T.);
#68314=ORIENTED_EDGE('',*,*,#48646,.F.);
#68315=ORIENTED_EDGE('',*,*,#48675,.T.);
#68316=ORIENTED_EDGE('',*,*,#48480,.F.);
#68317=ORIENTED_EDGE('',*,*,#48686,.T.);
#68318=ORIENTED_EDGE('',*,*,#48634,.F.);
#68319=ORIENTED_EDGE('',*,*,#48687,.T.);
#68320=ORIENTED_EDGE('',*,*,#48485,.F.);
#68321=ORIENTED_EDGE('',*,*,#48688,.T.);
#68322=ORIENTED_EDGE('',*,*,#48629,.F.);
#68323=ORIENTED_EDGE('',*,*,#48689,.F.);
#68324=ORIENTED_EDGE('',*,*,#48481,.F.);
#68325=ORIENTED_EDGE('',*,*,#48687,.F.);
#68326=ORIENTED_EDGE('',*,*,#48633,.F.);
#68327=ORIENTED_EDGE('',*,*,#48690,.F.);
#68328=ORIENTED_EDGE('',*,*,#48482,.F.);
#68329=ORIENTED_EDGE('',*,*,#48690,.T.);
#68330=ORIENTED_EDGE('',*,*,#48632,.F.);
#68331=ORIENTED_EDGE('',*,*,#48691,.F.);
#68332=ORIENTED_EDGE('',*,*,#48483,.F.);
#68333=ORIENTED_EDGE('',*,*,#48691,.T.);
#68334=ORIENTED_EDGE('',*,*,#48631,.F.);
#68335=ORIENTED_EDGE('',*,*,#48692,.F.);
#68336=ORIENTED_EDGE('',*,*,#48484,.F.);
#68337=ORIENTED_EDGE('',*,*,#48692,.T.);
#68338=ORIENTED_EDGE('',*,*,#48630,.F.);
#68339=ORIENTED_EDGE('',*,*,#48688,.F.);
#68340=ORIENTED_EDGE('',*,*,#48487,.F.);
#68341=ORIENTED_EDGE('',*,*,#48693,.F.);
#68342=ORIENTED_EDGE('',*,*,#48627,.F.);
#68343=ORIENTED_EDGE('',*,*,#48694,.F.);
#68344=ORIENTED_EDGE('',*,*,#48491,.F.);
#68345=ORIENTED_EDGE('',*,*,#48695,.T.);
#68346=ORIENTED_EDGE('',*,*,#48623,.F.);
#68347=ORIENTED_EDGE('',*,*,#48696,.F.);
#68348=ORIENTED_EDGE('',*,*,#48488,.F.);
#68349=ORIENTED_EDGE('',*,*,#48694,.T.);
#68350=ORIENTED_EDGE('',*,*,#48626,.F.);
#68351=ORIENTED_EDGE('',*,*,#48697,.F.);
#68352=ORIENTED_EDGE('',*,*,#48489,.F.);
#68353=ORIENTED_EDGE('',*,*,#48697,.T.);
#68354=ORIENTED_EDGE('',*,*,#48625,.F.);
#68355=ORIENTED_EDGE('',*,*,#48698,.F.);
#68356=ORIENTED_EDGE('',*,*,#48490,.F.);
#68357=ORIENTED_EDGE('',*,*,#48698,.T.);
#68358=ORIENTED_EDGE('',*,*,#48624,.F.);
#68359=ORIENTED_EDGE('',*,*,#48695,.F.);
#68360=ORIENTED_EDGE('',*,*,#48492,.F.);
#68361=ORIENTED_EDGE('',*,*,#48696,.T.);
#68362=ORIENTED_EDGE('',*,*,#48622,.F.);
#68363=ORIENTED_EDGE('',*,*,#48699,.T.);
#68364=ORIENTED_EDGE('',*,*,#48493,.F.);
#68365=ORIENTED_EDGE('',*,*,#48699,.F.);
#68366=ORIENTED_EDGE('',*,*,#48621,.F.);
#68367=ORIENTED_EDGE('',*,*,#48700,.F.);
#68368=ORIENTED_EDGE('',*,*,#48494,.F.);
#68369=ORIENTED_EDGE('',*,*,#48700,.T.);
#68370=ORIENTED_EDGE('',*,*,#48620,.F.);
#68371=ORIENTED_EDGE('',*,*,#48701,.F.);
#68372=ORIENTED_EDGE('',*,*,#48495,.F.);
#68373=ORIENTED_EDGE('',*,*,#48701,.T.);
#68374=ORIENTED_EDGE('',*,*,#48619,.F.);
#68375=ORIENTED_EDGE('',*,*,#48702,.F.);
#68376=ORIENTED_EDGE('',*,*,#48496,.F.);
#68377=ORIENTED_EDGE('',*,*,#48702,.T.);
#68378=ORIENTED_EDGE('',*,*,#48618,.F.);
#68379=ORIENTED_EDGE('',*,*,#48703,.F.);
#68380=ORIENTED_EDGE('',*,*,#48497,.F.);
#68381=ORIENTED_EDGE('',*,*,#48703,.T.);
#68382=ORIENTED_EDGE('',*,*,#48617,.F.);
#68383=ORIENTED_EDGE('',*,*,#48704,.F.);
#68384=ORIENTED_EDGE('',*,*,#48486,.F.);
#68385=ORIENTED_EDGE('',*,*,#48689,.T.);
#68386=ORIENTED_EDGE('',*,*,#48628,.F.);
#68387=ORIENTED_EDGE('',*,*,#48693,.T.);
#68388=ORIENTED_EDGE('',*,*,#48498,.F.);
#68389=ORIENTED_EDGE('',*,*,#48704,.T.);
#68390=ORIENTED_EDGE('',*,*,#48616,.F.);
#68391=ORIENTED_EDGE('',*,*,#48705,.T.);
#68392=ORIENTED_EDGE('',*,*,#48401,.F.);
#68393=ORIENTED_EDGE('',*,*,#48706,.T.);
#68394=ORIENTED_EDGE('',*,*,#48611,.F.);
#68395=ORIENTED_EDGE('',*,*,#48707,.F.);
#68396=ORIENTED_EDGE('',*,*,#48499,.F.);
#68397=ORIENTED_EDGE('',*,*,#48705,.F.);
#68398=ORIENTED_EDGE('',*,*,#48615,.F.);
#68399=ORIENTED_EDGE('',*,*,#48708,.F.);
#68400=ORIENTED_EDGE('',*,*,#48500,.F.);
#68401=ORIENTED_EDGE('',*,*,#48708,.T.);
#68402=ORIENTED_EDGE('',*,*,#48614,.F.);
#68403=ORIENTED_EDGE('',*,*,#48709,.F.);
#68404=ORIENTED_EDGE('',*,*,#48501,.F.);
#68405=ORIENTED_EDGE('',*,*,#48709,.T.);
#68406=ORIENTED_EDGE('',*,*,#48613,.F.);
#68407=ORIENTED_EDGE('',*,*,#48710,.F.);
#68408=ORIENTED_EDGE('',*,*,#48502,.F.);
#68409=ORIENTED_EDGE('',*,*,#48710,.T.);
#68410=ORIENTED_EDGE('',*,*,#48612,.F.);
#68411=ORIENTED_EDGE('',*,*,#48706,.F.);
#68412=ORIENTED_EDGE('',*,*,#48402,.F.);
#68413=ORIENTED_EDGE('',*,*,#48707,.T.);
#68414=ORIENTED_EDGE('',*,*,#48610,.F.);
#68415=ORIENTED_EDGE('',*,*,#48608,.T.);
#68416=ORIENTED_EDGE('',*,*,#48503,.F.);
#68417=ORIENTED_EDGE('',*,*,#48711,.T.);
#68418=ORIENTED_EDGE('',*,*,#48712,.F.);
#68419=ORIENTED_EDGE('',*,*,#48711,.F.);
#68420=ORIENTED_EDGE('',*,*,#48712,.T.);
#68421=ORIENTED_EDGE('',*,*,#48397,.T.);
#68422=ORIENTED_EDGE('',*,*,#48713,.T.);
#68423=ORIENTED_EDGE('',*,*,#48714,.T.);
#68424=ORIENTED_EDGE('',*,*,#48715,.T.);
#68425=ORIENTED_EDGE('',*,*,#48714,.F.);
#68426=ORIENTED_EDGE('',*,*,#48716,.F.);
#68427=ORIENTED_EDGE('',*,*,#48713,.F.);
#68428=ORIENTED_EDGE('',*,*,#48715,.F.);
#68429=ORIENTED_EDGE('',*,*,#48717,.T.);
#68430=ORIENTED_EDGE('',*,*,#48718,.T.);
#68431=ORIENTED_EDGE('',*,*,#48719,.T.);
#68432=ORIENTED_EDGE('',*,*,#48720,.T.);
#68433=ORIENTED_EDGE('',*,*,#48721,.T.);
#68434=ORIENTED_EDGE('',*,*,#48722,.F.);
#68435=ORIENTED_EDGE('',*,*,#48723,.F.);
#68436=ORIENTED_EDGE('',*,*,#48721,.F.);
#68437=ORIENTED_EDGE('',*,*,#48724,.T.);
#68438=ORIENTED_EDGE('',*,*,#48725,.T.);
#68439=ORIENTED_EDGE('',*,*,#48726,.T.);
#68440=ORIENTED_EDGE('',*,*,#48717,.F.);
#68441=ORIENTED_EDGE('',*,*,#48727,.T.);
#68442=ORIENTED_EDGE('',*,*,#48728,.T.);
#68443=ORIENTED_EDGE('',*,*,#48729,.T.);
#68444=ORIENTED_EDGE('',*,*,#48730,.T.);
#68445=ORIENTED_EDGE('',*,*,#48731,.T.);
#68446=ORIENTED_EDGE('',*,*,#48732,.T.);
#68447=ORIENTED_EDGE('',*,*,#48733,.T.);
#68448=ORIENTED_EDGE('',*,*,#48734,.T.);
#68449=ORIENTED_EDGE('',*,*,#48735,.T.);
#68450=ORIENTED_EDGE('',*,*,#48736,.T.);
#68451=ORIENTED_EDGE('',*,*,#48737,.T.);
#68452=ORIENTED_EDGE('',*,*,#48738,.T.);
#68453=ORIENTED_EDGE('',*,*,#48739,.T.);
#68454=ORIENTED_EDGE('',*,*,#48740,.T.);
#68455=ORIENTED_EDGE('',*,*,#48741,.T.);
#68456=ORIENTED_EDGE('',*,*,#48742,.T.);
#68457=ORIENTED_EDGE('',*,*,#48743,.T.);
#68458=ORIENTED_EDGE('',*,*,#48744,.T.);
#68459=ORIENTED_EDGE('',*,*,#48745,.T.);
#68460=ORIENTED_EDGE('',*,*,#48746,.T.);
#68461=ORIENTED_EDGE('',*,*,#48747,.T.);
#68462=ORIENTED_EDGE('',*,*,#48748,.T.);
#68463=ORIENTED_EDGE('',*,*,#48749,.T.);
#68464=ORIENTED_EDGE('',*,*,#48750,.T.);
#68465=ORIENTED_EDGE('',*,*,#48751,.T.);
#68466=ORIENTED_EDGE('',*,*,#48752,.T.);
#68467=ORIENTED_EDGE('',*,*,#48753,.T.);
#68468=ORIENTED_EDGE('',*,*,#48754,.T.);
#68469=ORIENTED_EDGE('',*,*,#48716,.T.);
#68470=ORIENTED_EDGE('',*,*,#48755,.T.);
#68471=ORIENTED_EDGE('',*,*,#48756,.T.);
#68472=ORIENTED_EDGE('',*,*,#48757,.T.);
#68473=ORIENTED_EDGE('',*,*,#48755,.F.);
#68474=ORIENTED_EDGE('',*,*,#48758,.F.);
#68475=ORIENTED_EDGE('',*,*,#48759,.T.);
#68476=ORIENTED_EDGE('',*,*,#48760,.T.);
#68477=ORIENTED_EDGE('',*,*,#48761,.T.);
#68478=ORIENTED_EDGE('',*,*,#48762,.T.);
#68479=ORIENTED_EDGE('',*,*,#48763,.T.);
#68480=ORIENTED_EDGE('',*,*,#48756,.F.);
#68481=ORIENTED_EDGE('',*,*,#48757,.F.);
#68482=ORIENTED_EDGE('',*,*,#48763,.F.);
#68483=ORIENTED_EDGE('',*,*,#48764,.T.);
#68484=ORIENTED_EDGE('',*,*,#48765,.T.);
#68485=ORIENTED_EDGE('',*,*,#48766,.T.);
#68486=ORIENTED_EDGE('',*,*,#48759,.F.);
#68487=ORIENTED_EDGE('',*,*,#48767,.T.);
#68488=ORIENTED_EDGE('',*,*,#48768,.T.);
#68489=ORIENTED_EDGE('',*,*,#48769,.T.);
#68490=ORIENTED_EDGE('',*,*,#48770,.T.);
#68491=ORIENTED_EDGE('',*,*,#48771,.T.);
#68492=ORIENTED_EDGE('',*,*,#48772,.T.);
#68493=ORIENTED_EDGE('',*,*,#48773,.T.);
#68494=ORIENTED_EDGE('',*,*,#48774,.T.);
#68495=ORIENTED_EDGE('',*,*,#48775,.T.);
#68496=ORIENTED_EDGE('',*,*,#48776,.T.);
#68497=ORIENTED_EDGE('',*,*,#48777,.T.);
#68498=ORIENTED_EDGE('',*,*,#48778,.T.);
#68499=ORIENTED_EDGE('',*,*,#48779,.T.);
#68500=ORIENTED_EDGE('',*,*,#48780,.T.);
#68501=ORIENTED_EDGE('',*,*,#48781,.T.);
#68502=ORIENTED_EDGE('',*,*,#48782,.T.);
#68503=ORIENTED_EDGE('',*,*,#48783,.T.);
#68504=ORIENTED_EDGE('',*,*,#48784,.T.);
#68505=ORIENTED_EDGE('',*,*,#48785,.T.);
#68506=ORIENTED_EDGE('',*,*,#48786,.T.);
#68507=ORIENTED_EDGE('',*,*,#48787,.T.);
#68508=ORIENTED_EDGE('',*,*,#48788,.T.);
#68509=ORIENTED_EDGE('',*,*,#48789,.T.);
#68510=ORIENTED_EDGE('',*,*,#48790,.T.);
#68511=ORIENTED_EDGE('',*,*,#48791,.T.);
#68512=ORIENTED_EDGE('',*,*,#48792,.T.);
#68513=ORIENTED_EDGE('',*,*,#48793,.T.);
#68514=ORIENTED_EDGE('',*,*,#48794,.T.);
#68515=ORIENTED_EDGE('',*,*,#48795,.T.);
#68516=ORIENTED_EDGE('',*,*,#48796,.T.);
#68517=ORIENTED_EDGE('',*,*,#48758,.T.);
#68518=ORIENTED_EDGE('',*,*,#48796,.F.);
#68519=ORIENTED_EDGE('',*,*,#48795,.F.);
#68520=ORIENTED_EDGE('',*,*,#48797,.F.);
#68521=ORIENTED_EDGE('',*,*,#48797,.T.);
#68522=ORIENTED_EDGE('',*,*,#48798,.T.);
#68523=ORIENTED_EDGE('',*,*,#48722,.T.);
#68524=ORIENTED_EDGE('',*,*,#48723,.T.);
#68525=ORIENTED_EDGE('',*,*,#48798,.F.);
#68526=ORIENTED_EDGE('',*,*,#48729,.F.);
#68527=ORIENTED_EDGE('',*,*,#48799,.F.);
#68528=ORIENTED_EDGE('',*,*,#48769,.F.);
#68529=ORIENTED_EDGE('',*,*,#48800,.F.);
#68530=ORIENTED_EDGE('',*,*,#48730,.F.);
#68531=ORIENTED_EDGE('',*,*,#48800,.T.);
#68532=ORIENTED_EDGE('',*,*,#48768,.F.);
#68533=ORIENTED_EDGE('',*,*,#48801,.T.);
#68534=ORIENTED_EDGE('',*,*,#48727,.F.);
#68535=ORIENTED_EDGE('',*,*,#48801,.F.);
#68536=ORIENTED_EDGE('',*,*,#48767,.F.);
#68537=ORIENTED_EDGE('',*,*,#48802,.F.);
#68538=ORIENTED_EDGE('',*,*,#48728,.F.);
#68539=ORIENTED_EDGE('',*,*,#48802,.T.);
#68540=ORIENTED_EDGE('',*,*,#48770,.F.);
#68541=ORIENTED_EDGE('',*,*,#48799,.T.);
#68542=ORIENTED_EDGE('',*,*,#48733,.F.);
#68543=ORIENTED_EDGE('',*,*,#48803,.F.);
#68544=ORIENTED_EDGE('',*,*,#48773,.F.);
#68545=ORIENTED_EDGE('',*,*,#48804,.F.);
#68546=ORIENTED_EDGE('',*,*,#48734,.F.);
#68547=ORIENTED_EDGE('',*,*,#48804,.T.);
#68548=ORIENTED_EDGE('',*,*,#48772,.F.);
#68549=ORIENTED_EDGE('',*,*,#48805,.T.);
#68550=ORIENTED_EDGE('',*,*,#48731,.F.);
#68551=ORIENTED_EDGE('',*,*,#48805,.F.);
#68552=ORIENTED_EDGE('',*,*,#48771,.F.);
#68553=ORIENTED_EDGE('',*,*,#48806,.F.);
#68554=ORIENTED_EDGE('',*,*,#48732,.F.);
#68555=ORIENTED_EDGE('',*,*,#48806,.T.);
#68556=ORIENTED_EDGE('',*,*,#48774,.F.);
#68557=ORIENTED_EDGE('',*,*,#48803,.T.);
#68558=ORIENTED_EDGE('',*,*,#48737,.F.);
#68559=ORIENTED_EDGE('',*,*,#48807,.F.);
#68560=ORIENTED_EDGE('',*,*,#48777,.F.);
#68561=ORIENTED_EDGE('',*,*,#48808,.F.);
#68562=ORIENTED_EDGE('',*,*,#48738,.F.);
#68563=ORIENTED_EDGE('',*,*,#48808,.T.);
#68564=ORIENTED_EDGE('',*,*,#48776,.F.);
#68565=ORIENTED_EDGE('',*,*,#48809,.T.);
#68566=ORIENTED_EDGE('',*,*,#48735,.F.);
#68567=ORIENTED_EDGE('',*,*,#48809,.F.);
#68568=ORIENTED_EDGE('',*,*,#48775,.F.);
#68569=ORIENTED_EDGE('',*,*,#48810,.F.);
#68570=ORIENTED_EDGE('',*,*,#48736,.F.);
#68571=ORIENTED_EDGE('',*,*,#48810,.T.);
#68572=ORIENTED_EDGE('',*,*,#48778,.F.);
#68573=ORIENTED_EDGE('',*,*,#48807,.T.);
#68574=ORIENTED_EDGE('',*,*,#48720,.F.);
#68575=ORIENTED_EDGE('',*,*,#48811,.F.);
#68576=ORIENTED_EDGE('',*,*,#48760,.F.);
#68577=ORIENTED_EDGE('',*,*,#48766,.F.);
#68578=ORIENTED_EDGE('',*,*,#48812,.F.);
#68579=ORIENTED_EDGE('',*,*,#48724,.F.);
#68580=ORIENTED_EDGE('',*,*,#48725,.F.);
#68581=ORIENTED_EDGE('',*,*,#48812,.T.);
#68582=ORIENTED_EDGE('',*,*,#48765,.F.);
#68583=ORIENTED_EDGE('',*,*,#48813,.T.);
#68584=ORIENTED_EDGE('',*,*,#48726,.F.);
#68585=ORIENTED_EDGE('',*,*,#48813,.F.);
#68586=ORIENTED_EDGE('',*,*,#48764,.F.);
#68587=ORIENTED_EDGE('',*,*,#48762,.F.);
#68588=ORIENTED_EDGE('',*,*,#48814,.F.);
#68589=ORIENTED_EDGE('',*,*,#48718,.F.);
#68590=ORIENTED_EDGE('',*,*,#48719,.F.);
#68591=ORIENTED_EDGE('',*,*,#48814,.T.);
#68592=ORIENTED_EDGE('',*,*,#48761,.F.);
#68593=ORIENTED_EDGE('',*,*,#48811,.T.);
#68594=ORIENTED_EDGE('',*,*,#48741,.F.);
#68595=ORIENTED_EDGE('',*,*,#48815,.F.);
#68596=ORIENTED_EDGE('',*,*,#48781,.F.);
#68597=ORIENTED_EDGE('',*,*,#48816,.F.);
#68598=ORIENTED_EDGE('',*,*,#48742,.F.);
#68599=ORIENTED_EDGE('',*,*,#48816,.T.);
#68600=ORIENTED_EDGE('',*,*,#48780,.F.);
#68601=ORIENTED_EDGE('',*,*,#48817,.T.);
#68602=ORIENTED_EDGE('',*,*,#48739,.F.);
#68603=ORIENTED_EDGE('',*,*,#48817,.F.);
#68604=ORIENTED_EDGE('',*,*,#48779,.F.);
#68605=ORIENTED_EDGE('',*,*,#48818,.F.);
#68606=ORIENTED_EDGE('',*,*,#48740,.F.);
#68607=ORIENTED_EDGE('',*,*,#48818,.T.);
#68608=ORIENTED_EDGE('',*,*,#48782,.F.);
#68609=ORIENTED_EDGE('',*,*,#48815,.T.);
#68610=ORIENTED_EDGE('',*,*,#48745,.F.);
#68611=ORIENTED_EDGE('',*,*,#48819,.F.);
#68612=ORIENTED_EDGE('',*,*,#48785,.F.);
#68613=ORIENTED_EDGE('',*,*,#48820,.F.);
#68614=ORIENTED_EDGE('',*,*,#48746,.F.);
#68615=ORIENTED_EDGE('',*,*,#48820,.T.);
#68616=ORIENTED_EDGE('',*,*,#48784,.F.);
#68617=ORIENTED_EDGE('',*,*,#48821,.T.);
#68618=ORIENTED_EDGE('',*,*,#48743,.F.);
#68619=ORIENTED_EDGE('',*,*,#48821,.F.);
#68620=ORIENTED_EDGE('',*,*,#48783,.F.);
#68621=ORIENTED_EDGE('',*,*,#48822,.F.);
#68622=ORIENTED_EDGE('',*,*,#48744,.F.);
#68623=ORIENTED_EDGE('',*,*,#48822,.T.);
#68624=ORIENTED_EDGE('',*,*,#48786,.F.);
#68625=ORIENTED_EDGE('',*,*,#48819,.T.);
#68626=ORIENTED_EDGE('',*,*,#48749,.F.);
#68627=ORIENTED_EDGE('',*,*,#48823,.F.);
#68628=ORIENTED_EDGE('',*,*,#48789,.F.);
#68629=ORIENTED_EDGE('',*,*,#48824,.F.);
#68630=ORIENTED_EDGE('',*,*,#48750,.F.);
#68631=ORIENTED_EDGE('',*,*,#48824,.T.);
#68632=ORIENTED_EDGE('',*,*,#48788,.F.);
#68633=ORIENTED_EDGE('',*,*,#48825,.T.);
#68634=ORIENTED_EDGE('',*,*,#48747,.F.);
#68635=ORIENTED_EDGE('',*,*,#48825,.F.);
#68636=ORIENTED_EDGE('',*,*,#48787,.F.);
#68637=ORIENTED_EDGE('',*,*,#48826,.F.);
#68638=ORIENTED_EDGE('',*,*,#48748,.F.);
#68639=ORIENTED_EDGE('',*,*,#48826,.T.);
#68640=ORIENTED_EDGE('',*,*,#48790,.F.);
#68641=ORIENTED_EDGE('',*,*,#48823,.T.);
#68642=ORIENTED_EDGE('',*,*,#48753,.F.);
#68643=ORIENTED_EDGE('',*,*,#48827,.F.);
#68644=ORIENTED_EDGE('',*,*,#48793,.F.);
#68645=ORIENTED_EDGE('',*,*,#48828,.F.);
#68646=ORIENTED_EDGE('',*,*,#48754,.F.);
#68647=ORIENTED_EDGE('',*,*,#48828,.T.);
#68648=ORIENTED_EDGE('',*,*,#48792,.F.);
#68649=ORIENTED_EDGE('',*,*,#48829,.T.);
#68650=ORIENTED_EDGE('',*,*,#48751,.F.);
#68651=ORIENTED_EDGE('',*,*,#48829,.F.);
#68652=ORIENTED_EDGE('',*,*,#48791,.F.);
#68653=ORIENTED_EDGE('',*,*,#48830,.F.);
#68654=ORIENTED_EDGE('',*,*,#48752,.F.);
#68655=ORIENTED_EDGE('',*,*,#48830,.T.);
#68656=ORIENTED_EDGE('',*,*,#48794,.F.);
#68657=ORIENTED_EDGE('',*,*,#48827,.T.);
#68658=ORIENTED_EDGE('',*,*,#48831,.T.);
#68659=ORIENTED_EDGE('',*,*,#48832,.T.);
#68660=ORIENTED_EDGE('',*,*,#48833,.T.);
#68661=ORIENTED_EDGE('',*,*,#48832,.F.);
#68662=ORIENTED_EDGE('',*,*,#48834,.F.);
#68663=ORIENTED_EDGE('',*,*,#48835,.T.);
#68664=ORIENTED_EDGE('',*,*,#48831,.F.);
#68665=ORIENTED_EDGE('',*,*,#48835,.F.);
#68666=ORIENTED_EDGE('',*,*,#48833,.F.);
#68667=ORIENTED_EDGE('',*,*,#48834,.T.);
#68668=ORIENTED_EDGE('',*,*,#48836,.T.);
#68669=ORIENTED_EDGE('',*,*,#48837,.T.);
#68670=ORIENTED_EDGE('',*,*,#48836,.F.);
#68671=ORIENTED_EDGE('',*,*,#48837,.F.);
#68672=ORIENTED_EDGE('',*,*,#48838,.T.);
#68673=ORIENTED_EDGE('',*,*,#48839,.T.);
#68674=ORIENTED_EDGE('',*,*,#48840,.T.);
#68675=ORIENTED_EDGE('',*,*,#48839,.F.);
#68676=ORIENTED_EDGE('',*,*,#48841,.F.);
#68677=ORIENTED_EDGE('',*,*,#48842,.T.);
#68678=ORIENTED_EDGE('',*,*,#48838,.F.);
#68679=ORIENTED_EDGE('',*,*,#48842,.F.);
#68680=ORIENTED_EDGE('',*,*,#48840,.F.);
#68681=ORIENTED_EDGE('',*,*,#48841,.T.);
#68682=ORIENTED_EDGE('',*,*,#48843,.T.);
#68683=ORIENTED_EDGE('',*,*,#48844,.T.);
#68684=ORIENTED_EDGE('',*,*,#48843,.F.);
#68685=ORIENTED_EDGE('',*,*,#48844,.F.);
#68686=ORIENTED_EDGE('',*,*,#48845,.T.);
#68687=ORIENTED_EDGE('',*,*,#48846,.T.);
#68688=ORIENTED_EDGE('',*,*,#48847,.T.);
#68689=ORIENTED_EDGE('',*,*,#48846,.F.);
#68690=ORIENTED_EDGE('',*,*,#48848,.F.);
#68691=ORIENTED_EDGE('',*,*,#48849,.T.);
#68692=ORIENTED_EDGE('',*,*,#48845,.F.);
#68693=ORIENTED_EDGE('',*,*,#48849,.F.);
#68694=ORIENTED_EDGE('',*,*,#48847,.F.);
#68695=ORIENTED_EDGE('',*,*,#48848,.T.);
#68696=ORIENTED_EDGE('',*,*,#48850,.T.);
#68697=ORIENTED_EDGE('',*,*,#48851,.T.);
#68698=ORIENTED_EDGE('',*,*,#48850,.F.);
#68699=ORIENTED_EDGE('',*,*,#48851,.F.);
#68700=ORIENTED_EDGE('',*,*,#48852,.T.);
#68701=ORIENTED_EDGE('',*,*,#48853,.T.);
#68702=ORIENTED_EDGE('',*,*,#48854,.T.);
#68703=ORIENTED_EDGE('',*,*,#48853,.F.);
#68704=ORIENTED_EDGE('',*,*,#48855,.F.);
#68705=ORIENTED_EDGE('',*,*,#48856,.T.);
#68706=ORIENTED_EDGE('',*,*,#48852,.F.);
#68707=ORIENTED_EDGE('',*,*,#48856,.F.);
#68708=ORIENTED_EDGE('',*,*,#48854,.F.);
#68709=ORIENTED_EDGE('',*,*,#48855,.T.);
#68710=ORIENTED_EDGE('',*,*,#48857,.T.);
#68711=ORIENTED_EDGE('',*,*,#48858,.T.);
#68712=ORIENTED_EDGE('',*,*,#48857,.F.);
#68713=ORIENTED_EDGE('',*,*,#48858,.F.);
#68714=ORIENTED_EDGE('',*,*,#48859,.T.);
#68715=ORIENTED_EDGE('',*,*,#48860,.T.);
#68716=ORIENTED_EDGE('',*,*,#48861,.T.);
#68717=ORIENTED_EDGE('',*,*,#48860,.F.);
#68718=ORIENTED_EDGE('',*,*,#48862,.F.);
#68719=ORIENTED_EDGE('',*,*,#48863,.T.);
#68720=ORIENTED_EDGE('',*,*,#48859,.F.);
#68721=ORIENTED_EDGE('',*,*,#48863,.F.);
#68722=ORIENTED_EDGE('',*,*,#48861,.F.);
#68723=ORIENTED_EDGE('',*,*,#48862,.T.);
#68724=ORIENTED_EDGE('',*,*,#48864,.T.);
#68725=ORIENTED_EDGE('',*,*,#48865,.T.);
#68726=ORIENTED_EDGE('',*,*,#48864,.F.);
#68727=ORIENTED_EDGE('',*,*,#48865,.F.);
#68728=ORIENTED_EDGE('',*,*,#48866,.T.);
#68729=ORIENTED_EDGE('',*,*,#48867,.T.);
#68730=ORIENTED_EDGE('',*,*,#48868,.T.);
#68731=ORIENTED_EDGE('',*,*,#48867,.F.);
#68732=ORIENTED_EDGE('',*,*,#48869,.F.);
#68733=ORIENTED_EDGE('',*,*,#48870,.T.);
#68734=ORIENTED_EDGE('',*,*,#48866,.F.);
#68735=ORIENTED_EDGE('',*,*,#48870,.F.);
#68736=ORIENTED_EDGE('',*,*,#48868,.F.);
#68737=ORIENTED_EDGE('',*,*,#48869,.T.);
#68738=ORIENTED_EDGE('',*,*,#48871,.T.);
#68739=ORIENTED_EDGE('',*,*,#48872,.T.);
#68740=ORIENTED_EDGE('',*,*,#48871,.F.);
#68741=ORIENTED_EDGE('',*,*,#48872,.F.);
#68742=ORIENTED_EDGE('',*,*,#48873,.T.);
#68743=ORIENTED_EDGE('',*,*,#48874,.T.);
#68744=ORIENTED_EDGE('',*,*,#48875,.T.);
#68745=ORIENTED_EDGE('',*,*,#48874,.F.);
#68746=ORIENTED_EDGE('',*,*,#48876,.F.);
#68747=ORIENTED_EDGE('',*,*,#48877,.T.);
#68748=ORIENTED_EDGE('',*,*,#48873,.F.);
#68749=ORIENTED_EDGE('',*,*,#48877,.F.);
#68750=ORIENTED_EDGE('',*,*,#48875,.F.);
#68751=ORIENTED_EDGE('',*,*,#48876,.T.);
#68752=ORIENTED_EDGE('',*,*,#48878,.T.);
#68753=ORIENTED_EDGE('',*,*,#48879,.T.);
#68754=ORIENTED_EDGE('',*,*,#48878,.F.);
#68755=ORIENTED_EDGE('',*,*,#48879,.F.);
#68756=ORIENTED_EDGE('',*,*,#48880,.T.);
#68757=ORIENTED_EDGE('',*,*,#48881,.T.);
#68758=ORIENTED_EDGE('',*,*,#48882,.T.);
#68759=ORIENTED_EDGE('',*,*,#48881,.F.);
#68760=ORIENTED_EDGE('',*,*,#48883,.F.);
#68761=ORIENTED_EDGE('',*,*,#48884,.T.);
#68762=ORIENTED_EDGE('',*,*,#48880,.F.);
#68763=ORIENTED_EDGE('',*,*,#48884,.F.);
#68764=ORIENTED_EDGE('',*,*,#48882,.F.);
#68765=ORIENTED_EDGE('',*,*,#48883,.T.);
#68766=ORIENTED_EDGE('',*,*,#48885,.T.);
#68767=ORIENTED_EDGE('',*,*,#48886,.T.);
#68768=ORIENTED_EDGE('',*,*,#48885,.F.);
#68769=ORIENTED_EDGE('',*,*,#48886,.F.);
#68770=ORIENTED_EDGE('',*,*,#48887,.F.);
#68771=ORIENTED_EDGE('',*,*,#48888,.T.);
#68772=ORIENTED_EDGE('',*,*,#48889,.T.);
#68773=ORIENTED_EDGE('',*,*,#48890,.F.);
#68774=ORIENTED_EDGE('',*,*,#48891,.F.);
#68775=ORIENTED_EDGE('',*,*,#48892,.T.);
#68776=ORIENTED_EDGE('',*,*,#48887,.T.);
#68777=ORIENTED_EDGE('',*,*,#48893,.F.);
#68778=ORIENTED_EDGE('',*,*,#48894,.F.);
#68779=ORIENTED_EDGE('',*,*,#48895,.T.);
#68780=ORIENTED_EDGE('',*,*,#48891,.T.);
#68781=ORIENTED_EDGE('',*,*,#48896,.F.);
#68782=ORIENTED_EDGE('',*,*,#48897,.F.);
#68783=ORIENTED_EDGE('',*,*,#48898,.T.);
#68784=ORIENTED_EDGE('',*,*,#48894,.T.);
#68785=ORIENTED_EDGE('',*,*,#48899,.F.);
#68786=ORIENTED_EDGE('',*,*,#48900,.F.);
#68787=ORIENTED_EDGE('',*,*,#48901,.T.);
#68788=ORIENTED_EDGE('',*,*,#48897,.T.);
#68789=ORIENTED_EDGE('',*,*,#48902,.F.);
#68790=ORIENTED_EDGE('',*,*,#48903,.F.);
#68791=ORIENTED_EDGE('',*,*,#48904,.T.);
#68792=ORIENTED_EDGE('',*,*,#48900,.T.);
#68793=ORIENTED_EDGE('',*,*,#48905,.F.);
#68794=ORIENTED_EDGE('',*,*,#48906,.F.);
#68795=ORIENTED_EDGE('',*,*,#48907,.T.);
#68796=ORIENTED_EDGE('',*,*,#48903,.T.);
#68797=ORIENTED_EDGE('',*,*,#48908,.F.);
#68798=ORIENTED_EDGE('',*,*,#48909,.F.);
#68799=ORIENTED_EDGE('',*,*,#48910,.T.);
#68800=ORIENTED_EDGE('',*,*,#48906,.T.);
#68801=ORIENTED_EDGE('',*,*,#48911,.F.);
#68802=ORIENTED_EDGE('',*,*,#48912,.F.);
#68803=ORIENTED_EDGE('',*,*,#48913,.T.);
#68804=ORIENTED_EDGE('',*,*,#48909,.T.);
#68805=ORIENTED_EDGE('',*,*,#48914,.F.);
#68806=ORIENTED_EDGE('',*,*,#48915,.F.);
#68807=ORIENTED_EDGE('',*,*,#48916,.T.);
#68808=ORIENTED_EDGE('',*,*,#48912,.T.);
#68809=ORIENTED_EDGE('',*,*,#48917,.F.);
#68810=ORIENTED_EDGE('',*,*,#48918,.F.);
#68811=ORIENTED_EDGE('',*,*,#48919,.T.);
#68812=ORIENTED_EDGE('',*,*,#48915,.T.);
#68813=ORIENTED_EDGE('',*,*,#48920,.F.);
#68814=ORIENTED_EDGE('',*,*,#48921,.F.);
#68815=ORIENTED_EDGE('',*,*,#48922,.T.);
#68816=ORIENTED_EDGE('',*,*,#48918,.T.);
#68817=ORIENTED_EDGE('',*,*,#48923,.F.);
#68818=ORIENTED_EDGE('',*,*,#48924,.F.);
#68819=ORIENTED_EDGE('',*,*,#48925,.T.);
#68820=ORIENTED_EDGE('',*,*,#48921,.T.);
#68821=ORIENTED_EDGE('',*,*,#48926,.F.);
#68822=ORIENTED_EDGE('',*,*,#48927,.F.);
#68823=ORIENTED_EDGE('',*,*,#48928,.T.);
#68824=ORIENTED_EDGE('',*,*,#48924,.T.);
#68825=ORIENTED_EDGE('',*,*,#48929,.F.);
#68826=ORIENTED_EDGE('',*,*,#48930,.F.);
#68827=ORIENTED_EDGE('',*,*,#48931,.T.);
#68828=ORIENTED_EDGE('',*,*,#48927,.T.);
#68829=ORIENTED_EDGE('',*,*,#48932,.F.);
#68830=ORIENTED_EDGE('',*,*,#48933,.F.);
#68831=ORIENTED_EDGE('',*,*,#48934,.T.);
#68832=ORIENTED_EDGE('',*,*,#48930,.T.);
#68833=ORIENTED_EDGE('',*,*,#48935,.F.);
#68834=ORIENTED_EDGE('',*,*,#48936,.F.);
#68835=ORIENTED_EDGE('',*,*,#48937,.T.);
#68836=ORIENTED_EDGE('',*,*,#48933,.T.);
#68837=ORIENTED_EDGE('',*,*,#48938,.F.);
#68838=ORIENTED_EDGE('',*,*,#48939,.F.);
#68839=ORIENTED_EDGE('',*,*,#48940,.T.);
#68840=ORIENTED_EDGE('',*,*,#48936,.T.);
#68841=ORIENTED_EDGE('',*,*,#48941,.F.);
#68842=ORIENTED_EDGE('',*,*,#48942,.F.);
#68843=ORIENTED_EDGE('',*,*,#48943,.T.);
#68844=ORIENTED_EDGE('',*,*,#48939,.T.);
#68845=ORIENTED_EDGE('',*,*,#48944,.F.);
#68846=ORIENTED_EDGE('',*,*,#48945,.F.);
#68847=ORIENTED_EDGE('',*,*,#48946,.T.);
#68848=ORIENTED_EDGE('',*,*,#48942,.T.);
#68849=ORIENTED_EDGE('',*,*,#48947,.F.);
#68850=ORIENTED_EDGE('',*,*,#48948,.F.);
#68851=ORIENTED_EDGE('',*,*,#48949,.T.);
#68852=ORIENTED_EDGE('',*,*,#48945,.T.);
#68853=ORIENTED_EDGE('',*,*,#48950,.F.);
#68854=ORIENTED_EDGE('',*,*,#48951,.F.);
#68855=ORIENTED_EDGE('',*,*,#48952,.T.);
#68856=ORIENTED_EDGE('',*,*,#48948,.T.);
#68857=ORIENTED_EDGE('',*,*,#48953,.F.);
#68858=ORIENTED_EDGE('',*,*,#48954,.F.);
#68859=ORIENTED_EDGE('',*,*,#48955,.T.);
#68860=ORIENTED_EDGE('',*,*,#48951,.T.);
#68861=ORIENTED_EDGE('',*,*,#48956,.F.);
#68862=ORIENTED_EDGE('',*,*,#48957,.F.);
#68863=ORIENTED_EDGE('',*,*,#48958,.T.);
#68864=ORIENTED_EDGE('',*,*,#48954,.T.);
#68865=ORIENTED_EDGE('',*,*,#48959,.F.);
#68866=ORIENTED_EDGE('',*,*,#48960,.F.);
#68867=ORIENTED_EDGE('',*,*,#48961,.T.);
#68868=ORIENTED_EDGE('',*,*,#48957,.T.);
#68869=ORIENTED_EDGE('',*,*,#48962,.F.);
#68870=ORIENTED_EDGE('',*,*,#48963,.F.);
#68871=ORIENTED_EDGE('',*,*,#48964,.T.);
#68872=ORIENTED_EDGE('',*,*,#48960,.T.);
#68873=ORIENTED_EDGE('',*,*,#48965,.F.);
#68874=ORIENTED_EDGE('',*,*,#48966,.F.);
#68875=ORIENTED_EDGE('',*,*,#48967,.T.);
#68876=ORIENTED_EDGE('',*,*,#48963,.T.);
#68877=ORIENTED_EDGE('',*,*,#48968,.F.);
#68878=ORIENTED_EDGE('',*,*,#48969,.F.);
#68879=ORIENTED_EDGE('',*,*,#48970,.T.);
#68880=ORIENTED_EDGE('',*,*,#48966,.T.);
#68881=ORIENTED_EDGE('',*,*,#48971,.F.);
#68882=ORIENTED_EDGE('',*,*,#48972,.F.);
#68883=ORIENTED_EDGE('',*,*,#48973,.T.);
#68884=ORIENTED_EDGE('',*,*,#48969,.T.);
#68885=ORIENTED_EDGE('',*,*,#48974,.F.);
#68886=ORIENTED_EDGE('',*,*,#48975,.F.);
#68887=ORIENTED_EDGE('',*,*,#48976,.T.);
#68888=ORIENTED_EDGE('',*,*,#48972,.T.);
#68889=ORIENTED_EDGE('',*,*,#48977,.F.);
#68890=ORIENTED_EDGE('',*,*,#48978,.F.);
#68891=ORIENTED_EDGE('',*,*,#48979,.T.);
#68892=ORIENTED_EDGE('',*,*,#48975,.T.);
#68893=ORIENTED_EDGE('',*,*,#48980,.F.);
#68894=ORIENTED_EDGE('',*,*,#48981,.F.);
#68895=ORIENTED_EDGE('',*,*,#48982,.F.);
#68896=ORIENTED_EDGE('',*,*,#48983,.T.);
#68897=ORIENTED_EDGE('',*,*,#48978,.T.);
#68898=ORIENTED_EDGE('',*,*,#48984,.F.);
#68899=ORIENTED_EDGE('',*,*,#48985,.F.);
#68900=ORIENTED_EDGE('',*,*,#48986,.T.);
#68901=ORIENTED_EDGE('',*,*,#48987,.T.);
#68902=ORIENTED_EDGE('',*,*,#48988,.F.);
#68903=ORIENTED_EDGE('',*,*,#48989,.F.);
#68904=ORIENTED_EDGE('',*,*,#48990,.T.);
#68905=ORIENTED_EDGE('',*,*,#48985,.T.);
#68906=ORIENTED_EDGE('',*,*,#48991,.F.);
#68907=ORIENTED_EDGE('',*,*,#48992,.F.);
#68908=ORIENTED_EDGE('',*,*,#48993,.T.);
#68909=ORIENTED_EDGE('',*,*,#48989,.T.);
#68910=ORIENTED_EDGE('',*,*,#48994,.F.);
#68911=ORIENTED_EDGE('',*,*,#48995,.F.);
#68912=ORIENTED_EDGE('',*,*,#48996,.T.);
#68913=ORIENTED_EDGE('',*,*,#48992,.T.);
#68914=ORIENTED_EDGE('',*,*,#48997,.F.);
#68915=ORIENTED_EDGE('',*,*,#48998,.F.);
#68916=ORIENTED_EDGE('',*,*,#48999,.T.);
#68917=ORIENTED_EDGE('',*,*,#48995,.T.);
#68918=ORIENTED_EDGE('',*,*,#49000,.F.);
#68919=ORIENTED_EDGE('',*,*,#49001,.F.);
#68920=ORIENTED_EDGE('',*,*,#49002,.T.);
#68921=ORIENTED_EDGE('',*,*,#48998,.T.);
#68922=ORIENTED_EDGE('',*,*,#49003,.F.);
#68923=ORIENTED_EDGE('',*,*,#49004,.F.);
#68924=ORIENTED_EDGE('',*,*,#49005,.T.);
#68925=ORIENTED_EDGE('',*,*,#49001,.T.);
#68926=ORIENTED_EDGE('',*,*,#49006,.F.);
#68927=ORIENTED_EDGE('',*,*,#49007,.F.);
#68928=ORIENTED_EDGE('',*,*,#49008,.T.);
#68929=ORIENTED_EDGE('',*,*,#49004,.T.);
#68930=ORIENTED_EDGE('',*,*,#49009,.F.);
#68931=ORIENTED_EDGE('',*,*,#49010,.F.);
#68932=ORIENTED_EDGE('',*,*,#49011,.T.);
#68933=ORIENTED_EDGE('',*,*,#49007,.T.);
#68934=ORIENTED_EDGE('',*,*,#49012,.F.);
#68935=ORIENTED_EDGE('',*,*,#49013,.F.);
#68936=ORIENTED_EDGE('',*,*,#49014,.T.);
#68937=ORIENTED_EDGE('',*,*,#49010,.T.);
#68938=ORIENTED_EDGE('',*,*,#49015,.F.);
#68939=ORIENTED_EDGE('',*,*,#49016,.F.);
#68940=ORIENTED_EDGE('',*,*,#49017,.T.);
#68941=ORIENTED_EDGE('',*,*,#49013,.T.);
#68942=ORIENTED_EDGE('',*,*,#49018,.F.);
#68943=ORIENTED_EDGE('',*,*,#49019,.F.);
#68944=ORIENTED_EDGE('',*,*,#49020,.T.);
#68945=ORIENTED_EDGE('',*,*,#49016,.T.);
#68946=ORIENTED_EDGE('',*,*,#49021,.F.);
#68947=ORIENTED_EDGE('',*,*,#49022,.F.);
#68948=ORIENTED_EDGE('',*,*,#49023,.T.);
#68949=ORIENTED_EDGE('',*,*,#49019,.T.);
#68950=ORIENTED_EDGE('',*,*,#49024,.F.);
#68951=ORIENTED_EDGE('',*,*,#49025,.F.);
#68952=ORIENTED_EDGE('',*,*,#49026,.T.);
#68953=ORIENTED_EDGE('',*,*,#49022,.T.);
#68954=ORIENTED_EDGE('',*,*,#49027,.F.);
#68955=ORIENTED_EDGE('',*,*,#49028,.F.);
#68956=ORIENTED_EDGE('',*,*,#49029,.T.);
#68957=ORIENTED_EDGE('',*,*,#49025,.T.);
#68958=ORIENTED_EDGE('',*,*,#49030,.F.);
#68959=ORIENTED_EDGE('',*,*,#49031,.F.);
#68960=ORIENTED_EDGE('',*,*,#49032,.T.);
#68961=ORIENTED_EDGE('',*,*,#49028,.T.);
#68962=ORIENTED_EDGE('',*,*,#49033,.F.);
#68963=ORIENTED_EDGE('',*,*,#49034,.F.);
#68964=ORIENTED_EDGE('',*,*,#49035,.T.);
#68965=ORIENTED_EDGE('',*,*,#49031,.T.);
#68966=ORIENTED_EDGE('',*,*,#49036,.F.);
#68967=ORIENTED_EDGE('',*,*,#49037,.F.);
#68968=ORIENTED_EDGE('',*,*,#49038,.T.);
#68969=ORIENTED_EDGE('',*,*,#49034,.T.);
#68970=ORIENTED_EDGE('',*,*,#49039,.F.);
#68971=ORIENTED_EDGE('',*,*,#49040,.F.);
#68972=ORIENTED_EDGE('',*,*,#49041,.T.);
#68973=ORIENTED_EDGE('',*,*,#49037,.T.);
#68974=ORIENTED_EDGE('',*,*,#49042,.F.);
#68975=ORIENTED_EDGE('',*,*,#49043,.F.);
#68976=ORIENTED_EDGE('',*,*,#49044,.T.);
#68977=ORIENTED_EDGE('',*,*,#49040,.T.);
#68978=ORIENTED_EDGE('',*,*,#49045,.F.);
#68979=ORIENTED_EDGE('',*,*,#49046,.F.);
#68980=ORIENTED_EDGE('',*,*,#49047,.T.);
#68981=ORIENTED_EDGE('',*,*,#49043,.T.);
#68982=ORIENTED_EDGE('',*,*,#49048,.F.);
#68983=ORIENTED_EDGE('',*,*,#49049,.F.);
#68984=ORIENTED_EDGE('',*,*,#49050,.T.);
#68985=ORIENTED_EDGE('',*,*,#49046,.T.);
#68986=ORIENTED_EDGE('',*,*,#49051,.F.);
#68987=ORIENTED_EDGE('',*,*,#49052,.F.);
#68988=ORIENTED_EDGE('',*,*,#49053,.T.);
#68989=ORIENTED_EDGE('',*,*,#49049,.T.);
#68990=ORIENTED_EDGE('',*,*,#49054,.F.);
#68991=ORIENTED_EDGE('',*,*,#49055,.F.);
#68992=ORIENTED_EDGE('',*,*,#49056,.T.);
#68993=ORIENTED_EDGE('',*,*,#49052,.T.);
#68994=ORIENTED_EDGE('',*,*,#49057,.F.);
#68995=ORIENTED_EDGE('',*,*,#49058,.F.);
#68996=ORIENTED_EDGE('',*,*,#49059,.T.);
#68997=ORIENTED_EDGE('',*,*,#49055,.T.);
#68998=ORIENTED_EDGE('',*,*,#49060,.F.);
#68999=ORIENTED_EDGE('',*,*,#49061,.F.);
#69000=ORIENTED_EDGE('',*,*,#49062,.T.);
#69001=ORIENTED_EDGE('',*,*,#49058,.T.);
#69002=ORIENTED_EDGE('',*,*,#49063,.F.);
#69003=ORIENTED_EDGE('',*,*,#49064,.F.);
#69004=ORIENTED_EDGE('',*,*,#49065,.T.);
#69005=ORIENTED_EDGE('',*,*,#49061,.T.);
#69006=ORIENTED_EDGE('',*,*,#49066,.F.);
#69007=ORIENTED_EDGE('',*,*,#49067,.F.);
#69008=ORIENTED_EDGE('',*,*,#49068,.T.);
#69009=ORIENTED_EDGE('',*,*,#49064,.T.);
#69010=ORIENTED_EDGE('',*,*,#49069,.F.);
#69011=ORIENTED_EDGE('',*,*,#49070,.F.);
#69012=ORIENTED_EDGE('',*,*,#49071,.T.);
#69013=ORIENTED_EDGE('',*,*,#49067,.T.);
#69014=ORIENTED_EDGE('',*,*,#49072,.F.);
#69015=ORIENTED_EDGE('',*,*,#49073,.F.);
#69016=ORIENTED_EDGE('',*,*,#49074,.T.);
#69017=ORIENTED_EDGE('',*,*,#49070,.T.);
#69018=ORIENTED_EDGE('',*,*,#49075,.F.);
#69019=ORIENTED_EDGE('',*,*,#49076,.F.);
#69020=ORIENTED_EDGE('',*,*,#49077,.T.);
#69021=ORIENTED_EDGE('',*,*,#49073,.T.);
#69022=ORIENTED_EDGE('',*,*,#49078,.F.);
#69023=ORIENTED_EDGE('',*,*,#49079,.F.);
#69024=ORIENTED_EDGE('',*,*,#49080,.T.);
#69025=ORIENTED_EDGE('',*,*,#49081,.F.);
#69026=ORIENTED_EDGE('',*,*,#49082,.F.);
#69027=ORIENTED_EDGE('',*,*,#49083,.F.);
#69028=ORIENTED_EDGE('',*,*,#49084,.T.);
#69029=ORIENTED_EDGE('',*,*,#49085,.T.);
#69030=ORIENTED_EDGE('',*,*,#49084,.F.);
#69031=ORIENTED_EDGE('',*,*,#48982,.T.);
#69032=ORIENTED_EDGE('',*,*,#49086,.T.);
#69033=ORIENTED_EDGE('',*,*,#49087,.T.);
#69034=ORIENTED_EDGE('',*,*,#49088,.F.);
#69035=ORIENTED_EDGE('',*,*,#49089,.T.);
#69036=ORIENTED_EDGE('',*,*,#49090,.T.);
#69037=ORIENTED_EDGE('',*,*,#49091,.F.);
#69038=ORIENTED_EDGE('',*,*,#49090,.F.);
#69039=ORIENTED_EDGE('',*,*,#49092,.T.);
#69040=ORIENTED_EDGE('',*,*,#49076,.T.);
#69041=ORIENTED_EDGE('',*,*,#49093,.F.);
#69042=ORIENTED_EDGE('',*,*,#49094,.F.);
#69043=ORIENTED_EDGE('',*,*,#49088,.T.);
#69044=ORIENTED_EDGE('',*,*,#49095,.T.);
#69045=ORIENTED_EDGE('',*,*,#49091,.T.);
#69046=ORIENTED_EDGE('',*,*,#49083,.T.);
#69047=ORIENTED_EDGE('',*,*,#48987,.F.);
#69048=ORIENTED_EDGE('',*,*,#49096,.F.);
#69049=ORIENTED_EDGE('',*,*,#48889,.F.);
#69050=ORIENTED_EDGE('',*,*,#49097,.F.);
#69051=ORIENTED_EDGE('',*,*,#49085,.F.);
#69052=ORIENTED_EDGE('',*,*,#49081,.T.);
#69053=ORIENTED_EDGE('',*,*,#49082,.T.);
#69054=ORIENTED_EDGE('',*,*,#49098,.F.);
#69055=ORIENTED_EDGE('',*,*,#49099,.F.);
#69056=ORIENTED_EDGE('',*,*,#49100,.F.);
#69057=ORIENTED_EDGE('',*,*,#49080,.F.);
#69058=ORIENTED_EDGE('',*,*,#49101,.F.);
#69059=ORIENTED_EDGE('',*,*,#49102,.F.);
#69060=ORIENTED_EDGE('',*,*,#49100,.T.);
#69061=ORIENTED_EDGE('',*,*,#49103,.F.);
#69062=ORIENTED_EDGE('',*,*,#49099,.T.);
#69063=ORIENTED_EDGE('',*,*,#49104,.F.);
#69064=ORIENTED_EDGE('',*,*,#49098,.T.);
#69065=ORIENTED_EDGE('',*,*,#49105,.F.);
#69066=ORIENTED_EDGE('',*,*,#49102,.T.);
#69067=ORIENTED_EDGE('',*,*,#49106,.F.);
#69068=ORIENTED_EDGE('',*,*,#49101,.T.);
#69069=ORIENTED_EDGE('',*,*,#49107,.F.);
#69070=ORIENTED_EDGE('',*,*,#49108,.T.);
#69071=ORIENTED_EDGE('',*,*,#49109,.T.);
#69072=ORIENTED_EDGE('',*,*,#49110,.T.);
#69073=ORIENTED_EDGE('',*,*,#49111,.T.);
#69074=ORIENTED_EDGE('',*,*,#49112,.T.);
#69075=ORIENTED_EDGE('',*,*,#49113,.T.);
#69076=ORIENTED_EDGE('',*,*,#49114,.T.);
#69077=ORIENTED_EDGE('',*,*,#49079,.T.);
#69078=ORIENTED_EDGE('',*,*,#49115,.F.);
#69079=ORIENTED_EDGE('',*,*,#49109,.F.);
#69080=ORIENTED_EDGE('',*,*,#49115,.T.);
#69081=ORIENTED_EDGE('',*,*,#49103,.T.);
#69082=ORIENTED_EDGE('',*,*,#49116,.F.);
#69083=ORIENTED_EDGE('',*,*,#49110,.F.);
#69084=ORIENTED_EDGE('',*,*,#49116,.T.);
#69085=ORIENTED_EDGE('',*,*,#49104,.T.);
#69086=ORIENTED_EDGE('',*,*,#49117,.F.);
#69087=ORIENTED_EDGE('',*,*,#49111,.F.);
#69088=ORIENTED_EDGE('',*,*,#49117,.T.);
#69089=ORIENTED_EDGE('',*,*,#49105,.T.);
#69090=ORIENTED_EDGE('',*,*,#49118,.F.);
#69091=ORIENTED_EDGE('',*,*,#49112,.F.);
#69092=ORIENTED_EDGE('',*,*,#49118,.T.);
#69093=ORIENTED_EDGE('',*,*,#49106,.T.);
#69094=ORIENTED_EDGE('',*,*,#49119,.F.);
#69095=ORIENTED_EDGE('',*,*,#49113,.F.);
#69096=ORIENTED_EDGE('',*,*,#49119,.T.);
#69097=ORIENTED_EDGE('',*,*,#49107,.T.);
#69098=ORIENTED_EDGE('',*,*,#49114,.F.);
#69099=ORIENTED_EDGE('',*,*,#49108,.F.);
#69100=ORIENTED_EDGE('',*,*,#49097,.T.);
#69101=ORIENTED_EDGE('',*,*,#48888,.F.);
#69102=ORIENTED_EDGE('',*,*,#48892,.F.);
#69103=ORIENTED_EDGE('',*,*,#48895,.F.);
#69104=ORIENTED_EDGE('',*,*,#48898,.F.);
#69105=ORIENTED_EDGE('',*,*,#48901,.F.);
#69106=ORIENTED_EDGE('',*,*,#48904,.F.);
#69107=ORIENTED_EDGE('',*,*,#48907,.F.);
#69108=ORIENTED_EDGE('',*,*,#48910,.F.);
#69109=ORIENTED_EDGE('',*,*,#48913,.F.);
#69110=ORIENTED_EDGE('',*,*,#48916,.F.);
#69111=ORIENTED_EDGE('',*,*,#48919,.F.);
#69112=ORIENTED_EDGE('',*,*,#48922,.F.);
#69113=ORIENTED_EDGE('',*,*,#48925,.F.);
#69114=ORIENTED_EDGE('',*,*,#48928,.F.);
#69115=ORIENTED_EDGE('',*,*,#48931,.F.);
#69116=ORIENTED_EDGE('',*,*,#48934,.F.);
#69117=ORIENTED_EDGE('',*,*,#48937,.F.);
#69118=ORIENTED_EDGE('',*,*,#48940,.F.);
#69119=ORIENTED_EDGE('',*,*,#48943,.F.);
#69120=ORIENTED_EDGE('',*,*,#48946,.F.);
#69121=ORIENTED_EDGE('',*,*,#48949,.F.);
#69122=ORIENTED_EDGE('',*,*,#48952,.F.);
#69123=ORIENTED_EDGE('',*,*,#48955,.F.);
#69124=ORIENTED_EDGE('',*,*,#48958,.F.);
#69125=ORIENTED_EDGE('',*,*,#48961,.F.);
#69126=ORIENTED_EDGE('',*,*,#48964,.F.);
#69127=ORIENTED_EDGE('',*,*,#48967,.F.);
#69128=ORIENTED_EDGE('',*,*,#48970,.F.);
#69129=ORIENTED_EDGE('',*,*,#48973,.F.);
#69130=ORIENTED_EDGE('',*,*,#48976,.F.);
#69131=ORIENTED_EDGE('',*,*,#48979,.F.);
#69132=ORIENTED_EDGE('',*,*,#48983,.F.);
#69133=ORIENTED_EDGE('',*,*,#49092,.F.);
#69134=ORIENTED_EDGE('',*,*,#49089,.F.);
#69135=ORIENTED_EDGE('',*,*,#49094,.T.);
#69136=ORIENTED_EDGE('',*,*,#49093,.T.);
#69137=ORIENTED_EDGE('',*,*,#49078,.T.);
#69138=ORIENTED_EDGE('',*,*,#49075,.T.);
#69139=ORIENTED_EDGE('',*,*,#49072,.T.);
#69140=ORIENTED_EDGE('',*,*,#49069,.T.);
#69141=ORIENTED_EDGE('',*,*,#49066,.T.);
#69142=ORIENTED_EDGE('',*,*,#49063,.T.);
#69143=ORIENTED_EDGE('',*,*,#49060,.T.);
#69144=ORIENTED_EDGE('',*,*,#49057,.T.);
#69145=ORIENTED_EDGE('',*,*,#49054,.T.);
#69146=ORIENTED_EDGE('',*,*,#49051,.T.);
#69147=ORIENTED_EDGE('',*,*,#49048,.T.);
#69148=ORIENTED_EDGE('',*,*,#49045,.T.);
#69149=ORIENTED_EDGE('',*,*,#49042,.T.);
#69150=ORIENTED_EDGE('',*,*,#49039,.T.);
#69151=ORIENTED_EDGE('',*,*,#49036,.T.);
#69152=ORIENTED_EDGE('',*,*,#49033,.T.);
#69153=ORIENTED_EDGE('',*,*,#49030,.T.);
#69154=ORIENTED_EDGE('',*,*,#49027,.T.);
#69155=ORIENTED_EDGE('',*,*,#49024,.T.);
#69156=ORIENTED_EDGE('',*,*,#49021,.T.);
#69157=ORIENTED_EDGE('',*,*,#49018,.T.);
#69158=ORIENTED_EDGE('',*,*,#49015,.T.);
#69159=ORIENTED_EDGE('',*,*,#49012,.T.);
#69160=ORIENTED_EDGE('',*,*,#49009,.T.);
#69161=ORIENTED_EDGE('',*,*,#49006,.T.);
#69162=ORIENTED_EDGE('',*,*,#49003,.T.);
#69163=ORIENTED_EDGE('',*,*,#49000,.T.);
#69164=ORIENTED_EDGE('',*,*,#48997,.T.);
#69165=ORIENTED_EDGE('',*,*,#48994,.T.);
#69166=ORIENTED_EDGE('',*,*,#48991,.T.);
#69167=ORIENTED_EDGE('',*,*,#48988,.T.);
#69168=ORIENTED_EDGE('',*,*,#48981,.T.);
#69169=ORIENTED_EDGE('',*,*,#49120,.F.);
#69170=ORIENTED_EDGE('',*,*,#49086,.F.);
#69171=ORIENTED_EDGE('',*,*,#49096,.T.);
#69172=ORIENTED_EDGE('',*,*,#48986,.F.);
#69173=ORIENTED_EDGE('',*,*,#48990,.F.);
#69174=ORIENTED_EDGE('',*,*,#48993,.F.);
#69175=ORIENTED_EDGE('',*,*,#48996,.F.);
#69176=ORIENTED_EDGE('',*,*,#48999,.F.);
#69177=ORIENTED_EDGE('',*,*,#49002,.F.);
#69178=ORIENTED_EDGE('',*,*,#49005,.F.);
#69179=ORIENTED_EDGE('',*,*,#49008,.F.);
#69180=ORIENTED_EDGE('',*,*,#49011,.F.);
#69181=ORIENTED_EDGE('',*,*,#49014,.F.);
#69182=ORIENTED_EDGE('',*,*,#49017,.F.);
#69183=ORIENTED_EDGE('',*,*,#49020,.F.);
#69184=ORIENTED_EDGE('',*,*,#49023,.F.);
#69185=ORIENTED_EDGE('',*,*,#49026,.F.);
#69186=ORIENTED_EDGE('',*,*,#49029,.F.);
#69187=ORIENTED_EDGE('',*,*,#49032,.F.);
#69188=ORIENTED_EDGE('',*,*,#49035,.F.);
#69189=ORIENTED_EDGE('',*,*,#49038,.F.);
#69190=ORIENTED_EDGE('',*,*,#49041,.F.);
#69191=ORIENTED_EDGE('',*,*,#49044,.F.);
#69192=ORIENTED_EDGE('',*,*,#49047,.F.);
#69193=ORIENTED_EDGE('',*,*,#49050,.F.);
#69194=ORIENTED_EDGE('',*,*,#49053,.F.);
#69195=ORIENTED_EDGE('',*,*,#49056,.F.);
#69196=ORIENTED_EDGE('',*,*,#49059,.F.);
#69197=ORIENTED_EDGE('',*,*,#49062,.F.);
#69198=ORIENTED_EDGE('',*,*,#49065,.F.);
#69199=ORIENTED_EDGE('',*,*,#49068,.F.);
#69200=ORIENTED_EDGE('',*,*,#49071,.F.);
#69201=ORIENTED_EDGE('',*,*,#49074,.F.);
#69202=ORIENTED_EDGE('',*,*,#49077,.F.);
#69203=ORIENTED_EDGE('',*,*,#49095,.F.);
#69204=ORIENTED_EDGE('',*,*,#49087,.F.);
#69205=ORIENTED_EDGE('',*,*,#49120,.T.);
#69206=ORIENTED_EDGE('',*,*,#48984,.T.);
#69207=ORIENTED_EDGE('',*,*,#48980,.T.);
#69208=ORIENTED_EDGE('',*,*,#48977,.T.);
#69209=ORIENTED_EDGE('',*,*,#48974,.T.);
#69210=ORIENTED_EDGE('',*,*,#48971,.T.);
#69211=ORIENTED_EDGE('',*,*,#48968,.T.);
#69212=ORIENTED_EDGE('',*,*,#48965,.T.);
#69213=ORIENTED_EDGE('',*,*,#48962,.T.);
#69214=ORIENTED_EDGE('',*,*,#48959,.T.);
#69215=ORIENTED_EDGE('',*,*,#48956,.T.);
#69216=ORIENTED_EDGE('',*,*,#48953,.T.);
#69217=ORIENTED_EDGE('',*,*,#48950,.T.);
#69218=ORIENTED_EDGE('',*,*,#48947,.T.);
#69219=ORIENTED_EDGE('',*,*,#48944,.T.);
#69220=ORIENTED_EDGE('',*,*,#48941,.T.);
#69221=ORIENTED_EDGE('',*,*,#48938,.T.);
#69222=ORIENTED_EDGE('',*,*,#48935,.T.);
#69223=ORIENTED_EDGE('',*,*,#48932,.T.);
#69224=ORIENTED_EDGE('',*,*,#48929,.T.);
#69225=ORIENTED_EDGE('',*,*,#48926,.T.);
#69226=ORIENTED_EDGE('',*,*,#48923,.T.);
#69227=ORIENTED_EDGE('',*,*,#48920,.T.);
#69228=ORIENTED_EDGE('',*,*,#48917,.T.);
#69229=ORIENTED_EDGE('',*,*,#48914,.T.);
#69230=ORIENTED_EDGE('',*,*,#48911,.T.);
#69231=ORIENTED_EDGE('',*,*,#48908,.T.);
#69232=ORIENTED_EDGE('',*,*,#48905,.T.);
#69233=ORIENTED_EDGE('',*,*,#48902,.T.);
#69234=ORIENTED_EDGE('',*,*,#48899,.T.);
#69235=ORIENTED_EDGE('',*,*,#48896,.T.);
#69236=ORIENTED_EDGE('',*,*,#48893,.T.);
#69237=ORIENTED_EDGE('',*,*,#48890,.T.);
#69238=ORIENTED_EDGE('',*,*,#49121,.F.);
#69239=ORIENTED_EDGE('',*,*,#49122,.T.);
#69240=ORIENTED_EDGE('',*,*,#49123,.F.);
#69241=ORIENTED_EDGE('',*,*,#49124,.F.);
#69242=ORIENTED_EDGE('',*,*,#49125,.F.);
#69243=ORIENTED_EDGE('',*,*,#49126,.T.);
#69244=ORIENTED_EDGE('',*,*,#49127,.T.);
#69245=ORIENTED_EDGE('',*,*,#49128,.T.);
#69246=ORIENTED_EDGE('',*,*,#49121,.T.);
#69247=ORIENTED_EDGE('',*,*,#49125,.T.);
#69248=ORIENTED_EDGE('',*,*,#49129,.F.);
#69249=ORIENTED_EDGE('',*,*,#49130,.F.);
#69250=ORIENTED_EDGE('',*,*,#49131,.T.);
#69251=ORIENTED_EDGE('',*,*,#49127,.F.);
#69252=ORIENTED_EDGE('',*,*,#49126,.F.);
#69253=ORIENTED_EDGE('',*,*,#49132,.F.);
#69254=ORIENTED_EDGE('',*,*,#49131,.F.);
#69255=ORIENTED_EDGE('',*,*,#49133,.F.);
#69256=ORIENTED_EDGE('',*,*,#49132,.T.);
#69257=ORIENTED_EDGE('',*,*,#49134,.F.);
#69258=ORIENTED_EDGE('',*,*,#49135,.F.);
#69259=ORIENTED_EDGE('',*,*,#49133,.T.);
#69260=ORIENTED_EDGE('',*,*,#49130,.T.);
#69261=ORIENTED_EDGE('',*,*,#49128,.F.);
#69262=ORIENTED_EDGE('',*,*,#49135,.T.);
#69263=ORIENTED_EDGE('',*,*,#49134,.T.);
#69264=ORIENTED_EDGE('',*,*,#49129,.T.);
#69265=ORIENTED_EDGE('',*,*,#49136,.T.);
#69266=ORIENTED_EDGE('',*,*,#49137,.T.);
#69267=ORIENTED_EDGE('',*,*,#49123,.T.);
#69268=ORIENTED_EDGE('',*,*,#49138,.T.);
#69269=ORIENTED_EDGE('',*,*,#49122,.F.);
#69270=ORIENTED_EDGE('',*,*,#49137,.F.);
#69271=ORIENTED_EDGE('',*,*,#49136,.F.);
#69272=ORIENTED_EDGE('',*,*,#49124,.T.);
#69273=ORIENTED_EDGE('',*,*,#49138,.F.);
#69274=ORIENTED_EDGE('',*,*,#49139,.F.);
#69275=ORIENTED_EDGE('',*,*,#49140,.T.);
#69276=ORIENTED_EDGE('',*,*,#49141,.T.);
#69277=ORIENTED_EDGE('',*,*,#49140,.F.);
#69278=ORIENTED_EDGE('',*,*,#49142,.F.);
#69279=ORIENTED_EDGE('',*,*,#49143,.T.);
#69280=ORIENTED_EDGE('',*,*,#49139,.T.);
#69281=ORIENTED_EDGE('',*,*,#49143,.F.);
#69282=ORIENTED_EDGE('',*,*,#49144,.F.);
#69283=ORIENTED_EDGE('',*,*,#49145,.T.);
#69284=ORIENTED_EDGE('',*,*,#49142,.T.);
#69285=ORIENTED_EDGE('',*,*,#49145,.F.);
#69286=ORIENTED_EDGE('',*,*,#49146,.F.);
#69287=ORIENTED_EDGE('',*,*,#49147,.T.);
#69288=ORIENTED_EDGE('',*,*,#49148,.T.);
#69289=ORIENTED_EDGE('',*,*,#49147,.F.);
#69290=ORIENTED_EDGE('',*,*,#49149,.F.);
#69291=ORIENTED_EDGE('',*,*,#49150,.F.);
#69292=ORIENTED_EDGE('',*,*,#49151,.T.);
#69293=ORIENTED_EDGE('',*,*,#49146,.T.);
#69294=ORIENTED_EDGE('',*,*,#49151,.F.);
#69295=ORIENTED_EDGE('',*,*,#49149,.T.);
#69296=ORIENTED_EDGE('',*,*,#49150,.T.);
#69297=ORIENTED_EDGE('',*,*,#49152,.T.);
#69298=ORIENTED_EDGE('',*,*,#49153,.F.);
#69299=ORIENTED_EDGE('',*,*,#49152,.F.);
#69300=ORIENTED_EDGE('',*,*,#49148,.F.);
#69301=ORIENTED_EDGE('',*,*,#49144,.T.);
#69302=ORIENTED_EDGE('',*,*,#49153,.T.);
#69303=ORIENTED_EDGE('',*,*,#49141,.F.);
#69304=ORIENTED_EDGE('',*,*,#49154,.F.);
#69305=ORIENTED_EDGE('',*,*,#49155,.T.);
#69306=ORIENTED_EDGE('',*,*,#49156,.T.);
#69307=ORIENTED_EDGE('',*,*,#49155,.F.);
#69308=ORIENTED_EDGE('',*,*,#49157,.F.);
#69309=ORIENTED_EDGE('',*,*,#49158,.T.);
#69310=ORIENTED_EDGE('',*,*,#49159,.T.);
#69311=ORIENTED_EDGE('',*,*,#49158,.F.);
#69312=ORIENTED_EDGE('',*,*,#49160,.F.);
#69313=ORIENTED_EDGE('',*,*,#49161,.F.);
#69314=ORIENTED_EDGE('',*,*,#49162,.T.);
#69315=ORIENTED_EDGE('',*,*,#49157,.T.);
#69316=ORIENTED_EDGE('',*,*,#49162,.F.);
#69317=ORIENTED_EDGE('',*,*,#49160,.T.);
#69318=ORIENTED_EDGE('',*,*,#49161,.T.);
#69319=ORIENTED_EDGE('',*,*,#49163,.T.);
#69320=ORIENTED_EDGE('',*,*,#49164,.F.);
#69321=ORIENTED_EDGE('',*,*,#49163,.F.);
#69322=ORIENTED_EDGE('',*,*,#49156,.F.);
#69323=ORIENTED_EDGE('',*,*,#49165,.T.);
#69324=ORIENTED_EDGE('',*,*,#49166,.T.);
#69325=ORIENTED_EDGE('',*,*,#49165,.F.);
#69326=ORIENTED_EDGE('',*,*,#49167,.F.);
#69327=ORIENTED_EDGE('',*,*,#49168,.T.);
#69328=ORIENTED_EDGE('',*,*,#49154,.T.);
#69329=ORIENTED_EDGE('',*,*,#49168,.F.);
#69330=ORIENTED_EDGE('',*,*,#49167,.T.);
#69331=ORIENTED_EDGE('',*,*,#49159,.F.);
#69332=ORIENTED_EDGE('',*,*,#49166,.F.);
#69333=ORIENTED_EDGE('',*,*,#49164,.T.);
#69334=ORIENTED_EDGE('',*,*,#49169,.T.);
#69335=ORIENTED_EDGE('',*,*,#49169,.F.);
#69336=ORIENTED_EDGE('',*,*,#49170,.T.);
#69337=ORIENTED_EDGE('',*,*,#49170,.F.);
#69338=ORIENTED_EDGE('',*,*,#49171,.T.);
#69339=ORIENTED_EDGE('',*,*,#49171,.F.);
#69340=ORIENTED_EDGE('',*,*,#49172,.T.);
#69341=ORIENTED_EDGE('',*,*,#49172,.F.);
#69342=ORIENTED_EDGE('',*,*,#49173,.T.);
#69343=ORIENTED_EDGE('',*,*,#49173,.F.);
#69344=ORIENTED_EDGE('',*,*,#49174,.T.);
#69345=ORIENTED_EDGE('',*,*,#49174,.F.);
#69346=ORIENTED_EDGE('',*,*,#49175,.T.);
#69347=ORIENTED_EDGE('',*,*,#49175,.F.);
#69348=ORIENTED_EDGE('',*,*,#49176,.T.);
#69349=ORIENTED_EDGE('',*,*,#49176,.F.);
#69350=ORIENTED_EDGE('',*,*,#49177,.T.);
#69351=ORIENTED_EDGE('',*,*,#49177,.F.);
#69352=ORIENTED_EDGE('',*,*,#49178,.T.);
#69353=ORIENTED_EDGE('',*,*,#49178,.F.);
#69354=ORIENTED_EDGE('',*,*,#49179,.T.);
#69355=ORIENTED_EDGE('',*,*,#49179,.F.);
#69356=ORIENTED_EDGE('',*,*,#49180,.T.);
#69357=ORIENTED_EDGE('',*,*,#49180,.F.);
#69358=ORIENTED_EDGE('',*,*,#49181,.F.);
#69359=ORIENTED_EDGE('',*,*,#49182,.T.);
#69360=ORIENTED_EDGE('',*,*,#49183,.T.);
#69361=ORIENTED_EDGE('',*,*,#49182,.F.);
#69362=ORIENTED_EDGE('',*,*,#49184,.F.);
#69363=ORIENTED_EDGE('',*,*,#49185,.T.);
#69364=ORIENTED_EDGE('',*,*,#49186,.T.);
#69365=ORIENTED_EDGE('',*,*,#49185,.F.);
#69366=ORIENTED_EDGE('',*,*,#49181,.T.);
#69367=ORIENTED_EDGE('',*,*,#49186,.F.);
#69368=ORIENTED_EDGE('',*,*,#49183,.F.);
#69369=ORIENTED_EDGE('',*,*,#49184,.T.);
#69370=ORIENTED_EDGE('',*,*,#49187,.F.);
#69371=ORIENTED_EDGE('',*,*,#49188,.T.);
#69372=ORIENTED_EDGE('',*,*,#49189,.T.);
#69373=ORIENTED_EDGE('',*,*,#49188,.F.);
#69374=ORIENTED_EDGE('',*,*,#49190,.F.);
#69375=ORIENTED_EDGE('',*,*,#49191,.T.);
#69376=ORIENTED_EDGE('',*,*,#49192,.T.);
#69377=ORIENTED_EDGE('',*,*,#49191,.F.);
#69378=ORIENTED_EDGE('',*,*,#49189,.F.);
#69379=ORIENTED_EDGE('',*,*,#49190,.T.);
#69380=ORIENTED_EDGE('',*,*,#49187,.T.);
#69381=ORIENTED_EDGE('',*,*,#49192,.F.);
#69382=ORIENTED_EDGE('',*,*,#49193,.F.);
#69383=ORIENTED_EDGE('',*,*,#49194,.F.);
#69384=ORIENTED_EDGE('',*,*,#49195,.F.);
#69385=ORIENTED_EDGE('',*,*,#49196,.F.);
#69386=ORIENTED_EDGE('',*,*,#49197,.F.);
#69387=ORIENTED_EDGE('',*,*,#49193,.T.);
#69388=ORIENTED_EDGE('',*,*,#49198,.F.);
#69389=ORIENTED_EDGE('',*,*,#49199,.T.);
#69390=ORIENTED_EDGE('',*,*,#49200,.F.);
#69391=ORIENTED_EDGE('',*,*,#49201,.F.);
#69392=ORIENTED_EDGE('',*,*,#49196,.T.);
#69393=ORIENTED_EDGE('',*,*,#49202,.T.);
#69394=ORIENTED_EDGE('',*,*,#49203,.F.);
#69395=ORIENTED_EDGE('',*,*,#49204,.F.);
#69396=ORIENTED_EDGE('',*,*,#49200,.T.);
#69397=ORIENTED_EDGE('',*,*,#49205,.T.);
#69398=ORIENTED_EDGE('',*,*,#49206,.F.);
#69399=ORIENTED_EDGE('',*,*,#49207,.F.);
#69400=ORIENTED_EDGE('',*,*,#49203,.T.);
#69401=ORIENTED_EDGE('',*,*,#49208,.T.);
#69402=ORIENTED_EDGE('',*,*,#49209,.F.);
#69403=ORIENTED_EDGE('',*,*,#49210,.F.);
#69404=ORIENTED_EDGE('',*,*,#49206,.T.);
#69405=ORIENTED_EDGE('',*,*,#49211,.T.);
#69406=ORIENTED_EDGE('',*,*,#49212,.F.);
#69407=ORIENTED_EDGE('',*,*,#49213,.F.);
#69408=ORIENTED_EDGE('',*,*,#49209,.T.);
#69409=ORIENTED_EDGE('',*,*,#49214,.T.);
#69410=ORIENTED_EDGE('',*,*,#49215,.F.);
#69411=ORIENTED_EDGE('',*,*,#49216,.F.);
#69412=ORIENTED_EDGE('',*,*,#49212,.T.);
#69413=ORIENTED_EDGE('',*,*,#49217,.T.);
#69414=ORIENTED_EDGE('',*,*,#49218,.F.);
#69415=ORIENTED_EDGE('',*,*,#49219,.F.);
#69416=ORIENTED_EDGE('',*,*,#49215,.T.);
#69417=ORIENTED_EDGE('',*,*,#49220,.T.);
#69418=ORIENTED_EDGE('',*,*,#49221,.F.);
#69419=ORIENTED_EDGE('',*,*,#49222,.F.);
#69420=ORIENTED_EDGE('',*,*,#49218,.T.);
#69421=ORIENTED_EDGE('',*,*,#49223,.T.);
#69422=ORIENTED_EDGE('',*,*,#49224,.F.);
#69423=ORIENTED_EDGE('',*,*,#49225,.F.);
#69424=ORIENTED_EDGE('',*,*,#49221,.T.);
#69425=ORIENTED_EDGE('',*,*,#49226,.T.);
#69426=ORIENTED_EDGE('',*,*,#49227,.F.);
#69427=ORIENTED_EDGE('',*,*,#49228,.F.);
#69428=ORIENTED_EDGE('',*,*,#49224,.T.);
#69429=ORIENTED_EDGE('',*,*,#49229,.T.);
#69430=ORIENTED_EDGE('',*,*,#49230,.F.);
#69431=ORIENTED_EDGE('',*,*,#49231,.F.);
#69432=ORIENTED_EDGE('',*,*,#49227,.T.);
#69433=ORIENTED_EDGE('',*,*,#49232,.T.);
#69434=ORIENTED_EDGE('',*,*,#49233,.F.);
#69435=ORIENTED_EDGE('',*,*,#49234,.F.);
#69436=ORIENTED_EDGE('',*,*,#49230,.T.);
#69437=ORIENTED_EDGE('',*,*,#49235,.T.);
#69438=ORIENTED_EDGE('',*,*,#49236,.F.);
#69439=ORIENTED_EDGE('',*,*,#49237,.F.);
#69440=ORIENTED_EDGE('',*,*,#49233,.T.);
#69441=ORIENTED_EDGE('',*,*,#49238,.T.);
#69442=ORIENTED_EDGE('',*,*,#49239,.F.);
#69443=ORIENTED_EDGE('',*,*,#49240,.F.);
#69444=ORIENTED_EDGE('',*,*,#49236,.T.);
#69445=ORIENTED_EDGE('',*,*,#49241,.T.);
#69446=ORIENTED_EDGE('',*,*,#49242,.F.);
#69447=ORIENTED_EDGE('',*,*,#49243,.T.);
#69448=ORIENTED_EDGE('',*,*,#49244,.T.);
#69449=ORIENTED_EDGE('',*,*,#49245,.F.);
#69450=ORIENTED_EDGE('',*,*,#49246,.F.);
#69451=ORIENTED_EDGE('',*,*,#49247,.T.);
#69452=ORIENTED_EDGE('',*,*,#49242,.T.);
#69453=ORIENTED_EDGE('',*,*,#49248,.F.);
#69454=ORIENTED_EDGE('',*,*,#49249,.F.);
#69455=ORIENTED_EDGE('',*,*,#49250,.T.);
#69456=ORIENTED_EDGE('',*,*,#49246,.T.);
#69457=ORIENTED_EDGE('',*,*,#49251,.F.);
#69458=ORIENTED_EDGE('',*,*,#49252,.F.);
#69459=ORIENTED_EDGE('',*,*,#49253,.T.);
#69460=ORIENTED_EDGE('',*,*,#49249,.T.);
#69461=ORIENTED_EDGE('',*,*,#49254,.F.);
#69462=ORIENTED_EDGE('',*,*,#49255,.F.);
#69463=ORIENTED_EDGE('',*,*,#49256,.T.);
#69464=ORIENTED_EDGE('',*,*,#49252,.T.);
#69465=ORIENTED_EDGE('',*,*,#49257,.F.);
#69466=ORIENTED_EDGE('',*,*,#49258,.F.);
#69467=ORIENTED_EDGE('',*,*,#49259,.T.);
#69468=ORIENTED_EDGE('',*,*,#49255,.T.);
#69469=ORIENTED_EDGE('',*,*,#49260,.F.);
#69470=ORIENTED_EDGE('',*,*,#49261,.F.);
#69471=ORIENTED_EDGE('',*,*,#49262,.T.);
#69472=ORIENTED_EDGE('',*,*,#49258,.T.);
#69473=ORIENTED_EDGE('',*,*,#49263,.F.);
#69474=ORIENTED_EDGE('',*,*,#49264,.F.);
#69475=ORIENTED_EDGE('',*,*,#49265,.T.);
#69476=ORIENTED_EDGE('',*,*,#49261,.T.);
#69477=ORIENTED_EDGE('',*,*,#49266,.F.);
#69478=ORIENTED_EDGE('',*,*,#49267,.F.);
#69479=ORIENTED_EDGE('',*,*,#49268,.T.);
#69480=ORIENTED_EDGE('',*,*,#49264,.T.);
#69481=ORIENTED_EDGE('',*,*,#49269,.F.);
#69482=ORIENTED_EDGE('',*,*,#49270,.F.);
#69483=ORIENTED_EDGE('',*,*,#49271,.T.);
#69484=ORIENTED_EDGE('',*,*,#49267,.T.);
#69485=ORIENTED_EDGE('',*,*,#49272,.F.);
#69486=ORIENTED_EDGE('',*,*,#49273,.F.);
#69487=ORIENTED_EDGE('',*,*,#49274,.T.);
#69488=ORIENTED_EDGE('',*,*,#49270,.T.);
#69489=ORIENTED_EDGE('',*,*,#49275,.F.);
#69490=ORIENTED_EDGE('',*,*,#49276,.F.);
#69491=ORIENTED_EDGE('',*,*,#49277,.T.);
#69492=ORIENTED_EDGE('',*,*,#49273,.T.);
#69493=ORIENTED_EDGE('',*,*,#49278,.F.);
#69494=ORIENTED_EDGE('',*,*,#49279,.F.);
#69495=ORIENTED_EDGE('',*,*,#49280,.T.);
#69496=ORIENTED_EDGE('',*,*,#49276,.T.);
#69497=ORIENTED_EDGE('',*,*,#49281,.F.);
#69498=ORIENTED_EDGE('',*,*,#49282,.F.);
#69499=ORIENTED_EDGE('',*,*,#49283,.T.);
#69500=ORIENTED_EDGE('',*,*,#49279,.T.);
#69501=ORIENTED_EDGE('',*,*,#49284,.F.);
#69502=ORIENTED_EDGE('',*,*,#49285,.F.);
#69503=ORIENTED_EDGE('',*,*,#49286,.T.);
#69504=ORIENTED_EDGE('',*,*,#49282,.T.);
#69505=ORIENTED_EDGE('',*,*,#49287,.F.);
#69506=ORIENTED_EDGE('',*,*,#49288,.F.);
#69507=ORIENTED_EDGE('',*,*,#49289,.T.);
#69508=ORIENTED_EDGE('',*,*,#49290,.F.);
#69509=ORIENTED_EDGE('',*,*,#49291,.F.);
#69510=ORIENTED_EDGE('',*,*,#49292,.F.);
#69511=ORIENTED_EDGE('',*,*,#49293,.T.);
#69512=ORIENTED_EDGE('',*,*,#49294,.T.);
#69513=ORIENTED_EDGE('',*,*,#49293,.F.);
#69514=ORIENTED_EDGE('',*,*,#49198,.T.);
#69515=ORIENTED_EDGE('',*,*,#49195,.T.);
#69516=ORIENTED_EDGE('',*,*,#49295,.T.);
#69517=ORIENTED_EDGE('',*,*,#49296,.F.);
#69518=ORIENTED_EDGE('',*,*,#49297,.T.);
#69519=ORIENTED_EDGE('',*,*,#49298,.T.);
#69520=ORIENTED_EDGE('',*,*,#49299,.F.);
#69521=ORIENTED_EDGE('',*,*,#49298,.F.);
#69522=ORIENTED_EDGE('',*,*,#49300,.T.);
#69523=ORIENTED_EDGE('',*,*,#49285,.T.);
#69524=ORIENTED_EDGE('',*,*,#49301,.F.);
#69525=ORIENTED_EDGE('',*,*,#49296,.T.);
#69526=ORIENTED_EDGE('',*,*,#49302,.T.);
#69527=ORIENTED_EDGE('',*,*,#49299,.T.);
#69528=ORIENTED_EDGE('',*,*,#49292,.T.);
#69529=ORIENTED_EDGE('',*,*,#49244,.F.);
#69530=ORIENTED_EDGE('',*,*,#49303,.F.);
#69531=ORIENTED_EDGE('',*,*,#49304,.F.);
#69532=ORIENTED_EDGE('',*,*,#49305,.F.);
#69533=ORIENTED_EDGE('',*,*,#49294,.F.);
#69534=ORIENTED_EDGE('',*,*,#49290,.T.);
#69535=ORIENTED_EDGE('',*,*,#49291,.T.);
#69536=ORIENTED_EDGE('',*,*,#49306,.F.);
#69537=ORIENTED_EDGE('',*,*,#49307,.F.);
#69538=ORIENTED_EDGE('',*,*,#49308,.F.);
#69539=ORIENTED_EDGE('',*,*,#49289,.F.);
#69540=ORIENTED_EDGE('',*,*,#49309,.F.);
#69541=ORIENTED_EDGE('',*,*,#49310,.F.);
#69542=ORIENTED_EDGE('',*,*,#49308,.T.);
#69543=ORIENTED_EDGE('',*,*,#49311,.F.);
#69544=ORIENTED_EDGE('',*,*,#49307,.T.);
#69545=ORIENTED_EDGE('',*,*,#49312,.F.);
#69546=ORIENTED_EDGE('',*,*,#49306,.T.);
#69547=ORIENTED_EDGE('',*,*,#49313,.F.);
#69548=ORIENTED_EDGE('',*,*,#49310,.T.);
#69549=ORIENTED_EDGE('',*,*,#49314,.F.);
#69550=ORIENTED_EDGE('',*,*,#49309,.T.);
#69551=ORIENTED_EDGE('',*,*,#49315,.F.);
#69552=ORIENTED_EDGE('',*,*,#49316,.T.);
#69553=ORIENTED_EDGE('',*,*,#49317,.T.);
#69554=ORIENTED_EDGE('',*,*,#49318,.T.);
#69555=ORIENTED_EDGE('',*,*,#49319,.T.);
#69556=ORIENTED_EDGE('',*,*,#49320,.T.);
#69557=ORIENTED_EDGE('',*,*,#49321,.T.);
#69558=ORIENTED_EDGE('',*,*,#49322,.T.);
#69559=ORIENTED_EDGE('',*,*,#49288,.T.);
#69560=ORIENTED_EDGE('',*,*,#49323,.F.);
#69561=ORIENTED_EDGE('',*,*,#49317,.F.);
#69562=ORIENTED_EDGE('',*,*,#49323,.T.);
#69563=ORIENTED_EDGE('',*,*,#49311,.T.);
#69564=ORIENTED_EDGE('',*,*,#49324,.F.);
#69565=ORIENTED_EDGE('',*,*,#49318,.F.);
#69566=ORIENTED_EDGE('',*,*,#49324,.T.);
#69567=ORIENTED_EDGE('',*,*,#49312,.T.);
#69568=ORIENTED_EDGE('',*,*,#49325,.F.);
#69569=ORIENTED_EDGE('',*,*,#49319,.F.);
#69570=ORIENTED_EDGE('',*,*,#49325,.T.);
#69571=ORIENTED_EDGE('',*,*,#49313,.T.);
#69572=ORIENTED_EDGE('',*,*,#49326,.F.);
#69573=ORIENTED_EDGE('',*,*,#49320,.F.);
#69574=ORIENTED_EDGE('',*,*,#49326,.T.);
#69575=ORIENTED_EDGE('',*,*,#49314,.T.);
#69576=ORIENTED_EDGE('',*,*,#49327,.F.);
#69577=ORIENTED_EDGE('',*,*,#49321,.F.);
#69578=ORIENTED_EDGE('',*,*,#49327,.T.);
#69579=ORIENTED_EDGE('',*,*,#49315,.T.);
#69580=ORIENTED_EDGE('',*,*,#49322,.F.);
#69581=ORIENTED_EDGE('',*,*,#49316,.F.);
#69582=ORIENTED_EDGE('',*,*,#49305,.T.);
#69583=ORIENTED_EDGE('',*,*,#49328,.F.);
#69584=ORIENTED_EDGE('',*,*,#49241,.F.);
#69585=ORIENTED_EDGE('',*,*,#49238,.F.);
#69586=ORIENTED_EDGE('',*,*,#49235,.F.);
#69587=ORIENTED_EDGE('',*,*,#49232,.F.);
#69588=ORIENTED_EDGE('',*,*,#49229,.F.);
#69589=ORIENTED_EDGE('',*,*,#49226,.F.);
#69590=ORIENTED_EDGE('',*,*,#49223,.F.);
#69591=ORIENTED_EDGE('',*,*,#49220,.F.);
#69592=ORIENTED_EDGE('',*,*,#49217,.F.);
#69593=ORIENTED_EDGE('',*,*,#49214,.F.);
#69594=ORIENTED_EDGE('',*,*,#49211,.F.);
#69595=ORIENTED_EDGE('',*,*,#49208,.F.);
#69596=ORIENTED_EDGE('',*,*,#49205,.F.);
#69597=ORIENTED_EDGE('',*,*,#49202,.F.);
#69598=ORIENTED_EDGE('',*,*,#49199,.F.);
#69599=ORIENTED_EDGE('',*,*,#49300,.F.);
#69600=ORIENTED_EDGE('',*,*,#49297,.F.);
#69601=ORIENTED_EDGE('',*,*,#49301,.T.);
#69602=ORIENTED_EDGE('',*,*,#49287,.T.);
#69603=ORIENTED_EDGE('',*,*,#49284,.T.);
#69604=ORIENTED_EDGE('',*,*,#49281,.T.);
#69605=ORIENTED_EDGE('',*,*,#49278,.T.);
#69606=ORIENTED_EDGE('',*,*,#49275,.T.);
#69607=ORIENTED_EDGE('',*,*,#49272,.T.);
#69608=ORIENTED_EDGE('',*,*,#49269,.T.);
#69609=ORIENTED_EDGE('',*,*,#49266,.T.);
#69610=ORIENTED_EDGE('',*,*,#49263,.T.);
#69611=ORIENTED_EDGE('',*,*,#49260,.T.);
#69612=ORIENTED_EDGE('',*,*,#49257,.T.);
#69613=ORIENTED_EDGE('',*,*,#49254,.T.);
#69614=ORIENTED_EDGE('',*,*,#49251,.T.);
#69615=ORIENTED_EDGE('',*,*,#49248,.T.);
#69616=ORIENTED_EDGE('',*,*,#49245,.T.);
#69617=ORIENTED_EDGE('',*,*,#49239,.T.);
#69618=ORIENTED_EDGE('',*,*,#49328,.T.);
#69619=ORIENTED_EDGE('',*,*,#49304,.T.);
#69620=ORIENTED_EDGE('',*,*,#49329,.F.);
#69621=ORIENTED_EDGE('',*,*,#49303,.T.);
#69622=ORIENTED_EDGE('',*,*,#49243,.F.);
#69623=ORIENTED_EDGE('',*,*,#49247,.F.);
#69624=ORIENTED_EDGE('',*,*,#49250,.F.);
#69625=ORIENTED_EDGE('',*,*,#49253,.F.);
#69626=ORIENTED_EDGE('',*,*,#49256,.F.);
#69627=ORIENTED_EDGE('',*,*,#49259,.F.);
#69628=ORIENTED_EDGE('',*,*,#49262,.F.);
#69629=ORIENTED_EDGE('',*,*,#49265,.F.);
#69630=ORIENTED_EDGE('',*,*,#49268,.F.);
#69631=ORIENTED_EDGE('',*,*,#49271,.F.);
#69632=ORIENTED_EDGE('',*,*,#49274,.F.);
#69633=ORIENTED_EDGE('',*,*,#49277,.F.);
#69634=ORIENTED_EDGE('',*,*,#49280,.F.);
#69635=ORIENTED_EDGE('',*,*,#49283,.F.);
#69636=ORIENTED_EDGE('',*,*,#49286,.F.);
#69637=ORIENTED_EDGE('',*,*,#49302,.F.);
#69638=ORIENTED_EDGE('',*,*,#49295,.F.);
#69639=ORIENTED_EDGE('',*,*,#49194,.T.);
#69640=ORIENTED_EDGE('',*,*,#49197,.T.);
#69641=ORIENTED_EDGE('',*,*,#49201,.T.);
#69642=ORIENTED_EDGE('',*,*,#49204,.T.);
#69643=ORIENTED_EDGE('',*,*,#49207,.T.);
#69644=ORIENTED_EDGE('',*,*,#49210,.T.);
#69645=ORIENTED_EDGE('',*,*,#49213,.T.);
#69646=ORIENTED_EDGE('',*,*,#49216,.T.);
#69647=ORIENTED_EDGE('',*,*,#49219,.T.);
#69648=ORIENTED_EDGE('',*,*,#49222,.T.);
#69649=ORIENTED_EDGE('',*,*,#49225,.T.);
#69650=ORIENTED_EDGE('',*,*,#49228,.T.);
#69651=ORIENTED_EDGE('',*,*,#49231,.T.);
#69652=ORIENTED_EDGE('',*,*,#49234,.T.);
#69653=ORIENTED_EDGE('',*,*,#49237,.T.);
#69654=ORIENTED_EDGE('',*,*,#49240,.T.);
#69655=ORIENTED_EDGE('',*,*,#49329,.T.);
#69656=ORIENTED_EDGE('',*,*,#49330,.F.);
#69657=ORIENTED_EDGE('',*,*,#49331,.T.);
#69658=ORIENTED_EDGE('',*,*,#49332,.T.);
#69659=ORIENTED_EDGE('',*,*,#49333,.F.);
#69660=ORIENTED_EDGE('',*,*,#49334,.F.);
#69661=ORIENTED_EDGE('',*,*,#49335,.T.);
#69662=ORIENTED_EDGE('',*,*,#49330,.T.);
#69663=ORIENTED_EDGE('',*,*,#49336,.F.);
#69664=ORIENTED_EDGE('',*,*,#49337,.F.);
#69665=ORIENTED_EDGE('',*,*,#49338,.T.);
#69666=ORIENTED_EDGE('',*,*,#49334,.T.);
#69667=ORIENTED_EDGE('',*,*,#49339,.F.);
#69668=ORIENTED_EDGE('',*,*,#49340,.F.);
#69669=ORIENTED_EDGE('',*,*,#49341,.T.);
#69670=ORIENTED_EDGE('',*,*,#49337,.T.);
#69671=ORIENTED_EDGE('',*,*,#49342,.F.);
#69672=ORIENTED_EDGE('',*,*,#49343,.F.);
#69673=ORIENTED_EDGE('',*,*,#49344,.T.);
#69674=ORIENTED_EDGE('',*,*,#49340,.T.);
#69675=ORIENTED_EDGE('',*,*,#49345,.F.);
#69676=ORIENTED_EDGE('',*,*,#49346,.F.);
#69677=ORIENTED_EDGE('',*,*,#49347,.T.);
#69678=ORIENTED_EDGE('',*,*,#49343,.T.);
#69679=ORIENTED_EDGE('',*,*,#49348,.F.);
#69680=ORIENTED_EDGE('',*,*,#49349,.F.);
#69681=ORIENTED_EDGE('',*,*,#49350,.T.);
#69682=ORIENTED_EDGE('',*,*,#49346,.T.);
#69683=ORIENTED_EDGE('',*,*,#49351,.F.);
#69684=ORIENTED_EDGE('',*,*,#49352,.F.);
#69685=ORIENTED_EDGE('',*,*,#49353,.T.);
#69686=ORIENTED_EDGE('',*,*,#49349,.T.);
#69687=ORIENTED_EDGE('',*,*,#49354,.F.);
#69688=ORIENTED_EDGE('',*,*,#49355,.F.);
#69689=ORIENTED_EDGE('',*,*,#49356,.T.);
#69690=ORIENTED_EDGE('',*,*,#49352,.T.);
#69691=ORIENTED_EDGE('',*,*,#49357,.F.);
#69692=ORIENTED_EDGE('',*,*,#49358,.F.);
#69693=ORIENTED_EDGE('',*,*,#49359,.T.);
#69694=ORIENTED_EDGE('',*,*,#49355,.T.);
#69695=ORIENTED_EDGE('',*,*,#49360,.F.);
#69696=ORIENTED_EDGE('',*,*,#49361,.F.);
#69697=ORIENTED_EDGE('',*,*,#49362,.T.);
#69698=ORIENTED_EDGE('',*,*,#49358,.T.);
#69699=ORIENTED_EDGE('',*,*,#49363,.F.);
#69700=ORIENTED_EDGE('',*,*,#49364,.F.);
#69701=ORIENTED_EDGE('',*,*,#49365,.T.);
#69702=ORIENTED_EDGE('',*,*,#49361,.T.);
#69703=ORIENTED_EDGE('',*,*,#49366,.F.);
#69704=ORIENTED_EDGE('',*,*,#49367,.F.);
#69705=ORIENTED_EDGE('',*,*,#49368,.T.);
#69706=ORIENTED_EDGE('',*,*,#49364,.T.);
#69707=ORIENTED_EDGE('',*,*,#49369,.F.);
#69708=ORIENTED_EDGE('',*,*,#49370,.F.);
#69709=ORIENTED_EDGE('',*,*,#49371,.T.);
#69710=ORIENTED_EDGE('',*,*,#49367,.T.);
#69711=ORIENTED_EDGE('',*,*,#49372,.F.);
#69712=ORIENTED_EDGE('',*,*,#49373,.F.);
#69713=ORIENTED_EDGE('',*,*,#49374,.F.);
#69714=ORIENTED_EDGE('',*,*,#49375,.T.);
#69715=ORIENTED_EDGE('',*,*,#49370,.T.);
#69716=ORIENTED_EDGE('',*,*,#49376,.F.);
#69717=ORIENTED_EDGE('',*,*,#49377,.F.);
#69718=ORIENTED_EDGE('',*,*,#49378,.F.);
#69719=ORIENTED_EDGE('',*,*,#49379,.T.);
#69720=ORIENTED_EDGE('',*,*,#49380,.T.);
#69721=ORIENTED_EDGE('',*,*,#49381,.F.);
#69722=ORIENTED_EDGE('',*,*,#49382,.F.);
#69723=ORIENTED_EDGE('',*,*,#49377,.T.);
#69724=ORIENTED_EDGE('',*,*,#49383,.T.);
#69725=ORIENTED_EDGE('',*,*,#49384,.F.);
#69726=ORIENTED_EDGE('',*,*,#49385,.F.);
#69727=ORIENTED_EDGE('',*,*,#49381,.T.);
#69728=ORIENTED_EDGE('',*,*,#49386,.T.);
#69729=ORIENTED_EDGE('',*,*,#49387,.F.);
#69730=ORIENTED_EDGE('',*,*,#49388,.F.);
#69731=ORIENTED_EDGE('',*,*,#49384,.T.);
#69732=ORIENTED_EDGE('',*,*,#49389,.T.);
#69733=ORIENTED_EDGE('',*,*,#49390,.F.);
#69734=ORIENTED_EDGE('',*,*,#49391,.F.);
#69735=ORIENTED_EDGE('',*,*,#49387,.T.);
#69736=ORIENTED_EDGE('',*,*,#49392,.T.);
#69737=ORIENTED_EDGE('',*,*,#49393,.F.);
#69738=ORIENTED_EDGE('',*,*,#49394,.F.);
#69739=ORIENTED_EDGE('',*,*,#49390,.T.);
#69740=ORIENTED_EDGE('',*,*,#49395,.T.);
#69741=ORIENTED_EDGE('',*,*,#49396,.F.);
#69742=ORIENTED_EDGE('',*,*,#49397,.F.);
#69743=ORIENTED_EDGE('',*,*,#49393,.T.);
#69744=ORIENTED_EDGE('',*,*,#49398,.T.);
#69745=ORIENTED_EDGE('',*,*,#49399,.F.);
#69746=ORIENTED_EDGE('',*,*,#49400,.F.);
#69747=ORIENTED_EDGE('',*,*,#49396,.T.);
#69748=ORIENTED_EDGE('',*,*,#49401,.T.);
#69749=ORIENTED_EDGE('',*,*,#49402,.F.);
#69750=ORIENTED_EDGE('',*,*,#49403,.F.);
#69751=ORIENTED_EDGE('',*,*,#49399,.T.);
#69752=ORIENTED_EDGE('',*,*,#49404,.T.);
#69753=ORIENTED_EDGE('',*,*,#49405,.F.);
#69754=ORIENTED_EDGE('',*,*,#49406,.F.);
#69755=ORIENTED_EDGE('',*,*,#49402,.T.);
#69756=ORIENTED_EDGE('',*,*,#49407,.T.);
#69757=ORIENTED_EDGE('',*,*,#49408,.F.);
#69758=ORIENTED_EDGE('',*,*,#49409,.F.);
#69759=ORIENTED_EDGE('',*,*,#49405,.T.);
#69760=ORIENTED_EDGE('',*,*,#49410,.T.);
#69761=ORIENTED_EDGE('',*,*,#49411,.F.);
#69762=ORIENTED_EDGE('',*,*,#49412,.F.);
#69763=ORIENTED_EDGE('',*,*,#49408,.T.);
#69764=ORIENTED_EDGE('',*,*,#49413,.T.);
#69765=ORIENTED_EDGE('',*,*,#49414,.F.);
#69766=ORIENTED_EDGE('',*,*,#49415,.F.);
#69767=ORIENTED_EDGE('',*,*,#49411,.T.);
#69768=ORIENTED_EDGE('',*,*,#49416,.T.);
#69769=ORIENTED_EDGE('',*,*,#49417,.F.);
#69770=ORIENTED_EDGE('',*,*,#49418,.F.);
#69771=ORIENTED_EDGE('',*,*,#49414,.T.);
#69772=ORIENTED_EDGE('',*,*,#49419,.T.);
#69773=ORIENTED_EDGE('',*,*,#49374,.T.);
#69774=ORIENTED_EDGE('',*,*,#49420,.T.);
#69775=ORIENTED_EDGE('',*,*,#49421,.T.);
#69776=ORIENTED_EDGE('',*,*,#49379,.F.);
#69777=ORIENTED_EDGE('',*,*,#49422,.T.);
#69778=ORIENTED_EDGE('',*,*,#49423,.T.);
#69779=ORIENTED_EDGE('',*,*,#49424,.F.);
#69780=ORIENTED_EDGE('',*,*,#49423,.F.);
#69781=ORIENTED_EDGE('',*,*,#49425,.T.);
#69782=ORIENTED_EDGE('',*,*,#49417,.T.);
#69783=ORIENTED_EDGE('',*,*,#49426,.T.);
#69784=ORIENTED_EDGE('',*,*,#49427,.F.);
#69785=ORIENTED_EDGE('',*,*,#49428,.F.);
#69786=ORIENTED_EDGE('',*,*,#49429,.T.);
#69787=ORIENTED_EDGE('',*,*,#49430,.F.);
#69788=ORIENTED_EDGE('',*,*,#49431,.F.);
#69789=ORIENTED_EDGE('',*,*,#49432,.T.);
#69790=ORIENTED_EDGE('',*,*,#49433,.T.);
#69791=ORIENTED_EDGE('',*,*,#49432,.F.);
#69792=ORIENTED_EDGE('',*,*,#49433,.F.);
#69793=ORIENTED_EDGE('',*,*,#49434,.T.);
#69794=ORIENTED_EDGE('',*,*,#49435,.T.);
#69795=ORIENTED_EDGE('',*,*,#49436,.F.);
#69796=ORIENTED_EDGE('',*,*,#49427,.T.);
#69797=ORIENTED_EDGE('',*,*,#49437,.F.);
#69798=ORIENTED_EDGE('',*,*,#49438,.T.);
#69799=ORIENTED_EDGE('',*,*,#49434,.F.);
#69800=ORIENTED_EDGE('',*,*,#49431,.T.);
#69801=ORIENTED_EDGE('',*,*,#49439,.T.);
#69802=ORIENTED_EDGE('',*,*,#49440,.T.);
#69803=ORIENTED_EDGE('',*,*,#49441,.T.);
#69804=ORIENTED_EDGE('',*,*,#49442,.T.);
#69805=ORIENTED_EDGE('',*,*,#49443,.T.);
#69806=ORIENTED_EDGE('',*,*,#49430,.T.);
#69807=ORIENTED_EDGE('',*,*,#49444,.F.);
#69808=ORIENTED_EDGE('',*,*,#49435,.F.);
#69809=ORIENTED_EDGE('',*,*,#49438,.F.);
#69810=ORIENTED_EDGE('',*,*,#49445,.F.);
#69811=ORIENTED_EDGE('',*,*,#49332,.F.);
#69812=ORIENTED_EDGE('',*,*,#49446,.T.);
#69813=ORIENTED_EDGE('',*,*,#49441,.F.);
#69814=ORIENTED_EDGE('',*,*,#49447,.T.);
#69815=ORIENTED_EDGE('',*,*,#49440,.F.);
#69816=ORIENTED_EDGE('',*,*,#49448,.T.);
#69817=ORIENTED_EDGE('',*,*,#49439,.F.);
#69818=ORIENTED_EDGE('',*,*,#49449,.T.);
#69819=ORIENTED_EDGE('',*,*,#49443,.F.);
#69820=ORIENTED_EDGE('',*,*,#49450,.T.);
#69821=ORIENTED_EDGE('',*,*,#49442,.F.);
#69822=ORIENTED_EDGE('',*,*,#49451,.T.);
#69823=ORIENTED_EDGE('',*,*,#49452,.T.);
#69824=ORIENTED_EDGE('',*,*,#49453,.T.);
#69825=ORIENTED_EDGE('',*,*,#49454,.T.);
#69826=ORIENTED_EDGE('',*,*,#49455,.T.);
#69827=ORIENTED_EDGE('',*,*,#49456,.T.);
#69828=ORIENTED_EDGE('',*,*,#49446,.F.);
#69829=ORIENTED_EDGE('',*,*,#49457,.F.);
#69830=ORIENTED_EDGE('',*,*,#49452,.F.);
#69831=ORIENTED_EDGE('',*,*,#49458,.T.);
#69832=ORIENTED_EDGE('',*,*,#49447,.F.);
#69833=ORIENTED_EDGE('',*,*,#49459,.F.);
#69834=ORIENTED_EDGE('',*,*,#49453,.F.);
#69835=ORIENTED_EDGE('',*,*,#49457,.T.);
#69836=ORIENTED_EDGE('',*,*,#49448,.F.);
#69837=ORIENTED_EDGE('',*,*,#49460,.F.);
#69838=ORIENTED_EDGE('',*,*,#49454,.F.);
#69839=ORIENTED_EDGE('',*,*,#49459,.T.);
#69840=ORIENTED_EDGE('',*,*,#49429,.F.);
#69841=ORIENTED_EDGE('',*,*,#49461,.F.);
#69842=ORIENTED_EDGE('',*,*,#49455,.F.);
#69843=ORIENTED_EDGE('',*,*,#49460,.T.);
#69844=ORIENTED_EDGE('',*,*,#49449,.F.);
#69845=ORIENTED_EDGE('',*,*,#49462,.F.);
#69846=ORIENTED_EDGE('',*,*,#49456,.F.);
#69847=ORIENTED_EDGE('',*,*,#49461,.T.);
#69848=ORIENTED_EDGE('',*,*,#49450,.F.);
#69849=ORIENTED_EDGE('',*,*,#49458,.F.);
#69850=ORIENTED_EDGE('',*,*,#49451,.F.);
#69851=ORIENTED_EDGE('',*,*,#49462,.T.);
#69852=ORIENTED_EDGE('',*,*,#49424,.T.);
#69853=ORIENTED_EDGE('',*,*,#49378,.T.);
#69854=ORIENTED_EDGE('',*,*,#49382,.T.);
#69855=ORIENTED_EDGE('',*,*,#49385,.T.);
#69856=ORIENTED_EDGE('',*,*,#49388,.T.);
#69857=ORIENTED_EDGE('',*,*,#49391,.T.);
#69858=ORIENTED_EDGE('',*,*,#49394,.T.);
#69859=ORIENTED_EDGE('',*,*,#49397,.T.);
#69860=ORIENTED_EDGE('',*,*,#49400,.T.);
#69861=ORIENTED_EDGE('',*,*,#49403,.T.);
#69862=ORIENTED_EDGE('',*,*,#49406,.T.);
#69863=ORIENTED_EDGE('',*,*,#49409,.T.);
#69864=ORIENTED_EDGE('',*,*,#49412,.T.);
#69865=ORIENTED_EDGE('',*,*,#49415,.T.);
#69866=ORIENTED_EDGE('',*,*,#49418,.T.);
#69867=ORIENTED_EDGE('',*,*,#49428,.T.);
#69868=ORIENTED_EDGE('',*,*,#49436,.T.);
#69869=ORIENTED_EDGE('',*,*,#49444,.T.);
#69870=ORIENTED_EDGE('',*,*,#49331,.F.);
#69871=ORIENTED_EDGE('',*,*,#49335,.F.);
#69872=ORIENTED_EDGE('',*,*,#49338,.F.);
#69873=ORIENTED_EDGE('',*,*,#49341,.F.);
#69874=ORIENTED_EDGE('',*,*,#49344,.F.);
#69875=ORIENTED_EDGE('',*,*,#49347,.F.);
#69876=ORIENTED_EDGE('',*,*,#49350,.F.);
#69877=ORIENTED_EDGE('',*,*,#49353,.F.);
#69878=ORIENTED_EDGE('',*,*,#49356,.F.);
#69879=ORIENTED_EDGE('',*,*,#49359,.F.);
#69880=ORIENTED_EDGE('',*,*,#49362,.F.);
#69881=ORIENTED_EDGE('',*,*,#49365,.F.);
#69882=ORIENTED_EDGE('',*,*,#49368,.F.);
#69883=ORIENTED_EDGE('',*,*,#49371,.F.);
#69884=ORIENTED_EDGE('',*,*,#49375,.F.);
#69885=ORIENTED_EDGE('',*,*,#49425,.F.);
#69886=ORIENTED_EDGE('',*,*,#49422,.F.);
#69887=ORIENTED_EDGE('',*,*,#49373,.T.);
#69888=ORIENTED_EDGE('',*,*,#49463,.F.);
#69889=ORIENTED_EDGE('',*,*,#49420,.F.);
#69890=ORIENTED_EDGE('',*,*,#49445,.T.);
#69891=ORIENTED_EDGE('',*,*,#49437,.T.);
#69892=ORIENTED_EDGE('',*,*,#49426,.F.);
#69893=ORIENTED_EDGE('',*,*,#49419,.F.);
#69894=ORIENTED_EDGE('',*,*,#49416,.F.);
#69895=ORIENTED_EDGE('',*,*,#49413,.F.);
#69896=ORIENTED_EDGE('',*,*,#49410,.F.);
#69897=ORIENTED_EDGE('',*,*,#49407,.F.);
#69898=ORIENTED_EDGE('',*,*,#49404,.F.);
#69899=ORIENTED_EDGE('',*,*,#49401,.F.);
#69900=ORIENTED_EDGE('',*,*,#49398,.F.);
#69901=ORIENTED_EDGE('',*,*,#49395,.F.);
#69902=ORIENTED_EDGE('',*,*,#49392,.F.);
#69903=ORIENTED_EDGE('',*,*,#49389,.F.);
#69904=ORIENTED_EDGE('',*,*,#49386,.F.);
#69905=ORIENTED_EDGE('',*,*,#49383,.F.);
#69906=ORIENTED_EDGE('',*,*,#49380,.F.);
#69907=ORIENTED_EDGE('',*,*,#49421,.F.);
#69908=ORIENTED_EDGE('',*,*,#49463,.T.);
#69909=ORIENTED_EDGE('',*,*,#49376,.T.);
#69910=ORIENTED_EDGE('',*,*,#49372,.T.);
#69911=ORIENTED_EDGE('',*,*,#49369,.T.);
#69912=ORIENTED_EDGE('',*,*,#49366,.T.);
#69913=ORIENTED_EDGE('',*,*,#49363,.T.);
#69914=ORIENTED_EDGE('',*,*,#49360,.T.);
#69915=ORIENTED_EDGE('',*,*,#49357,.T.);
#69916=ORIENTED_EDGE('',*,*,#49354,.T.);
#69917=ORIENTED_EDGE('',*,*,#49351,.T.);
#69918=ORIENTED_EDGE('',*,*,#49348,.T.);
#69919=ORIENTED_EDGE('',*,*,#49345,.T.);
#69920=ORIENTED_EDGE('',*,*,#49342,.T.);
#69921=ORIENTED_EDGE('',*,*,#49339,.T.);
#69922=ORIENTED_EDGE('',*,*,#49336,.T.);
#69923=ORIENTED_EDGE('',*,*,#49333,.T.);
#69924=ORIENTED_EDGE('',*,*,#49464,.F.);
#69925=ORIENTED_EDGE('',*,*,#49465,.F.);
#69926=ORIENTED_EDGE('',*,*,#49466,.T.);
#69927=ORIENTED_EDGE('',*,*,#49467,.F.);
#69928=ORIENTED_EDGE('',*,*,#49468,.F.);
#69929=ORIENTED_EDGE('',*,*,#49464,.T.);
#69930=ORIENTED_EDGE('',*,*,#49469,.T.);
#69931=ORIENTED_EDGE('',*,*,#49470,.F.);
#69932=ORIENTED_EDGE('',*,*,#49471,.F.);
#69933=ORIENTED_EDGE('',*,*,#49467,.T.);
#69934=ORIENTED_EDGE('',*,*,#49472,.T.);
#69935=ORIENTED_EDGE('',*,*,#49473,.F.);
#69936=ORIENTED_EDGE('',*,*,#49474,.F.);
#69937=ORIENTED_EDGE('',*,*,#49470,.T.);
#69938=ORIENTED_EDGE('',*,*,#49475,.T.);
#69939=ORIENTED_EDGE('',*,*,#49476,.F.);
#69940=ORIENTED_EDGE('',*,*,#49477,.F.);
#69941=ORIENTED_EDGE('',*,*,#49473,.T.);
#69942=ORIENTED_EDGE('',*,*,#49478,.T.);
#69943=ORIENTED_EDGE('',*,*,#49479,.F.);
#69944=ORIENTED_EDGE('',*,*,#49480,.F.);
#69945=ORIENTED_EDGE('',*,*,#49476,.T.);
#69946=ORIENTED_EDGE('',*,*,#49481,.T.);
#69947=ORIENTED_EDGE('',*,*,#49482,.F.);
#69948=ORIENTED_EDGE('',*,*,#49483,.F.);
#69949=ORIENTED_EDGE('',*,*,#49479,.T.);
#69950=ORIENTED_EDGE('',*,*,#49484,.T.);
#69951=ORIENTED_EDGE('',*,*,#49485,.F.);
#69952=ORIENTED_EDGE('',*,*,#49486,.F.);
#69953=ORIENTED_EDGE('',*,*,#49482,.T.);
#69954=ORIENTED_EDGE('',*,*,#49487,.T.);
#69955=ORIENTED_EDGE('',*,*,#49488,.F.);
#69956=ORIENTED_EDGE('',*,*,#49489,.F.);
#69957=ORIENTED_EDGE('',*,*,#49485,.T.);
#69958=ORIENTED_EDGE('',*,*,#49490,.T.);
#69959=ORIENTED_EDGE('',*,*,#49491,.F.);
#69960=ORIENTED_EDGE('',*,*,#49492,.F.);
#69961=ORIENTED_EDGE('',*,*,#49488,.T.);
#69962=ORIENTED_EDGE('',*,*,#49493,.T.);
#69963=ORIENTED_EDGE('',*,*,#49494,.F.);
#69964=ORIENTED_EDGE('',*,*,#49495,.F.);
#69965=ORIENTED_EDGE('',*,*,#49491,.T.);
#69966=ORIENTED_EDGE('',*,*,#49496,.T.);
#69967=ORIENTED_EDGE('',*,*,#49497,.F.);
#69968=ORIENTED_EDGE('',*,*,#49498,.F.);
#69969=ORIENTED_EDGE('',*,*,#49494,.T.);
#69970=ORIENTED_EDGE('',*,*,#49499,.T.);
#69971=ORIENTED_EDGE('',*,*,#49500,.F.);
#69972=ORIENTED_EDGE('',*,*,#49501,.F.);
#69973=ORIENTED_EDGE('',*,*,#49497,.T.);
#69974=ORIENTED_EDGE('',*,*,#49502,.T.);
#69975=ORIENTED_EDGE('',*,*,#49503,.F.);
#69976=ORIENTED_EDGE('',*,*,#49504,.F.);
#69977=ORIENTED_EDGE('',*,*,#49500,.T.);
#69978=ORIENTED_EDGE('',*,*,#49505,.T.);
#69979=ORIENTED_EDGE('',*,*,#49506,.F.);
#69980=ORIENTED_EDGE('',*,*,#49507,.F.);
#69981=ORIENTED_EDGE('',*,*,#49503,.T.);
#69982=ORIENTED_EDGE('',*,*,#49508,.T.);
#69983=ORIENTED_EDGE('',*,*,#49509,.F.);
#69984=ORIENTED_EDGE('',*,*,#49510,.F.);
#69985=ORIENTED_EDGE('',*,*,#49506,.T.);
#69986=ORIENTED_EDGE('',*,*,#49511,.T.);
#69987=ORIENTED_EDGE('',*,*,#49512,.F.);
#69988=ORIENTED_EDGE('',*,*,#49513,.F.);
#69989=ORIENTED_EDGE('',*,*,#49509,.T.);
#69990=ORIENTED_EDGE('',*,*,#49514,.T.);
#69991=ORIENTED_EDGE('',*,*,#49515,.F.);
#69992=ORIENTED_EDGE('',*,*,#49516,.F.);
#69993=ORIENTED_EDGE('',*,*,#49512,.T.);
#69994=ORIENTED_EDGE('',*,*,#49517,.T.);
#69995=ORIENTED_EDGE('',*,*,#49518,.F.);
#69996=ORIENTED_EDGE('',*,*,#49519,.F.);
#69997=ORIENTED_EDGE('',*,*,#49515,.T.);
#69998=ORIENTED_EDGE('',*,*,#49520,.T.);
#69999=ORIENTED_EDGE('',*,*,#49521,.F.);
#70000=ORIENTED_EDGE('',*,*,#49522,.F.);
#70001=ORIENTED_EDGE('',*,*,#49518,.T.);
#70002=ORIENTED_EDGE('',*,*,#49523,.T.);
#70003=ORIENTED_EDGE('',*,*,#49524,.F.);
#70004=ORIENTED_EDGE('',*,*,#49525,.F.);
#70005=ORIENTED_EDGE('',*,*,#49521,.T.);
#70006=ORIENTED_EDGE('',*,*,#49526,.T.);
#70007=ORIENTED_EDGE('',*,*,#49527,.F.);
#70008=ORIENTED_EDGE('',*,*,#49528,.F.);
#70009=ORIENTED_EDGE('',*,*,#49524,.T.);
#70010=ORIENTED_EDGE('',*,*,#49529,.T.);
#70011=ORIENTED_EDGE('',*,*,#49530,.F.);
#70012=ORIENTED_EDGE('',*,*,#49531,.F.);
#70013=ORIENTED_EDGE('',*,*,#49527,.T.);
#70014=ORIENTED_EDGE('',*,*,#49532,.T.);
#70015=ORIENTED_EDGE('',*,*,#49533,.F.);
#70016=ORIENTED_EDGE('',*,*,#49534,.F.);
#70017=ORIENTED_EDGE('',*,*,#49530,.T.);
#70018=ORIENTED_EDGE('',*,*,#49535,.T.);
#70019=ORIENTED_EDGE('',*,*,#49536,.F.);
#70020=ORIENTED_EDGE('',*,*,#49537,.F.);
#70021=ORIENTED_EDGE('',*,*,#49533,.T.);
#70022=ORIENTED_EDGE('',*,*,#49538,.T.);
#70023=ORIENTED_EDGE('',*,*,#49539,.F.);
#70024=ORIENTED_EDGE('',*,*,#49540,.F.);
#70025=ORIENTED_EDGE('',*,*,#49536,.T.);
#70026=ORIENTED_EDGE('',*,*,#49541,.T.);
#70027=ORIENTED_EDGE('',*,*,#49542,.F.);
#70028=ORIENTED_EDGE('',*,*,#49543,.F.);
#70029=ORIENTED_EDGE('',*,*,#49539,.T.);
#70030=ORIENTED_EDGE('',*,*,#49544,.T.);
#70031=ORIENTED_EDGE('',*,*,#49545,.F.);
#70032=ORIENTED_EDGE('',*,*,#49546,.F.);
#70033=ORIENTED_EDGE('',*,*,#49542,.T.);
#70034=ORIENTED_EDGE('',*,*,#49547,.T.);
#70035=ORIENTED_EDGE('',*,*,#49548,.F.);
#70036=ORIENTED_EDGE('',*,*,#49549,.F.);
#70037=ORIENTED_EDGE('',*,*,#49545,.T.);
#70038=ORIENTED_EDGE('',*,*,#49550,.T.);
#70039=ORIENTED_EDGE('',*,*,#49551,.F.);
#70040=ORIENTED_EDGE('',*,*,#49552,.T.);
#70041=ORIENTED_EDGE('',*,*,#49553,.F.);
#70042=ORIENTED_EDGE('',*,*,#49554,.T.);
#70043=ORIENTED_EDGE('',*,*,#49555,.T.);
#70044=ORIENTED_EDGE('',*,*,#49554,.F.);
#70045=ORIENTED_EDGE('',*,*,#49556,.F.);
#70046=ORIENTED_EDGE('',*,*,#49557,.T.);
#70047=ORIENTED_EDGE('',*,*,#49558,.F.);
#70048=ORIENTED_EDGE('',*,*,#49559,.T.);
#70049=ORIENTED_EDGE('',*,*,#49551,.T.);
#70050=ORIENTED_EDGE('',*,*,#49560,.T.);
#70051=ORIENTED_EDGE('',*,*,#49561,.F.);
#70052=ORIENTED_EDGE('',*,*,#49562,.T.);
#70053=ORIENTED_EDGE('',*,*,#49558,.T.);
#70054=ORIENTED_EDGE('',*,*,#49563,.T.);
#70055=ORIENTED_EDGE('',*,*,#49564,.F.);
#70056=ORIENTED_EDGE('',*,*,#49565,.T.);
#70057=ORIENTED_EDGE('',*,*,#49561,.T.);
#70058=ORIENTED_EDGE('',*,*,#49566,.T.);
#70059=ORIENTED_EDGE('',*,*,#49567,.F.);
#70060=ORIENTED_EDGE('',*,*,#49568,.T.);
#70061=ORIENTED_EDGE('',*,*,#49564,.T.);
#70062=ORIENTED_EDGE('',*,*,#49569,.T.);
#70063=ORIENTED_EDGE('',*,*,#49570,.F.);
#70064=ORIENTED_EDGE('',*,*,#49571,.T.);
#70065=ORIENTED_EDGE('',*,*,#49567,.T.);
#70066=ORIENTED_EDGE('',*,*,#49572,.T.);
#70067=ORIENTED_EDGE('',*,*,#49573,.F.);
#70068=ORIENTED_EDGE('',*,*,#49574,.T.);
#70069=ORIENTED_EDGE('',*,*,#49570,.T.);
#70070=ORIENTED_EDGE('',*,*,#49575,.T.);
#70071=ORIENTED_EDGE('',*,*,#49576,.F.);
#70072=ORIENTED_EDGE('',*,*,#49577,.T.);
#70073=ORIENTED_EDGE('',*,*,#49573,.T.);
#70074=ORIENTED_EDGE('',*,*,#49578,.T.);
#70075=ORIENTED_EDGE('',*,*,#49579,.F.);
#70076=ORIENTED_EDGE('',*,*,#49580,.T.);
#70077=ORIENTED_EDGE('',*,*,#49576,.T.);
#70078=ORIENTED_EDGE('',*,*,#49581,.T.);
#70079=ORIENTED_EDGE('',*,*,#49582,.F.);
#70080=ORIENTED_EDGE('',*,*,#49583,.T.);
#70081=ORIENTED_EDGE('',*,*,#49579,.T.);
#70082=ORIENTED_EDGE('',*,*,#49584,.T.);
#70083=ORIENTED_EDGE('',*,*,#49585,.F.);
#70084=ORIENTED_EDGE('',*,*,#49586,.T.);
#70085=ORIENTED_EDGE('',*,*,#49582,.T.);
#70086=ORIENTED_EDGE('',*,*,#49587,.T.);
#70087=ORIENTED_EDGE('',*,*,#49588,.F.);
#70088=ORIENTED_EDGE('',*,*,#49589,.T.);
#70089=ORIENTED_EDGE('',*,*,#49585,.T.);
#70090=ORIENTED_EDGE('',*,*,#49590,.T.);
#70091=ORIENTED_EDGE('',*,*,#49591,.F.);
#70092=ORIENTED_EDGE('',*,*,#49592,.T.);
#70093=ORIENTED_EDGE('',*,*,#49588,.T.);
#70094=ORIENTED_EDGE('',*,*,#49593,.T.);
#70095=ORIENTED_EDGE('',*,*,#49594,.F.);
#70096=ORIENTED_EDGE('',*,*,#49595,.T.);
#70097=ORIENTED_EDGE('',*,*,#49591,.T.);
#70098=ORIENTED_EDGE('',*,*,#49596,.T.);
#70099=ORIENTED_EDGE('',*,*,#49597,.F.);
#70100=ORIENTED_EDGE('',*,*,#49598,.T.);
#70101=ORIENTED_EDGE('',*,*,#49594,.T.);
#70102=ORIENTED_EDGE('',*,*,#49599,.T.);
#70103=ORIENTED_EDGE('',*,*,#49600,.F.);
#70104=ORIENTED_EDGE('',*,*,#49601,.T.);
#70105=ORIENTED_EDGE('',*,*,#49597,.T.);
#70106=ORIENTED_EDGE('',*,*,#49602,.T.);
#70107=ORIENTED_EDGE('',*,*,#49603,.F.);
#70108=ORIENTED_EDGE('',*,*,#49604,.T.);
#70109=ORIENTED_EDGE('',*,*,#49600,.T.);
#70110=ORIENTED_EDGE('',*,*,#49605,.T.);
#70111=ORIENTED_EDGE('',*,*,#49606,.F.);
#70112=ORIENTED_EDGE('',*,*,#49607,.T.);
#70113=ORIENTED_EDGE('',*,*,#49603,.T.);
#70114=ORIENTED_EDGE('',*,*,#49608,.T.);
#70115=ORIENTED_EDGE('',*,*,#49609,.F.);
#70116=ORIENTED_EDGE('',*,*,#49610,.T.);
#70117=ORIENTED_EDGE('',*,*,#49606,.T.);
#70118=ORIENTED_EDGE('',*,*,#49611,.T.);
#70119=ORIENTED_EDGE('',*,*,#49612,.F.);
#70120=ORIENTED_EDGE('',*,*,#49613,.T.);
#70121=ORIENTED_EDGE('',*,*,#49609,.T.);
#70122=ORIENTED_EDGE('',*,*,#49614,.T.);
#70123=ORIENTED_EDGE('',*,*,#49615,.F.);
#70124=ORIENTED_EDGE('',*,*,#49616,.T.);
#70125=ORIENTED_EDGE('',*,*,#49612,.T.);
#70126=ORIENTED_EDGE('',*,*,#49617,.T.);
#70127=ORIENTED_EDGE('',*,*,#49618,.F.);
#70128=ORIENTED_EDGE('',*,*,#49619,.T.);
#70129=ORIENTED_EDGE('',*,*,#49615,.T.);
#70130=ORIENTED_EDGE('',*,*,#49620,.T.);
#70131=ORIENTED_EDGE('',*,*,#49621,.F.);
#70132=ORIENTED_EDGE('',*,*,#49622,.T.);
#70133=ORIENTED_EDGE('',*,*,#49618,.T.);
#70134=ORIENTED_EDGE('',*,*,#49623,.T.);
#70135=ORIENTED_EDGE('',*,*,#49624,.F.);
#70136=ORIENTED_EDGE('',*,*,#49625,.T.);
#70137=ORIENTED_EDGE('',*,*,#49621,.T.);
#70138=ORIENTED_EDGE('',*,*,#49626,.T.);
#70139=ORIENTED_EDGE('',*,*,#49627,.F.);
#70140=ORIENTED_EDGE('',*,*,#49628,.T.);
#70141=ORIENTED_EDGE('',*,*,#49624,.T.);
#70142=ORIENTED_EDGE('',*,*,#49629,.T.);
#70143=ORIENTED_EDGE('',*,*,#49630,.F.);
#70144=ORIENTED_EDGE('',*,*,#49631,.T.);
#70145=ORIENTED_EDGE('',*,*,#49627,.T.);
#70146=ORIENTED_EDGE('',*,*,#49632,.T.);
#70147=ORIENTED_EDGE('',*,*,#49633,.F.);
#70148=ORIENTED_EDGE('',*,*,#49634,.T.);
#70149=ORIENTED_EDGE('',*,*,#49630,.T.);
#70150=ORIENTED_EDGE('',*,*,#49635,.T.);
#70151=ORIENTED_EDGE('',*,*,#49636,.F.);
#70152=ORIENTED_EDGE('',*,*,#49637,.T.);
#70153=ORIENTED_EDGE('',*,*,#49633,.T.);
#70154=ORIENTED_EDGE('',*,*,#49638,.T.);
#70155=ORIENTED_EDGE('',*,*,#49639,.F.);
#70156=ORIENTED_EDGE('',*,*,#49640,.F.);
#70157=ORIENTED_EDGE('',*,*,#49641,.F.);
#70158=ORIENTED_EDGE('',*,*,#49642,.F.);
#70159=ORIENTED_EDGE('',*,*,#49643,.F.);
#70160=ORIENTED_EDGE('',*,*,#49644,.F.);
#70161=ORIENTED_EDGE('',*,*,#49645,.T.);
#70162=ORIENTED_EDGE('',*,*,#49643,.T.);
#70163=ORIENTED_EDGE('',*,*,#49646,.T.);
#70164=ORIENTED_EDGE('',*,*,#49647,.F.);
#70165=ORIENTED_EDGE('',*,*,#49648,.F.);
#70166=ORIENTED_EDGE('',*,*,#49649,.F.);
#70167=ORIENTED_EDGE('',*,*,#49639,.T.);
#70168=ORIENTED_EDGE('',*,*,#49650,.F.);
#70169=ORIENTED_EDGE('',*,*,#49556,.T.);
#70170=ORIENTED_EDGE('',*,*,#49553,.T.);
#70171=ORIENTED_EDGE('',*,*,#49636,.T.);
#70172=ORIENTED_EDGE('',*,*,#49651,.T.);
#70173=ORIENTED_EDGE('',*,*,#49648,.T.);
#70174=ORIENTED_EDGE('',*,*,#49652,.T.);
#70175=ORIENTED_EDGE('',*,*,#49555,.F.);
#70176=ORIENTED_EDGE('',*,*,#49653,.T.);
#70177=ORIENTED_EDGE('',*,*,#49654,.T.);
#70178=ORIENTED_EDGE('',*,*,#49653,.F.);
#70179=ORIENTED_EDGE('',*,*,#49655,.T.);
#70180=ORIENTED_EDGE('',*,*,#49656,.F.);
#70181=ORIENTED_EDGE('',*,*,#49657,.F.);
#70182=ORIENTED_EDGE('',*,*,#49658,.F.);
#70183=ORIENTED_EDGE('',*,*,#49659,.T.);
#70184=ORIENTED_EDGE('',*,*,#49660,.F.);
#70185=ORIENTED_EDGE('',*,*,#49661,.F.);
#70186=ORIENTED_EDGE('',*,*,#49655,.F.);
#70187=ORIENTED_EDGE('',*,*,#49662,.T.);
#70188=ORIENTED_EDGE('',*,*,#49663,.T.);
#70189=ORIENTED_EDGE('',*,*,#49664,.F.);
#70190=ORIENTED_EDGE('',*,*,#49665,.T.);
#70191=ORIENTED_EDGE('',*,*,#49666,.T.);
#70192=ORIENTED_EDGE('',*,*,#49665,.F.);
#70193=ORIENTED_EDGE('',*,*,#49667,.F.);
#70194=ORIENTED_EDGE('',*,*,#49668,.T.);
#70195=ORIENTED_EDGE('',*,*,#49664,.T.);
#70196=ORIENTED_EDGE('',*,*,#49668,.F.);
#70197=ORIENTED_EDGE('',*,*,#49669,.F.);
#70198=ORIENTED_EDGE('',*,*,#49670,.T.);
#70199=ORIENTED_EDGE('',*,*,#49667,.T.);
#70200=ORIENTED_EDGE('',*,*,#49670,.F.);
#70201=ORIENTED_EDGE('',*,*,#49671,.T.);
#70202=ORIENTED_EDGE('',*,*,#49672,.T.);
#70203=ORIENTED_EDGE('',*,*,#49673,.T.);
#70204=ORIENTED_EDGE('',*,*,#49674,.T.);
#70205=ORIENTED_EDGE('',*,*,#49675,.T.);
#70206=ORIENTED_EDGE('',*,*,#49676,.T.);
#70207=ORIENTED_EDGE('',*,*,#49677,.T.);
#70208=ORIENTED_EDGE('',*,*,#49678,.T.);
#70209=ORIENTED_EDGE('',*,*,#49679,.T.);
#70210=ORIENTED_EDGE('',*,*,#49680,.T.);
#70211=ORIENTED_EDGE('',*,*,#49681,.T.);
#70212=ORIENTED_EDGE('',*,*,#49682,.T.);
#70213=ORIENTED_EDGE('',*,*,#49683,.T.);
#70214=ORIENTED_EDGE('',*,*,#49684,.T.);
#70215=ORIENTED_EDGE('',*,*,#49685,.T.);
#70216=ORIENTED_EDGE('',*,*,#49686,.T.);
#70217=ORIENTED_EDGE('',*,*,#49687,.T.);
#70218=ORIENTED_EDGE('',*,*,#49688,.T.);
#70219=ORIENTED_EDGE('',*,*,#49689,.T.);
#70220=ORIENTED_EDGE('',*,*,#49690,.T.);
#70221=ORIENTED_EDGE('',*,*,#49691,.T.);
#70222=ORIENTED_EDGE('',*,*,#49692,.T.);
#70223=ORIENTED_EDGE('',*,*,#49693,.T.);
#70224=ORIENTED_EDGE('',*,*,#49694,.T.);
#70225=ORIENTED_EDGE('',*,*,#49695,.T.);
#70226=ORIENTED_EDGE('',*,*,#49696,.T.);
#70227=ORIENTED_EDGE('',*,*,#49697,.T.);
#70228=ORIENTED_EDGE('',*,*,#49698,.T.);
#70229=ORIENTED_EDGE('',*,*,#49699,.T.);
#70230=ORIENTED_EDGE('',*,*,#49700,.T.);
#70231=ORIENTED_EDGE('',*,*,#49701,.T.);
#70232=ORIENTED_EDGE('',*,*,#49702,.T.);
#70233=ORIENTED_EDGE('',*,*,#49703,.T.);
#70234=ORIENTED_EDGE('',*,*,#49704,.T.);
#70235=ORIENTED_EDGE('',*,*,#49705,.T.);
#70236=ORIENTED_EDGE('',*,*,#49706,.T.);
#70237=ORIENTED_EDGE('',*,*,#49707,.T.);
#70238=ORIENTED_EDGE('',*,*,#49708,.T.);
#70239=ORIENTED_EDGE('',*,*,#49709,.T.);
#70240=ORIENTED_EDGE('',*,*,#49710,.T.);
#70241=ORIENTED_EDGE('',*,*,#49711,.T.);
#70242=ORIENTED_EDGE('',*,*,#49712,.T.);
#70243=ORIENTED_EDGE('',*,*,#49713,.T.);
#70244=ORIENTED_EDGE('',*,*,#49714,.T.);
#70245=ORIENTED_EDGE('',*,*,#49715,.T.);
#70246=ORIENTED_EDGE('',*,*,#49716,.T.);
#70247=ORIENTED_EDGE('',*,*,#49717,.T.);
#70248=ORIENTED_EDGE('',*,*,#49718,.T.);
#70249=ORIENTED_EDGE('',*,*,#49719,.T.);
#70250=ORIENTED_EDGE('',*,*,#49720,.T.);
#70251=ORIENTED_EDGE('',*,*,#49721,.T.);
#70252=ORIENTED_EDGE('',*,*,#49722,.T.);
#70253=ORIENTED_EDGE('',*,*,#49723,.T.);
#70254=ORIENTED_EDGE('',*,*,#49724,.T.);
#70255=ORIENTED_EDGE('',*,*,#49725,.T.);
#70256=ORIENTED_EDGE('',*,*,#49726,.T.);
#70257=ORIENTED_EDGE('',*,*,#49727,.T.);
#70258=ORIENTED_EDGE('',*,*,#49728,.T.);
#70259=ORIENTED_EDGE('',*,*,#49729,.T.);
#70260=ORIENTED_EDGE('',*,*,#49730,.T.);
#70261=ORIENTED_EDGE('',*,*,#49731,.T.);
#70262=ORIENTED_EDGE('',*,*,#49732,.T.);
#70263=ORIENTED_EDGE('',*,*,#49733,.T.);
#70264=ORIENTED_EDGE('',*,*,#49734,.T.);
#70265=ORIENTED_EDGE('',*,*,#49735,.T.);
#70266=ORIENTED_EDGE('',*,*,#49736,.T.);
#70267=ORIENTED_EDGE('',*,*,#49737,.T.);
#70268=ORIENTED_EDGE('',*,*,#49738,.T.);
#70269=ORIENTED_EDGE('',*,*,#49739,.T.);
#70270=ORIENTED_EDGE('',*,*,#49740,.T.);
#70271=ORIENTED_EDGE('',*,*,#49741,.T.);
#70272=ORIENTED_EDGE('',*,*,#49742,.T.);
#70273=ORIENTED_EDGE('',*,*,#49743,.T.);
#70274=ORIENTED_EDGE('',*,*,#49744,.T.);
#70275=ORIENTED_EDGE('',*,*,#49745,.T.);
#70276=ORIENTED_EDGE('',*,*,#49746,.T.);
#70277=ORIENTED_EDGE('',*,*,#49747,.T.);
#70278=ORIENTED_EDGE('',*,*,#49748,.T.);
#70279=ORIENTED_EDGE('',*,*,#49749,.T.);
#70280=ORIENTED_EDGE('',*,*,#49750,.T.);
#70281=ORIENTED_EDGE('',*,*,#49751,.T.);
#70282=ORIENTED_EDGE('',*,*,#49752,.T.);
#70283=ORIENTED_EDGE('',*,*,#49753,.T.);
#70284=ORIENTED_EDGE('',*,*,#49754,.T.);
#70285=ORIENTED_EDGE('',*,*,#49755,.T.);
#70286=ORIENTED_EDGE('',*,*,#49756,.T.);
#70287=ORIENTED_EDGE('',*,*,#49757,.T.);
#70288=ORIENTED_EDGE('',*,*,#49758,.T.);
#70289=ORIENTED_EDGE('',*,*,#49759,.T.);
#70290=ORIENTED_EDGE('',*,*,#49760,.T.);
#70291=ORIENTED_EDGE('',*,*,#49761,.T.);
#70292=ORIENTED_EDGE('',*,*,#49762,.T.);
#70293=ORIENTED_EDGE('',*,*,#49763,.T.);
#70294=ORIENTED_EDGE('',*,*,#49764,.T.);
#70295=ORIENTED_EDGE('',*,*,#49765,.T.);
#70296=ORIENTED_EDGE('',*,*,#49766,.T.);
#70297=ORIENTED_EDGE('',*,*,#49767,.T.);
#70298=ORIENTED_EDGE('',*,*,#49768,.T.);
#70299=ORIENTED_EDGE('',*,*,#49769,.T.);
#70300=ORIENTED_EDGE('',*,*,#49770,.T.);
#70301=ORIENTED_EDGE('',*,*,#49771,.T.);
#70302=ORIENTED_EDGE('',*,*,#49772,.T.);
#70303=ORIENTED_EDGE('',*,*,#49773,.T.);
#70304=ORIENTED_EDGE('',*,*,#49774,.T.);
#70305=ORIENTED_EDGE('',*,*,#49775,.T.);
#70306=ORIENTED_EDGE('',*,*,#49776,.T.);
#70307=ORIENTED_EDGE('',*,*,#49777,.T.);
#70308=ORIENTED_EDGE('',*,*,#49778,.T.);
#70309=ORIENTED_EDGE('',*,*,#49779,.T.);
#70310=ORIENTED_EDGE('',*,*,#49780,.T.);
#70311=ORIENTED_EDGE('',*,*,#49781,.T.);
#70312=ORIENTED_EDGE('',*,*,#49782,.T.);
#70313=ORIENTED_EDGE('',*,*,#49783,.T.);
#70314=ORIENTED_EDGE('',*,*,#49784,.T.);
#70315=ORIENTED_EDGE('',*,*,#49785,.T.);
#70316=ORIENTED_EDGE('',*,*,#49786,.T.);
#70317=ORIENTED_EDGE('',*,*,#49787,.T.);
#70318=ORIENTED_EDGE('',*,*,#49788,.T.);
#70319=ORIENTED_EDGE('',*,*,#49789,.T.);
#70320=ORIENTED_EDGE('',*,*,#49790,.T.);
#70321=ORIENTED_EDGE('',*,*,#49791,.T.);
#70322=ORIENTED_EDGE('',*,*,#49792,.T.);
#70323=ORIENTED_EDGE('',*,*,#49793,.T.);
#70324=ORIENTED_EDGE('',*,*,#49794,.T.);
#70325=ORIENTED_EDGE('',*,*,#49795,.T.);
#70326=ORIENTED_EDGE('',*,*,#49796,.T.);
#70327=ORIENTED_EDGE('',*,*,#49797,.T.);
#70328=ORIENTED_EDGE('',*,*,#49798,.T.);
#70329=ORIENTED_EDGE('',*,*,#49799,.T.);
#70330=ORIENTED_EDGE('',*,*,#49800,.T.);
#70331=ORIENTED_EDGE('',*,*,#49801,.T.);
#70332=ORIENTED_EDGE('',*,*,#49802,.T.);
#70333=ORIENTED_EDGE('',*,*,#49803,.T.);
#70334=ORIENTED_EDGE('',*,*,#49804,.T.);
#70335=ORIENTED_EDGE('',*,*,#49805,.T.);
#70336=ORIENTED_EDGE('',*,*,#49806,.T.);
#70337=ORIENTED_EDGE('',*,*,#49807,.T.);
#70338=ORIENTED_EDGE('',*,*,#49808,.T.);
#70339=ORIENTED_EDGE('',*,*,#49809,.T.);
#70340=ORIENTED_EDGE('',*,*,#49810,.T.);
#70341=ORIENTED_EDGE('',*,*,#49811,.T.);
#70342=ORIENTED_EDGE('',*,*,#49812,.T.);
#70343=ORIENTED_EDGE('',*,*,#49813,.T.);
#70344=ORIENTED_EDGE('',*,*,#49814,.T.);
#70345=ORIENTED_EDGE('',*,*,#49815,.T.);
#70346=ORIENTED_EDGE('',*,*,#49816,.T.);
#70347=ORIENTED_EDGE('',*,*,#49817,.T.);
#70348=ORIENTED_EDGE('',*,*,#49818,.T.);
#70349=ORIENTED_EDGE('',*,*,#49819,.T.);
#70350=ORIENTED_EDGE('',*,*,#49820,.T.);
#70351=ORIENTED_EDGE('',*,*,#49821,.T.);
#70352=ORIENTED_EDGE('',*,*,#49822,.T.);
#70353=ORIENTED_EDGE('',*,*,#49823,.T.);
#70354=ORIENTED_EDGE('',*,*,#49824,.T.);
#70355=ORIENTED_EDGE('',*,*,#49825,.T.);
#70356=ORIENTED_EDGE('',*,*,#49826,.T.);
#70357=ORIENTED_EDGE('',*,*,#49827,.T.);
#70358=ORIENTED_EDGE('',*,*,#49828,.T.);
#70359=ORIENTED_EDGE('',*,*,#49829,.T.);
#70360=ORIENTED_EDGE('',*,*,#49830,.T.);
#70361=ORIENTED_EDGE('',*,*,#49831,.T.);
#70362=ORIENTED_EDGE('',*,*,#49832,.T.);
#70363=ORIENTED_EDGE('',*,*,#49833,.T.);
#70364=ORIENTED_EDGE('',*,*,#49834,.T.);
#70365=ORIENTED_EDGE('',*,*,#49835,.T.);
#70366=ORIENTED_EDGE('',*,*,#49836,.T.);
#70367=ORIENTED_EDGE('',*,*,#49837,.T.);
#70368=ORIENTED_EDGE('',*,*,#49838,.T.);
#70369=ORIENTED_EDGE('',*,*,#49839,.T.);
#70370=ORIENTED_EDGE('',*,*,#49840,.T.);
#70371=ORIENTED_EDGE('',*,*,#49841,.T.);
#70372=ORIENTED_EDGE('',*,*,#49842,.T.);
#70373=ORIENTED_EDGE('',*,*,#49843,.T.);
#70374=ORIENTED_EDGE('',*,*,#49844,.T.);
#70375=ORIENTED_EDGE('',*,*,#49845,.T.);
#70376=ORIENTED_EDGE('',*,*,#49846,.T.);
#70377=ORIENTED_EDGE('',*,*,#49847,.T.);
#70378=ORIENTED_EDGE('',*,*,#49848,.T.);
#70379=ORIENTED_EDGE('',*,*,#49849,.T.);
#70380=ORIENTED_EDGE('',*,*,#49850,.T.);
#70381=ORIENTED_EDGE('',*,*,#49851,.T.);
#70382=ORIENTED_EDGE('',*,*,#49852,.T.);
#70383=ORIENTED_EDGE('',*,*,#49853,.T.);
#70384=ORIENTED_EDGE('',*,*,#49854,.T.);
#70385=ORIENTED_EDGE('',*,*,#49855,.T.);
#70386=ORIENTED_EDGE('',*,*,#49856,.T.);
#70387=ORIENTED_EDGE('',*,*,#49857,.T.);
#70388=ORIENTED_EDGE('',*,*,#49858,.T.);
#70389=ORIENTED_EDGE('',*,*,#49859,.T.);
#70390=ORIENTED_EDGE('',*,*,#49860,.T.);
#70391=ORIENTED_EDGE('',*,*,#49861,.T.);
#70392=ORIENTED_EDGE('',*,*,#49862,.T.);
#70393=ORIENTED_EDGE('',*,*,#49863,.T.);
#70394=ORIENTED_EDGE('',*,*,#49864,.T.);
#70395=ORIENTED_EDGE('',*,*,#49865,.T.);
#70396=ORIENTED_EDGE('',*,*,#49866,.T.);
#70397=ORIENTED_EDGE('',*,*,#49867,.T.);
#70398=ORIENTED_EDGE('',*,*,#49868,.T.);
#70399=ORIENTED_EDGE('',*,*,#49869,.F.);
#70400=ORIENTED_EDGE('',*,*,#49870,.F.);
#70401=ORIENTED_EDGE('',*,*,#49868,.F.);
#70402=ORIENTED_EDGE('',*,*,#49871,.T.);
#70403=ORIENTED_EDGE('',*,*,#49872,.T.);
#70404=ORIENTED_EDGE('',*,*,#49873,.T.);
#70405=ORIENTED_EDGE('',*,*,#49874,.T.);
#70406=ORIENTED_EDGE('',*,*,#49875,.T.);
#70407=ORIENTED_EDGE('',*,*,#49876,.T.);
#70408=ORIENTED_EDGE('',*,*,#49877,.T.);
#70409=ORIENTED_EDGE('',*,*,#49878,.T.);
#70410=ORIENTED_EDGE('',*,*,#49879,.T.);
#70411=ORIENTED_EDGE('',*,*,#49880,.T.);
#70412=ORIENTED_EDGE('',*,*,#49881,.T.);
#70413=ORIENTED_EDGE('',*,*,#49882,.T.);
#70414=ORIENTED_EDGE('',*,*,#49883,.T.);
#70415=ORIENTED_EDGE('',*,*,#49884,.T.);
#70416=ORIENTED_EDGE('',*,*,#49885,.T.);
#70417=ORIENTED_EDGE('',*,*,#49886,.T.);
#70418=ORIENTED_EDGE('',*,*,#49887,.T.);
#70419=ORIENTED_EDGE('',*,*,#49888,.T.);
#70420=ORIENTED_EDGE('',*,*,#49889,.T.);
#70421=ORIENTED_EDGE('',*,*,#49890,.T.);
#70422=ORIENTED_EDGE('',*,*,#49891,.T.);
#70423=ORIENTED_EDGE('',*,*,#49892,.T.);
#70424=ORIENTED_EDGE('',*,*,#49893,.T.);
#70425=ORIENTED_EDGE('',*,*,#49894,.T.);
#70426=ORIENTED_EDGE('',*,*,#49895,.T.);
#70427=ORIENTED_EDGE('',*,*,#49896,.T.);
#70428=ORIENTED_EDGE('',*,*,#49897,.T.);
#70429=ORIENTED_EDGE('',*,*,#49898,.T.);
#70430=ORIENTED_EDGE('',*,*,#49899,.T.);
#70431=ORIENTED_EDGE('',*,*,#49900,.T.);
#70432=ORIENTED_EDGE('',*,*,#49901,.T.);
#70433=ORIENTED_EDGE('',*,*,#49902,.T.);
#70434=ORIENTED_EDGE('',*,*,#49903,.T.);
#70435=ORIENTED_EDGE('',*,*,#49904,.T.);
#70436=ORIENTED_EDGE('',*,*,#49905,.T.);
#70437=ORIENTED_EDGE('',*,*,#49906,.T.);
#70438=ORIENTED_EDGE('',*,*,#49907,.T.);
#70439=ORIENTED_EDGE('',*,*,#49908,.T.);
#70440=ORIENTED_EDGE('',*,*,#49909,.T.);
#70441=ORIENTED_EDGE('',*,*,#49910,.T.);
#70442=ORIENTED_EDGE('',*,*,#49911,.T.);
#70443=ORIENTED_EDGE('',*,*,#49912,.T.);
#70444=ORIENTED_EDGE('',*,*,#49913,.T.);
#70445=ORIENTED_EDGE('',*,*,#49914,.T.);
#70446=ORIENTED_EDGE('',*,*,#49915,.T.);
#70447=ORIENTED_EDGE('',*,*,#49916,.T.);
#70448=ORIENTED_EDGE('',*,*,#49917,.T.);
#70449=ORIENTED_EDGE('',*,*,#49918,.T.);
#70450=ORIENTED_EDGE('',*,*,#49919,.T.);
#70451=ORIENTED_EDGE('',*,*,#49920,.T.);
#70452=ORIENTED_EDGE('',*,*,#49921,.T.);
#70453=ORIENTED_EDGE('',*,*,#49922,.T.);
#70454=ORIENTED_EDGE('',*,*,#49923,.T.);
#70455=ORIENTED_EDGE('',*,*,#49924,.T.);
#70456=ORIENTED_EDGE('',*,*,#49925,.T.);
#70457=ORIENTED_EDGE('',*,*,#49926,.T.);
#70458=ORIENTED_EDGE('',*,*,#49927,.T.);
#70459=ORIENTED_EDGE('',*,*,#49928,.T.);
#70460=ORIENTED_EDGE('',*,*,#49929,.T.);
#70461=ORIENTED_EDGE('',*,*,#49930,.T.);
#70462=ORIENTED_EDGE('',*,*,#49931,.T.);
#70463=ORIENTED_EDGE('',*,*,#49932,.T.);
#70464=ORIENTED_EDGE('',*,*,#49933,.T.);
#70465=ORIENTED_EDGE('',*,*,#49934,.T.);
#70466=ORIENTED_EDGE('',*,*,#49935,.T.);
#70467=ORIENTED_EDGE('',*,*,#49936,.T.);
#70468=ORIENTED_EDGE('',*,*,#49937,.T.);
#70469=ORIENTED_EDGE('',*,*,#49938,.T.);
#70470=ORIENTED_EDGE('',*,*,#49939,.T.);
#70471=ORIENTED_EDGE('',*,*,#49940,.T.);
#70472=ORIENTED_EDGE('',*,*,#49941,.T.);
#70473=ORIENTED_EDGE('',*,*,#49942,.T.);
#70474=ORIENTED_EDGE('',*,*,#49943,.T.);
#70475=ORIENTED_EDGE('',*,*,#49944,.T.);
#70476=ORIENTED_EDGE('',*,*,#49945,.T.);
#70477=ORIENTED_EDGE('',*,*,#49946,.T.);
#70478=ORIENTED_EDGE('',*,*,#49947,.T.);
#70479=ORIENTED_EDGE('',*,*,#49948,.T.);
#70480=ORIENTED_EDGE('',*,*,#49949,.T.);
#70481=ORIENTED_EDGE('',*,*,#49950,.T.);
#70482=ORIENTED_EDGE('',*,*,#49951,.T.);
#70483=ORIENTED_EDGE('',*,*,#49952,.T.);
#70484=ORIENTED_EDGE('',*,*,#49953,.T.);
#70485=ORIENTED_EDGE('',*,*,#49954,.T.);
#70486=ORIENTED_EDGE('',*,*,#49955,.T.);
#70487=ORIENTED_EDGE('',*,*,#49956,.T.);
#70488=ORIENTED_EDGE('',*,*,#49957,.T.);
#70489=ORIENTED_EDGE('',*,*,#49958,.T.);
#70490=ORIENTED_EDGE('',*,*,#49959,.T.);
#70491=ORIENTED_EDGE('',*,*,#49960,.T.);
#70492=ORIENTED_EDGE('',*,*,#49961,.T.);
#70493=ORIENTED_EDGE('',*,*,#49962,.T.);
#70494=ORIENTED_EDGE('',*,*,#49963,.T.);
#70495=ORIENTED_EDGE('',*,*,#49964,.T.);
#70496=ORIENTED_EDGE('',*,*,#49965,.T.);
#70497=ORIENTED_EDGE('',*,*,#49966,.T.);
#70498=ORIENTED_EDGE('',*,*,#49967,.T.);
#70499=ORIENTED_EDGE('',*,*,#49968,.T.);
#70500=ORIENTED_EDGE('',*,*,#49969,.T.);
#70501=ORIENTED_EDGE('',*,*,#49970,.T.);
#70502=ORIENTED_EDGE('',*,*,#49971,.T.);
#70503=ORIENTED_EDGE('',*,*,#49972,.T.);
#70504=ORIENTED_EDGE('',*,*,#49973,.T.);
#70505=ORIENTED_EDGE('',*,*,#49974,.T.);
#70506=ORIENTED_EDGE('',*,*,#49975,.T.);
#70507=ORIENTED_EDGE('',*,*,#49976,.T.);
#70508=ORIENTED_EDGE('',*,*,#49977,.T.);
#70509=ORIENTED_EDGE('',*,*,#49978,.T.);
#70510=ORIENTED_EDGE('',*,*,#49979,.T.);
#70511=ORIENTED_EDGE('',*,*,#49980,.T.);
#70512=ORIENTED_EDGE('',*,*,#49981,.T.);
#70513=ORIENTED_EDGE('',*,*,#49982,.T.);
#70514=ORIENTED_EDGE('',*,*,#49983,.T.);
#70515=ORIENTED_EDGE('',*,*,#49984,.T.);
#70516=ORIENTED_EDGE('',*,*,#49985,.T.);
#70517=ORIENTED_EDGE('',*,*,#49986,.T.);
#70518=ORIENTED_EDGE('',*,*,#49987,.T.);
#70519=ORIENTED_EDGE('',*,*,#49988,.T.);
#70520=ORIENTED_EDGE('',*,*,#49989,.T.);
#70521=ORIENTED_EDGE('',*,*,#49990,.T.);
#70522=ORIENTED_EDGE('',*,*,#49991,.T.);
#70523=ORIENTED_EDGE('',*,*,#49992,.T.);
#70524=ORIENTED_EDGE('',*,*,#49993,.T.);
#70525=ORIENTED_EDGE('',*,*,#49994,.T.);
#70526=ORIENTED_EDGE('',*,*,#49995,.T.);
#70527=ORIENTED_EDGE('',*,*,#49996,.T.);
#70528=ORIENTED_EDGE('',*,*,#49997,.T.);
#70529=ORIENTED_EDGE('',*,*,#49998,.T.);
#70530=ORIENTED_EDGE('',*,*,#49999,.T.);
#70531=ORIENTED_EDGE('',*,*,#50000,.T.);
#70532=ORIENTED_EDGE('',*,*,#50001,.T.);
#70533=ORIENTED_EDGE('',*,*,#50002,.T.);
#70534=ORIENTED_EDGE('',*,*,#50003,.T.);
#70535=ORIENTED_EDGE('',*,*,#50004,.T.);
#70536=ORIENTED_EDGE('',*,*,#50005,.T.);
#70537=ORIENTED_EDGE('',*,*,#50006,.T.);
#70538=ORIENTED_EDGE('',*,*,#50007,.T.);
#70539=ORIENTED_EDGE('',*,*,#50008,.T.);
#70540=ORIENTED_EDGE('',*,*,#50009,.T.);
#70541=ORIENTED_EDGE('',*,*,#50010,.T.);
#70542=ORIENTED_EDGE('',*,*,#50011,.T.);
#70543=ORIENTED_EDGE('',*,*,#50012,.T.);
#70544=ORIENTED_EDGE('',*,*,#50013,.T.);
#70545=ORIENTED_EDGE('',*,*,#50014,.T.);
#70546=ORIENTED_EDGE('',*,*,#50015,.T.);
#70547=ORIENTED_EDGE('',*,*,#50016,.T.);
#70548=ORIENTED_EDGE('',*,*,#50017,.T.);
#70549=ORIENTED_EDGE('',*,*,#50018,.T.);
#70550=ORIENTED_EDGE('',*,*,#50019,.T.);
#70551=ORIENTED_EDGE('',*,*,#50020,.T.);
#70552=ORIENTED_EDGE('',*,*,#50021,.T.);
#70553=ORIENTED_EDGE('',*,*,#50022,.T.);
#70554=ORIENTED_EDGE('',*,*,#50023,.T.);
#70555=ORIENTED_EDGE('',*,*,#50024,.T.);
#70556=ORIENTED_EDGE('',*,*,#50025,.T.);
#70557=ORIENTED_EDGE('',*,*,#50026,.T.);
#70558=ORIENTED_EDGE('',*,*,#50027,.T.);
#70559=ORIENTED_EDGE('',*,*,#50028,.T.);
#70560=ORIENTED_EDGE('',*,*,#50029,.T.);
#70561=ORIENTED_EDGE('',*,*,#50030,.T.);
#70562=ORIENTED_EDGE('',*,*,#50031,.T.);
#70563=ORIENTED_EDGE('',*,*,#50032,.T.);
#70564=ORIENTED_EDGE('',*,*,#50033,.T.);
#70565=ORIENTED_EDGE('',*,*,#50034,.T.);
#70566=ORIENTED_EDGE('',*,*,#50035,.T.);
#70567=ORIENTED_EDGE('',*,*,#50036,.T.);
#70568=ORIENTED_EDGE('',*,*,#50037,.T.);
#70569=ORIENTED_EDGE('',*,*,#50038,.T.);
#70570=ORIENTED_EDGE('',*,*,#50039,.T.);
#70571=ORIENTED_EDGE('',*,*,#50040,.T.);
#70572=ORIENTED_EDGE('',*,*,#50041,.T.);
#70573=ORIENTED_EDGE('',*,*,#50042,.T.);
#70574=ORIENTED_EDGE('',*,*,#50043,.T.);
#70575=ORIENTED_EDGE('',*,*,#50044,.T.);
#70576=ORIENTED_EDGE('',*,*,#50045,.T.);
#70577=ORIENTED_EDGE('',*,*,#50046,.T.);
#70578=ORIENTED_EDGE('',*,*,#50047,.T.);
#70579=ORIENTED_EDGE('',*,*,#50048,.T.);
#70580=ORIENTED_EDGE('',*,*,#50049,.T.);
#70581=ORIENTED_EDGE('',*,*,#50050,.T.);
#70582=ORIENTED_EDGE('',*,*,#50051,.T.);
#70583=ORIENTED_EDGE('',*,*,#50052,.T.);
#70584=ORIENTED_EDGE('',*,*,#50053,.T.);
#70585=ORIENTED_EDGE('',*,*,#50054,.T.);
#70586=ORIENTED_EDGE('',*,*,#50055,.T.);
#70587=ORIENTED_EDGE('',*,*,#50056,.T.);
#70588=ORIENTED_EDGE('',*,*,#50057,.T.);
#70589=ORIENTED_EDGE('',*,*,#50058,.T.);
#70590=ORIENTED_EDGE('',*,*,#50059,.T.);
#70591=ORIENTED_EDGE('',*,*,#50060,.T.);
#70592=ORIENTED_EDGE('',*,*,#50061,.T.);
#70593=ORIENTED_EDGE('',*,*,#50062,.T.);
#70594=ORIENTED_EDGE('',*,*,#50063,.T.);
#70595=ORIENTED_EDGE('',*,*,#50064,.T.);
#70596=ORIENTED_EDGE('',*,*,#50065,.T.);
#70597=ORIENTED_EDGE('',*,*,#50066,.T.);
#70598=ORIENTED_EDGE('',*,*,#50067,.F.);
#70599=ORIENTED_EDGE('',*,*,#50068,.T.);
#70600=ORIENTED_EDGE('',*,*,#49869,.T.);
#70601=ORIENTED_EDGE('',*,*,#49870,.T.);
#70602=ORIENTED_EDGE('',*,*,#50068,.F.);
#70603=ORIENTED_EDGE('',*,*,#50069,.F.);
#70604=ORIENTED_EDGE('',*,*,#50070,.T.);
#70605=ORIENTED_EDGE('',*,*,#50071,.F.);
#70606=ORIENTED_EDGE('',*,*,#50072,.T.);
#70607=ORIENTED_EDGE('',*,*,#50073,.F.);
#70608=ORIENTED_EDGE('',*,*,#50074,.T.);
#70609=ORIENTED_EDGE('',*,*,#50075,.F.);
#70610=ORIENTED_EDGE('',*,*,#50076,.T.);
#70611=ORIENTED_EDGE('',*,*,#50077,.F.);
#70612=ORIENTED_EDGE('',*,*,#50078,.T.);
#70613=ORIENTED_EDGE('',*,*,#50079,.F.);
#70614=ORIENTED_EDGE('',*,*,#50080,.T.);
#70615=ORIENTED_EDGE('',*,*,#50081,.F.);
#70616=ORIENTED_EDGE('',*,*,#50082,.T.);
#70617=ORIENTED_EDGE('',*,*,#50083,.F.);
#70618=ORIENTED_EDGE('',*,*,#50084,.T.);
#70619=ORIENTED_EDGE('',*,*,#50085,.F.);
#70620=ORIENTED_EDGE('',*,*,#50086,.T.);
#70621=ORIENTED_EDGE('',*,*,#50087,.F.);
#70622=ORIENTED_EDGE('',*,*,#50088,.T.);
#70623=ORIENTED_EDGE('',*,*,#50089,.F.);
#70624=ORIENTED_EDGE('',*,*,#50090,.T.);
#70625=ORIENTED_EDGE('',*,*,#50091,.F.);
#70626=ORIENTED_EDGE('',*,*,#50092,.T.);
#70627=ORIENTED_EDGE('',*,*,#50093,.F.);
#70628=ORIENTED_EDGE('',*,*,#50094,.T.);
#70629=ORIENTED_EDGE('',*,*,#50095,.F.);
#70630=ORIENTED_EDGE('',*,*,#50096,.T.);
#70631=ORIENTED_EDGE('',*,*,#50097,.F.);
#70632=ORIENTED_EDGE('',*,*,#50098,.T.);
#70633=ORIENTED_EDGE('',*,*,#50099,.F.);
#70634=ORIENTED_EDGE('',*,*,#50100,.T.);
#70635=ORIENTED_EDGE('',*,*,#50101,.F.);
#70636=ORIENTED_EDGE('',*,*,#50102,.T.);
#70637=ORIENTED_EDGE('',*,*,#50103,.F.);
#70638=ORIENTED_EDGE('',*,*,#50104,.T.);
#70639=ORIENTED_EDGE('',*,*,#50105,.F.);
#70640=ORIENTED_EDGE('',*,*,#50106,.T.);
#70641=ORIENTED_EDGE('',*,*,#50107,.F.);
#70642=ORIENTED_EDGE('',*,*,#50108,.T.);
#70643=ORIENTED_EDGE('',*,*,#50109,.F.);
#70644=ORIENTED_EDGE('',*,*,#50110,.T.);
#70645=ORIENTED_EDGE('',*,*,#50111,.F.);
#70646=ORIENTED_EDGE('',*,*,#50112,.T.);
#70647=ORIENTED_EDGE('',*,*,#50113,.F.);
#70648=ORIENTED_EDGE('',*,*,#50114,.T.);
#70649=ORIENTED_EDGE('',*,*,#50115,.F.);
#70650=ORIENTED_EDGE('',*,*,#50116,.T.);
#70651=ORIENTED_EDGE('',*,*,#50117,.F.);
#70652=ORIENTED_EDGE('',*,*,#50118,.T.);
#70653=ORIENTED_EDGE('',*,*,#50119,.F.);
#70654=ORIENTED_EDGE('',*,*,#50120,.T.);
#70655=ORIENTED_EDGE('',*,*,#50121,.F.);
#70656=ORIENTED_EDGE('',*,*,#50122,.T.);
#70657=ORIENTED_EDGE('',*,*,#50123,.F.);
#70658=ORIENTED_EDGE('',*,*,#50124,.T.);
#70659=ORIENTED_EDGE('',*,*,#50125,.F.);
#70660=ORIENTED_EDGE('',*,*,#50126,.T.);
#70661=ORIENTED_EDGE('',*,*,#50127,.F.);
#70662=ORIENTED_EDGE('',*,*,#50128,.T.);
#70663=ORIENTED_EDGE('',*,*,#50129,.F.);
#70664=ORIENTED_EDGE('',*,*,#50130,.T.);
#70665=ORIENTED_EDGE('',*,*,#50131,.F.);
#70666=ORIENTED_EDGE('',*,*,#50132,.T.);
#70667=ORIENTED_EDGE('',*,*,#50133,.F.);
#70668=ORIENTED_EDGE('',*,*,#50134,.T.);
#70669=ORIENTED_EDGE('',*,*,#50135,.F.);
#70670=ORIENTED_EDGE('',*,*,#50136,.T.);
#70671=ORIENTED_EDGE('',*,*,#50137,.F.);
#70672=ORIENTED_EDGE('',*,*,#50138,.T.);
#70673=ORIENTED_EDGE('',*,*,#50139,.F.);
#70674=ORIENTED_EDGE('',*,*,#50140,.T.);
#70675=ORIENTED_EDGE('',*,*,#50141,.F.);
#70676=ORIENTED_EDGE('',*,*,#50142,.T.);
#70677=ORIENTED_EDGE('',*,*,#50143,.F.);
#70678=ORIENTED_EDGE('',*,*,#50144,.T.);
#70679=ORIENTED_EDGE('',*,*,#50145,.F.);
#70680=ORIENTED_EDGE('',*,*,#50146,.T.);
#70681=ORIENTED_EDGE('',*,*,#50147,.F.);
#70682=ORIENTED_EDGE('',*,*,#50148,.T.);
#70683=ORIENTED_EDGE('',*,*,#50149,.F.);
#70684=ORIENTED_EDGE('',*,*,#50150,.T.);
#70685=ORIENTED_EDGE('',*,*,#50151,.F.);
#70686=ORIENTED_EDGE('',*,*,#50152,.T.);
#70687=ORIENTED_EDGE('',*,*,#50153,.F.);
#70688=ORIENTED_EDGE('',*,*,#50154,.T.);
#70689=ORIENTED_EDGE('',*,*,#50155,.F.);
#70690=ORIENTED_EDGE('',*,*,#50156,.T.);
#70691=ORIENTED_EDGE('',*,*,#50157,.F.);
#70692=ORIENTED_EDGE('',*,*,#50158,.T.);
#70693=ORIENTED_EDGE('',*,*,#50159,.F.);
#70694=ORIENTED_EDGE('',*,*,#50160,.T.);
#70695=ORIENTED_EDGE('',*,*,#50161,.F.);
#70696=ORIENTED_EDGE('',*,*,#50162,.T.);
#70697=ORIENTED_EDGE('',*,*,#50163,.F.);
#70698=ORIENTED_EDGE('',*,*,#50164,.T.);
#70699=ORIENTED_EDGE('',*,*,#50165,.F.);
#70700=ORIENTED_EDGE('',*,*,#50166,.T.);
#70701=ORIENTED_EDGE('',*,*,#50167,.F.);
#70702=ORIENTED_EDGE('',*,*,#50168,.T.);
#70703=ORIENTED_EDGE('',*,*,#50169,.F.);
#70704=ORIENTED_EDGE('',*,*,#50170,.T.);
#70705=ORIENTED_EDGE('',*,*,#50171,.F.);
#70706=ORIENTED_EDGE('',*,*,#50172,.T.);
#70707=ORIENTED_EDGE('',*,*,#50173,.F.);
#70708=ORIENTED_EDGE('',*,*,#50174,.T.);
#70709=ORIENTED_EDGE('',*,*,#50175,.F.);
#70710=ORIENTED_EDGE('',*,*,#50176,.T.);
#70711=ORIENTED_EDGE('',*,*,#50177,.F.);
#70712=ORIENTED_EDGE('',*,*,#50178,.T.);
#70713=ORIENTED_EDGE('',*,*,#50179,.F.);
#70714=ORIENTED_EDGE('',*,*,#50180,.T.);
#70715=ORIENTED_EDGE('',*,*,#50181,.F.);
#70716=ORIENTED_EDGE('',*,*,#50182,.T.);
#70717=ORIENTED_EDGE('',*,*,#50183,.F.);
#70718=ORIENTED_EDGE('',*,*,#50184,.T.);
#70719=ORIENTED_EDGE('',*,*,#50185,.F.);
#70720=ORIENTED_EDGE('',*,*,#50186,.T.);
#70721=ORIENTED_EDGE('',*,*,#50187,.F.);
#70722=ORIENTED_EDGE('',*,*,#50188,.T.);
#70723=ORIENTED_EDGE('',*,*,#50189,.F.);
#70724=ORIENTED_EDGE('',*,*,#50190,.T.);
#70725=ORIENTED_EDGE('',*,*,#50191,.F.);
#70726=ORIENTED_EDGE('',*,*,#50192,.T.);
#70727=ORIENTED_EDGE('',*,*,#50193,.F.);
#70728=ORIENTED_EDGE('',*,*,#50194,.T.);
#70729=ORIENTED_EDGE('',*,*,#50195,.F.);
#70730=ORIENTED_EDGE('',*,*,#50196,.T.);
#70731=ORIENTED_EDGE('',*,*,#50197,.F.);
#70732=ORIENTED_EDGE('',*,*,#50198,.T.);
#70733=ORIENTED_EDGE('',*,*,#50199,.F.);
#70734=ORIENTED_EDGE('',*,*,#50200,.T.);
#70735=ORIENTED_EDGE('',*,*,#50201,.F.);
#70736=ORIENTED_EDGE('',*,*,#50202,.T.);
#70737=ORIENTED_EDGE('',*,*,#50203,.F.);
#70738=ORIENTED_EDGE('',*,*,#50204,.T.);
#70739=ORIENTED_EDGE('',*,*,#50205,.F.);
#70740=ORIENTED_EDGE('',*,*,#50206,.T.);
#70741=ORIENTED_EDGE('',*,*,#50207,.F.);
#70742=ORIENTED_EDGE('',*,*,#50208,.T.);
#70743=ORIENTED_EDGE('',*,*,#50209,.F.);
#70744=ORIENTED_EDGE('',*,*,#50210,.T.);
#70745=ORIENTED_EDGE('',*,*,#50211,.F.);
#70746=ORIENTED_EDGE('',*,*,#50212,.T.);
#70747=ORIENTED_EDGE('',*,*,#50213,.F.);
#70748=ORIENTED_EDGE('',*,*,#50214,.T.);
#70749=ORIENTED_EDGE('',*,*,#50215,.F.);
#70750=ORIENTED_EDGE('',*,*,#50216,.T.);
#70751=ORIENTED_EDGE('',*,*,#50217,.F.);
#70752=ORIENTED_EDGE('',*,*,#50218,.T.);
#70753=ORIENTED_EDGE('',*,*,#50219,.F.);
#70754=ORIENTED_EDGE('',*,*,#50220,.T.);
#70755=ORIENTED_EDGE('',*,*,#50221,.F.);
#70756=ORIENTED_EDGE('',*,*,#50222,.T.);
#70757=ORIENTED_EDGE('',*,*,#50223,.F.);
#70758=ORIENTED_EDGE('',*,*,#50224,.T.);
#70759=ORIENTED_EDGE('',*,*,#50225,.F.);
#70760=ORIENTED_EDGE('',*,*,#50226,.T.);
#70761=ORIENTED_EDGE('',*,*,#50227,.F.);
#70762=ORIENTED_EDGE('',*,*,#50228,.T.);
#70763=ORIENTED_EDGE('',*,*,#50229,.F.);
#70764=ORIENTED_EDGE('',*,*,#50230,.T.);
#70765=ORIENTED_EDGE('',*,*,#50231,.F.);
#70766=ORIENTED_EDGE('',*,*,#50232,.T.);
#70767=ORIENTED_EDGE('',*,*,#50233,.F.);
#70768=ORIENTED_EDGE('',*,*,#50234,.T.);
#70769=ORIENTED_EDGE('',*,*,#50235,.F.);
#70770=ORIENTED_EDGE('',*,*,#50236,.T.);
#70771=ORIENTED_EDGE('',*,*,#50237,.F.);
#70772=ORIENTED_EDGE('',*,*,#50238,.T.);
#70773=ORIENTED_EDGE('',*,*,#50239,.F.);
#70774=ORIENTED_EDGE('',*,*,#50240,.T.);
#70775=ORIENTED_EDGE('',*,*,#50241,.F.);
#70776=ORIENTED_EDGE('',*,*,#50242,.T.);
#70777=ORIENTED_EDGE('',*,*,#50243,.F.);
#70778=ORIENTED_EDGE('',*,*,#50244,.T.);
#70779=ORIENTED_EDGE('',*,*,#50245,.F.);
#70780=ORIENTED_EDGE('',*,*,#50246,.T.);
#70781=ORIENTED_EDGE('',*,*,#50247,.F.);
#70782=ORIENTED_EDGE('',*,*,#50248,.T.);
#70783=ORIENTED_EDGE('',*,*,#50249,.F.);
#70784=ORIENTED_EDGE('',*,*,#50250,.T.);
#70785=ORIENTED_EDGE('',*,*,#50251,.F.);
#70786=ORIENTED_EDGE('',*,*,#50252,.T.);
#70787=ORIENTED_EDGE('',*,*,#50253,.F.);
#70788=ORIENTED_EDGE('',*,*,#50254,.T.);
#70789=ORIENTED_EDGE('',*,*,#50255,.F.);
#70790=ORIENTED_EDGE('',*,*,#50256,.T.);
#70791=ORIENTED_EDGE('',*,*,#50257,.F.);
#70792=ORIENTED_EDGE('',*,*,#50258,.T.);
#70793=ORIENTED_EDGE('',*,*,#50259,.F.);
#70794=ORIENTED_EDGE('',*,*,#50260,.T.);
#70795=ORIENTED_EDGE('',*,*,#50261,.F.);
#70796=ORIENTED_EDGE('',*,*,#50262,.T.);
#70797=ORIENTED_EDGE('',*,*,#50263,.F.);
#70798=ORIENTED_EDGE('',*,*,#50264,.T.);
#70799=ORIENTED_EDGE('',*,*,#50265,.F.);
#70800=ORIENTED_EDGE('',*,*,#50266,.T.);
#70801=ORIENTED_EDGE('',*,*,#50267,.F.);
#70802=ORIENTED_EDGE('',*,*,#50268,.T.);
#70803=ORIENTED_EDGE('',*,*,#50269,.F.);
#70804=ORIENTED_EDGE('',*,*,#50270,.T.);
#70805=ORIENTED_EDGE('',*,*,#50271,.F.);
#70806=ORIENTED_EDGE('',*,*,#50272,.T.);
#70807=ORIENTED_EDGE('',*,*,#50273,.F.);
#70808=ORIENTED_EDGE('',*,*,#50274,.T.);
#70809=ORIENTED_EDGE('',*,*,#50275,.F.);
#70810=ORIENTED_EDGE('',*,*,#50276,.T.);
#70811=ORIENTED_EDGE('',*,*,#50277,.F.);
#70812=ORIENTED_EDGE('',*,*,#50278,.T.);
#70813=ORIENTED_EDGE('',*,*,#50279,.F.);
#70814=ORIENTED_EDGE('',*,*,#50280,.T.);
#70815=ORIENTED_EDGE('',*,*,#50281,.F.);
#70816=ORIENTED_EDGE('',*,*,#50282,.T.);
#70817=ORIENTED_EDGE('',*,*,#50283,.F.);
#70818=ORIENTED_EDGE('',*,*,#50284,.T.);
#70819=ORIENTED_EDGE('',*,*,#50285,.F.);
#70820=ORIENTED_EDGE('',*,*,#50286,.T.);
#70821=ORIENTED_EDGE('',*,*,#50287,.F.);
#70822=ORIENTED_EDGE('',*,*,#50288,.T.);
#70823=ORIENTED_EDGE('',*,*,#50289,.F.);
#70824=ORIENTED_EDGE('',*,*,#50290,.T.);
#70825=ORIENTED_EDGE('',*,*,#50291,.F.);
#70826=ORIENTED_EDGE('',*,*,#50292,.T.);
#70827=ORIENTED_EDGE('',*,*,#50293,.F.);
#70828=ORIENTED_EDGE('',*,*,#50294,.T.);
#70829=ORIENTED_EDGE('',*,*,#50295,.F.);
#70830=ORIENTED_EDGE('',*,*,#50296,.T.);
#70831=ORIENTED_EDGE('',*,*,#50297,.F.);
#70832=ORIENTED_EDGE('',*,*,#50298,.T.);
#70833=ORIENTED_EDGE('',*,*,#50299,.F.);
#70834=ORIENTED_EDGE('',*,*,#50300,.T.);
#70835=ORIENTED_EDGE('',*,*,#50301,.F.);
#70836=ORIENTED_EDGE('',*,*,#50302,.T.);
#70837=ORIENTED_EDGE('',*,*,#50303,.F.);
#70838=ORIENTED_EDGE('',*,*,#50304,.T.);
#70839=ORIENTED_EDGE('',*,*,#50305,.F.);
#70840=ORIENTED_EDGE('',*,*,#50306,.T.);
#70841=ORIENTED_EDGE('',*,*,#50307,.F.);
#70842=ORIENTED_EDGE('',*,*,#50308,.T.);
#70843=ORIENTED_EDGE('',*,*,#50309,.F.);
#70844=ORIENTED_EDGE('',*,*,#50310,.T.);
#70845=ORIENTED_EDGE('',*,*,#50311,.F.);
#70846=ORIENTED_EDGE('',*,*,#50312,.T.);
#70847=ORIENTED_EDGE('',*,*,#50313,.F.);
#70848=ORIENTED_EDGE('',*,*,#50314,.T.);
#70849=ORIENTED_EDGE('',*,*,#50315,.F.);
#70850=ORIENTED_EDGE('',*,*,#50316,.T.);
#70851=ORIENTED_EDGE('',*,*,#50317,.F.);
#70852=ORIENTED_EDGE('',*,*,#50318,.T.);
#70853=ORIENTED_EDGE('',*,*,#50319,.F.);
#70854=ORIENTED_EDGE('',*,*,#50320,.T.);
#70855=ORIENTED_EDGE('',*,*,#50321,.F.);
#70856=ORIENTED_EDGE('',*,*,#50322,.T.);
#70857=ORIENTED_EDGE('',*,*,#50323,.F.);
#70858=ORIENTED_EDGE('',*,*,#50324,.T.);
#70859=ORIENTED_EDGE('',*,*,#50325,.F.);
#70860=ORIENTED_EDGE('',*,*,#50326,.T.);
#70861=ORIENTED_EDGE('',*,*,#50327,.F.);
#70862=ORIENTED_EDGE('',*,*,#50328,.T.);
#70863=ORIENTED_EDGE('',*,*,#50329,.F.);
#70864=ORIENTED_EDGE('',*,*,#50330,.T.);
#70865=ORIENTED_EDGE('',*,*,#50331,.F.);
#70866=ORIENTED_EDGE('',*,*,#50332,.T.);
#70867=ORIENTED_EDGE('',*,*,#50333,.F.);
#70868=ORIENTED_EDGE('',*,*,#50334,.T.);
#70869=ORIENTED_EDGE('',*,*,#50335,.F.);
#70870=ORIENTED_EDGE('',*,*,#50336,.T.);
#70871=ORIENTED_EDGE('',*,*,#50337,.F.);
#70872=ORIENTED_EDGE('',*,*,#50338,.T.);
#70873=ORIENTED_EDGE('',*,*,#50339,.F.);
#70874=ORIENTED_EDGE('',*,*,#50340,.T.);
#70875=ORIENTED_EDGE('',*,*,#50341,.F.);
#70876=ORIENTED_EDGE('',*,*,#50342,.T.);
#70877=ORIENTED_EDGE('',*,*,#50343,.F.);
#70878=ORIENTED_EDGE('',*,*,#50344,.T.);
#70879=ORIENTED_EDGE('',*,*,#50345,.F.);
#70880=ORIENTED_EDGE('',*,*,#50346,.T.);
#70881=ORIENTED_EDGE('',*,*,#50347,.F.);
#70882=ORIENTED_EDGE('',*,*,#50348,.T.);
#70883=ORIENTED_EDGE('',*,*,#50349,.F.);
#70884=ORIENTED_EDGE('',*,*,#50350,.T.);
#70885=ORIENTED_EDGE('',*,*,#50351,.F.);
#70886=ORIENTED_EDGE('',*,*,#50352,.T.);
#70887=ORIENTED_EDGE('',*,*,#50353,.F.);
#70888=ORIENTED_EDGE('',*,*,#50354,.T.);
#70889=ORIENTED_EDGE('',*,*,#50355,.F.);
#70890=ORIENTED_EDGE('',*,*,#50356,.T.);
#70891=ORIENTED_EDGE('',*,*,#50357,.F.);
#70892=ORIENTED_EDGE('',*,*,#50358,.T.);
#70893=ORIENTED_EDGE('',*,*,#50359,.F.);
#70894=ORIENTED_EDGE('',*,*,#50360,.T.);
#70895=ORIENTED_EDGE('',*,*,#50361,.F.);
#70896=ORIENTED_EDGE('',*,*,#50362,.T.);
#70897=ORIENTED_EDGE('',*,*,#50363,.F.);
#70898=ORIENTED_EDGE('',*,*,#50364,.T.);
#70899=ORIENTED_EDGE('',*,*,#49669,.T.);
#70900=ORIENTED_EDGE('',*,*,#50364,.F.);
#70901=ORIENTED_EDGE('',*,*,#50365,.F.);
#70902=ORIENTED_EDGE('',*,*,#50366,.T.);
#70903=ORIENTED_EDGE('',*,*,#50367,.F.);
#70904=ORIENTED_EDGE('',*,*,#50368,.T.);
#70905=ORIENTED_EDGE('',*,*,#50369,.F.);
#70906=ORIENTED_EDGE('',*,*,#50370,.T.);
#70907=ORIENTED_EDGE('',*,*,#50371,.F.);
#70908=ORIENTED_EDGE('',*,*,#50372,.T.);
#70909=ORIENTED_EDGE('',*,*,#50373,.F.);
#70910=ORIENTED_EDGE('',*,*,#50374,.T.);
#70911=ORIENTED_EDGE('',*,*,#50375,.F.);
#70912=ORIENTED_EDGE('',*,*,#50376,.T.);
#70913=ORIENTED_EDGE('',*,*,#50377,.F.);
#70914=ORIENTED_EDGE('',*,*,#50378,.T.);
#70915=ORIENTED_EDGE('',*,*,#50379,.F.);
#70916=ORIENTED_EDGE('',*,*,#50380,.T.);
#70917=ORIENTED_EDGE('',*,*,#50381,.F.);
#70918=ORIENTED_EDGE('',*,*,#50382,.T.);
#70919=ORIENTED_EDGE('',*,*,#50383,.F.);
#70920=ORIENTED_EDGE('',*,*,#50384,.T.);
#70921=ORIENTED_EDGE('',*,*,#50385,.F.);
#70922=ORIENTED_EDGE('',*,*,#50386,.T.);
#70923=ORIENTED_EDGE('',*,*,#50387,.F.);
#70924=ORIENTED_EDGE('',*,*,#50388,.T.);
#70925=ORIENTED_EDGE('',*,*,#50389,.F.);
#70926=ORIENTED_EDGE('',*,*,#50390,.T.);
#70927=ORIENTED_EDGE('',*,*,#50391,.F.);
#70928=ORIENTED_EDGE('',*,*,#50392,.T.);
#70929=ORIENTED_EDGE('',*,*,#50393,.F.);
#70930=ORIENTED_EDGE('',*,*,#50394,.T.);
#70931=ORIENTED_EDGE('',*,*,#50395,.F.);
#70932=ORIENTED_EDGE('',*,*,#50396,.T.);
#70933=ORIENTED_EDGE('',*,*,#50397,.F.);
#70934=ORIENTED_EDGE('',*,*,#50398,.T.);
#70935=ORIENTED_EDGE('',*,*,#50399,.F.);
#70936=ORIENTED_EDGE('',*,*,#50400,.T.);
#70937=ORIENTED_EDGE('',*,*,#50401,.F.);
#70938=ORIENTED_EDGE('',*,*,#50402,.T.);
#70939=ORIENTED_EDGE('',*,*,#50403,.F.);
#70940=ORIENTED_EDGE('',*,*,#50404,.T.);
#70941=ORIENTED_EDGE('',*,*,#50405,.F.);
#70942=ORIENTED_EDGE('',*,*,#50406,.T.);
#70943=ORIENTED_EDGE('',*,*,#50407,.F.);
#70944=ORIENTED_EDGE('',*,*,#50408,.T.);
#70945=ORIENTED_EDGE('',*,*,#50409,.F.);
#70946=ORIENTED_EDGE('',*,*,#50410,.T.);
#70947=ORIENTED_EDGE('',*,*,#50411,.F.);
#70948=ORIENTED_EDGE('',*,*,#50412,.T.);
#70949=ORIENTED_EDGE('',*,*,#50413,.F.);
#70950=ORIENTED_EDGE('',*,*,#50414,.T.);
#70951=ORIENTED_EDGE('',*,*,#50415,.F.);
#70952=ORIENTED_EDGE('',*,*,#50416,.T.);
#70953=ORIENTED_EDGE('',*,*,#50417,.F.);
#70954=ORIENTED_EDGE('',*,*,#50418,.T.);
#70955=ORIENTED_EDGE('',*,*,#50419,.F.);
#70956=ORIENTED_EDGE('',*,*,#50420,.T.);
#70957=ORIENTED_EDGE('',*,*,#50421,.F.);
#70958=ORIENTED_EDGE('',*,*,#50422,.T.);
#70959=ORIENTED_EDGE('',*,*,#50423,.F.);
#70960=ORIENTED_EDGE('',*,*,#50424,.T.);
#70961=ORIENTED_EDGE('',*,*,#50425,.F.);
#70962=ORIENTED_EDGE('',*,*,#50426,.T.);
#70963=ORIENTED_EDGE('',*,*,#50427,.F.);
#70964=ORIENTED_EDGE('',*,*,#50428,.T.);
#70965=ORIENTED_EDGE('',*,*,#50429,.F.);
#70966=ORIENTED_EDGE('',*,*,#50430,.T.);
#70967=ORIENTED_EDGE('',*,*,#50431,.F.);
#70968=ORIENTED_EDGE('',*,*,#50432,.T.);
#70969=ORIENTED_EDGE('',*,*,#50433,.F.);
#70970=ORIENTED_EDGE('',*,*,#50434,.T.);
#70971=ORIENTED_EDGE('',*,*,#50435,.F.);
#70972=ORIENTED_EDGE('',*,*,#50436,.T.);
#70973=ORIENTED_EDGE('',*,*,#50437,.F.);
#70974=ORIENTED_EDGE('',*,*,#50438,.T.);
#70975=ORIENTED_EDGE('',*,*,#50439,.F.);
#70976=ORIENTED_EDGE('',*,*,#50440,.T.);
#70977=ORIENTED_EDGE('',*,*,#50441,.F.);
#70978=ORIENTED_EDGE('',*,*,#50442,.T.);
#70979=ORIENTED_EDGE('',*,*,#50443,.F.);
#70980=ORIENTED_EDGE('',*,*,#50444,.T.);
#70981=ORIENTED_EDGE('',*,*,#50445,.F.);
#70982=ORIENTED_EDGE('',*,*,#50446,.T.);
#70983=ORIENTED_EDGE('',*,*,#50447,.F.);
#70984=ORIENTED_EDGE('',*,*,#50448,.T.);
#70985=ORIENTED_EDGE('',*,*,#50449,.F.);
#70986=ORIENTED_EDGE('',*,*,#50450,.T.);
#70987=ORIENTED_EDGE('',*,*,#50451,.F.);
#70988=ORIENTED_EDGE('',*,*,#50452,.T.);
#70989=ORIENTED_EDGE('',*,*,#50453,.F.);
#70990=ORIENTED_EDGE('',*,*,#50454,.T.);
#70991=ORIENTED_EDGE('',*,*,#50455,.F.);
#70992=ORIENTED_EDGE('',*,*,#50456,.T.);
#70993=ORIENTED_EDGE('',*,*,#50457,.F.);
#70994=ORIENTED_EDGE('',*,*,#50458,.T.);
#70995=ORIENTED_EDGE('',*,*,#50459,.F.);
#70996=ORIENTED_EDGE('',*,*,#50460,.T.);
#70997=ORIENTED_EDGE('',*,*,#50461,.F.);
#70998=ORIENTED_EDGE('',*,*,#50462,.T.);
#70999=ORIENTED_EDGE('',*,*,#50463,.F.);
#71000=ORIENTED_EDGE('',*,*,#50464,.T.);
#71001=ORIENTED_EDGE('',*,*,#50465,.F.);
#71002=ORIENTED_EDGE('',*,*,#50466,.T.);
#71003=ORIENTED_EDGE('',*,*,#50467,.F.);
#71004=ORIENTED_EDGE('',*,*,#50468,.T.);
#71005=ORIENTED_EDGE('',*,*,#50469,.F.);
#71006=ORIENTED_EDGE('',*,*,#50470,.T.);
#71007=ORIENTED_EDGE('',*,*,#50471,.F.);
#71008=ORIENTED_EDGE('',*,*,#50472,.T.);
#71009=ORIENTED_EDGE('',*,*,#50473,.F.);
#71010=ORIENTED_EDGE('',*,*,#50474,.T.);
#71011=ORIENTED_EDGE('',*,*,#50475,.F.);
#71012=ORIENTED_EDGE('',*,*,#50476,.T.);
#71013=ORIENTED_EDGE('',*,*,#50477,.F.);
#71014=ORIENTED_EDGE('',*,*,#50478,.T.);
#71015=ORIENTED_EDGE('',*,*,#50479,.F.);
#71016=ORIENTED_EDGE('',*,*,#50480,.T.);
#71017=ORIENTED_EDGE('',*,*,#50481,.F.);
#71018=ORIENTED_EDGE('',*,*,#50482,.T.);
#71019=ORIENTED_EDGE('',*,*,#50483,.F.);
#71020=ORIENTED_EDGE('',*,*,#50484,.T.);
#71021=ORIENTED_EDGE('',*,*,#50485,.F.);
#71022=ORIENTED_EDGE('',*,*,#50486,.T.);
#71023=ORIENTED_EDGE('',*,*,#50487,.F.);
#71024=ORIENTED_EDGE('',*,*,#50488,.T.);
#71025=ORIENTED_EDGE('',*,*,#50489,.F.);
#71026=ORIENTED_EDGE('',*,*,#50490,.T.);
#71027=ORIENTED_EDGE('',*,*,#50491,.F.);
#71028=ORIENTED_EDGE('',*,*,#50492,.T.);
#71029=ORIENTED_EDGE('',*,*,#50493,.F.);
#71030=ORIENTED_EDGE('',*,*,#50494,.T.);
#71031=ORIENTED_EDGE('',*,*,#50495,.F.);
#71032=ORIENTED_EDGE('',*,*,#50496,.T.);
#71033=ORIENTED_EDGE('',*,*,#50497,.F.);
#71034=ORIENTED_EDGE('',*,*,#50498,.T.);
#71035=ORIENTED_EDGE('',*,*,#50499,.F.);
#71036=ORIENTED_EDGE('',*,*,#50500,.T.);
#71037=ORIENTED_EDGE('',*,*,#50501,.F.);
#71038=ORIENTED_EDGE('',*,*,#50502,.T.);
#71039=ORIENTED_EDGE('',*,*,#50503,.F.);
#71040=ORIENTED_EDGE('',*,*,#50504,.T.);
#71041=ORIENTED_EDGE('',*,*,#50505,.F.);
#71042=ORIENTED_EDGE('',*,*,#50506,.T.);
#71043=ORIENTED_EDGE('',*,*,#50507,.F.);
#71044=ORIENTED_EDGE('',*,*,#50508,.T.);
#71045=ORIENTED_EDGE('',*,*,#50509,.F.);
#71046=ORIENTED_EDGE('',*,*,#50510,.T.);
#71047=ORIENTED_EDGE('',*,*,#50511,.F.);
#71048=ORIENTED_EDGE('',*,*,#50512,.T.);
#71049=ORIENTED_EDGE('',*,*,#50513,.F.);
#71050=ORIENTED_EDGE('',*,*,#50514,.T.);
#71051=ORIENTED_EDGE('',*,*,#50515,.F.);
#71052=ORIENTED_EDGE('',*,*,#50516,.T.);
#71053=ORIENTED_EDGE('',*,*,#50517,.F.);
#71054=ORIENTED_EDGE('',*,*,#50518,.T.);
#71055=ORIENTED_EDGE('',*,*,#50519,.F.);
#71056=ORIENTED_EDGE('',*,*,#50520,.T.);
#71057=ORIENTED_EDGE('',*,*,#50521,.F.);
#71058=ORIENTED_EDGE('',*,*,#50522,.T.);
#71059=ORIENTED_EDGE('',*,*,#50523,.F.);
#71060=ORIENTED_EDGE('',*,*,#50524,.T.);
#71061=ORIENTED_EDGE('',*,*,#50525,.F.);
#71062=ORIENTED_EDGE('',*,*,#50526,.T.);
#71063=ORIENTED_EDGE('',*,*,#50527,.F.);
#71064=ORIENTED_EDGE('',*,*,#50528,.T.);
#71065=ORIENTED_EDGE('',*,*,#50529,.F.);
#71066=ORIENTED_EDGE('',*,*,#50530,.T.);
#71067=ORIENTED_EDGE('',*,*,#50531,.F.);
#71068=ORIENTED_EDGE('',*,*,#50532,.T.);
#71069=ORIENTED_EDGE('',*,*,#50533,.F.);
#71070=ORIENTED_EDGE('',*,*,#50534,.T.);
#71071=ORIENTED_EDGE('',*,*,#50535,.F.);
#71072=ORIENTED_EDGE('',*,*,#50536,.T.);
#71073=ORIENTED_EDGE('',*,*,#50537,.F.);
#71074=ORIENTED_EDGE('',*,*,#50538,.T.);
#71075=ORIENTED_EDGE('',*,*,#50539,.F.);
#71076=ORIENTED_EDGE('',*,*,#50540,.T.);
#71077=ORIENTED_EDGE('',*,*,#50541,.F.);
#71078=ORIENTED_EDGE('',*,*,#50542,.T.);
#71079=ORIENTED_EDGE('',*,*,#50543,.F.);
#71080=ORIENTED_EDGE('',*,*,#50544,.T.);
#71081=ORIENTED_EDGE('',*,*,#50545,.F.);
#71082=ORIENTED_EDGE('',*,*,#50546,.T.);
#71083=ORIENTED_EDGE('',*,*,#50547,.F.);
#71084=ORIENTED_EDGE('',*,*,#50548,.T.);
#71085=ORIENTED_EDGE('',*,*,#50549,.F.);
#71086=ORIENTED_EDGE('',*,*,#50550,.T.);
#71087=ORIENTED_EDGE('',*,*,#50551,.F.);
#71088=ORIENTED_EDGE('',*,*,#50552,.T.);
#71089=ORIENTED_EDGE('',*,*,#50553,.F.);
#71090=ORIENTED_EDGE('',*,*,#50554,.T.);
#71091=ORIENTED_EDGE('',*,*,#50555,.F.);
#71092=ORIENTED_EDGE('',*,*,#50556,.T.);
#71093=ORIENTED_EDGE('',*,*,#50557,.F.);
#71094=ORIENTED_EDGE('',*,*,#50558,.T.);
#71095=ORIENTED_EDGE('',*,*,#50559,.F.);
#71096=ORIENTED_EDGE('',*,*,#50560,.T.);
#71097=ORIENTED_EDGE('',*,*,#50561,.F.);
#71098=ORIENTED_EDGE('',*,*,#50562,.T.);
#71099=ORIENTED_EDGE('',*,*,#50563,.F.);
#71100=ORIENTED_EDGE('',*,*,#50564,.T.);
#71101=ORIENTED_EDGE('',*,*,#50565,.F.);
#71102=ORIENTED_EDGE('',*,*,#50566,.T.);
#71103=ORIENTED_EDGE('',*,*,#50567,.F.);
#71104=ORIENTED_EDGE('',*,*,#50568,.T.);
#71105=ORIENTED_EDGE('',*,*,#50569,.F.);
#71106=ORIENTED_EDGE('',*,*,#50570,.T.);
#71107=ORIENTED_EDGE('',*,*,#50571,.F.);
#71108=ORIENTED_EDGE('',*,*,#50572,.T.);
#71109=ORIENTED_EDGE('',*,*,#50573,.F.);
#71110=ORIENTED_EDGE('',*,*,#50574,.T.);
#71111=ORIENTED_EDGE('',*,*,#50575,.F.);
#71112=ORIENTED_EDGE('',*,*,#50576,.T.);
#71113=ORIENTED_EDGE('',*,*,#50577,.F.);
#71114=ORIENTED_EDGE('',*,*,#50578,.T.);
#71115=ORIENTED_EDGE('',*,*,#50579,.F.);
#71116=ORIENTED_EDGE('',*,*,#50580,.T.);
#71117=ORIENTED_EDGE('',*,*,#50581,.F.);
#71118=ORIENTED_EDGE('',*,*,#50582,.T.);
#71119=ORIENTED_EDGE('',*,*,#50583,.F.);
#71120=ORIENTED_EDGE('',*,*,#50584,.T.);
#71121=ORIENTED_EDGE('',*,*,#50585,.F.);
#71122=ORIENTED_EDGE('',*,*,#50586,.T.);
#71123=ORIENTED_EDGE('',*,*,#50587,.F.);
#71124=ORIENTED_EDGE('',*,*,#50588,.T.);
#71125=ORIENTED_EDGE('',*,*,#50589,.F.);
#71126=ORIENTED_EDGE('',*,*,#50590,.T.);
#71127=ORIENTED_EDGE('',*,*,#50591,.F.);
#71128=ORIENTED_EDGE('',*,*,#50592,.T.);
#71129=ORIENTED_EDGE('',*,*,#50593,.F.);
#71130=ORIENTED_EDGE('',*,*,#50594,.T.);
#71131=ORIENTED_EDGE('',*,*,#50595,.F.);
#71132=ORIENTED_EDGE('',*,*,#50596,.T.);
#71133=ORIENTED_EDGE('',*,*,#50597,.F.);
#71134=ORIENTED_EDGE('',*,*,#50598,.T.);
#71135=ORIENTED_EDGE('',*,*,#50599,.F.);
#71136=ORIENTED_EDGE('',*,*,#50600,.T.);
#71137=ORIENTED_EDGE('',*,*,#50601,.F.);
#71138=ORIENTED_EDGE('',*,*,#50602,.T.);
#71139=ORIENTED_EDGE('',*,*,#50603,.F.);
#71140=ORIENTED_EDGE('',*,*,#50604,.T.);
#71141=ORIENTED_EDGE('',*,*,#50605,.F.);
#71142=ORIENTED_EDGE('',*,*,#50606,.T.);
#71143=ORIENTED_EDGE('',*,*,#50607,.F.);
#71144=ORIENTED_EDGE('',*,*,#50608,.T.);
#71145=ORIENTED_EDGE('',*,*,#50609,.F.);
#71146=ORIENTED_EDGE('',*,*,#50610,.T.);
#71147=ORIENTED_EDGE('',*,*,#50611,.F.);
#71148=ORIENTED_EDGE('',*,*,#50612,.T.);
#71149=ORIENTED_EDGE('',*,*,#50613,.F.);
#71150=ORIENTED_EDGE('',*,*,#50614,.T.);
#71151=ORIENTED_EDGE('',*,*,#50615,.F.);
#71152=ORIENTED_EDGE('',*,*,#50616,.T.);
#71153=ORIENTED_EDGE('',*,*,#50617,.F.);
#71154=ORIENTED_EDGE('',*,*,#50618,.T.);
#71155=ORIENTED_EDGE('',*,*,#50619,.F.);
#71156=ORIENTED_EDGE('',*,*,#50620,.T.);
#71157=ORIENTED_EDGE('',*,*,#50621,.F.);
#71158=ORIENTED_EDGE('',*,*,#50622,.T.);
#71159=ORIENTED_EDGE('',*,*,#50623,.F.);
#71160=ORIENTED_EDGE('',*,*,#50624,.T.);
#71161=ORIENTED_EDGE('',*,*,#50625,.F.);
#71162=ORIENTED_EDGE('',*,*,#50626,.T.);
#71163=ORIENTED_EDGE('',*,*,#50627,.F.);
#71164=ORIENTED_EDGE('',*,*,#50628,.T.);
#71165=ORIENTED_EDGE('',*,*,#50629,.F.);
#71166=ORIENTED_EDGE('',*,*,#50630,.T.);
#71167=ORIENTED_EDGE('',*,*,#50631,.F.);
#71168=ORIENTED_EDGE('',*,*,#50632,.T.);
#71169=ORIENTED_EDGE('',*,*,#50633,.F.);
#71170=ORIENTED_EDGE('',*,*,#50634,.T.);
#71171=ORIENTED_EDGE('',*,*,#50635,.F.);
#71172=ORIENTED_EDGE('',*,*,#50636,.T.);
#71173=ORIENTED_EDGE('',*,*,#50637,.F.);
#71174=ORIENTED_EDGE('',*,*,#50638,.T.);
#71175=ORIENTED_EDGE('',*,*,#50639,.F.);
#71176=ORIENTED_EDGE('',*,*,#50640,.T.);
#71177=ORIENTED_EDGE('',*,*,#50641,.F.);
#71178=ORIENTED_EDGE('',*,*,#50642,.T.);
#71179=ORIENTED_EDGE('',*,*,#50643,.F.);
#71180=ORIENTED_EDGE('',*,*,#50644,.T.);
#71181=ORIENTED_EDGE('',*,*,#50645,.F.);
#71182=ORIENTED_EDGE('',*,*,#50646,.T.);
#71183=ORIENTED_EDGE('',*,*,#50647,.F.);
#71184=ORIENTED_EDGE('',*,*,#50648,.T.);
#71185=ORIENTED_EDGE('',*,*,#50649,.F.);
#71186=ORIENTED_EDGE('',*,*,#50650,.T.);
#71187=ORIENTED_EDGE('',*,*,#50651,.F.);
#71188=ORIENTED_EDGE('',*,*,#50652,.T.);
#71189=ORIENTED_EDGE('',*,*,#50653,.F.);
#71190=ORIENTED_EDGE('',*,*,#50654,.T.);
#71191=ORIENTED_EDGE('',*,*,#50655,.F.);
#71192=ORIENTED_EDGE('',*,*,#50656,.T.);
#71193=ORIENTED_EDGE('',*,*,#50657,.F.);
#71194=ORIENTED_EDGE('',*,*,#50658,.T.);
#71195=ORIENTED_EDGE('',*,*,#50069,.T.);
#71196=ORIENTED_EDGE('',*,*,#50659,.T.);
#71197=ORIENTED_EDGE('',*,*,#49871,.F.);
#71198=ORIENTED_EDGE('',*,*,#49867,.F.);
#71199=ORIENTED_EDGE('',*,*,#50660,.T.);
#71200=ORIENTED_EDGE('',*,*,#49835,.F.);
#71201=ORIENTED_EDGE('',*,*,#50661,.T.);
#71202=ORIENTED_EDGE('',*,*,#50117,.T.);
#71203=ORIENTED_EDGE('',*,*,#50662,.T.);
#71204=ORIENTED_EDGE('',*,*,#50123,.T.);
#71205=ORIENTED_EDGE('',*,*,#50663,.T.);
#71206=ORIENTED_EDGE('',*,*,#49831,.F.);
#71207=ORIENTED_EDGE('',*,*,#50664,.T.);
#71208=ORIENTED_EDGE('',*,*,#50129,.T.);
#71209=ORIENTED_EDGE('',*,*,#50665,.T.);
#71210=ORIENTED_EDGE('',*,*,#49827,.F.);
#71211=ORIENTED_EDGE('',*,*,#50666,.T.);
#71212=ORIENTED_EDGE('',*,*,#50135,.T.);
#71213=ORIENTED_EDGE('',*,*,#50667,.T.);
#71214=ORIENTED_EDGE('',*,*,#49823,.F.);
#71215=ORIENTED_EDGE('',*,*,#50668,.T.);
#71216=ORIENTED_EDGE('',*,*,#50141,.T.);
#71217=ORIENTED_EDGE('',*,*,#50669,.T.);
#71218=ORIENTED_EDGE('',*,*,#49819,.F.);
#71219=ORIENTED_EDGE('',*,*,#50670,.T.);
#71220=ORIENTED_EDGE('',*,*,#50147,.T.);
#71221=ORIENTED_EDGE('',*,*,#50671,.T.);
#71222=ORIENTED_EDGE('',*,*,#49815,.F.);
#71223=ORIENTED_EDGE('',*,*,#50672,.T.);
#71224=ORIENTED_EDGE('',*,*,#50153,.T.);
#71225=ORIENTED_EDGE('',*,*,#50673,.T.);
#71226=ORIENTED_EDGE('',*,*,#49811,.F.);
#71227=ORIENTED_EDGE('',*,*,#50674,.T.);
#71228=ORIENTED_EDGE('',*,*,#50159,.T.);
#71229=ORIENTED_EDGE('',*,*,#50675,.T.);
#71230=ORIENTED_EDGE('',*,*,#49807,.F.);
#71231=ORIENTED_EDGE('',*,*,#50676,.T.);
#71232=ORIENTED_EDGE('',*,*,#50165,.T.);
#71233=ORIENTED_EDGE('',*,*,#50677,.T.);
#71234=ORIENTED_EDGE('',*,*,#49803,.F.);
#71235=ORIENTED_EDGE('',*,*,#50678,.T.);
#71236=ORIENTED_EDGE('',*,*,#50171,.T.);
#71237=ORIENTED_EDGE('',*,*,#50679,.T.);
#71238=ORIENTED_EDGE('',*,*,#49799,.F.);
#71239=ORIENTED_EDGE('',*,*,#50680,.T.);
#71240=ORIENTED_EDGE('',*,*,#50177,.T.);
#71241=ORIENTED_EDGE('',*,*,#50681,.T.);
#71242=ORIENTED_EDGE('',*,*,#49795,.F.);
#71243=ORIENTED_EDGE('',*,*,#50682,.T.);
#71244=ORIENTED_EDGE('',*,*,#50183,.T.);
#71245=ORIENTED_EDGE('',*,*,#50683,.T.);
#71246=ORIENTED_EDGE('',*,*,#49791,.F.);
#71247=ORIENTED_EDGE('',*,*,#50684,.T.);
#71248=ORIENTED_EDGE('',*,*,#50189,.T.);
#71249=ORIENTED_EDGE('',*,*,#50685,.T.);
#71250=ORIENTED_EDGE('',*,*,#49787,.F.);
#71251=ORIENTED_EDGE('',*,*,#50686,.T.);
#71252=ORIENTED_EDGE('',*,*,#50195,.T.);
#71253=ORIENTED_EDGE('',*,*,#50687,.T.);
#71254=ORIENTED_EDGE('',*,*,#49783,.F.);
#71255=ORIENTED_EDGE('',*,*,#50688,.T.);
#71256=ORIENTED_EDGE('',*,*,#50201,.T.);
#71257=ORIENTED_EDGE('',*,*,#50689,.T.);
#71258=ORIENTED_EDGE('',*,*,#49779,.F.);
#71259=ORIENTED_EDGE('',*,*,#50690,.T.);
#71260=ORIENTED_EDGE('',*,*,#50207,.T.);
#71261=ORIENTED_EDGE('',*,*,#50691,.T.);
#71262=ORIENTED_EDGE('',*,*,#49775,.F.);
#71263=ORIENTED_EDGE('',*,*,#50692,.T.);
#71264=ORIENTED_EDGE('',*,*,#50213,.T.);
#71265=ORIENTED_EDGE('',*,*,#50693,.T.);
#71266=ORIENTED_EDGE('',*,*,#49771,.F.);
#71267=ORIENTED_EDGE('',*,*,#50694,.T.);
#71268=ORIENTED_EDGE('',*,*,#50219,.T.);
#71269=ORIENTED_EDGE('',*,*,#50695,.T.);
#71270=ORIENTED_EDGE('',*,*,#49767,.F.);
#71271=ORIENTED_EDGE('',*,*,#50696,.T.);
#71272=ORIENTED_EDGE('',*,*,#50225,.T.);
#71273=ORIENTED_EDGE('',*,*,#50697,.T.);
#71274=ORIENTED_EDGE('',*,*,#49763,.F.);
#71275=ORIENTED_EDGE('',*,*,#50698,.T.);
#71276=ORIENTED_EDGE('',*,*,#50231,.T.);
#71277=ORIENTED_EDGE('',*,*,#50699,.T.);
#71278=ORIENTED_EDGE('',*,*,#49759,.F.);
#71279=ORIENTED_EDGE('',*,*,#50700,.T.);
#71280=ORIENTED_EDGE('',*,*,#50237,.T.);
#71281=ORIENTED_EDGE('',*,*,#50701,.T.);
#71282=ORIENTED_EDGE('',*,*,#49755,.F.);
#71283=ORIENTED_EDGE('',*,*,#50702,.T.);
#71284=ORIENTED_EDGE('',*,*,#50243,.T.);
#71285=ORIENTED_EDGE('',*,*,#50703,.T.);
#71286=ORIENTED_EDGE('',*,*,#49751,.F.);
#71287=ORIENTED_EDGE('',*,*,#50704,.T.);
#71288=ORIENTED_EDGE('',*,*,#50249,.T.);
#71289=ORIENTED_EDGE('',*,*,#50705,.T.);
#71290=ORIENTED_EDGE('',*,*,#49747,.F.);
#71291=ORIENTED_EDGE('',*,*,#50706,.T.);
#71292=ORIENTED_EDGE('',*,*,#50255,.T.);
#71293=ORIENTED_EDGE('',*,*,#50707,.T.);
#71294=ORIENTED_EDGE('',*,*,#49743,.F.);
#71295=ORIENTED_EDGE('',*,*,#50708,.T.);
#71296=ORIENTED_EDGE('',*,*,#50261,.T.);
#71297=ORIENTED_EDGE('',*,*,#50709,.T.);
#71298=ORIENTED_EDGE('',*,*,#49739,.F.);
#71299=ORIENTED_EDGE('',*,*,#50710,.T.);
#71300=ORIENTED_EDGE('',*,*,#50267,.T.);
#71301=ORIENTED_EDGE('',*,*,#50711,.T.);
#71302=ORIENTED_EDGE('',*,*,#49735,.F.);
#71303=ORIENTED_EDGE('',*,*,#50712,.T.);
#71304=ORIENTED_EDGE('',*,*,#50273,.T.);
#71305=ORIENTED_EDGE('',*,*,#50713,.T.);
#71306=ORIENTED_EDGE('',*,*,#49731,.F.);
#71307=ORIENTED_EDGE('',*,*,#50714,.T.);
#71308=ORIENTED_EDGE('',*,*,#50279,.T.);
#71309=ORIENTED_EDGE('',*,*,#50715,.T.);
#71310=ORIENTED_EDGE('',*,*,#49727,.F.);
#71311=ORIENTED_EDGE('',*,*,#50716,.T.);
#71312=ORIENTED_EDGE('',*,*,#50285,.T.);
#71313=ORIENTED_EDGE('',*,*,#50717,.T.);
#71314=ORIENTED_EDGE('',*,*,#49723,.F.);
#71315=ORIENTED_EDGE('',*,*,#50718,.T.);
#71316=ORIENTED_EDGE('',*,*,#50291,.T.);
#71317=ORIENTED_EDGE('',*,*,#50719,.T.);
#71318=ORIENTED_EDGE('',*,*,#49719,.F.);
#71319=ORIENTED_EDGE('',*,*,#50720,.T.);
#71320=ORIENTED_EDGE('',*,*,#50297,.T.);
#71321=ORIENTED_EDGE('',*,*,#50721,.T.);
#71322=ORIENTED_EDGE('',*,*,#49715,.F.);
#71323=ORIENTED_EDGE('',*,*,#50722,.T.);
#71324=ORIENTED_EDGE('',*,*,#50303,.T.);
#71325=ORIENTED_EDGE('',*,*,#50723,.T.);
#71326=ORIENTED_EDGE('',*,*,#49711,.F.);
#71327=ORIENTED_EDGE('',*,*,#50724,.T.);
#71328=ORIENTED_EDGE('',*,*,#50309,.T.);
#71329=ORIENTED_EDGE('',*,*,#50725,.T.);
#71330=ORIENTED_EDGE('',*,*,#49707,.F.);
#71331=ORIENTED_EDGE('',*,*,#50726,.T.);
#71332=ORIENTED_EDGE('',*,*,#50315,.T.);
#71333=ORIENTED_EDGE('',*,*,#50727,.T.);
#71334=ORIENTED_EDGE('',*,*,#49703,.F.);
#71335=ORIENTED_EDGE('',*,*,#50728,.T.);
#71336=ORIENTED_EDGE('',*,*,#50321,.T.);
#71337=ORIENTED_EDGE('',*,*,#50729,.T.);
#71338=ORIENTED_EDGE('',*,*,#49699,.F.);
#71339=ORIENTED_EDGE('',*,*,#50730,.T.);
#71340=ORIENTED_EDGE('',*,*,#50327,.T.);
#71341=ORIENTED_EDGE('',*,*,#50731,.T.);
#71342=ORIENTED_EDGE('',*,*,#49695,.F.);
#71343=ORIENTED_EDGE('',*,*,#50732,.T.);
#71344=ORIENTED_EDGE('',*,*,#50333,.T.);
#71345=ORIENTED_EDGE('',*,*,#50733,.T.);
#71346=ORIENTED_EDGE('',*,*,#49691,.F.);
#71347=ORIENTED_EDGE('',*,*,#50734,.T.);
#71348=ORIENTED_EDGE('',*,*,#50339,.T.);
#71349=ORIENTED_EDGE('',*,*,#50735,.T.);
#71350=ORIENTED_EDGE('',*,*,#49687,.F.);
#71351=ORIENTED_EDGE('',*,*,#50736,.T.);
#71352=ORIENTED_EDGE('',*,*,#50345,.T.);
#71353=ORIENTED_EDGE('',*,*,#50737,.T.);
#71354=ORIENTED_EDGE('',*,*,#49683,.F.);
#71355=ORIENTED_EDGE('',*,*,#50738,.T.);
#71356=ORIENTED_EDGE('',*,*,#50351,.T.);
#71357=ORIENTED_EDGE('',*,*,#50739,.T.);
#71358=ORIENTED_EDGE('',*,*,#49679,.F.);
#71359=ORIENTED_EDGE('',*,*,#50740,.T.);
#71360=ORIENTED_EDGE('',*,*,#50357,.T.);
#71361=ORIENTED_EDGE('',*,*,#50741,.T.);
#71362=ORIENTED_EDGE('',*,*,#49675,.F.);
#71363=ORIENTED_EDGE('',*,*,#50742,.T.);
#71364=ORIENTED_EDGE('',*,*,#50365,.T.);
#71365=ORIENTED_EDGE('',*,*,#50363,.T.);
#71366=ORIENTED_EDGE('',*,*,#50743,.T.);
#71367=ORIENTED_EDGE('',*,*,#49671,.F.);
#71368=ORIENTED_EDGE('',*,*,#50744,.T.);
#71369=ORIENTED_EDGE('',*,*,#50371,.T.);
#71370=ORIENTED_EDGE('',*,*,#50745,.T.);
#71371=ORIENTED_EDGE('',*,*,#50063,.F.);
#71372=ORIENTED_EDGE('',*,*,#50746,.T.);
#71373=ORIENTED_EDGE('',*,*,#50377,.T.);
#71374=ORIENTED_EDGE('',*,*,#50747,.T.);
#71375=ORIENTED_EDGE('',*,*,#50059,.F.);
#71376=ORIENTED_EDGE('',*,*,#50748,.T.);
#71377=ORIENTED_EDGE('',*,*,#50383,.T.);
#71378=ORIENTED_EDGE('',*,*,#50749,.T.);
#71379=ORIENTED_EDGE('',*,*,#50055,.F.);
#71380=ORIENTED_EDGE('',*,*,#50750,.T.);
#71381=ORIENTED_EDGE('',*,*,#50389,.T.);
#71382=ORIENTED_EDGE('',*,*,#50751,.T.);
#71383=ORIENTED_EDGE('',*,*,#50051,.F.);
#71384=ORIENTED_EDGE('',*,*,#50752,.T.);
#71385=ORIENTED_EDGE('',*,*,#50395,.T.);
#71386=ORIENTED_EDGE('',*,*,#50753,.T.);
#71387=ORIENTED_EDGE('',*,*,#50047,.F.);
#71388=ORIENTED_EDGE('',*,*,#50754,.T.);
#71389=ORIENTED_EDGE('',*,*,#50401,.T.);
#71390=ORIENTED_EDGE('',*,*,#50755,.T.);
#71391=ORIENTED_EDGE('',*,*,#50043,.F.);
#71392=ORIENTED_EDGE('',*,*,#50756,.T.);
#71393=ORIENTED_EDGE('',*,*,#50407,.T.);
#71394=ORIENTED_EDGE('',*,*,#50757,.T.);
#71395=ORIENTED_EDGE('',*,*,#50039,.F.);
#71396=ORIENTED_EDGE('',*,*,#50758,.T.);
#71397=ORIENTED_EDGE('',*,*,#50413,.T.);
#71398=ORIENTED_EDGE('',*,*,#50759,.T.);
#71399=ORIENTED_EDGE('',*,*,#50035,.F.);
#71400=ORIENTED_EDGE('',*,*,#50760,.T.);
#71401=ORIENTED_EDGE('',*,*,#50419,.T.);
#71402=ORIENTED_EDGE('',*,*,#50761,.T.);
#71403=ORIENTED_EDGE('',*,*,#50031,.F.);
#71404=ORIENTED_EDGE('',*,*,#50762,.T.);
#71405=ORIENTED_EDGE('',*,*,#50425,.T.);
#71406=ORIENTED_EDGE('',*,*,#50763,.T.);
#71407=ORIENTED_EDGE('',*,*,#50027,.F.);
#71408=ORIENTED_EDGE('',*,*,#50764,.T.);
#71409=ORIENTED_EDGE('',*,*,#50431,.T.);
#71410=ORIENTED_EDGE('',*,*,#50765,.T.);
#71411=ORIENTED_EDGE('',*,*,#50023,.F.);
#71412=ORIENTED_EDGE('',*,*,#50766,.T.);
#71413=ORIENTED_EDGE('',*,*,#50437,.T.);
#71414=ORIENTED_EDGE('',*,*,#50767,.T.);
#71415=ORIENTED_EDGE('',*,*,#50019,.F.);
#71416=ORIENTED_EDGE('',*,*,#50768,.T.);
#71417=ORIENTED_EDGE('',*,*,#50443,.T.);
#71418=ORIENTED_EDGE('',*,*,#50769,.T.);
#71419=ORIENTED_EDGE('',*,*,#50015,.F.);
#71420=ORIENTED_EDGE('',*,*,#50770,.T.);
#71421=ORIENTED_EDGE('',*,*,#50449,.T.);
#71422=ORIENTED_EDGE('',*,*,#50771,.T.);
#71423=ORIENTED_EDGE('',*,*,#50011,.F.);
#71424=ORIENTED_EDGE('',*,*,#50772,.T.);
#71425=ORIENTED_EDGE('',*,*,#50455,.T.);
#71426=ORIENTED_EDGE('',*,*,#50773,.T.);
#71427=ORIENTED_EDGE('',*,*,#50007,.F.);
#71428=ORIENTED_EDGE('',*,*,#50774,.T.);
#71429=ORIENTED_EDGE('',*,*,#50461,.T.);
#71430=ORIENTED_EDGE('',*,*,#50775,.T.);
#71431=ORIENTED_EDGE('',*,*,#50003,.F.);
#71432=ORIENTED_EDGE('',*,*,#50776,.T.);
#71433=ORIENTED_EDGE('',*,*,#50467,.T.);
#71434=ORIENTED_EDGE('',*,*,#50777,.T.);
#71435=ORIENTED_EDGE('',*,*,#49999,.F.);
#71436=ORIENTED_EDGE('',*,*,#50778,.T.);
#71437=ORIENTED_EDGE('',*,*,#50473,.T.);
#71438=ORIENTED_EDGE('',*,*,#50779,.T.);
#71439=ORIENTED_EDGE('',*,*,#49995,.F.);
#71440=ORIENTED_EDGE('',*,*,#50780,.T.);
#71441=ORIENTED_EDGE('',*,*,#50479,.T.);
#71442=ORIENTED_EDGE('',*,*,#50781,.T.);
#71443=ORIENTED_EDGE('',*,*,#49991,.F.);
#71444=ORIENTED_EDGE('',*,*,#50782,.T.);
#71445=ORIENTED_EDGE('',*,*,#50485,.T.);
#71446=ORIENTED_EDGE('',*,*,#50783,.T.);
#71447=ORIENTED_EDGE('',*,*,#49987,.F.);
#71448=ORIENTED_EDGE('',*,*,#50784,.T.);
#71449=ORIENTED_EDGE('',*,*,#50491,.T.);
#71450=ORIENTED_EDGE('',*,*,#50785,.T.);
#71451=ORIENTED_EDGE('',*,*,#49983,.F.);
#71452=ORIENTED_EDGE('',*,*,#50786,.T.);
#71453=ORIENTED_EDGE('',*,*,#50497,.T.);
#71454=ORIENTED_EDGE('',*,*,#50787,.T.);
#71455=ORIENTED_EDGE('',*,*,#49979,.F.);
#71456=ORIENTED_EDGE('',*,*,#50788,.T.);
#71457=ORIENTED_EDGE('',*,*,#49839,.F.);
#71458=ORIENTED_EDGE('',*,*,#50789,.T.);
#71459=ORIENTED_EDGE('',*,*,#50111,.T.);
#71460=ORIENTED_EDGE('',*,*,#50790,.T.);
#71461=ORIENTED_EDGE('',*,*,#49843,.F.);
#71462=ORIENTED_EDGE('',*,*,#50791,.T.);
#71463=ORIENTED_EDGE('',*,*,#50105,.T.);
#71464=ORIENTED_EDGE('',*,*,#50792,.T.);
#71465=ORIENTED_EDGE('',*,*,#49847,.F.);
#71466=ORIENTED_EDGE('',*,*,#50793,.T.);
#71467=ORIENTED_EDGE('',*,*,#50099,.T.);
#71468=ORIENTED_EDGE('',*,*,#50794,.T.);
#71469=ORIENTED_EDGE('',*,*,#49851,.F.);
#71470=ORIENTED_EDGE('',*,*,#50795,.T.);
#71471=ORIENTED_EDGE('',*,*,#50093,.T.);
#71472=ORIENTED_EDGE('',*,*,#50796,.T.);
#71473=ORIENTED_EDGE('',*,*,#49855,.F.);
#71474=ORIENTED_EDGE('',*,*,#50797,.T.);
#71475=ORIENTED_EDGE('',*,*,#50087,.T.);
#71476=ORIENTED_EDGE('',*,*,#50798,.T.);
#71477=ORIENTED_EDGE('',*,*,#49859,.F.);
#71478=ORIENTED_EDGE('',*,*,#50799,.T.);
#71479=ORIENTED_EDGE('',*,*,#50081,.T.);
#71480=ORIENTED_EDGE('',*,*,#50800,.T.);
#71481=ORIENTED_EDGE('',*,*,#49863,.F.);
#71482=ORIENTED_EDGE('',*,*,#50801,.T.);
#71483=ORIENTED_EDGE('',*,*,#50075,.T.);
#71484=ORIENTED_EDGE('',*,*,#50802,.T.);
#71485=ORIENTED_EDGE('',*,*,#49875,.F.);
#71486=ORIENTED_EDGE('',*,*,#50803,.T.);
#71487=ORIENTED_EDGE('',*,*,#50653,.T.);
#71488=ORIENTED_EDGE('',*,*,#50804,.T.);
#71489=ORIENTED_EDGE('',*,*,#49879,.F.);
#71490=ORIENTED_EDGE('',*,*,#50805,.T.);
#71491=ORIENTED_EDGE('',*,*,#50647,.T.);
#71492=ORIENTED_EDGE('',*,*,#50806,.T.);
#71493=ORIENTED_EDGE('',*,*,#49883,.F.);
#71494=ORIENTED_EDGE('',*,*,#50807,.T.);
#71495=ORIENTED_EDGE('',*,*,#50641,.T.);
#71496=ORIENTED_EDGE('',*,*,#50808,.T.);
#71497=ORIENTED_EDGE('',*,*,#49887,.F.);
#71498=ORIENTED_EDGE('',*,*,#50809,.T.);
#71499=ORIENTED_EDGE('',*,*,#50635,.T.);
#71500=ORIENTED_EDGE('',*,*,#50810,.T.);
#71501=ORIENTED_EDGE('',*,*,#49891,.F.);
#71502=ORIENTED_EDGE('',*,*,#50811,.T.);
#71503=ORIENTED_EDGE('',*,*,#50629,.T.);
#71504=ORIENTED_EDGE('',*,*,#50812,.T.);
#71505=ORIENTED_EDGE('',*,*,#49895,.F.);
#71506=ORIENTED_EDGE('',*,*,#50813,.T.);
#71507=ORIENTED_EDGE('',*,*,#50623,.T.);
#71508=ORIENTED_EDGE('',*,*,#50814,.T.);
#71509=ORIENTED_EDGE('',*,*,#49899,.F.);
#71510=ORIENTED_EDGE('',*,*,#50815,.T.);
#71511=ORIENTED_EDGE('',*,*,#50617,.T.);
#71512=ORIENTED_EDGE('',*,*,#50816,.T.);
#71513=ORIENTED_EDGE('',*,*,#49903,.F.);
#71514=ORIENTED_EDGE('',*,*,#50817,.T.);
#71515=ORIENTED_EDGE('',*,*,#50611,.T.);
#71516=ORIENTED_EDGE('',*,*,#50818,.T.);
#71517=ORIENTED_EDGE('',*,*,#49907,.F.);
#71518=ORIENTED_EDGE('',*,*,#50819,.T.);
#71519=ORIENTED_EDGE('',*,*,#50605,.T.);
#71520=ORIENTED_EDGE('',*,*,#50820,.T.);
#71521=ORIENTED_EDGE('',*,*,#49911,.F.);
#71522=ORIENTED_EDGE('',*,*,#50821,.T.);
#71523=ORIENTED_EDGE('',*,*,#50599,.T.);
#71524=ORIENTED_EDGE('',*,*,#50822,.T.);
#71525=ORIENTED_EDGE('',*,*,#49915,.F.);
#71526=ORIENTED_EDGE('',*,*,#50823,.T.);
#71527=ORIENTED_EDGE('',*,*,#50593,.T.);
#71528=ORIENTED_EDGE('',*,*,#50824,.T.);
#71529=ORIENTED_EDGE('',*,*,#49919,.F.);
#71530=ORIENTED_EDGE('',*,*,#50825,.T.);
#71531=ORIENTED_EDGE('',*,*,#50587,.T.);
#71532=ORIENTED_EDGE('',*,*,#50826,.T.);
#71533=ORIENTED_EDGE('',*,*,#49923,.F.);
#71534=ORIENTED_EDGE('',*,*,#50827,.T.);
#71535=ORIENTED_EDGE('',*,*,#50581,.T.);
#71536=ORIENTED_EDGE('',*,*,#50828,.T.);
#71537=ORIENTED_EDGE('',*,*,#49927,.F.);
#71538=ORIENTED_EDGE('',*,*,#50829,.T.);
#71539=ORIENTED_EDGE('',*,*,#50575,.T.);
#71540=ORIENTED_EDGE('',*,*,#50830,.T.);
#71541=ORIENTED_EDGE('',*,*,#49931,.F.);
#71542=ORIENTED_EDGE('',*,*,#50831,.T.);
#71543=ORIENTED_EDGE('',*,*,#50569,.T.);
#71544=ORIENTED_EDGE('',*,*,#50832,.T.);
#71545=ORIENTED_EDGE('',*,*,#49935,.F.);
#71546=ORIENTED_EDGE('',*,*,#50833,.T.);
#71547=ORIENTED_EDGE('',*,*,#50563,.T.);
#71548=ORIENTED_EDGE('',*,*,#50834,.T.);
#71549=ORIENTED_EDGE('',*,*,#49939,.F.);
#71550=ORIENTED_EDGE('',*,*,#50835,.T.);
#71551=ORIENTED_EDGE('',*,*,#50557,.T.);
#71552=ORIENTED_EDGE('',*,*,#50836,.T.);
#71553=ORIENTED_EDGE('',*,*,#49943,.F.);
#71554=ORIENTED_EDGE('',*,*,#50837,.T.);
#71555=ORIENTED_EDGE('',*,*,#50551,.T.);
#71556=ORIENTED_EDGE('',*,*,#50838,.T.);
#71557=ORIENTED_EDGE('',*,*,#49947,.F.);
#71558=ORIENTED_EDGE('',*,*,#50839,.T.);
#71559=ORIENTED_EDGE('',*,*,#50545,.T.);
#71560=ORIENTED_EDGE('',*,*,#50840,.T.);
#71561=ORIENTED_EDGE('',*,*,#49951,.F.);
#71562=ORIENTED_EDGE('',*,*,#50841,.T.);
#71563=ORIENTED_EDGE('',*,*,#50539,.T.);
#71564=ORIENTED_EDGE('',*,*,#50842,.T.);
#71565=ORIENTED_EDGE('',*,*,#49955,.F.);
#71566=ORIENTED_EDGE('',*,*,#50843,.T.);
#71567=ORIENTED_EDGE('',*,*,#50533,.T.);
#71568=ORIENTED_EDGE('',*,*,#50844,.T.);
#71569=ORIENTED_EDGE('',*,*,#49959,.F.);
#71570=ORIENTED_EDGE('',*,*,#50845,.T.);
#71571=ORIENTED_EDGE('',*,*,#50527,.T.);
#71572=ORIENTED_EDGE('',*,*,#50846,.T.);
#71573=ORIENTED_EDGE('',*,*,#49963,.F.);
#71574=ORIENTED_EDGE('',*,*,#50847,.T.);
#71575=ORIENTED_EDGE('',*,*,#50521,.T.);
#71576=ORIENTED_EDGE('',*,*,#50848,.T.);
#71577=ORIENTED_EDGE('',*,*,#49967,.F.);
#71578=ORIENTED_EDGE('',*,*,#50849,.T.);
#71579=ORIENTED_EDGE('',*,*,#50515,.T.);
#71580=ORIENTED_EDGE('',*,*,#50850,.T.);
#71581=ORIENTED_EDGE('',*,*,#50503,.T.);
#71582=ORIENTED_EDGE('',*,*,#50851,.T.);
#71583=ORIENTED_EDGE('',*,*,#49975,.F.);
#71584=ORIENTED_EDGE('',*,*,#50852,.T.);
#71585=ORIENTED_EDGE('',*,*,#50853,.T.);
#71586=ORIENTED_EDGE('',*,*,#50854,.T.);
#71587=ORIENTED_EDGE('',*,*,#50855,.F.);
#71588=ORIENTED_EDGE('',*,*,#50856,.T.);
#71589=ORIENTED_EDGE('',*,*,#50857,.T.);
#71590=ORIENTED_EDGE('',*,*,#50858,.T.);
#71591=ORIENTED_EDGE('',*,*,#50853,.F.);
#71592=ORIENTED_EDGE('',*,*,#50859,.T.);
#71593=ORIENTED_EDGE('',*,*,#50860,.T.);
#71594=ORIENTED_EDGE('',*,*,#50855,.T.);
#71595=ORIENTED_EDGE('',*,*,#50861,.T.);
#71596=ORIENTED_EDGE('',*,*,#50862,.T.);
#71597=ORIENTED_EDGE('',*,*,#50863,.T.);
#71598=ORIENTED_EDGE('',*,*,#50864,.T.);
#71599=ORIENTED_EDGE('',*,*,#50865,.T.);
#71600=ORIENTED_EDGE('',*,*,#49661,.T.);
#71601=ORIENTED_EDGE('',*,*,#50866,.T.);
#71602=ORIENTED_EDGE('',*,*,#50867,.T.);
#71603=ORIENTED_EDGE('',*,*,#49660,.T.);
#71604=ORIENTED_EDGE('',*,*,#50868,.T.);
#71605=ORIENTED_EDGE('',*,*,#50869,.T.);
#71606=ORIENTED_EDGE('',*,*,#49659,.F.);
#71607=ORIENTED_EDGE('',*,*,#50870,.T.);
#71608=ORIENTED_EDGE('',*,*,#50871,.T.);
#71609=ORIENTED_EDGE('',*,*,#49658,.T.);
#71610=ORIENTED_EDGE('',*,*,#50872,.T.);
#71611=ORIENTED_EDGE('',*,*,#50873,.T.);
#71612=ORIENTED_EDGE('',*,*,#49657,.T.);
#71613=ORIENTED_EDGE('',*,*,#50874,.T.);
#71614=ORIENTED_EDGE('',*,*,#50067,.T.);
#71615=ORIENTED_EDGE('',*,*,#50875,.F.);
#71616=ORIENTED_EDGE('',*,*,#50876,.F.);
#71617=ORIENTED_EDGE('',*,*,#49663,.F.);
#71618=ORIENTED_EDGE('',*,*,#50877,.F.);
#71619=ORIENTED_EDGE('',*,*,#50878,.F.);
#71620=ORIENTED_EDGE('',*,*,#50879,.F.);
#71621=ORIENTED_EDGE('',*,*,#50509,.T.);
#71622=ORIENTED_EDGE('',*,*,#50880,.T.);
#71623=ORIENTED_EDGE('',*,*,#49971,.F.);
#71624=ORIENTED_EDGE('',*,*,#50881,.T.);
#71625=ORIENTED_EDGE('',*,*,#50882,.T.);
#71626=ORIENTED_EDGE('',*,*,#50883,.F.);
#71627=ORIENTED_EDGE('',*,*,#50884,.F.);
#71628=ORIENTED_EDGE('',*,*,#50868,.F.);
#71629=ORIENTED_EDGE('',*,*,#50869,.F.);
#71630=ORIENTED_EDGE('',*,*,#50885,.T.);
#71631=ORIENTED_EDGE('',*,*,#49662,.F.);
#71632=ORIENTED_EDGE('',*,*,#50882,.F.);
#71633=ORIENTED_EDGE('',*,*,#50870,.F.);
#71634=ORIENTED_EDGE('',*,*,#50871,.F.);
#71635=ORIENTED_EDGE('',*,*,#50886,.T.);
#71636=ORIENTED_EDGE('',*,*,#50887,.F.);
#71637=ORIENTED_EDGE('',*,*,#50885,.F.);
#71638=ORIENTED_EDGE('',*,*,#50872,.F.);
#71639=ORIENTED_EDGE('',*,*,#50873,.F.);
#71640=ORIENTED_EDGE('',*,*,#50888,.T.);
#71641=ORIENTED_EDGE('',*,*,#50889,.F.);
#71642=ORIENTED_EDGE('',*,*,#50886,.F.);
#71643=ORIENTED_EDGE('',*,*,#50874,.F.);
#71644=ORIENTED_EDGE('',*,*,#50890,.F.);
#71645=ORIENTED_EDGE('',*,*,#50891,.T.);
#71646=ORIENTED_EDGE('',*,*,#50892,.F.);
#71647=ORIENTED_EDGE('',*,*,#50888,.F.);
#71648=ORIENTED_EDGE('',*,*,#50893,.F.);
#71649=ORIENTED_EDGE('',*,*,#50865,.F.);
#71650=ORIENTED_EDGE('',*,*,#50884,.T.);
#71651=ORIENTED_EDGE('',*,*,#50894,.F.);
#71652=ORIENTED_EDGE('',*,*,#50891,.F.);
#71653=ORIENTED_EDGE('',*,*,#50866,.F.);
#71654=ORIENTED_EDGE('',*,*,#50867,.F.);
#71655=ORIENTED_EDGE('',*,*,#50890,.T.);
#71656=ORIENTED_EDGE('',*,*,#49656,.T.);
#71657=ORIENTED_EDGE('',*,*,#50893,.T.);
#71658=ORIENTED_EDGE('',*,*,#50894,.T.);
#71659=ORIENTED_EDGE('',*,*,#50875,.T.);
#71660=ORIENTED_EDGE('',*,*,#50889,.T.);
#71661=ORIENTED_EDGE('',*,*,#50878,.T.);
#71662=ORIENTED_EDGE('',*,*,#50887,.T.);
#71663=ORIENTED_EDGE('',*,*,#50877,.T.);
#71664=ORIENTED_EDGE('',*,*,#50892,.T.);
#71665=ORIENTED_EDGE('',*,*,#50879,.T.);
#71666=ORIENTED_EDGE('',*,*,#50883,.T.);
#71667=ORIENTED_EDGE('',*,*,#50876,.T.);
#71668=ORIENTED_EDGE('',*,*,#49666,.F.);
#71669=ORIENTED_EDGE('',*,*,#49654,.F.);
#71670=ORIENTED_EDGE('',*,*,#49466,.F.);
#71671=ORIENTED_EDGE('',*,*,#49646,.F.);
#71672=ORIENTED_EDGE('',*,*,#49645,.F.);
#71673=ORIENTED_EDGE('',*,*,#49548,.T.);
#71674=ORIENTED_EDGE('',*,*,#50895,.T.);
#71675=ORIENTED_EDGE('',*,*,#49641,.T.);
#71676=ORIENTED_EDGE('',*,*,#50896,.F.);
#71677=ORIENTED_EDGE('',*,*,#49557,.F.);
#71678=ORIENTED_EDGE('',*,*,#49650,.T.);
#71679=ORIENTED_EDGE('',*,*,#49642,.T.);
#71680=ORIENTED_EDGE('',*,*,#50895,.F.);
#71681=ORIENTED_EDGE('',*,*,#49550,.F.);
#71682=ORIENTED_EDGE('',*,*,#49547,.F.);
#71683=ORIENTED_EDGE('',*,*,#49544,.F.);
#71684=ORIENTED_EDGE('',*,*,#49541,.F.);
#71685=ORIENTED_EDGE('',*,*,#49538,.F.);
#71686=ORIENTED_EDGE('',*,*,#49535,.F.);
#71687=ORIENTED_EDGE('',*,*,#49532,.F.);
#71688=ORIENTED_EDGE('',*,*,#49529,.F.);
#71689=ORIENTED_EDGE('',*,*,#49526,.F.);
#71690=ORIENTED_EDGE('',*,*,#49523,.F.);
#71691=ORIENTED_EDGE('',*,*,#49520,.F.);
#71692=ORIENTED_EDGE('',*,*,#49517,.F.);
#71693=ORIENTED_EDGE('',*,*,#49514,.F.);
#71694=ORIENTED_EDGE('',*,*,#49511,.F.);
#71695=ORIENTED_EDGE('',*,*,#49508,.F.);
#71696=ORIENTED_EDGE('',*,*,#49505,.F.);
#71697=ORIENTED_EDGE('',*,*,#49502,.F.);
#71698=ORIENTED_EDGE('',*,*,#49499,.F.);
#71699=ORIENTED_EDGE('',*,*,#49496,.F.);
#71700=ORIENTED_EDGE('',*,*,#49493,.F.);
#71701=ORIENTED_EDGE('',*,*,#49490,.F.);
#71702=ORIENTED_EDGE('',*,*,#49487,.F.);
#71703=ORIENTED_EDGE('',*,*,#49484,.F.);
#71704=ORIENTED_EDGE('',*,*,#49481,.F.);
#71705=ORIENTED_EDGE('',*,*,#49478,.F.);
#71706=ORIENTED_EDGE('',*,*,#49475,.F.);
#71707=ORIENTED_EDGE('',*,*,#49472,.F.);
#71708=ORIENTED_EDGE('',*,*,#49469,.F.);
#71709=ORIENTED_EDGE('',*,*,#49644,.T.);
#71710=ORIENTED_EDGE('',*,*,#49649,.T.);
#71711=ORIENTED_EDGE('',*,*,#49651,.F.);
#71712=ORIENTED_EDGE('',*,*,#49638,.F.);
#71713=ORIENTED_EDGE('',*,*,#49635,.F.);
#71714=ORIENTED_EDGE('',*,*,#49632,.F.);
#71715=ORIENTED_EDGE('',*,*,#49629,.F.);
#71716=ORIENTED_EDGE('',*,*,#49626,.F.);
#71717=ORIENTED_EDGE('',*,*,#49623,.F.);
#71718=ORIENTED_EDGE('',*,*,#49620,.F.);
#71719=ORIENTED_EDGE('',*,*,#49617,.F.);
#71720=ORIENTED_EDGE('',*,*,#49614,.F.);
#71721=ORIENTED_EDGE('',*,*,#49611,.F.);
#71722=ORIENTED_EDGE('',*,*,#49608,.F.);
#71723=ORIENTED_EDGE('',*,*,#49605,.F.);
#71724=ORIENTED_EDGE('',*,*,#49602,.F.);
#71725=ORIENTED_EDGE('',*,*,#49599,.F.);
#71726=ORIENTED_EDGE('',*,*,#49596,.F.);
#71727=ORIENTED_EDGE('',*,*,#49593,.F.);
#71728=ORIENTED_EDGE('',*,*,#49590,.F.);
#71729=ORIENTED_EDGE('',*,*,#49587,.F.);
#71730=ORIENTED_EDGE('',*,*,#49584,.F.);
#71731=ORIENTED_EDGE('',*,*,#49581,.F.);
#71732=ORIENTED_EDGE('',*,*,#49578,.F.);
#71733=ORIENTED_EDGE('',*,*,#49575,.F.);
#71734=ORIENTED_EDGE('',*,*,#49572,.F.);
#71735=ORIENTED_EDGE('',*,*,#49569,.F.);
#71736=ORIENTED_EDGE('',*,*,#49566,.F.);
#71737=ORIENTED_EDGE('',*,*,#49563,.F.);
#71738=ORIENTED_EDGE('',*,*,#49560,.F.);
#71739=ORIENTED_EDGE('',*,*,#49465,.T.);
#71740=ORIENTED_EDGE('',*,*,#49468,.T.);
#71741=ORIENTED_EDGE('',*,*,#49471,.T.);
#71742=ORIENTED_EDGE('',*,*,#49474,.T.);
#71743=ORIENTED_EDGE('',*,*,#49477,.T.);
#71744=ORIENTED_EDGE('',*,*,#49480,.T.);
#71745=ORIENTED_EDGE('',*,*,#49483,.T.);
#71746=ORIENTED_EDGE('',*,*,#49486,.T.);
#71747=ORIENTED_EDGE('',*,*,#49489,.T.);
#71748=ORIENTED_EDGE('',*,*,#49492,.T.);
#71749=ORIENTED_EDGE('',*,*,#49495,.T.);
#71750=ORIENTED_EDGE('',*,*,#49498,.T.);
#71751=ORIENTED_EDGE('',*,*,#49501,.T.);
#71752=ORIENTED_EDGE('',*,*,#49504,.T.);
#71753=ORIENTED_EDGE('',*,*,#49507,.T.);
#71754=ORIENTED_EDGE('',*,*,#49510,.T.);
#71755=ORIENTED_EDGE('',*,*,#49513,.T.);
#71756=ORIENTED_EDGE('',*,*,#49516,.T.);
#71757=ORIENTED_EDGE('',*,*,#49519,.T.);
#71758=ORIENTED_EDGE('',*,*,#49522,.T.);
#71759=ORIENTED_EDGE('',*,*,#49525,.T.);
#71760=ORIENTED_EDGE('',*,*,#49528,.T.);
#71761=ORIENTED_EDGE('',*,*,#49531,.T.);
#71762=ORIENTED_EDGE('',*,*,#49534,.T.);
#71763=ORIENTED_EDGE('',*,*,#49537,.T.);
#71764=ORIENTED_EDGE('',*,*,#49540,.T.);
#71765=ORIENTED_EDGE('',*,*,#49543,.T.);
#71766=ORIENTED_EDGE('',*,*,#49546,.T.);
#71767=ORIENTED_EDGE('',*,*,#49549,.T.);
#71768=ORIENTED_EDGE('',*,*,#50896,.T.);
#71769=ORIENTED_EDGE('',*,*,#49640,.T.);
#71770=ORIENTED_EDGE('',*,*,#49552,.F.);
#71771=ORIENTED_EDGE('',*,*,#49559,.F.);
#71772=ORIENTED_EDGE('',*,*,#49562,.F.);
#71773=ORIENTED_EDGE('',*,*,#49565,.F.);
#71774=ORIENTED_EDGE('',*,*,#49568,.F.);
#71775=ORIENTED_EDGE('',*,*,#49571,.F.);
#71776=ORIENTED_EDGE('',*,*,#49574,.F.);
#71777=ORIENTED_EDGE('',*,*,#49577,.F.);
#71778=ORIENTED_EDGE('',*,*,#49580,.F.);
#71779=ORIENTED_EDGE('',*,*,#49583,.F.);
#71780=ORIENTED_EDGE('',*,*,#49586,.F.);
#71781=ORIENTED_EDGE('',*,*,#49589,.F.);
#71782=ORIENTED_EDGE('',*,*,#49592,.F.);
#71783=ORIENTED_EDGE('',*,*,#49595,.F.);
#71784=ORIENTED_EDGE('',*,*,#49598,.F.);
#71785=ORIENTED_EDGE('',*,*,#49601,.F.);
#71786=ORIENTED_EDGE('',*,*,#49604,.F.);
#71787=ORIENTED_EDGE('',*,*,#49607,.F.);
#71788=ORIENTED_EDGE('',*,*,#49610,.F.);
#71789=ORIENTED_EDGE('',*,*,#49613,.F.);
#71790=ORIENTED_EDGE('',*,*,#49616,.F.);
#71791=ORIENTED_EDGE('',*,*,#49619,.F.);
#71792=ORIENTED_EDGE('',*,*,#49622,.F.);
#71793=ORIENTED_EDGE('',*,*,#49625,.F.);
#71794=ORIENTED_EDGE('',*,*,#49628,.F.);
#71795=ORIENTED_EDGE('',*,*,#49631,.F.);
#71796=ORIENTED_EDGE('',*,*,#49634,.F.);
#71797=ORIENTED_EDGE('',*,*,#49637,.F.);
#71798=ORIENTED_EDGE('',*,*,#49652,.F.);
#71799=ORIENTED_EDGE('',*,*,#49647,.T.);
#71800=ORIENTED_EDGE('',*,*,#50897,.T.);
#71801=ORIENTED_EDGE('',*,*,#50898,.T.);
#71802=ORIENTED_EDGE('',*,*,#50899,.T.);
#71803=ORIENTED_EDGE('',*,*,#50900,.F.);
#71804=ORIENTED_EDGE('',*,*,#50859,.F.);
#71805=ORIENTED_EDGE('',*,*,#50901,.F.);
#71806=ORIENTED_EDGE('',*,*,#50897,.F.);
#71807=ORIENTED_EDGE('',*,*,#50902,.F.);
#71808=ORIENTED_EDGE('',*,*,#50860,.F.);
#71809=ORIENTED_EDGE('',*,*,#50903,.F.);
#71810=ORIENTED_EDGE('',*,*,#50510,.F.);
#71811=ORIENTED_EDGE('',*,*,#50901,.T.);
#71812=ORIENTED_EDGE('',*,*,#50856,.F.);
#71813=ORIENTED_EDGE('',*,*,#50904,.F.);
#71814=ORIENTED_EDGE('',*,*,#50903,.T.);
#71815=ORIENTED_EDGE('',*,*,#50900,.T.);
#71816=ORIENTED_EDGE('',*,*,#50905,.F.);
#71817=ORIENTED_EDGE('',*,*,#50511,.T.);
#71818=ORIENTED_EDGE('',*,*,#50902,.T.);
#71819=ORIENTED_EDGE('',*,*,#50881,.F.);
#71820=ORIENTED_EDGE('',*,*,#50906,.F.);
#71821=ORIENTED_EDGE('',*,*,#50857,.F.);
#71822=ORIENTED_EDGE('',*,*,#50904,.T.);
#71823=ORIENTED_EDGE('',*,*,#50864,.F.);
#71824=ORIENTED_EDGE('',*,*,#50907,.F.);
#71825=ORIENTED_EDGE('',*,*,#50898,.F.);
#71826=ORIENTED_EDGE('',*,*,#50905,.T.);
#71827=ORIENTED_EDGE('',*,*,#50899,.F.);
#71828=ORIENTED_EDGE('',*,*,#50908,.F.);
#71829=ORIENTED_EDGE('',*,*,#50512,.F.);
#71830=ORIENTED_EDGE('',*,*,#50906,.T.);
#71831=ORIENTED_EDGE('',*,*,#49970,.F.);
#71832=ORIENTED_EDGE('',*,*,#50909,.F.);
#71833=ORIENTED_EDGE('',*,*,#50858,.F.);
#71834=ORIENTED_EDGE('',*,*,#50908,.T.);
#71835=ORIENTED_EDGE('',*,*,#50907,.T.);
#71836=ORIENTED_EDGE('',*,*,#50910,.F.);
#71837=ORIENTED_EDGE('',*,*,#50513,.T.);
#71838=ORIENTED_EDGE('',*,*,#50909,.T.);
#71839=ORIENTED_EDGE('',*,*,#49969,.F.);
#71840=ORIENTED_EDGE('',*,*,#50911,.F.);
#71841=ORIENTED_EDGE('',*,*,#50854,.F.);
#71842=ORIENTED_EDGE('',*,*,#50910,.T.);
#71843=ORIENTED_EDGE('',*,*,#50863,.F.);
#71844=ORIENTED_EDGE('',*,*,#50912,.F.);
#71845=ORIENTED_EDGE('',*,*,#50514,.F.);
#71846=ORIENTED_EDGE('',*,*,#50911,.T.);
#71847=ORIENTED_EDGE('',*,*,#49968,.F.);
#71848=ORIENTED_EDGE('',*,*,#50913,.F.);
#71849=ORIENTED_EDGE('',*,*,#50861,.F.);
#71850=ORIENTED_EDGE('',*,*,#50912,.T.);
#71851=ORIENTED_EDGE('',*,*,#50862,.F.);
#71852=ORIENTED_EDGE('',*,*,#50913,.T.);
#71853=ORIENTED_EDGE('',*,*,#50850,.F.);
#71854=ORIENTED_EDGE('',*,*,#50914,.T.);
#71855=ORIENTED_EDGE('',*,*,#50915,.T.);
#71856=ORIENTED_EDGE('',*,*,#50916,.T.);
#71857=ORIENTED_EDGE('',*,*,#50917,.T.);
#71858=ORIENTED_EDGE('',*,*,#50918,.T.);
#71859=ORIENTED_EDGE('',*,*,#50919,.T.);
#71860=ORIENTED_EDGE('',*,*,#50920,.T.);
#71861=ORIENTED_EDGE('',*,*,#50921,.F.);
#71862=ORIENTED_EDGE('',*,*,#50922,.T.);
#71863=ORIENTED_EDGE('',*,*,#50923,.T.);
#71864=ORIENTED_EDGE('',*,*,#50921,.T.);
#71865=ORIENTED_EDGE('',*,*,#50924,.T.);
#71866=ORIENTED_EDGE('',*,*,#50914,.F.);
#71867=ORIENTED_EDGE('',*,*,#50925,.T.);
#71868=ORIENTED_EDGE('',*,*,#50926,.F.);
#71869=ORIENTED_EDGE('',*,*,#50922,.F.);
#71870=ORIENTED_EDGE('',*,*,#50927,.F.);
#71871=ORIENTED_EDGE('',*,*,#50928,.F.);
#71872=ORIENTED_EDGE('',*,*,#50927,.T.);
#71873=ORIENTED_EDGE('',*,*,#50925,.F.);
#71874=ORIENTED_EDGE('',*,*,#50929,.F.);
#71875=ORIENTED_EDGE('',*,*,#50929,.T.);
#71876=ORIENTED_EDGE('',*,*,#50918,.F.);
#71877=ORIENTED_EDGE('',*,*,#50930,.F.);
#71878=ORIENTED_EDGE('',*,*,#50931,.F.);
#71879=ORIENTED_EDGE('',*,*,#50932,.T.);
#71880=ORIENTED_EDGE('',*,*,#50933,.F.);
#71881=ORIENTED_EDGE('',*,*,#50934,.F.);
#71882=ORIENTED_EDGE('',*,*,#50506,.F.);
#71883=ORIENTED_EDGE('',*,*,#50935,.T.);
#71884=ORIENTED_EDGE('',*,*,#50926,.T.);
#71885=ORIENTED_EDGE('',*,*,#50932,.F.);
#71886=ORIENTED_EDGE('',*,*,#50505,.T.);
#71887=ORIENTED_EDGE('',*,*,#50936,.F.);
#71888=ORIENTED_EDGE('',*,*,#50923,.F.);
#71889=ORIENTED_EDGE('',*,*,#50935,.F.);
#71890=ORIENTED_EDGE('',*,*,#50504,.F.);
#71891=ORIENTED_EDGE('',*,*,#50936,.T.);
#71892=ORIENTED_EDGE('',*,*,#50852,.F.);
#71893=ORIENTED_EDGE('',*,*,#50937,.F.);
#71894=ORIENTED_EDGE('',*,*,#50919,.F.);
#71895=ORIENTED_EDGE('',*,*,#50937,.T.);
#71896=ORIENTED_EDGE('',*,*,#49974,.F.);
#71897=ORIENTED_EDGE('',*,*,#50938,.F.);
#71898=ORIENTED_EDGE('',*,*,#50920,.F.);
#71899=ORIENTED_EDGE('',*,*,#50938,.T.);
#71900=ORIENTED_EDGE('',*,*,#49973,.F.);
#71901=ORIENTED_EDGE('',*,*,#50939,.F.);
#71902=ORIENTED_EDGE('',*,*,#50924,.F.);
#71903=ORIENTED_EDGE('',*,*,#50939,.T.);
#71904=ORIENTED_EDGE('',*,*,#49972,.F.);
#71905=ORIENTED_EDGE('',*,*,#50940,.F.);
#71906=ORIENTED_EDGE('',*,*,#50915,.F.);
#71907=ORIENTED_EDGE('',*,*,#50941,.T.);
#71908=ORIENTED_EDGE('',*,*,#50916,.F.);
#71909=ORIENTED_EDGE('',*,*,#50940,.T.);
#71910=ORIENTED_EDGE('',*,*,#50880,.F.);
#71911=ORIENTED_EDGE('',*,*,#50942,.T.);
#71912=ORIENTED_EDGE('',*,*,#50917,.F.);
#71913=ORIENTED_EDGE('',*,*,#50941,.F.);
#71914=ORIENTED_EDGE('',*,*,#50508,.F.);
#71915=ORIENTED_EDGE('',*,*,#50934,.T.);
#71916=ORIENTED_EDGE('',*,*,#50930,.T.);
#71917=ORIENTED_EDGE('',*,*,#50942,.F.);
#71918=ORIENTED_EDGE('',*,*,#50507,.T.);
#71919=ORIENTED_EDGE('',*,*,#50928,.T.);
#71920=ORIENTED_EDGE('',*,*,#50931,.T.);
#71921=ORIENTED_EDGE('',*,*,#50933,.T.);
#71922=ORIENTED_EDGE('',*,*,#50943,.T.);
#71923=ORIENTED_EDGE('',*,*,#50944,.T.);
#71924=ORIENTED_EDGE('',*,*,#50945,.T.);
#71925=ORIENTED_EDGE('',*,*,#50946,.T.);
#71926=ORIENTED_EDGE('',*,*,#50947,.T.);
#71927=ORIENTED_EDGE('',*,*,#50948,.T.);
#71928=ORIENTED_EDGE('',*,*,#50949,.T.);
#71929=ORIENTED_EDGE('',*,*,#50950,.F.);
#71930=ORIENTED_EDGE('',*,*,#50951,.T.);
#71931=ORIENTED_EDGE('',*,*,#50952,.T.);
#71932=ORIENTED_EDGE('',*,*,#50950,.T.);
#71933=ORIENTED_EDGE('',*,*,#50953,.T.);
#71934=ORIENTED_EDGE('',*,*,#50943,.F.);
#71935=ORIENTED_EDGE('',*,*,#50954,.T.);
#71936=ORIENTED_EDGE('',*,*,#50955,.F.);
#71937=ORIENTED_EDGE('',*,*,#50951,.F.);
#71938=ORIENTED_EDGE('',*,*,#50956,.F.);
#71939=ORIENTED_EDGE('',*,*,#50957,.F.);
#71940=ORIENTED_EDGE('',*,*,#50956,.T.);
#71941=ORIENTED_EDGE('',*,*,#50954,.F.);
#71942=ORIENTED_EDGE('',*,*,#50958,.F.);
#71943=ORIENTED_EDGE('',*,*,#50958,.T.);
#71944=ORIENTED_EDGE('',*,*,#50947,.F.);
#71945=ORIENTED_EDGE('',*,*,#50959,.F.);
#71946=ORIENTED_EDGE('',*,*,#50960,.F.);
#71947=ORIENTED_EDGE('',*,*,#50961,.T.);
#71948=ORIENTED_EDGE('',*,*,#50962,.F.);
#71949=ORIENTED_EDGE('',*,*,#50963,.F.);
#71950=ORIENTED_EDGE('',*,*,#50518,.F.);
#71951=ORIENTED_EDGE('',*,*,#50964,.T.);
#71952=ORIENTED_EDGE('',*,*,#50955,.T.);
#71953=ORIENTED_EDGE('',*,*,#50961,.F.);
#71954=ORIENTED_EDGE('',*,*,#50517,.T.);
#71955=ORIENTED_EDGE('',*,*,#50965,.F.);
#71956=ORIENTED_EDGE('',*,*,#50952,.F.);
#71957=ORIENTED_EDGE('',*,*,#50964,.F.);
#71958=ORIENTED_EDGE('',*,*,#50516,.F.);
#71959=ORIENTED_EDGE('',*,*,#50965,.T.);
#71960=ORIENTED_EDGE('',*,*,#50849,.F.);
#71961=ORIENTED_EDGE('',*,*,#50966,.F.);
#71962=ORIENTED_EDGE('',*,*,#50948,.F.);
#71963=ORIENTED_EDGE('',*,*,#50966,.T.);
#71964=ORIENTED_EDGE('',*,*,#49966,.F.);
#71965=ORIENTED_EDGE('',*,*,#50967,.F.);
#71966=ORIENTED_EDGE('',*,*,#50949,.F.);
#71967=ORIENTED_EDGE('',*,*,#50967,.T.);
#71968=ORIENTED_EDGE('',*,*,#49965,.F.);
#71969=ORIENTED_EDGE('',*,*,#50968,.F.);
#71970=ORIENTED_EDGE('',*,*,#50953,.F.);
#71971=ORIENTED_EDGE('',*,*,#50968,.T.);
#71972=ORIENTED_EDGE('',*,*,#49964,.F.);
#71973=ORIENTED_EDGE('',*,*,#50969,.F.);
#71974=ORIENTED_EDGE('',*,*,#50944,.F.);
#71975=ORIENTED_EDGE('',*,*,#50970,.T.);
#71976=ORIENTED_EDGE('',*,*,#50945,.F.);
#71977=ORIENTED_EDGE('',*,*,#50969,.T.);
#71978=ORIENTED_EDGE('',*,*,#50848,.F.);
#71979=ORIENTED_EDGE('',*,*,#50971,.T.);
#71980=ORIENTED_EDGE('',*,*,#50946,.F.);
#71981=ORIENTED_EDGE('',*,*,#50970,.F.);
#71982=ORIENTED_EDGE('',*,*,#50520,.F.);
#71983=ORIENTED_EDGE('',*,*,#50963,.T.);
#71984=ORIENTED_EDGE('',*,*,#50959,.T.);
#71985=ORIENTED_EDGE('',*,*,#50971,.F.);
#71986=ORIENTED_EDGE('',*,*,#50519,.T.);
#71987=ORIENTED_EDGE('',*,*,#50957,.T.);
#71988=ORIENTED_EDGE('',*,*,#50960,.T.);
#71989=ORIENTED_EDGE('',*,*,#50962,.T.);
#71990=ORIENTED_EDGE('',*,*,#50972,.T.);
#71991=ORIENTED_EDGE('',*,*,#50973,.T.);
#71992=ORIENTED_EDGE('',*,*,#50974,.T.);
#71993=ORIENTED_EDGE('',*,*,#50975,.T.);
#71994=ORIENTED_EDGE('',*,*,#50976,.T.);
#71995=ORIENTED_EDGE('',*,*,#50977,.T.);
#71996=ORIENTED_EDGE('',*,*,#50978,.T.);
#71997=ORIENTED_EDGE('',*,*,#50979,.F.);
#71998=ORIENTED_EDGE('',*,*,#50980,.T.);
#71999=ORIENTED_EDGE('',*,*,#50981,.T.);
#72000=ORIENTED_EDGE('',*,*,#50979,.T.);
#72001=ORIENTED_EDGE('',*,*,#50982,.T.);
#72002=ORIENTED_EDGE('',*,*,#50972,.F.);
#72003=ORIENTED_EDGE('',*,*,#50983,.T.);
#72004=ORIENTED_EDGE('',*,*,#50984,.F.);
#72005=ORIENTED_EDGE('',*,*,#50980,.F.);
#72006=ORIENTED_EDGE('',*,*,#50985,.F.);
#72007=ORIENTED_EDGE('',*,*,#50986,.F.);
#72008=ORIENTED_EDGE('',*,*,#50985,.T.);
#72009=ORIENTED_EDGE('',*,*,#50983,.F.);
#72010=ORIENTED_EDGE('',*,*,#50987,.F.);
#72011=ORIENTED_EDGE('',*,*,#50987,.T.);
#72012=ORIENTED_EDGE('',*,*,#50976,.F.);
#72013=ORIENTED_EDGE('',*,*,#50988,.F.);
#72014=ORIENTED_EDGE('',*,*,#50989,.F.);
#72015=ORIENTED_EDGE('',*,*,#50990,.T.);
#72016=ORIENTED_EDGE('',*,*,#50991,.F.);
#72017=ORIENTED_EDGE('',*,*,#50992,.F.);
#72018=ORIENTED_EDGE('',*,*,#50524,.F.);
#72019=ORIENTED_EDGE('',*,*,#50993,.T.);
#72020=ORIENTED_EDGE('',*,*,#50984,.T.);
#72021=ORIENTED_EDGE('',*,*,#50990,.F.);
#72022=ORIENTED_EDGE('',*,*,#50523,.T.);
#72023=ORIENTED_EDGE('',*,*,#50994,.F.);
#72024=ORIENTED_EDGE('',*,*,#50981,.F.);
#72025=ORIENTED_EDGE('',*,*,#50993,.F.);
#72026=ORIENTED_EDGE('',*,*,#50522,.F.);
#72027=ORIENTED_EDGE('',*,*,#50994,.T.);
#72028=ORIENTED_EDGE('',*,*,#50847,.F.);
#72029=ORIENTED_EDGE('',*,*,#50995,.F.);
#72030=ORIENTED_EDGE('',*,*,#50977,.F.);
#72031=ORIENTED_EDGE('',*,*,#50995,.T.);
#72032=ORIENTED_EDGE('',*,*,#49962,.F.);
#72033=ORIENTED_EDGE('',*,*,#50996,.F.);
#72034=ORIENTED_EDGE('',*,*,#50978,.F.);
#72035=ORIENTED_EDGE('',*,*,#50996,.T.);
#72036=ORIENTED_EDGE('',*,*,#49961,.F.);
#72037=ORIENTED_EDGE('',*,*,#50997,.F.);
#72038=ORIENTED_EDGE('',*,*,#50982,.F.);
#72039=ORIENTED_EDGE('',*,*,#50997,.T.);
#72040=ORIENTED_EDGE('',*,*,#49960,.F.);
#72041=ORIENTED_EDGE('',*,*,#50998,.F.);
#72042=ORIENTED_EDGE('',*,*,#50973,.F.);
#72043=ORIENTED_EDGE('',*,*,#50999,.T.);
#72044=ORIENTED_EDGE('',*,*,#50974,.F.);
#72045=ORIENTED_EDGE('',*,*,#50998,.T.);
#72046=ORIENTED_EDGE('',*,*,#50846,.F.);
#72047=ORIENTED_EDGE('',*,*,#51000,.T.);
#72048=ORIENTED_EDGE('',*,*,#50975,.F.);
#72049=ORIENTED_EDGE('',*,*,#50999,.F.);
#72050=ORIENTED_EDGE('',*,*,#50526,.F.);
#72051=ORIENTED_EDGE('',*,*,#50992,.T.);
#72052=ORIENTED_EDGE('',*,*,#50988,.T.);
#72053=ORIENTED_EDGE('',*,*,#51000,.F.);
#72054=ORIENTED_EDGE('',*,*,#50525,.T.);
#72055=ORIENTED_EDGE('',*,*,#50986,.T.);
#72056=ORIENTED_EDGE('',*,*,#50989,.T.);
#72057=ORIENTED_EDGE('',*,*,#50991,.T.);
#72058=ORIENTED_EDGE('',*,*,#51001,.T.);
#72059=ORIENTED_EDGE('',*,*,#51002,.T.);
#72060=ORIENTED_EDGE('',*,*,#51003,.T.);
#72061=ORIENTED_EDGE('',*,*,#51004,.T.);
#72062=ORIENTED_EDGE('',*,*,#51005,.T.);
#72063=ORIENTED_EDGE('',*,*,#51006,.T.);
#72064=ORIENTED_EDGE('',*,*,#51007,.T.);
#72065=ORIENTED_EDGE('',*,*,#51008,.F.);
#72066=ORIENTED_EDGE('',*,*,#51009,.T.);
#72067=ORIENTED_EDGE('',*,*,#51010,.T.);
#72068=ORIENTED_EDGE('',*,*,#51008,.T.);
#72069=ORIENTED_EDGE('',*,*,#51011,.T.);
#72070=ORIENTED_EDGE('',*,*,#51001,.F.);
#72071=ORIENTED_EDGE('',*,*,#51012,.T.);
#72072=ORIENTED_EDGE('',*,*,#51013,.F.);
#72073=ORIENTED_EDGE('',*,*,#51009,.F.);
#72074=ORIENTED_EDGE('',*,*,#51014,.F.);
#72075=ORIENTED_EDGE('',*,*,#51015,.F.);
#72076=ORIENTED_EDGE('',*,*,#51014,.T.);
#72077=ORIENTED_EDGE('',*,*,#51012,.F.);
#72078=ORIENTED_EDGE('',*,*,#51016,.F.);
#72079=ORIENTED_EDGE('',*,*,#51016,.T.);
#72080=ORIENTED_EDGE('',*,*,#51005,.F.);
#72081=ORIENTED_EDGE('',*,*,#51017,.F.);
#72082=ORIENTED_EDGE('',*,*,#51018,.F.);
#72083=ORIENTED_EDGE('',*,*,#51019,.T.);
#72084=ORIENTED_EDGE('',*,*,#51020,.F.);
#72085=ORIENTED_EDGE('',*,*,#51021,.F.);
#72086=ORIENTED_EDGE('',*,*,#50530,.F.);
#72087=ORIENTED_EDGE('',*,*,#51022,.T.);
#72088=ORIENTED_EDGE('',*,*,#51013,.T.);
#72089=ORIENTED_EDGE('',*,*,#51019,.F.);
#72090=ORIENTED_EDGE('',*,*,#50529,.T.);
#72091=ORIENTED_EDGE('',*,*,#51023,.F.);
#72092=ORIENTED_EDGE('',*,*,#51010,.F.);
#72093=ORIENTED_EDGE('',*,*,#51022,.F.);
#72094=ORIENTED_EDGE('',*,*,#50528,.F.);
#72095=ORIENTED_EDGE('',*,*,#51023,.T.);
#72096=ORIENTED_EDGE('',*,*,#50845,.F.);
#72097=ORIENTED_EDGE('',*,*,#51024,.F.);
#72098=ORIENTED_EDGE('',*,*,#51006,.F.);
#72099=ORIENTED_EDGE('',*,*,#51024,.T.);
#72100=ORIENTED_EDGE('',*,*,#49958,.F.);
#72101=ORIENTED_EDGE('',*,*,#51025,.F.);
#72102=ORIENTED_EDGE('',*,*,#51007,.F.);
#72103=ORIENTED_EDGE('',*,*,#51025,.T.);
#72104=ORIENTED_EDGE('',*,*,#49957,.F.);
#72105=ORIENTED_EDGE('',*,*,#51026,.F.);
#72106=ORIENTED_EDGE('',*,*,#51011,.F.);
#72107=ORIENTED_EDGE('',*,*,#51026,.T.);
#72108=ORIENTED_EDGE('',*,*,#49956,.F.);
#72109=ORIENTED_EDGE('',*,*,#51027,.F.);
#72110=ORIENTED_EDGE('',*,*,#51002,.F.);
#72111=ORIENTED_EDGE('',*,*,#51028,.T.);
#72112=ORIENTED_EDGE('',*,*,#51003,.F.);
#72113=ORIENTED_EDGE('',*,*,#51027,.T.);
#72114=ORIENTED_EDGE('',*,*,#50844,.F.);
#72115=ORIENTED_EDGE('',*,*,#51029,.T.);
#72116=ORIENTED_EDGE('',*,*,#51004,.F.);
#72117=ORIENTED_EDGE('',*,*,#51028,.F.);
#72118=ORIENTED_EDGE('',*,*,#50532,.F.);
#72119=ORIENTED_EDGE('',*,*,#51021,.T.);
#72120=ORIENTED_EDGE('',*,*,#51017,.T.);
#72121=ORIENTED_EDGE('',*,*,#51029,.F.);
#72122=ORIENTED_EDGE('',*,*,#50531,.T.);
#72123=ORIENTED_EDGE('',*,*,#51015,.T.);
#72124=ORIENTED_EDGE('',*,*,#51018,.T.);
#72125=ORIENTED_EDGE('',*,*,#51020,.T.);
#72126=ORIENTED_EDGE('',*,*,#51030,.T.);
#72127=ORIENTED_EDGE('',*,*,#51031,.T.);
#72128=ORIENTED_EDGE('',*,*,#51032,.T.);
#72129=ORIENTED_EDGE('',*,*,#51033,.T.);
#72130=ORIENTED_EDGE('',*,*,#51034,.T.);
#72131=ORIENTED_EDGE('',*,*,#51035,.T.);
#72132=ORIENTED_EDGE('',*,*,#51036,.T.);
#72133=ORIENTED_EDGE('',*,*,#51037,.F.);
#72134=ORIENTED_EDGE('',*,*,#51038,.T.);
#72135=ORIENTED_EDGE('',*,*,#51039,.T.);
#72136=ORIENTED_EDGE('',*,*,#51037,.T.);
#72137=ORIENTED_EDGE('',*,*,#51040,.T.);
#72138=ORIENTED_EDGE('',*,*,#51030,.F.);
#72139=ORIENTED_EDGE('',*,*,#51041,.T.);
#72140=ORIENTED_EDGE('',*,*,#51042,.F.);
#72141=ORIENTED_EDGE('',*,*,#51038,.F.);
#72142=ORIENTED_EDGE('',*,*,#51043,.F.);
#72143=ORIENTED_EDGE('',*,*,#51044,.F.);
#72144=ORIENTED_EDGE('',*,*,#51043,.T.);
#72145=ORIENTED_EDGE('',*,*,#51041,.F.);
#72146=ORIENTED_EDGE('',*,*,#51045,.F.);
#72147=ORIENTED_EDGE('',*,*,#51045,.T.);
#72148=ORIENTED_EDGE('',*,*,#51034,.F.);
#72149=ORIENTED_EDGE('',*,*,#51046,.F.);
#72150=ORIENTED_EDGE('',*,*,#51047,.F.);
#72151=ORIENTED_EDGE('',*,*,#51048,.T.);
#72152=ORIENTED_EDGE('',*,*,#51049,.F.);
#72153=ORIENTED_EDGE('',*,*,#51050,.F.);
#72154=ORIENTED_EDGE('',*,*,#50536,.F.);
#72155=ORIENTED_EDGE('',*,*,#51051,.T.);
#72156=ORIENTED_EDGE('',*,*,#51042,.T.);
#72157=ORIENTED_EDGE('',*,*,#51048,.F.);
#72158=ORIENTED_EDGE('',*,*,#50535,.T.);
#72159=ORIENTED_EDGE('',*,*,#51052,.F.);
#72160=ORIENTED_EDGE('',*,*,#51039,.F.);
#72161=ORIENTED_EDGE('',*,*,#51051,.F.);
#72162=ORIENTED_EDGE('',*,*,#50534,.F.);
#72163=ORIENTED_EDGE('',*,*,#51052,.T.);
#72164=ORIENTED_EDGE('',*,*,#50843,.F.);
#72165=ORIENTED_EDGE('',*,*,#51053,.F.);
#72166=ORIENTED_EDGE('',*,*,#51035,.F.);
#72167=ORIENTED_EDGE('',*,*,#51053,.T.);
#72168=ORIENTED_EDGE('',*,*,#49954,.F.);
#72169=ORIENTED_EDGE('',*,*,#51054,.F.);
#72170=ORIENTED_EDGE('',*,*,#51036,.F.);
#72171=ORIENTED_EDGE('',*,*,#51054,.T.);
#72172=ORIENTED_EDGE('',*,*,#49953,.F.);
#72173=ORIENTED_EDGE('',*,*,#51055,.F.);
#72174=ORIENTED_EDGE('',*,*,#51040,.F.);
#72175=ORIENTED_EDGE('',*,*,#51055,.T.);
#72176=ORIENTED_EDGE('',*,*,#49952,.F.);
#72177=ORIENTED_EDGE('',*,*,#51056,.F.);
#72178=ORIENTED_EDGE('',*,*,#51031,.F.);
#72179=ORIENTED_EDGE('',*,*,#51057,.T.);
#72180=ORIENTED_EDGE('',*,*,#51032,.F.);
#72181=ORIENTED_EDGE('',*,*,#51056,.T.);
#72182=ORIENTED_EDGE('',*,*,#50842,.F.);
#72183=ORIENTED_EDGE('',*,*,#51058,.T.);
#72184=ORIENTED_EDGE('',*,*,#51033,.F.);
#72185=ORIENTED_EDGE('',*,*,#51057,.F.);
#72186=ORIENTED_EDGE('',*,*,#50538,.F.);
#72187=ORIENTED_EDGE('',*,*,#51050,.T.);
#72188=ORIENTED_EDGE('',*,*,#51046,.T.);
#72189=ORIENTED_EDGE('',*,*,#51058,.F.);
#72190=ORIENTED_EDGE('',*,*,#50537,.T.);
#72191=ORIENTED_EDGE('',*,*,#51044,.T.);
#72192=ORIENTED_EDGE('',*,*,#51047,.T.);
#72193=ORIENTED_EDGE('',*,*,#51049,.T.);
#72194=ORIENTED_EDGE('',*,*,#51059,.T.);
#72195=ORIENTED_EDGE('',*,*,#51060,.T.);
#72196=ORIENTED_EDGE('',*,*,#51061,.T.);
#72197=ORIENTED_EDGE('',*,*,#51062,.T.);
#72198=ORIENTED_EDGE('',*,*,#51063,.T.);
#72199=ORIENTED_EDGE('',*,*,#51064,.T.);
#72200=ORIENTED_EDGE('',*,*,#51065,.T.);
#72201=ORIENTED_EDGE('',*,*,#51066,.F.);
#72202=ORIENTED_EDGE('',*,*,#51067,.T.);
#72203=ORIENTED_EDGE('',*,*,#51068,.T.);
#72204=ORIENTED_EDGE('',*,*,#51066,.T.);
#72205=ORIENTED_EDGE('',*,*,#51069,.T.);
#72206=ORIENTED_EDGE('',*,*,#51059,.F.);
#72207=ORIENTED_EDGE('',*,*,#51070,.T.);
#72208=ORIENTED_EDGE('',*,*,#51071,.F.);
#72209=ORIENTED_EDGE('',*,*,#51067,.F.);
#72210=ORIENTED_EDGE('',*,*,#51072,.F.);
#72211=ORIENTED_EDGE('',*,*,#51073,.F.);
#72212=ORIENTED_EDGE('',*,*,#51072,.T.);
#72213=ORIENTED_EDGE('',*,*,#51070,.F.);
#72214=ORIENTED_EDGE('',*,*,#51074,.F.);
#72215=ORIENTED_EDGE('',*,*,#51074,.T.);
#72216=ORIENTED_EDGE('',*,*,#51063,.F.);
#72217=ORIENTED_EDGE('',*,*,#51075,.F.);
#72218=ORIENTED_EDGE('',*,*,#51076,.F.);
#72219=ORIENTED_EDGE('',*,*,#51077,.T.);
#72220=ORIENTED_EDGE('',*,*,#51078,.F.);
#72221=ORIENTED_EDGE('',*,*,#51079,.F.);
#72222=ORIENTED_EDGE('',*,*,#50542,.F.);
#72223=ORIENTED_EDGE('',*,*,#51080,.T.);
#72224=ORIENTED_EDGE('',*,*,#51071,.T.);
#72225=ORIENTED_EDGE('',*,*,#51077,.F.);
#72226=ORIENTED_EDGE('',*,*,#50541,.T.);
#72227=ORIENTED_EDGE('',*,*,#51081,.F.);
#72228=ORIENTED_EDGE('',*,*,#51068,.F.);
#72229=ORIENTED_EDGE('',*,*,#51080,.F.);
#72230=ORIENTED_EDGE('',*,*,#50540,.F.);
#72231=ORIENTED_EDGE('',*,*,#51081,.T.);
#72232=ORIENTED_EDGE('',*,*,#50841,.F.);
#72233=ORIENTED_EDGE('',*,*,#51082,.F.);
#72234=ORIENTED_EDGE('',*,*,#51064,.F.);
#72235=ORIENTED_EDGE('',*,*,#51082,.T.);
#72236=ORIENTED_EDGE('',*,*,#49950,.F.);
#72237=ORIENTED_EDGE('',*,*,#51083,.F.);
#72238=ORIENTED_EDGE('',*,*,#51065,.F.);
#72239=ORIENTED_EDGE('',*,*,#51083,.T.);
#72240=ORIENTED_EDGE('',*,*,#49949,.F.);
#72241=ORIENTED_EDGE('',*,*,#51084,.F.);
#72242=ORIENTED_EDGE('',*,*,#51069,.F.);
#72243=ORIENTED_EDGE('',*,*,#51084,.T.);
#72244=ORIENTED_EDGE('',*,*,#49948,.F.);
#72245=ORIENTED_EDGE('',*,*,#51085,.F.);
#72246=ORIENTED_EDGE('',*,*,#51060,.F.);
#72247=ORIENTED_EDGE('',*,*,#51086,.T.);
#72248=ORIENTED_EDGE('',*,*,#51061,.F.);
#72249=ORIENTED_EDGE('',*,*,#51085,.T.);
#72250=ORIENTED_EDGE('',*,*,#50840,.F.);
#72251=ORIENTED_EDGE('',*,*,#51087,.T.);
#72252=ORIENTED_EDGE('',*,*,#51062,.F.);
#72253=ORIENTED_EDGE('',*,*,#51086,.F.);
#72254=ORIENTED_EDGE('',*,*,#50544,.F.);
#72255=ORIENTED_EDGE('',*,*,#51079,.T.);
#72256=ORIENTED_EDGE('',*,*,#51075,.T.);
#72257=ORIENTED_EDGE('',*,*,#51087,.F.);
#72258=ORIENTED_EDGE('',*,*,#50543,.T.);
#72259=ORIENTED_EDGE('',*,*,#51073,.T.);
#72260=ORIENTED_EDGE('',*,*,#51076,.T.);
#72261=ORIENTED_EDGE('',*,*,#51078,.T.);
#72262=ORIENTED_EDGE('',*,*,#51088,.T.);
#72263=ORIENTED_EDGE('',*,*,#51089,.T.);
#72264=ORIENTED_EDGE('',*,*,#51090,.T.);
#72265=ORIENTED_EDGE('',*,*,#51091,.T.);
#72266=ORIENTED_EDGE('',*,*,#51092,.T.);
#72267=ORIENTED_EDGE('',*,*,#51093,.T.);
#72268=ORIENTED_EDGE('',*,*,#51094,.T.);
#72269=ORIENTED_EDGE('',*,*,#51095,.F.);
#72270=ORIENTED_EDGE('',*,*,#51096,.T.);
#72271=ORIENTED_EDGE('',*,*,#51097,.T.);
#72272=ORIENTED_EDGE('',*,*,#51095,.T.);
#72273=ORIENTED_EDGE('',*,*,#51098,.T.);
#72274=ORIENTED_EDGE('',*,*,#51088,.F.);
#72275=ORIENTED_EDGE('',*,*,#51099,.T.);
#72276=ORIENTED_EDGE('',*,*,#51100,.F.);
#72277=ORIENTED_EDGE('',*,*,#51096,.F.);
#72278=ORIENTED_EDGE('',*,*,#51101,.F.);
#72279=ORIENTED_EDGE('',*,*,#51102,.F.);
#72280=ORIENTED_EDGE('',*,*,#51101,.T.);
#72281=ORIENTED_EDGE('',*,*,#51099,.F.);
#72282=ORIENTED_EDGE('',*,*,#51103,.F.);
#72283=ORIENTED_EDGE('',*,*,#51103,.T.);
#72284=ORIENTED_EDGE('',*,*,#51092,.F.);
#72285=ORIENTED_EDGE('',*,*,#51104,.F.);
#72286=ORIENTED_EDGE('',*,*,#51105,.F.);
#72287=ORIENTED_EDGE('',*,*,#51106,.T.);
#72288=ORIENTED_EDGE('',*,*,#51107,.F.);
#72289=ORIENTED_EDGE('',*,*,#51108,.F.);
#72290=ORIENTED_EDGE('',*,*,#50548,.F.);
#72291=ORIENTED_EDGE('',*,*,#51109,.T.);
#72292=ORIENTED_EDGE('',*,*,#51100,.T.);
#72293=ORIENTED_EDGE('',*,*,#51106,.F.);
#72294=ORIENTED_EDGE('',*,*,#50547,.T.);
#72295=ORIENTED_EDGE('',*,*,#51110,.F.);
#72296=ORIENTED_EDGE('',*,*,#51097,.F.);
#72297=ORIENTED_EDGE('',*,*,#51109,.F.);
#72298=ORIENTED_EDGE('',*,*,#50546,.F.);
#72299=ORIENTED_EDGE('',*,*,#51110,.T.);
#72300=ORIENTED_EDGE('',*,*,#50839,.F.);
#72301=ORIENTED_EDGE('',*,*,#51111,.F.);
#72302=ORIENTED_EDGE('',*,*,#51093,.F.);
#72303=ORIENTED_EDGE('',*,*,#51111,.T.);
#72304=ORIENTED_EDGE('',*,*,#49946,.F.);
#72305=ORIENTED_EDGE('',*,*,#51112,.F.);
#72306=ORIENTED_EDGE('',*,*,#51094,.F.);
#72307=ORIENTED_EDGE('',*,*,#51112,.T.);
#72308=ORIENTED_EDGE('',*,*,#49945,.F.);
#72309=ORIENTED_EDGE('',*,*,#51113,.F.);
#72310=ORIENTED_EDGE('',*,*,#51098,.F.);
#72311=ORIENTED_EDGE('',*,*,#51113,.T.);
#72312=ORIENTED_EDGE('',*,*,#49944,.F.);
#72313=ORIENTED_EDGE('',*,*,#51114,.F.);
#72314=ORIENTED_EDGE('',*,*,#51089,.F.);
#72315=ORIENTED_EDGE('',*,*,#51115,.T.);
#72316=ORIENTED_EDGE('',*,*,#51090,.F.);
#72317=ORIENTED_EDGE('',*,*,#51114,.T.);
#72318=ORIENTED_EDGE('',*,*,#50838,.F.);
#72319=ORIENTED_EDGE('',*,*,#51116,.T.);
#72320=ORIENTED_EDGE('',*,*,#51091,.F.);
#72321=ORIENTED_EDGE('',*,*,#51115,.F.);
#72322=ORIENTED_EDGE('',*,*,#50550,.F.);
#72323=ORIENTED_EDGE('',*,*,#51108,.T.);
#72324=ORIENTED_EDGE('',*,*,#51104,.T.);
#72325=ORIENTED_EDGE('',*,*,#51116,.F.);
#72326=ORIENTED_EDGE('',*,*,#50549,.T.);
#72327=ORIENTED_EDGE('',*,*,#51102,.T.);
#72328=ORIENTED_EDGE('',*,*,#51105,.T.);
#72329=ORIENTED_EDGE('',*,*,#51107,.T.);
#72330=ORIENTED_EDGE('',*,*,#51117,.T.);
#72331=ORIENTED_EDGE('',*,*,#51118,.T.);
#72332=ORIENTED_EDGE('',*,*,#51119,.T.);
#72333=ORIENTED_EDGE('',*,*,#51120,.T.);
#72334=ORIENTED_EDGE('',*,*,#51121,.T.);
#72335=ORIENTED_EDGE('',*,*,#51122,.T.);
#72336=ORIENTED_EDGE('',*,*,#51123,.T.);
#72337=ORIENTED_EDGE('',*,*,#51124,.F.);
#72338=ORIENTED_EDGE('',*,*,#51125,.T.);
#72339=ORIENTED_EDGE('',*,*,#51126,.T.);
#72340=ORIENTED_EDGE('',*,*,#51124,.T.);
#72341=ORIENTED_EDGE('',*,*,#51127,.T.);
#72342=ORIENTED_EDGE('',*,*,#51117,.F.);
#72343=ORIENTED_EDGE('',*,*,#51128,.T.);
#72344=ORIENTED_EDGE('',*,*,#51129,.F.);
#72345=ORIENTED_EDGE('',*,*,#51125,.F.);
#72346=ORIENTED_EDGE('',*,*,#51130,.F.);
#72347=ORIENTED_EDGE('',*,*,#51131,.F.);
#72348=ORIENTED_EDGE('',*,*,#51130,.T.);
#72349=ORIENTED_EDGE('',*,*,#51128,.F.);
#72350=ORIENTED_EDGE('',*,*,#51132,.F.);
#72351=ORIENTED_EDGE('',*,*,#51132,.T.);
#72352=ORIENTED_EDGE('',*,*,#51121,.F.);
#72353=ORIENTED_EDGE('',*,*,#51133,.F.);
#72354=ORIENTED_EDGE('',*,*,#51134,.F.);
#72355=ORIENTED_EDGE('',*,*,#51135,.T.);
#72356=ORIENTED_EDGE('',*,*,#51136,.F.);
#72357=ORIENTED_EDGE('',*,*,#51137,.F.);
#72358=ORIENTED_EDGE('',*,*,#50554,.F.);
#72359=ORIENTED_EDGE('',*,*,#51138,.T.);
#72360=ORIENTED_EDGE('',*,*,#51129,.T.);
#72361=ORIENTED_EDGE('',*,*,#51135,.F.);
#72362=ORIENTED_EDGE('',*,*,#50553,.T.);
#72363=ORIENTED_EDGE('',*,*,#51139,.F.);
#72364=ORIENTED_EDGE('',*,*,#51126,.F.);
#72365=ORIENTED_EDGE('',*,*,#51138,.F.);
#72366=ORIENTED_EDGE('',*,*,#50552,.F.);
#72367=ORIENTED_EDGE('',*,*,#51139,.T.);
#72368=ORIENTED_EDGE('',*,*,#50837,.F.);
#72369=ORIENTED_EDGE('',*,*,#51140,.F.);
#72370=ORIENTED_EDGE('',*,*,#51122,.F.);
#72371=ORIENTED_EDGE('',*,*,#51140,.T.);
#72372=ORIENTED_EDGE('',*,*,#49942,.F.);
#72373=ORIENTED_EDGE('',*,*,#51141,.F.);
#72374=ORIENTED_EDGE('',*,*,#51123,.F.);
#72375=ORIENTED_EDGE('',*,*,#51141,.T.);
#72376=ORIENTED_EDGE('',*,*,#49941,.F.);
#72377=ORIENTED_EDGE('',*,*,#51142,.F.);
#72378=ORIENTED_EDGE('',*,*,#51127,.F.);
#72379=ORIENTED_EDGE('',*,*,#51142,.T.);
#72380=ORIENTED_EDGE('',*,*,#49940,.F.);
#72381=ORIENTED_EDGE('',*,*,#51143,.F.);
#72382=ORIENTED_EDGE('',*,*,#51118,.F.);
#72383=ORIENTED_EDGE('',*,*,#51144,.T.);
#72384=ORIENTED_EDGE('',*,*,#51119,.F.);
#72385=ORIENTED_EDGE('',*,*,#51143,.T.);
#72386=ORIENTED_EDGE('',*,*,#50836,.F.);
#72387=ORIENTED_EDGE('',*,*,#51145,.T.);
#72388=ORIENTED_EDGE('',*,*,#51120,.F.);
#72389=ORIENTED_EDGE('',*,*,#51144,.F.);
#72390=ORIENTED_EDGE('',*,*,#50556,.F.);
#72391=ORIENTED_EDGE('',*,*,#51137,.T.);
#72392=ORIENTED_EDGE('',*,*,#51133,.T.);
#72393=ORIENTED_EDGE('',*,*,#51145,.F.);
#72394=ORIENTED_EDGE('',*,*,#50555,.T.);
#72395=ORIENTED_EDGE('',*,*,#51131,.T.);
#72396=ORIENTED_EDGE('',*,*,#51134,.T.);
#72397=ORIENTED_EDGE('',*,*,#51136,.T.);
#72398=ORIENTED_EDGE('',*,*,#51146,.T.);
#72399=ORIENTED_EDGE('',*,*,#51147,.T.);
#72400=ORIENTED_EDGE('',*,*,#51148,.T.);
#72401=ORIENTED_EDGE('',*,*,#51149,.T.);
#72402=ORIENTED_EDGE('',*,*,#51150,.T.);
#72403=ORIENTED_EDGE('',*,*,#51151,.T.);
#72404=ORIENTED_EDGE('',*,*,#51152,.T.);
#72405=ORIENTED_EDGE('',*,*,#51153,.F.);
#72406=ORIENTED_EDGE('',*,*,#51154,.T.);
#72407=ORIENTED_EDGE('',*,*,#51155,.T.);
#72408=ORIENTED_EDGE('',*,*,#51153,.T.);
#72409=ORIENTED_EDGE('',*,*,#51156,.T.);
#72410=ORIENTED_EDGE('',*,*,#51146,.F.);
#72411=ORIENTED_EDGE('',*,*,#51157,.T.);
#72412=ORIENTED_EDGE('',*,*,#51158,.F.);
#72413=ORIENTED_EDGE('',*,*,#51154,.F.);
#72414=ORIENTED_EDGE('',*,*,#51159,.F.);
#72415=ORIENTED_EDGE('',*,*,#51160,.F.);
#72416=ORIENTED_EDGE('',*,*,#51159,.T.);
#72417=ORIENTED_EDGE('',*,*,#51157,.F.);
#72418=ORIENTED_EDGE('',*,*,#51161,.F.);
#72419=ORIENTED_EDGE('',*,*,#51161,.T.);
#72420=ORIENTED_EDGE('',*,*,#51150,.F.);
#72421=ORIENTED_EDGE('',*,*,#51162,.F.);
#72422=ORIENTED_EDGE('',*,*,#51163,.F.);
#72423=ORIENTED_EDGE('',*,*,#51164,.T.);
#72424=ORIENTED_EDGE('',*,*,#51165,.F.);
#72425=ORIENTED_EDGE('',*,*,#51166,.F.);
#72426=ORIENTED_EDGE('',*,*,#50560,.F.);
#72427=ORIENTED_EDGE('',*,*,#51167,.T.);
#72428=ORIENTED_EDGE('',*,*,#51158,.T.);
#72429=ORIENTED_EDGE('',*,*,#51164,.F.);
#72430=ORIENTED_EDGE('',*,*,#50559,.T.);
#72431=ORIENTED_EDGE('',*,*,#51168,.F.);
#72432=ORIENTED_EDGE('',*,*,#51155,.F.);
#72433=ORIENTED_EDGE('',*,*,#51167,.F.);
#72434=ORIENTED_EDGE('',*,*,#50558,.F.);
#72435=ORIENTED_EDGE('',*,*,#51168,.T.);
#72436=ORIENTED_EDGE('',*,*,#50835,.F.);
#72437=ORIENTED_EDGE('',*,*,#51169,.F.);
#72438=ORIENTED_EDGE('',*,*,#51151,.F.);
#72439=ORIENTED_EDGE('',*,*,#51169,.T.);
#72440=ORIENTED_EDGE('',*,*,#49938,.F.);
#72441=ORIENTED_EDGE('',*,*,#51170,.F.);
#72442=ORIENTED_EDGE('',*,*,#51152,.F.);
#72443=ORIENTED_EDGE('',*,*,#51170,.T.);
#72444=ORIENTED_EDGE('',*,*,#49937,.F.);
#72445=ORIENTED_EDGE('',*,*,#51171,.F.);
#72446=ORIENTED_EDGE('',*,*,#51156,.F.);
#72447=ORIENTED_EDGE('',*,*,#51171,.T.);
#72448=ORIENTED_EDGE('',*,*,#49936,.F.);
#72449=ORIENTED_EDGE('',*,*,#51172,.F.);
#72450=ORIENTED_EDGE('',*,*,#51147,.F.);
#72451=ORIENTED_EDGE('',*,*,#51173,.T.);
#72452=ORIENTED_EDGE('',*,*,#51148,.F.);
#72453=ORIENTED_EDGE('',*,*,#51172,.T.);
#72454=ORIENTED_EDGE('',*,*,#50834,.F.);
#72455=ORIENTED_EDGE('',*,*,#51174,.T.);
#72456=ORIENTED_EDGE('',*,*,#51149,.F.);
#72457=ORIENTED_EDGE('',*,*,#51173,.F.);
#72458=ORIENTED_EDGE('',*,*,#50562,.F.);
#72459=ORIENTED_EDGE('',*,*,#51166,.T.);
#72460=ORIENTED_EDGE('',*,*,#51162,.T.);
#72461=ORIENTED_EDGE('',*,*,#51174,.F.);
#72462=ORIENTED_EDGE('',*,*,#50561,.T.);
#72463=ORIENTED_EDGE('',*,*,#51160,.T.);
#72464=ORIENTED_EDGE('',*,*,#51163,.T.);
#72465=ORIENTED_EDGE('',*,*,#51165,.T.);
#72466=ORIENTED_EDGE('',*,*,#51175,.T.);
#72467=ORIENTED_EDGE('',*,*,#51176,.T.);
#72468=ORIENTED_EDGE('',*,*,#51177,.T.);
#72469=ORIENTED_EDGE('',*,*,#51178,.T.);
#72470=ORIENTED_EDGE('',*,*,#51179,.T.);
#72471=ORIENTED_EDGE('',*,*,#51180,.T.);
#72472=ORIENTED_EDGE('',*,*,#51181,.T.);
#72473=ORIENTED_EDGE('',*,*,#51182,.F.);
#72474=ORIENTED_EDGE('',*,*,#51183,.T.);
#72475=ORIENTED_EDGE('',*,*,#51184,.T.);
#72476=ORIENTED_EDGE('',*,*,#51182,.T.);
#72477=ORIENTED_EDGE('',*,*,#51185,.T.);
#72478=ORIENTED_EDGE('',*,*,#51175,.F.);
#72479=ORIENTED_EDGE('',*,*,#51186,.T.);
#72480=ORIENTED_EDGE('',*,*,#51187,.F.);
#72481=ORIENTED_EDGE('',*,*,#51183,.F.);
#72482=ORIENTED_EDGE('',*,*,#51188,.F.);
#72483=ORIENTED_EDGE('',*,*,#51189,.F.);
#72484=ORIENTED_EDGE('',*,*,#51188,.T.);
#72485=ORIENTED_EDGE('',*,*,#51186,.F.);
#72486=ORIENTED_EDGE('',*,*,#51190,.F.);
#72487=ORIENTED_EDGE('',*,*,#51190,.T.);
#72488=ORIENTED_EDGE('',*,*,#51179,.F.);
#72489=ORIENTED_EDGE('',*,*,#51191,.F.);
#72490=ORIENTED_EDGE('',*,*,#51192,.F.);
#72491=ORIENTED_EDGE('',*,*,#51193,.T.);
#72492=ORIENTED_EDGE('',*,*,#51194,.F.);
#72493=ORIENTED_EDGE('',*,*,#51195,.F.);
#72494=ORIENTED_EDGE('',*,*,#50566,.F.);
#72495=ORIENTED_EDGE('',*,*,#51196,.T.);
#72496=ORIENTED_EDGE('',*,*,#51187,.T.);
#72497=ORIENTED_EDGE('',*,*,#51193,.F.);
#72498=ORIENTED_EDGE('',*,*,#50565,.T.);
#72499=ORIENTED_EDGE('',*,*,#51197,.F.);
#72500=ORIENTED_EDGE('',*,*,#51184,.F.);
#72501=ORIENTED_EDGE('',*,*,#51196,.F.);
#72502=ORIENTED_EDGE('',*,*,#50564,.F.);
#72503=ORIENTED_EDGE('',*,*,#51197,.T.);
#72504=ORIENTED_EDGE('',*,*,#50833,.F.);
#72505=ORIENTED_EDGE('',*,*,#51198,.F.);
#72506=ORIENTED_EDGE('',*,*,#51180,.F.);
#72507=ORIENTED_EDGE('',*,*,#51198,.T.);
#72508=ORIENTED_EDGE('',*,*,#49934,.F.);
#72509=ORIENTED_EDGE('',*,*,#51199,.F.);
#72510=ORIENTED_EDGE('',*,*,#51181,.F.);
#72511=ORIENTED_EDGE('',*,*,#51199,.T.);
#72512=ORIENTED_EDGE('',*,*,#49933,.F.);
#72513=ORIENTED_EDGE('',*,*,#51200,.F.);
#72514=ORIENTED_EDGE('',*,*,#51185,.F.);
#72515=ORIENTED_EDGE('',*,*,#51200,.T.);
#72516=ORIENTED_EDGE('',*,*,#49932,.F.);
#72517=ORIENTED_EDGE('',*,*,#51201,.F.);
#72518=ORIENTED_EDGE('',*,*,#51176,.F.);
#72519=ORIENTED_EDGE('',*,*,#51202,.T.);
#72520=ORIENTED_EDGE('',*,*,#51177,.F.);
#72521=ORIENTED_EDGE('',*,*,#51201,.T.);
#72522=ORIENTED_EDGE('',*,*,#50832,.F.);
#72523=ORIENTED_EDGE('',*,*,#51203,.T.);
#72524=ORIENTED_EDGE('',*,*,#51178,.F.);
#72525=ORIENTED_EDGE('',*,*,#51202,.F.);
#72526=ORIENTED_EDGE('',*,*,#50568,.F.);
#72527=ORIENTED_EDGE('',*,*,#51195,.T.);
#72528=ORIENTED_EDGE('',*,*,#51191,.T.);
#72529=ORIENTED_EDGE('',*,*,#51203,.F.);
#72530=ORIENTED_EDGE('',*,*,#50567,.T.);
#72531=ORIENTED_EDGE('',*,*,#51189,.T.);
#72532=ORIENTED_EDGE('',*,*,#51192,.T.);
#72533=ORIENTED_EDGE('',*,*,#51194,.T.);
#72534=ORIENTED_EDGE('',*,*,#51204,.T.);
#72535=ORIENTED_EDGE('',*,*,#51205,.T.);
#72536=ORIENTED_EDGE('',*,*,#51206,.T.);
#72537=ORIENTED_EDGE('',*,*,#51207,.T.);
#72538=ORIENTED_EDGE('',*,*,#51208,.T.);
#72539=ORIENTED_EDGE('',*,*,#51209,.T.);
#72540=ORIENTED_EDGE('',*,*,#51210,.T.);
#72541=ORIENTED_EDGE('',*,*,#51211,.F.);
#72542=ORIENTED_EDGE('',*,*,#51212,.T.);
#72543=ORIENTED_EDGE('',*,*,#51213,.T.);
#72544=ORIENTED_EDGE('',*,*,#51211,.T.);
#72545=ORIENTED_EDGE('',*,*,#51214,.T.);
#72546=ORIENTED_EDGE('',*,*,#51204,.F.);
#72547=ORIENTED_EDGE('',*,*,#51215,.T.);
#72548=ORIENTED_EDGE('',*,*,#51216,.F.);
#72549=ORIENTED_EDGE('',*,*,#51212,.F.);
#72550=ORIENTED_EDGE('',*,*,#51217,.F.);
#72551=ORIENTED_EDGE('',*,*,#51218,.F.);
#72552=ORIENTED_EDGE('',*,*,#51217,.T.);
#72553=ORIENTED_EDGE('',*,*,#51215,.F.);
#72554=ORIENTED_EDGE('',*,*,#51219,.F.);
#72555=ORIENTED_EDGE('',*,*,#51219,.T.);
#72556=ORIENTED_EDGE('',*,*,#51208,.F.);
#72557=ORIENTED_EDGE('',*,*,#51220,.F.);
#72558=ORIENTED_EDGE('',*,*,#51221,.F.);
#72559=ORIENTED_EDGE('',*,*,#51222,.T.);
#72560=ORIENTED_EDGE('',*,*,#51223,.F.);
#72561=ORIENTED_EDGE('',*,*,#51224,.F.);
#72562=ORIENTED_EDGE('',*,*,#50572,.F.);
#72563=ORIENTED_EDGE('',*,*,#51225,.T.);
#72564=ORIENTED_EDGE('',*,*,#51216,.T.);
#72565=ORIENTED_EDGE('',*,*,#51222,.F.);
#72566=ORIENTED_EDGE('',*,*,#50571,.T.);
#72567=ORIENTED_EDGE('',*,*,#51226,.F.);
#72568=ORIENTED_EDGE('',*,*,#51213,.F.);
#72569=ORIENTED_EDGE('',*,*,#51225,.F.);
#72570=ORIENTED_EDGE('',*,*,#50570,.F.);
#72571=ORIENTED_EDGE('',*,*,#51226,.T.);
#72572=ORIENTED_EDGE('',*,*,#50831,.F.);
#72573=ORIENTED_EDGE('',*,*,#51227,.F.);
#72574=ORIENTED_EDGE('',*,*,#51209,.F.);
#72575=ORIENTED_EDGE('',*,*,#51227,.T.);
#72576=ORIENTED_EDGE('',*,*,#49930,.F.);
#72577=ORIENTED_EDGE('',*,*,#51228,.F.);
#72578=ORIENTED_EDGE('',*,*,#51210,.F.);
#72579=ORIENTED_EDGE('',*,*,#51228,.T.);
#72580=ORIENTED_EDGE('',*,*,#49929,.F.);
#72581=ORIENTED_EDGE('',*,*,#51229,.F.);
#72582=ORIENTED_EDGE('',*,*,#51214,.F.);
#72583=ORIENTED_EDGE('',*,*,#51229,.T.);
#72584=ORIENTED_EDGE('',*,*,#49928,.F.);
#72585=ORIENTED_EDGE('',*,*,#51230,.F.);
#72586=ORIENTED_EDGE('',*,*,#51205,.F.);
#72587=ORIENTED_EDGE('',*,*,#51231,.T.);
#72588=ORIENTED_EDGE('',*,*,#51206,.F.);
#72589=ORIENTED_EDGE('',*,*,#51230,.T.);
#72590=ORIENTED_EDGE('',*,*,#50830,.F.);
#72591=ORIENTED_EDGE('',*,*,#51232,.T.);
#72592=ORIENTED_EDGE('',*,*,#51207,.F.);
#72593=ORIENTED_EDGE('',*,*,#51231,.F.);
#72594=ORIENTED_EDGE('',*,*,#50574,.F.);
#72595=ORIENTED_EDGE('',*,*,#51224,.T.);
#72596=ORIENTED_EDGE('',*,*,#51220,.T.);
#72597=ORIENTED_EDGE('',*,*,#51232,.F.);
#72598=ORIENTED_EDGE('',*,*,#50573,.T.);
#72599=ORIENTED_EDGE('',*,*,#51218,.T.);
#72600=ORIENTED_EDGE('',*,*,#51221,.T.);
#72601=ORIENTED_EDGE('',*,*,#51223,.T.);
#72602=ORIENTED_EDGE('',*,*,#51233,.T.);
#72603=ORIENTED_EDGE('',*,*,#51234,.T.);
#72604=ORIENTED_EDGE('',*,*,#51235,.T.);
#72605=ORIENTED_EDGE('',*,*,#51236,.T.);
#72606=ORIENTED_EDGE('',*,*,#51237,.T.);
#72607=ORIENTED_EDGE('',*,*,#51238,.T.);
#72608=ORIENTED_EDGE('',*,*,#51239,.T.);
#72609=ORIENTED_EDGE('',*,*,#51240,.F.);
#72610=ORIENTED_EDGE('',*,*,#51241,.T.);
#72611=ORIENTED_EDGE('',*,*,#51242,.T.);
#72612=ORIENTED_EDGE('',*,*,#51240,.T.);
#72613=ORIENTED_EDGE('',*,*,#51243,.T.);
#72614=ORIENTED_EDGE('',*,*,#51233,.F.);
#72615=ORIENTED_EDGE('',*,*,#51244,.T.);
#72616=ORIENTED_EDGE('',*,*,#51245,.F.);
#72617=ORIENTED_EDGE('',*,*,#51241,.F.);
#72618=ORIENTED_EDGE('',*,*,#51246,.F.);
#72619=ORIENTED_EDGE('',*,*,#51247,.F.);
#72620=ORIENTED_EDGE('',*,*,#51246,.T.);
#72621=ORIENTED_EDGE('',*,*,#51244,.F.);
#72622=ORIENTED_EDGE('',*,*,#51248,.F.);
#72623=ORIENTED_EDGE('',*,*,#51248,.T.);
#72624=ORIENTED_EDGE('',*,*,#51237,.F.);
#72625=ORIENTED_EDGE('',*,*,#51249,.F.);
#72626=ORIENTED_EDGE('',*,*,#51250,.F.);
#72627=ORIENTED_EDGE('',*,*,#51251,.T.);
#72628=ORIENTED_EDGE('',*,*,#51252,.F.);
#72629=ORIENTED_EDGE('',*,*,#51253,.F.);
#72630=ORIENTED_EDGE('',*,*,#50578,.F.);
#72631=ORIENTED_EDGE('',*,*,#51254,.T.);
#72632=ORIENTED_EDGE('',*,*,#51245,.T.);
#72633=ORIENTED_EDGE('',*,*,#51251,.F.);
#72634=ORIENTED_EDGE('',*,*,#50577,.T.);
#72635=ORIENTED_EDGE('',*,*,#51255,.F.);
#72636=ORIENTED_EDGE('',*,*,#51242,.F.);
#72637=ORIENTED_EDGE('',*,*,#51254,.F.);
#72638=ORIENTED_EDGE('',*,*,#50576,.F.);
#72639=ORIENTED_EDGE('',*,*,#51255,.T.);
#72640=ORIENTED_EDGE('',*,*,#50829,.F.);
#72641=ORIENTED_EDGE('',*,*,#51256,.F.);
#72642=ORIENTED_EDGE('',*,*,#51238,.F.);
#72643=ORIENTED_EDGE('',*,*,#51256,.T.);
#72644=ORIENTED_EDGE('',*,*,#49926,.F.);
#72645=ORIENTED_EDGE('',*,*,#51257,.F.);
#72646=ORIENTED_EDGE('',*,*,#51239,.F.);
#72647=ORIENTED_EDGE('',*,*,#51257,.T.);
#72648=ORIENTED_EDGE('',*,*,#49925,.F.);
#72649=ORIENTED_EDGE('',*,*,#51258,.F.);
#72650=ORIENTED_EDGE('',*,*,#51243,.F.);
#72651=ORIENTED_EDGE('',*,*,#51258,.T.);
#72652=ORIENTED_EDGE('',*,*,#49924,.F.);
#72653=ORIENTED_EDGE('',*,*,#51259,.F.);
#72654=ORIENTED_EDGE('',*,*,#51234,.F.);
#72655=ORIENTED_EDGE('',*,*,#51260,.T.);
#72656=ORIENTED_EDGE('',*,*,#51235,.F.);
#72657=ORIENTED_EDGE('',*,*,#51259,.T.);
#72658=ORIENTED_EDGE('',*,*,#50828,.F.);
#72659=ORIENTED_EDGE('',*,*,#51261,.T.);
#72660=ORIENTED_EDGE('',*,*,#51236,.F.);
#72661=ORIENTED_EDGE('',*,*,#51260,.F.);
#72662=ORIENTED_EDGE('',*,*,#50580,.F.);
#72663=ORIENTED_EDGE('',*,*,#51253,.T.);
#72664=ORIENTED_EDGE('',*,*,#51249,.T.);
#72665=ORIENTED_EDGE('',*,*,#51261,.F.);
#72666=ORIENTED_EDGE('',*,*,#50579,.T.);
#72667=ORIENTED_EDGE('',*,*,#51247,.T.);
#72668=ORIENTED_EDGE('',*,*,#51250,.T.);
#72669=ORIENTED_EDGE('',*,*,#51252,.T.);
#72670=ORIENTED_EDGE('',*,*,#51262,.T.);
#72671=ORIENTED_EDGE('',*,*,#51263,.T.);
#72672=ORIENTED_EDGE('',*,*,#51264,.T.);
#72673=ORIENTED_EDGE('',*,*,#51265,.T.);
#72674=ORIENTED_EDGE('',*,*,#51266,.T.);
#72675=ORIENTED_EDGE('',*,*,#51267,.T.);
#72676=ORIENTED_EDGE('',*,*,#51268,.T.);
#72677=ORIENTED_EDGE('',*,*,#51269,.F.);
#72678=ORIENTED_EDGE('',*,*,#51270,.T.);
#72679=ORIENTED_EDGE('',*,*,#51271,.T.);
#72680=ORIENTED_EDGE('',*,*,#51269,.T.);
#72681=ORIENTED_EDGE('',*,*,#51272,.T.);
#72682=ORIENTED_EDGE('',*,*,#51262,.F.);
#72683=ORIENTED_EDGE('',*,*,#51273,.T.);
#72684=ORIENTED_EDGE('',*,*,#51274,.F.);
#72685=ORIENTED_EDGE('',*,*,#51270,.F.);
#72686=ORIENTED_EDGE('',*,*,#51275,.F.);
#72687=ORIENTED_EDGE('',*,*,#51276,.F.);
#72688=ORIENTED_EDGE('',*,*,#51275,.T.);
#72689=ORIENTED_EDGE('',*,*,#51273,.F.);
#72690=ORIENTED_EDGE('',*,*,#51277,.F.);
#72691=ORIENTED_EDGE('',*,*,#51277,.T.);
#72692=ORIENTED_EDGE('',*,*,#51266,.F.);
#72693=ORIENTED_EDGE('',*,*,#51278,.F.);
#72694=ORIENTED_EDGE('',*,*,#51279,.F.);
#72695=ORIENTED_EDGE('',*,*,#51280,.T.);
#72696=ORIENTED_EDGE('',*,*,#51281,.F.);
#72697=ORIENTED_EDGE('',*,*,#51282,.F.);
#72698=ORIENTED_EDGE('',*,*,#50584,.F.);
#72699=ORIENTED_EDGE('',*,*,#51283,.T.);
#72700=ORIENTED_EDGE('',*,*,#51274,.T.);
#72701=ORIENTED_EDGE('',*,*,#51280,.F.);
#72702=ORIENTED_EDGE('',*,*,#50583,.T.);
#72703=ORIENTED_EDGE('',*,*,#51284,.F.);
#72704=ORIENTED_EDGE('',*,*,#51271,.F.);
#72705=ORIENTED_EDGE('',*,*,#51283,.F.);
#72706=ORIENTED_EDGE('',*,*,#50582,.F.);
#72707=ORIENTED_EDGE('',*,*,#51284,.T.);
#72708=ORIENTED_EDGE('',*,*,#50827,.F.);
#72709=ORIENTED_EDGE('',*,*,#51285,.F.);
#72710=ORIENTED_EDGE('',*,*,#51267,.F.);
#72711=ORIENTED_EDGE('',*,*,#51285,.T.);
#72712=ORIENTED_EDGE('',*,*,#49922,.F.);
#72713=ORIENTED_EDGE('',*,*,#51286,.F.);
#72714=ORIENTED_EDGE('',*,*,#51268,.F.);
#72715=ORIENTED_EDGE('',*,*,#51286,.T.);
#72716=ORIENTED_EDGE('',*,*,#49921,.F.);
#72717=ORIENTED_EDGE('',*,*,#51287,.F.);
#72718=ORIENTED_EDGE('',*,*,#51272,.F.);
#72719=ORIENTED_EDGE('',*,*,#51287,.T.);
#72720=ORIENTED_EDGE('',*,*,#49920,.F.);
#72721=ORIENTED_EDGE('',*,*,#51288,.F.);
#72722=ORIENTED_EDGE('',*,*,#51263,.F.);
#72723=ORIENTED_EDGE('',*,*,#51289,.T.);
#72724=ORIENTED_EDGE('',*,*,#51264,.F.);
#72725=ORIENTED_EDGE('',*,*,#51288,.T.);
#72726=ORIENTED_EDGE('',*,*,#50826,.F.);
#72727=ORIENTED_EDGE('',*,*,#51290,.T.);
#72728=ORIENTED_EDGE('',*,*,#51265,.F.);
#72729=ORIENTED_EDGE('',*,*,#51289,.F.);
#72730=ORIENTED_EDGE('',*,*,#50586,.F.);
#72731=ORIENTED_EDGE('',*,*,#51282,.T.);
#72732=ORIENTED_EDGE('',*,*,#51278,.T.);
#72733=ORIENTED_EDGE('',*,*,#51290,.F.);
#72734=ORIENTED_EDGE('',*,*,#50585,.T.);
#72735=ORIENTED_EDGE('',*,*,#51276,.T.);
#72736=ORIENTED_EDGE('',*,*,#51279,.T.);
#72737=ORIENTED_EDGE('',*,*,#51281,.T.);
#72738=ORIENTED_EDGE('',*,*,#51291,.T.);
#72739=ORIENTED_EDGE('',*,*,#51292,.T.);
#72740=ORIENTED_EDGE('',*,*,#51293,.T.);
#72741=ORIENTED_EDGE('',*,*,#51294,.T.);
#72742=ORIENTED_EDGE('',*,*,#51295,.T.);
#72743=ORIENTED_EDGE('',*,*,#51296,.T.);
#72744=ORIENTED_EDGE('',*,*,#51297,.T.);
#72745=ORIENTED_EDGE('',*,*,#51298,.F.);
#72746=ORIENTED_EDGE('',*,*,#51299,.T.);
#72747=ORIENTED_EDGE('',*,*,#51300,.T.);
#72748=ORIENTED_EDGE('',*,*,#51298,.T.);
#72749=ORIENTED_EDGE('',*,*,#51301,.T.);
#72750=ORIENTED_EDGE('',*,*,#51291,.F.);
#72751=ORIENTED_EDGE('',*,*,#51302,.T.);
#72752=ORIENTED_EDGE('',*,*,#51303,.F.);
#72753=ORIENTED_EDGE('',*,*,#51299,.F.);
#72754=ORIENTED_EDGE('',*,*,#51304,.F.);
#72755=ORIENTED_EDGE('',*,*,#51305,.F.);
#72756=ORIENTED_EDGE('',*,*,#51304,.T.);
#72757=ORIENTED_EDGE('',*,*,#51302,.F.);
#72758=ORIENTED_EDGE('',*,*,#51306,.F.);
#72759=ORIENTED_EDGE('',*,*,#51306,.T.);
#72760=ORIENTED_EDGE('',*,*,#51295,.F.);
#72761=ORIENTED_EDGE('',*,*,#51307,.F.);
#72762=ORIENTED_EDGE('',*,*,#51308,.F.);
#72763=ORIENTED_EDGE('',*,*,#51309,.T.);
#72764=ORIENTED_EDGE('',*,*,#51310,.F.);
#72765=ORIENTED_EDGE('',*,*,#51311,.F.);
#72766=ORIENTED_EDGE('',*,*,#50590,.F.);
#72767=ORIENTED_EDGE('',*,*,#51312,.T.);
#72768=ORIENTED_EDGE('',*,*,#51303,.T.);
#72769=ORIENTED_EDGE('',*,*,#51309,.F.);
#72770=ORIENTED_EDGE('',*,*,#50589,.T.);
#72771=ORIENTED_EDGE('',*,*,#51313,.F.);
#72772=ORIENTED_EDGE('',*,*,#51300,.F.);
#72773=ORIENTED_EDGE('',*,*,#51312,.F.);
#72774=ORIENTED_EDGE('',*,*,#50588,.F.);
#72775=ORIENTED_EDGE('',*,*,#51313,.T.);
#72776=ORIENTED_EDGE('',*,*,#50825,.F.);
#72777=ORIENTED_EDGE('',*,*,#51314,.F.);
#72778=ORIENTED_EDGE('',*,*,#51296,.F.);
#72779=ORIENTED_EDGE('',*,*,#51314,.T.);
#72780=ORIENTED_EDGE('',*,*,#49918,.F.);
#72781=ORIENTED_EDGE('',*,*,#51315,.F.);
#72782=ORIENTED_EDGE('',*,*,#51297,.F.);
#72783=ORIENTED_EDGE('',*,*,#51315,.T.);
#72784=ORIENTED_EDGE('',*,*,#49917,.F.);
#72785=ORIENTED_EDGE('',*,*,#51316,.F.);
#72786=ORIENTED_EDGE('',*,*,#51301,.F.);
#72787=ORIENTED_EDGE('',*,*,#51316,.T.);
#72788=ORIENTED_EDGE('',*,*,#49916,.F.);
#72789=ORIENTED_EDGE('',*,*,#51317,.F.);
#72790=ORIENTED_EDGE('',*,*,#51292,.F.);
#72791=ORIENTED_EDGE('',*,*,#51318,.T.);
#72792=ORIENTED_EDGE('',*,*,#51293,.F.);
#72793=ORIENTED_EDGE('',*,*,#51317,.T.);
#72794=ORIENTED_EDGE('',*,*,#50824,.F.);
#72795=ORIENTED_EDGE('',*,*,#51319,.T.);
#72796=ORIENTED_EDGE('',*,*,#51294,.F.);
#72797=ORIENTED_EDGE('',*,*,#51318,.F.);
#72798=ORIENTED_EDGE('',*,*,#50592,.F.);
#72799=ORIENTED_EDGE('',*,*,#51311,.T.);
#72800=ORIENTED_EDGE('',*,*,#51307,.T.);
#72801=ORIENTED_EDGE('',*,*,#51319,.F.);
#72802=ORIENTED_EDGE('',*,*,#50591,.T.);
#72803=ORIENTED_EDGE('',*,*,#51305,.T.);
#72804=ORIENTED_EDGE('',*,*,#51308,.T.);
#72805=ORIENTED_EDGE('',*,*,#51310,.T.);
#72806=ORIENTED_EDGE('',*,*,#51320,.T.);
#72807=ORIENTED_EDGE('',*,*,#51321,.T.);
#72808=ORIENTED_EDGE('',*,*,#51322,.T.);
#72809=ORIENTED_EDGE('',*,*,#51323,.T.);
#72810=ORIENTED_EDGE('',*,*,#51324,.T.);
#72811=ORIENTED_EDGE('',*,*,#51325,.T.);
#72812=ORIENTED_EDGE('',*,*,#51326,.T.);
#72813=ORIENTED_EDGE('',*,*,#51327,.F.);
#72814=ORIENTED_EDGE('',*,*,#51328,.T.);
#72815=ORIENTED_EDGE('',*,*,#51329,.T.);
#72816=ORIENTED_EDGE('',*,*,#51327,.T.);
#72817=ORIENTED_EDGE('',*,*,#51330,.T.);
#72818=ORIENTED_EDGE('',*,*,#51320,.F.);
#72819=ORIENTED_EDGE('',*,*,#51331,.T.);
#72820=ORIENTED_EDGE('',*,*,#51332,.F.);
#72821=ORIENTED_EDGE('',*,*,#51328,.F.);
#72822=ORIENTED_EDGE('',*,*,#51333,.F.);
#72823=ORIENTED_EDGE('',*,*,#51334,.F.);
#72824=ORIENTED_EDGE('',*,*,#51333,.T.);
#72825=ORIENTED_EDGE('',*,*,#51331,.F.);
#72826=ORIENTED_EDGE('',*,*,#51335,.F.);
#72827=ORIENTED_EDGE('',*,*,#51335,.T.);
#72828=ORIENTED_EDGE('',*,*,#51324,.F.);
#72829=ORIENTED_EDGE('',*,*,#51336,.F.);
#72830=ORIENTED_EDGE('',*,*,#51337,.F.);
#72831=ORIENTED_EDGE('',*,*,#51338,.T.);
#72832=ORIENTED_EDGE('',*,*,#51339,.F.);
#72833=ORIENTED_EDGE('',*,*,#51340,.F.);
#72834=ORIENTED_EDGE('',*,*,#50596,.F.);
#72835=ORIENTED_EDGE('',*,*,#51341,.T.);
#72836=ORIENTED_EDGE('',*,*,#51332,.T.);
#72837=ORIENTED_EDGE('',*,*,#51338,.F.);
#72838=ORIENTED_EDGE('',*,*,#50595,.T.);
#72839=ORIENTED_EDGE('',*,*,#51342,.F.);
#72840=ORIENTED_EDGE('',*,*,#51329,.F.);
#72841=ORIENTED_EDGE('',*,*,#51341,.F.);
#72842=ORIENTED_EDGE('',*,*,#50594,.F.);
#72843=ORIENTED_EDGE('',*,*,#51342,.T.);
#72844=ORIENTED_EDGE('',*,*,#50823,.F.);
#72845=ORIENTED_EDGE('',*,*,#51343,.F.);
#72846=ORIENTED_EDGE('',*,*,#51325,.F.);
#72847=ORIENTED_EDGE('',*,*,#51343,.T.);
#72848=ORIENTED_EDGE('',*,*,#49914,.F.);
#72849=ORIENTED_EDGE('',*,*,#51344,.F.);
#72850=ORIENTED_EDGE('',*,*,#51326,.F.);
#72851=ORIENTED_EDGE('',*,*,#51344,.T.);
#72852=ORIENTED_EDGE('',*,*,#49913,.F.);
#72853=ORIENTED_EDGE('',*,*,#51345,.F.);
#72854=ORIENTED_EDGE('',*,*,#51330,.F.);
#72855=ORIENTED_EDGE('',*,*,#51345,.T.);
#72856=ORIENTED_EDGE('',*,*,#49912,.F.);
#72857=ORIENTED_EDGE('',*,*,#51346,.F.);
#72858=ORIENTED_EDGE('',*,*,#51321,.F.);
#72859=ORIENTED_EDGE('',*,*,#51347,.T.);
#72860=ORIENTED_EDGE('',*,*,#51322,.F.);
#72861=ORIENTED_EDGE('',*,*,#51346,.T.);
#72862=ORIENTED_EDGE('',*,*,#50822,.F.);
#72863=ORIENTED_EDGE('',*,*,#51348,.T.);
#72864=ORIENTED_EDGE('',*,*,#51323,.F.);
#72865=ORIENTED_EDGE('',*,*,#51347,.F.);
#72866=ORIENTED_EDGE('',*,*,#50598,.F.);
#72867=ORIENTED_EDGE('',*,*,#51340,.T.);
#72868=ORIENTED_EDGE('',*,*,#51336,.T.);
#72869=ORIENTED_EDGE('',*,*,#51348,.F.);
#72870=ORIENTED_EDGE('',*,*,#50597,.T.);
#72871=ORIENTED_EDGE('',*,*,#51334,.T.);
#72872=ORIENTED_EDGE('',*,*,#51337,.T.);
#72873=ORIENTED_EDGE('',*,*,#51339,.T.);
#72874=ORIENTED_EDGE('',*,*,#51349,.T.);
#72875=ORIENTED_EDGE('',*,*,#51350,.T.);
#72876=ORIENTED_EDGE('',*,*,#51351,.T.);
#72877=ORIENTED_EDGE('',*,*,#51352,.T.);
#72878=ORIENTED_EDGE('',*,*,#51353,.T.);
#72879=ORIENTED_EDGE('',*,*,#51354,.T.);
#72880=ORIENTED_EDGE('',*,*,#51355,.T.);
#72881=ORIENTED_EDGE('',*,*,#51356,.F.);
#72882=ORIENTED_EDGE('',*,*,#51357,.T.);
#72883=ORIENTED_EDGE('',*,*,#51358,.T.);
#72884=ORIENTED_EDGE('',*,*,#51356,.T.);
#72885=ORIENTED_EDGE('',*,*,#51359,.T.);
#72886=ORIENTED_EDGE('',*,*,#51349,.F.);
#72887=ORIENTED_EDGE('',*,*,#51360,.T.);
#72888=ORIENTED_EDGE('',*,*,#51361,.F.);
#72889=ORIENTED_EDGE('',*,*,#51357,.F.);
#72890=ORIENTED_EDGE('',*,*,#51362,.F.);
#72891=ORIENTED_EDGE('',*,*,#51363,.F.);
#72892=ORIENTED_EDGE('',*,*,#51362,.T.);
#72893=ORIENTED_EDGE('',*,*,#51360,.F.);
#72894=ORIENTED_EDGE('',*,*,#51364,.F.);
#72895=ORIENTED_EDGE('',*,*,#51364,.T.);
#72896=ORIENTED_EDGE('',*,*,#51353,.F.);
#72897=ORIENTED_EDGE('',*,*,#51365,.F.);
#72898=ORIENTED_EDGE('',*,*,#51366,.F.);
#72899=ORIENTED_EDGE('',*,*,#51367,.T.);
#72900=ORIENTED_EDGE('',*,*,#51368,.F.);
#72901=ORIENTED_EDGE('',*,*,#51369,.F.);
#72902=ORIENTED_EDGE('',*,*,#50602,.F.);
#72903=ORIENTED_EDGE('',*,*,#51370,.T.);
#72904=ORIENTED_EDGE('',*,*,#51361,.T.);
#72905=ORIENTED_EDGE('',*,*,#51367,.F.);
#72906=ORIENTED_EDGE('',*,*,#50601,.T.);
#72907=ORIENTED_EDGE('',*,*,#51371,.F.);
#72908=ORIENTED_EDGE('',*,*,#51358,.F.);
#72909=ORIENTED_EDGE('',*,*,#51370,.F.);
#72910=ORIENTED_EDGE('',*,*,#50600,.F.);
#72911=ORIENTED_EDGE('',*,*,#51371,.T.);
#72912=ORIENTED_EDGE('',*,*,#50821,.F.);
#72913=ORIENTED_EDGE('',*,*,#51372,.F.);
#72914=ORIENTED_EDGE('',*,*,#51354,.F.);
#72915=ORIENTED_EDGE('',*,*,#51372,.T.);
#72916=ORIENTED_EDGE('',*,*,#49910,.F.);
#72917=ORIENTED_EDGE('',*,*,#51373,.F.);
#72918=ORIENTED_EDGE('',*,*,#51355,.F.);
#72919=ORIENTED_EDGE('',*,*,#51373,.T.);
#72920=ORIENTED_EDGE('',*,*,#49909,.F.);
#72921=ORIENTED_EDGE('',*,*,#51374,.F.);
#72922=ORIENTED_EDGE('',*,*,#51359,.F.);
#72923=ORIENTED_EDGE('',*,*,#51374,.T.);
#72924=ORIENTED_EDGE('',*,*,#49908,.F.);
#72925=ORIENTED_EDGE('',*,*,#51375,.F.);
#72926=ORIENTED_EDGE('',*,*,#51350,.F.);
#72927=ORIENTED_EDGE('',*,*,#51376,.T.);
#72928=ORIENTED_EDGE('',*,*,#51351,.F.);
#72929=ORIENTED_EDGE('',*,*,#51375,.T.);
#72930=ORIENTED_EDGE('',*,*,#50820,.F.);
#72931=ORIENTED_EDGE('',*,*,#51377,.T.);
#72932=ORIENTED_EDGE('',*,*,#51352,.F.);
#72933=ORIENTED_EDGE('',*,*,#51376,.F.);
#72934=ORIENTED_EDGE('',*,*,#50604,.F.);
#72935=ORIENTED_EDGE('',*,*,#51369,.T.);
#72936=ORIENTED_EDGE('',*,*,#51365,.T.);
#72937=ORIENTED_EDGE('',*,*,#51377,.F.);
#72938=ORIENTED_EDGE('',*,*,#50603,.T.);
#72939=ORIENTED_EDGE('',*,*,#51363,.T.);
#72940=ORIENTED_EDGE('',*,*,#51366,.T.);
#72941=ORIENTED_EDGE('',*,*,#51368,.T.);
#72942=ORIENTED_EDGE('',*,*,#51378,.T.);
#72943=ORIENTED_EDGE('',*,*,#51379,.T.);
#72944=ORIENTED_EDGE('',*,*,#51380,.T.);
#72945=ORIENTED_EDGE('',*,*,#51381,.T.);
#72946=ORIENTED_EDGE('',*,*,#51382,.T.);
#72947=ORIENTED_EDGE('',*,*,#51383,.T.);
#72948=ORIENTED_EDGE('',*,*,#51384,.T.);
#72949=ORIENTED_EDGE('',*,*,#51385,.F.);
#72950=ORIENTED_EDGE('',*,*,#51386,.T.);
#72951=ORIENTED_EDGE('',*,*,#51387,.T.);
#72952=ORIENTED_EDGE('',*,*,#51385,.T.);
#72953=ORIENTED_EDGE('',*,*,#51388,.T.);
#72954=ORIENTED_EDGE('',*,*,#51378,.F.);
#72955=ORIENTED_EDGE('',*,*,#51389,.T.);
#72956=ORIENTED_EDGE('',*,*,#51390,.F.);
#72957=ORIENTED_EDGE('',*,*,#51386,.F.);
#72958=ORIENTED_EDGE('',*,*,#51391,.F.);
#72959=ORIENTED_EDGE('',*,*,#51392,.F.);
#72960=ORIENTED_EDGE('',*,*,#51391,.T.);
#72961=ORIENTED_EDGE('',*,*,#51389,.F.);
#72962=ORIENTED_EDGE('',*,*,#51393,.F.);
#72963=ORIENTED_EDGE('',*,*,#51393,.T.);
#72964=ORIENTED_EDGE('',*,*,#51382,.F.);
#72965=ORIENTED_EDGE('',*,*,#51394,.F.);
#72966=ORIENTED_EDGE('',*,*,#51395,.F.);
#72967=ORIENTED_EDGE('',*,*,#51396,.T.);
#72968=ORIENTED_EDGE('',*,*,#51397,.F.);
#72969=ORIENTED_EDGE('',*,*,#51398,.F.);
#72970=ORIENTED_EDGE('',*,*,#50608,.F.);
#72971=ORIENTED_EDGE('',*,*,#51399,.T.);
#72972=ORIENTED_EDGE('',*,*,#51390,.T.);
#72973=ORIENTED_EDGE('',*,*,#51396,.F.);
#72974=ORIENTED_EDGE('',*,*,#50607,.T.);
#72975=ORIENTED_EDGE('',*,*,#51400,.F.);
#72976=ORIENTED_EDGE('',*,*,#51387,.F.);
#72977=ORIENTED_EDGE('',*,*,#51399,.F.);
#72978=ORIENTED_EDGE('',*,*,#50606,.F.);
#72979=ORIENTED_EDGE('',*,*,#51400,.T.);
#72980=ORIENTED_EDGE('',*,*,#50819,.F.);
#72981=ORIENTED_EDGE('',*,*,#51401,.F.);
#72982=ORIENTED_EDGE('',*,*,#51383,.F.);
#72983=ORIENTED_EDGE('',*,*,#51401,.T.);
#72984=ORIENTED_EDGE('',*,*,#49906,.F.);
#72985=ORIENTED_EDGE('',*,*,#51402,.F.);
#72986=ORIENTED_EDGE('',*,*,#51384,.F.);
#72987=ORIENTED_EDGE('',*,*,#51402,.T.);
#72988=ORIENTED_EDGE('',*,*,#49905,.F.);
#72989=ORIENTED_EDGE('',*,*,#51403,.F.);
#72990=ORIENTED_EDGE('',*,*,#51388,.F.);
#72991=ORIENTED_EDGE('',*,*,#51403,.T.);
#72992=ORIENTED_EDGE('',*,*,#49904,.F.);
#72993=ORIENTED_EDGE('',*,*,#51404,.F.);
#72994=ORIENTED_EDGE('',*,*,#51379,.F.);
#72995=ORIENTED_EDGE('',*,*,#51405,.T.);
#72996=ORIENTED_EDGE('',*,*,#51380,.F.);
#72997=ORIENTED_EDGE('',*,*,#51404,.T.);
#72998=ORIENTED_EDGE('',*,*,#50818,.F.);
#72999=ORIENTED_EDGE('',*,*,#51406,.T.);
#73000=ORIENTED_EDGE('',*,*,#51381,.F.);
#73001=ORIENTED_EDGE('',*,*,#51405,.F.);
#73002=ORIENTED_EDGE('',*,*,#50610,.F.);
#73003=ORIENTED_EDGE('',*,*,#51398,.T.);
#73004=ORIENTED_EDGE('',*,*,#51394,.T.);
#73005=ORIENTED_EDGE('',*,*,#51406,.F.);
#73006=ORIENTED_EDGE('',*,*,#50609,.T.);
#73007=ORIENTED_EDGE('',*,*,#51392,.T.);
#73008=ORIENTED_EDGE('',*,*,#51395,.T.);
#73009=ORIENTED_EDGE('',*,*,#51397,.T.);
#73010=ORIENTED_EDGE('',*,*,#51407,.T.);
#73011=ORIENTED_EDGE('',*,*,#51408,.T.);
#73012=ORIENTED_EDGE('',*,*,#51409,.T.);
#73013=ORIENTED_EDGE('',*,*,#51410,.T.);
#73014=ORIENTED_EDGE('',*,*,#51411,.T.);
#73015=ORIENTED_EDGE('',*,*,#51412,.T.);
#73016=ORIENTED_EDGE('',*,*,#51413,.T.);
#73017=ORIENTED_EDGE('',*,*,#51414,.F.);
#73018=ORIENTED_EDGE('',*,*,#51415,.T.);
#73019=ORIENTED_EDGE('',*,*,#51416,.T.);
#73020=ORIENTED_EDGE('',*,*,#51414,.T.);
#73021=ORIENTED_EDGE('',*,*,#51417,.T.);
#73022=ORIENTED_EDGE('',*,*,#51407,.F.);
#73023=ORIENTED_EDGE('',*,*,#51418,.T.);
#73024=ORIENTED_EDGE('',*,*,#51419,.F.);
#73025=ORIENTED_EDGE('',*,*,#51415,.F.);
#73026=ORIENTED_EDGE('',*,*,#51420,.F.);
#73027=ORIENTED_EDGE('',*,*,#51421,.F.);
#73028=ORIENTED_EDGE('',*,*,#51420,.T.);
#73029=ORIENTED_EDGE('',*,*,#51418,.F.);
#73030=ORIENTED_EDGE('',*,*,#51422,.F.);
#73031=ORIENTED_EDGE('',*,*,#51422,.T.);
#73032=ORIENTED_EDGE('',*,*,#51411,.F.);
#73033=ORIENTED_EDGE('',*,*,#51423,.F.);
#73034=ORIENTED_EDGE('',*,*,#51424,.F.);
#73035=ORIENTED_EDGE('',*,*,#51425,.T.);
#73036=ORIENTED_EDGE('',*,*,#51426,.F.);
#73037=ORIENTED_EDGE('',*,*,#51427,.F.);
#73038=ORIENTED_EDGE('',*,*,#50614,.F.);
#73039=ORIENTED_EDGE('',*,*,#51428,.T.);
#73040=ORIENTED_EDGE('',*,*,#51419,.T.);
#73041=ORIENTED_EDGE('',*,*,#51425,.F.);
#73042=ORIENTED_EDGE('',*,*,#50613,.T.);
#73043=ORIENTED_EDGE('',*,*,#51429,.F.);
#73044=ORIENTED_EDGE('',*,*,#51416,.F.);
#73045=ORIENTED_EDGE('',*,*,#51428,.F.);
#73046=ORIENTED_EDGE('',*,*,#50612,.F.);
#73047=ORIENTED_EDGE('',*,*,#51429,.T.);
#73048=ORIENTED_EDGE('',*,*,#50817,.F.);
#73049=ORIENTED_EDGE('',*,*,#51430,.F.);
#73050=ORIENTED_EDGE('',*,*,#51412,.F.);
#73051=ORIENTED_EDGE('',*,*,#51430,.T.);
#73052=ORIENTED_EDGE('',*,*,#49902,.F.);
#73053=ORIENTED_EDGE('',*,*,#51431,.F.);
#73054=ORIENTED_EDGE('',*,*,#51413,.F.);
#73055=ORIENTED_EDGE('',*,*,#51431,.T.);
#73056=ORIENTED_EDGE('',*,*,#49901,.F.);
#73057=ORIENTED_EDGE('',*,*,#51432,.F.);
#73058=ORIENTED_EDGE('',*,*,#51417,.F.);
#73059=ORIENTED_EDGE('',*,*,#51432,.T.);
#73060=ORIENTED_EDGE('',*,*,#49900,.F.);
#73061=ORIENTED_EDGE('',*,*,#51433,.F.);
#73062=ORIENTED_EDGE('',*,*,#51408,.F.);
#73063=ORIENTED_EDGE('',*,*,#51434,.T.);
#73064=ORIENTED_EDGE('',*,*,#51409,.F.);
#73065=ORIENTED_EDGE('',*,*,#51433,.T.);
#73066=ORIENTED_EDGE('',*,*,#50816,.F.);
#73067=ORIENTED_EDGE('',*,*,#51435,.T.);
#73068=ORIENTED_EDGE('',*,*,#51410,.F.);
#73069=ORIENTED_EDGE('',*,*,#51434,.F.);
#73070=ORIENTED_EDGE('',*,*,#50616,.F.);
#73071=ORIENTED_EDGE('',*,*,#51427,.T.);
#73072=ORIENTED_EDGE('',*,*,#51423,.T.);
#73073=ORIENTED_EDGE('',*,*,#51435,.F.);
#73074=ORIENTED_EDGE('',*,*,#50615,.T.);
#73075=ORIENTED_EDGE('',*,*,#51421,.T.);
#73076=ORIENTED_EDGE('',*,*,#51424,.T.);
#73077=ORIENTED_EDGE('',*,*,#51426,.T.);
#73078=ORIENTED_EDGE('',*,*,#51436,.T.);
#73079=ORIENTED_EDGE('',*,*,#51437,.T.);
#73080=ORIENTED_EDGE('',*,*,#51438,.T.);
#73081=ORIENTED_EDGE('',*,*,#51439,.T.);
#73082=ORIENTED_EDGE('',*,*,#51440,.T.);
#73083=ORIENTED_EDGE('',*,*,#51441,.T.);
#73084=ORIENTED_EDGE('',*,*,#51442,.T.);
#73085=ORIENTED_EDGE('',*,*,#51443,.F.);
#73086=ORIENTED_EDGE('',*,*,#51444,.T.);
#73087=ORIENTED_EDGE('',*,*,#51445,.T.);
#73088=ORIENTED_EDGE('',*,*,#51443,.T.);
#73089=ORIENTED_EDGE('',*,*,#51446,.T.);
#73090=ORIENTED_EDGE('',*,*,#51436,.F.);
#73091=ORIENTED_EDGE('',*,*,#51447,.T.);
#73092=ORIENTED_EDGE('',*,*,#51448,.F.);
#73093=ORIENTED_EDGE('',*,*,#51444,.F.);
#73094=ORIENTED_EDGE('',*,*,#51449,.F.);
#73095=ORIENTED_EDGE('',*,*,#51450,.F.);
#73096=ORIENTED_EDGE('',*,*,#51449,.T.);
#73097=ORIENTED_EDGE('',*,*,#51447,.F.);
#73098=ORIENTED_EDGE('',*,*,#51451,.F.);
#73099=ORIENTED_EDGE('',*,*,#51451,.T.);
#73100=ORIENTED_EDGE('',*,*,#51440,.F.);
#73101=ORIENTED_EDGE('',*,*,#51452,.F.);
#73102=ORIENTED_EDGE('',*,*,#51453,.F.);
#73103=ORIENTED_EDGE('',*,*,#51454,.T.);
#73104=ORIENTED_EDGE('',*,*,#51455,.F.);
#73105=ORIENTED_EDGE('',*,*,#51456,.F.);
#73106=ORIENTED_EDGE('',*,*,#50620,.F.);
#73107=ORIENTED_EDGE('',*,*,#51457,.T.);
#73108=ORIENTED_EDGE('',*,*,#51448,.T.);
#73109=ORIENTED_EDGE('',*,*,#51454,.F.);
#73110=ORIENTED_EDGE('',*,*,#50619,.T.);
#73111=ORIENTED_EDGE('',*,*,#51458,.F.);
#73112=ORIENTED_EDGE('',*,*,#51445,.F.);
#73113=ORIENTED_EDGE('',*,*,#51457,.F.);
#73114=ORIENTED_EDGE('',*,*,#50618,.F.);
#73115=ORIENTED_EDGE('',*,*,#51458,.T.);
#73116=ORIENTED_EDGE('',*,*,#50815,.F.);
#73117=ORIENTED_EDGE('',*,*,#51459,.F.);
#73118=ORIENTED_EDGE('',*,*,#51441,.F.);
#73119=ORIENTED_EDGE('',*,*,#51459,.T.);
#73120=ORIENTED_EDGE('',*,*,#49898,.F.);
#73121=ORIENTED_EDGE('',*,*,#51460,.F.);
#73122=ORIENTED_EDGE('',*,*,#51442,.F.);
#73123=ORIENTED_EDGE('',*,*,#51460,.T.);
#73124=ORIENTED_EDGE('',*,*,#49897,.F.);
#73125=ORIENTED_EDGE('',*,*,#51461,.F.);
#73126=ORIENTED_EDGE('',*,*,#51446,.F.);
#73127=ORIENTED_EDGE('',*,*,#51461,.T.);
#73128=ORIENTED_EDGE('',*,*,#49896,.F.);
#73129=ORIENTED_EDGE('',*,*,#51462,.F.);
#73130=ORIENTED_EDGE('',*,*,#51437,.F.);
#73131=ORIENTED_EDGE('',*,*,#51463,.T.);
#73132=ORIENTED_EDGE('',*,*,#51438,.F.);
#73133=ORIENTED_EDGE('',*,*,#51462,.T.);
#73134=ORIENTED_EDGE('',*,*,#50814,.F.);
#73135=ORIENTED_EDGE('',*,*,#51464,.T.);
#73136=ORIENTED_EDGE('',*,*,#51439,.F.);
#73137=ORIENTED_EDGE('',*,*,#51463,.F.);
#73138=ORIENTED_EDGE('',*,*,#50622,.F.);
#73139=ORIENTED_EDGE('',*,*,#51456,.T.);
#73140=ORIENTED_EDGE('',*,*,#51452,.T.);
#73141=ORIENTED_EDGE('',*,*,#51464,.F.);
#73142=ORIENTED_EDGE('',*,*,#50621,.T.);
#73143=ORIENTED_EDGE('',*,*,#51450,.T.);
#73144=ORIENTED_EDGE('',*,*,#51453,.T.);
#73145=ORIENTED_EDGE('',*,*,#51455,.T.);
#73146=ORIENTED_EDGE('',*,*,#51465,.T.);
#73147=ORIENTED_EDGE('',*,*,#51466,.T.);
#73148=ORIENTED_EDGE('',*,*,#51467,.T.);
#73149=ORIENTED_EDGE('',*,*,#51468,.T.);
#73150=ORIENTED_EDGE('',*,*,#51469,.T.);
#73151=ORIENTED_EDGE('',*,*,#51470,.T.);
#73152=ORIENTED_EDGE('',*,*,#51471,.T.);
#73153=ORIENTED_EDGE('',*,*,#51472,.F.);
#73154=ORIENTED_EDGE('',*,*,#51473,.T.);
#73155=ORIENTED_EDGE('',*,*,#51474,.T.);
#73156=ORIENTED_EDGE('',*,*,#51472,.T.);
#73157=ORIENTED_EDGE('',*,*,#51475,.T.);
#73158=ORIENTED_EDGE('',*,*,#51465,.F.);
#73159=ORIENTED_EDGE('',*,*,#51476,.T.);
#73160=ORIENTED_EDGE('',*,*,#51477,.F.);
#73161=ORIENTED_EDGE('',*,*,#51473,.F.);
#73162=ORIENTED_EDGE('',*,*,#51478,.F.);
#73163=ORIENTED_EDGE('',*,*,#51479,.F.);
#73164=ORIENTED_EDGE('',*,*,#51478,.T.);
#73165=ORIENTED_EDGE('',*,*,#51476,.F.);
#73166=ORIENTED_EDGE('',*,*,#51480,.F.);
#73167=ORIENTED_EDGE('',*,*,#51480,.T.);
#73168=ORIENTED_EDGE('',*,*,#51469,.F.);
#73169=ORIENTED_EDGE('',*,*,#51481,.F.);
#73170=ORIENTED_EDGE('',*,*,#51482,.F.);
#73171=ORIENTED_EDGE('',*,*,#51483,.T.);
#73172=ORIENTED_EDGE('',*,*,#51484,.F.);
#73173=ORIENTED_EDGE('',*,*,#51485,.F.);
#73174=ORIENTED_EDGE('',*,*,#50626,.F.);
#73175=ORIENTED_EDGE('',*,*,#51486,.T.);
#73176=ORIENTED_EDGE('',*,*,#51477,.T.);
#73177=ORIENTED_EDGE('',*,*,#51483,.F.);
#73178=ORIENTED_EDGE('',*,*,#50625,.T.);
#73179=ORIENTED_EDGE('',*,*,#51487,.F.);
#73180=ORIENTED_EDGE('',*,*,#51474,.F.);
#73181=ORIENTED_EDGE('',*,*,#51486,.F.);
#73182=ORIENTED_EDGE('',*,*,#50624,.F.);
#73183=ORIENTED_EDGE('',*,*,#51487,.T.);
#73184=ORIENTED_EDGE('',*,*,#50813,.F.);
#73185=ORIENTED_EDGE('',*,*,#51488,.F.);
#73186=ORIENTED_EDGE('',*,*,#51470,.F.);
#73187=ORIENTED_EDGE('',*,*,#51488,.T.);
#73188=ORIENTED_EDGE('',*,*,#49894,.F.);
#73189=ORIENTED_EDGE('',*,*,#51489,.F.);
#73190=ORIENTED_EDGE('',*,*,#51471,.F.);
#73191=ORIENTED_EDGE('',*,*,#51489,.T.);
#73192=ORIENTED_EDGE('',*,*,#49893,.F.);
#73193=ORIENTED_EDGE('',*,*,#51490,.F.);
#73194=ORIENTED_EDGE('',*,*,#51475,.F.);
#73195=ORIENTED_EDGE('',*,*,#51490,.T.);
#73196=ORIENTED_EDGE('',*,*,#49892,.F.);
#73197=ORIENTED_EDGE('',*,*,#51491,.F.);
#73198=ORIENTED_EDGE('',*,*,#51466,.F.);
#73199=ORIENTED_EDGE('',*,*,#51492,.T.);
#73200=ORIENTED_EDGE('',*,*,#51467,.F.);
#73201=ORIENTED_EDGE('',*,*,#51491,.T.);
#73202=ORIENTED_EDGE('',*,*,#50812,.F.);
#73203=ORIENTED_EDGE('',*,*,#51493,.T.);
#73204=ORIENTED_EDGE('',*,*,#51468,.F.);
#73205=ORIENTED_EDGE('',*,*,#51492,.F.);
#73206=ORIENTED_EDGE('',*,*,#50628,.F.);
#73207=ORIENTED_EDGE('',*,*,#51485,.T.);
#73208=ORIENTED_EDGE('',*,*,#51481,.T.);
#73209=ORIENTED_EDGE('',*,*,#51493,.F.);
#73210=ORIENTED_EDGE('',*,*,#50627,.T.);
#73211=ORIENTED_EDGE('',*,*,#51479,.T.);
#73212=ORIENTED_EDGE('',*,*,#51482,.T.);
#73213=ORIENTED_EDGE('',*,*,#51484,.T.);
#73214=ORIENTED_EDGE('',*,*,#51494,.T.);
#73215=ORIENTED_EDGE('',*,*,#51495,.T.);
#73216=ORIENTED_EDGE('',*,*,#51496,.T.);
#73217=ORIENTED_EDGE('',*,*,#51497,.T.);
#73218=ORIENTED_EDGE('',*,*,#51498,.T.);
#73219=ORIENTED_EDGE('',*,*,#51499,.T.);
#73220=ORIENTED_EDGE('',*,*,#51500,.T.);
#73221=ORIENTED_EDGE('',*,*,#51501,.F.);
#73222=ORIENTED_EDGE('',*,*,#51502,.T.);
#73223=ORIENTED_EDGE('',*,*,#51503,.T.);
#73224=ORIENTED_EDGE('',*,*,#51501,.T.);
#73225=ORIENTED_EDGE('',*,*,#51504,.T.);
#73226=ORIENTED_EDGE('',*,*,#51494,.F.);
#73227=ORIENTED_EDGE('',*,*,#51505,.T.);
#73228=ORIENTED_EDGE('',*,*,#51506,.F.);
#73229=ORIENTED_EDGE('',*,*,#51502,.F.);
#73230=ORIENTED_EDGE('',*,*,#51507,.F.);
#73231=ORIENTED_EDGE('',*,*,#51508,.F.);
#73232=ORIENTED_EDGE('',*,*,#51507,.T.);
#73233=ORIENTED_EDGE('',*,*,#51505,.F.);
#73234=ORIENTED_EDGE('',*,*,#51509,.F.);
#73235=ORIENTED_EDGE('',*,*,#51509,.T.);
#73236=ORIENTED_EDGE('',*,*,#51498,.F.);
#73237=ORIENTED_EDGE('',*,*,#51510,.F.);
#73238=ORIENTED_EDGE('',*,*,#51511,.F.);
#73239=ORIENTED_EDGE('',*,*,#51512,.T.);
#73240=ORIENTED_EDGE('',*,*,#51513,.F.);
#73241=ORIENTED_EDGE('',*,*,#51514,.F.);
#73242=ORIENTED_EDGE('',*,*,#50632,.F.);
#73243=ORIENTED_EDGE('',*,*,#51515,.T.);
#73244=ORIENTED_EDGE('',*,*,#51506,.T.);
#73245=ORIENTED_EDGE('',*,*,#51512,.F.);
#73246=ORIENTED_EDGE('',*,*,#50631,.T.);
#73247=ORIENTED_EDGE('',*,*,#51516,.F.);
#73248=ORIENTED_EDGE('',*,*,#51503,.F.);
#73249=ORIENTED_EDGE('',*,*,#51515,.F.);
#73250=ORIENTED_EDGE('',*,*,#50630,.F.);
#73251=ORIENTED_EDGE('',*,*,#51516,.T.);
#73252=ORIENTED_EDGE('',*,*,#50811,.F.);
#73253=ORIENTED_EDGE('',*,*,#51517,.F.);
#73254=ORIENTED_EDGE('',*,*,#51499,.F.);
#73255=ORIENTED_EDGE('',*,*,#51517,.T.);
#73256=ORIENTED_EDGE('',*,*,#49890,.F.);
#73257=ORIENTED_EDGE('',*,*,#51518,.F.);
#73258=ORIENTED_EDGE('',*,*,#51500,.F.);
#73259=ORIENTED_EDGE('',*,*,#51518,.T.);
#73260=ORIENTED_EDGE('',*,*,#49889,.F.);
#73261=ORIENTED_EDGE('',*,*,#51519,.F.);
#73262=ORIENTED_EDGE('',*,*,#51504,.F.);
#73263=ORIENTED_EDGE('',*,*,#51519,.T.);
#73264=ORIENTED_EDGE('',*,*,#49888,.F.);
#73265=ORIENTED_EDGE('',*,*,#51520,.F.);
#73266=ORIENTED_EDGE('',*,*,#51495,.F.);
#73267=ORIENTED_EDGE('',*,*,#51521,.T.);
#73268=ORIENTED_EDGE('',*,*,#51496,.F.);
#73269=ORIENTED_EDGE('',*,*,#51520,.T.);
#73270=ORIENTED_EDGE('',*,*,#50810,.F.);
#73271=ORIENTED_EDGE('',*,*,#51522,.T.);
#73272=ORIENTED_EDGE('',*,*,#51497,.F.);
#73273=ORIENTED_EDGE('',*,*,#51521,.F.);
#73274=ORIENTED_EDGE('',*,*,#50634,.F.);
#73275=ORIENTED_EDGE('',*,*,#51514,.T.);
#73276=ORIENTED_EDGE('',*,*,#51510,.T.);
#73277=ORIENTED_EDGE('',*,*,#51522,.F.);
#73278=ORIENTED_EDGE('',*,*,#50633,.T.);
#73279=ORIENTED_EDGE('',*,*,#51508,.T.);
#73280=ORIENTED_EDGE('',*,*,#51511,.T.);
#73281=ORIENTED_EDGE('',*,*,#51513,.T.);
#73282=ORIENTED_EDGE('',*,*,#51523,.T.);
#73283=ORIENTED_EDGE('',*,*,#51524,.T.);
#73284=ORIENTED_EDGE('',*,*,#51525,.T.);
#73285=ORIENTED_EDGE('',*,*,#51526,.T.);
#73286=ORIENTED_EDGE('',*,*,#51527,.T.);
#73287=ORIENTED_EDGE('',*,*,#51528,.T.);
#73288=ORIENTED_EDGE('',*,*,#51529,.T.);
#73289=ORIENTED_EDGE('',*,*,#51530,.F.);
#73290=ORIENTED_EDGE('',*,*,#51531,.T.);
#73291=ORIENTED_EDGE('',*,*,#51532,.T.);
#73292=ORIENTED_EDGE('',*,*,#51530,.T.);
#73293=ORIENTED_EDGE('',*,*,#51533,.T.);
#73294=ORIENTED_EDGE('',*,*,#51523,.F.);
#73295=ORIENTED_EDGE('',*,*,#51534,.T.);
#73296=ORIENTED_EDGE('',*,*,#51535,.F.);
#73297=ORIENTED_EDGE('',*,*,#51531,.F.);
#73298=ORIENTED_EDGE('',*,*,#51536,.F.);
#73299=ORIENTED_EDGE('',*,*,#51537,.F.);
#73300=ORIENTED_EDGE('',*,*,#51536,.T.);
#73301=ORIENTED_EDGE('',*,*,#51534,.F.);
#73302=ORIENTED_EDGE('',*,*,#51538,.F.);
#73303=ORIENTED_EDGE('',*,*,#51538,.T.);
#73304=ORIENTED_EDGE('',*,*,#51527,.F.);
#73305=ORIENTED_EDGE('',*,*,#51539,.F.);
#73306=ORIENTED_EDGE('',*,*,#51540,.F.);
#73307=ORIENTED_EDGE('',*,*,#51541,.T.);
#73308=ORIENTED_EDGE('',*,*,#51542,.F.);
#73309=ORIENTED_EDGE('',*,*,#51543,.F.);
#73310=ORIENTED_EDGE('',*,*,#50638,.F.);
#73311=ORIENTED_EDGE('',*,*,#51544,.T.);
#73312=ORIENTED_EDGE('',*,*,#51535,.T.);
#73313=ORIENTED_EDGE('',*,*,#51541,.F.);
#73314=ORIENTED_EDGE('',*,*,#50637,.T.);
#73315=ORIENTED_EDGE('',*,*,#51545,.F.);
#73316=ORIENTED_EDGE('',*,*,#51532,.F.);
#73317=ORIENTED_EDGE('',*,*,#51544,.F.);
#73318=ORIENTED_EDGE('',*,*,#50636,.F.);
#73319=ORIENTED_EDGE('',*,*,#51545,.T.);
#73320=ORIENTED_EDGE('',*,*,#50809,.F.);
#73321=ORIENTED_EDGE('',*,*,#51546,.F.);
#73322=ORIENTED_EDGE('',*,*,#51528,.F.);
#73323=ORIENTED_EDGE('',*,*,#51546,.T.);
#73324=ORIENTED_EDGE('',*,*,#49886,.F.);
#73325=ORIENTED_EDGE('',*,*,#51547,.F.);
#73326=ORIENTED_EDGE('',*,*,#51529,.F.);
#73327=ORIENTED_EDGE('',*,*,#51547,.T.);
#73328=ORIENTED_EDGE('',*,*,#49885,.F.);
#73329=ORIENTED_EDGE('',*,*,#51548,.F.);
#73330=ORIENTED_EDGE('',*,*,#51533,.F.);
#73331=ORIENTED_EDGE('',*,*,#51548,.T.);
#73332=ORIENTED_EDGE('',*,*,#49884,.F.);
#73333=ORIENTED_EDGE('',*,*,#51549,.F.);
#73334=ORIENTED_EDGE('',*,*,#51524,.F.);
#73335=ORIENTED_EDGE('',*,*,#51550,.T.);
#73336=ORIENTED_EDGE('',*,*,#51525,.F.);
#73337=ORIENTED_EDGE('',*,*,#51549,.T.);
#73338=ORIENTED_EDGE('',*,*,#50808,.F.);
#73339=ORIENTED_EDGE('',*,*,#51551,.T.);
#73340=ORIENTED_EDGE('',*,*,#51526,.F.);
#73341=ORIENTED_EDGE('',*,*,#51550,.F.);
#73342=ORIENTED_EDGE('',*,*,#50640,.F.);
#73343=ORIENTED_EDGE('',*,*,#51543,.T.);
#73344=ORIENTED_EDGE('',*,*,#51539,.T.);
#73345=ORIENTED_EDGE('',*,*,#51551,.F.);
#73346=ORIENTED_EDGE('',*,*,#50639,.T.);
#73347=ORIENTED_EDGE('',*,*,#51537,.T.);
#73348=ORIENTED_EDGE('',*,*,#51540,.T.);
#73349=ORIENTED_EDGE('',*,*,#51542,.T.);
#73350=ORIENTED_EDGE('',*,*,#51552,.T.);
#73351=ORIENTED_EDGE('',*,*,#51553,.T.);
#73352=ORIENTED_EDGE('',*,*,#51554,.T.);
#73353=ORIENTED_EDGE('',*,*,#51555,.T.);
#73354=ORIENTED_EDGE('',*,*,#51556,.T.);
#73355=ORIENTED_EDGE('',*,*,#51557,.T.);
#73356=ORIENTED_EDGE('',*,*,#51558,.T.);
#73357=ORIENTED_EDGE('',*,*,#51559,.F.);
#73358=ORIENTED_EDGE('',*,*,#51560,.T.);
#73359=ORIENTED_EDGE('',*,*,#51561,.T.);
#73360=ORIENTED_EDGE('',*,*,#51559,.T.);
#73361=ORIENTED_EDGE('',*,*,#51562,.T.);
#73362=ORIENTED_EDGE('',*,*,#51552,.F.);
#73363=ORIENTED_EDGE('',*,*,#51563,.T.);
#73364=ORIENTED_EDGE('',*,*,#51564,.F.);
#73365=ORIENTED_EDGE('',*,*,#51560,.F.);
#73366=ORIENTED_EDGE('',*,*,#51565,.F.);
#73367=ORIENTED_EDGE('',*,*,#51566,.F.);
#73368=ORIENTED_EDGE('',*,*,#51565,.T.);
#73369=ORIENTED_EDGE('',*,*,#51563,.F.);
#73370=ORIENTED_EDGE('',*,*,#51567,.F.);
#73371=ORIENTED_EDGE('',*,*,#51567,.T.);
#73372=ORIENTED_EDGE('',*,*,#51556,.F.);
#73373=ORIENTED_EDGE('',*,*,#51568,.F.);
#73374=ORIENTED_EDGE('',*,*,#51569,.F.);
#73375=ORIENTED_EDGE('',*,*,#51570,.T.);
#73376=ORIENTED_EDGE('',*,*,#51571,.F.);
#73377=ORIENTED_EDGE('',*,*,#51572,.F.);
#73378=ORIENTED_EDGE('',*,*,#50644,.F.);
#73379=ORIENTED_EDGE('',*,*,#51573,.T.);
#73380=ORIENTED_EDGE('',*,*,#51564,.T.);
#73381=ORIENTED_EDGE('',*,*,#51570,.F.);
#73382=ORIENTED_EDGE('',*,*,#50643,.T.);
#73383=ORIENTED_EDGE('',*,*,#51574,.F.);
#73384=ORIENTED_EDGE('',*,*,#51561,.F.);
#73385=ORIENTED_EDGE('',*,*,#51573,.F.);
#73386=ORIENTED_EDGE('',*,*,#50642,.F.);
#73387=ORIENTED_EDGE('',*,*,#51574,.T.);
#73388=ORIENTED_EDGE('',*,*,#50807,.F.);
#73389=ORIENTED_EDGE('',*,*,#51575,.F.);
#73390=ORIENTED_EDGE('',*,*,#51557,.F.);
#73391=ORIENTED_EDGE('',*,*,#51575,.T.);
#73392=ORIENTED_EDGE('',*,*,#49882,.F.);
#73393=ORIENTED_EDGE('',*,*,#51576,.F.);
#73394=ORIENTED_EDGE('',*,*,#51558,.F.);
#73395=ORIENTED_EDGE('',*,*,#51576,.T.);
#73396=ORIENTED_EDGE('',*,*,#49881,.F.);
#73397=ORIENTED_EDGE('',*,*,#51577,.F.);
#73398=ORIENTED_EDGE('',*,*,#51562,.F.);
#73399=ORIENTED_EDGE('',*,*,#51577,.T.);
#73400=ORIENTED_EDGE('',*,*,#49880,.F.);
#73401=ORIENTED_EDGE('',*,*,#51578,.F.);
#73402=ORIENTED_EDGE('',*,*,#51553,.F.);
#73403=ORIENTED_EDGE('',*,*,#51579,.T.);
#73404=ORIENTED_EDGE('',*,*,#51554,.F.);
#73405=ORIENTED_EDGE('',*,*,#51578,.T.);
#73406=ORIENTED_EDGE('',*,*,#50806,.F.);
#73407=ORIENTED_EDGE('',*,*,#51580,.T.);
#73408=ORIENTED_EDGE('',*,*,#51555,.F.);
#73409=ORIENTED_EDGE('',*,*,#51579,.F.);
#73410=ORIENTED_EDGE('',*,*,#50646,.F.);
#73411=ORIENTED_EDGE('',*,*,#51572,.T.);
#73412=ORIENTED_EDGE('',*,*,#51568,.T.);
#73413=ORIENTED_EDGE('',*,*,#51580,.F.);
#73414=ORIENTED_EDGE('',*,*,#50645,.T.);
#73415=ORIENTED_EDGE('',*,*,#51566,.T.);
#73416=ORIENTED_EDGE('',*,*,#51569,.T.);
#73417=ORIENTED_EDGE('',*,*,#51571,.T.);
#73418=ORIENTED_EDGE('',*,*,#51581,.T.);
#73419=ORIENTED_EDGE('',*,*,#51582,.T.);
#73420=ORIENTED_EDGE('',*,*,#51583,.T.);
#73421=ORIENTED_EDGE('',*,*,#51584,.T.);
#73422=ORIENTED_EDGE('',*,*,#51585,.T.);
#73423=ORIENTED_EDGE('',*,*,#51586,.T.);
#73424=ORIENTED_EDGE('',*,*,#51587,.T.);
#73425=ORIENTED_EDGE('',*,*,#51588,.F.);
#73426=ORIENTED_EDGE('',*,*,#51589,.T.);
#73427=ORIENTED_EDGE('',*,*,#51590,.T.);
#73428=ORIENTED_EDGE('',*,*,#51588,.T.);
#73429=ORIENTED_EDGE('',*,*,#51591,.T.);
#73430=ORIENTED_EDGE('',*,*,#51581,.F.);
#73431=ORIENTED_EDGE('',*,*,#51592,.T.);
#73432=ORIENTED_EDGE('',*,*,#51593,.F.);
#73433=ORIENTED_EDGE('',*,*,#51589,.F.);
#73434=ORIENTED_EDGE('',*,*,#51594,.F.);
#73435=ORIENTED_EDGE('',*,*,#51595,.F.);
#73436=ORIENTED_EDGE('',*,*,#51594,.T.);
#73437=ORIENTED_EDGE('',*,*,#51592,.F.);
#73438=ORIENTED_EDGE('',*,*,#51596,.F.);
#73439=ORIENTED_EDGE('',*,*,#51596,.T.);
#73440=ORIENTED_EDGE('',*,*,#51585,.F.);
#73441=ORIENTED_EDGE('',*,*,#51597,.F.);
#73442=ORIENTED_EDGE('',*,*,#51598,.F.);
#73443=ORIENTED_EDGE('',*,*,#51599,.T.);
#73444=ORIENTED_EDGE('',*,*,#51600,.F.);
#73445=ORIENTED_EDGE('',*,*,#51601,.F.);
#73446=ORIENTED_EDGE('',*,*,#50650,.F.);
#73447=ORIENTED_EDGE('',*,*,#51602,.T.);
#73448=ORIENTED_EDGE('',*,*,#51593,.T.);
#73449=ORIENTED_EDGE('',*,*,#51599,.F.);
#73450=ORIENTED_EDGE('',*,*,#50649,.T.);
#73451=ORIENTED_EDGE('',*,*,#51603,.F.);
#73452=ORIENTED_EDGE('',*,*,#51590,.F.);
#73453=ORIENTED_EDGE('',*,*,#51602,.F.);
#73454=ORIENTED_EDGE('',*,*,#50648,.F.);
#73455=ORIENTED_EDGE('',*,*,#51603,.T.);
#73456=ORIENTED_EDGE('',*,*,#50805,.F.);
#73457=ORIENTED_EDGE('',*,*,#51604,.F.);
#73458=ORIENTED_EDGE('',*,*,#51586,.F.);
#73459=ORIENTED_EDGE('',*,*,#51604,.T.);
#73460=ORIENTED_EDGE('',*,*,#49878,.F.);
#73461=ORIENTED_EDGE('',*,*,#51605,.F.);
#73462=ORIENTED_EDGE('',*,*,#51587,.F.);
#73463=ORIENTED_EDGE('',*,*,#51605,.T.);
#73464=ORIENTED_EDGE('',*,*,#49877,.F.);
#73465=ORIENTED_EDGE('',*,*,#51606,.F.);
#73466=ORIENTED_EDGE('',*,*,#51591,.F.);
#73467=ORIENTED_EDGE('',*,*,#51606,.T.);
#73468=ORIENTED_EDGE('',*,*,#49876,.F.);
#73469=ORIENTED_EDGE('',*,*,#51607,.F.);
#73470=ORIENTED_EDGE('',*,*,#51582,.F.);
#73471=ORIENTED_EDGE('',*,*,#51608,.T.);
#73472=ORIENTED_EDGE('',*,*,#51583,.F.);
#73473=ORIENTED_EDGE('',*,*,#51607,.T.);
#73474=ORIENTED_EDGE('',*,*,#50804,.F.);
#73475=ORIENTED_EDGE('',*,*,#51609,.T.);
#73476=ORIENTED_EDGE('',*,*,#51584,.F.);
#73477=ORIENTED_EDGE('',*,*,#51608,.F.);
#73478=ORIENTED_EDGE('',*,*,#50652,.F.);
#73479=ORIENTED_EDGE('',*,*,#51601,.T.);
#73480=ORIENTED_EDGE('',*,*,#51597,.T.);
#73481=ORIENTED_EDGE('',*,*,#51609,.F.);
#73482=ORIENTED_EDGE('',*,*,#50651,.T.);
#73483=ORIENTED_EDGE('',*,*,#51595,.T.);
#73484=ORIENTED_EDGE('',*,*,#51598,.T.);
#73485=ORIENTED_EDGE('',*,*,#51600,.T.);
#73486=ORIENTED_EDGE('',*,*,#51610,.T.);
#73487=ORIENTED_EDGE('',*,*,#51611,.T.);
#73488=ORIENTED_EDGE('',*,*,#51612,.T.);
#73489=ORIENTED_EDGE('',*,*,#51613,.T.);
#73490=ORIENTED_EDGE('',*,*,#51614,.T.);
#73491=ORIENTED_EDGE('',*,*,#51615,.T.);
#73492=ORIENTED_EDGE('',*,*,#51616,.T.);
#73493=ORIENTED_EDGE('',*,*,#51617,.F.);
#73494=ORIENTED_EDGE('',*,*,#51618,.T.);
#73495=ORIENTED_EDGE('',*,*,#51619,.T.);
#73496=ORIENTED_EDGE('',*,*,#51617,.T.);
#73497=ORIENTED_EDGE('',*,*,#51620,.T.);
#73498=ORIENTED_EDGE('',*,*,#51610,.F.);
#73499=ORIENTED_EDGE('',*,*,#51621,.T.);
#73500=ORIENTED_EDGE('',*,*,#51622,.F.);
#73501=ORIENTED_EDGE('',*,*,#51618,.F.);
#73502=ORIENTED_EDGE('',*,*,#51623,.F.);
#73503=ORIENTED_EDGE('',*,*,#51624,.F.);
#73504=ORIENTED_EDGE('',*,*,#51623,.T.);
#73505=ORIENTED_EDGE('',*,*,#51621,.F.);
#73506=ORIENTED_EDGE('',*,*,#51625,.F.);
#73507=ORIENTED_EDGE('',*,*,#51625,.T.);
#73508=ORIENTED_EDGE('',*,*,#51614,.F.);
#73509=ORIENTED_EDGE('',*,*,#51626,.F.);
#73510=ORIENTED_EDGE('',*,*,#51627,.F.);
#73511=ORIENTED_EDGE('',*,*,#51628,.T.);
#73512=ORIENTED_EDGE('',*,*,#51629,.F.);
#73513=ORIENTED_EDGE('',*,*,#51630,.F.);
#73514=ORIENTED_EDGE('',*,*,#50656,.F.);
#73515=ORIENTED_EDGE('',*,*,#51631,.T.);
#73516=ORIENTED_EDGE('',*,*,#51622,.T.);
#73517=ORIENTED_EDGE('',*,*,#51628,.F.);
#73518=ORIENTED_EDGE('',*,*,#50655,.T.);
#73519=ORIENTED_EDGE('',*,*,#51632,.F.);
#73520=ORIENTED_EDGE('',*,*,#51619,.F.);
#73521=ORIENTED_EDGE('',*,*,#51631,.F.);
#73522=ORIENTED_EDGE('',*,*,#50654,.F.);
#73523=ORIENTED_EDGE('',*,*,#51632,.T.);
#73524=ORIENTED_EDGE('',*,*,#50803,.F.);
#73525=ORIENTED_EDGE('',*,*,#51633,.F.);
#73526=ORIENTED_EDGE('',*,*,#51615,.F.);
#73527=ORIENTED_EDGE('',*,*,#51633,.T.);
#73528=ORIENTED_EDGE('',*,*,#49874,.F.);
#73529=ORIENTED_EDGE('',*,*,#51634,.F.);
#73530=ORIENTED_EDGE('',*,*,#51616,.F.);
#73531=ORIENTED_EDGE('',*,*,#51634,.T.);
#73532=ORIENTED_EDGE('',*,*,#49873,.F.);
#73533=ORIENTED_EDGE('',*,*,#51635,.F.);
#73534=ORIENTED_EDGE('',*,*,#51620,.F.);
#73535=ORIENTED_EDGE('',*,*,#51635,.T.);
#73536=ORIENTED_EDGE('',*,*,#49872,.F.);
#73537=ORIENTED_EDGE('',*,*,#51636,.F.);
#73538=ORIENTED_EDGE('',*,*,#51611,.F.);
#73539=ORIENTED_EDGE('',*,*,#51637,.T.);
#73540=ORIENTED_EDGE('',*,*,#51612,.F.);
#73541=ORIENTED_EDGE('',*,*,#51636,.T.);
#73542=ORIENTED_EDGE('',*,*,#50659,.F.);
#73543=ORIENTED_EDGE('',*,*,#51638,.T.);
#73544=ORIENTED_EDGE('',*,*,#51613,.F.);
#73545=ORIENTED_EDGE('',*,*,#51637,.F.);
#73546=ORIENTED_EDGE('',*,*,#50658,.F.);
#73547=ORIENTED_EDGE('',*,*,#51630,.T.);
#73548=ORIENTED_EDGE('',*,*,#51626,.T.);
#73549=ORIENTED_EDGE('',*,*,#51638,.F.);
#73550=ORIENTED_EDGE('',*,*,#50657,.T.);
#73551=ORIENTED_EDGE('',*,*,#51624,.T.);
#73552=ORIENTED_EDGE('',*,*,#51627,.T.);
#73553=ORIENTED_EDGE('',*,*,#51629,.T.);
#73554=ORIENTED_EDGE('',*,*,#51639,.T.);
#73555=ORIENTED_EDGE('',*,*,#51640,.T.);
#73556=ORIENTED_EDGE('',*,*,#51641,.T.);
#73557=ORIENTED_EDGE('',*,*,#51642,.T.);
#73558=ORIENTED_EDGE('',*,*,#51643,.T.);
#73559=ORIENTED_EDGE('',*,*,#51644,.T.);
#73560=ORIENTED_EDGE('',*,*,#51645,.T.);
#73561=ORIENTED_EDGE('',*,*,#51646,.F.);
#73562=ORIENTED_EDGE('',*,*,#51647,.T.);
#73563=ORIENTED_EDGE('',*,*,#51648,.T.);
#73564=ORIENTED_EDGE('',*,*,#51646,.T.);
#73565=ORIENTED_EDGE('',*,*,#51649,.T.);
#73566=ORIENTED_EDGE('',*,*,#51639,.F.);
#73567=ORIENTED_EDGE('',*,*,#51650,.T.);
#73568=ORIENTED_EDGE('',*,*,#51651,.F.);
#73569=ORIENTED_EDGE('',*,*,#51647,.F.);
#73570=ORIENTED_EDGE('',*,*,#51652,.F.);
#73571=ORIENTED_EDGE('',*,*,#51653,.F.);
#73572=ORIENTED_EDGE('',*,*,#51652,.T.);
#73573=ORIENTED_EDGE('',*,*,#51650,.F.);
#73574=ORIENTED_EDGE('',*,*,#51654,.F.);
#73575=ORIENTED_EDGE('',*,*,#51654,.T.);
#73576=ORIENTED_EDGE('',*,*,#51643,.F.);
#73577=ORIENTED_EDGE('',*,*,#51655,.F.);
#73578=ORIENTED_EDGE('',*,*,#51656,.F.);
#73579=ORIENTED_EDGE('',*,*,#51657,.T.);
#73580=ORIENTED_EDGE('',*,*,#51658,.F.);
#73581=ORIENTED_EDGE('',*,*,#51659,.F.);
#73582=ORIENTED_EDGE('',*,*,#50072,.F.);
#73583=ORIENTED_EDGE('',*,*,#51660,.T.);
#73584=ORIENTED_EDGE('',*,*,#51651,.T.);
#73585=ORIENTED_EDGE('',*,*,#51657,.F.);
#73586=ORIENTED_EDGE('',*,*,#50071,.T.);
#73587=ORIENTED_EDGE('',*,*,#51661,.F.);
#73588=ORIENTED_EDGE('',*,*,#51648,.F.);
#73589=ORIENTED_EDGE('',*,*,#51660,.F.);
#73590=ORIENTED_EDGE('',*,*,#50070,.F.);
#73591=ORIENTED_EDGE('',*,*,#51661,.T.);
#73592=ORIENTED_EDGE('',*,*,#50660,.F.);
#73593=ORIENTED_EDGE('',*,*,#51662,.F.);
#73594=ORIENTED_EDGE('',*,*,#51644,.F.);
#73595=ORIENTED_EDGE('',*,*,#51662,.T.);
#73596=ORIENTED_EDGE('',*,*,#49866,.F.);
#73597=ORIENTED_EDGE('',*,*,#51663,.F.);
#73598=ORIENTED_EDGE('',*,*,#51645,.F.);
#73599=ORIENTED_EDGE('',*,*,#51663,.T.);
#73600=ORIENTED_EDGE('',*,*,#49865,.F.);
#73601=ORIENTED_EDGE('',*,*,#51664,.F.);
#73602=ORIENTED_EDGE('',*,*,#51649,.F.);
#73603=ORIENTED_EDGE('',*,*,#51664,.T.);
#73604=ORIENTED_EDGE('',*,*,#49864,.F.);
#73605=ORIENTED_EDGE('',*,*,#51665,.F.);
#73606=ORIENTED_EDGE('',*,*,#51640,.F.);
#73607=ORIENTED_EDGE('',*,*,#51666,.T.);
#73608=ORIENTED_EDGE('',*,*,#51641,.F.);
#73609=ORIENTED_EDGE('',*,*,#51665,.T.);
#73610=ORIENTED_EDGE('',*,*,#50802,.F.);
#73611=ORIENTED_EDGE('',*,*,#51667,.T.);
#73612=ORIENTED_EDGE('',*,*,#51642,.F.);
#73613=ORIENTED_EDGE('',*,*,#51666,.F.);
#73614=ORIENTED_EDGE('',*,*,#50074,.F.);
#73615=ORIENTED_EDGE('',*,*,#51659,.T.);
#73616=ORIENTED_EDGE('',*,*,#51655,.T.);
#73617=ORIENTED_EDGE('',*,*,#51667,.F.);
#73618=ORIENTED_EDGE('',*,*,#50073,.T.);
#73619=ORIENTED_EDGE('',*,*,#51653,.T.);
#73620=ORIENTED_EDGE('',*,*,#51656,.T.);
#73621=ORIENTED_EDGE('',*,*,#51658,.T.);
#73622=ORIENTED_EDGE('',*,*,#51668,.T.);
#73623=ORIENTED_EDGE('',*,*,#51669,.T.);
#73624=ORIENTED_EDGE('',*,*,#51670,.T.);
#73625=ORIENTED_EDGE('',*,*,#51671,.T.);
#73626=ORIENTED_EDGE('',*,*,#51672,.T.);
#73627=ORIENTED_EDGE('',*,*,#51673,.T.);
#73628=ORIENTED_EDGE('',*,*,#51674,.T.);
#73629=ORIENTED_EDGE('',*,*,#51675,.F.);
#73630=ORIENTED_EDGE('',*,*,#51676,.T.);
#73631=ORIENTED_EDGE('',*,*,#51677,.T.);
#73632=ORIENTED_EDGE('',*,*,#51675,.T.);
#73633=ORIENTED_EDGE('',*,*,#51678,.T.);
#73634=ORIENTED_EDGE('',*,*,#51668,.F.);
#73635=ORIENTED_EDGE('',*,*,#51679,.T.);
#73636=ORIENTED_EDGE('',*,*,#51680,.F.);
#73637=ORIENTED_EDGE('',*,*,#51676,.F.);
#73638=ORIENTED_EDGE('',*,*,#51681,.F.);
#73639=ORIENTED_EDGE('',*,*,#51682,.F.);
#73640=ORIENTED_EDGE('',*,*,#51681,.T.);
#73641=ORIENTED_EDGE('',*,*,#51679,.F.);
#73642=ORIENTED_EDGE('',*,*,#51683,.F.);
#73643=ORIENTED_EDGE('',*,*,#51683,.T.);
#73644=ORIENTED_EDGE('',*,*,#51672,.F.);
#73645=ORIENTED_EDGE('',*,*,#51684,.F.);
#73646=ORIENTED_EDGE('',*,*,#51685,.F.);
#73647=ORIENTED_EDGE('',*,*,#51686,.T.);
#73648=ORIENTED_EDGE('',*,*,#51687,.F.);
#73649=ORIENTED_EDGE('',*,*,#51688,.F.);
#73650=ORIENTED_EDGE('',*,*,#50078,.F.);
#73651=ORIENTED_EDGE('',*,*,#51689,.T.);
#73652=ORIENTED_EDGE('',*,*,#51680,.T.);
#73653=ORIENTED_EDGE('',*,*,#51686,.F.);
#73654=ORIENTED_EDGE('',*,*,#50077,.T.);
#73655=ORIENTED_EDGE('',*,*,#51690,.F.);
#73656=ORIENTED_EDGE('',*,*,#51677,.F.);
#73657=ORIENTED_EDGE('',*,*,#51689,.F.);
#73658=ORIENTED_EDGE('',*,*,#50076,.F.);
#73659=ORIENTED_EDGE('',*,*,#51690,.T.);
#73660=ORIENTED_EDGE('',*,*,#50801,.F.);
#73661=ORIENTED_EDGE('',*,*,#51691,.F.);
#73662=ORIENTED_EDGE('',*,*,#51673,.F.);
#73663=ORIENTED_EDGE('',*,*,#51691,.T.);
#73664=ORIENTED_EDGE('',*,*,#49862,.F.);
#73665=ORIENTED_EDGE('',*,*,#51692,.F.);
#73666=ORIENTED_EDGE('',*,*,#51674,.F.);
#73667=ORIENTED_EDGE('',*,*,#51692,.T.);
#73668=ORIENTED_EDGE('',*,*,#49861,.F.);
#73669=ORIENTED_EDGE('',*,*,#51693,.F.);
#73670=ORIENTED_EDGE('',*,*,#51678,.F.);
#73671=ORIENTED_EDGE('',*,*,#51693,.T.);
#73672=ORIENTED_EDGE('',*,*,#49860,.F.);
#73673=ORIENTED_EDGE('',*,*,#51694,.F.);
#73674=ORIENTED_EDGE('',*,*,#51669,.F.);
#73675=ORIENTED_EDGE('',*,*,#51695,.T.);
#73676=ORIENTED_EDGE('',*,*,#51670,.F.);
#73677=ORIENTED_EDGE('',*,*,#51694,.T.);
#73678=ORIENTED_EDGE('',*,*,#50800,.F.);
#73679=ORIENTED_EDGE('',*,*,#51696,.T.);
#73680=ORIENTED_EDGE('',*,*,#51671,.F.);
#73681=ORIENTED_EDGE('',*,*,#51695,.F.);
#73682=ORIENTED_EDGE('',*,*,#50080,.F.);
#73683=ORIENTED_EDGE('',*,*,#51688,.T.);
#73684=ORIENTED_EDGE('',*,*,#51684,.T.);
#73685=ORIENTED_EDGE('',*,*,#51696,.F.);
#73686=ORIENTED_EDGE('',*,*,#50079,.T.);
#73687=ORIENTED_EDGE('',*,*,#51682,.T.);
#73688=ORIENTED_EDGE('',*,*,#51685,.T.);
#73689=ORIENTED_EDGE('',*,*,#51687,.T.);
#73690=ORIENTED_EDGE('',*,*,#51697,.T.);
#73691=ORIENTED_EDGE('',*,*,#51698,.T.);
#73692=ORIENTED_EDGE('',*,*,#51699,.T.);
#73693=ORIENTED_EDGE('',*,*,#51700,.T.);
#73694=ORIENTED_EDGE('',*,*,#51701,.T.);
#73695=ORIENTED_EDGE('',*,*,#51702,.T.);
#73696=ORIENTED_EDGE('',*,*,#51703,.T.);
#73697=ORIENTED_EDGE('',*,*,#51704,.F.);
#73698=ORIENTED_EDGE('',*,*,#51705,.T.);
#73699=ORIENTED_EDGE('',*,*,#51706,.T.);
#73700=ORIENTED_EDGE('',*,*,#51704,.T.);
#73701=ORIENTED_EDGE('',*,*,#51707,.T.);
#73702=ORIENTED_EDGE('',*,*,#51697,.F.);
#73703=ORIENTED_EDGE('',*,*,#51708,.T.);
#73704=ORIENTED_EDGE('',*,*,#51709,.F.);
#73705=ORIENTED_EDGE('',*,*,#51705,.F.);
#73706=ORIENTED_EDGE('',*,*,#51710,.F.);
#73707=ORIENTED_EDGE('',*,*,#51711,.F.);
#73708=ORIENTED_EDGE('',*,*,#51710,.T.);
#73709=ORIENTED_EDGE('',*,*,#51708,.F.);
#73710=ORIENTED_EDGE('',*,*,#51712,.F.);
#73711=ORIENTED_EDGE('',*,*,#51712,.T.);
#73712=ORIENTED_EDGE('',*,*,#51701,.F.);
#73713=ORIENTED_EDGE('',*,*,#51713,.F.);
#73714=ORIENTED_EDGE('',*,*,#51714,.F.);
#73715=ORIENTED_EDGE('',*,*,#51715,.T.);
#73716=ORIENTED_EDGE('',*,*,#51716,.F.);
#73717=ORIENTED_EDGE('',*,*,#51717,.F.);
#73718=ORIENTED_EDGE('',*,*,#50084,.F.);
#73719=ORIENTED_EDGE('',*,*,#51718,.T.);
#73720=ORIENTED_EDGE('',*,*,#51709,.T.);
#73721=ORIENTED_EDGE('',*,*,#51715,.F.);
#73722=ORIENTED_EDGE('',*,*,#50083,.T.);
#73723=ORIENTED_EDGE('',*,*,#51719,.F.);
#73724=ORIENTED_EDGE('',*,*,#51706,.F.);
#73725=ORIENTED_EDGE('',*,*,#51718,.F.);
#73726=ORIENTED_EDGE('',*,*,#50082,.F.);
#73727=ORIENTED_EDGE('',*,*,#51719,.T.);
#73728=ORIENTED_EDGE('',*,*,#50799,.F.);
#73729=ORIENTED_EDGE('',*,*,#51720,.F.);
#73730=ORIENTED_EDGE('',*,*,#51702,.F.);
#73731=ORIENTED_EDGE('',*,*,#51720,.T.);
#73732=ORIENTED_EDGE('',*,*,#49858,.F.);
#73733=ORIENTED_EDGE('',*,*,#51721,.F.);
#73734=ORIENTED_EDGE('',*,*,#51703,.F.);
#73735=ORIENTED_EDGE('',*,*,#51721,.T.);
#73736=ORIENTED_EDGE('',*,*,#49857,.F.);
#73737=ORIENTED_EDGE('',*,*,#51722,.F.);
#73738=ORIENTED_EDGE('',*,*,#51707,.F.);
#73739=ORIENTED_EDGE('',*,*,#51722,.T.);
#73740=ORIENTED_EDGE('',*,*,#49856,.F.);
#73741=ORIENTED_EDGE('',*,*,#51723,.F.);
#73742=ORIENTED_EDGE('',*,*,#51698,.F.);
#73743=ORIENTED_EDGE('',*,*,#51724,.T.);
#73744=ORIENTED_EDGE('',*,*,#51699,.F.);
#73745=ORIENTED_EDGE('',*,*,#51723,.T.);
#73746=ORIENTED_EDGE('',*,*,#50798,.F.);
#73747=ORIENTED_EDGE('',*,*,#51725,.T.);
#73748=ORIENTED_EDGE('',*,*,#51700,.F.);
#73749=ORIENTED_EDGE('',*,*,#51724,.F.);
#73750=ORIENTED_EDGE('',*,*,#50086,.F.);
#73751=ORIENTED_EDGE('',*,*,#51717,.T.);
#73752=ORIENTED_EDGE('',*,*,#51713,.T.);
#73753=ORIENTED_EDGE('',*,*,#51725,.F.);
#73754=ORIENTED_EDGE('',*,*,#50085,.T.);
#73755=ORIENTED_EDGE('',*,*,#51711,.T.);
#73756=ORIENTED_EDGE('',*,*,#51714,.T.);
#73757=ORIENTED_EDGE('',*,*,#51716,.T.);
#73758=ORIENTED_EDGE('',*,*,#51726,.T.);
#73759=ORIENTED_EDGE('',*,*,#51727,.T.);
#73760=ORIENTED_EDGE('',*,*,#51728,.T.);
#73761=ORIENTED_EDGE('',*,*,#51729,.T.);
#73762=ORIENTED_EDGE('',*,*,#51730,.T.);
#73763=ORIENTED_EDGE('',*,*,#51731,.T.);
#73764=ORIENTED_EDGE('',*,*,#51732,.T.);
#73765=ORIENTED_EDGE('',*,*,#51733,.F.);
#73766=ORIENTED_EDGE('',*,*,#51734,.T.);
#73767=ORIENTED_EDGE('',*,*,#51735,.T.);
#73768=ORIENTED_EDGE('',*,*,#51733,.T.);
#73769=ORIENTED_EDGE('',*,*,#51736,.T.);
#73770=ORIENTED_EDGE('',*,*,#51726,.F.);
#73771=ORIENTED_EDGE('',*,*,#51737,.T.);
#73772=ORIENTED_EDGE('',*,*,#51738,.F.);
#73773=ORIENTED_EDGE('',*,*,#51734,.F.);
#73774=ORIENTED_EDGE('',*,*,#51739,.F.);
#73775=ORIENTED_EDGE('',*,*,#51740,.F.);
#73776=ORIENTED_EDGE('',*,*,#51739,.T.);
#73777=ORIENTED_EDGE('',*,*,#51737,.F.);
#73778=ORIENTED_EDGE('',*,*,#51741,.F.);
#73779=ORIENTED_EDGE('',*,*,#51741,.T.);
#73780=ORIENTED_EDGE('',*,*,#51730,.F.);
#73781=ORIENTED_EDGE('',*,*,#51742,.F.);
#73782=ORIENTED_EDGE('',*,*,#51743,.F.);
#73783=ORIENTED_EDGE('',*,*,#51744,.T.);
#73784=ORIENTED_EDGE('',*,*,#51745,.F.);
#73785=ORIENTED_EDGE('',*,*,#51746,.F.);
#73786=ORIENTED_EDGE('',*,*,#50090,.F.);
#73787=ORIENTED_EDGE('',*,*,#51747,.T.);
#73788=ORIENTED_EDGE('',*,*,#51738,.T.);
#73789=ORIENTED_EDGE('',*,*,#51744,.F.);
#73790=ORIENTED_EDGE('',*,*,#50089,.T.);
#73791=ORIENTED_EDGE('',*,*,#51748,.F.);
#73792=ORIENTED_EDGE('',*,*,#51735,.F.);
#73793=ORIENTED_EDGE('',*,*,#51747,.F.);
#73794=ORIENTED_EDGE('',*,*,#50088,.F.);
#73795=ORIENTED_EDGE('',*,*,#51748,.T.);
#73796=ORIENTED_EDGE('',*,*,#50797,.F.);
#73797=ORIENTED_EDGE('',*,*,#51749,.F.);
#73798=ORIENTED_EDGE('',*,*,#51731,.F.);
#73799=ORIENTED_EDGE('',*,*,#51749,.T.);
#73800=ORIENTED_EDGE('',*,*,#49854,.F.);
#73801=ORIENTED_EDGE('',*,*,#51750,.F.);
#73802=ORIENTED_EDGE('',*,*,#51732,.F.);
#73803=ORIENTED_EDGE('',*,*,#51750,.T.);
#73804=ORIENTED_EDGE('',*,*,#49853,.F.);
#73805=ORIENTED_EDGE('',*,*,#51751,.F.);
#73806=ORIENTED_EDGE('',*,*,#51736,.F.);
#73807=ORIENTED_EDGE('',*,*,#51751,.T.);
#73808=ORIENTED_EDGE('',*,*,#49852,.F.);
#73809=ORIENTED_EDGE('',*,*,#51752,.F.);
#73810=ORIENTED_EDGE('',*,*,#51727,.F.);
#73811=ORIENTED_EDGE('',*,*,#51753,.T.);
#73812=ORIENTED_EDGE('',*,*,#51728,.F.);
#73813=ORIENTED_EDGE('',*,*,#51752,.T.);
#73814=ORIENTED_EDGE('',*,*,#50796,.F.);
#73815=ORIENTED_EDGE('',*,*,#51754,.T.);
#73816=ORIENTED_EDGE('',*,*,#51729,.F.);
#73817=ORIENTED_EDGE('',*,*,#51753,.F.);
#73818=ORIENTED_EDGE('',*,*,#50092,.F.);
#73819=ORIENTED_EDGE('',*,*,#51746,.T.);
#73820=ORIENTED_EDGE('',*,*,#51742,.T.);
#73821=ORIENTED_EDGE('',*,*,#51754,.F.);
#73822=ORIENTED_EDGE('',*,*,#50091,.T.);
#73823=ORIENTED_EDGE('',*,*,#51740,.T.);
#73824=ORIENTED_EDGE('',*,*,#51743,.T.);
#73825=ORIENTED_EDGE('',*,*,#51745,.T.);
#73826=ORIENTED_EDGE('',*,*,#51755,.T.);
#73827=ORIENTED_EDGE('',*,*,#51756,.T.);
#73828=ORIENTED_EDGE('',*,*,#51757,.T.);
#73829=ORIENTED_EDGE('',*,*,#51758,.T.);
#73830=ORIENTED_EDGE('',*,*,#51759,.T.);
#73831=ORIENTED_EDGE('',*,*,#51760,.T.);
#73832=ORIENTED_EDGE('',*,*,#51761,.T.);
#73833=ORIENTED_EDGE('',*,*,#51762,.F.);
#73834=ORIENTED_EDGE('',*,*,#51763,.T.);
#73835=ORIENTED_EDGE('',*,*,#51764,.T.);
#73836=ORIENTED_EDGE('',*,*,#51762,.T.);
#73837=ORIENTED_EDGE('',*,*,#51765,.T.);
#73838=ORIENTED_EDGE('',*,*,#51755,.F.);
#73839=ORIENTED_EDGE('',*,*,#51766,.T.);
#73840=ORIENTED_EDGE('',*,*,#51767,.F.);
#73841=ORIENTED_EDGE('',*,*,#51763,.F.);
#73842=ORIENTED_EDGE('',*,*,#51768,.F.);
#73843=ORIENTED_EDGE('',*,*,#51769,.F.);
#73844=ORIENTED_EDGE('',*,*,#51768,.T.);
#73845=ORIENTED_EDGE('',*,*,#51766,.F.);
#73846=ORIENTED_EDGE('',*,*,#51770,.F.);
#73847=ORIENTED_EDGE('',*,*,#51770,.T.);
#73848=ORIENTED_EDGE('',*,*,#51759,.F.);
#73849=ORIENTED_EDGE('',*,*,#51771,.F.);
#73850=ORIENTED_EDGE('',*,*,#51772,.F.);
#73851=ORIENTED_EDGE('',*,*,#51773,.T.);
#73852=ORIENTED_EDGE('',*,*,#51774,.F.);
#73853=ORIENTED_EDGE('',*,*,#51775,.F.);
#73854=ORIENTED_EDGE('',*,*,#50096,.F.);
#73855=ORIENTED_EDGE('',*,*,#51776,.T.);
#73856=ORIENTED_EDGE('',*,*,#51767,.T.);
#73857=ORIENTED_EDGE('',*,*,#51773,.F.);
#73858=ORIENTED_EDGE('',*,*,#50095,.T.);
#73859=ORIENTED_EDGE('',*,*,#51777,.F.);
#73860=ORIENTED_EDGE('',*,*,#51764,.F.);
#73861=ORIENTED_EDGE('',*,*,#51776,.F.);
#73862=ORIENTED_EDGE('',*,*,#50094,.F.);
#73863=ORIENTED_EDGE('',*,*,#51777,.T.);
#73864=ORIENTED_EDGE('',*,*,#50795,.F.);
#73865=ORIENTED_EDGE('',*,*,#51778,.F.);
#73866=ORIENTED_EDGE('',*,*,#51760,.F.);
#73867=ORIENTED_EDGE('',*,*,#51778,.T.);
#73868=ORIENTED_EDGE('',*,*,#49850,.F.);
#73869=ORIENTED_EDGE('',*,*,#51779,.F.);
#73870=ORIENTED_EDGE('',*,*,#51761,.F.);
#73871=ORIENTED_EDGE('',*,*,#51779,.T.);
#73872=ORIENTED_EDGE('',*,*,#49849,.F.);
#73873=ORIENTED_EDGE('',*,*,#51780,.F.);
#73874=ORIENTED_EDGE('',*,*,#51765,.F.);
#73875=ORIENTED_EDGE('',*,*,#51780,.T.);
#73876=ORIENTED_EDGE('',*,*,#49848,.F.);
#73877=ORIENTED_EDGE('',*,*,#51781,.F.);
#73878=ORIENTED_EDGE('',*,*,#51756,.F.);
#73879=ORIENTED_EDGE('',*,*,#51782,.T.);
#73880=ORIENTED_EDGE('',*,*,#51757,.F.);
#73881=ORIENTED_EDGE('',*,*,#51781,.T.);
#73882=ORIENTED_EDGE('',*,*,#50794,.F.);
#73883=ORIENTED_EDGE('',*,*,#51783,.T.);
#73884=ORIENTED_EDGE('',*,*,#51758,.F.);
#73885=ORIENTED_EDGE('',*,*,#51782,.F.);
#73886=ORIENTED_EDGE('',*,*,#50098,.F.);
#73887=ORIENTED_EDGE('',*,*,#51775,.T.);
#73888=ORIENTED_EDGE('',*,*,#51771,.T.);
#73889=ORIENTED_EDGE('',*,*,#51783,.F.);
#73890=ORIENTED_EDGE('',*,*,#50097,.T.);
#73891=ORIENTED_EDGE('',*,*,#51769,.T.);
#73892=ORIENTED_EDGE('',*,*,#51772,.T.);
#73893=ORIENTED_EDGE('',*,*,#51774,.T.);
#73894=ORIENTED_EDGE('',*,*,#51784,.T.);
#73895=ORIENTED_EDGE('',*,*,#51785,.T.);
#73896=ORIENTED_EDGE('',*,*,#51786,.T.);
#73897=ORIENTED_EDGE('',*,*,#51787,.T.);
#73898=ORIENTED_EDGE('',*,*,#51788,.T.);
#73899=ORIENTED_EDGE('',*,*,#51789,.T.);
#73900=ORIENTED_EDGE('',*,*,#51790,.T.);
#73901=ORIENTED_EDGE('',*,*,#51791,.F.);
#73902=ORIENTED_EDGE('',*,*,#51792,.T.);
#73903=ORIENTED_EDGE('',*,*,#51793,.T.);
#73904=ORIENTED_EDGE('',*,*,#51791,.T.);
#73905=ORIENTED_EDGE('',*,*,#51794,.T.);
#73906=ORIENTED_EDGE('',*,*,#51784,.F.);
#73907=ORIENTED_EDGE('',*,*,#51795,.T.);
#73908=ORIENTED_EDGE('',*,*,#51796,.F.);
#73909=ORIENTED_EDGE('',*,*,#51792,.F.);
#73910=ORIENTED_EDGE('',*,*,#51797,.F.);
#73911=ORIENTED_EDGE('',*,*,#51798,.F.);
#73912=ORIENTED_EDGE('',*,*,#51797,.T.);
#73913=ORIENTED_EDGE('',*,*,#51795,.F.);
#73914=ORIENTED_EDGE('',*,*,#51799,.F.);
#73915=ORIENTED_EDGE('',*,*,#51799,.T.);
#73916=ORIENTED_EDGE('',*,*,#51788,.F.);
#73917=ORIENTED_EDGE('',*,*,#51800,.F.);
#73918=ORIENTED_EDGE('',*,*,#51801,.F.);
#73919=ORIENTED_EDGE('',*,*,#51802,.T.);
#73920=ORIENTED_EDGE('',*,*,#51803,.F.);
#73921=ORIENTED_EDGE('',*,*,#51804,.F.);
#73922=ORIENTED_EDGE('',*,*,#50102,.F.);
#73923=ORIENTED_EDGE('',*,*,#51805,.T.);
#73924=ORIENTED_EDGE('',*,*,#51796,.T.);
#73925=ORIENTED_EDGE('',*,*,#51802,.F.);
#73926=ORIENTED_EDGE('',*,*,#50101,.T.);
#73927=ORIENTED_EDGE('',*,*,#51806,.F.);
#73928=ORIENTED_EDGE('',*,*,#51793,.F.);
#73929=ORIENTED_EDGE('',*,*,#51805,.F.);
#73930=ORIENTED_EDGE('',*,*,#50100,.F.);
#73931=ORIENTED_EDGE('',*,*,#51806,.T.);
#73932=ORIENTED_EDGE('',*,*,#50793,.F.);
#73933=ORIENTED_EDGE('',*,*,#51807,.F.);
#73934=ORIENTED_EDGE('',*,*,#51789,.F.);
#73935=ORIENTED_EDGE('',*,*,#51807,.T.);
#73936=ORIENTED_EDGE('',*,*,#49846,.F.);
#73937=ORIENTED_EDGE('',*,*,#51808,.F.);
#73938=ORIENTED_EDGE('',*,*,#51790,.F.);
#73939=ORIENTED_EDGE('',*,*,#51808,.T.);
#73940=ORIENTED_EDGE('',*,*,#49845,.F.);
#73941=ORIENTED_EDGE('',*,*,#51809,.F.);
#73942=ORIENTED_EDGE('',*,*,#51794,.F.);
#73943=ORIENTED_EDGE('',*,*,#51809,.T.);
#73944=ORIENTED_EDGE('',*,*,#49844,.F.);
#73945=ORIENTED_EDGE('',*,*,#51810,.F.);
#73946=ORIENTED_EDGE('',*,*,#51785,.F.);
#73947=ORIENTED_EDGE('',*,*,#51811,.T.);
#73948=ORIENTED_EDGE('',*,*,#51786,.F.);
#73949=ORIENTED_EDGE('',*,*,#51810,.T.);
#73950=ORIENTED_EDGE('',*,*,#50792,.F.);
#73951=ORIENTED_EDGE('',*,*,#51812,.T.);
#73952=ORIENTED_EDGE('',*,*,#51787,.F.);
#73953=ORIENTED_EDGE('',*,*,#51811,.F.);
#73954=ORIENTED_EDGE('',*,*,#50104,.F.);
#73955=ORIENTED_EDGE('',*,*,#51804,.T.);
#73956=ORIENTED_EDGE('',*,*,#51800,.T.);
#73957=ORIENTED_EDGE('',*,*,#51812,.F.);
#73958=ORIENTED_EDGE('',*,*,#50103,.T.);
#73959=ORIENTED_EDGE('',*,*,#51798,.T.);
#73960=ORIENTED_EDGE('',*,*,#51801,.T.);
#73961=ORIENTED_EDGE('',*,*,#51803,.T.);
#73962=ORIENTED_EDGE('',*,*,#51813,.T.);
#73963=ORIENTED_EDGE('',*,*,#51814,.T.);
#73964=ORIENTED_EDGE('',*,*,#51815,.T.);
#73965=ORIENTED_EDGE('',*,*,#51816,.T.);
#73966=ORIENTED_EDGE('',*,*,#51817,.T.);
#73967=ORIENTED_EDGE('',*,*,#51818,.T.);
#73968=ORIENTED_EDGE('',*,*,#51819,.T.);
#73969=ORIENTED_EDGE('',*,*,#51820,.F.);
#73970=ORIENTED_EDGE('',*,*,#51821,.T.);
#73971=ORIENTED_EDGE('',*,*,#51822,.T.);
#73972=ORIENTED_EDGE('',*,*,#51820,.T.);
#73973=ORIENTED_EDGE('',*,*,#51823,.T.);
#73974=ORIENTED_EDGE('',*,*,#51813,.F.);
#73975=ORIENTED_EDGE('',*,*,#51824,.T.);
#73976=ORIENTED_EDGE('',*,*,#51825,.F.);
#73977=ORIENTED_EDGE('',*,*,#51821,.F.);
#73978=ORIENTED_EDGE('',*,*,#51826,.F.);
#73979=ORIENTED_EDGE('',*,*,#51827,.F.);
#73980=ORIENTED_EDGE('',*,*,#51826,.T.);
#73981=ORIENTED_EDGE('',*,*,#51824,.F.);
#73982=ORIENTED_EDGE('',*,*,#51828,.F.);
#73983=ORIENTED_EDGE('',*,*,#51828,.T.);
#73984=ORIENTED_EDGE('',*,*,#51817,.F.);
#73985=ORIENTED_EDGE('',*,*,#51829,.F.);
#73986=ORIENTED_EDGE('',*,*,#51830,.F.);
#73987=ORIENTED_EDGE('',*,*,#51831,.T.);
#73988=ORIENTED_EDGE('',*,*,#51832,.F.);
#73989=ORIENTED_EDGE('',*,*,#51833,.F.);
#73990=ORIENTED_EDGE('',*,*,#50108,.F.);
#73991=ORIENTED_EDGE('',*,*,#51834,.T.);
#73992=ORIENTED_EDGE('',*,*,#51825,.T.);
#73993=ORIENTED_EDGE('',*,*,#51831,.F.);
#73994=ORIENTED_EDGE('',*,*,#50107,.T.);
#73995=ORIENTED_EDGE('',*,*,#51835,.F.);
#73996=ORIENTED_EDGE('',*,*,#51822,.F.);
#73997=ORIENTED_EDGE('',*,*,#51834,.F.);
#73998=ORIENTED_EDGE('',*,*,#50106,.F.);
#73999=ORIENTED_EDGE('',*,*,#51835,.T.);
#74000=ORIENTED_EDGE('',*,*,#50791,.F.);
#74001=ORIENTED_EDGE('',*,*,#51836,.F.);
#74002=ORIENTED_EDGE('',*,*,#51818,.F.);
#74003=ORIENTED_EDGE('',*,*,#51836,.T.);
#74004=ORIENTED_EDGE('',*,*,#49842,.F.);
#74005=ORIENTED_EDGE('',*,*,#51837,.F.);
#74006=ORIENTED_EDGE('',*,*,#51819,.F.);
#74007=ORIENTED_EDGE('',*,*,#51837,.T.);
#74008=ORIENTED_EDGE('',*,*,#49841,.F.);
#74009=ORIENTED_EDGE('',*,*,#51838,.F.);
#74010=ORIENTED_EDGE('',*,*,#51823,.F.);
#74011=ORIENTED_EDGE('',*,*,#51838,.T.);
#74012=ORIENTED_EDGE('',*,*,#49840,.F.);
#74013=ORIENTED_EDGE('',*,*,#51839,.F.);
#74014=ORIENTED_EDGE('',*,*,#51814,.F.);
#74015=ORIENTED_EDGE('',*,*,#51840,.T.);
#74016=ORIENTED_EDGE('',*,*,#51815,.F.);
#74017=ORIENTED_EDGE('',*,*,#51839,.T.);
#74018=ORIENTED_EDGE('',*,*,#50790,.F.);
#74019=ORIENTED_EDGE('',*,*,#51841,.T.);
#74020=ORIENTED_EDGE('',*,*,#51816,.F.);
#74021=ORIENTED_EDGE('',*,*,#51840,.F.);
#74022=ORIENTED_EDGE('',*,*,#50110,.F.);
#74023=ORIENTED_EDGE('',*,*,#51833,.T.);
#74024=ORIENTED_EDGE('',*,*,#51829,.T.);
#74025=ORIENTED_EDGE('',*,*,#51841,.F.);
#74026=ORIENTED_EDGE('',*,*,#50109,.T.);
#74027=ORIENTED_EDGE('',*,*,#51827,.T.);
#74028=ORIENTED_EDGE('',*,*,#51830,.T.);
#74029=ORIENTED_EDGE('',*,*,#51832,.T.);
#74030=ORIENTED_EDGE('',*,*,#51842,.T.);
#74031=ORIENTED_EDGE('',*,*,#51843,.T.);
#74032=ORIENTED_EDGE('',*,*,#51844,.T.);
#74033=ORIENTED_EDGE('',*,*,#51845,.T.);
#74034=ORIENTED_EDGE('',*,*,#51846,.T.);
#74035=ORIENTED_EDGE('',*,*,#51847,.T.);
#74036=ORIENTED_EDGE('',*,*,#51848,.T.);
#74037=ORIENTED_EDGE('',*,*,#51849,.F.);
#74038=ORIENTED_EDGE('',*,*,#51850,.T.);
#74039=ORIENTED_EDGE('',*,*,#51851,.T.);
#74040=ORIENTED_EDGE('',*,*,#51849,.T.);
#74041=ORIENTED_EDGE('',*,*,#51852,.T.);
#74042=ORIENTED_EDGE('',*,*,#51842,.F.);
#74043=ORIENTED_EDGE('',*,*,#51853,.T.);
#74044=ORIENTED_EDGE('',*,*,#51854,.F.);
#74045=ORIENTED_EDGE('',*,*,#51850,.F.);
#74046=ORIENTED_EDGE('',*,*,#51855,.F.);
#74047=ORIENTED_EDGE('',*,*,#51856,.F.);
#74048=ORIENTED_EDGE('',*,*,#51855,.T.);
#74049=ORIENTED_EDGE('',*,*,#51853,.F.);
#74050=ORIENTED_EDGE('',*,*,#51857,.F.);
#74051=ORIENTED_EDGE('',*,*,#51857,.T.);
#74052=ORIENTED_EDGE('',*,*,#51846,.F.);
#74053=ORIENTED_EDGE('',*,*,#51858,.F.);
#74054=ORIENTED_EDGE('',*,*,#51859,.F.);
#74055=ORIENTED_EDGE('',*,*,#51860,.T.);
#74056=ORIENTED_EDGE('',*,*,#51861,.F.);
#74057=ORIENTED_EDGE('',*,*,#51862,.F.);
#74058=ORIENTED_EDGE('',*,*,#50114,.F.);
#74059=ORIENTED_EDGE('',*,*,#51863,.T.);
#74060=ORIENTED_EDGE('',*,*,#51854,.T.);
#74061=ORIENTED_EDGE('',*,*,#51860,.F.);
#74062=ORIENTED_EDGE('',*,*,#50113,.T.);
#74063=ORIENTED_EDGE('',*,*,#51864,.F.);
#74064=ORIENTED_EDGE('',*,*,#51851,.F.);
#74065=ORIENTED_EDGE('',*,*,#51863,.F.);
#74066=ORIENTED_EDGE('',*,*,#50112,.F.);
#74067=ORIENTED_EDGE('',*,*,#51864,.T.);
#74068=ORIENTED_EDGE('',*,*,#50789,.F.);
#74069=ORIENTED_EDGE('',*,*,#51865,.F.);
#74070=ORIENTED_EDGE('',*,*,#51847,.F.);
#74071=ORIENTED_EDGE('',*,*,#51865,.T.);
#74072=ORIENTED_EDGE('',*,*,#49838,.F.);
#74073=ORIENTED_EDGE('',*,*,#51866,.F.);
#74074=ORIENTED_EDGE('',*,*,#51848,.F.);
#74075=ORIENTED_EDGE('',*,*,#51866,.T.);
#74076=ORIENTED_EDGE('',*,*,#49837,.F.);
#74077=ORIENTED_EDGE('',*,*,#51867,.F.);
#74078=ORIENTED_EDGE('',*,*,#51852,.F.);
#74079=ORIENTED_EDGE('',*,*,#51867,.T.);
#74080=ORIENTED_EDGE('',*,*,#49836,.F.);
#74081=ORIENTED_EDGE('',*,*,#51868,.F.);
#74082=ORIENTED_EDGE('',*,*,#51843,.F.);
#74083=ORIENTED_EDGE('',*,*,#51869,.T.);
#74084=ORIENTED_EDGE('',*,*,#51844,.F.);
#74085=ORIENTED_EDGE('',*,*,#51868,.T.);
#74086=ORIENTED_EDGE('',*,*,#50662,.F.);
#74087=ORIENTED_EDGE('',*,*,#51870,.T.);
#74088=ORIENTED_EDGE('',*,*,#51845,.F.);
#74089=ORIENTED_EDGE('',*,*,#51869,.F.);
#74090=ORIENTED_EDGE('',*,*,#50116,.F.);
#74091=ORIENTED_EDGE('',*,*,#51862,.T.);
#74092=ORIENTED_EDGE('',*,*,#51858,.T.);
#74093=ORIENTED_EDGE('',*,*,#51870,.F.);
#74094=ORIENTED_EDGE('',*,*,#50115,.T.);
#74095=ORIENTED_EDGE('',*,*,#51856,.T.);
#74096=ORIENTED_EDGE('',*,*,#51859,.T.);
#74097=ORIENTED_EDGE('',*,*,#51861,.T.);
#74098=ORIENTED_EDGE('',*,*,#51871,.T.);
#74099=ORIENTED_EDGE('',*,*,#51872,.T.);
#74100=ORIENTED_EDGE('',*,*,#51873,.T.);
#74101=ORIENTED_EDGE('',*,*,#51874,.T.);
#74102=ORIENTED_EDGE('',*,*,#51875,.T.);
#74103=ORIENTED_EDGE('',*,*,#51876,.T.);
#74104=ORIENTED_EDGE('',*,*,#51877,.T.);
#74105=ORIENTED_EDGE('',*,*,#51878,.F.);
#74106=ORIENTED_EDGE('',*,*,#51879,.T.);
#74107=ORIENTED_EDGE('',*,*,#51880,.T.);
#74108=ORIENTED_EDGE('',*,*,#51878,.T.);
#74109=ORIENTED_EDGE('',*,*,#51881,.T.);
#74110=ORIENTED_EDGE('',*,*,#51871,.F.);
#74111=ORIENTED_EDGE('',*,*,#51882,.T.);
#74112=ORIENTED_EDGE('',*,*,#51883,.F.);
#74113=ORIENTED_EDGE('',*,*,#51879,.F.);
#74114=ORIENTED_EDGE('',*,*,#51884,.F.);
#74115=ORIENTED_EDGE('',*,*,#51885,.F.);
#74116=ORIENTED_EDGE('',*,*,#51884,.T.);
#74117=ORIENTED_EDGE('',*,*,#51882,.F.);
#74118=ORIENTED_EDGE('',*,*,#51886,.F.);
#74119=ORIENTED_EDGE('',*,*,#51886,.T.);
#74120=ORIENTED_EDGE('',*,*,#51875,.F.);
#74121=ORIENTED_EDGE('',*,*,#51887,.F.);
#74122=ORIENTED_EDGE('',*,*,#51888,.F.);
#74123=ORIENTED_EDGE('',*,*,#51889,.T.);
#74124=ORIENTED_EDGE('',*,*,#51890,.F.);
#74125=ORIENTED_EDGE('',*,*,#51891,.F.);
#74126=ORIENTED_EDGE('',*,*,#50500,.F.);
#74127=ORIENTED_EDGE('',*,*,#51892,.T.);
#74128=ORIENTED_EDGE('',*,*,#51883,.T.);
#74129=ORIENTED_EDGE('',*,*,#51889,.F.);
#74130=ORIENTED_EDGE('',*,*,#50499,.T.);
#74131=ORIENTED_EDGE('',*,*,#51893,.F.);
#74132=ORIENTED_EDGE('',*,*,#51880,.F.);
#74133=ORIENTED_EDGE('',*,*,#51892,.F.);
#74134=ORIENTED_EDGE('',*,*,#50498,.F.);
#74135=ORIENTED_EDGE('',*,*,#51893,.T.);
#74136=ORIENTED_EDGE('',*,*,#50788,.F.);
#74137=ORIENTED_EDGE('',*,*,#51894,.F.);
#74138=ORIENTED_EDGE('',*,*,#51876,.F.);
#74139=ORIENTED_EDGE('',*,*,#51894,.T.);
#74140=ORIENTED_EDGE('',*,*,#49978,.F.);
#74141=ORIENTED_EDGE('',*,*,#51895,.F.);
#74142=ORIENTED_EDGE('',*,*,#51877,.F.);
#74143=ORIENTED_EDGE('',*,*,#51895,.T.);
#74144=ORIENTED_EDGE('',*,*,#49977,.F.);
#74145=ORIENTED_EDGE('',*,*,#51896,.F.);
#74146=ORIENTED_EDGE('',*,*,#51881,.F.);
#74147=ORIENTED_EDGE('',*,*,#51896,.T.);
#74148=ORIENTED_EDGE('',*,*,#49976,.F.);
#74149=ORIENTED_EDGE('',*,*,#51897,.F.);
#74150=ORIENTED_EDGE('',*,*,#51872,.F.);
#74151=ORIENTED_EDGE('',*,*,#51898,.T.);
#74152=ORIENTED_EDGE('',*,*,#51873,.F.);
#74153=ORIENTED_EDGE('',*,*,#51897,.T.);
#74154=ORIENTED_EDGE('',*,*,#50851,.F.);
#74155=ORIENTED_EDGE('',*,*,#51899,.T.);
#74156=ORIENTED_EDGE('',*,*,#51874,.F.);
#74157=ORIENTED_EDGE('',*,*,#51898,.F.);
#74158=ORIENTED_EDGE('',*,*,#50502,.F.);
#74159=ORIENTED_EDGE('',*,*,#51891,.T.);
#74160=ORIENTED_EDGE('',*,*,#51887,.T.);
#74161=ORIENTED_EDGE('',*,*,#51899,.F.);
#74162=ORIENTED_EDGE('',*,*,#50501,.T.);
#74163=ORIENTED_EDGE('',*,*,#51885,.T.);
#74164=ORIENTED_EDGE('',*,*,#51888,.T.);
#74165=ORIENTED_EDGE('',*,*,#51890,.T.);
#74166=ORIENTED_EDGE('',*,*,#51900,.T.);
#74167=ORIENTED_EDGE('',*,*,#51901,.T.);
#74168=ORIENTED_EDGE('',*,*,#51902,.T.);
#74169=ORIENTED_EDGE('',*,*,#51903,.T.);
#74170=ORIENTED_EDGE('',*,*,#51904,.T.);
#74171=ORIENTED_EDGE('',*,*,#51905,.T.);
#74172=ORIENTED_EDGE('',*,*,#51906,.T.);
#74173=ORIENTED_EDGE('',*,*,#51907,.F.);
#74174=ORIENTED_EDGE('',*,*,#51908,.T.);
#74175=ORIENTED_EDGE('',*,*,#51909,.T.);
#74176=ORIENTED_EDGE('',*,*,#51907,.T.);
#74177=ORIENTED_EDGE('',*,*,#51910,.T.);
#74178=ORIENTED_EDGE('',*,*,#51900,.F.);
#74179=ORIENTED_EDGE('',*,*,#51911,.T.);
#74180=ORIENTED_EDGE('',*,*,#51912,.F.);
#74181=ORIENTED_EDGE('',*,*,#51908,.F.);
#74182=ORIENTED_EDGE('',*,*,#51913,.F.);
#74183=ORIENTED_EDGE('',*,*,#51914,.F.);
#74184=ORIENTED_EDGE('',*,*,#51913,.T.);
#74185=ORIENTED_EDGE('',*,*,#51911,.F.);
#74186=ORIENTED_EDGE('',*,*,#51915,.F.);
#74187=ORIENTED_EDGE('',*,*,#51915,.T.);
#74188=ORIENTED_EDGE('',*,*,#51904,.F.);
#74189=ORIENTED_EDGE('',*,*,#51916,.F.);
#74190=ORIENTED_EDGE('',*,*,#51917,.F.);
#74191=ORIENTED_EDGE('',*,*,#51918,.T.);
#74192=ORIENTED_EDGE('',*,*,#51919,.F.);
#74193=ORIENTED_EDGE('',*,*,#51920,.F.);
#74194=ORIENTED_EDGE('',*,*,#50494,.F.);
#74195=ORIENTED_EDGE('',*,*,#51921,.T.);
#74196=ORIENTED_EDGE('',*,*,#51912,.T.);
#74197=ORIENTED_EDGE('',*,*,#51918,.F.);
#74198=ORIENTED_EDGE('',*,*,#50493,.T.);
#74199=ORIENTED_EDGE('',*,*,#51922,.F.);
#74200=ORIENTED_EDGE('',*,*,#51909,.F.);
#74201=ORIENTED_EDGE('',*,*,#51921,.F.);
#74202=ORIENTED_EDGE('',*,*,#50492,.F.);
#74203=ORIENTED_EDGE('',*,*,#51922,.T.);
#74204=ORIENTED_EDGE('',*,*,#50786,.F.);
#74205=ORIENTED_EDGE('',*,*,#51923,.F.);
#74206=ORIENTED_EDGE('',*,*,#51905,.F.);
#74207=ORIENTED_EDGE('',*,*,#51923,.T.);
#74208=ORIENTED_EDGE('',*,*,#49982,.F.);
#74209=ORIENTED_EDGE('',*,*,#51924,.F.);
#74210=ORIENTED_EDGE('',*,*,#51906,.F.);
#74211=ORIENTED_EDGE('',*,*,#51924,.T.);
#74212=ORIENTED_EDGE('',*,*,#49981,.F.);
#74213=ORIENTED_EDGE('',*,*,#51925,.F.);
#74214=ORIENTED_EDGE('',*,*,#51910,.F.);
#74215=ORIENTED_EDGE('',*,*,#51925,.T.);
#74216=ORIENTED_EDGE('',*,*,#49980,.F.);
#74217=ORIENTED_EDGE('',*,*,#51926,.F.);
#74218=ORIENTED_EDGE('',*,*,#51901,.F.);
#74219=ORIENTED_EDGE('',*,*,#51927,.T.);
#74220=ORIENTED_EDGE('',*,*,#51902,.F.);
#74221=ORIENTED_EDGE('',*,*,#51926,.T.);
#74222=ORIENTED_EDGE('',*,*,#50787,.F.);
#74223=ORIENTED_EDGE('',*,*,#51928,.T.);
#74224=ORIENTED_EDGE('',*,*,#51903,.F.);
#74225=ORIENTED_EDGE('',*,*,#51927,.F.);
#74226=ORIENTED_EDGE('',*,*,#50496,.F.);
#74227=ORIENTED_EDGE('',*,*,#51920,.T.);
#74228=ORIENTED_EDGE('',*,*,#51916,.T.);
#74229=ORIENTED_EDGE('',*,*,#51928,.F.);
#74230=ORIENTED_EDGE('',*,*,#50495,.T.);
#74231=ORIENTED_EDGE('',*,*,#51914,.T.);
#74232=ORIENTED_EDGE('',*,*,#51917,.T.);
#74233=ORIENTED_EDGE('',*,*,#51919,.T.);
#74234=ORIENTED_EDGE('',*,*,#51929,.T.);
#74235=ORIENTED_EDGE('',*,*,#51930,.T.);
#74236=ORIENTED_EDGE('',*,*,#51931,.T.);
#74237=ORIENTED_EDGE('',*,*,#51932,.T.);
#74238=ORIENTED_EDGE('',*,*,#51933,.T.);
#74239=ORIENTED_EDGE('',*,*,#51934,.T.);
#74240=ORIENTED_EDGE('',*,*,#51935,.T.);
#74241=ORIENTED_EDGE('',*,*,#51936,.F.);
#74242=ORIENTED_EDGE('',*,*,#51937,.T.);
#74243=ORIENTED_EDGE('',*,*,#51938,.T.);
#74244=ORIENTED_EDGE('',*,*,#51936,.T.);
#74245=ORIENTED_EDGE('',*,*,#51939,.T.);
#74246=ORIENTED_EDGE('',*,*,#51929,.F.);
#74247=ORIENTED_EDGE('',*,*,#51940,.T.);
#74248=ORIENTED_EDGE('',*,*,#51941,.F.);
#74249=ORIENTED_EDGE('',*,*,#51937,.F.);
#74250=ORIENTED_EDGE('',*,*,#51942,.F.);
#74251=ORIENTED_EDGE('',*,*,#51943,.F.);
#74252=ORIENTED_EDGE('',*,*,#51942,.T.);
#74253=ORIENTED_EDGE('',*,*,#51940,.F.);
#74254=ORIENTED_EDGE('',*,*,#51944,.F.);
#74255=ORIENTED_EDGE('',*,*,#51944,.T.);
#74256=ORIENTED_EDGE('',*,*,#51933,.F.);
#74257=ORIENTED_EDGE('',*,*,#51945,.F.);
#74258=ORIENTED_EDGE('',*,*,#51946,.F.);
#74259=ORIENTED_EDGE('',*,*,#51947,.T.);
#74260=ORIENTED_EDGE('',*,*,#51948,.F.);
#74261=ORIENTED_EDGE('',*,*,#51949,.F.);
#74262=ORIENTED_EDGE('',*,*,#50488,.F.);
#74263=ORIENTED_EDGE('',*,*,#51950,.T.);
#74264=ORIENTED_EDGE('',*,*,#51941,.T.);
#74265=ORIENTED_EDGE('',*,*,#51947,.F.);
#74266=ORIENTED_EDGE('',*,*,#50487,.T.);
#74267=ORIENTED_EDGE('',*,*,#51951,.F.);
#74268=ORIENTED_EDGE('',*,*,#51938,.F.);
#74269=ORIENTED_EDGE('',*,*,#51950,.F.);
#74270=ORIENTED_EDGE('',*,*,#50486,.F.);
#74271=ORIENTED_EDGE('',*,*,#51951,.T.);
#74272=ORIENTED_EDGE('',*,*,#50784,.F.);
#74273=ORIENTED_EDGE('',*,*,#51952,.F.);
#74274=ORIENTED_EDGE('',*,*,#51934,.F.);
#74275=ORIENTED_EDGE('',*,*,#51952,.T.);
#74276=ORIENTED_EDGE('',*,*,#49986,.F.);
#74277=ORIENTED_EDGE('',*,*,#51953,.F.);
#74278=ORIENTED_EDGE('',*,*,#51935,.F.);
#74279=ORIENTED_EDGE('',*,*,#51953,.T.);
#74280=ORIENTED_EDGE('',*,*,#49985,.F.);
#74281=ORIENTED_EDGE('',*,*,#51954,.F.);
#74282=ORIENTED_EDGE('',*,*,#51939,.F.);
#74283=ORIENTED_EDGE('',*,*,#51954,.T.);
#74284=ORIENTED_EDGE('',*,*,#49984,.F.);
#74285=ORIENTED_EDGE('',*,*,#51955,.F.);
#74286=ORIENTED_EDGE('',*,*,#51930,.F.);
#74287=ORIENTED_EDGE('',*,*,#51956,.T.);
#74288=ORIENTED_EDGE('',*,*,#51931,.F.);
#74289=ORIENTED_EDGE('',*,*,#51955,.T.);
#74290=ORIENTED_EDGE('',*,*,#50785,.F.);
#74291=ORIENTED_EDGE('',*,*,#51957,.T.);
#74292=ORIENTED_EDGE('',*,*,#51932,.F.);
#74293=ORIENTED_EDGE('',*,*,#51956,.F.);
#74294=ORIENTED_EDGE('',*,*,#50490,.F.);
#74295=ORIENTED_EDGE('',*,*,#51949,.T.);
#74296=ORIENTED_EDGE('',*,*,#51945,.T.);
#74297=ORIENTED_EDGE('',*,*,#51957,.F.);
#74298=ORIENTED_EDGE('',*,*,#50489,.T.);
#74299=ORIENTED_EDGE('',*,*,#51943,.T.);
#74300=ORIENTED_EDGE('',*,*,#51946,.T.);
#74301=ORIENTED_EDGE('',*,*,#51948,.T.);
#74302=ORIENTED_EDGE('',*,*,#51958,.T.);
#74303=ORIENTED_EDGE('',*,*,#51959,.T.);
#74304=ORIENTED_EDGE('',*,*,#51960,.T.);
#74305=ORIENTED_EDGE('',*,*,#51961,.T.);
#74306=ORIENTED_EDGE('',*,*,#51962,.T.);
#74307=ORIENTED_EDGE('',*,*,#51963,.T.);
#74308=ORIENTED_EDGE('',*,*,#51964,.T.);
#74309=ORIENTED_EDGE('',*,*,#51965,.F.);
#74310=ORIENTED_EDGE('',*,*,#51966,.T.);
#74311=ORIENTED_EDGE('',*,*,#51967,.T.);
#74312=ORIENTED_EDGE('',*,*,#51965,.T.);
#74313=ORIENTED_EDGE('',*,*,#51968,.T.);
#74314=ORIENTED_EDGE('',*,*,#51958,.F.);
#74315=ORIENTED_EDGE('',*,*,#51969,.T.);
#74316=ORIENTED_EDGE('',*,*,#51970,.F.);
#74317=ORIENTED_EDGE('',*,*,#51966,.F.);
#74318=ORIENTED_EDGE('',*,*,#51971,.F.);
#74319=ORIENTED_EDGE('',*,*,#51972,.F.);
#74320=ORIENTED_EDGE('',*,*,#51971,.T.);
#74321=ORIENTED_EDGE('',*,*,#51969,.F.);
#74322=ORIENTED_EDGE('',*,*,#51973,.F.);
#74323=ORIENTED_EDGE('',*,*,#51973,.T.);
#74324=ORIENTED_EDGE('',*,*,#51962,.F.);
#74325=ORIENTED_EDGE('',*,*,#51974,.F.);
#74326=ORIENTED_EDGE('',*,*,#51975,.F.);
#74327=ORIENTED_EDGE('',*,*,#51976,.T.);
#74328=ORIENTED_EDGE('',*,*,#51977,.F.);
#74329=ORIENTED_EDGE('',*,*,#51978,.F.);
#74330=ORIENTED_EDGE('',*,*,#50482,.F.);
#74331=ORIENTED_EDGE('',*,*,#51979,.T.);
#74332=ORIENTED_EDGE('',*,*,#51970,.T.);
#74333=ORIENTED_EDGE('',*,*,#51976,.F.);
#74334=ORIENTED_EDGE('',*,*,#50481,.T.);
#74335=ORIENTED_EDGE('',*,*,#51980,.F.);
#74336=ORIENTED_EDGE('',*,*,#51967,.F.);
#74337=ORIENTED_EDGE('',*,*,#51979,.F.);
#74338=ORIENTED_EDGE('',*,*,#50480,.F.);
#74339=ORIENTED_EDGE('',*,*,#51980,.T.);
#74340=ORIENTED_EDGE('',*,*,#50782,.F.);
#74341=ORIENTED_EDGE('',*,*,#51981,.F.);
#74342=ORIENTED_EDGE('',*,*,#51963,.F.);
#74343=ORIENTED_EDGE('',*,*,#51981,.T.);
#74344=ORIENTED_EDGE('',*,*,#49990,.F.);
#74345=ORIENTED_EDGE('',*,*,#51982,.F.);
#74346=ORIENTED_EDGE('',*,*,#51964,.F.);
#74347=ORIENTED_EDGE('',*,*,#51982,.T.);
#74348=ORIENTED_EDGE('',*,*,#49989,.F.);
#74349=ORIENTED_EDGE('',*,*,#51983,.F.);
#74350=ORIENTED_EDGE('',*,*,#51968,.F.);
#74351=ORIENTED_EDGE('',*,*,#51983,.T.);
#74352=ORIENTED_EDGE('',*,*,#49988,.F.);
#74353=ORIENTED_EDGE('',*,*,#51984,.F.);
#74354=ORIENTED_EDGE('',*,*,#51959,.F.);
#74355=ORIENTED_EDGE('',*,*,#51985,.T.);
#74356=ORIENTED_EDGE('',*,*,#51960,.F.);
#74357=ORIENTED_EDGE('',*,*,#51984,.T.);
#74358=ORIENTED_EDGE('',*,*,#50783,.F.);
#74359=ORIENTED_EDGE('',*,*,#51986,.T.);
#74360=ORIENTED_EDGE('',*,*,#51961,.F.);
#74361=ORIENTED_EDGE('',*,*,#51985,.F.);
#74362=ORIENTED_EDGE('',*,*,#50484,.F.);
#74363=ORIENTED_EDGE('',*,*,#51978,.T.);
#74364=ORIENTED_EDGE('',*,*,#51974,.T.);
#74365=ORIENTED_EDGE('',*,*,#51986,.F.);
#74366=ORIENTED_EDGE('',*,*,#50483,.T.);
#74367=ORIENTED_EDGE('',*,*,#51972,.T.);
#74368=ORIENTED_EDGE('',*,*,#51975,.T.);
#74369=ORIENTED_EDGE('',*,*,#51977,.T.);
#74370=ORIENTED_EDGE('',*,*,#51987,.T.);
#74371=ORIENTED_EDGE('',*,*,#51988,.T.);
#74372=ORIENTED_EDGE('',*,*,#51989,.T.);
#74373=ORIENTED_EDGE('',*,*,#51990,.T.);
#74374=ORIENTED_EDGE('',*,*,#51991,.T.);
#74375=ORIENTED_EDGE('',*,*,#51992,.T.);
#74376=ORIENTED_EDGE('',*,*,#51993,.T.);
#74377=ORIENTED_EDGE('',*,*,#51994,.F.);
#74378=ORIENTED_EDGE('',*,*,#51995,.T.);
#74379=ORIENTED_EDGE('',*,*,#51996,.T.);
#74380=ORIENTED_EDGE('',*,*,#51994,.T.);
#74381=ORIENTED_EDGE('',*,*,#51997,.T.);
#74382=ORIENTED_EDGE('',*,*,#51987,.F.);
#74383=ORIENTED_EDGE('',*,*,#51998,.T.);
#74384=ORIENTED_EDGE('',*,*,#51999,.F.);
#74385=ORIENTED_EDGE('',*,*,#51995,.F.);
#74386=ORIENTED_EDGE('',*,*,#52000,.F.);
#74387=ORIENTED_EDGE('',*,*,#52001,.F.);
#74388=ORIENTED_EDGE('',*,*,#52000,.T.);
#74389=ORIENTED_EDGE('',*,*,#51998,.F.);
#74390=ORIENTED_EDGE('',*,*,#52002,.F.);
#74391=ORIENTED_EDGE('',*,*,#52002,.T.);
#74392=ORIENTED_EDGE('',*,*,#51991,.F.);
#74393=ORIENTED_EDGE('',*,*,#52003,.F.);
#74394=ORIENTED_EDGE('',*,*,#52004,.F.);
#74395=ORIENTED_EDGE('',*,*,#52005,.T.);
#74396=ORIENTED_EDGE('',*,*,#52006,.F.);
#74397=ORIENTED_EDGE('',*,*,#52007,.F.);
#74398=ORIENTED_EDGE('',*,*,#50476,.F.);
#74399=ORIENTED_EDGE('',*,*,#52008,.T.);
#74400=ORIENTED_EDGE('',*,*,#51999,.T.);
#74401=ORIENTED_EDGE('',*,*,#52005,.F.);
#74402=ORIENTED_EDGE('',*,*,#50475,.T.);
#74403=ORIENTED_EDGE('',*,*,#52009,.F.);
#74404=ORIENTED_EDGE('',*,*,#51996,.F.);
#74405=ORIENTED_EDGE('',*,*,#52008,.F.);
#74406=ORIENTED_EDGE('',*,*,#50474,.F.);
#74407=ORIENTED_EDGE('',*,*,#52009,.T.);
#74408=ORIENTED_EDGE('',*,*,#50780,.F.);
#74409=ORIENTED_EDGE('',*,*,#52010,.F.);
#74410=ORIENTED_EDGE('',*,*,#51992,.F.);
#74411=ORIENTED_EDGE('',*,*,#52010,.T.);
#74412=ORIENTED_EDGE('',*,*,#49994,.F.);
#74413=ORIENTED_EDGE('',*,*,#52011,.F.);
#74414=ORIENTED_EDGE('',*,*,#51993,.F.);
#74415=ORIENTED_EDGE('',*,*,#52011,.T.);
#74416=ORIENTED_EDGE('',*,*,#49993,.F.);
#74417=ORIENTED_EDGE('',*,*,#52012,.F.);
#74418=ORIENTED_EDGE('',*,*,#51997,.F.);
#74419=ORIENTED_EDGE('',*,*,#52012,.T.);
#74420=ORIENTED_EDGE('',*,*,#49992,.F.);
#74421=ORIENTED_EDGE('',*,*,#52013,.F.);
#74422=ORIENTED_EDGE('',*,*,#51988,.F.);
#74423=ORIENTED_EDGE('',*,*,#52014,.T.);
#74424=ORIENTED_EDGE('',*,*,#51989,.F.);
#74425=ORIENTED_EDGE('',*,*,#52013,.T.);
#74426=ORIENTED_EDGE('',*,*,#50781,.F.);
#74427=ORIENTED_EDGE('',*,*,#52015,.T.);
#74428=ORIENTED_EDGE('',*,*,#51990,.F.);
#74429=ORIENTED_EDGE('',*,*,#52014,.F.);
#74430=ORIENTED_EDGE('',*,*,#50478,.F.);
#74431=ORIENTED_EDGE('',*,*,#52007,.T.);
#74432=ORIENTED_EDGE('',*,*,#52003,.T.);
#74433=ORIENTED_EDGE('',*,*,#52015,.F.);
#74434=ORIENTED_EDGE('',*,*,#50477,.T.);
#74435=ORIENTED_EDGE('',*,*,#52001,.T.);
#74436=ORIENTED_EDGE('',*,*,#52004,.T.);
#74437=ORIENTED_EDGE('',*,*,#52006,.T.);
#74438=ORIENTED_EDGE('',*,*,#52016,.T.);
#74439=ORIENTED_EDGE('',*,*,#52017,.T.);
#74440=ORIENTED_EDGE('',*,*,#52018,.T.);
#74441=ORIENTED_EDGE('',*,*,#52019,.T.);
#74442=ORIENTED_EDGE('',*,*,#52020,.T.);
#74443=ORIENTED_EDGE('',*,*,#52021,.T.);
#74444=ORIENTED_EDGE('',*,*,#52022,.T.);
#74445=ORIENTED_EDGE('',*,*,#52023,.F.);
#74446=ORIENTED_EDGE('',*,*,#52024,.T.);
#74447=ORIENTED_EDGE('',*,*,#52025,.T.);
#74448=ORIENTED_EDGE('',*,*,#52023,.T.);
#74449=ORIENTED_EDGE('',*,*,#52026,.T.);
#74450=ORIENTED_EDGE('',*,*,#52016,.F.);
#74451=ORIENTED_EDGE('',*,*,#52027,.T.);
#74452=ORIENTED_EDGE('',*,*,#52028,.F.);
#74453=ORIENTED_EDGE('',*,*,#52024,.F.);
#74454=ORIENTED_EDGE('',*,*,#52029,.F.);
#74455=ORIENTED_EDGE('',*,*,#52030,.F.);
#74456=ORIENTED_EDGE('',*,*,#52029,.T.);
#74457=ORIENTED_EDGE('',*,*,#52027,.F.);
#74458=ORIENTED_EDGE('',*,*,#52031,.F.);
#74459=ORIENTED_EDGE('',*,*,#52031,.T.);
#74460=ORIENTED_EDGE('',*,*,#52020,.F.);
#74461=ORIENTED_EDGE('',*,*,#52032,.F.);
#74462=ORIENTED_EDGE('',*,*,#52033,.F.);
#74463=ORIENTED_EDGE('',*,*,#52034,.T.);
#74464=ORIENTED_EDGE('',*,*,#52035,.F.);
#74465=ORIENTED_EDGE('',*,*,#52036,.F.);
#74466=ORIENTED_EDGE('',*,*,#50470,.F.);
#74467=ORIENTED_EDGE('',*,*,#52037,.T.);
#74468=ORIENTED_EDGE('',*,*,#52028,.T.);
#74469=ORIENTED_EDGE('',*,*,#52034,.F.);
#74470=ORIENTED_EDGE('',*,*,#50469,.T.);
#74471=ORIENTED_EDGE('',*,*,#52038,.F.);
#74472=ORIENTED_EDGE('',*,*,#52025,.F.);
#74473=ORIENTED_EDGE('',*,*,#52037,.F.);
#74474=ORIENTED_EDGE('',*,*,#50468,.F.);
#74475=ORIENTED_EDGE('',*,*,#52038,.T.);
#74476=ORIENTED_EDGE('',*,*,#50778,.F.);
#74477=ORIENTED_EDGE('',*,*,#52039,.F.);
#74478=ORIENTED_EDGE('',*,*,#52021,.F.);
#74479=ORIENTED_EDGE('',*,*,#52039,.T.);
#74480=ORIENTED_EDGE('',*,*,#49998,.F.);
#74481=ORIENTED_EDGE('',*,*,#52040,.F.);
#74482=ORIENTED_EDGE('',*,*,#52022,.F.);
#74483=ORIENTED_EDGE('',*,*,#52040,.T.);
#74484=ORIENTED_EDGE('',*,*,#49997,.F.);
#74485=ORIENTED_EDGE('',*,*,#52041,.F.);
#74486=ORIENTED_EDGE('',*,*,#52026,.F.);
#74487=ORIENTED_EDGE('',*,*,#52041,.T.);
#74488=ORIENTED_EDGE('',*,*,#49996,.F.);
#74489=ORIENTED_EDGE('',*,*,#52042,.F.);
#74490=ORIENTED_EDGE('',*,*,#52017,.F.);
#74491=ORIENTED_EDGE('',*,*,#52043,.T.);
#74492=ORIENTED_EDGE('',*,*,#52018,.F.);
#74493=ORIENTED_EDGE('',*,*,#52042,.T.);
#74494=ORIENTED_EDGE('',*,*,#50779,.F.);
#74495=ORIENTED_EDGE('',*,*,#52044,.T.);
#74496=ORIENTED_EDGE('',*,*,#52019,.F.);
#74497=ORIENTED_EDGE('',*,*,#52043,.F.);
#74498=ORIENTED_EDGE('',*,*,#50472,.F.);
#74499=ORIENTED_EDGE('',*,*,#52036,.T.);
#74500=ORIENTED_EDGE('',*,*,#52032,.T.);
#74501=ORIENTED_EDGE('',*,*,#52044,.F.);
#74502=ORIENTED_EDGE('',*,*,#50471,.T.);
#74503=ORIENTED_EDGE('',*,*,#52030,.T.);
#74504=ORIENTED_EDGE('',*,*,#52033,.T.);
#74505=ORIENTED_EDGE('',*,*,#52035,.T.);
#74506=ORIENTED_EDGE('',*,*,#52045,.T.);
#74507=ORIENTED_EDGE('',*,*,#52046,.T.);
#74508=ORIENTED_EDGE('',*,*,#52047,.T.);
#74509=ORIENTED_EDGE('',*,*,#52048,.T.);
#74510=ORIENTED_EDGE('',*,*,#52049,.T.);
#74511=ORIENTED_EDGE('',*,*,#52050,.T.);
#74512=ORIENTED_EDGE('',*,*,#52051,.T.);
#74513=ORIENTED_EDGE('',*,*,#52052,.F.);
#74514=ORIENTED_EDGE('',*,*,#52053,.T.);
#74515=ORIENTED_EDGE('',*,*,#52054,.T.);
#74516=ORIENTED_EDGE('',*,*,#52052,.T.);
#74517=ORIENTED_EDGE('',*,*,#52055,.T.);
#74518=ORIENTED_EDGE('',*,*,#52045,.F.);
#74519=ORIENTED_EDGE('',*,*,#52056,.T.);
#74520=ORIENTED_EDGE('',*,*,#52057,.F.);
#74521=ORIENTED_EDGE('',*,*,#52053,.F.);
#74522=ORIENTED_EDGE('',*,*,#52058,.F.);
#74523=ORIENTED_EDGE('',*,*,#52059,.F.);
#74524=ORIENTED_EDGE('',*,*,#52058,.T.);
#74525=ORIENTED_EDGE('',*,*,#52056,.F.);
#74526=ORIENTED_EDGE('',*,*,#52060,.F.);
#74527=ORIENTED_EDGE('',*,*,#52060,.T.);
#74528=ORIENTED_EDGE('',*,*,#52049,.F.);
#74529=ORIENTED_EDGE('',*,*,#52061,.F.);
#74530=ORIENTED_EDGE('',*,*,#52062,.F.);
#74531=ORIENTED_EDGE('',*,*,#52063,.T.);
#74532=ORIENTED_EDGE('',*,*,#52064,.F.);
#74533=ORIENTED_EDGE('',*,*,#52065,.F.);
#74534=ORIENTED_EDGE('',*,*,#50464,.F.);
#74535=ORIENTED_EDGE('',*,*,#52066,.T.);
#74536=ORIENTED_EDGE('',*,*,#52057,.T.);
#74537=ORIENTED_EDGE('',*,*,#52063,.F.);
#74538=ORIENTED_EDGE('',*,*,#50463,.T.);
#74539=ORIENTED_EDGE('',*,*,#52067,.F.);
#74540=ORIENTED_EDGE('',*,*,#52054,.F.);
#74541=ORIENTED_EDGE('',*,*,#52066,.F.);
#74542=ORIENTED_EDGE('',*,*,#50462,.F.);
#74543=ORIENTED_EDGE('',*,*,#52067,.T.);
#74544=ORIENTED_EDGE('',*,*,#50776,.F.);
#74545=ORIENTED_EDGE('',*,*,#52068,.F.);
#74546=ORIENTED_EDGE('',*,*,#52050,.F.);
#74547=ORIENTED_EDGE('',*,*,#52068,.T.);
#74548=ORIENTED_EDGE('',*,*,#50002,.F.);
#74549=ORIENTED_EDGE('',*,*,#52069,.F.);
#74550=ORIENTED_EDGE('',*,*,#52051,.F.);
#74551=ORIENTED_EDGE('',*,*,#52069,.T.);
#74552=ORIENTED_EDGE('',*,*,#50001,.F.);
#74553=ORIENTED_EDGE('',*,*,#52070,.F.);
#74554=ORIENTED_EDGE('',*,*,#52055,.F.);
#74555=ORIENTED_EDGE('',*,*,#52070,.T.);
#74556=ORIENTED_EDGE('',*,*,#50000,.F.);
#74557=ORIENTED_EDGE('',*,*,#52071,.F.);
#74558=ORIENTED_EDGE('',*,*,#52046,.F.);
#74559=ORIENTED_EDGE('',*,*,#52072,.T.);
#74560=ORIENTED_EDGE('',*,*,#52047,.F.);
#74561=ORIENTED_EDGE('',*,*,#52071,.T.);
#74562=ORIENTED_EDGE('',*,*,#50777,.F.);
#74563=ORIENTED_EDGE('',*,*,#52073,.T.);
#74564=ORIENTED_EDGE('',*,*,#52048,.F.);
#74565=ORIENTED_EDGE('',*,*,#52072,.F.);
#74566=ORIENTED_EDGE('',*,*,#50466,.F.);
#74567=ORIENTED_EDGE('',*,*,#52065,.T.);
#74568=ORIENTED_EDGE('',*,*,#52061,.T.);
#74569=ORIENTED_EDGE('',*,*,#52073,.F.);
#74570=ORIENTED_EDGE('',*,*,#50465,.T.);
#74571=ORIENTED_EDGE('',*,*,#52059,.T.);
#74572=ORIENTED_EDGE('',*,*,#52062,.T.);
#74573=ORIENTED_EDGE('',*,*,#52064,.T.);
#74574=ORIENTED_EDGE('',*,*,#52074,.T.);
#74575=ORIENTED_EDGE('',*,*,#52075,.T.);
#74576=ORIENTED_EDGE('',*,*,#52076,.T.);
#74577=ORIENTED_EDGE('',*,*,#52077,.T.);
#74578=ORIENTED_EDGE('',*,*,#52078,.T.);
#74579=ORIENTED_EDGE('',*,*,#52079,.T.);
#74580=ORIENTED_EDGE('',*,*,#52080,.T.);
#74581=ORIENTED_EDGE('',*,*,#52081,.F.);
#74582=ORIENTED_EDGE('',*,*,#52082,.T.);
#74583=ORIENTED_EDGE('',*,*,#52083,.T.);
#74584=ORIENTED_EDGE('',*,*,#52081,.T.);
#74585=ORIENTED_EDGE('',*,*,#52084,.T.);
#74586=ORIENTED_EDGE('',*,*,#52074,.F.);
#74587=ORIENTED_EDGE('',*,*,#52085,.T.);
#74588=ORIENTED_EDGE('',*,*,#52086,.F.);
#74589=ORIENTED_EDGE('',*,*,#52082,.F.);
#74590=ORIENTED_EDGE('',*,*,#52087,.F.);
#74591=ORIENTED_EDGE('',*,*,#52088,.F.);
#74592=ORIENTED_EDGE('',*,*,#52087,.T.);
#74593=ORIENTED_EDGE('',*,*,#52085,.F.);
#74594=ORIENTED_EDGE('',*,*,#52089,.F.);
#74595=ORIENTED_EDGE('',*,*,#52089,.T.);
#74596=ORIENTED_EDGE('',*,*,#52078,.F.);
#74597=ORIENTED_EDGE('',*,*,#52090,.F.);
#74598=ORIENTED_EDGE('',*,*,#52091,.F.);
#74599=ORIENTED_EDGE('',*,*,#52092,.T.);
#74600=ORIENTED_EDGE('',*,*,#52093,.F.);
#74601=ORIENTED_EDGE('',*,*,#52094,.F.);
#74602=ORIENTED_EDGE('',*,*,#50458,.F.);
#74603=ORIENTED_EDGE('',*,*,#52095,.T.);
#74604=ORIENTED_EDGE('',*,*,#52086,.T.);
#74605=ORIENTED_EDGE('',*,*,#52092,.F.);
#74606=ORIENTED_EDGE('',*,*,#50457,.T.);
#74607=ORIENTED_EDGE('',*,*,#52096,.F.);
#74608=ORIENTED_EDGE('',*,*,#52083,.F.);
#74609=ORIENTED_EDGE('',*,*,#52095,.F.);
#74610=ORIENTED_EDGE('',*,*,#50456,.F.);
#74611=ORIENTED_EDGE('',*,*,#52096,.T.);
#74612=ORIENTED_EDGE('',*,*,#50774,.F.);
#74613=ORIENTED_EDGE('',*,*,#52097,.F.);
#74614=ORIENTED_EDGE('',*,*,#52079,.F.);
#74615=ORIENTED_EDGE('',*,*,#52097,.T.);
#74616=ORIENTED_EDGE('',*,*,#50006,.F.);
#74617=ORIENTED_EDGE('',*,*,#52098,.F.);
#74618=ORIENTED_EDGE('',*,*,#52080,.F.);
#74619=ORIENTED_EDGE('',*,*,#52098,.T.);
#74620=ORIENTED_EDGE('',*,*,#50005,.F.);
#74621=ORIENTED_EDGE('',*,*,#52099,.F.);
#74622=ORIENTED_EDGE('',*,*,#52084,.F.);
#74623=ORIENTED_EDGE('',*,*,#52099,.T.);
#74624=ORIENTED_EDGE('',*,*,#50004,.F.);
#74625=ORIENTED_EDGE('',*,*,#52100,.F.);
#74626=ORIENTED_EDGE('',*,*,#52075,.F.);
#74627=ORIENTED_EDGE('',*,*,#52101,.T.);
#74628=ORIENTED_EDGE('',*,*,#52076,.F.);
#74629=ORIENTED_EDGE('',*,*,#52100,.T.);
#74630=ORIENTED_EDGE('',*,*,#50775,.F.);
#74631=ORIENTED_EDGE('',*,*,#52102,.T.);
#74632=ORIENTED_EDGE('',*,*,#52077,.F.);
#74633=ORIENTED_EDGE('',*,*,#52101,.F.);
#74634=ORIENTED_EDGE('',*,*,#50460,.F.);
#74635=ORIENTED_EDGE('',*,*,#52094,.T.);
#74636=ORIENTED_EDGE('',*,*,#52090,.T.);
#74637=ORIENTED_EDGE('',*,*,#52102,.F.);
#74638=ORIENTED_EDGE('',*,*,#50459,.T.);
#74639=ORIENTED_EDGE('',*,*,#52088,.T.);
#74640=ORIENTED_EDGE('',*,*,#52091,.T.);
#74641=ORIENTED_EDGE('',*,*,#52093,.T.);
#74642=ORIENTED_EDGE('',*,*,#52103,.T.);
#74643=ORIENTED_EDGE('',*,*,#52104,.T.);
#74644=ORIENTED_EDGE('',*,*,#52105,.T.);
#74645=ORIENTED_EDGE('',*,*,#52106,.T.);
#74646=ORIENTED_EDGE('',*,*,#52107,.T.);
#74647=ORIENTED_EDGE('',*,*,#52108,.T.);
#74648=ORIENTED_EDGE('',*,*,#52109,.T.);
#74649=ORIENTED_EDGE('',*,*,#52110,.F.);
#74650=ORIENTED_EDGE('',*,*,#52111,.T.);
#74651=ORIENTED_EDGE('',*,*,#52112,.T.);
#74652=ORIENTED_EDGE('',*,*,#52110,.T.);
#74653=ORIENTED_EDGE('',*,*,#52113,.T.);
#74654=ORIENTED_EDGE('',*,*,#52103,.F.);
#74655=ORIENTED_EDGE('',*,*,#52114,.T.);
#74656=ORIENTED_EDGE('',*,*,#52115,.F.);
#74657=ORIENTED_EDGE('',*,*,#52111,.F.);
#74658=ORIENTED_EDGE('',*,*,#52116,.F.);
#74659=ORIENTED_EDGE('',*,*,#52117,.F.);
#74660=ORIENTED_EDGE('',*,*,#52116,.T.);
#74661=ORIENTED_EDGE('',*,*,#52114,.F.);
#74662=ORIENTED_EDGE('',*,*,#52118,.F.);
#74663=ORIENTED_EDGE('',*,*,#52118,.T.);
#74664=ORIENTED_EDGE('',*,*,#52107,.F.);
#74665=ORIENTED_EDGE('',*,*,#52119,.F.);
#74666=ORIENTED_EDGE('',*,*,#52120,.F.);
#74667=ORIENTED_EDGE('',*,*,#52121,.T.);
#74668=ORIENTED_EDGE('',*,*,#52122,.F.);
#74669=ORIENTED_EDGE('',*,*,#52123,.F.);
#74670=ORIENTED_EDGE('',*,*,#50452,.F.);
#74671=ORIENTED_EDGE('',*,*,#52124,.T.);
#74672=ORIENTED_EDGE('',*,*,#52115,.T.);
#74673=ORIENTED_EDGE('',*,*,#52121,.F.);
#74674=ORIENTED_EDGE('',*,*,#50451,.T.);
#74675=ORIENTED_EDGE('',*,*,#52125,.F.);
#74676=ORIENTED_EDGE('',*,*,#52112,.F.);
#74677=ORIENTED_EDGE('',*,*,#52124,.F.);
#74678=ORIENTED_EDGE('',*,*,#50450,.F.);
#74679=ORIENTED_EDGE('',*,*,#52125,.T.);
#74680=ORIENTED_EDGE('',*,*,#50772,.F.);
#74681=ORIENTED_EDGE('',*,*,#52126,.F.);
#74682=ORIENTED_EDGE('',*,*,#52108,.F.);
#74683=ORIENTED_EDGE('',*,*,#52126,.T.);
#74684=ORIENTED_EDGE('',*,*,#50010,.F.);
#74685=ORIENTED_EDGE('',*,*,#52127,.F.);
#74686=ORIENTED_EDGE('',*,*,#52109,.F.);
#74687=ORIENTED_EDGE('',*,*,#52127,.T.);
#74688=ORIENTED_EDGE('',*,*,#50009,.F.);
#74689=ORIENTED_EDGE('',*,*,#52128,.F.);
#74690=ORIENTED_EDGE('',*,*,#52113,.F.);
#74691=ORIENTED_EDGE('',*,*,#52128,.T.);
#74692=ORIENTED_EDGE('',*,*,#50008,.F.);
#74693=ORIENTED_EDGE('',*,*,#52129,.F.);
#74694=ORIENTED_EDGE('',*,*,#52104,.F.);
#74695=ORIENTED_EDGE('',*,*,#52130,.T.);
#74696=ORIENTED_EDGE('',*,*,#52105,.F.);
#74697=ORIENTED_EDGE('',*,*,#52129,.T.);
#74698=ORIENTED_EDGE('',*,*,#50773,.F.);
#74699=ORIENTED_EDGE('',*,*,#52131,.T.);
#74700=ORIENTED_EDGE('',*,*,#52106,.F.);
#74701=ORIENTED_EDGE('',*,*,#52130,.F.);
#74702=ORIENTED_EDGE('',*,*,#50454,.F.);
#74703=ORIENTED_EDGE('',*,*,#52123,.T.);
#74704=ORIENTED_EDGE('',*,*,#52119,.T.);
#74705=ORIENTED_EDGE('',*,*,#52131,.F.);
#74706=ORIENTED_EDGE('',*,*,#50453,.T.);
#74707=ORIENTED_EDGE('',*,*,#52117,.T.);
#74708=ORIENTED_EDGE('',*,*,#52120,.T.);
#74709=ORIENTED_EDGE('',*,*,#52122,.T.);
#74710=ORIENTED_EDGE('',*,*,#52132,.T.);
#74711=ORIENTED_EDGE('',*,*,#52133,.T.);
#74712=ORIENTED_EDGE('',*,*,#52134,.T.);
#74713=ORIENTED_EDGE('',*,*,#52135,.T.);
#74714=ORIENTED_EDGE('',*,*,#52136,.T.);
#74715=ORIENTED_EDGE('',*,*,#52137,.T.);
#74716=ORIENTED_EDGE('',*,*,#52138,.T.);
#74717=ORIENTED_EDGE('',*,*,#52139,.F.);
#74718=ORIENTED_EDGE('',*,*,#52140,.T.);
#74719=ORIENTED_EDGE('',*,*,#52141,.T.);
#74720=ORIENTED_EDGE('',*,*,#52139,.T.);
#74721=ORIENTED_EDGE('',*,*,#52142,.T.);
#74722=ORIENTED_EDGE('',*,*,#52132,.F.);
#74723=ORIENTED_EDGE('',*,*,#52143,.T.);
#74724=ORIENTED_EDGE('',*,*,#52144,.F.);
#74725=ORIENTED_EDGE('',*,*,#52140,.F.);
#74726=ORIENTED_EDGE('',*,*,#52145,.F.);
#74727=ORIENTED_EDGE('',*,*,#52146,.F.);
#74728=ORIENTED_EDGE('',*,*,#52145,.T.);
#74729=ORIENTED_EDGE('',*,*,#52143,.F.);
#74730=ORIENTED_EDGE('',*,*,#52147,.F.);
#74731=ORIENTED_EDGE('',*,*,#52147,.T.);
#74732=ORIENTED_EDGE('',*,*,#52136,.F.);
#74733=ORIENTED_EDGE('',*,*,#52148,.F.);
#74734=ORIENTED_EDGE('',*,*,#52149,.F.);
#74735=ORIENTED_EDGE('',*,*,#52150,.T.);
#74736=ORIENTED_EDGE('',*,*,#52151,.F.);
#74737=ORIENTED_EDGE('',*,*,#52152,.F.);
#74738=ORIENTED_EDGE('',*,*,#50446,.F.);
#74739=ORIENTED_EDGE('',*,*,#52153,.T.);
#74740=ORIENTED_EDGE('',*,*,#52144,.T.);
#74741=ORIENTED_EDGE('',*,*,#52150,.F.);
#74742=ORIENTED_EDGE('',*,*,#50445,.T.);
#74743=ORIENTED_EDGE('',*,*,#52154,.F.);
#74744=ORIENTED_EDGE('',*,*,#52141,.F.);
#74745=ORIENTED_EDGE('',*,*,#52153,.F.);
#74746=ORIENTED_EDGE('',*,*,#50444,.F.);
#74747=ORIENTED_EDGE('',*,*,#52154,.T.);
#74748=ORIENTED_EDGE('',*,*,#50770,.F.);
#74749=ORIENTED_EDGE('',*,*,#52155,.F.);
#74750=ORIENTED_EDGE('',*,*,#52137,.F.);
#74751=ORIENTED_EDGE('',*,*,#52155,.T.);
#74752=ORIENTED_EDGE('',*,*,#50014,.F.);
#74753=ORIENTED_EDGE('',*,*,#52156,.F.);
#74754=ORIENTED_EDGE('',*,*,#52138,.F.);
#74755=ORIENTED_EDGE('',*,*,#52156,.T.);
#74756=ORIENTED_EDGE('',*,*,#50013,.F.);
#74757=ORIENTED_EDGE('',*,*,#52157,.F.);
#74758=ORIENTED_EDGE('',*,*,#52142,.F.);
#74759=ORIENTED_EDGE('',*,*,#52157,.T.);
#74760=ORIENTED_EDGE('',*,*,#50012,.F.);
#74761=ORIENTED_EDGE('',*,*,#52158,.F.);
#74762=ORIENTED_EDGE('',*,*,#52133,.F.);
#74763=ORIENTED_EDGE('',*,*,#52159,.T.);
#74764=ORIENTED_EDGE('',*,*,#52134,.F.);
#74765=ORIENTED_EDGE('',*,*,#52158,.T.);
#74766=ORIENTED_EDGE('',*,*,#50771,.F.);
#74767=ORIENTED_EDGE('',*,*,#52160,.T.);
#74768=ORIENTED_EDGE('',*,*,#52135,.F.);
#74769=ORIENTED_EDGE('',*,*,#52159,.F.);
#74770=ORIENTED_EDGE('',*,*,#50448,.F.);
#74771=ORIENTED_EDGE('',*,*,#52152,.T.);
#74772=ORIENTED_EDGE('',*,*,#52148,.T.);
#74773=ORIENTED_EDGE('',*,*,#52160,.F.);
#74774=ORIENTED_EDGE('',*,*,#50447,.T.);
#74775=ORIENTED_EDGE('',*,*,#52146,.T.);
#74776=ORIENTED_EDGE('',*,*,#52149,.T.);
#74777=ORIENTED_EDGE('',*,*,#52151,.T.);
#74778=ORIENTED_EDGE('',*,*,#52161,.T.);
#74779=ORIENTED_EDGE('',*,*,#52162,.T.);
#74780=ORIENTED_EDGE('',*,*,#52163,.T.);
#74781=ORIENTED_EDGE('',*,*,#52164,.T.);
#74782=ORIENTED_EDGE('',*,*,#52165,.T.);
#74783=ORIENTED_EDGE('',*,*,#52166,.T.);
#74784=ORIENTED_EDGE('',*,*,#52167,.T.);
#74785=ORIENTED_EDGE('',*,*,#52168,.F.);
#74786=ORIENTED_EDGE('',*,*,#52169,.T.);
#74787=ORIENTED_EDGE('',*,*,#52170,.T.);
#74788=ORIENTED_EDGE('',*,*,#52168,.T.);
#74789=ORIENTED_EDGE('',*,*,#52171,.T.);
#74790=ORIENTED_EDGE('',*,*,#52161,.F.);
#74791=ORIENTED_EDGE('',*,*,#52172,.T.);
#74792=ORIENTED_EDGE('',*,*,#52173,.F.);
#74793=ORIENTED_EDGE('',*,*,#52169,.F.);
#74794=ORIENTED_EDGE('',*,*,#52174,.F.);
#74795=ORIENTED_EDGE('',*,*,#52175,.F.);
#74796=ORIENTED_EDGE('',*,*,#52174,.T.);
#74797=ORIENTED_EDGE('',*,*,#52172,.F.);
#74798=ORIENTED_EDGE('',*,*,#52176,.F.);
#74799=ORIENTED_EDGE('',*,*,#52176,.T.);
#74800=ORIENTED_EDGE('',*,*,#52165,.F.);
#74801=ORIENTED_EDGE('',*,*,#52177,.F.);
#74802=ORIENTED_EDGE('',*,*,#52178,.F.);
#74803=ORIENTED_EDGE('',*,*,#52179,.T.);
#74804=ORIENTED_EDGE('',*,*,#52180,.F.);
#74805=ORIENTED_EDGE('',*,*,#52181,.F.);
#74806=ORIENTED_EDGE('',*,*,#50440,.F.);
#74807=ORIENTED_EDGE('',*,*,#52182,.T.);
#74808=ORIENTED_EDGE('',*,*,#52173,.T.);
#74809=ORIENTED_EDGE('',*,*,#52179,.F.);
#74810=ORIENTED_EDGE('',*,*,#50439,.T.);
#74811=ORIENTED_EDGE('',*,*,#52183,.F.);
#74812=ORIENTED_EDGE('',*,*,#52170,.F.);
#74813=ORIENTED_EDGE('',*,*,#52182,.F.);
#74814=ORIENTED_EDGE('',*,*,#50438,.F.);
#74815=ORIENTED_EDGE('',*,*,#52183,.T.);
#74816=ORIENTED_EDGE('',*,*,#50768,.F.);
#74817=ORIENTED_EDGE('',*,*,#52184,.F.);
#74818=ORIENTED_EDGE('',*,*,#52166,.F.);
#74819=ORIENTED_EDGE('',*,*,#52184,.T.);
#74820=ORIENTED_EDGE('',*,*,#50018,.F.);
#74821=ORIENTED_EDGE('',*,*,#52185,.F.);
#74822=ORIENTED_EDGE('',*,*,#52167,.F.);
#74823=ORIENTED_EDGE('',*,*,#52185,.T.);
#74824=ORIENTED_EDGE('',*,*,#50017,.F.);
#74825=ORIENTED_EDGE('',*,*,#52186,.F.);
#74826=ORIENTED_EDGE('',*,*,#52171,.F.);
#74827=ORIENTED_EDGE('',*,*,#52186,.T.);
#74828=ORIENTED_EDGE('',*,*,#50016,.F.);
#74829=ORIENTED_EDGE('',*,*,#52187,.F.);
#74830=ORIENTED_EDGE('',*,*,#52162,.F.);
#74831=ORIENTED_EDGE('',*,*,#52188,.T.);
#74832=ORIENTED_EDGE('',*,*,#52163,.F.);
#74833=ORIENTED_EDGE('',*,*,#52187,.T.);
#74834=ORIENTED_EDGE('',*,*,#50769,.F.);
#74835=ORIENTED_EDGE('',*,*,#52189,.T.);
#74836=ORIENTED_EDGE('',*,*,#52164,.F.);
#74837=ORIENTED_EDGE('',*,*,#52188,.F.);
#74838=ORIENTED_EDGE('',*,*,#50442,.F.);
#74839=ORIENTED_EDGE('',*,*,#52181,.T.);
#74840=ORIENTED_EDGE('',*,*,#52177,.T.);
#74841=ORIENTED_EDGE('',*,*,#52189,.F.);
#74842=ORIENTED_EDGE('',*,*,#50441,.T.);
#74843=ORIENTED_EDGE('',*,*,#52175,.T.);
#74844=ORIENTED_EDGE('',*,*,#52178,.T.);
#74845=ORIENTED_EDGE('',*,*,#52180,.T.);
#74846=ORIENTED_EDGE('',*,*,#52190,.T.);
#74847=ORIENTED_EDGE('',*,*,#52191,.T.);
#74848=ORIENTED_EDGE('',*,*,#52192,.T.);
#74849=ORIENTED_EDGE('',*,*,#52193,.T.);
#74850=ORIENTED_EDGE('',*,*,#52194,.T.);
#74851=ORIENTED_EDGE('',*,*,#52195,.T.);
#74852=ORIENTED_EDGE('',*,*,#52196,.T.);
#74853=ORIENTED_EDGE('',*,*,#52197,.F.);
#74854=ORIENTED_EDGE('',*,*,#52198,.T.);
#74855=ORIENTED_EDGE('',*,*,#52199,.T.);
#74856=ORIENTED_EDGE('',*,*,#52197,.T.);
#74857=ORIENTED_EDGE('',*,*,#52200,.T.);
#74858=ORIENTED_EDGE('',*,*,#52190,.F.);
#74859=ORIENTED_EDGE('',*,*,#52201,.T.);
#74860=ORIENTED_EDGE('',*,*,#52202,.F.);
#74861=ORIENTED_EDGE('',*,*,#52198,.F.);
#74862=ORIENTED_EDGE('',*,*,#52203,.F.);
#74863=ORIENTED_EDGE('',*,*,#52204,.F.);
#74864=ORIENTED_EDGE('',*,*,#52203,.T.);
#74865=ORIENTED_EDGE('',*,*,#52201,.F.);
#74866=ORIENTED_EDGE('',*,*,#52205,.F.);
#74867=ORIENTED_EDGE('',*,*,#52205,.T.);
#74868=ORIENTED_EDGE('',*,*,#52194,.F.);
#74869=ORIENTED_EDGE('',*,*,#52206,.F.);
#74870=ORIENTED_EDGE('',*,*,#52207,.F.);
#74871=ORIENTED_EDGE('',*,*,#52208,.T.);
#74872=ORIENTED_EDGE('',*,*,#52209,.F.);
#74873=ORIENTED_EDGE('',*,*,#52210,.F.);
#74874=ORIENTED_EDGE('',*,*,#50434,.F.);
#74875=ORIENTED_EDGE('',*,*,#52211,.T.);
#74876=ORIENTED_EDGE('',*,*,#52202,.T.);
#74877=ORIENTED_EDGE('',*,*,#52208,.F.);
#74878=ORIENTED_EDGE('',*,*,#50433,.T.);
#74879=ORIENTED_EDGE('',*,*,#52212,.F.);
#74880=ORIENTED_EDGE('',*,*,#52199,.F.);
#74881=ORIENTED_EDGE('',*,*,#52211,.F.);
#74882=ORIENTED_EDGE('',*,*,#50432,.F.);
#74883=ORIENTED_EDGE('',*,*,#52212,.T.);
#74884=ORIENTED_EDGE('',*,*,#50766,.F.);
#74885=ORIENTED_EDGE('',*,*,#52213,.F.);
#74886=ORIENTED_EDGE('',*,*,#52195,.F.);
#74887=ORIENTED_EDGE('',*,*,#52213,.T.);
#74888=ORIENTED_EDGE('',*,*,#50022,.F.);
#74889=ORIENTED_EDGE('',*,*,#52214,.F.);
#74890=ORIENTED_EDGE('',*,*,#52196,.F.);
#74891=ORIENTED_EDGE('',*,*,#52214,.T.);
#74892=ORIENTED_EDGE('',*,*,#50021,.F.);
#74893=ORIENTED_EDGE('',*,*,#52215,.F.);
#74894=ORIENTED_EDGE('',*,*,#52200,.F.);
#74895=ORIENTED_EDGE('',*,*,#52215,.T.);
#74896=ORIENTED_EDGE('',*,*,#50020,.F.);
#74897=ORIENTED_EDGE('',*,*,#52216,.F.);
#74898=ORIENTED_EDGE('',*,*,#52191,.F.);
#74899=ORIENTED_EDGE('',*,*,#52217,.T.);
#74900=ORIENTED_EDGE('',*,*,#52192,.F.);
#74901=ORIENTED_EDGE('',*,*,#52216,.T.);
#74902=ORIENTED_EDGE('',*,*,#50767,.F.);
#74903=ORIENTED_EDGE('',*,*,#52218,.T.);
#74904=ORIENTED_EDGE('',*,*,#52193,.F.);
#74905=ORIENTED_EDGE('',*,*,#52217,.F.);
#74906=ORIENTED_EDGE('',*,*,#50436,.F.);
#74907=ORIENTED_EDGE('',*,*,#52210,.T.);
#74908=ORIENTED_EDGE('',*,*,#52206,.T.);
#74909=ORIENTED_EDGE('',*,*,#52218,.F.);
#74910=ORIENTED_EDGE('',*,*,#50435,.T.);
#74911=ORIENTED_EDGE('',*,*,#52204,.T.);
#74912=ORIENTED_EDGE('',*,*,#52207,.T.);
#74913=ORIENTED_EDGE('',*,*,#52209,.T.);
#74914=ORIENTED_EDGE('',*,*,#52219,.T.);
#74915=ORIENTED_EDGE('',*,*,#52220,.T.);
#74916=ORIENTED_EDGE('',*,*,#52221,.T.);
#74917=ORIENTED_EDGE('',*,*,#52222,.T.);
#74918=ORIENTED_EDGE('',*,*,#52223,.T.);
#74919=ORIENTED_EDGE('',*,*,#52224,.T.);
#74920=ORIENTED_EDGE('',*,*,#52225,.T.);
#74921=ORIENTED_EDGE('',*,*,#52226,.F.);
#74922=ORIENTED_EDGE('',*,*,#52227,.T.);
#74923=ORIENTED_EDGE('',*,*,#52228,.T.);
#74924=ORIENTED_EDGE('',*,*,#52226,.T.);
#74925=ORIENTED_EDGE('',*,*,#52229,.T.);
#74926=ORIENTED_EDGE('',*,*,#52219,.F.);
#74927=ORIENTED_EDGE('',*,*,#52230,.T.);
#74928=ORIENTED_EDGE('',*,*,#52231,.F.);
#74929=ORIENTED_EDGE('',*,*,#52227,.F.);
#74930=ORIENTED_EDGE('',*,*,#52232,.F.);
#74931=ORIENTED_EDGE('',*,*,#52233,.F.);
#74932=ORIENTED_EDGE('',*,*,#52232,.T.);
#74933=ORIENTED_EDGE('',*,*,#52230,.F.);
#74934=ORIENTED_EDGE('',*,*,#52234,.F.);
#74935=ORIENTED_EDGE('',*,*,#52234,.T.);
#74936=ORIENTED_EDGE('',*,*,#52223,.F.);
#74937=ORIENTED_EDGE('',*,*,#52235,.F.);
#74938=ORIENTED_EDGE('',*,*,#52236,.F.);
#74939=ORIENTED_EDGE('',*,*,#52237,.T.);
#74940=ORIENTED_EDGE('',*,*,#52238,.F.);
#74941=ORIENTED_EDGE('',*,*,#52239,.F.);
#74942=ORIENTED_EDGE('',*,*,#50428,.F.);
#74943=ORIENTED_EDGE('',*,*,#52240,.T.);
#74944=ORIENTED_EDGE('',*,*,#52231,.T.);
#74945=ORIENTED_EDGE('',*,*,#52237,.F.);
#74946=ORIENTED_EDGE('',*,*,#50427,.T.);
#74947=ORIENTED_EDGE('',*,*,#52241,.F.);
#74948=ORIENTED_EDGE('',*,*,#52228,.F.);
#74949=ORIENTED_EDGE('',*,*,#52240,.F.);
#74950=ORIENTED_EDGE('',*,*,#50426,.F.);
#74951=ORIENTED_EDGE('',*,*,#52241,.T.);
#74952=ORIENTED_EDGE('',*,*,#50764,.F.);
#74953=ORIENTED_EDGE('',*,*,#52242,.F.);
#74954=ORIENTED_EDGE('',*,*,#52224,.F.);
#74955=ORIENTED_EDGE('',*,*,#52242,.T.);
#74956=ORIENTED_EDGE('',*,*,#50026,.F.);
#74957=ORIENTED_EDGE('',*,*,#52243,.F.);
#74958=ORIENTED_EDGE('',*,*,#52225,.F.);
#74959=ORIENTED_EDGE('',*,*,#52243,.T.);
#74960=ORIENTED_EDGE('',*,*,#50025,.F.);
#74961=ORIENTED_EDGE('',*,*,#52244,.F.);
#74962=ORIENTED_EDGE('',*,*,#52229,.F.);
#74963=ORIENTED_EDGE('',*,*,#52244,.T.);
#74964=ORIENTED_EDGE('',*,*,#50024,.F.);
#74965=ORIENTED_EDGE('',*,*,#52245,.F.);
#74966=ORIENTED_EDGE('',*,*,#52220,.F.);
#74967=ORIENTED_EDGE('',*,*,#52246,.T.);
#74968=ORIENTED_EDGE('',*,*,#52221,.F.);
#74969=ORIENTED_EDGE('',*,*,#52245,.T.);
#74970=ORIENTED_EDGE('',*,*,#50765,.F.);
#74971=ORIENTED_EDGE('',*,*,#52247,.T.);
#74972=ORIENTED_EDGE('',*,*,#52222,.F.);
#74973=ORIENTED_EDGE('',*,*,#52246,.F.);
#74974=ORIENTED_EDGE('',*,*,#50430,.F.);
#74975=ORIENTED_EDGE('',*,*,#52239,.T.);
#74976=ORIENTED_EDGE('',*,*,#52235,.T.);
#74977=ORIENTED_EDGE('',*,*,#52247,.F.);
#74978=ORIENTED_EDGE('',*,*,#50429,.T.);
#74979=ORIENTED_EDGE('',*,*,#52233,.T.);
#74980=ORIENTED_EDGE('',*,*,#52236,.T.);
#74981=ORIENTED_EDGE('',*,*,#52238,.T.);
#74982=ORIENTED_EDGE('',*,*,#52248,.T.);
#74983=ORIENTED_EDGE('',*,*,#52249,.T.);
#74984=ORIENTED_EDGE('',*,*,#52250,.T.);
#74985=ORIENTED_EDGE('',*,*,#52251,.T.);
#74986=ORIENTED_EDGE('',*,*,#52252,.T.);
#74987=ORIENTED_EDGE('',*,*,#52253,.T.);
#74988=ORIENTED_EDGE('',*,*,#52254,.T.);
#74989=ORIENTED_EDGE('',*,*,#52255,.F.);
#74990=ORIENTED_EDGE('',*,*,#52256,.T.);
#74991=ORIENTED_EDGE('',*,*,#52257,.T.);
#74992=ORIENTED_EDGE('',*,*,#52255,.T.);
#74993=ORIENTED_EDGE('',*,*,#52258,.T.);
#74994=ORIENTED_EDGE('',*,*,#52248,.F.);
#74995=ORIENTED_EDGE('',*,*,#52259,.T.);
#74996=ORIENTED_EDGE('',*,*,#52260,.F.);
#74997=ORIENTED_EDGE('',*,*,#52256,.F.);
#74998=ORIENTED_EDGE('',*,*,#52261,.F.);
#74999=ORIENTED_EDGE('',*,*,#52262,.F.);
#75000=ORIENTED_EDGE('',*,*,#52261,.T.);
#75001=ORIENTED_EDGE('',*,*,#52259,.F.);
#75002=ORIENTED_EDGE('',*,*,#52263,.F.);
#75003=ORIENTED_EDGE('',*,*,#52263,.T.);
#75004=ORIENTED_EDGE('',*,*,#52252,.F.);
#75005=ORIENTED_EDGE('',*,*,#52264,.F.);
#75006=ORIENTED_EDGE('',*,*,#52265,.F.);
#75007=ORIENTED_EDGE('',*,*,#52266,.T.);
#75008=ORIENTED_EDGE('',*,*,#52267,.F.);
#75009=ORIENTED_EDGE('',*,*,#52268,.F.);
#75010=ORIENTED_EDGE('',*,*,#50422,.F.);
#75011=ORIENTED_EDGE('',*,*,#52269,.T.);
#75012=ORIENTED_EDGE('',*,*,#52260,.T.);
#75013=ORIENTED_EDGE('',*,*,#52266,.F.);
#75014=ORIENTED_EDGE('',*,*,#50421,.T.);
#75015=ORIENTED_EDGE('',*,*,#52270,.F.);
#75016=ORIENTED_EDGE('',*,*,#52257,.F.);
#75017=ORIENTED_EDGE('',*,*,#52269,.F.);
#75018=ORIENTED_EDGE('',*,*,#50420,.F.);
#75019=ORIENTED_EDGE('',*,*,#52270,.T.);
#75020=ORIENTED_EDGE('',*,*,#50762,.F.);
#75021=ORIENTED_EDGE('',*,*,#52271,.F.);
#75022=ORIENTED_EDGE('',*,*,#52253,.F.);
#75023=ORIENTED_EDGE('',*,*,#52271,.T.);
#75024=ORIENTED_EDGE('',*,*,#50030,.F.);
#75025=ORIENTED_EDGE('',*,*,#52272,.F.);
#75026=ORIENTED_EDGE('',*,*,#52254,.F.);
#75027=ORIENTED_EDGE('',*,*,#52272,.T.);
#75028=ORIENTED_EDGE('',*,*,#50029,.F.);
#75029=ORIENTED_EDGE('',*,*,#52273,.F.);
#75030=ORIENTED_EDGE('',*,*,#52258,.F.);
#75031=ORIENTED_EDGE('',*,*,#52273,.T.);
#75032=ORIENTED_EDGE('',*,*,#50028,.F.);
#75033=ORIENTED_EDGE('',*,*,#52274,.F.);
#75034=ORIENTED_EDGE('',*,*,#52249,.F.);
#75035=ORIENTED_EDGE('',*,*,#52275,.T.);
#75036=ORIENTED_EDGE('',*,*,#52250,.F.);
#75037=ORIENTED_EDGE('',*,*,#52274,.T.);
#75038=ORIENTED_EDGE('',*,*,#50763,.F.);
#75039=ORIENTED_EDGE('',*,*,#52276,.T.);
#75040=ORIENTED_EDGE('',*,*,#52251,.F.);
#75041=ORIENTED_EDGE('',*,*,#52275,.F.);
#75042=ORIENTED_EDGE('',*,*,#50424,.F.);
#75043=ORIENTED_EDGE('',*,*,#52268,.T.);
#75044=ORIENTED_EDGE('',*,*,#52264,.T.);
#75045=ORIENTED_EDGE('',*,*,#52276,.F.);
#75046=ORIENTED_EDGE('',*,*,#50423,.T.);
#75047=ORIENTED_EDGE('',*,*,#52262,.T.);
#75048=ORIENTED_EDGE('',*,*,#52265,.T.);
#75049=ORIENTED_EDGE('',*,*,#52267,.T.);
#75050=ORIENTED_EDGE('',*,*,#52277,.T.);
#75051=ORIENTED_EDGE('',*,*,#52278,.T.);
#75052=ORIENTED_EDGE('',*,*,#52279,.T.);
#75053=ORIENTED_EDGE('',*,*,#52280,.T.);
#75054=ORIENTED_EDGE('',*,*,#52281,.T.);
#75055=ORIENTED_EDGE('',*,*,#52282,.T.);
#75056=ORIENTED_EDGE('',*,*,#52283,.T.);
#75057=ORIENTED_EDGE('',*,*,#52284,.F.);
#75058=ORIENTED_EDGE('',*,*,#52285,.T.);
#75059=ORIENTED_EDGE('',*,*,#52286,.T.);
#75060=ORIENTED_EDGE('',*,*,#52284,.T.);
#75061=ORIENTED_EDGE('',*,*,#52287,.T.);
#75062=ORIENTED_EDGE('',*,*,#52277,.F.);
#75063=ORIENTED_EDGE('',*,*,#52288,.T.);
#75064=ORIENTED_EDGE('',*,*,#52289,.F.);
#75065=ORIENTED_EDGE('',*,*,#52285,.F.);
#75066=ORIENTED_EDGE('',*,*,#52290,.F.);
#75067=ORIENTED_EDGE('',*,*,#52291,.F.);
#75068=ORIENTED_EDGE('',*,*,#52290,.T.);
#75069=ORIENTED_EDGE('',*,*,#52288,.F.);
#75070=ORIENTED_EDGE('',*,*,#52292,.F.);
#75071=ORIENTED_EDGE('',*,*,#52292,.T.);
#75072=ORIENTED_EDGE('',*,*,#52281,.F.);
#75073=ORIENTED_EDGE('',*,*,#52293,.F.);
#75074=ORIENTED_EDGE('',*,*,#52294,.F.);
#75075=ORIENTED_EDGE('',*,*,#52295,.T.);
#75076=ORIENTED_EDGE('',*,*,#52296,.F.);
#75077=ORIENTED_EDGE('',*,*,#52297,.F.);
#75078=ORIENTED_EDGE('',*,*,#50416,.F.);
#75079=ORIENTED_EDGE('',*,*,#52298,.T.);
#75080=ORIENTED_EDGE('',*,*,#52289,.T.);
#75081=ORIENTED_EDGE('',*,*,#52295,.F.);
#75082=ORIENTED_EDGE('',*,*,#50415,.T.);
#75083=ORIENTED_EDGE('',*,*,#52299,.F.);
#75084=ORIENTED_EDGE('',*,*,#52286,.F.);
#75085=ORIENTED_EDGE('',*,*,#52298,.F.);
#75086=ORIENTED_EDGE('',*,*,#50414,.F.);
#75087=ORIENTED_EDGE('',*,*,#52299,.T.);
#75088=ORIENTED_EDGE('',*,*,#50760,.F.);
#75089=ORIENTED_EDGE('',*,*,#52300,.F.);
#75090=ORIENTED_EDGE('',*,*,#52282,.F.);
#75091=ORIENTED_EDGE('',*,*,#52300,.T.);
#75092=ORIENTED_EDGE('',*,*,#50034,.F.);
#75093=ORIENTED_EDGE('',*,*,#52301,.F.);
#75094=ORIENTED_EDGE('',*,*,#52283,.F.);
#75095=ORIENTED_EDGE('',*,*,#52301,.T.);
#75096=ORIENTED_EDGE('',*,*,#50033,.F.);
#75097=ORIENTED_EDGE('',*,*,#52302,.F.);
#75098=ORIENTED_EDGE('',*,*,#52287,.F.);
#75099=ORIENTED_EDGE('',*,*,#52302,.T.);
#75100=ORIENTED_EDGE('',*,*,#50032,.F.);
#75101=ORIENTED_EDGE('',*,*,#52303,.F.);
#75102=ORIENTED_EDGE('',*,*,#52278,.F.);
#75103=ORIENTED_EDGE('',*,*,#52304,.T.);
#75104=ORIENTED_EDGE('',*,*,#52279,.F.);
#75105=ORIENTED_EDGE('',*,*,#52303,.T.);
#75106=ORIENTED_EDGE('',*,*,#50761,.F.);
#75107=ORIENTED_EDGE('',*,*,#52305,.T.);
#75108=ORIENTED_EDGE('',*,*,#52280,.F.);
#75109=ORIENTED_EDGE('',*,*,#52304,.F.);
#75110=ORIENTED_EDGE('',*,*,#50418,.F.);
#75111=ORIENTED_EDGE('',*,*,#52297,.T.);
#75112=ORIENTED_EDGE('',*,*,#52293,.T.);
#75113=ORIENTED_EDGE('',*,*,#52305,.F.);
#75114=ORIENTED_EDGE('',*,*,#50417,.T.);
#75115=ORIENTED_EDGE('',*,*,#52291,.T.);
#75116=ORIENTED_EDGE('',*,*,#52294,.T.);
#75117=ORIENTED_EDGE('',*,*,#52296,.T.);
#75118=ORIENTED_EDGE('',*,*,#52306,.T.);
#75119=ORIENTED_EDGE('',*,*,#52307,.T.);
#75120=ORIENTED_EDGE('',*,*,#52308,.T.);
#75121=ORIENTED_EDGE('',*,*,#52309,.T.);
#75122=ORIENTED_EDGE('',*,*,#52310,.T.);
#75123=ORIENTED_EDGE('',*,*,#52311,.T.);
#75124=ORIENTED_EDGE('',*,*,#52312,.T.);
#75125=ORIENTED_EDGE('',*,*,#52313,.F.);
#75126=ORIENTED_EDGE('',*,*,#52314,.T.);
#75127=ORIENTED_EDGE('',*,*,#52315,.T.);
#75128=ORIENTED_EDGE('',*,*,#52313,.T.);
#75129=ORIENTED_EDGE('',*,*,#52316,.T.);
#75130=ORIENTED_EDGE('',*,*,#52306,.F.);
#75131=ORIENTED_EDGE('',*,*,#52317,.T.);
#75132=ORIENTED_EDGE('',*,*,#52318,.F.);
#75133=ORIENTED_EDGE('',*,*,#52314,.F.);
#75134=ORIENTED_EDGE('',*,*,#52319,.F.);
#75135=ORIENTED_EDGE('',*,*,#52320,.F.);
#75136=ORIENTED_EDGE('',*,*,#52319,.T.);
#75137=ORIENTED_EDGE('',*,*,#52317,.F.);
#75138=ORIENTED_EDGE('',*,*,#52321,.F.);
#75139=ORIENTED_EDGE('',*,*,#52321,.T.);
#75140=ORIENTED_EDGE('',*,*,#52310,.F.);
#75141=ORIENTED_EDGE('',*,*,#52322,.F.);
#75142=ORIENTED_EDGE('',*,*,#52323,.F.);
#75143=ORIENTED_EDGE('',*,*,#52324,.T.);
#75144=ORIENTED_EDGE('',*,*,#52325,.F.);
#75145=ORIENTED_EDGE('',*,*,#52326,.F.);
#75146=ORIENTED_EDGE('',*,*,#50410,.F.);
#75147=ORIENTED_EDGE('',*,*,#52327,.T.);
#75148=ORIENTED_EDGE('',*,*,#52318,.T.);
#75149=ORIENTED_EDGE('',*,*,#52324,.F.);
#75150=ORIENTED_EDGE('',*,*,#50409,.T.);
#75151=ORIENTED_EDGE('',*,*,#52328,.F.);
#75152=ORIENTED_EDGE('',*,*,#52315,.F.);
#75153=ORIENTED_EDGE('',*,*,#52327,.F.);
#75154=ORIENTED_EDGE('',*,*,#50408,.F.);
#75155=ORIENTED_EDGE('',*,*,#52328,.T.);
#75156=ORIENTED_EDGE('',*,*,#50758,.F.);
#75157=ORIENTED_EDGE('',*,*,#52329,.F.);
#75158=ORIENTED_EDGE('',*,*,#52311,.F.);
#75159=ORIENTED_EDGE('',*,*,#52329,.T.);
#75160=ORIENTED_EDGE('',*,*,#50038,.F.);
#75161=ORIENTED_EDGE('',*,*,#52330,.F.);
#75162=ORIENTED_EDGE('',*,*,#52312,.F.);
#75163=ORIENTED_EDGE('',*,*,#52330,.T.);
#75164=ORIENTED_EDGE('',*,*,#50037,.F.);
#75165=ORIENTED_EDGE('',*,*,#52331,.F.);
#75166=ORIENTED_EDGE('',*,*,#52316,.F.);
#75167=ORIENTED_EDGE('',*,*,#52331,.T.);
#75168=ORIENTED_EDGE('',*,*,#50036,.F.);
#75169=ORIENTED_EDGE('',*,*,#52332,.F.);
#75170=ORIENTED_EDGE('',*,*,#52307,.F.);
#75171=ORIENTED_EDGE('',*,*,#52333,.T.);
#75172=ORIENTED_EDGE('',*,*,#52308,.F.);
#75173=ORIENTED_EDGE('',*,*,#52332,.T.);
#75174=ORIENTED_EDGE('',*,*,#50759,.F.);
#75175=ORIENTED_EDGE('',*,*,#52334,.T.);
#75176=ORIENTED_EDGE('',*,*,#52309,.F.);
#75177=ORIENTED_EDGE('',*,*,#52333,.F.);
#75178=ORIENTED_EDGE('',*,*,#50412,.F.);
#75179=ORIENTED_EDGE('',*,*,#52326,.T.);
#75180=ORIENTED_EDGE('',*,*,#52322,.T.);
#75181=ORIENTED_EDGE('',*,*,#52334,.F.);
#75182=ORIENTED_EDGE('',*,*,#50411,.T.);
#75183=ORIENTED_EDGE('',*,*,#52320,.T.);
#75184=ORIENTED_EDGE('',*,*,#52323,.T.);
#75185=ORIENTED_EDGE('',*,*,#52325,.T.);
#75186=ORIENTED_EDGE('',*,*,#52335,.T.);
#75187=ORIENTED_EDGE('',*,*,#52336,.T.);
#75188=ORIENTED_EDGE('',*,*,#52337,.T.);
#75189=ORIENTED_EDGE('',*,*,#52338,.T.);
#75190=ORIENTED_EDGE('',*,*,#52339,.T.);
#75191=ORIENTED_EDGE('',*,*,#52340,.T.);
#75192=ORIENTED_EDGE('',*,*,#52341,.T.);
#75193=ORIENTED_EDGE('',*,*,#52342,.F.);
#75194=ORIENTED_EDGE('',*,*,#52343,.T.);
#75195=ORIENTED_EDGE('',*,*,#52344,.T.);
#75196=ORIENTED_EDGE('',*,*,#52342,.T.);
#75197=ORIENTED_EDGE('',*,*,#52345,.T.);
#75198=ORIENTED_EDGE('',*,*,#52335,.F.);
#75199=ORIENTED_EDGE('',*,*,#52346,.T.);
#75200=ORIENTED_EDGE('',*,*,#52347,.F.);
#75201=ORIENTED_EDGE('',*,*,#52343,.F.);
#75202=ORIENTED_EDGE('',*,*,#52348,.F.);
#75203=ORIENTED_EDGE('',*,*,#52349,.F.);
#75204=ORIENTED_EDGE('',*,*,#52348,.T.);
#75205=ORIENTED_EDGE('',*,*,#52346,.F.);
#75206=ORIENTED_EDGE('',*,*,#52350,.F.);
#75207=ORIENTED_EDGE('',*,*,#52350,.T.);
#75208=ORIENTED_EDGE('',*,*,#52339,.F.);
#75209=ORIENTED_EDGE('',*,*,#52351,.F.);
#75210=ORIENTED_EDGE('',*,*,#52352,.F.);
#75211=ORIENTED_EDGE('',*,*,#52353,.T.);
#75212=ORIENTED_EDGE('',*,*,#52354,.F.);
#75213=ORIENTED_EDGE('',*,*,#52355,.F.);
#75214=ORIENTED_EDGE('',*,*,#50404,.F.);
#75215=ORIENTED_EDGE('',*,*,#52356,.T.);
#75216=ORIENTED_EDGE('',*,*,#52347,.T.);
#75217=ORIENTED_EDGE('',*,*,#52353,.F.);
#75218=ORIENTED_EDGE('',*,*,#50403,.T.);
#75219=ORIENTED_EDGE('',*,*,#52357,.F.);
#75220=ORIENTED_EDGE('',*,*,#52344,.F.);
#75221=ORIENTED_EDGE('',*,*,#52356,.F.);
#75222=ORIENTED_EDGE('',*,*,#50402,.F.);
#75223=ORIENTED_EDGE('',*,*,#52357,.T.);
#75224=ORIENTED_EDGE('',*,*,#50756,.F.);
#75225=ORIENTED_EDGE('',*,*,#52358,.F.);
#75226=ORIENTED_EDGE('',*,*,#52340,.F.);
#75227=ORIENTED_EDGE('',*,*,#52358,.T.);
#75228=ORIENTED_EDGE('',*,*,#50042,.F.);
#75229=ORIENTED_EDGE('',*,*,#52359,.F.);
#75230=ORIENTED_EDGE('',*,*,#52341,.F.);
#75231=ORIENTED_EDGE('',*,*,#52359,.T.);
#75232=ORIENTED_EDGE('',*,*,#50041,.F.);
#75233=ORIENTED_EDGE('',*,*,#52360,.F.);
#75234=ORIENTED_EDGE('',*,*,#52345,.F.);
#75235=ORIENTED_EDGE('',*,*,#52360,.T.);
#75236=ORIENTED_EDGE('',*,*,#50040,.F.);
#75237=ORIENTED_EDGE('',*,*,#52361,.F.);
#75238=ORIENTED_EDGE('',*,*,#52336,.F.);
#75239=ORIENTED_EDGE('',*,*,#52362,.T.);
#75240=ORIENTED_EDGE('',*,*,#52337,.F.);
#75241=ORIENTED_EDGE('',*,*,#52361,.T.);
#75242=ORIENTED_EDGE('',*,*,#50757,.F.);
#75243=ORIENTED_EDGE('',*,*,#52363,.T.);
#75244=ORIENTED_EDGE('',*,*,#52338,.F.);
#75245=ORIENTED_EDGE('',*,*,#52362,.F.);
#75246=ORIENTED_EDGE('',*,*,#50406,.F.);
#75247=ORIENTED_EDGE('',*,*,#52355,.T.);
#75248=ORIENTED_EDGE('',*,*,#52351,.T.);
#75249=ORIENTED_EDGE('',*,*,#52363,.F.);
#75250=ORIENTED_EDGE('',*,*,#50405,.T.);
#75251=ORIENTED_EDGE('',*,*,#52349,.T.);
#75252=ORIENTED_EDGE('',*,*,#52352,.T.);
#75253=ORIENTED_EDGE('',*,*,#52354,.T.);
#75254=ORIENTED_EDGE('',*,*,#52364,.T.);
#75255=ORIENTED_EDGE('',*,*,#52365,.T.);
#75256=ORIENTED_EDGE('',*,*,#52366,.T.);
#75257=ORIENTED_EDGE('',*,*,#52367,.T.);
#75258=ORIENTED_EDGE('',*,*,#52368,.T.);
#75259=ORIENTED_EDGE('',*,*,#52369,.T.);
#75260=ORIENTED_EDGE('',*,*,#52370,.T.);
#75261=ORIENTED_EDGE('',*,*,#52371,.F.);
#75262=ORIENTED_EDGE('',*,*,#52372,.T.);
#75263=ORIENTED_EDGE('',*,*,#52373,.T.);
#75264=ORIENTED_EDGE('',*,*,#52371,.T.);
#75265=ORIENTED_EDGE('',*,*,#52374,.T.);
#75266=ORIENTED_EDGE('',*,*,#52364,.F.);
#75267=ORIENTED_EDGE('',*,*,#52375,.T.);
#75268=ORIENTED_EDGE('',*,*,#52376,.F.);
#75269=ORIENTED_EDGE('',*,*,#52372,.F.);
#75270=ORIENTED_EDGE('',*,*,#52377,.F.);
#75271=ORIENTED_EDGE('',*,*,#52378,.F.);
#75272=ORIENTED_EDGE('',*,*,#52377,.T.);
#75273=ORIENTED_EDGE('',*,*,#52375,.F.);
#75274=ORIENTED_EDGE('',*,*,#52379,.F.);
#75275=ORIENTED_EDGE('',*,*,#52379,.T.);
#75276=ORIENTED_EDGE('',*,*,#52368,.F.);
#75277=ORIENTED_EDGE('',*,*,#52380,.F.);
#75278=ORIENTED_EDGE('',*,*,#52381,.F.);
#75279=ORIENTED_EDGE('',*,*,#52382,.T.);
#75280=ORIENTED_EDGE('',*,*,#52383,.F.);
#75281=ORIENTED_EDGE('',*,*,#52384,.F.);
#75282=ORIENTED_EDGE('',*,*,#50398,.F.);
#75283=ORIENTED_EDGE('',*,*,#52385,.T.);
#75284=ORIENTED_EDGE('',*,*,#52376,.T.);
#75285=ORIENTED_EDGE('',*,*,#52382,.F.);
#75286=ORIENTED_EDGE('',*,*,#50397,.T.);
#75287=ORIENTED_EDGE('',*,*,#52386,.F.);
#75288=ORIENTED_EDGE('',*,*,#52373,.F.);
#75289=ORIENTED_EDGE('',*,*,#52385,.F.);
#75290=ORIENTED_EDGE('',*,*,#50396,.F.);
#75291=ORIENTED_EDGE('',*,*,#52386,.T.);
#75292=ORIENTED_EDGE('',*,*,#50754,.F.);
#75293=ORIENTED_EDGE('',*,*,#52387,.F.);
#75294=ORIENTED_EDGE('',*,*,#52369,.F.);
#75295=ORIENTED_EDGE('',*,*,#52387,.T.);
#75296=ORIENTED_EDGE('',*,*,#50046,.F.);
#75297=ORIENTED_EDGE('',*,*,#52388,.F.);
#75298=ORIENTED_EDGE('',*,*,#52370,.F.);
#75299=ORIENTED_EDGE('',*,*,#52388,.T.);
#75300=ORIENTED_EDGE('',*,*,#50045,.F.);
#75301=ORIENTED_EDGE('',*,*,#52389,.F.);
#75302=ORIENTED_EDGE('',*,*,#52374,.F.);
#75303=ORIENTED_EDGE('',*,*,#52389,.T.);
#75304=ORIENTED_EDGE('',*,*,#50044,.F.);
#75305=ORIENTED_EDGE('',*,*,#52390,.F.);
#75306=ORIENTED_EDGE('',*,*,#52365,.F.);
#75307=ORIENTED_EDGE('',*,*,#52391,.T.);
#75308=ORIENTED_EDGE('',*,*,#52366,.F.);
#75309=ORIENTED_EDGE('',*,*,#52390,.T.);
#75310=ORIENTED_EDGE('',*,*,#50755,.F.);
#75311=ORIENTED_EDGE('',*,*,#52392,.T.);
#75312=ORIENTED_EDGE('',*,*,#52367,.F.);
#75313=ORIENTED_EDGE('',*,*,#52391,.F.);
#75314=ORIENTED_EDGE('',*,*,#50400,.F.);
#75315=ORIENTED_EDGE('',*,*,#52384,.T.);
#75316=ORIENTED_EDGE('',*,*,#52380,.T.);
#75317=ORIENTED_EDGE('',*,*,#52392,.F.);
#75318=ORIENTED_EDGE('',*,*,#50399,.T.);
#75319=ORIENTED_EDGE('',*,*,#52378,.T.);
#75320=ORIENTED_EDGE('',*,*,#52381,.T.);
#75321=ORIENTED_EDGE('',*,*,#52383,.T.);
#75322=ORIENTED_EDGE('',*,*,#52393,.T.);
#75323=ORIENTED_EDGE('',*,*,#52394,.T.);
#75324=ORIENTED_EDGE('',*,*,#52395,.T.);
#75325=ORIENTED_EDGE('',*,*,#52396,.T.);
#75326=ORIENTED_EDGE('',*,*,#52397,.T.);
#75327=ORIENTED_EDGE('',*,*,#52398,.T.);
#75328=ORIENTED_EDGE('',*,*,#52399,.T.);
#75329=ORIENTED_EDGE('',*,*,#52400,.F.);
#75330=ORIENTED_EDGE('',*,*,#52401,.T.);
#75331=ORIENTED_EDGE('',*,*,#52402,.T.);
#75332=ORIENTED_EDGE('',*,*,#52400,.T.);
#75333=ORIENTED_EDGE('',*,*,#52403,.T.);
#75334=ORIENTED_EDGE('',*,*,#52393,.F.);
#75335=ORIENTED_EDGE('',*,*,#52404,.T.);
#75336=ORIENTED_EDGE('',*,*,#52405,.F.);
#75337=ORIENTED_EDGE('',*,*,#52401,.F.);
#75338=ORIENTED_EDGE('',*,*,#52406,.F.);
#75339=ORIENTED_EDGE('',*,*,#52407,.F.);
#75340=ORIENTED_EDGE('',*,*,#52406,.T.);
#75341=ORIENTED_EDGE('',*,*,#52404,.F.);
#75342=ORIENTED_EDGE('',*,*,#52408,.F.);
#75343=ORIENTED_EDGE('',*,*,#52408,.T.);
#75344=ORIENTED_EDGE('',*,*,#52397,.F.);
#75345=ORIENTED_EDGE('',*,*,#52409,.F.);
#75346=ORIENTED_EDGE('',*,*,#52410,.F.);
#75347=ORIENTED_EDGE('',*,*,#52411,.T.);
#75348=ORIENTED_EDGE('',*,*,#52412,.F.);
#75349=ORIENTED_EDGE('',*,*,#52413,.F.);
#75350=ORIENTED_EDGE('',*,*,#50392,.F.);
#75351=ORIENTED_EDGE('',*,*,#52414,.T.);
#75352=ORIENTED_EDGE('',*,*,#52405,.T.);
#75353=ORIENTED_EDGE('',*,*,#52411,.F.);
#75354=ORIENTED_EDGE('',*,*,#50391,.T.);
#75355=ORIENTED_EDGE('',*,*,#52415,.F.);
#75356=ORIENTED_EDGE('',*,*,#52402,.F.);
#75357=ORIENTED_EDGE('',*,*,#52414,.F.);
#75358=ORIENTED_EDGE('',*,*,#50390,.F.);
#75359=ORIENTED_EDGE('',*,*,#52415,.T.);
#75360=ORIENTED_EDGE('',*,*,#50752,.F.);
#75361=ORIENTED_EDGE('',*,*,#52416,.F.);
#75362=ORIENTED_EDGE('',*,*,#52398,.F.);
#75363=ORIENTED_EDGE('',*,*,#52416,.T.);
#75364=ORIENTED_EDGE('',*,*,#50050,.F.);
#75365=ORIENTED_EDGE('',*,*,#52417,.F.);
#75366=ORIENTED_EDGE('',*,*,#52399,.F.);
#75367=ORIENTED_EDGE('',*,*,#52417,.T.);
#75368=ORIENTED_EDGE('',*,*,#50049,.F.);
#75369=ORIENTED_EDGE('',*,*,#52418,.F.);
#75370=ORIENTED_EDGE('',*,*,#52403,.F.);
#75371=ORIENTED_EDGE('',*,*,#52418,.T.);
#75372=ORIENTED_EDGE('',*,*,#50048,.F.);
#75373=ORIENTED_EDGE('',*,*,#52419,.F.);
#75374=ORIENTED_EDGE('',*,*,#52394,.F.);
#75375=ORIENTED_EDGE('',*,*,#52420,.T.);
#75376=ORIENTED_EDGE('',*,*,#52395,.F.);
#75377=ORIENTED_EDGE('',*,*,#52419,.T.);
#75378=ORIENTED_EDGE('',*,*,#50753,.F.);
#75379=ORIENTED_EDGE('',*,*,#52421,.T.);
#75380=ORIENTED_EDGE('',*,*,#52396,.F.);
#75381=ORIENTED_EDGE('',*,*,#52420,.F.);
#75382=ORIENTED_EDGE('',*,*,#50394,.F.);
#75383=ORIENTED_EDGE('',*,*,#52413,.T.);
#75384=ORIENTED_EDGE('',*,*,#52409,.T.);
#75385=ORIENTED_EDGE('',*,*,#52421,.F.);
#75386=ORIENTED_EDGE('',*,*,#50393,.T.);
#75387=ORIENTED_EDGE('',*,*,#52407,.T.);
#75388=ORIENTED_EDGE('',*,*,#52410,.T.);
#75389=ORIENTED_EDGE('',*,*,#52412,.T.);
#75390=ORIENTED_EDGE('',*,*,#52422,.T.);
#75391=ORIENTED_EDGE('',*,*,#52423,.T.);
#75392=ORIENTED_EDGE('',*,*,#52424,.T.);
#75393=ORIENTED_EDGE('',*,*,#52425,.T.);
#75394=ORIENTED_EDGE('',*,*,#52426,.T.);
#75395=ORIENTED_EDGE('',*,*,#52427,.T.);
#75396=ORIENTED_EDGE('',*,*,#52428,.T.);
#75397=ORIENTED_EDGE('',*,*,#52429,.F.);
#75398=ORIENTED_EDGE('',*,*,#52430,.T.);
#75399=ORIENTED_EDGE('',*,*,#52431,.T.);
#75400=ORIENTED_EDGE('',*,*,#52429,.T.);
#75401=ORIENTED_EDGE('',*,*,#52432,.T.);
#75402=ORIENTED_EDGE('',*,*,#52422,.F.);
#75403=ORIENTED_EDGE('',*,*,#52433,.T.);
#75404=ORIENTED_EDGE('',*,*,#52434,.F.);
#75405=ORIENTED_EDGE('',*,*,#52430,.F.);
#75406=ORIENTED_EDGE('',*,*,#52435,.F.);
#75407=ORIENTED_EDGE('',*,*,#52436,.F.);
#75408=ORIENTED_EDGE('',*,*,#52435,.T.);
#75409=ORIENTED_EDGE('',*,*,#52433,.F.);
#75410=ORIENTED_EDGE('',*,*,#52437,.F.);
#75411=ORIENTED_EDGE('',*,*,#52437,.T.);
#75412=ORIENTED_EDGE('',*,*,#52426,.F.);
#75413=ORIENTED_EDGE('',*,*,#52438,.F.);
#75414=ORIENTED_EDGE('',*,*,#52439,.F.);
#75415=ORIENTED_EDGE('',*,*,#52440,.T.);
#75416=ORIENTED_EDGE('',*,*,#52441,.F.);
#75417=ORIENTED_EDGE('',*,*,#52442,.F.);
#75418=ORIENTED_EDGE('',*,*,#50386,.F.);
#75419=ORIENTED_EDGE('',*,*,#52443,.T.);
#75420=ORIENTED_EDGE('',*,*,#52434,.T.);
#75421=ORIENTED_EDGE('',*,*,#52440,.F.);
#75422=ORIENTED_EDGE('',*,*,#50385,.T.);
#75423=ORIENTED_EDGE('',*,*,#52444,.F.);
#75424=ORIENTED_EDGE('',*,*,#52431,.F.);
#75425=ORIENTED_EDGE('',*,*,#52443,.F.);
#75426=ORIENTED_EDGE('',*,*,#50384,.F.);
#75427=ORIENTED_EDGE('',*,*,#52444,.T.);
#75428=ORIENTED_EDGE('',*,*,#50750,.F.);
#75429=ORIENTED_EDGE('',*,*,#52445,.F.);
#75430=ORIENTED_EDGE('',*,*,#52427,.F.);
#75431=ORIENTED_EDGE('',*,*,#52445,.T.);
#75432=ORIENTED_EDGE('',*,*,#50054,.F.);
#75433=ORIENTED_EDGE('',*,*,#52446,.F.);
#75434=ORIENTED_EDGE('',*,*,#52428,.F.);
#75435=ORIENTED_EDGE('',*,*,#52446,.T.);
#75436=ORIENTED_EDGE('',*,*,#50053,.F.);
#75437=ORIENTED_EDGE('',*,*,#52447,.F.);
#75438=ORIENTED_EDGE('',*,*,#52432,.F.);
#75439=ORIENTED_EDGE('',*,*,#52447,.T.);
#75440=ORIENTED_EDGE('',*,*,#50052,.F.);
#75441=ORIENTED_EDGE('',*,*,#52448,.F.);
#75442=ORIENTED_EDGE('',*,*,#52423,.F.);
#75443=ORIENTED_EDGE('',*,*,#52449,.T.);
#75444=ORIENTED_EDGE('',*,*,#52424,.F.);
#75445=ORIENTED_EDGE('',*,*,#52448,.T.);
#75446=ORIENTED_EDGE('',*,*,#50751,.F.);
#75447=ORIENTED_EDGE('',*,*,#52450,.T.);
#75448=ORIENTED_EDGE('',*,*,#52425,.F.);
#75449=ORIENTED_EDGE('',*,*,#52449,.F.);
#75450=ORIENTED_EDGE('',*,*,#50388,.F.);
#75451=ORIENTED_EDGE('',*,*,#52442,.T.);
#75452=ORIENTED_EDGE('',*,*,#52438,.T.);
#75453=ORIENTED_EDGE('',*,*,#52450,.F.);
#75454=ORIENTED_EDGE('',*,*,#50387,.T.);
#75455=ORIENTED_EDGE('',*,*,#52436,.T.);
#75456=ORIENTED_EDGE('',*,*,#52439,.T.);
#75457=ORIENTED_EDGE('',*,*,#52441,.T.);
#75458=ORIENTED_EDGE('',*,*,#52451,.T.);
#75459=ORIENTED_EDGE('',*,*,#52452,.T.);
#75460=ORIENTED_EDGE('',*,*,#52453,.T.);
#75461=ORIENTED_EDGE('',*,*,#52454,.T.);
#75462=ORIENTED_EDGE('',*,*,#52455,.T.);
#75463=ORIENTED_EDGE('',*,*,#52456,.T.);
#75464=ORIENTED_EDGE('',*,*,#52457,.T.);
#75465=ORIENTED_EDGE('',*,*,#52458,.F.);
#75466=ORIENTED_EDGE('',*,*,#52459,.T.);
#75467=ORIENTED_EDGE('',*,*,#52460,.T.);
#75468=ORIENTED_EDGE('',*,*,#52458,.T.);
#75469=ORIENTED_EDGE('',*,*,#52461,.T.);
#75470=ORIENTED_EDGE('',*,*,#52451,.F.);
#75471=ORIENTED_EDGE('',*,*,#52462,.T.);
#75472=ORIENTED_EDGE('',*,*,#52463,.F.);
#75473=ORIENTED_EDGE('',*,*,#52459,.F.);
#75474=ORIENTED_EDGE('',*,*,#52464,.F.);
#75475=ORIENTED_EDGE('',*,*,#52465,.F.);
#75476=ORIENTED_EDGE('',*,*,#52464,.T.);
#75477=ORIENTED_EDGE('',*,*,#52462,.F.);
#75478=ORIENTED_EDGE('',*,*,#52466,.F.);
#75479=ORIENTED_EDGE('',*,*,#52466,.T.);
#75480=ORIENTED_EDGE('',*,*,#52455,.F.);
#75481=ORIENTED_EDGE('',*,*,#52467,.F.);
#75482=ORIENTED_EDGE('',*,*,#52468,.F.);
#75483=ORIENTED_EDGE('',*,*,#52469,.T.);
#75484=ORIENTED_EDGE('',*,*,#52470,.F.);
#75485=ORIENTED_EDGE('',*,*,#52471,.F.);
#75486=ORIENTED_EDGE('',*,*,#50380,.F.);
#75487=ORIENTED_EDGE('',*,*,#52472,.T.);
#75488=ORIENTED_EDGE('',*,*,#52463,.T.);
#75489=ORIENTED_EDGE('',*,*,#52469,.F.);
#75490=ORIENTED_EDGE('',*,*,#50379,.T.);
#75491=ORIENTED_EDGE('',*,*,#52473,.F.);
#75492=ORIENTED_EDGE('',*,*,#52460,.F.);
#75493=ORIENTED_EDGE('',*,*,#52472,.F.);
#75494=ORIENTED_EDGE('',*,*,#50378,.F.);
#75495=ORIENTED_EDGE('',*,*,#52473,.T.);
#75496=ORIENTED_EDGE('',*,*,#50748,.F.);
#75497=ORIENTED_EDGE('',*,*,#52474,.F.);
#75498=ORIENTED_EDGE('',*,*,#52456,.F.);
#75499=ORIENTED_EDGE('',*,*,#52474,.T.);
#75500=ORIENTED_EDGE('',*,*,#50058,.F.);
#75501=ORIENTED_EDGE('',*,*,#52475,.F.);
#75502=ORIENTED_EDGE('',*,*,#52457,.F.);
#75503=ORIENTED_EDGE('',*,*,#52475,.T.);
#75504=ORIENTED_EDGE('',*,*,#50057,.F.);
#75505=ORIENTED_EDGE('',*,*,#52476,.F.);
#75506=ORIENTED_EDGE('',*,*,#52461,.F.);
#75507=ORIENTED_EDGE('',*,*,#52476,.T.);
#75508=ORIENTED_EDGE('',*,*,#50056,.F.);
#75509=ORIENTED_EDGE('',*,*,#52477,.F.);
#75510=ORIENTED_EDGE('',*,*,#52452,.F.);
#75511=ORIENTED_EDGE('',*,*,#52478,.T.);
#75512=ORIENTED_EDGE('',*,*,#52453,.F.);
#75513=ORIENTED_EDGE('',*,*,#52477,.T.);
#75514=ORIENTED_EDGE('',*,*,#50749,.F.);
#75515=ORIENTED_EDGE('',*,*,#52479,.T.);
#75516=ORIENTED_EDGE('',*,*,#52454,.F.);
#75517=ORIENTED_EDGE('',*,*,#52478,.F.);
#75518=ORIENTED_EDGE('',*,*,#50382,.F.);
#75519=ORIENTED_EDGE('',*,*,#52471,.T.);
#75520=ORIENTED_EDGE('',*,*,#52467,.T.);
#75521=ORIENTED_EDGE('',*,*,#52479,.F.);
#75522=ORIENTED_EDGE('',*,*,#50381,.T.);
#75523=ORIENTED_EDGE('',*,*,#52465,.T.);
#75524=ORIENTED_EDGE('',*,*,#52468,.T.);
#75525=ORIENTED_EDGE('',*,*,#52470,.T.);
#75526=ORIENTED_EDGE('',*,*,#52480,.T.);
#75527=ORIENTED_EDGE('',*,*,#52481,.T.);
#75528=ORIENTED_EDGE('',*,*,#52482,.T.);
#75529=ORIENTED_EDGE('',*,*,#52483,.T.);
#75530=ORIENTED_EDGE('',*,*,#52484,.T.);
#75531=ORIENTED_EDGE('',*,*,#52485,.T.);
#75532=ORIENTED_EDGE('',*,*,#52486,.T.);
#75533=ORIENTED_EDGE('',*,*,#52487,.F.);
#75534=ORIENTED_EDGE('',*,*,#52488,.T.);
#75535=ORIENTED_EDGE('',*,*,#52489,.T.);
#75536=ORIENTED_EDGE('',*,*,#52487,.T.);
#75537=ORIENTED_EDGE('',*,*,#52490,.T.);
#75538=ORIENTED_EDGE('',*,*,#52480,.F.);
#75539=ORIENTED_EDGE('',*,*,#52491,.T.);
#75540=ORIENTED_EDGE('',*,*,#52492,.F.);
#75541=ORIENTED_EDGE('',*,*,#52488,.F.);
#75542=ORIENTED_EDGE('',*,*,#52493,.F.);
#75543=ORIENTED_EDGE('',*,*,#52494,.F.);
#75544=ORIENTED_EDGE('',*,*,#52493,.T.);
#75545=ORIENTED_EDGE('',*,*,#52491,.F.);
#75546=ORIENTED_EDGE('',*,*,#52495,.F.);
#75547=ORIENTED_EDGE('',*,*,#52495,.T.);
#75548=ORIENTED_EDGE('',*,*,#52484,.F.);
#75549=ORIENTED_EDGE('',*,*,#52496,.F.);
#75550=ORIENTED_EDGE('',*,*,#52497,.F.);
#75551=ORIENTED_EDGE('',*,*,#52498,.T.);
#75552=ORIENTED_EDGE('',*,*,#52499,.F.);
#75553=ORIENTED_EDGE('',*,*,#52500,.F.);
#75554=ORIENTED_EDGE('',*,*,#50374,.F.);
#75555=ORIENTED_EDGE('',*,*,#52501,.T.);
#75556=ORIENTED_EDGE('',*,*,#52492,.T.);
#75557=ORIENTED_EDGE('',*,*,#52498,.F.);
#75558=ORIENTED_EDGE('',*,*,#50373,.T.);
#75559=ORIENTED_EDGE('',*,*,#52502,.F.);
#75560=ORIENTED_EDGE('',*,*,#52489,.F.);
#75561=ORIENTED_EDGE('',*,*,#52501,.F.);
#75562=ORIENTED_EDGE('',*,*,#50372,.F.);
#75563=ORIENTED_EDGE('',*,*,#52502,.T.);
#75564=ORIENTED_EDGE('',*,*,#50746,.F.);
#75565=ORIENTED_EDGE('',*,*,#52503,.F.);
#75566=ORIENTED_EDGE('',*,*,#52485,.F.);
#75567=ORIENTED_EDGE('',*,*,#52503,.T.);
#75568=ORIENTED_EDGE('',*,*,#50062,.F.);
#75569=ORIENTED_EDGE('',*,*,#52504,.F.);
#75570=ORIENTED_EDGE('',*,*,#52486,.F.);
#75571=ORIENTED_EDGE('',*,*,#52504,.T.);
#75572=ORIENTED_EDGE('',*,*,#50061,.F.);
#75573=ORIENTED_EDGE('',*,*,#52505,.F.);
#75574=ORIENTED_EDGE('',*,*,#52490,.F.);
#75575=ORIENTED_EDGE('',*,*,#52505,.T.);
#75576=ORIENTED_EDGE('',*,*,#50060,.F.);
#75577=ORIENTED_EDGE('',*,*,#52506,.F.);
#75578=ORIENTED_EDGE('',*,*,#52481,.F.);
#75579=ORIENTED_EDGE('',*,*,#52507,.T.);
#75580=ORIENTED_EDGE('',*,*,#52482,.F.);
#75581=ORIENTED_EDGE('',*,*,#52506,.T.);
#75582=ORIENTED_EDGE('',*,*,#50747,.F.);
#75583=ORIENTED_EDGE('',*,*,#52508,.T.);
#75584=ORIENTED_EDGE('',*,*,#52483,.F.);
#75585=ORIENTED_EDGE('',*,*,#52507,.F.);
#75586=ORIENTED_EDGE('',*,*,#50376,.F.);
#75587=ORIENTED_EDGE('',*,*,#52500,.T.);
#75588=ORIENTED_EDGE('',*,*,#52496,.T.);
#75589=ORIENTED_EDGE('',*,*,#52508,.F.);
#75590=ORIENTED_EDGE('',*,*,#50375,.T.);
#75591=ORIENTED_EDGE('',*,*,#52494,.T.);
#75592=ORIENTED_EDGE('',*,*,#52497,.T.);
#75593=ORIENTED_EDGE('',*,*,#52499,.T.);
#75594=ORIENTED_EDGE('',*,*,#52509,.T.);
#75595=ORIENTED_EDGE('',*,*,#52510,.T.);
#75596=ORIENTED_EDGE('',*,*,#52511,.T.);
#75597=ORIENTED_EDGE('',*,*,#52512,.T.);
#75598=ORIENTED_EDGE('',*,*,#52513,.T.);
#75599=ORIENTED_EDGE('',*,*,#52514,.T.);
#75600=ORIENTED_EDGE('',*,*,#52515,.T.);
#75601=ORIENTED_EDGE('',*,*,#52516,.F.);
#75602=ORIENTED_EDGE('',*,*,#52517,.T.);
#75603=ORIENTED_EDGE('',*,*,#52518,.T.);
#75604=ORIENTED_EDGE('',*,*,#52516,.T.);
#75605=ORIENTED_EDGE('',*,*,#52519,.T.);
#75606=ORIENTED_EDGE('',*,*,#52509,.F.);
#75607=ORIENTED_EDGE('',*,*,#52520,.T.);
#75608=ORIENTED_EDGE('',*,*,#52521,.F.);
#75609=ORIENTED_EDGE('',*,*,#52517,.F.);
#75610=ORIENTED_EDGE('',*,*,#52522,.F.);
#75611=ORIENTED_EDGE('',*,*,#52523,.F.);
#75612=ORIENTED_EDGE('',*,*,#52522,.T.);
#75613=ORIENTED_EDGE('',*,*,#52520,.F.);
#75614=ORIENTED_EDGE('',*,*,#52524,.F.);
#75615=ORIENTED_EDGE('',*,*,#52524,.T.);
#75616=ORIENTED_EDGE('',*,*,#52513,.F.);
#75617=ORIENTED_EDGE('',*,*,#52525,.F.);
#75618=ORIENTED_EDGE('',*,*,#52526,.F.);
#75619=ORIENTED_EDGE('',*,*,#52527,.T.);
#75620=ORIENTED_EDGE('',*,*,#52528,.F.);
#75621=ORIENTED_EDGE('',*,*,#52529,.F.);
#75622=ORIENTED_EDGE('',*,*,#50368,.F.);
#75623=ORIENTED_EDGE('',*,*,#52530,.T.);
#75624=ORIENTED_EDGE('',*,*,#52521,.T.);
#75625=ORIENTED_EDGE('',*,*,#52527,.F.);
#75626=ORIENTED_EDGE('',*,*,#50367,.T.);
#75627=ORIENTED_EDGE('',*,*,#52531,.F.);
#75628=ORIENTED_EDGE('',*,*,#52518,.F.);
#75629=ORIENTED_EDGE('',*,*,#52530,.F.);
#75630=ORIENTED_EDGE('',*,*,#50366,.F.);
#75631=ORIENTED_EDGE('',*,*,#52531,.T.);
#75632=ORIENTED_EDGE('',*,*,#50744,.F.);
#75633=ORIENTED_EDGE('',*,*,#52532,.F.);
#75634=ORIENTED_EDGE('',*,*,#52514,.F.);
#75635=ORIENTED_EDGE('',*,*,#52532,.T.);
#75636=ORIENTED_EDGE('',*,*,#50066,.F.);
#75637=ORIENTED_EDGE('',*,*,#52533,.F.);
#75638=ORIENTED_EDGE('',*,*,#52515,.F.);
#75639=ORIENTED_EDGE('',*,*,#52533,.T.);
#75640=ORIENTED_EDGE('',*,*,#50065,.F.);
#75641=ORIENTED_EDGE('',*,*,#52534,.F.);
#75642=ORIENTED_EDGE('',*,*,#52519,.F.);
#75643=ORIENTED_EDGE('',*,*,#52534,.T.);
#75644=ORIENTED_EDGE('',*,*,#50064,.F.);
#75645=ORIENTED_EDGE('',*,*,#52535,.F.);
#75646=ORIENTED_EDGE('',*,*,#52510,.F.);
#75647=ORIENTED_EDGE('',*,*,#52536,.T.);
#75648=ORIENTED_EDGE('',*,*,#52511,.F.);
#75649=ORIENTED_EDGE('',*,*,#52535,.T.);
#75650=ORIENTED_EDGE('',*,*,#50745,.F.);
#75651=ORIENTED_EDGE('',*,*,#52537,.T.);
#75652=ORIENTED_EDGE('',*,*,#52512,.F.);
#75653=ORIENTED_EDGE('',*,*,#52536,.F.);
#75654=ORIENTED_EDGE('',*,*,#50370,.F.);
#75655=ORIENTED_EDGE('',*,*,#52529,.T.);
#75656=ORIENTED_EDGE('',*,*,#52525,.T.);
#75657=ORIENTED_EDGE('',*,*,#52537,.F.);
#75658=ORIENTED_EDGE('',*,*,#50369,.T.);
#75659=ORIENTED_EDGE('',*,*,#52523,.T.);
#75660=ORIENTED_EDGE('',*,*,#52526,.T.);
#75661=ORIENTED_EDGE('',*,*,#52528,.T.);
#75662=ORIENTED_EDGE('',*,*,#52538,.T.);
#75663=ORIENTED_EDGE('',*,*,#52539,.T.);
#75664=ORIENTED_EDGE('',*,*,#52540,.T.);
#75665=ORIENTED_EDGE('',*,*,#52541,.T.);
#75666=ORIENTED_EDGE('',*,*,#52542,.T.);
#75667=ORIENTED_EDGE('',*,*,#52543,.T.);
#75668=ORIENTED_EDGE('',*,*,#52544,.T.);
#75669=ORIENTED_EDGE('',*,*,#52545,.F.);
#75670=ORIENTED_EDGE('',*,*,#52546,.T.);
#75671=ORIENTED_EDGE('',*,*,#52547,.T.);
#75672=ORIENTED_EDGE('',*,*,#52545,.T.);
#75673=ORIENTED_EDGE('',*,*,#52548,.T.);
#75674=ORIENTED_EDGE('',*,*,#52538,.F.);
#75675=ORIENTED_EDGE('',*,*,#52549,.T.);
#75676=ORIENTED_EDGE('',*,*,#52550,.F.);
#75677=ORIENTED_EDGE('',*,*,#52546,.F.);
#75678=ORIENTED_EDGE('',*,*,#52551,.F.);
#75679=ORIENTED_EDGE('',*,*,#52552,.F.);
#75680=ORIENTED_EDGE('',*,*,#52551,.T.);
#75681=ORIENTED_EDGE('',*,*,#52549,.F.);
#75682=ORIENTED_EDGE('',*,*,#52553,.F.);
#75683=ORIENTED_EDGE('',*,*,#52553,.T.);
#75684=ORIENTED_EDGE('',*,*,#52542,.F.);
#75685=ORIENTED_EDGE('',*,*,#52554,.F.);
#75686=ORIENTED_EDGE('',*,*,#52555,.F.);
#75687=ORIENTED_EDGE('',*,*,#52556,.T.);
#75688=ORIENTED_EDGE('',*,*,#52557,.F.);
#75689=ORIENTED_EDGE('',*,*,#52558,.F.);
#75690=ORIENTED_EDGE('',*,*,#50360,.F.);
#75691=ORIENTED_EDGE('',*,*,#52559,.T.);
#75692=ORIENTED_EDGE('',*,*,#52550,.T.);
#75693=ORIENTED_EDGE('',*,*,#52556,.F.);
#75694=ORIENTED_EDGE('',*,*,#50359,.T.);
#75695=ORIENTED_EDGE('',*,*,#52560,.F.);
#75696=ORIENTED_EDGE('',*,*,#52547,.F.);
#75697=ORIENTED_EDGE('',*,*,#52559,.F.);
#75698=ORIENTED_EDGE('',*,*,#50358,.F.);
#75699=ORIENTED_EDGE('',*,*,#52560,.T.);
#75700=ORIENTED_EDGE('',*,*,#50742,.F.);
#75701=ORIENTED_EDGE('',*,*,#52561,.F.);
#75702=ORIENTED_EDGE('',*,*,#52543,.F.);
#75703=ORIENTED_EDGE('',*,*,#52561,.T.);
#75704=ORIENTED_EDGE('',*,*,#49674,.F.);
#75705=ORIENTED_EDGE('',*,*,#52562,.F.);
#75706=ORIENTED_EDGE('',*,*,#52544,.F.);
#75707=ORIENTED_EDGE('',*,*,#52562,.T.);
#75708=ORIENTED_EDGE('',*,*,#49673,.F.);
#75709=ORIENTED_EDGE('',*,*,#52563,.F.);
#75710=ORIENTED_EDGE('',*,*,#52548,.F.);
#75711=ORIENTED_EDGE('',*,*,#52563,.T.);
#75712=ORIENTED_EDGE('',*,*,#49672,.F.);
#75713=ORIENTED_EDGE('',*,*,#52564,.F.);
#75714=ORIENTED_EDGE('',*,*,#52539,.F.);
#75715=ORIENTED_EDGE('',*,*,#52565,.T.);
#75716=ORIENTED_EDGE('',*,*,#52540,.F.);
#75717=ORIENTED_EDGE('',*,*,#52564,.T.);
#75718=ORIENTED_EDGE('',*,*,#50743,.F.);
#75719=ORIENTED_EDGE('',*,*,#52566,.T.);
#75720=ORIENTED_EDGE('',*,*,#52541,.F.);
#75721=ORIENTED_EDGE('',*,*,#52565,.F.);
#75722=ORIENTED_EDGE('',*,*,#50362,.F.);
#75723=ORIENTED_EDGE('',*,*,#52558,.T.);
#75724=ORIENTED_EDGE('',*,*,#52554,.T.);
#75725=ORIENTED_EDGE('',*,*,#52566,.F.);
#75726=ORIENTED_EDGE('',*,*,#50361,.T.);
#75727=ORIENTED_EDGE('',*,*,#52552,.T.);
#75728=ORIENTED_EDGE('',*,*,#52555,.T.);
#75729=ORIENTED_EDGE('',*,*,#52557,.T.);
#75730=ORIENTED_EDGE('',*,*,#52567,.T.);
#75731=ORIENTED_EDGE('',*,*,#52568,.T.);
#75732=ORIENTED_EDGE('',*,*,#52569,.T.);
#75733=ORIENTED_EDGE('',*,*,#52570,.T.);
#75734=ORIENTED_EDGE('',*,*,#52571,.T.);
#75735=ORIENTED_EDGE('',*,*,#52572,.T.);
#75736=ORIENTED_EDGE('',*,*,#52573,.T.);
#75737=ORIENTED_EDGE('',*,*,#52574,.F.);
#75738=ORIENTED_EDGE('',*,*,#52575,.T.);
#75739=ORIENTED_EDGE('',*,*,#52576,.T.);
#75740=ORIENTED_EDGE('',*,*,#52574,.T.);
#75741=ORIENTED_EDGE('',*,*,#52577,.T.);
#75742=ORIENTED_EDGE('',*,*,#52567,.F.);
#75743=ORIENTED_EDGE('',*,*,#52578,.T.);
#75744=ORIENTED_EDGE('',*,*,#52579,.F.);
#75745=ORIENTED_EDGE('',*,*,#52575,.F.);
#75746=ORIENTED_EDGE('',*,*,#52580,.F.);
#75747=ORIENTED_EDGE('',*,*,#52581,.F.);
#75748=ORIENTED_EDGE('',*,*,#52580,.T.);
#75749=ORIENTED_EDGE('',*,*,#52578,.F.);
#75750=ORIENTED_EDGE('',*,*,#52582,.F.);
#75751=ORIENTED_EDGE('',*,*,#52582,.T.);
#75752=ORIENTED_EDGE('',*,*,#52571,.F.);
#75753=ORIENTED_EDGE('',*,*,#52583,.F.);
#75754=ORIENTED_EDGE('',*,*,#52584,.F.);
#75755=ORIENTED_EDGE('',*,*,#52585,.T.);
#75756=ORIENTED_EDGE('',*,*,#52586,.F.);
#75757=ORIENTED_EDGE('',*,*,#52587,.F.);
#75758=ORIENTED_EDGE('',*,*,#50354,.F.);
#75759=ORIENTED_EDGE('',*,*,#52588,.T.);
#75760=ORIENTED_EDGE('',*,*,#52579,.T.);
#75761=ORIENTED_EDGE('',*,*,#52585,.F.);
#75762=ORIENTED_EDGE('',*,*,#50353,.T.);
#75763=ORIENTED_EDGE('',*,*,#52589,.F.);
#75764=ORIENTED_EDGE('',*,*,#52576,.F.);
#75765=ORIENTED_EDGE('',*,*,#52588,.F.);
#75766=ORIENTED_EDGE('',*,*,#50352,.F.);
#75767=ORIENTED_EDGE('',*,*,#52589,.T.);
#75768=ORIENTED_EDGE('',*,*,#50740,.F.);
#75769=ORIENTED_EDGE('',*,*,#52590,.F.);
#75770=ORIENTED_EDGE('',*,*,#52572,.F.);
#75771=ORIENTED_EDGE('',*,*,#52590,.T.);
#75772=ORIENTED_EDGE('',*,*,#49678,.F.);
#75773=ORIENTED_EDGE('',*,*,#52591,.F.);
#75774=ORIENTED_EDGE('',*,*,#52573,.F.);
#75775=ORIENTED_EDGE('',*,*,#52591,.T.);
#75776=ORIENTED_EDGE('',*,*,#49677,.F.);
#75777=ORIENTED_EDGE('',*,*,#52592,.F.);
#75778=ORIENTED_EDGE('',*,*,#52577,.F.);
#75779=ORIENTED_EDGE('',*,*,#52592,.T.);
#75780=ORIENTED_EDGE('',*,*,#49676,.F.);
#75781=ORIENTED_EDGE('',*,*,#52593,.F.);
#75782=ORIENTED_EDGE('',*,*,#52568,.F.);
#75783=ORIENTED_EDGE('',*,*,#52594,.T.);
#75784=ORIENTED_EDGE('',*,*,#52569,.F.);
#75785=ORIENTED_EDGE('',*,*,#52593,.T.);
#75786=ORIENTED_EDGE('',*,*,#50741,.F.);
#75787=ORIENTED_EDGE('',*,*,#52595,.T.);
#75788=ORIENTED_EDGE('',*,*,#52570,.F.);
#75789=ORIENTED_EDGE('',*,*,#52594,.F.);
#75790=ORIENTED_EDGE('',*,*,#50356,.F.);
#75791=ORIENTED_EDGE('',*,*,#52587,.T.);
#75792=ORIENTED_EDGE('',*,*,#52583,.T.);
#75793=ORIENTED_EDGE('',*,*,#52595,.F.);
#75794=ORIENTED_EDGE('',*,*,#50355,.T.);
#75795=ORIENTED_EDGE('',*,*,#52581,.T.);
#75796=ORIENTED_EDGE('',*,*,#52584,.T.);
#75797=ORIENTED_EDGE('',*,*,#52586,.T.);
#75798=ORIENTED_EDGE('',*,*,#52596,.T.);
#75799=ORIENTED_EDGE('',*,*,#52597,.T.);
#75800=ORIENTED_EDGE('',*,*,#52598,.T.);
#75801=ORIENTED_EDGE('',*,*,#52599,.T.);
#75802=ORIENTED_EDGE('',*,*,#52600,.T.);
#75803=ORIENTED_EDGE('',*,*,#52601,.T.);
#75804=ORIENTED_EDGE('',*,*,#52602,.T.);
#75805=ORIENTED_EDGE('',*,*,#52603,.F.);
#75806=ORIENTED_EDGE('',*,*,#52604,.T.);
#75807=ORIENTED_EDGE('',*,*,#52605,.T.);
#75808=ORIENTED_EDGE('',*,*,#52603,.T.);
#75809=ORIENTED_EDGE('',*,*,#52606,.T.);
#75810=ORIENTED_EDGE('',*,*,#52596,.F.);
#75811=ORIENTED_EDGE('',*,*,#52607,.T.);
#75812=ORIENTED_EDGE('',*,*,#52608,.F.);
#75813=ORIENTED_EDGE('',*,*,#52604,.F.);
#75814=ORIENTED_EDGE('',*,*,#52609,.F.);
#75815=ORIENTED_EDGE('',*,*,#52610,.F.);
#75816=ORIENTED_EDGE('',*,*,#52609,.T.);
#75817=ORIENTED_EDGE('',*,*,#52607,.F.);
#75818=ORIENTED_EDGE('',*,*,#52611,.F.);
#75819=ORIENTED_EDGE('',*,*,#52611,.T.);
#75820=ORIENTED_EDGE('',*,*,#52600,.F.);
#75821=ORIENTED_EDGE('',*,*,#52612,.F.);
#75822=ORIENTED_EDGE('',*,*,#52613,.F.);
#75823=ORIENTED_EDGE('',*,*,#52614,.T.);
#75824=ORIENTED_EDGE('',*,*,#52615,.F.);
#75825=ORIENTED_EDGE('',*,*,#52616,.F.);
#75826=ORIENTED_EDGE('',*,*,#50348,.F.);
#75827=ORIENTED_EDGE('',*,*,#52617,.T.);
#75828=ORIENTED_EDGE('',*,*,#52608,.T.);
#75829=ORIENTED_EDGE('',*,*,#52614,.F.);
#75830=ORIENTED_EDGE('',*,*,#50347,.T.);
#75831=ORIENTED_EDGE('',*,*,#52618,.F.);
#75832=ORIENTED_EDGE('',*,*,#52605,.F.);
#75833=ORIENTED_EDGE('',*,*,#52617,.F.);
#75834=ORIENTED_EDGE('',*,*,#50346,.F.);
#75835=ORIENTED_EDGE('',*,*,#52618,.T.);
#75836=ORIENTED_EDGE('',*,*,#50738,.F.);
#75837=ORIENTED_EDGE('',*,*,#52619,.F.);
#75838=ORIENTED_EDGE('',*,*,#52601,.F.);
#75839=ORIENTED_EDGE('',*,*,#52619,.T.);
#75840=ORIENTED_EDGE('',*,*,#49682,.F.);
#75841=ORIENTED_EDGE('',*,*,#52620,.F.);
#75842=ORIENTED_EDGE('',*,*,#52602,.F.);
#75843=ORIENTED_EDGE('',*,*,#52620,.T.);
#75844=ORIENTED_EDGE('',*,*,#49681,.F.);
#75845=ORIENTED_EDGE('',*,*,#52621,.F.);
#75846=ORIENTED_EDGE('',*,*,#52606,.F.);
#75847=ORIENTED_EDGE('',*,*,#52621,.T.);
#75848=ORIENTED_EDGE('',*,*,#49680,.F.);
#75849=ORIENTED_EDGE('',*,*,#52622,.F.);
#75850=ORIENTED_EDGE('',*,*,#52597,.F.);
#75851=ORIENTED_EDGE('',*,*,#52623,.T.);
#75852=ORIENTED_EDGE('',*,*,#52598,.F.);
#75853=ORIENTED_EDGE('',*,*,#52622,.T.);
#75854=ORIENTED_EDGE('',*,*,#50739,.F.);
#75855=ORIENTED_EDGE('',*,*,#52624,.T.);
#75856=ORIENTED_EDGE('',*,*,#52599,.F.);
#75857=ORIENTED_EDGE('',*,*,#52623,.F.);
#75858=ORIENTED_EDGE('',*,*,#50350,.F.);
#75859=ORIENTED_EDGE('',*,*,#52616,.T.);
#75860=ORIENTED_EDGE('',*,*,#52612,.T.);
#75861=ORIENTED_EDGE('',*,*,#52624,.F.);
#75862=ORIENTED_EDGE('',*,*,#50349,.T.);
#75863=ORIENTED_EDGE('',*,*,#52610,.T.);
#75864=ORIENTED_EDGE('',*,*,#52613,.T.);
#75865=ORIENTED_EDGE('',*,*,#52615,.T.);
#75866=ORIENTED_EDGE('',*,*,#52625,.T.);
#75867=ORIENTED_EDGE('',*,*,#52626,.T.);
#75868=ORIENTED_EDGE('',*,*,#52627,.T.);
#75869=ORIENTED_EDGE('',*,*,#52628,.T.);
#75870=ORIENTED_EDGE('',*,*,#52629,.T.);
#75871=ORIENTED_EDGE('',*,*,#52630,.T.);
#75872=ORIENTED_EDGE('',*,*,#52631,.T.);
#75873=ORIENTED_EDGE('',*,*,#52632,.F.);
#75874=ORIENTED_EDGE('',*,*,#52633,.T.);
#75875=ORIENTED_EDGE('',*,*,#52634,.T.);
#75876=ORIENTED_EDGE('',*,*,#52632,.T.);
#75877=ORIENTED_EDGE('',*,*,#52635,.T.);
#75878=ORIENTED_EDGE('',*,*,#52625,.F.);
#75879=ORIENTED_EDGE('',*,*,#52636,.T.);
#75880=ORIENTED_EDGE('',*,*,#52637,.F.);
#75881=ORIENTED_EDGE('',*,*,#52633,.F.);
#75882=ORIENTED_EDGE('',*,*,#52638,.F.);
#75883=ORIENTED_EDGE('',*,*,#52639,.F.);
#75884=ORIENTED_EDGE('',*,*,#52638,.T.);
#75885=ORIENTED_EDGE('',*,*,#52636,.F.);
#75886=ORIENTED_EDGE('',*,*,#52640,.F.);
#75887=ORIENTED_EDGE('',*,*,#52640,.T.);
#75888=ORIENTED_EDGE('',*,*,#52629,.F.);
#75889=ORIENTED_EDGE('',*,*,#52641,.F.);
#75890=ORIENTED_EDGE('',*,*,#52642,.F.);
#75891=ORIENTED_EDGE('',*,*,#52643,.T.);
#75892=ORIENTED_EDGE('',*,*,#52644,.F.);
#75893=ORIENTED_EDGE('',*,*,#52645,.F.);
#75894=ORIENTED_EDGE('',*,*,#50342,.F.);
#75895=ORIENTED_EDGE('',*,*,#52646,.T.);
#75896=ORIENTED_EDGE('',*,*,#52637,.T.);
#75897=ORIENTED_EDGE('',*,*,#52643,.F.);
#75898=ORIENTED_EDGE('',*,*,#50341,.T.);
#75899=ORIENTED_EDGE('',*,*,#52647,.F.);
#75900=ORIENTED_EDGE('',*,*,#52634,.F.);
#75901=ORIENTED_EDGE('',*,*,#52646,.F.);
#75902=ORIENTED_EDGE('',*,*,#50340,.F.);
#75903=ORIENTED_EDGE('',*,*,#52647,.T.);
#75904=ORIENTED_EDGE('',*,*,#50736,.F.);
#75905=ORIENTED_EDGE('',*,*,#52648,.F.);
#75906=ORIENTED_EDGE('',*,*,#52630,.F.);
#75907=ORIENTED_EDGE('',*,*,#52648,.T.);
#75908=ORIENTED_EDGE('',*,*,#49686,.F.);
#75909=ORIENTED_EDGE('',*,*,#52649,.F.);
#75910=ORIENTED_EDGE('',*,*,#52631,.F.);
#75911=ORIENTED_EDGE('',*,*,#52649,.T.);
#75912=ORIENTED_EDGE('',*,*,#49685,.F.);
#75913=ORIENTED_EDGE('',*,*,#52650,.F.);
#75914=ORIENTED_EDGE('',*,*,#52635,.F.);
#75915=ORIENTED_EDGE('',*,*,#52650,.T.);
#75916=ORIENTED_EDGE('',*,*,#49684,.F.);
#75917=ORIENTED_EDGE('',*,*,#52651,.F.);
#75918=ORIENTED_EDGE('',*,*,#52626,.F.);
#75919=ORIENTED_EDGE('',*,*,#52652,.T.);
#75920=ORIENTED_EDGE('',*,*,#52627,.F.);
#75921=ORIENTED_EDGE('',*,*,#52651,.T.);
#75922=ORIENTED_EDGE('',*,*,#50737,.F.);
#75923=ORIENTED_EDGE('',*,*,#52653,.T.);
#75924=ORIENTED_EDGE('',*,*,#52628,.F.);
#75925=ORIENTED_EDGE('',*,*,#52652,.F.);
#75926=ORIENTED_EDGE('',*,*,#50344,.F.);
#75927=ORIENTED_EDGE('',*,*,#52645,.T.);
#75928=ORIENTED_EDGE('',*,*,#52641,.T.);
#75929=ORIENTED_EDGE('',*,*,#52653,.F.);
#75930=ORIENTED_EDGE('',*,*,#50343,.T.);
#75931=ORIENTED_EDGE('',*,*,#52639,.T.);
#75932=ORIENTED_EDGE('',*,*,#52642,.T.);
#75933=ORIENTED_EDGE('',*,*,#52644,.T.);
#75934=ORIENTED_EDGE('',*,*,#52654,.T.);
#75935=ORIENTED_EDGE('',*,*,#52655,.T.);
#75936=ORIENTED_EDGE('',*,*,#52656,.T.);
#75937=ORIENTED_EDGE('',*,*,#52657,.T.);
#75938=ORIENTED_EDGE('',*,*,#52658,.T.);
#75939=ORIENTED_EDGE('',*,*,#52659,.T.);
#75940=ORIENTED_EDGE('',*,*,#52660,.T.);
#75941=ORIENTED_EDGE('',*,*,#52661,.F.);
#75942=ORIENTED_EDGE('',*,*,#52662,.T.);
#75943=ORIENTED_EDGE('',*,*,#52663,.T.);
#75944=ORIENTED_EDGE('',*,*,#52661,.T.);
#75945=ORIENTED_EDGE('',*,*,#52664,.T.);
#75946=ORIENTED_EDGE('',*,*,#52654,.F.);
#75947=ORIENTED_EDGE('',*,*,#52665,.T.);
#75948=ORIENTED_EDGE('',*,*,#52666,.F.);
#75949=ORIENTED_EDGE('',*,*,#52662,.F.);
#75950=ORIENTED_EDGE('',*,*,#52667,.F.);
#75951=ORIENTED_EDGE('',*,*,#52668,.F.);
#75952=ORIENTED_EDGE('',*,*,#52667,.T.);
#75953=ORIENTED_EDGE('',*,*,#52665,.F.);
#75954=ORIENTED_EDGE('',*,*,#52669,.F.);
#75955=ORIENTED_EDGE('',*,*,#52669,.T.);
#75956=ORIENTED_EDGE('',*,*,#52658,.F.);
#75957=ORIENTED_EDGE('',*,*,#52670,.F.);
#75958=ORIENTED_EDGE('',*,*,#52671,.F.);
#75959=ORIENTED_EDGE('',*,*,#52672,.T.);
#75960=ORIENTED_EDGE('',*,*,#52673,.F.);
#75961=ORIENTED_EDGE('',*,*,#52674,.F.);
#75962=ORIENTED_EDGE('',*,*,#50336,.F.);
#75963=ORIENTED_EDGE('',*,*,#52675,.T.);
#75964=ORIENTED_EDGE('',*,*,#52666,.T.);
#75965=ORIENTED_EDGE('',*,*,#52672,.F.);
#75966=ORIENTED_EDGE('',*,*,#50335,.T.);
#75967=ORIENTED_EDGE('',*,*,#52676,.F.);
#75968=ORIENTED_EDGE('',*,*,#52663,.F.);
#75969=ORIENTED_EDGE('',*,*,#52675,.F.);
#75970=ORIENTED_EDGE('',*,*,#50334,.F.);
#75971=ORIENTED_EDGE('',*,*,#52676,.T.);
#75972=ORIENTED_EDGE('',*,*,#50734,.F.);
#75973=ORIENTED_EDGE('',*,*,#52677,.F.);
#75974=ORIENTED_EDGE('',*,*,#52659,.F.);
#75975=ORIENTED_EDGE('',*,*,#52677,.T.);
#75976=ORIENTED_EDGE('',*,*,#49690,.F.);
#75977=ORIENTED_EDGE('',*,*,#52678,.F.);
#75978=ORIENTED_EDGE('',*,*,#52660,.F.);
#75979=ORIENTED_EDGE('',*,*,#52678,.T.);
#75980=ORIENTED_EDGE('',*,*,#49689,.F.);
#75981=ORIENTED_EDGE('',*,*,#52679,.F.);
#75982=ORIENTED_EDGE('',*,*,#52664,.F.);
#75983=ORIENTED_EDGE('',*,*,#52679,.T.);
#75984=ORIENTED_EDGE('',*,*,#49688,.F.);
#75985=ORIENTED_EDGE('',*,*,#52680,.F.);
#75986=ORIENTED_EDGE('',*,*,#52655,.F.);
#75987=ORIENTED_EDGE('',*,*,#52681,.T.);
#75988=ORIENTED_EDGE('',*,*,#52656,.F.);
#75989=ORIENTED_EDGE('',*,*,#52680,.T.);
#75990=ORIENTED_EDGE('',*,*,#50735,.F.);
#75991=ORIENTED_EDGE('',*,*,#52682,.T.);
#75992=ORIENTED_EDGE('',*,*,#52657,.F.);
#75993=ORIENTED_EDGE('',*,*,#52681,.F.);
#75994=ORIENTED_EDGE('',*,*,#50338,.F.);
#75995=ORIENTED_EDGE('',*,*,#52674,.T.);
#75996=ORIENTED_EDGE('',*,*,#52670,.T.);
#75997=ORIENTED_EDGE('',*,*,#52682,.F.);
#75998=ORIENTED_EDGE('',*,*,#50337,.T.);
#75999=ORIENTED_EDGE('',*,*,#52668,.T.);
#76000=ORIENTED_EDGE('',*,*,#52671,.T.);
#76001=ORIENTED_EDGE('',*,*,#52673,.T.);
#76002=ORIENTED_EDGE('',*,*,#52683,.T.);
#76003=ORIENTED_EDGE('',*,*,#52684,.T.);
#76004=ORIENTED_EDGE('',*,*,#52685,.T.);
#76005=ORIENTED_EDGE('',*,*,#52686,.T.);
#76006=ORIENTED_EDGE('',*,*,#52687,.T.);
#76007=ORIENTED_EDGE('',*,*,#52688,.T.);
#76008=ORIENTED_EDGE('',*,*,#52689,.T.);
#76009=ORIENTED_EDGE('',*,*,#52690,.F.);
#76010=ORIENTED_EDGE('',*,*,#52691,.T.);
#76011=ORIENTED_EDGE('',*,*,#52692,.T.);
#76012=ORIENTED_EDGE('',*,*,#52690,.T.);
#76013=ORIENTED_EDGE('',*,*,#52693,.T.);
#76014=ORIENTED_EDGE('',*,*,#52683,.F.);
#76015=ORIENTED_EDGE('',*,*,#52694,.T.);
#76016=ORIENTED_EDGE('',*,*,#52695,.F.);
#76017=ORIENTED_EDGE('',*,*,#52691,.F.);
#76018=ORIENTED_EDGE('',*,*,#52696,.F.);
#76019=ORIENTED_EDGE('',*,*,#52697,.F.);
#76020=ORIENTED_EDGE('',*,*,#52696,.T.);
#76021=ORIENTED_EDGE('',*,*,#52694,.F.);
#76022=ORIENTED_EDGE('',*,*,#52698,.F.);
#76023=ORIENTED_EDGE('',*,*,#52698,.T.);
#76024=ORIENTED_EDGE('',*,*,#52687,.F.);
#76025=ORIENTED_EDGE('',*,*,#52699,.F.);
#76026=ORIENTED_EDGE('',*,*,#52700,.F.);
#76027=ORIENTED_EDGE('',*,*,#52701,.T.);
#76028=ORIENTED_EDGE('',*,*,#52702,.F.);
#76029=ORIENTED_EDGE('',*,*,#52703,.F.);
#76030=ORIENTED_EDGE('',*,*,#50330,.F.);
#76031=ORIENTED_EDGE('',*,*,#52704,.T.);
#76032=ORIENTED_EDGE('',*,*,#52695,.T.);
#76033=ORIENTED_EDGE('',*,*,#52701,.F.);
#76034=ORIENTED_EDGE('',*,*,#50329,.T.);
#76035=ORIENTED_EDGE('',*,*,#52705,.F.);
#76036=ORIENTED_EDGE('',*,*,#52692,.F.);
#76037=ORIENTED_EDGE('',*,*,#52704,.F.);
#76038=ORIENTED_EDGE('',*,*,#50328,.F.);
#76039=ORIENTED_EDGE('',*,*,#52705,.T.);
#76040=ORIENTED_EDGE('',*,*,#50732,.F.);
#76041=ORIENTED_EDGE('',*,*,#52706,.F.);
#76042=ORIENTED_EDGE('',*,*,#52688,.F.);
#76043=ORIENTED_EDGE('',*,*,#52706,.T.);
#76044=ORIENTED_EDGE('',*,*,#49694,.F.);
#76045=ORIENTED_EDGE('',*,*,#52707,.F.);
#76046=ORIENTED_EDGE('',*,*,#52689,.F.);
#76047=ORIENTED_EDGE('',*,*,#52707,.T.);
#76048=ORIENTED_EDGE('',*,*,#49693,.F.);
#76049=ORIENTED_EDGE('',*,*,#52708,.F.);
#76050=ORIENTED_EDGE('',*,*,#52693,.F.);
#76051=ORIENTED_EDGE('',*,*,#52708,.T.);
#76052=ORIENTED_EDGE('',*,*,#49692,.F.);
#76053=ORIENTED_EDGE('',*,*,#52709,.F.);
#76054=ORIENTED_EDGE('',*,*,#52684,.F.);
#76055=ORIENTED_EDGE('',*,*,#52710,.T.);
#76056=ORIENTED_EDGE('',*,*,#52685,.F.);
#76057=ORIENTED_EDGE('',*,*,#52709,.T.);
#76058=ORIENTED_EDGE('',*,*,#50733,.F.);
#76059=ORIENTED_EDGE('',*,*,#52711,.T.);
#76060=ORIENTED_EDGE('',*,*,#52686,.F.);
#76061=ORIENTED_EDGE('',*,*,#52710,.F.);
#76062=ORIENTED_EDGE('',*,*,#50332,.F.);
#76063=ORIENTED_EDGE('',*,*,#52703,.T.);
#76064=ORIENTED_EDGE('',*,*,#52699,.T.);
#76065=ORIENTED_EDGE('',*,*,#52711,.F.);
#76066=ORIENTED_EDGE('',*,*,#50331,.T.);
#76067=ORIENTED_EDGE('',*,*,#52697,.T.);
#76068=ORIENTED_EDGE('',*,*,#52700,.T.);
#76069=ORIENTED_EDGE('',*,*,#52702,.T.);
#76070=ORIENTED_EDGE('',*,*,#52712,.T.);
#76071=ORIENTED_EDGE('',*,*,#52713,.T.);
#76072=ORIENTED_EDGE('',*,*,#52714,.T.);
#76073=ORIENTED_EDGE('',*,*,#52715,.T.);
#76074=ORIENTED_EDGE('',*,*,#52716,.T.);
#76075=ORIENTED_EDGE('',*,*,#52717,.T.);
#76076=ORIENTED_EDGE('',*,*,#52718,.T.);
#76077=ORIENTED_EDGE('',*,*,#52719,.F.);
#76078=ORIENTED_EDGE('',*,*,#52720,.T.);
#76079=ORIENTED_EDGE('',*,*,#52721,.T.);
#76080=ORIENTED_EDGE('',*,*,#52719,.T.);
#76081=ORIENTED_EDGE('',*,*,#52722,.T.);
#76082=ORIENTED_EDGE('',*,*,#52712,.F.);
#76083=ORIENTED_EDGE('',*,*,#52723,.T.);
#76084=ORIENTED_EDGE('',*,*,#52724,.F.);
#76085=ORIENTED_EDGE('',*,*,#52720,.F.);
#76086=ORIENTED_EDGE('',*,*,#52725,.F.);
#76087=ORIENTED_EDGE('',*,*,#52726,.F.);
#76088=ORIENTED_EDGE('',*,*,#52725,.T.);
#76089=ORIENTED_EDGE('',*,*,#52723,.F.);
#76090=ORIENTED_EDGE('',*,*,#52727,.F.);
#76091=ORIENTED_EDGE('',*,*,#52727,.T.);
#76092=ORIENTED_EDGE('',*,*,#52716,.F.);
#76093=ORIENTED_EDGE('',*,*,#52728,.F.);
#76094=ORIENTED_EDGE('',*,*,#52729,.F.);
#76095=ORIENTED_EDGE('',*,*,#52730,.T.);
#76096=ORIENTED_EDGE('',*,*,#52731,.F.);
#76097=ORIENTED_EDGE('',*,*,#52732,.F.);
#76098=ORIENTED_EDGE('',*,*,#50324,.F.);
#76099=ORIENTED_EDGE('',*,*,#52733,.T.);
#76100=ORIENTED_EDGE('',*,*,#52724,.T.);
#76101=ORIENTED_EDGE('',*,*,#52730,.F.);
#76102=ORIENTED_EDGE('',*,*,#50323,.T.);
#76103=ORIENTED_EDGE('',*,*,#52734,.F.);
#76104=ORIENTED_EDGE('',*,*,#52721,.F.);
#76105=ORIENTED_EDGE('',*,*,#52733,.F.);
#76106=ORIENTED_EDGE('',*,*,#50322,.F.);
#76107=ORIENTED_EDGE('',*,*,#52734,.T.);
#76108=ORIENTED_EDGE('',*,*,#50730,.F.);
#76109=ORIENTED_EDGE('',*,*,#52735,.F.);
#76110=ORIENTED_EDGE('',*,*,#52717,.F.);
#76111=ORIENTED_EDGE('',*,*,#52735,.T.);
#76112=ORIENTED_EDGE('',*,*,#49698,.F.);
#76113=ORIENTED_EDGE('',*,*,#52736,.F.);
#76114=ORIENTED_EDGE('',*,*,#52718,.F.);
#76115=ORIENTED_EDGE('',*,*,#52736,.T.);
#76116=ORIENTED_EDGE('',*,*,#49697,.F.);
#76117=ORIENTED_EDGE('',*,*,#52737,.F.);
#76118=ORIENTED_EDGE('',*,*,#52722,.F.);
#76119=ORIENTED_EDGE('',*,*,#52737,.T.);
#76120=ORIENTED_EDGE('',*,*,#49696,.F.);
#76121=ORIENTED_EDGE('',*,*,#52738,.F.);
#76122=ORIENTED_EDGE('',*,*,#52713,.F.);
#76123=ORIENTED_EDGE('',*,*,#52739,.T.);
#76124=ORIENTED_EDGE('',*,*,#52714,.F.);
#76125=ORIENTED_EDGE('',*,*,#52738,.T.);
#76126=ORIENTED_EDGE('',*,*,#50731,.F.);
#76127=ORIENTED_EDGE('',*,*,#52740,.T.);
#76128=ORIENTED_EDGE('',*,*,#52715,.F.);
#76129=ORIENTED_EDGE('',*,*,#52739,.F.);
#76130=ORIENTED_EDGE('',*,*,#50326,.F.);
#76131=ORIENTED_EDGE('',*,*,#52732,.T.);
#76132=ORIENTED_EDGE('',*,*,#52728,.T.);
#76133=ORIENTED_EDGE('',*,*,#52740,.F.);
#76134=ORIENTED_EDGE('',*,*,#50325,.T.);
#76135=ORIENTED_EDGE('',*,*,#52726,.T.);
#76136=ORIENTED_EDGE('',*,*,#52729,.T.);
#76137=ORIENTED_EDGE('',*,*,#52731,.T.);
#76138=ORIENTED_EDGE('',*,*,#52741,.T.);
#76139=ORIENTED_EDGE('',*,*,#52742,.T.);
#76140=ORIENTED_EDGE('',*,*,#52743,.T.);
#76141=ORIENTED_EDGE('',*,*,#52744,.T.);
#76142=ORIENTED_EDGE('',*,*,#52745,.T.);
#76143=ORIENTED_EDGE('',*,*,#52746,.T.);
#76144=ORIENTED_EDGE('',*,*,#52747,.T.);
#76145=ORIENTED_EDGE('',*,*,#52748,.F.);
#76146=ORIENTED_EDGE('',*,*,#52749,.T.);
#76147=ORIENTED_EDGE('',*,*,#52750,.T.);
#76148=ORIENTED_EDGE('',*,*,#52748,.T.);
#76149=ORIENTED_EDGE('',*,*,#52751,.T.);
#76150=ORIENTED_EDGE('',*,*,#52741,.F.);
#76151=ORIENTED_EDGE('',*,*,#52752,.T.);
#76152=ORIENTED_EDGE('',*,*,#52753,.F.);
#76153=ORIENTED_EDGE('',*,*,#52749,.F.);
#76154=ORIENTED_EDGE('',*,*,#52754,.F.);
#76155=ORIENTED_EDGE('',*,*,#52755,.F.);
#76156=ORIENTED_EDGE('',*,*,#52754,.T.);
#76157=ORIENTED_EDGE('',*,*,#52752,.F.);
#76158=ORIENTED_EDGE('',*,*,#52756,.F.);
#76159=ORIENTED_EDGE('',*,*,#52756,.T.);
#76160=ORIENTED_EDGE('',*,*,#52745,.F.);
#76161=ORIENTED_EDGE('',*,*,#52757,.F.);
#76162=ORIENTED_EDGE('',*,*,#52758,.F.);
#76163=ORIENTED_EDGE('',*,*,#52759,.T.);
#76164=ORIENTED_EDGE('',*,*,#52760,.F.);
#76165=ORIENTED_EDGE('',*,*,#52761,.F.);
#76166=ORIENTED_EDGE('',*,*,#50318,.F.);
#76167=ORIENTED_EDGE('',*,*,#52762,.T.);
#76168=ORIENTED_EDGE('',*,*,#52753,.T.);
#76169=ORIENTED_EDGE('',*,*,#52759,.F.);
#76170=ORIENTED_EDGE('',*,*,#50317,.T.);
#76171=ORIENTED_EDGE('',*,*,#52763,.F.);
#76172=ORIENTED_EDGE('',*,*,#52750,.F.);
#76173=ORIENTED_EDGE('',*,*,#52762,.F.);
#76174=ORIENTED_EDGE('',*,*,#50316,.F.);
#76175=ORIENTED_EDGE('',*,*,#52763,.T.);
#76176=ORIENTED_EDGE('',*,*,#50728,.F.);
#76177=ORIENTED_EDGE('',*,*,#52764,.F.);
#76178=ORIENTED_EDGE('',*,*,#52746,.F.);
#76179=ORIENTED_EDGE('',*,*,#52764,.T.);
#76180=ORIENTED_EDGE('',*,*,#49702,.F.);
#76181=ORIENTED_EDGE('',*,*,#52765,.F.);
#76182=ORIENTED_EDGE('',*,*,#52747,.F.);
#76183=ORIENTED_EDGE('',*,*,#52765,.T.);
#76184=ORIENTED_EDGE('',*,*,#49701,.F.);
#76185=ORIENTED_EDGE('',*,*,#52766,.F.);
#76186=ORIENTED_EDGE('',*,*,#52751,.F.);
#76187=ORIENTED_EDGE('',*,*,#52766,.T.);
#76188=ORIENTED_EDGE('',*,*,#49700,.F.);
#76189=ORIENTED_EDGE('',*,*,#52767,.F.);
#76190=ORIENTED_EDGE('',*,*,#52742,.F.);
#76191=ORIENTED_EDGE('',*,*,#52768,.T.);
#76192=ORIENTED_EDGE('',*,*,#52743,.F.);
#76193=ORIENTED_EDGE('',*,*,#52767,.T.);
#76194=ORIENTED_EDGE('',*,*,#50729,.F.);
#76195=ORIENTED_EDGE('',*,*,#52769,.T.);
#76196=ORIENTED_EDGE('',*,*,#52744,.F.);
#76197=ORIENTED_EDGE('',*,*,#52768,.F.);
#76198=ORIENTED_EDGE('',*,*,#50320,.F.);
#76199=ORIENTED_EDGE('',*,*,#52761,.T.);
#76200=ORIENTED_EDGE('',*,*,#52757,.T.);
#76201=ORIENTED_EDGE('',*,*,#52769,.F.);
#76202=ORIENTED_EDGE('',*,*,#50319,.T.);
#76203=ORIENTED_EDGE('',*,*,#52755,.T.);
#76204=ORIENTED_EDGE('',*,*,#52758,.T.);
#76205=ORIENTED_EDGE('',*,*,#52760,.T.);
#76206=ORIENTED_EDGE('',*,*,#52770,.T.);
#76207=ORIENTED_EDGE('',*,*,#52771,.T.);
#76208=ORIENTED_EDGE('',*,*,#52772,.T.);
#76209=ORIENTED_EDGE('',*,*,#52773,.T.);
#76210=ORIENTED_EDGE('',*,*,#52774,.T.);
#76211=ORIENTED_EDGE('',*,*,#52775,.T.);
#76212=ORIENTED_EDGE('',*,*,#52776,.T.);
#76213=ORIENTED_EDGE('',*,*,#52777,.F.);
#76214=ORIENTED_EDGE('',*,*,#52778,.T.);
#76215=ORIENTED_EDGE('',*,*,#52779,.T.);
#76216=ORIENTED_EDGE('',*,*,#52777,.T.);
#76217=ORIENTED_EDGE('',*,*,#52780,.T.);
#76218=ORIENTED_EDGE('',*,*,#52770,.F.);
#76219=ORIENTED_EDGE('',*,*,#52781,.T.);
#76220=ORIENTED_EDGE('',*,*,#52782,.F.);
#76221=ORIENTED_EDGE('',*,*,#52778,.F.);
#76222=ORIENTED_EDGE('',*,*,#52783,.F.);
#76223=ORIENTED_EDGE('',*,*,#52784,.F.);
#76224=ORIENTED_EDGE('',*,*,#52783,.T.);
#76225=ORIENTED_EDGE('',*,*,#52781,.F.);
#76226=ORIENTED_EDGE('',*,*,#52785,.F.);
#76227=ORIENTED_EDGE('',*,*,#52785,.T.);
#76228=ORIENTED_EDGE('',*,*,#52774,.F.);
#76229=ORIENTED_EDGE('',*,*,#52786,.F.);
#76230=ORIENTED_EDGE('',*,*,#52787,.F.);
#76231=ORIENTED_EDGE('',*,*,#52788,.T.);
#76232=ORIENTED_EDGE('',*,*,#52789,.F.);
#76233=ORIENTED_EDGE('',*,*,#52790,.F.);
#76234=ORIENTED_EDGE('',*,*,#50312,.F.);
#76235=ORIENTED_EDGE('',*,*,#52791,.T.);
#76236=ORIENTED_EDGE('',*,*,#52782,.T.);
#76237=ORIENTED_EDGE('',*,*,#52788,.F.);
#76238=ORIENTED_EDGE('',*,*,#50311,.T.);
#76239=ORIENTED_EDGE('',*,*,#52792,.F.);
#76240=ORIENTED_EDGE('',*,*,#52779,.F.);
#76241=ORIENTED_EDGE('',*,*,#52791,.F.);
#76242=ORIENTED_EDGE('',*,*,#50310,.F.);
#76243=ORIENTED_EDGE('',*,*,#52792,.T.);
#76244=ORIENTED_EDGE('',*,*,#50726,.F.);
#76245=ORIENTED_EDGE('',*,*,#52793,.F.);
#76246=ORIENTED_EDGE('',*,*,#52775,.F.);
#76247=ORIENTED_EDGE('',*,*,#52793,.T.);
#76248=ORIENTED_EDGE('',*,*,#49706,.F.);
#76249=ORIENTED_EDGE('',*,*,#52794,.F.);
#76250=ORIENTED_EDGE('',*,*,#52776,.F.);
#76251=ORIENTED_EDGE('',*,*,#52794,.T.);
#76252=ORIENTED_EDGE('',*,*,#49705,.F.);
#76253=ORIENTED_EDGE('',*,*,#52795,.F.);
#76254=ORIENTED_EDGE('',*,*,#52780,.F.);
#76255=ORIENTED_EDGE('',*,*,#52795,.T.);
#76256=ORIENTED_EDGE('',*,*,#49704,.F.);
#76257=ORIENTED_EDGE('',*,*,#52796,.F.);
#76258=ORIENTED_EDGE('',*,*,#52771,.F.);
#76259=ORIENTED_EDGE('',*,*,#52797,.T.);
#76260=ORIENTED_EDGE('',*,*,#52772,.F.);
#76261=ORIENTED_EDGE('',*,*,#52796,.T.);
#76262=ORIENTED_EDGE('',*,*,#50727,.F.);
#76263=ORIENTED_EDGE('',*,*,#52798,.T.);
#76264=ORIENTED_EDGE('',*,*,#52773,.F.);
#76265=ORIENTED_EDGE('',*,*,#52797,.F.);
#76266=ORIENTED_EDGE('',*,*,#50314,.F.);
#76267=ORIENTED_EDGE('',*,*,#52790,.T.);
#76268=ORIENTED_EDGE('',*,*,#52786,.T.);
#76269=ORIENTED_EDGE('',*,*,#52798,.F.);
#76270=ORIENTED_EDGE('',*,*,#50313,.T.);
#76271=ORIENTED_EDGE('',*,*,#52784,.T.);
#76272=ORIENTED_EDGE('',*,*,#52787,.T.);
#76273=ORIENTED_EDGE('',*,*,#52789,.T.);
#76274=ORIENTED_EDGE('',*,*,#52799,.T.);
#76275=ORIENTED_EDGE('',*,*,#52800,.T.);
#76276=ORIENTED_EDGE('',*,*,#52801,.T.);
#76277=ORIENTED_EDGE('',*,*,#52802,.T.);
#76278=ORIENTED_EDGE('',*,*,#52803,.T.);
#76279=ORIENTED_EDGE('',*,*,#52804,.T.);
#76280=ORIENTED_EDGE('',*,*,#52805,.T.);
#76281=ORIENTED_EDGE('',*,*,#52806,.F.);
#76282=ORIENTED_EDGE('',*,*,#52807,.T.);
#76283=ORIENTED_EDGE('',*,*,#52808,.T.);
#76284=ORIENTED_EDGE('',*,*,#52806,.T.);
#76285=ORIENTED_EDGE('',*,*,#52809,.T.);
#76286=ORIENTED_EDGE('',*,*,#52799,.F.);
#76287=ORIENTED_EDGE('',*,*,#52810,.T.);
#76288=ORIENTED_EDGE('',*,*,#52811,.F.);
#76289=ORIENTED_EDGE('',*,*,#52807,.F.);
#76290=ORIENTED_EDGE('',*,*,#52812,.F.);
#76291=ORIENTED_EDGE('',*,*,#52813,.F.);
#76292=ORIENTED_EDGE('',*,*,#52812,.T.);
#76293=ORIENTED_EDGE('',*,*,#52810,.F.);
#76294=ORIENTED_EDGE('',*,*,#52814,.F.);
#76295=ORIENTED_EDGE('',*,*,#52814,.T.);
#76296=ORIENTED_EDGE('',*,*,#52803,.F.);
#76297=ORIENTED_EDGE('',*,*,#52815,.F.);
#76298=ORIENTED_EDGE('',*,*,#52816,.F.);
#76299=ORIENTED_EDGE('',*,*,#52817,.T.);
#76300=ORIENTED_EDGE('',*,*,#52818,.F.);
#76301=ORIENTED_EDGE('',*,*,#52819,.F.);
#76302=ORIENTED_EDGE('',*,*,#50306,.F.);
#76303=ORIENTED_EDGE('',*,*,#52820,.T.);
#76304=ORIENTED_EDGE('',*,*,#52811,.T.);
#76305=ORIENTED_EDGE('',*,*,#52817,.F.);
#76306=ORIENTED_EDGE('',*,*,#50305,.T.);
#76307=ORIENTED_EDGE('',*,*,#52821,.F.);
#76308=ORIENTED_EDGE('',*,*,#52808,.F.);
#76309=ORIENTED_EDGE('',*,*,#52820,.F.);
#76310=ORIENTED_EDGE('',*,*,#50304,.F.);
#76311=ORIENTED_EDGE('',*,*,#52821,.T.);
#76312=ORIENTED_EDGE('',*,*,#50724,.F.);
#76313=ORIENTED_EDGE('',*,*,#52822,.F.);
#76314=ORIENTED_EDGE('',*,*,#52804,.F.);
#76315=ORIENTED_EDGE('',*,*,#52822,.T.);
#76316=ORIENTED_EDGE('',*,*,#49710,.F.);
#76317=ORIENTED_EDGE('',*,*,#52823,.F.);
#76318=ORIENTED_EDGE('',*,*,#52805,.F.);
#76319=ORIENTED_EDGE('',*,*,#52823,.T.);
#76320=ORIENTED_EDGE('',*,*,#49709,.F.);
#76321=ORIENTED_EDGE('',*,*,#52824,.F.);
#76322=ORIENTED_EDGE('',*,*,#52809,.F.);
#76323=ORIENTED_EDGE('',*,*,#52824,.T.);
#76324=ORIENTED_EDGE('',*,*,#49708,.F.);
#76325=ORIENTED_EDGE('',*,*,#52825,.F.);
#76326=ORIENTED_EDGE('',*,*,#52800,.F.);
#76327=ORIENTED_EDGE('',*,*,#52826,.T.);
#76328=ORIENTED_EDGE('',*,*,#52801,.F.);
#76329=ORIENTED_EDGE('',*,*,#52825,.T.);
#76330=ORIENTED_EDGE('',*,*,#50725,.F.);
#76331=ORIENTED_EDGE('',*,*,#52827,.T.);
#76332=ORIENTED_EDGE('',*,*,#52802,.F.);
#76333=ORIENTED_EDGE('',*,*,#52826,.F.);
#76334=ORIENTED_EDGE('',*,*,#50308,.F.);
#76335=ORIENTED_EDGE('',*,*,#52819,.T.);
#76336=ORIENTED_EDGE('',*,*,#52815,.T.);
#76337=ORIENTED_EDGE('',*,*,#52827,.F.);
#76338=ORIENTED_EDGE('',*,*,#50307,.T.);
#76339=ORIENTED_EDGE('',*,*,#52813,.T.);
#76340=ORIENTED_EDGE('',*,*,#52816,.T.);
#76341=ORIENTED_EDGE('',*,*,#52818,.T.);
#76342=ORIENTED_EDGE('',*,*,#52828,.T.);
#76343=ORIENTED_EDGE('',*,*,#52829,.T.);
#76344=ORIENTED_EDGE('',*,*,#52830,.T.);
#76345=ORIENTED_EDGE('',*,*,#52831,.T.);
#76346=ORIENTED_EDGE('',*,*,#52832,.T.);
#76347=ORIENTED_EDGE('',*,*,#52833,.T.);
#76348=ORIENTED_EDGE('',*,*,#52834,.T.);
#76349=ORIENTED_EDGE('',*,*,#52835,.F.);
#76350=ORIENTED_EDGE('',*,*,#52836,.T.);
#76351=ORIENTED_EDGE('',*,*,#52837,.T.);
#76352=ORIENTED_EDGE('',*,*,#52835,.T.);
#76353=ORIENTED_EDGE('',*,*,#52838,.T.);
#76354=ORIENTED_EDGE('',*,*,#52828,.F.);
#76355=ORIENTED_EDGE('',*,*,#52839,.T.);
#76356=ORIENTED_EDGE('',*,*,#52840,.F.);
#76357=ORIENTED_EDGE('',*,*,#52836,.F.);
#76358=ORIENTED_EDGE('',*,*,#52841,.F.);
#76359=ORIENTED_EDGE('',*,*,#52842,.F.);
#76360=ORIENTED_EDGE('',*,*,#52841,.T.);
#76361=ORIENTED_EDGE('',*,*,#52839,.F.);
#76362=ORIENTED_EDGE('',*,*,#52843,.F.);
#76363=ORIENTED_EDGE('',*,*,#52843,.T.);
#76364=ORIENTED_EDGE('',*,*,#52832,.F.);
#76365=ORIENTED_EDGE('',*,*,#52844,.F.);
#76366=ORIENTED_EDGE('',*,*,#52845,.F.);
#76367=ORIENTED_EDGE('',*,*,#52846,.T.);
#76368=ORIENTED_EDGE('',*,*,#52847,.F.);
#76369=ORIENTED_EDGE('',*,*,#52848,.F.);
#76370=ORIENTED_EDGE('',*,*,#50300,.F.);
#76371=ORIENTED_EDGE('',*,*,#52849,.T.);
#76372=ORIENTED_EDGE('',*,*,#52840,.T.);
#76373=ORIENTED_EDGE('',*,*,#52846,.F.);
#76374=ORIENTED_EDGE('',*,*,#50299,.T.);
#76375=ORIENTED_EDGE('',*,*,#52850,.F.);
#76376=ORIENTED_EDGE('',*,*,#52837,.F.);
#76377=ORIENTED_EDGE('',*,*,#52849,.F.);
#76378=ORIENTED_EDGE('',*,*,#50298,.F.);
#76379=ORIENTED_EDGE('',*,*,#52850,.T.);
#76380=ORIENTED_EDGE('',*,*,#50722,.F.);
#76381=ORIENTED_EDGE('',*,*,#52851,.F.);
#76382=ORIENTED_EDGE('',*,*,#52833,.F.);
#76383=ORIENTED_EDGE('',*,*,#52851,.T.);
#76384=ORIENTED_EDGE('',*,*,#49714,.F.);
#76385=ORIENTED_EDGE('',*,*,#52852,.F.);
#76386=ORIENTED_EDGE('',*,*,#52834,.F.);
#76387=ORIENTED_EDGE('',*,*,#52852,.T.);
#76388=ORIENTED_EDGE('',*,*,#49713,.F.);
#76389=ORIENTED_EDGE('',*,*,#52853,.F.);
#76390=ORIENTED_EDGE('',*,*,#52838,.F.);
#76391=ORIENTED_EDGE('',*,*,#52853,.T.);
#76392=ORIENTED_EDGE('',*,*,#49712,.F.);
#76393=ORIENTED_EDGE('',*,*,#52854,.F.);
#76394=ORIENTED_EDGE('',*,*,#52829,.F.);
#76395=ORIENTED_EDGE('',*,*,#52855,.T.);
#76396=ORIENTED_EDGE('',*,*,#52830,.F.);
#76397=ORIENTED_EDGE('',*,*,#52854,.T.);
#76398=ORIENTED_EDGE('',*,*,#50723,.F.);
#76399=ORIENTED_EDGE('',*,*,#52856,.T.);
#76400=ORIENTED_EDGE('',*,*,#52831,.F.);
#76401=ORIENTED_EDGE('',*,*,#52855,.F.);
#76402=ORIENTED_EDGE('',*,*,#50302,.F.);
#76403=ORIENTED_EDGE('',*,*,#52848,.T.);
#76404=ORIENTED_EDGE('',*,*,#52844,.T.);
#76405=ORIENTED_EDGE('',*,*,#52856,.F.);
#76406=ORIENTED_EDGE('',*,*,#50301,.T.);
#76407=ORIENTED_EDGE('',*,*,#52842,.T.);
#76408=ORIENTED_EDGE('',*,*,#52845,.T.);
#76409=ORIENTED_EDGE('',*,*,#52847,.T.);
#76410=ORIENTED_EDGE('',*,*,#52857,.T.);
#76411=ORIENTED_EDGE('',*,*,#52858,.T.);
#76412=ORIENTED_EDGE('',*,*,#52859,.T.);
#76413=ORIENTED_EDGE('',*,*,#52860,.T.);
#76414=ORIENTED_EDGE('',*,*,#52861,.T.);
#76415=ORIENTED_EDGE('',*,*,#52862,.T.);
#76416=ORIENTED_EDGE('',*,*,#52863,.T.);
#76417=ORIENTED_EDGE('',*,*,#52864,.F.);
#76418=ORIENTED_EDGE('',*,*,#52865,.T.);
#76419=ORIENTED_EDGE('',*,*,#52866,.T.);
#76420=ORIENTED_EDGE('',*,*,#52864,.T.);
#76421=ORIENTED_EDGE('',*,*,#52867,.T.);
#76422=ORIENTED_EDGE('',*,*,#52857,.F.);
#76423=ORIENTED_EDGE('',*,*,#52868,.T.);
#76424=ORIENTED_EDGE('',*,*,#52869,.F.);
#76425=ORIENTED_EDGE('',*,*,#52865,.F.);
#76426=ORIENTED_EDGE('',*,*,#52870,.F.);
#76427=ORIENTED_EDGE('',*,*,#52871,.F.);
#76428=ORIENTED_EDGE('',*,*,#52870,.T.);
#76429=ORIENTED_EDGE('',*,*,#52868,.F.);
#76430=ORIENTED_EDGE('',*,*,#52872,.F.);
#76431=ORIENTED_EDGE('',*,*,#52872,.T.);
#76432=ORIENTED_EDGE('',*,*,#52861,.F.);
#76433=ORIENTED_EDGE('',*,*,#52873,.F.);
#76434=ORIENTED_EDGE('',*,*,#52874,.F.);
#76435=ORIENTED_EDGE('',*,*,#52875,.T.);
#76436=ORIENTED_EDGE('',*,*,#52876,.F.);
#76437=ORIENTED_EDGE('',*,*,#52877,.F.);
#76438=ORIENTED_EDGE('',*,*,#50294,.F.);
#76439=ORIENTED_EDGE('',*,*,#52878,.T.);
#76440=ORIENTED_EDGE('',*,*,#52869,.T.);
#76441=ORIENTED_EDGE('',*,*,#52875,.F.);
#76442=ORIENTED_EDGE('',*,*,#50293,.T.);
#76443=ORIENTED_EDGE('',*,*,#52879,.F.);
#76444=ORIENTED_EDGE('',*,*,#52866,.F.);
#76445=ORIENTED_EDGE('',*,*,#52878,.F.);
#76446=ORIENTED_EDGE('',*,*,#50292,.F.);
#76447=ORIENTED_EDGE('',*,*,#52879,.T.);
#76448=ORIENTED_EDGE('',*,*,#50720,.F.);
#76449=ORIENTED_EDGE('',*,*,#52880,.F.);
#76450=ORIENTED_EDGE('',*,*,#52862,.F.);
#76451=ORIENTED_EDGE('',*,*,#52880,.T.);
#76452=ORIENTED_EDGE('',*,*,#49718,.F.);
#76453=ORIENTED_EDGE('',*,*,#52881,.F.);
#76454=ORIENTED_EDGE('',*,*,#52863,.F.);
#76455=ORIENTED_EDGE('',*,*,#52881,.T.);
#76456=ORIENTED_EDGE('',*,*,#49717,.F.);
#76457=ORIENTED_EDGE('',*,*,#52882,.F.);
#76458=ORIENTED_EDGE('',*,*,#52867,.F.);
#76459=ORIENTED_EDGE('',*,*,#52882,.T.);
#76460=ORIENTED_EDGE('',*,*,#49716,.F.);
#76461=ORIENTED_EDGE('',*,*,#52883,.F.);
#76462=ORIENTED_EDGE('',*,*,#52858,.F.);
#76463=ORIENTED_EDGE('',*,*,#52884,.T.);
#76464=ORIENTED_EDGE('',*,*,#52859,.F.);
#76465=ORIENTED_EDGE('',*,*,#52883,.T.);
#76466=ORIENTED_EDGE('',*,*,#50721,.F.);
#76467=ORIENTED_EDGE('',*,*,#52885,.T.);
#76468=ORIENTED_EDGE('',*,*,#52860,.F.);
#76469=ORIENTED_EDGE('',*,*,#52884,.F.);
#76470=ORIENTED_EDGE('',*,*,#50296,.F.);
#76471=ORIENTED_EDGE('',*,*,#52877,.T.);
#76472=ORIENTED_EDGE('',*,*,#52873,.T.);
#76473=ORIENTED_EDGE('',*,*,#52885,.F.);
#76474=ORIENTED_EDGE('',*,*,#50295,.T.);
#76475=ORIENTED_EDGE('',*,*,#52871,.T.);
#76476=ORIENTED_EDGE('',*,*,#52874,.T.);
#76477=ORIENTED_EDGE('',*,*,#52876,.T.);
#76478=ORIENTED_EDGE('',*,*,#52886,.T.);
#76479=ORIENTED_EDGE('',*,*,#52887,.T.);
#76480=ORIENTED_EDGE('',*,*,#52888,.T.);
#76481=ORIENTED_EDGE('',*,*,#52889,.T.);
#76482=ORIENTED_EDGE('',*,*,#52890,.T.);
#76483=ORIENTED_EDGE('',*,*,#52891,.T.);
#76484=ORIENTED_EDGE('',*,*,#52892,.T.);
#76485=ORIENTED_EDGE('',*,*,#52893,.F.);
#76486=ORIENTED_EDGE('',*,*,#52894,.T.);
#76487=ORIENTED_EDGE('',*,*,#52895,.T.);
#76488=ORIENTED_EDGE('',*,*,#52893,.T.);
#76489=ORIENTED_EDGE('',*,*,#52896,.T.);
#76490=ORIENTED_EDGE('',*,*,#52886,.F.);
#76491=ORIENTED_EDGE('',*,*,#52897,.T.);
#76492=ORIENTED_EDGE('',*,*,#52898,.F.);
#76493=ORIENTED_EDGE('',*,*,#52894,.F.);
#76494=ORIENTED_EDGE('',*,*,#52899,.F.);
#76495=ORIENTED_EDGE('',*,*,#52900,.F.);
#76496=ORIENTED_EDGE('',*,*,#52899,.T.);
#76497=ORIENTED_EDGE('',*,*,#52897,.F.);
#76498=ORIENTED_EDGE('',*,*,#52901,.F.);
#76499=ORIENTED_EDGE('',*,*,#52901,.T.);
#76500=ORIENTED_EDGE('',*,*,#52890,.F.);
#76501=ORIENTED_EDGE('',*,*,#52902,.F.);
#76502=ORIENTED_EDGE('',*,*,#52903,.F.);
#76503=ORIENTED_EDGE('',*,*,#52904,.T.);
#76504=ORIENTED_EDGE('',*,*,#52905,.F.);
#76505=ORIENTED_EDGE('',*,*,#52906,.F.);
#76506=ORIENTED_EDGE('',*,*,#50288,.F.);
#76507=ORIENTED_EDGE('',*,*,#52907,.T.);
#76508=ORIENTED_EDGE('',*,*,#52898,.T.);
#76509=ORIENTED_EDGE('',*,*,#52904,.F.);
#76510=ORIENTED_EDGE('',*,*,#50287,.T.);
#76511=ORIENTED_EDGE('',*,*,#52908,.F.);
#76512=ORIENTED_EDGE('',*,*,#52895,.F.);
#76513=ORIENTED_EDGE('',*,*,#52907,.F.);
#76514=ORIENTED_EDGE('',*,*,#50286,.F.);
#76515=ORIENTED_EDGE('',*,*,#52908,.T.);
#76516=ORIENTED_EDGE('',*,*,#50718,.F.);
#76517=ORIENTED_EDGE('',*,*,#52909,.F.);
#76518=ORIENTED_EDGE('',*,*,#52891,.F.);
#76519=ORIENTED_EDGE('',*,*,#52909,.T.);
#76520=ORIENTED_EDGE('',*,*,#49722,.F.);
#76521=ORIENTED_EDGE('',*,*,#52910,.F.);
#76522=ORIENTED_EDGE('',*,*,#52892,.F.);
#76523=ORIENTED_EDGE('',*,*,#52910,.T.);
#76524=ORIENTED_EDGE('',*,*,#49721,.F.);
#76525=ORIENTED_EDGE('',*,*,#52911,.F.);
#76526=ORIENTED_EDGE('',*,*,#52896,.F.);
#76527=ORIENTED_EDGE('',*,*,#52911,.T.);
#76528=ORIENTED_EDGE('',*,*,#49720,.F.);
#76529=ORIENTED_EDGE('',*,*,#52912,.F.);
#76530=ORIENTED_EDGE('',*,*,#52887,.F.);
#76531=ORIENTED_EDGE('',*,*,#52913,.T.);
#76532=ORIENTED_EDGE('',*,*,#52888,.F.);
#76533=ORIENTED_EDGE('',*,*,#52912,.T.);
#76534=ORIENTED_EDGE('',*,*,#50719,.F.);
#76535=ORIENTED_EDGE('',*,*,#52914,.T.);
#76536=ORIENTED_EDGE('',*,*,#52889,.F.);
#76537=ORIENTED_EDGE('',*,*,#52913,.F.);
#76538=ORIENTED_EDGE('',*,*,#50290,.F.);
#76539=ORIENTED_EDGE('',*,*,#52906,.T.);
#76540=ORIENTED_EDGE('',*,*,#52902,.T.);
#76541=ORIENTED_EDGE('',*,*,#52914,.F.);
#76542=ORIENTED_EDGE('',*,*,#50289,.T.);
#76543=ORIENTED_EDGE('',*,*,#52900,.T.);
#76544=ORIENTED_EDGE('',*,*,#52903,.T.);
#76545=ORIENTED_EDGE('',*,*,#52905,.T.);
#76546=ORIENTED_EDGE('',*,*,#52915,.T.);
#76547=ORIENTED_EDGE('',*,*,#52916,.T.);
#76548=ORIENTED_EDGE('',*,*,#52917,.T.);
#76549=ORIENTED_EDGE('',*,*,#52918,.T.);
#76550=ORIENTED_EDGE('',*,*,#52919,.T.);
#76551=ORIENTED_EDGE('',*,*,#52920,.T.);
#76552=ORIENTED_EDGE('',*,*,#52921,.T.);
#76553=ORIENTED_EDGE('',*,*,#52922,.F.);
#76554=ORIENTED_EDGE('',*,*,#52923,.T.);
#76555=ORIENTED_EDGE('',*,*,#52924,.T.);
#76556=ORIENTED_EDGE('',*,*,#52922,.T.);
#76557=ORIENTED_EDGE('',*,*,#52925,.T.);
#76558=ORIENTED_EDGE('',*,*,#52915,.F.);
#76559=ORIENTED_EDGE('',*,*,#52926,.T.);
#76560=ORIENTED_EDGE('',*,*,#52927,.F.);
#76561=ORIENTED_EDGE('',*,*,#52923,.F.);
#76562=ORIENTED_EDGE('',*,*,#52928,.F.);
#76563=ORIENTED_EDGE('',*,*,#52929,.F.);
#76564=ORIENTED_EDGE('',*,*,#52928,.T.);
#76565=ORIENTED_EDGE('',*,*,#52926,.F.);
#76566=ORIENTED_EDGE('',*,*,#52930,.F.);
#76567=ORIENTED_EDGE('',*,*,#52930,.T.);
#76568=ORIENTED_EDGE('',*,*,#52919,.F.);
#76569=ORIENTED_EDGE('',*,*,#52931,.F.);
#76570=ORIENTED_EDGE('',*,*,#52932,.F.);
#76571=ORIENTED_EDGE('',*,*,#52933,.T.);
#76572=ORIENTED_EDGE('',*,*,#52934,.F.);
#76573=ORIENTED_EDGE('',*,*,#52935,.F.);
#76574=ORIENTED_EDGE('',*,*,#50282,.F.);
#76575=ORIENTED_EDGE('',*,*,#52936,.T.);
#76576=ORIENTED_EDGE('',*,*,#52927,.T.);
#76577=ORIENTED_EDGE('',*,*,#52933,.F.);
#76578=ORIENTED_EDGE('',*,*,#50281,.T.);
#76579=ORIENTED_EDGE('',*,*,#52937,.F.);
#76580=ORIENTED_EDGE('',*,*,#52924,.F.);
#76581=ORIENTED_EDGE('',*,*,#52936,.F.);
#76582=ORIENTED_EDGE('',*,*,#50280,.F.);
#76583=ORIENTED_EDGE('',*,*,#52937,.T.);
#76584=ORIENTED_EDGE('',*,*,#50716,.F.);
#76585=ORIENTED_EDGE('',*,*,#52938,.F.);
#76586=ORIENTED_EDGE('',*,*,#52920,.F.);
#76587=ORIENTED_EDGE('',*,*,#52938,.T.);
#76588=ORIENTED_EDGE('',*,*,#49726,.F.);
#76589=ORIENTED_EDGE('',*,*,#52939,.F.);
#76590=ORIENTED_EDGE('',*,*,#52921,.F.);
#76591=ORIENTED_EDGE('',*,*,#52939,.T.);
#76592=ORIENTED_EDGE('',*,*,#49725,.F.);
#76593=ORIENTED_EDGE('',*,*,#52940,.F.);
#76594=ORIENTED_EDGE('',*,*,#52925,.F.);
#76595=ORIENTED_EDGE('',*,*,#52940,.T.);
#76596=ORIENTED_EDGE('',*,*,#49724,.F.);
#76597=ORIENTED_EDGE('',*,*,#52941,.F.);
#76598=ORIENTED_EDGE('',*,*,#52916,.F.);
#76599=ORIENTED_EDGE('',*,*,#52942,.T.);
#76600=ORIENTED_EDGE('',*,*,#52917,.F.);
#76601=ORIENTED_EDGE('',*,*,#52941,.T.);
#76602=ORIENTED_EDGE('',*,*,#50717,.F.);
#76603=ORIENTED_EDGE('',*,*,#52943,.T.);
#76604=ORIENTED_EDGE('',*,*,#52918,.F.);
#76605=ORIENTED_EDGE('',*,*,#52942,.F.);
#76606=ORIENTED_EDGE('',*,*,#50284,.F.);
#76607=ORIENTED_EDGE('',*,*,#52935,.T.);
#76608=ORIENTED_EDGE('',*,*,#52931,.T.);
#76609=ORIENTED_EDGE('',*,*,#52943,.F.);
#76610=ORIENTED_EDGE('',*,*,#50283,.T.);
#76611=ORIENTED_EDGE('',*,*,#52929,.T.);
#76612=ORIENTED_EDGE('',*,*,#52932,.T.);
#76613=ORIENTED_EDGE('',*,*,#52934,.T.);
#76614=ORIENTED_EDGE('',*,*,#52944,.T.);
#76615=ORIENTED_EDGE('',*,*,#52945,.T.);
#76616=ORIENTED_EDGE('',*,*,#52946,.T.);
#76617=ORIENTED_EDGE('',*,*,#52947,.T.);
#76618=ORIENTED_EDGE('',*,*,#52948,.T.);
#76619=ORIENTED_EDGE('',*,*,#52949,.T.);
#76620=ORIENTED_EDGE('',*,*,#52950,.T.);
#76621=ORIENTED_EDGE('',*,*,#52951,.F.);
#76622=ORIENTED_EDGE('',*,*,#52952,.T.);
#76623=ORIENTED_EDGE('',*,*,#52953,.T.);
#76624=ORIENTED_EDGE('',*,*,#52951,.T.);
#76625=ORIENTED_EDGE('',*,*,#52954,.T.);
#76626=ORIENTED_EDGE('',*,*,#52944,.F.);
#76627=ORIENTED_EDGE('',*,*,#52955,.T.);
#76628=ORIENTED_EDGE('',*,*,#52956,.F.);
#76629=ORIENTED_EDGE('',*,*,#52952,.F.);
#76630=ORIENTED_EDGE('',*,*,#52957,.F.);
#76631=ORIENTED_EDGE('',*,*,#52958,.F.);
#76632=ORIENTED_EDGE('',*,*,#52957,.T.);
#76633=ORIENTED_EDGE('',*,*,#52955,.F.);
#76634=ORIENTED_EDGE('',*,*,#52959,.F.);
#76635=ORIENTED_EDGE('',*,*,#52959,.T.);
#76636=ORIENTED_EDGE('',*,*,#52948,.F.);
#76637=ORIENTED_EDGE('',*,*,#52960,.F.);
#76638=ORIENTED_EDGE('',*,*,#52961,.F.);
#76639=ORIENTED_EDGE('',*,*,#52962,.T.);
#76640=ORIENTED_EDGE('',*,*,#52963,.F.);
#76641=ORIENTED_EDGE('',*,*,#52964,.F.);
#76642=ORIENTED_EDGE('',*,*,#50276,.F.);
#76643=ORIENTED_EDGE('',*,*,#52965,.T.);
#76644=ORIENTED_EDGE('',*,*,#52956,.T.);
#76645=ORIENTED_EDGE('',*,*,#52962,.F.);
#76646=ORIENTED_EDGE('',*,*,#50275,.T.);
#76647=ORIENTED_EDGE('',*,*,#52966,.F.);
#76648=ORIENTED_EDGE('',*,*,#52953,.F.);
#76649=ORIENTED_EDGE('',*,*,#52965,.F.);
#76650=ORIENTED_EDGE('',*,*,#50274,.F.);
#76651=ORIENTED_EDGE('',*,*,#52966,.T.);
#76652=ORIENTED_EDGE('',*,*,#50714,.F.);
#76653=ORIENTED_EDGE('',*,*,#52967,.F.);
#76654=ORIENTED_EDGE('',*,*,#52949,.F.);
#76655=ORIENTED_EDGE('',*,*,#52967,.T.);
#76656=ORIENTED_EDGE('',*,*,#49730,.F.);
#76657=ORIENTED_EDGE('',*,*,#52968,.F.);
#76658=ORIENTED_EDGE('',*,*,#52950,.F.);
#76659=ORIENTED_EDGE('',*,*,#52968,.T.);
#76660=ORIENTED_EDGE('',*,*,#49729,.F.);
#76661=ORIENTED_EDGE('',*,*,#52969,.F.);
#76662=ORIENTED_EDGE('',*,*,#52954,.F.);
#76663=ORIENTED_EDGE('',*,*,#52969,.T.);
#76664=ORIENTED_EDGE('',*,*,#49728,.F.);
#76665=ORIENTED_EDGE('',*,*,#52970,.F.);
#76666=ORIENTED_EDGE('',*,*,#52945,.F.);
#76667=ORIENTED_EDGE('',*,*,#52971,.T.);
#76668=ORIENTED_EDGE('',*,*,#52946,.F.);
#76669=ORIENTED_EDGE('',*,*,#52970,.T.);
#76670=ORIENTED_EDGE('',*,*,#50715,.F.);
#76671=ORIENTED_EDGE('',*,*,#52972,.T.);
#76672=ORIENTED_EDGE('',*,*,#52947,.F.);
#76673=ORIENTED_EDGE('',*,*,#52971,.F.);
#76674=ORIENTED_EDGE('',*,*,#50278,.F.);
#76675=ORIENTED_EDGE('',*,*,#52964,.T.);
#76676=ORIENTED_EDGE('',*,*,#52960,.T.);
#76677=ORIENTED_EDGE('',*,*,#52972,.F.);
#76678=ORIENTED_EDGE('',*,*,#50277,.T.);
#76679=ORIENTED_EDGE('',*,*,#52958,.T.);
#76680=ORIENTED_EDGE('',*,*,#52961,.T.);
#76681=ORIENTED_EDGE('',*,*,#52963,.T.);
#76682=ORIENTED_EDGE('',*,*,#52973,.T.);
#76683=ORIENTED_EDGE('',*,*,#52974,.T.);
#76684=ORIENTED_EDGE('',*,*,#52975,.T.);
#76685=ORIENTED_EDGE('',*,*,#52976,.T.);
#76686=ORIENTED_EDGE('',*,*,#52977,.T.);
#76687=ORIENTED_EDGE('',*,*,#52978,.T.);
#76688=ORIENTED_EDGE('',*,*,#52979,.T.);
#76689=ORIENTED_EDGE('',*,*,#52980,.F.);
#76690=ORIENTED_EDGE('',*,*,#52981,.T.);
#76691=ORIENTED_EDGE('',*,*,#52982,.T.);
#76692=ORIENTED_EDGE('',*,*,#52980,.T.);
#76693=ORIENTED_EDGE('',*,*,#52983,.T.);
#76694=ORIENTED_EDGE('',*,*,#52973,.F.);
#76695=ORIENTED_EDGE('',*,*,#52984,.T.);
#76696=ORIENTED_EDGE('',*,*,#52985,.F.);
#76697=ORIENTED_EDGE('',*,*,#52981,.F.);
#76698=ORIENTED_EDGE('',*,*,#52986,.F.);
#76699=ORIENTED_EDGE('',*,*,#52987,.F.);
#76700=ORIENTED_EDGE('',*,*,#52986,.T.);
#76701=ORIENTED_EDGE('',*,*,#52984,.F.);
#76702=ORIENTED_EDGE('',*,*,#52988,.F.);
#76703=ORIENTED_EDGE('',*,*,#52988,.T.);
#76704=ORIENTED_EDGE('',*,*,#52977,.F.);
#76705=ORIENTED_EDGE('',*,*,#52989,.F.);
#76706=ORIENTED_EDGE('',*,*,#52990,.F.);
#76707=ORIENTED_EDGE('',*,*,#52991,.T.);
#76708=ORIENTED_EDGE('',*,*,#52992,.F.);
#76709=ORIENTED_EDGE('',*,*,#52993,.F.);
#76710=ORIENTED_EDGE('',*,*,#50270,.F.);
#76711=ORIENTED_EDGE('',*,*,#52994,.T.);
#76712=ORIENTED_EDGE('',*,*,#52985,.T.);
#76713=ORIENTED_EDGE('',*,*,#52991,.F.);
#76714=ORIENTED_EDGE('',*,*,#50269,.T.);
#76715=ORIENTED_EDGE('',*,*,#52995,.F.);
#76716=ORIENTED_EDGE('',*,*,#52982,.F.);
#76717=ORIENTED_EDGE('',*,*,#52994,.F.);
#76718=ORIENTED_EDGE('',*,*,#50268,.F.);
#76719=ORIENTED_EDGE('',*,*,#52995,.T.);
#76720=ORIENTED_EDGE('',*,*,#50712,.F.);
#76721=ORIENTED_EDGE('',*,*,#52996,.F.);
#76722=ORIENTED_EDGE('',*,*,#52978,.F.);
#76723=ORIENTED_EDGE('',*,*,#52996,.T.);
#76724=ORIENTED_EDGE('',*,*,#49734,.F.);
#76725=ORIENTED_EDGE('',*,*,#52997,.F.);
#76726=ORIENTED_EDGE('',*,*,#52979,.F.);
#76727=ORIENTED_EDGE('',*,*,#52997,.T.);
#76728=ORIENTED_EDGE('',*,*,#49733,.F.);
#76729=ORIENTED_EDGE('',*,*,#52998,.F.);
#76730=ORIENTED_EDGE('',*,*,#52983,.F.);
#76731=ORIENTED_EDGE('',*,*,#52998,.T.);
#76732=ORIENTED_EDGE('',*,*,#49732,.F.);
#76733=ORIENTED_EDGE('',*,*,#52999,.F.);
#76734=ORIENTED_EDGE('',*,*,#52974,.F.);
#76735=ORIENTED_EDGE('',*,*,#53000,.T.);
#76736=ORIENTED_EDGE('',*,*,#52975,.F.);
#76737=ORIENTED_EDGE('',*,*,#52999,.T.);
#76738=ORIENTED_EDGE('',*,*,#50713,.F.);
#76739=ORIENTED_EDGE('',*,*,#53001,.T.);
#76740=ORIENTED_EDGE('',*,*,#52976,.F.);
#76741=ORIENTED_EDGE('',*,*,#53000,.F.);
#76742=ORIENTED_EDGE('',*,*,#50272,.F.);
#76743=ORIENTED_EDGE('',*,*,#52993,.T.);
#76744=ORIENTED_EDGE('',*,*,#52989,.T.);
#76745=ORIENTED_EDGE('',*,*,#53001,.F.);
#76746=ORIENTED_EDGE('',*,*,#50271,.T.);
#76747=ORIENTED_EDGE('',*,*,#52987,.T.);
#76748=ORIENTED_EDGE('',*,*,#52990,.T.);
#76749=ORIENTED_EDGE('',*,*,#52992,.T.);
#76750=ORIENTED_EDGE('',*,*,#53002,.T.);
#76751=ORIENTED_EDGE('',*,*,#53003,.T.);
#76752=ORIENTED_EDGE('',*,*,#53004,.T.);
#76753=ORIENTED_EDGE('',*,*,#53005,.T.);
#76754=ORIENTED_EDGE('',*,*,#53006,.T.);
#76755=ORIENTED_EDGE('',*,*,#53007,.T.);
#76756=ORIENTED_EDGE('',*,*,#53008,.T.);
#76757=ORIENTED_EDGE('',*,*,#53009,.F.);
#76758=ORIENTED_EDGE('',*,*,#53010,.T.);
#76759=ORIENTED_EDGE('',*,*,#53011,.T.);
#76760=ORIENTED_EDGE('',*,*,#53009,.T.);
#76761=ORIENTED_EDGE('',*,*,#53012,.T.);
#76762=ORIENTED_EDGE('',*,*,#53002,.F.);
#76763=ORIENTED_EDGE('',*,*,#53013,.T.);
#76764=ORIENTED_EDGE('',*,*,#53014,.F.);
#76765=ORIENTED_EDGE('',*,*,#53010,.F.);
#76766=ORIENTED_EDGE('',*,*,#53015,.F.);
#76767=ORIENTED_EDGE('',*,*,#53016,.F.);
#76768=ORIENTED_EDGE('',*,*,#53015,.T.);
#76769=ORIENTED_EDGE('',*,*,#53013,.F.);
#76770=ORIENTED_EDGE('',*,*,#53017,.F.);
#76771=ORIENTED_EDGE('',*,*,#53017,.T.);
#76772=ORIENTED_EDGE('',*,*,#53006,.F.);
#76773=ORIENTED_EDGE('',*,*,#53018,.F.);
#76774=ORIENTED_EDGE('',*,*,#53019,.F.);
#76775=ORIENTED_EDGE('',*,*,#53020,.T.);
#76776=ORIENTED_EDGE('',*,*,#53021,.F.);
#76777=ORIENTED_EDGE('',*,*,#53022,.F.);
#76778=ORIENTED_EDGE('',*,*,#50264,.F.);
#76779=ORIENTED_EDGE('',*,*,#53023,.T.);
#76780=ORIENTED_EDGE('',*,*,#53014,.T.);
#76781=ORIENTED_EDGE('',*,*,#53020,.F.);
#76782=ORIENTED_EDGE('',*,*,#50263,.T.);
#76783=ORIENTED_EDGE('',*,*,#53024,.F.);
#76784=ORIENTED_EDGE('',*,*,#53011,.F.);
#76785=ORIENTED_EDGE('',*,*,#53023,.F.);
#76786=ORIENTED_EDGE('',*,*,#50262,.F.);
#76787=ORIENTED_EDGE('',*,*,#53024,.T.);
#76788=ORIENTED_EDGE('',*,*,#50710,.F.);
#76789=ORIENTED_EDGE('',*,*,#53025,.F.);
#76790=ORIENTED_EDGE('',*,*,#53007,.F.);
#76791=ORIENTED_EDGE('',*,*,#53025,.T.);
#76792=ORIENTED_EDGE('',*,*,#49738,.F.);
#76793=ORIENTED_EDGE('',*,*,#53026,.F.);
#76794=ORIENTED_EDGE('',*,*,#53008,.F.);
#76795=ORIENTED_EDGE('',*,*,#53026,.T.);
#76796=ORIENTED_EDGE('',*,*,#49737,.F.);
#76797=ORIENTED_EDGE('',*,*,#53027,.F.);
#76798=ORIENTED_EDGE('',*,*,#53012,.F.);
#76799=ORIENTED_EDGE('',*,*,#53027,.T.);
#76800=ORIENTED_EDGE('',*,*,#49736,.F.);
#76801=ORIENTED_EDGE('',*,*,#53028,.F.);
#76802=ORIENTED_EDGE('',*,*,#53003,.F.);
#76803=ORIENTED_EDGE('',*,*,#53029,.T.);
#76804=ORIENTED_EDGE('',*,*,#53004,.F.);
#76805=ORIENTED_EDGE('',*,*,#53028,.T.);
#76806=ORIENTED_EDGE('',*,*,#50711,.F.);
#76807=ORIENTED_EDGE('',*,*,#53030,.T.);
#76808=ORIENTED_EDGE('',*,*,#53005,.F.);
#76809=ORIENTED_EDGE('',*,*,#53029,.F.);
#76810=ORIENTED_EDGE('',*,*,#50266,.F.);
#76811=ORIENTED_EDGE('',*,*,#53022,.T.);
#76812=ORIENTED_EDGE('',*,*,#53018,.T.);
#76813=ORIENTED_EDGE('',*,*,#53030,.F.);
#76814=ORIENTED_EDGE('',*,*,#50265,.T.);
#76815=ORIENTED_EDGE('',*,*,#53016,.T.);
#76816=ORIENTED_EDGE('',*,*,#53019,.T.);
#76817=ORIENTED_EDGE('',*,*,#53021,.T.);
#76818=ORIENTED_EDGE('',*,*,#53031,.T.);
#76819=ORIENTED_EDGE('',*,*,#53032,.T.);
#76820=ORIENTED_EDGE('',*,*,#53033,.T.);
#76821=ORIENTED_EDGE('',*,*,#53034,.T.);
#76822=ORIENTED_EDGE('',*,*,#53035,.T.);
#76823=ORIENTED_EDGE('',*,*,#53036,.T.);
#76824=ORIENTED_EDGE('',*,*,#53037,.T.);
#76825=ORIENTED_EDGE('',*,*,#53038,.F.);
#76826=ORIENTED_EDGE('',*,*,#53039,.T.);
#76827=ORIENTED_EDGE('',*,*,#53040,.T.);
#76828=ORIENTED_EDGE('',*,*,#53038,.T.);
#76829=ORIENTED_EDGE('',*,*,#53041,.T.);
#76830=ORIENTED_EDGE('',*,*,#53031,.F.);
#76831=ORIENTED_EDGE('',*,*,#53042,.T.);
#76832=ORIENTED_EDGE('',*,*,#53043,.F.);
#76833=ORIENTED_EDGE('',*,*,#53039,.F.);
#76834=ORIENTED_EDGE('',*,*,#53044,.F.);
#76835=ORIENTED_EDGE('',*,*,#53045,.F.);
#76836=ORIENTED_EDGE('',*,*,#53044,.T.);
#76837=ORIENTED_EDGE('',*,*,#53042,.F.);
#76838=ORIENTED_EDGE('',*,*,#53046,.F.);
#76839=ORIENTED_EDGE('',*,*,#53046,.T.);
#76840=ORIENTED_EDGE('',*,*,#53035,.F.);
#76841=ORIENTED_EDGE('',*,*,#53047,.F.);
#76842=ORIENTED_EDGE('',*,*,#53048,.F.);
#76843=ORIENTED_EDGE('',*,*,#53049,.T.);
#76844=ORIENTED_EDGE('',*,*,#53050,.F.);
#76845=ORIENTED_EDGE('',*,*,#53051,.F.);
#76846=ORIENTED_EDGE('',*,*,#50258,.F.);
#76847=ORIENTED_EDGE('',*,*,#53052,.T.);
#76848=ORIENTED_EDGE('',*,*,#53043,.T.);
#76849=ORIENTED_EDGE('',*,*,#53049,.F.);
#76850=ORIENTED_EDGE('',*,*,#50257,.T.);
#76851=ORIENTED_EDGE('',*,*,#53053,.F.);
#76852=ORIENTED_EDGE('',*,*,#53040,.F.);
#76853=ORIENTED_EDGE('',*,*,#53052,.F.);
#76854=ORIENTED_EDGE('',*,*,#50256,.F.);
#76855=ORIENTED_EDGE('',*,*,#53053,.T.);
#76856=ORIENTED_EDGE('',*,*,#50708,.F.);
#76857=ORIENTED_EDGE('',*,*,#53054,.F.);
#76858=ORIENTED_EDGE('',*,*,#53036,.F.);
#76859=ORIENTED_EDGE('',*,*,#53054,.T.);
#76860=ORIENTED_EDGE('',*,*,#49742,.F.);
#76861=ORIENTED_EDGE('',*,*,#53055,.F.);
#76862=ORIENTED_EDGE('',*,*,#53037,.F.);
#76863=ORIENTED_EDGE('',*,*,#53055,.T.);
#76864=ORIENTED_EDGE('',*,*,#49741,.F.);
#76865=ORIENTED_EDGE('',*,*,#53056,.F.);
#76866=ORIENTED_EDGE('',*,*,#53041,.F.);
#76867=ORIENTED_EDGE('',*,*,#53056,.T.);
#76868=ORIENTED_EDGE('',*,*,#49740,.F.);
#76869=ORIENTED_EDGE('',*,*,#53057,.F.);
#76870=ORIENTED_EDGE('',*,*,#53032,.F.);
#76871=ORIENTED_EDGE('',*,*,#53058,.T.);
#76872=ORIENTED_EDGE('',*,*,#53033,.F.);
#76873=ORIENTED_EDGE('',*,*,#53057,.T.);
#76874=ORIENTED_EDGE('',*,*,#50709,.F.);
#76875=ORIENTED_EDGE('',*,*,#53059,.T.);
#76876=ORIENTED_EDGE('',*,*,#53034,.F.);
#76877=ORIENTED_EDGE('',*,*,#53058,.F.);
#76878=ORIENTED_EDGE('',*,*,#50260,.F.);
#76879=ORIENTED_EDGE('',*,*,#53051,.T.);
#76880=ORIENTED_EDGE('',*,*,#53047,.T.);
#76881=ORIENTED_EDGE('',*,*,#53059,.F.);
#76882=ORIENTED_EDGE('',*,*,#50259,.T.);
#76883=ORIENTED_EDGE('',*,*,#53045,.T.);
#76884=ORIENTED_EDGE('',*,*,#53048,.T.);
#76885=ORIENTED_EDGE('',*,*,#53050,.T.);
#76886=ORIENTED_EDGE('',*,*,#53060,.T.);
#76887=ORIENTED_EDGE('',*,*,#53061,.T.);
#76888=ORIENTED_EDGE('',*,*,#53062,.T.);
#76889=ORIENTED_EDGE('',*,*,#53063,.T.);
#76890=ORIENTED_EDGE('',*,*,#53064,.T.);
#76891=ORIENTED_EDGE('',*,*,#53065,.T.);
#76892=ORIENTED_EDGE('',*,*,#53066,.T.);
#76893=ORIENTED_EDGE('',*,*,#53067,.F.);
#76894=ORIENTED_EDGE('',*,*,#53068,.T.);
#76895=ORIENTED_EDGE('',*,*,#53069,.T.);
#76896=ORIENTED_EDGE('',*,*,#53067,.T.);
#76897=ORIENTED_EDGE('',*,*,#53070,.T.);
#76898=ORIENTED_EDGE('',*,*,#53060,.F.);
#76899=ORIENTED_EDGE('',*,*,#53071,.T.);
#76900=ORIENTED_EDGE('',*,*,#53072,.F.);
#76901=ORIENTED_EDGE('',*,*,#53068,.F.);
#76902=ORIENTED_EDGE('',*,*,#53073,.F.);
#76903=ORIENTED_EDGE('',*,*,#53074,.F.);
#76904=ORIENTED_EDGE('',*,*,#53073,.T.);
#76905=ORIENTED_EDGE('',*,*,#53071,.F.);
#76906=ORIENTED_EDGE('',*,*,#53075,.F.);
#76907=ORIENTED_EDGE('',*,*,#53075,.T.);
#76908=ORIENTED_EDGE('',*,*,#53064,.F.);
#76909=ORIENTED_EDGE('',*,*,#53076,.F.);
#76910=ORIENTED_EDGE('',*,*,#53077,.F.);
#76911=ORIENTED_EDGE('',*,*,#53078,.T.);
#76912=ORIENTED_EDGE('',*,*,#53079,.F.);
#76913=ORIENTED_EDGE('',*,*,#53080,.F.);
#76914=ORIENTED_EDGE('',*,*,#50252,.F.);
#76915=ORIENTED_EDGE('',*,*,#53081,.T.);
#76916=ORIENTED_EDGE('',*,*,#53072,.T.);
#76917=ORIENTED_EDGE('',*,*,#53078,.F.);
#76918=ORIENTED_EDGE('',*,*,#50251,.T.);
#76919=ORIENTED_EDGE('',*,*,#53082,.F.);
#76920=ORIENTED_EDGE('',*,*,#53069,.F.);
#76921=ORIENTED_EDGE('',*,*,#53081,.F.);
#76922=ORIENTED_EDGE('',*,*,#50250,.F.);
#76923=ORIENTED_EDGE('',*,*,#53082,.T.);
#76924=ORIENTED_EDGE('',*,*,#50706,.F.);
#76925=ORIENTED_EDGE('',*,*,#53083,.F.);
#76926=ORIENTED_EDGE('',*,*,#53065,.F.);
#76927=ORIENTED_EDGE('',*,*,#53083,.T.);
#76928=ORIENTED_EDGE('',*,*,#49746,.F.);
#76929=ORIENTED_EDGE('',*,*,#53084,.F.);
#76930=ORIENTED_EDGE('',*,*,#53066,.F.);
#76931=ORIENTED_EDGE('',*,*,#53084,.T.);
#76932=ORIENTED_EDGE('',*,*,#49745,.F.);
#76933=ORIENTED_EDGE('',*,*,#53085,.F.);
#76934=ORIENTED_EDGE('',*,*,#53070,.F.);
#76935=ORIENTED_EDGE('',*,*,#53085,.T.);
#76936=ORIENTED_EDGE('',*,*,#49744,.F.);
#76937=ORIENTED_EDGE('',*,*,#53086,.F.);
#76938=ORIENTED_EDGE('',*,*,#53061,.F.);
#76939=ORIENTED_EDGE('',*,*,#53087,.T.);
#76940=ORIENTED_EDGE('',*,*,#53062,.F.);
#76941=ORIENTED_EDGE('',*,*,#53086,.T.);
#76942=ORIENTED_EDGE('',*,*,#50707,.F.);
#76943=ORIENTED_EDGE('',*,*,#53088,.T.);
#76944=ORIENTED_EDGE('',*,*,#53063,.F.);
#76945=ORIENTED_EDGE('',*,*,#53087,.F.);
#76946=ORIENTED_EDGE('',*,*,#50254,.F.);
#76947=ORIENTED_EDGE('',*,*,#53080,.T.);
#76948=ORIENTED_EDGE('',*,*,#53076,.T.);
#76949=ORIENTED_EDGE('',*,*,#53088,.F.);
#76950=ORIENTED_EDGE('',*,*,#50253,.T.);
#76951=ORIENTED_EDGE('',*,*,#53074,.T.);
#76952=ORIENTED_EDGE('',*,*,#53077,.T.);
#76953=ORIENTED_EDGE('',*,*,#53079,.T.);
#76954=ORIENTED_EDGE('',*,*,#53089,.T.);
#76955=ORIENTED_EDGE('',*,*,#53090,.T.);
#76956=ORIENTED_EDGE('',*,*,#53091,.T.);
#76957=ORIENTED_EDGE('',*,*,#53092,.T.);
#76958=ORIENTED_EDGE('',*,*,#53093,.T.);
#76959=ORIENTED_EDGE('',*,*,#53094,.T.);
#76960=ORIENTED_EDGE('',*,*,#53095,.T.);
#76961=ORIENTED_EDGE('',*,*,#53096,.F.);
#76962=ORIENTED_EDGE('',*,*,#53097,.T.);
#76963=ORIENTED_EDGE('',*,*,#53098,.T.);
#76964=ORIENTED_EDGE('',*,*,#53096,.T.);
#76965=ORIENTED_EDGE('',*,*,#53099,.T.);
#76966=ORIENTED_EDGE('',*,*,#53089,.F.);
#76967=ORIENTED_EDGE('',*,*,#53100,.T.);
#76968=ORIENTED_EDGE('',*,*,#53101,.F.);
#76969=ORIENTED_EDGE('',*,*,#53097,.F.);
#76970=ORIENTED_EDGE('',*,*,#53102,.F.);
#76971=ORIENTED_EDGE('',*,*,#53103,.F.);
#76972=ORIENTED_EDGE('',*,*,#53102,.T.);
#76973=ORIENTED_EDGE('',*,*,#53100,.F.);
#76974=ORIENTED_EDGE('',*,*,#53104,.F.);
#76975=ORIENTED_EDGE('',*,*,#53104,.T.);
#76976=ORIENTED_EDGE('',*,*,#53093,.F.);
#76977=ORIENTED_EDGE('',*,*,#53105,.F.);
#76978=ORIENTED_EDGE('',*,*,#53106,.F.);
#76979=ORIENTED_EDGE('',*,*,#53107,.T.);
#76980=ORIENTED_EDGE('',*,*,#53108,.F.);
#76981=ORIENTED_EDGE('',*,*,#53109,.F.);
#76982=ORIENTED_EDGE('',*,*,#50246,.F.);
#76983=ORIENTED_EDGE('',*,*,#53110,.T.);
#76984=ORIENTED_EDGE('',*,*,#53101,.T.);
#76985=ORIENTED_EDGE('',*,*,#53107,.F.);
#76986=ORIENTED_EDGE('',*,*,#50245,.T.);
#76987=ORIENTED_EDGE('',*,*,#53111,.F.);
#76988=ORIENTED_EDGE('',*,*,#53098,.F.);
#76989=ORIENTED_EDGE('',*,*,#53110,.F.);
#76990=ORIENTED_EDGE('',*,*,#50244,.F.);
#76991=ORIENTED_EDGE('',*,*,#53111,.T.);
#76992=ORIENTED_EDGE('',*,*,#50704,.F.);
#76993=ORIENTED_EDGE('',*,*,#53112,.F.);
#76994=ORIENTED_EDGE('',*,*,#53094,.F.);
#76995=ORIENTED_EDGE('',*,*,#53112,.T.);
#76996=ORIENTED_EDGE('',*,*,#49750,.F.);
#76997=ORIENTED_EDGE('',*,*,#53113,.F.);
#76998=ORIENTED_EDGE('',*,*,#53095,.F.);
#76999=ORIENTED_EDGE('',*,*,#53113,.T.);
#77000=ORIENTED_EDGE('',*,*,#49749,.F.);
#77001=ORIENTED_EDGE('',*,*,#53114,.F.);
#77002=ORIENTED_EDGE('',*,*,#53099,.F.);
#77003=ORIENTED_EDGE('',*,*,#53114,.T.);
#77004=ORIENTED_EDGE('',*,*,#49748,.F.);
#77005=ORIENTED_EDGE('',*,*,#53115,.F.);
#77006=ORIENTED_EDGE('',*,*,#53090,.F.);
#77007=ORIENTED_EDGE('',*,*,#53116,.T.);
#77008=ORIENTED_EDGE('',*,*,#53091,.F.);
#77009=ORIENTED_EDGE('',*,*,#53115,.T.);
#77010=ORIENTED_EDGE('',*,*,#50705,.F.);
#77011=ORIENTED_EDGE('',*,*,#53117,.T.);
#77012=ORIENTED_EDGE('',*,*,#53092,.F.);
#77013=ORIENTED_EDGE('',*,*,#53116,.F.);
#77014=ORIENTED_EDGE('',*,*,#50248,.F.);
#77015=ORIENTED_EDGE('',*,*,#53109,.T.);
#77016=ORIENTED_EDGE('',*,*,#53105,.T.);
#77017=ORIENTED_EDGE('',*,*,#53117,.F.);
#77018=ORIENTED_EDGE('',*,*,#50247,.T.);
#77019=ORIENTED_EDGE('',*,*,#53103,.T.);
#77020=ORIENTED_EDGE('',*,*,#53106,.T.);
#77021=ORIENTED_EDGE('',*,*,#53108,.T.);
#77022=ORIENTED_EDGE('',*,*,#53118,.T.);
#77023=ORIENTED_EDGE('',*,*,#53119,.T.);
#77024=ORIENTED_EDGE('',*,*,#53120,.T.);
#77025=ORIENTED_EDGE('',*,*,#53121,.T.);
#77026=ORIENTED_EDGE('',*,*,#53122,.T.);
#77027=ORIENTED_EDGE('',*,*,#53123,.T.);
#77028=ORIENTED_EDGE('',*,*,#53124,.T.);
#77029=ORIENTED_EDGE('',*,*,#53125,.F.);
#77030=ORIENTED_EDGE('',*,*,#53126,.T.);
#77031=ORIENTED_EDGE('',*,*,#53127,.T.);
#77032=ORIENTED_EDGE('',*,*,#53125,.T.);
#77033=ORIENTED_EDGE('',*,*,#53128,.T.);
#77034=ORIENTED_EDGE('',*,*,#53118,.F.);
#77035=ORIENTED_EDGE('',*,*,#53129,.T.);
#77036=ORIENTED_EDGE('',*,*,#53130,.F.);
#77037=ORIENTED_EDGE('',*,*,#53126,.F.);
#77038=ORIENTED_EDGE('',*,*,#53131,.F.);
#77039=ORIENTED_EDGE('',*,*,#53132,.F.);
#77040=ORIENTED_EDGE('',*,*,#53131,.T.);
#77041=ORIENTED_EDGE('',*,*,#53129,.F.);
#77042=ORIENTED_EDGE('',*,*,#53133,.F.);
#77043=ORIENTED_EDGE('',*,*,#53133,.T.);
#77044=ORIENTED_EDGE('',*,*,#53122,.F.);
#77045=ORIENTED_EDGE('',*,*,#53134,.F.);
#77046=ORIENTED_EDGE('',*,*,#53135,.F.);
#77047=ORIENTED_EDGE('',*,*,#53136,.T.);
#77048=ORIENTED_EDGE('',*,*,#53137,.F.);
#77049=ORIENTED_EDGE('',*,*,#53138,.F.);
#77050=ORIENTED_EDGE('',*,*,#50240,.F.);
#77051=ORIENTED_EDGE('',*,*,#53139,.T.);
#77052=ORIENTED_EDGE('',*,*,#53130,.T.);
#77053=ORIENTED_EDGE('',*,*,#53136,.F.);
#77054=ORIENTED_EDGE('',*,*,#50239,.T.);
#77055=ORIENTED_EDGE('',*,*,#53140,.F.);
#77056=ORIENTED_EDGE('',*,*,#53127,.F.);
#77057=ORIENTED_EDGE('',*,*,#53139,.F.);
#77058=ORIENTED_EDGE('',*,*,#50238,.F.);
#77059=ORIENTED_EDGE('',*,*,#53140,.T.);
#77060=ORIENTED_EDGE('',*,*,#50702,.F.);
#77061=ORIENTED_EDGE('',*,*,#53141,.F.);
#77062=ORIENTED_EDGE('',*,*,#53123,.F.);
#77063=ORIENTED_EDGE('',*,*,#53141,.T.);
#77064=ORIENTED_EDGE('',*,*,#49754,.F.);
#77065=ORIENTED_EDGE('',*,*,#53142,.F.);
#77066=ORIENTED_EDGE('',*,*,#53124,.F.);
#77067=ORIENTED_EDGE('',*,*,#53142,.T.);
#77068=ORIENTED_EDGE('',*,*,#49753,.F.);
#77069=ORIENTED_EDGE('',*,*,#53143,.F.);
#77070=ORIENTED_EDGE('',*,*,#53128,.F.);
#77071=ORIENTED_EDGE('',*,*,#53143,.T.);
#77072=ORIENTED_EDGE('',*,*,#49752,.F.);
#77073=ORIENTED_EDGE('',*,*,#53144,.F.);
#77074=ORIENTED_EDGE('',*,*,#53119,.F.);
#77075=ORIENTED_EDGE('',*,*,#53145,.T.);
#77076=ORIENTED_EDGE('',*,*,#53120,.F.);
#77077=ORIENTED_EDGE('',*,*,#53144,.T.);
#77078=ORIENTED_EDGE('',*,*,#50703,.F.);
#77079=ORIENTED_EDGE('',*,*,#53146,.T.);
#77080=ORIENTED_EDGE('',*,*,#53121,.F.);
#77081=ORIENTED_EDGE('',*,*,#53145,.F.);
#77082=ORIENTED_EDGE('',*,*,#50242,.F.);
#77083=ORIENTED_EDGE('',*,*,#53138,.T.);
#77084=ORIENTED_EDGE('',*,*,#53134,.T.);
#77085=ORIENTED_EDGE('',*,*,#53146,.F.);
#77086=ORIENTED_EDGE('',*,*,#50241,.T.);
#77087=ORIENTED_EDGE('',*,*,#53132,.T.);
#77088=ORIENTED_EDGE('',*,*,#53135,.T.);
#77089=ORIENTED_EDGE('',*,*,#53137,.T.);
#77090=ORIENTED_EDGE('',*,*,#53147,.T.);
#77091=ORIENTED_EDGE('',*,*,#53148,.T.);
#77092=ORIENTED_EDGE('',*,*,#53149,.T.);
#77093=ORIENTED_EDGE('',*,*,#53150,.T.);
#77094=ORIENTED_EDGE('',*,*,#53151,.T.);
#77095=ORIENTED_EDGE('',*,*,#53152,.T.);
#77096=ORIENTED_EDGE('',*,*,#53153,.T.);
#77097=ORIENTED_EDGE('',*,*,#53154,.F.);
#77098=ORIENTED_EDGE('',*,*,#53155,.T.);
#77099=ORIENTED_EDGE('',*,*,#53156,.T.);
#77100=ORIENTED_EDGE('',*,*,#53154,.T.);
#77101=ORIENTED_EDGE('',*,*,#53157,.T.);
#77102=ORIENTED_EDGE('',*,*,#53147,.F.);
#77103=ORIENTED_EDGE('',*,*,#53158,.T.);
#77104=ORIENTED_EDGE('',*,*,#53159,.F.);
#77105=ORIENTED_EDGE('',*,*,#53155,.F.);
#77106=ORIENTED_EDGE('',*,*,#53160,.F.);
#77107=ORIENTED_EDGE('',*,*,#53161,.F.);
#77108=ORIENTED_EDGE('',*,*,#53160,.T.);
#77109=ORIENTED_EDGE('',*,*,#53158,.F.);
#77110=ORIENTED_EDGE('',*,*,#53162,.F.);
#77111=ORIENTED_EDGE('',*,*,#53162,.T.);
#77112=ORIENTED_EDGE('',*,*,#53151,.F.);
#77113=ORIENTED_EDGE('',*,*,#53163,.F.);
#77114=ORIENTED_EDGE('',*,*,#53164,.F.);
#77115=ORIENTED_EDGE('',*,*,#53165,.T.);
#77116=ORIENTED_EDGE('',*,*,#53166,.F.);
#77117=ORIENTED_EDGE('',*,*,#53167,.F.);
#77118=ORIENTED_EDGE('',*,*,#50234,.F.);
#77119=ORIENTED_EDGE('',*,*,#53168,.T.);
#77120=ORIENTED_EDGE('',*,*,#53159,.T.);
#77121=ORIENTED_EDGE('',*,*,#53165,.F.);
#77122=ORIENTED_EDGE('',*,*,#50233,.T.);
#77123=ORIENTED_EDGE('',*,*,#53169,.F.);
#77124=ORIENTED_EDGE('',*,*,#53156,.F.);
#77125=ORIENTED_EDGE('',*,*,#53168,.F.);
#77126=ORIENTED_EDGE('',*,*,#50232,.F.);
#77127=ORIENTED_EDGE('',*,*,#53169,.T.);
#77128=ORIENTED_EDGE('',*,*,#50700,.F.);
#77129=ORIENTED_EDGE('',*,*,#53170,.F.);
#77130=ORIENTED_EDGE('',*,*,#53152,.F.);
#77131=ORIENTED_EDGE('',*,*,#53170,.T.);
#77132=ORIENTED_EDGE('',*,*,#49758,.F.);
#77133=ORIENTED_EDGE('',*,*,#53171,.F.);
#77134=ORIENTED_EDGE('',*,*,#53153,.F.);
#77135=ORIENTED_EDGE('',*,*,#53171,.T.);
#77136=ORIENTED_EDGE('',*,*,#49757,.F.);
#77137=ORIENTED_EDGE('',*,*,#53172,.F.);
#77138=ORIENTED_EDGE('',*,*,#53157,.F.);
#77139=ORIENTED_EDGE('',*,*,#53172,.T.);
#77140=ORIENTED_EDGE('',*,*,#49756,.F.);
#77141=ORIENTED_EDGE('',*,*,#53173,.F.);
#77142=ORIENTED_EDGE('',*,*,#53148,.F.);
#77143=ORIENTED_EDGE('',*,*,#53174,.T.);
#77144=ORIENTED_EDGE('',*,*,#53149,.F.);
#77145=ORIENTED_EDGE('',*,*,#53173,.T.);
#77146=ORIENTED_EDGE('',*,*,#50701,.F.);
#77147=ORIENTED_EDGE('',*,*,#53175,.T.);
#77148=ORIENTED_EDGE('',*,*,#53150,.F.);
#77149=ORIENTED_EDGE('',*,*,#53174,.F.);
#77150=ORIENTED_EDGE('',*,*,#50236,.F.);
#77151=ORIENTED_EDGE('',*,*,#53167,.T.);
#77152=ORIENTED_EDGE('',*,*,#53163,.T.);
#77153=ORIENTED_EDGE('',*,*,#53175,.F.);
#77154=ORIENTED_EDGE('',*,*,#50235,.T.);
#77155=ORIENTED_EDGE('',*,*,#53161,.T.);
#77156=ORIENTED_EDGE('',*,*,#53164,.T.);
#77157=ORIENTED_EDGE('',*,*,#53166,.T.);
#77158=ORIENTED_EDGE('',*,*,#53176,.T.);
#77159=ORIENTED_EDGE('',*,*,#53177,.T.);
#77160=ORIENTED_EDGE('',*,*,#53178,.T.);
#77161=ORIENTED_EDGE('',*,*,#53179,.T.);
#77162=ORIENTED_EDGE('',*,*,#53180,.T.);
#77163=ORIENTED_EDGE('',*,*,#53181,.T.);
#77164=ORIENTED_EDGE('',*,*,#53182,.T.);
#77165=ORIENTED_EDGE('',*,*,#53183,.F.);
#77166=ORIENTED_EDGE('',*,*,#53184,.T.);
#77167=ORIENTED_EDGE('',*,*,#53185,.T.);
#77168=ORIENTED_EDGE('',*,*,#53183,.T.);
#77169=ORIENTED_EDGE('',*,*,#53186,.T.);
#77170=ORIENTED_EDGE('',*,*,#53176,.F.);
#77171=ORIENTED_EDGE('',*,*,#53187,.T.);
#77172=ORIENTED_EDGE('',*,*,#53188,.F.);
#77173=ORIENTED_EDGE('',*,*,#53184,.F.);
#77174=ORIENTED_EDGE('',*,*,#53189,.F.);
#77175=ORIENTED_EDGE('',*,*,#53190,.F.);
#77176=ORIENTED_EDGE('',*,*,#53189,.T.);
#77177=ORIENTED_EDGE('',*,*,#53187,.F.);
#77178=ORIENTED_EDGE('',*,*,#53191,.F.);
#77179=ORIENTED_EDGE('',*,*,#53191,.T.);
#77180=ORIENTED_EDGE('',*,*,#53180,.F.);
#77181=ORIENTED_EDGE('',*,*,#53192,.F.);
#77182=ORIENTED_EDGE('',*,*,#53193,.F.);
#77183=ORIENTED_EDGE('',*,*,#53194,.T.);
#77184=ORIENTED_EDGE('',*,*,#53195,.F.);
#77185=ORIENTED_EDGE('',*,*,#53196,.F.);
#77186=ORIENTED_EDGE('',*,*,#50228,.F.);
#77187=ORIENTED_EDGE('',*,*,#53197,.T.);
#77188=ORIENTED_EDGE('',*,*,#53188,.T.);
#77189=ORIENTED_EDGE('',*,*,#53194,.F.);
#77190=ORIENTED_EDGE('',*,*,#50227,.T.);
#77191=ORIENTED_EDGE('',*,*,#53198,.F.);
#77192=ORIENTED_EDGE('',*,*,#53185,.F.);
#77193=ORIENTED_EDGE('',*,*,#53197,.F.);
#77194=ORIENTED_EDGE('',*,*,#50226,.F.);
#77195=ORIENTED_EDGE('',*,*,#53198,.T.);
#77196=ORIENTED_EDGE('',*,*,#50698,.F.);
#77197=ORIENTED_EDGE('',*,*,#53199,.F.);
#77198=ORIENTED_EDGE('',*,*,#53181,.F.);
#77199=ORIENTED_EDGE('',*,*,#53199,.T.);
#77200=ORIENTED_EDGE('',*,*,#49762,.F.);
#77201=ORIENTED_EDGE('',*,*,#53200,.F.);
#77202=ORIENTED_EDGE('',*,*,#53182,.F.);
#77203=ORIENTED_EDGE('',*,*,#53200,.T.);
#77204=ORIENTED_EDGE('',*,*,#49761,.F.);
#77205=ORIENTED_EDGE('',*,*,#53201,.F.);
#77206=ORIENTED_EDGE('',*,*,#53186,.F.);
#77207=ORIENTED_EDGE('',*,*,#53201,.T.);
#77208=ORIENTED_EDGE('',*,*,#49760,.F.);
#77209=ORIENTED_EDGE('',*,*,#53202,.F.);
#77210=ORIENTED_EDGE('',*,*,#53177,.F.);
#77211=ORIENTED_EDGE('',*,*,#53203,.T.);
#77212=ORIENTED_EDGE('',*,*,#53178,.F.);
#77213=ORIENTED_EDGE('',*,*,#53202,.T.);
#77214=ORIENTED_EDGE('',*,*,#50699,.F.);
#77215=ORIENTED_EDGE('',*,*,#53204,.T.);
#77216=ORIENTED_EDGE('',*,*,#53179,.F.);
#77217=ORIENTED_EDGE('',*,*,#53203,.F.);
#77218=ORIENTED_EDGE('',*,*,#50230,.F.);
#77219=ORIENTED_EDGE('',*,*,#53196,.T.);
#77220=ORIENTED_EDGE('',*,*,#53192,.T.);
#77221=ORIENTED_EDGE('',*,*,#53204,.F.);
#77222=ORIENTED_EDGE('',*,*,#50229,.T.);
#77223=ORIENTED_EDGE('',*,*,#53190,.T.);
#77224=ORIENTED_EDGE('',*,*,#53193,.T.);
#77225=ORIENTED_EDGE('',*,*,#53195,.T.);
#77226=ORIENTED_EDGE('',*,*,#53205,.T.);
#77227=ORIENTED_EDGE('',*,*,#53206,.T.);
#77228=ORIENTED_EDGE('',*,*,#53207,.T.);
#77229=ORIENTED_EDGE('',*,*,#53208,.T.);
#77230=ORIENTED_EDGE('',*,*,#53209,.T.);
#77231=ORIENTED_EDGE('',*,*,#53210,.T.);
#77232=ORIENTED_EDGE('',*,*,#53211,.T.);
#77233=ORIENTED_EDGE('',*,*,#53212,.F.);
#77234=ORIENTED_EDGE('',*,*,#53213,.T.);
#77235=ORIENTED_EDGE('',*,*,#53214,.T.);
#77236=ORIENTED_EDGE('',*,*,#53212,.T.);
#77237=ORIENTED_EDGE('',*,*,#53215,.T.);
#77238=ORIENTED_EDGE('',*,*,#53205,.F.);
#77239=ORIENTED_EDGE('',*,*,#53216,.T.);
#77240=ORIENTED_EDGE('',*,*,#53217,.F.);
#77241=ORIENTED_EDGE('',*,*,#53213,.F.);
#77242=ORIENTED_EDGE('',*,*,#53218,.F.);
#77243=ORIENTED_EDGE('',*,*,#53219,.F.);
#77244=ORIENTED_EDGE('',*,*,#53218,.T.);
#77245=ORIENTED_EDGE('',*,*,#53216,.F.);
#77246=ORIENTED_EDGE('',*,*,#53220,.F.);
#77247=ORIENTED_EDGE('',*,*,#53220,.T.);
#77248=ORIENTED_EDGE('',*,*,#53209,.F.);
#77249=ORIENTED_EDGE('',*,*,#53221,.F.);
#77250=ORIENTED_EDGE('',*,*,#53222,.F.);
#77251=ORIENTED_EDGE('',*,*,#53223,.T.);
#77252=ORIENTED_EDGE('',*,*,#53224,.F.);
#77253=ORIENTED_EDGE('',*,*,#53225,.F.);
#77254=ORIENTED_EDGE('',*,*,#50222,.F.);
#77255=ORIENTED_EDGE('',*,*,#53226,.T.);
#77256=ORIENTED_EDGE('',*,*,#53217,.T.);
#77257=ORIENTED_EDGE('',*,*,#53223,.F.);
#77258=ORIENTED_EDGE('',*,*,#50221,.T.);
#77259=ORIENTED_EDGE('',*,*,#53227,.F.);
#77260=ORIENTED_EDGE('',*,*,#53214,.F.);
#77261=ORIENTED_EDGE('',*,*,#53226,.F.);
#77262=ORIENTED_EDGE('',*,*,#50220,.F.);
#77263=ORIENTED_EDGE('',*,*,#53227,.T.);
#77264=ORIENTED_EDGE('',*,*,#50696,.F.);
#77265=ORIENTED_EDGE('',*,*,#53228,.F.);
#77266=ORIENTED_EDGE('',*,*,#53210,.F.);
#77267=ORIENTED_EDGE('',*,*,#53228,.T.);
#77268=ORIENTED_EDGE('',*,*,#49766,.F.);
#77269=ORIENTED_EDGE('',*,*,#53229,.F.);
#77270=ORIENTED_EDGE('',*,*,#53211,.F.);
#77271=ORIENTED_EDGE('',*,*,#53229,.T.);
#77272=ORIENTED_EDGE('',*,*,#49765,.F.);
#77273=ORIENTED_EDGE('',*,*,#53230,.F.);
#77274=ORIENTED_EDGE('',*,*,#53215,.F.);
#77275=ORIENTED_EDGE('',*,*,#53230,.T.);
#77276=ORIENTED_EDGE('',*,*,#49764,.F.);
#77277=ORIENTED_EDGE('',*,*,#53231,.F.);
#77278=ORIENTED_EDGE('',*,*,#53206,.F.);
#77279=ORIENTED_EDGE('',*,*,#53232,.T.);
#77280=ORIENTED_EDGE('',*,*,#53207,.F.);
#77281=ORIENTED_EDGE('',*,*,#53231,.T.);
#77282=ORIENTED_EDGE('',*,*,#50697,.F.);
#77283=ORIENTED_EDGE('',*,*,#53233,.T.);
#77284=ORIENTED_EDGE('',*,*,#53208,.F.);
#77285=ORIENTED_EDGE('',*,*,#53232,.F.);
#77286=ORIENTED_EDGE('',*,*,#50224,.F.);
#77287=ORIENTED_EDGE('',*,*,#53225,.T.);
#77288=ORIENTED_EDGE('',*,*,#53221,.T.);
#77289=ORIENTED_EDGE('',*,*,#53233,.F.);
#77290=ORIENTED_EDGE('',*,*,#50223,.T.);
#77291=ORIENTED_EDGE('',*,*,#53219,.T.);
#77292=ORIENTED_EDGE('',*,*,#53222,.T.);
#77293=ORIENTED_EDGE('',*,*,#53224,.T.);
#77294=ORIENTED_EDGE('',*,*,#53234,.T.);
#77295=ORIENTED_EDGE('',*,*,#53235,.T.);
#77296=ORIENTED_EDGE('',*,*,#53236,.T.);
#77297=ORIENTED_EDGE('',*,*,#53237,.T.);
#77298=ORIENTED_EDGE('',*,*,#53238,.T.);
#77299=ORIENTED_EDGE('',*,*,#53239,.T.);
#77300=ORIENTED_EDGE('',*,*,#53240,.T.);
#77301=ORIENTED_EDGE('',*,*,#53241,.F.);
#77302=ORIENTED_EDGE('',*,*,#53242,.T.);
#77303=ORIENTED_EDGE('',*,*,#53243,.T.);
#77304=ORIENTED_EDGE('',*,*,#53241,.T.);
#77305=ORIENTED_EDGE('',*,*,#53244,.T.);
#77306=ORIENTED_EDGE('',*,*,#53234,.F.);
#77307=ORIENTED_EDGE('',*,*,#53245,.T.);
#77308=ORIENTED_EDGE('',*,*,#53246,.F.);
#77309=ORIENTED_EDGE('',*,*,#53242,.F.);
#77310=ORIENTED_EDGE('',*,*,#53247,.F.);
#77311=ORIENTED_EDGE('',*,*,#53248,.F.);
#77312=ORIENTED_EDGE('',*,*,#53247,.T.);
#77313=ORIENTED_EDGE('',*,*,#53245,.F.);
#77314=ORIENTED_EDGE('',*,*,#53249,.F.);
#77315=ORIENTED_EDGE('',*,*,#53249,.T.);
#77316=ORIENTED_EDGE('',*,*,#53238,.F.);
#77317=ORIENTED_EDGE('',*,*,#53250,.F.);
#77318=ORIENTED_EDGE('',*,*,#53251,.F.);
#77319=ORIENTED_EDGE('',*,*,#53252,.T.);
#77320=ORIENTED_EDGE('',*,*,#53253,.F.);
#77321=ORIENTED_EDGE('',*,*,#53254,.F.);
#77322=ORIENTED_EDGE('',*,*,#50216,.F.);
#77323=ORIENTED_EDGE('',*,*,#53255,.T.);
#77324=ORIENTED_EDGE('',*,*,#53246,.T.);
#77325=ORIENTED_EDGE('',*,*,#53252,.F.);
#77326=ORIENTED_EDGE('',*,*,#50215,.T.);
#77327=ORIENTED_EDGE('',*,*,#53256,.F.);
#77328=ORIENTED_EDGE('',*,*,#53243,.F.);
#77329=ORIENTED_EDGE('',*,*,#53255,.F.);
#77330=ORIENTED_EDGE('',*,*,#50214,.F.);
#77331=ORIENTED_EDGE('',*,*,#53256,.T.);
#77332=ORIENTED_EDGE('',*,*,#50694,.F.);
#77333=ORIENTED_EDGE('',*,*,#53257,.F.);
#77334=ORIENTED_EDGE('',*,*,#53239,.F.);
#77335=ORIENTED_EDGE('',*,*,#53257,.T.);
#77336=ORIENTED_EDGE('',*,*,#49770,.F.);
#77337=ORIENTED_EDGE('',*,*,#53258,.F.);
#77338=ORIENTED_EDGE('',*,*,#53240,.F.);
#77339=ORIENTED_EDGE('',*,*,#53258,.T.);
#77340=ORIENTED_EDGE('',*,*,#49769,.F.);
#77341=ORIENTED_EDGE('',*,*,#53259,.F.);
#77342=ORIENTED_EDGE('',*,*,#53244,.F.);
#77343=ORIENTED_EDGE('',*,*,#53259,.T.);
#77344=ORIENTED_EDGE('',*,*,#49768,.F.);
#77345=ORIENTED_EDGE('',*,*,#53260,.F.);
#77346=ORIENTED_EDGE('',*,*,#53235,.F.);
#77347=ORIENTED_EDGE('',*,*,#53261,.T.);
#77348=ORIENTED_EDGE('',*,*,#53236,.F.);
#77349=ORIENTED_EDGE('',*,*,#53260,.T.);
#77350=ORIENTED_EDGE('',*,*,#50695,.F.);
#77351=ORIENTED_EDGE('',*,*,#53262,.T.);
#77352=ORIENTED_EDGE('',*,*,#53237,.F.);
#77353=ORIENTED_EDGE('',*,*,#53261,.F.);
#77354=ORIENTED_EDGE('',*,*,#50218,.F.);
#77355=ORIENTED_EDGE('',*,*,#53254,.T.);
#77356=ORIENTED_EDGE('',*,*,#53250,.T.);
#77357=ORIENTED_EDGE('',*,*,#53262,.F.);
#77358=ORIENTED_EDGE('',*,*,#50217,.T.);
#77359=ORIENTED_EDGE('',*,*,#53248,.T.);
#77360=ORIENTED_EDGE('',*,*,#53251,.T.);
#77361=ORIENTED_EDGE('',*,*,#53253,.T.);
#77362=ORIENTED_EDGE('',*,*,#53263,.T.);
#77363=ORIENTED_EDGE('',*,*,#53264,.T.);
#77364=ORIENTED_EDGE('',*,*,#53265,.T.);
#77365=ORIENTED_EDGE('',*,*,#53266,.T.);
#77366=ORIENTED_EDGE('',*,*,#53267,.T.);
#77367=ORIENTED_EDGE('',*,*,#53268,.T.);
#77368=ORIENTED_EDGE('',*,*,#53269,.T.);
#77369=ORIENTED_EDGE('',*,*,#53270,.F.);
#77370=ORIENTED_EDGE('',*,*,#53271,.T.);
#77371=ORIENTED_EDGE('',*,*,#53272,.T.);
#77372=ORIENTED_EDGE('',*,*,#53270,.T.);
#77373=ORIENTED_EDGE('',*,*,#53273,.T.);
#77374=ORIENTED_EDGE('',*,*,#53263,.F.);
#77375=ORIENTED_EDGE('',*,*,#53274,.T.);
#77376=ORIENTED_EDGE('',*,*,#53275,.F.);
#77377=ORIENTED_EDGE('',*,*,#53271,.F.);
#77378=ORIENTED_EDGE('',*,*,#53276,.F.);
#77379=ORIENTED_EDGE('',*,*,#53277,.F.);
#77380=ORIENTED_EDGE('',*,*,#53276,.T.);
#77381=ORIENTED_EDGE('',*,*,#53274,.F.);
#77382=ORIENTED_EDGE('',*,*,#53278,.F.);
#77383=ORIENTED_EDGE('',*,*,#53278,.T.);
#77384=ORIENTED_EDGE('',*,*,#53267,.F.);
#77385=ORIENTED_EDGE('',*,*,#53279,.F.);
#77386=ORIENTED_EDGE('',*,*,#53280,.F.);
#77387=ORIENTED_EDGE('',*,*,#53281,.T.);
#77388=ORIENTED_EDGE('',*,*,#53282,.F.);
#77389=ORIENTED_EDGE('',*,*,#53283,.F.);
#77390=ORIENTED_EDGE('',*,*,#50210,.F.);
#77391=ORIENTED_EDGE('',*,*,#53284,.T.);
#77392=ORIENTED_EDGE('',*,*,#53275,.T.);
#77393=ORIENTED_EDGE('',*,*,#53281,.F.);
#77394=ORIENTED_EDGE('',*,*,#50209,.T.);
#77395=ORIENTED_EDGE('',*,*,#53285,.F.);
#77396=ORIENTED_EDGE('',*,*,#53272,.F.);
#77397=ORIENTED_EDGE('',*,*,#53284,.F.);
#77398=ORIENTED_EDGE('',*,*,#50208,.F.);
#77399=ORIENTED_EDGE('',*,*,#53285,.T.);
#77400=ORIENTED_EDGE('',*,*,#50692,.F.);
#77401=ORIENTED_EDGE('',*,*,#53286,.F.);
#77402=ORIENTED_EDGE('',*,*,#53268,.F.);
#77403=ORIENTED_EDGE('',*,*,#53286,.T.);
#77404=ORIENTED_EDGE('',*,*,#49774,.F.);
#77405=ORIENTED_EDGE('',*,*,#53287,.F.);
#77406=ORIENTED_EDGE('',*,*,#53269,.F.);
#77407=ORIENTED_EDGE('',*,*,#53287,.T.);
#77408=ORIENTED_EDGE('',*,*,#49773,.F.);
#77409=ORIENTED_EDGE('',*,*,#53288,.F.);
#77410=ORIENTED_EDGE('',*,*,#53273,.F.);
#77411=ORIENTED_EDGE('',*,*,#53288,.T.);
#77412=ORIENTED_EDGE('',*,*,#49772,.F.);
#77413=ORIENTED_EDGE('',*,*,#53289,.F.);
#77414=ORIENTED_EDGE('',*,*,#53264,.F.);
#77415=ORIENTED_EDGE('',*,*,#53290,.T.);
#77416=ORIENTED_EDGE('',*,*,#53265,.F.);
#77417=ORIENTED_EDGE('',*,*,#53289,.T.);
#77418=ORIENTED_EDGE('',*,*,#50693,.F.);
#77419=ORIENTED_EDGE('',*,*,#53291,.T.);
#77420=ORIENTED_EDGE('',*,*,#53266,.F.);
#77421=ORIENTED_EDGE('',*,*,#53290,.F.);
#77422=ORIENTED_EDGE('',*,*,#50212,.F.);
#77423=ORIENTED_EDGE('',*,*,#53283,.T.);
#77424=ORIENTED_EDGE('',*,*,#53279,.T.);
#77425=ORIENTED_EDGE('',*,*,#53291,.F.);
#77426=ORIENTED_EDGE('',*,*,#50211,.T.);
#77427=ORIENTED_EDGE('',*,*,#53277,.T.);
#77428=ORIENTED_EDGE('',*,*,#53280,.T.);
#77429=ORIENTED_EDGE('',*,*,#53282,.T.);
#77430=ORIENTED_EDGE('',*,*,#53292,.T.);
#77431=ORIENTED_EDGE('',*,*,#53293,.T.);
#77432=ORIENTED_EDGE('',*,*,#53294,.T.);
#77433=ORIENTED_EDGE('',*,*,#53295,.T.);
#77434=ORIENTED_EDGE('',*,*,#53296,.T.);
#77435=ORIENTED_EDGE('',*,*,#53297,.T.);
#77436=ORIENTED_EDGE('',*,*,#53298,.T.);
#77437=ORIENTED_EDGE('',*,*,#53299,.F.);
#77438=ORIENTED_EDGE('',*,*,#53300,.T.);
#77439=ORIENTED_EDGE('',*,*,#53301,.T.);
#77440=ORIENTED_EDGE('',*,*,#53299,.T.);
#77441=ORIENTED_EDGE('',*,*,#53302,.T.);
#77442=ORIENTED_EDGE('',*,*,#53292,.F.);
#77443=ORIENTED_EDGE('',*,*,#53303,.T.);
#77444=ORIENTED_EDGE('',*,*,#53304,.F.);
#77445=ORIENTED_EDGE('',*,*,#53300,.F.);
#77446=ORIENTED_EDGE('',*,*,#53305,.F.);
#77447=ORIENTED_EDGE('',*,*,#53306,.F.);
#77448=ORIENTED_EDGE('',*,*,#53305,.T.);
#77449=ORIENTED_EDGE('',*,*,#53303,.F.);
#77450=ORIENTED_EDGE('',*,*,#53307,.F.);
#77451=ORIENTED_EDGE('',*,*,#53307,.T.);
#77452=ORIENTED_EDGE('',*,*,#53296,.F.);
#77453=ORIENTED_EDGE('',*,*,#53308,.F.);
#77454=ORIENTED_EDGE('',*,*,#53309,.F.);
#77455=ORIENTED_EDGE('',*,*,#53310,.T.);
#77456=ORIENTED_EDGE('',*,*,#53311,.F.);
#77457=ORIENTED_EDGE('',*,*,#53312,.F.);
#77458=ORIENTED_EDGE('',*,*,#50204,.F.);
#77459=ORIENTED_EDGE('',*,*,#53313,.T.);
#77460=ORIENTED_EDGE('',*,*,#53304,.T.);
#77461=ORIENTED_EDGE('',*,*,#53310,.F.);
#77462=ORIENTED_EDGE('',*,*,#50203,.T.);
#77463=ORIENTED_EDGE('',*,*,#53314,.F.);
#77464=ORIENTED_EDGE('',*,*,#53301,.F.);
#77465=ORIENTED_EDGE('',*,*,#53313,.F.);
#77466=ORIENTED_EDGE('',*,*,#50202,.F.);
#77467=ORIENTED_EDGE('',*,*,#53314,.T.);
#77468=ORIENTED_EDGE('',*,*,#50690,.F.);
#77469=ORIENTED_EDGE('',*,*,#53315,.F.);
#77470=ORIENTED_EDGE('',*,*,#53297,.F.);
#77471=ORIENTED_EDGE('',*,*,#53315,.T.);
#77472=ORIENTED_EDGE('',*,*,#49778,.F.);
#77473=ORIENTED_EDGE('',*,*,#53316,.F.);
#77474=ORIENTED_EDGE('',*,*,#53298,.F.);
#77475=ORIENTED_EDGE('',*,*,#53316,.T.);
#77476=ORIENTED_EDGE('',*,*,#49777,.F.);
#77477=ORIENTED_EDGE('',*,*,#53317,.F.);
#77478=ORIENTED_EDGE('',*,*,#53302,.F.);
#77479=ORIENTED_EDGE('',*,*,#53317,.T.);
#77480=ORIENTED_EDGE('',*,*,#49776,.F.);
#77481=ORIENTED_EDGE('',*,*,#53318,.F.);
#77482=ORIENTED_EDGE('',*,*,#53293,.F.);
#77483=ORIENTED_EDGE('',*,*,#53319,.T.);
#77484=ORIENTED_EDGE('',*,*,#53294,.F.);
#77485=ORIENTED_EDGE('',*,*,#53318,.T.);
#77486=ORIENTED_EDGE('',*,*,#50691,.F.);
#77487=ORIENTED_EDGE('',*,*,#53320,.T.);
#77488=ORIENTED_EDGE('',*,*,#53295,.F.);
#77489=ORIENTED_EDGE('',*,*,#53319,.F.);
#77490=ORIENTED_EDGE('',*,*,#50206,.F.);
#77491=ORIENTED_EDGE('',*,*,#53312,.T.);
#77492=ORIENTED_EDGE('',*,*,#53308,.T.);
#77493=ORIENTED_EDGE('',*,*,#53320,.F.);
#77494=ORIENTED_EDGE('',*,*,#50205,.T.);
#77495=ORIENTED_EDGE('',*,*,#53306,.T.);
#77496=ORIENTED_EDGE('',*,*,#53309,.T.);
#77497=ORIENTED_EDGE('',*,*,#53311,.T.);
#77498=ORIENTED_EDGE('',*,*,#53321,.T.);
#77499=ORIENTED_EDGE('',*,*,#53322,.T.);
#77500=ORIENTED_EDGE('',*,*,#53323,.T.);
#77501=ORIENTED_EDGE('',*,*,#53324,.T.);
#77502=ORIENTED_EDGE('',*,*,#53325,.T.);
#77503=ORIENTED_EDGE('',*,*,#53326,.T.);
#77504=ORIENTED_EDGE('',*,*,#53327,.T.);
#77505=ORIENTED_EDGE('',*,*,#53328,.F.);
#77506=ORIENTED_EDGE('',*,*,#53329,.T.);
#77507=ORIENTED_EDGE('',*,*,#53330,.T.);
#77508=ORIENTED_EDGE('',*,*,#53328,.T.);
#77509=ORIENTED_EDGE('',*,*,#53331,.T.);
#77510=ORIENTED_EDGE('',*,*,#53321,.F.);
#77511=ORIENTED_EDGE('',*,*,#53332,.T.);
#77512=ORIENTED_EDGE('',*,*,#53333,.F.);
#77513=ORIENTED_EDGE('',*,*,#53329,.F.);
#77514=ORIENTED_EDGE('',*,*,#53334,.F.);
#77515=ORIENTED_EDGE('',*,*,#53335,.F.);
#77516=ORIENTED_EDGE('',*,*,#53334,.T.);
#77517=ORIENTED_EDGE('',*,*,#53332,.F.);
#77518=ORIENTED_EDGE('',*,*,#53336,.F.);
#77519=ORIENTED_EDGE('',*,*,#53336,.T.);
#77520=ORIENTED_EDGE('',*,*,#53325,.F.);
#77521=ORIENTED_EDGE('',*,*,#53337,.F.);
#77522=ORIENTED_EDGE('',*,*,#53338,.F.);
#77523=ORIENTED_EDGE('',*,*,#53339,.T.);
#77524=ORIENTED_EDGE('',*,*,#53340,.F.);
#77525=ORIENTED_EDGE('',*,*,#53341,.F.);
#77526=ORIENTED_EDGE('',*,*,#50198,.F.);
#77527=ORIENTED_EDGE('',*,*,#53342,.T.);
#77528=ORIENTED_EDGE('',*,*,#53333,.T.);
#77529=ORIENTED_EDGE('',*,*,#53339,.F.);
#77530=ORIENTED_EDGE('',*,*,#50197,.T.);
#77531=ORIENTED_EDGE('',*,*,#53343,.F.);
#77532=ORIENTED_EDGE('',*,*,#53330,.F.);
#77533=ORIENTED_EDGE('',*,*,#53342,.F.);
#77534=ORIENTED_EDGE('',*,*,#50196,.F.);
#77535=ORIENTED_EDGE('',*,*,#53343,.T.);
#77536=ORIENTED_EDGE('',*,*,#50688,.F.);
#77537=ORIENTED_EDGE('',*,*,#53344,.F.);
#77538=ORIENTED_EDGE('',*,*,#53326,.F.);
#77539=ORIENTED_EDGE('',*,*,#53344,.T.);
#77540=ORIENTED_EDGE('',*,*,#49782,.F.);
#77541=ORIENTED_EDGE('',*,*,#53345,.F.);
#77542=ORIENTED_EDGE('',*,*,#53327,.F.);
#77543=ORIENTED_EDGE('',*,*,#53345,.T.);
#77544=ORIENTED_EDGE('',*,*,#49781,.F.);
#77545=ORIENTED_EDGE('',*,*,#53346,.F.);
#77546=ORIENTED_EDGE('',*,*,#53331,.F.);
#77547=ORIENTED_EDGE('',*,*,#53346,.T.);
#77548=ORIENTED_EDGE('',*,*,#49780,.F.);
#77549=ORIENTED_EDGE('',*,*,#53347,.F.);
#77550=ORIENTED_EDGE('',*,*,#53322,.F.);
#77551=ORIENTED_EDGE('',*,*,#53348,.T.);
#77552=ORIENTED_EDGE('',*,*,#53323,.F.);
#77553=ORIENTED_EDGE('',*,*,#53347,.T.);
#77554=ORIENTED_EDGE('',*,*,#50689,.F.);
#77555=ORIENTED_EDGE('',*,*,#53349,.T.);
#77556=ORIENTED_EDGE('',*,*,#53324,.F.);
#77557=ORIENTED_EDGE('',*,*,#53348,.F.);
#77558=ORIENTED_EDGE('',*,*,#50200,.F.);
#77559=ORIENTED_EDGE('',*,*,#53341,.T.);
#77560=ORIENTED_EDGE('',*,*,#53337,.T.);
#77561=ORIENTED_EDGE('',*,*,#53349,.F.);
#77562=ORIENTED_EDGE('',*,*,#50199,.T.);
#77563=ORIENTED_EDGE('',*,*,#53335,.T.);
#77564=ORIENTED_EDGE('',*,*,#53338,.T.);
#77565=ORIENTED_EDGE('',*,*,#53340,.T.);
#77566=ORIENTED_EDGE('',*,*,#53350,.T.);
#77567=ORIENTED_EDGE('',*,*,#53351,.T.);
#77568=ORIENTED_EDGE('',*,*,#53352,.T.);
#77569=ORIENTED_EDGE('',*,*,#53353,.T.);
#77570=ORIENTED_EDGE('',*,*,#53354,.T.);
#77571=ORIENTED_EDGE('',*,*,#53355,.T.);
#77572=ORIENTED_EDGE('',*,*,#53356,.T.);
#77573=ORIENTED_EDGE('',*,*,#53357,.F.);
#77574=ORIENTED_EDGE('',*,*,#53358,.T.);
#77575=ORIENTED_EDGE('',*,*,#53359,.T.);
#77576=ORIENTED_EDGE('',*,*,#53357,.T.);
#77577=ORIENTED_EDGE('',*,*,#53360,.T.);
#77578=ORIENTED_EDGE('',*,*,#53350,.F.);
#77579=ORIENTED_EDGE('',*,*,#53361,.T.);
#77580=ORIENTED_EDGE('',*,*,#53362,.F.);
#77581=ORIENTED_EDGE('',*,*,#53358,.F.);
#77582=ORIENTED_EDGE('',*,*,#53363,.F.);
#77583=ORIENTED_EDGE('',*,*,#53364,.F.);
#77584=ORIENTED_EDGE('',*,*,#53363,.T.);
#77585=ORIENTED_EDGE('',*,*,#53361,.F.);
#77586=ORIENTED_EDGE('',*,*,#53365,.F.);
#77587=ORIENTED_EDGE('',*,*,#53365,.T.);
#77588=ORIENTED_EDGE('',*,*,#53354,.F.);
#77589=ORIENTED_EDGE('',*,*,#53366,.F.);
#77590=ORIENTED_EDGE('',*,*,#53367,.F.);
#77591=ORIENTED_EDGE('',*,*,#53368,.T.);
#77592=ORIENTED_EDGE('',*,*,#53369,.F.);
#77593=ORIENTED_EDGE('',*,*,#53370,.F.);
#77594=ORIENTED_EDGE('',*,*,#50192,.F.);
#77595=ORIENTED_EDGE('',*,*,#53371,.T.);
#77596=ORIENTED_EDGE('',*,*,#53362,.T.);
#77597=ORIENTED_EDGE('',*,*,#53368,.F.);
#77598=ORIENTED_EDGE('',*,*,#50191,.T.);
#77599=ORIENTED_EDGE('',*,*,#53372,.F.);
#77600=ORIENTED_EDGE('',*,*,#53359,.F.);
#77601=ORIENTED_EDGE('',*,*,#53371,.F.);
#77602=ORIENTED_EDGE('',*,*,#50190,.F.);
#77603=ORIENTED_EDGE('',*,*,#53372,.T.);
#77604=ORIENTED_EDGE('',*,*,#50686,.F.);
#77605=ORIENTED_EDGE('',*,*,#53373,.F.);
#77606=ORIENTED_EDGE('',*,*,#53355,.F.);
#77607=ORIENTED_EDGE('',*,*,#53373,.T.);
#77608=ORIENTED_EDGE('',*,*,#49786,.F.);
#77609=ORIENTED_EDGE('',*,*,#53374,.F.);
#77610=ORIENTED_EDGE('',*,*,#53356,.F.);
#77611=ORIENTED_EDGE('',*,*,#53374,.T.);
#77612=ORIENTED_EDGE('',*,*,#49785,.F.);
#77613=ORIENTED_EDGE('',*,*,#53375,.F.);
#77614=ORIENTED_EDGE('',*,*,#53360,.F.);
#77615=ORIENTED_EDGE('',*,*,#53375,.T.);
#77616=ORIENTED_EDGE('',*,*,#49784,.F.);
#77617=ORIENTED_EDGE('',*,*,#53376,.F.);
#77618=ORIENTED_EDGE('',*,*,#53351,.F.);
#77619=ORIENTED_EDGE('',*,*,#53377,.T.);
#77620=ORIENTED_EDGE('',*,*,#53352,.F.);
#77621=ORIENTED_EDGE('',*,*,#53376,.T.);
#77622=ORIENTED_EDGE('',*,*,#50687,.F.);
#77623=ORIENTED_EDGE('',*,*,#53378,.T.);
#77624=ORIENTED_EDGE('',*,*,#53353,.F.);
#77625=ORIENTED_EDGE('',*,*,#53377,.F.);
#77626=ORIENTED_EDGE('',*,*,#50194,.F.);
#77627=ORIENTED_EDGE('',*,*,#53370,.T.);
#77628=ORIENTED_EDGE('',*,*,#53366,.T.);
#77629=ORIENTED_EDGE('',*,*,#53378,.F.);
#77630=ORIENTED_EDGE('',*,*,#50193,.T.);
#77631=ORIENTED_EDGE('',*,*,#53364,.T.);
#77632=ORIENTED_EDGE('',*,*,#53367,.T.);
#77633=ORIENTED_EDGE('',*,*,#53369,.T.);
#77634=ORIENTED_EDGE('',*,*,#53379,.T.);
#77635=ORIENTED_EDGE('',*,*,#53380,.T.);
#77636=ORIENTED_EDGE('',*,*,#53381,.T.);
#77637=ORIENTED_EDGE('',*,*,#53382,.T.);
#77638=ORIENTED_EDGE('',*,*,#53383,.T.);
#77639=ORIENTED_EDGE('',*,*,#53384,.T.);
#77640=ORIENTED_EDGE('',*,*,#53385,.T.);
#77641=ORIENTED_EDGE('',*,*,#53386,.F.);
#77642=ORIENTED_EDGE('',*,*,#53387,.T.);
#77643=ORIENTED_EDGE('',*,*,#53388,.T.);
#77644=ORIENTED_EDGE('',*,*,#53386,.T.);
#77645=ORIENTED_EDGE('',*,*,#53389,.T.);
#77646=ORIENTED_EDGE('',*,*,#53379,.F.);
#77647=ORIENTED_EDGE('',*,*,#53390,.T.);
#77648=ORIENTED_EDGE('',*,*,#53391,.F.);
#77649=ORIENTED_EDGE('',*,*,#53387,.F.);
#77650=ORIENTED_EDGE('',*,*,#53392,.F.);
#77651=ORIENTED_EDGE('',*,*,#53393,.F.);
#77652=ORIENTED_EDGE('',*,*,#53392,.T.);
#77653=ORIENTED_EDGE('',*,*,#53390,.F.);
#77654=ORIENTED_EDGE('',*,*,#53394,.F.);
#77655=ORIENTED_EDGE('',*,*,#53394,.T.);
#77656=ORIENTED_EDGE('',*,*,#53383,.F.);
#77657=ORIENTED_EDGE('',*,*,#53395,.F.);
#77658=ORIENTED_EDGE('',*,*,#53396,.F.);
#77659=ORIENTED_EDGE('',*,*,#53397,.T.);
#77660=ORIENTED_EDGE('',*,*,#53398,.F.);
#77661=ORIENTED_EDGE('',*,*,#53399,.F.);
#77662=ORIENTED_EDGE('',*,*,#50186,.F.);
#77663=ORIENTED_EDGE('',*,*,#53400,.T.);
#77664=ORIENTED_EDGE('',*,*,#53391,.T.);
#77665=ORIENTED_EDGE('',*,*,#53397,.F.);
#77666=ORIENTED_EDGE('',*,*,#50185,.T.);
#77667=ORIENTED_EDGE('',*,*,#53401,.F.);
#77668=ORIENTED_EDGE('',*,*,#53388,.F.);
#77669=ORIENTED_EDGE('',*,*,#53400,.F.);
#77670=ORIENTED_EDGE('',*,*,#50184,.F.);
#77671=ORIENTED_EDGE('',*,*,#53401,.T.);
#77672=ORIENTED_EDGE('',*,*,#50684,.F.);
#77673=ORIENTED_EDGE('',*,*,#53402,.F.);
#77674=ORIENTED_EDGE('',*,*,#53384,.F.);
#77675=ORIENTED_EDGE('',*,*,#53402,.T.);
#77676=ORIENTED_EDGE('',*,*,#49790,.F.);
#77677=ORIENTED_EDGE('',*,*,#53403,.F.);
#77678=ORIENTED_EDGE('',*,*,#53385,.F.);
#77679=ORIENTED_EDGE('',*,*,#53403,.T.);
#77680=ORIENTED_EDGE('',*,*,#49789,.F.);
#77681=ORIENTED_EDGE('',*,*,#53404,.F.);
#77682=ORIENTED_EDGE('',*,*,#53389,.F.);
#77683=ORIENTED_EDGE('',*,*,#53404,.T.);
#77684=ORIENTED_EDGE('',*,*,#49788,.F.);
#77685=ORIENTED_EDGE('',*,*,#53405,.F.);
#77686=ORIENTED_EDGE('',*,*,#53380,.F.);
#77687=ORIENTED_EDGE('',*,*,#53406,.T.);
#77688=ORIENTED_EDGE('',*,*,#53381,.F.);
#77689=ORIENTED_EDGE('',*,*,#53405,.T.);
#77690=ORIENTED_EDGE('',*,*,#50685,.F.);
#77691=ORIENTED_EDGE('',*,*,#53407,.T.);
#77692=ORIENTED_EDGE('',*,*,#53382,.F.);
#77693=ORIENTED_EDGE('',*,*,#53406,.F.);
#77694=ORIENTED_EDGE('',*,*,#50188,.F.);
#77695=ORIENTED_EDGE('',*,*,#53399,.T.);
#77696=ORIENTED_EDGE('',*,*,#53395,.T.);
#77697=ORIENTED_EDGE('',*,*,#53407,.F.);
#77698=ORIENTED_EDGE('',*,*,#50187,.T.);
#77699=ORIENTED_EDGE('',*,*,#53393,.T.);
#77700=ORIENTED_EDGE('',*,*,#53396,.T.);
#77701=ORIENTED_EDGE('',*,*,#53398,.T.);
#77702=ORIENTED_EDGE('',*,*,#53408,.T.);
#77703=ORIENTED_EDGE('',*,*,#53409,.T.);
#77704=ORIENTED_EDGE('',*,*,#53410,.T.);
#77705=ORIENTED_EDGE('',*,*,#53411,.T.);
#77706=ORIENTED_EDGE('',*,*,#53412,.T.);
#77707=ORIENTED_EDGE('',*,*,#53413,.T.);
#77708=ORIENTED_EDGE('',*,*,#53414,.T.);
#77709=ORIENTED_EDGE('',*,*,#53415,.F.);
#77710=ORIENTED_EDGE('',*,*,#53416,.T.);
#77711=ORIENTED_EDGE('',*,*,#53417,.T.);
#77712=ORIENTED_EDGE('',*,*,#53415,.T.);
#77713=ORIENTED_EDGE('',*,*,#53418,.T.);
#77714=ORIENTED_EDGE('',*,*,#53408,.F.);
#77715=ORIENTED_EDGE('',*,*,#53419,.T.);
#77716=ORIENTED_EDGE('',*,*,#53420,.F.);
#77717=ORIENTED_EDGE('',*,*,#53416,.F.);
#77718=ORIENTED_EDGE('',*,*,#53421,.F.);
#77719=ORIENTED_EDGE('',*,*,#53422,.F.);
#77720=ORIENTED_EDGE('',*,*,#53421,.T.);
#77721=ORIENTED_EDGE('',*,*,#53419,.F.);
#77722=ORIENTED_EDGE('',*,*,#53423,.F.);
#77723=ORIENTED_EDGE('',*,*,#53423,.T.);
#77724=ORIENTED_EDGE('',*,*,#53412,.F.);
#77725=ORIENTED_EDGE('',*,*,#53424,.F.);
#77726=ORIENTED_EDGE('',*,*,#53425,.F.);
#77727=ORIENTED_EDGE('',*,*,#53426,.T.);
#77728=ORIENTED_EDGE('',*,*,#53427,.F.);
#77729=ORIENTED_EDGE('',*,*,#53428,.F.);
#77730=ORIENTED_EDGE('',*,*,#50180,.F.);
#77731=ORIENTED_EDGE('',*,*,#53429,.T.);
#77732=ORIENTED_EDGE('',*,*,#53420,.T.);
#77733=ORIENTED_EDGE('',*,*,#53426,.F.);
#77734=ORIENTED_EDGE('',*,*,#50179,.T.);
#77735=ORIENTED_EDGE('',*,*,#53430,.F.);
#77736=ORIENTED_EDGE('',*,*,#53417,.F.);
#77737=ORIENTED_EDGE('',*,*,#53429,.F.);
#77738=ORIENTED_EDGE('',*,*,#50178,.F.);
#77739=ORIENTED_EDGE('',*,*,#53430,.T.);
#77740=ORIENTED_EDGE('',*,*,#50682,.F.);
#77741=ORIENTED_EDGE('',*,*,#53431,.F.);
#77742=ORIENTED_EDGE('',*,*,#53413,.F.);
#77743=ORIENTED_EDGE('',*,*,#53431,.T.);
#77744=ORIENTED_EDGE('',*,*,#49794,.F.);
#77745=ORIENTED_EDGE('',*,*,#53432,.F.);
#77746=ORIENTED_EDGE('',*,*,#53414,.F.);
#77747=ORIENTED_EDGE('',*,*,#53432,.T.);
#77748=ORIENTED_EDGE('',*,*,#49793,.F.);
#77749=ORIENTED_EDGE('',*,*,#53433,.F.);
#77750=ORIENTED_EDGE('',*,*,#53418,.F.);
#77751=ORIENTED_EDGE('',*,*,#53433,.T.);
#77752=ORIENTED_EDGE('',*,*,#49792,.F.);
#77753=ORIENTED_EDGE('',*,*,#53434,.F.);
#77754=ORIENTED_EDGE('',*,*,#53409,.F.);
#77755=ORIENTED_EDGE('',*,*,#53435,.T.);
#77756=ORIENTED_EDGE('',*,*,#53410,.F.);
#77757=ORIENTED_EDGE('',*,*,#53434,.T.);
#77758=ORIENTED_EDGE('',*,*,#50683,.F.);
#77759=ORIENTED_EDGE('',*,*,#53436,.T.);
#77760=ORIENTED_EDGE('',*,*,#53411,.F.);
#77761=ORIENTED_EDGE('',*,*,#53435,.F.);
#77762=ORIENTED_EDGE('',*,*,#50182,.F.);
#77763=ORIENTED_EDGE('',*,*,#53428,.T.);
#77764=ORIENTED_EDGE('',*,*,#53424,.T.);
#77765=ORIENTED_EDGE('',*,*,#53436,.F.);
#77766=ORIENTED_EDGE('',*,*,#50181,.T.);
#77767=ORIENTED_EDGE('',*,*,#53422,.T.);
#77768=ORIENTED_EDGE('',*,*,#53425,.T.);
#77769=ORIENTED_EDGE('',*,*,#53427,.T.);
#77770=ORIENTED_EDGE('',*,*,#53437,.T.);
#77771=ORIENTED_EDGE('',*,*,#53438,.T.);
#77772=ORIENTED_EDGE('',*,*,#53439,.T.);
#77773=ORIENTED_EDGE('',*,*,#53440,.T.);
#77774=ORIENTED_EDGE('',*,*,#53441,.T.);
#77775=ORIENTED_EDGE('',*,*,#53442,.T.);
#77776=ORIENTED_EDGE('',*,*,#53443,.T.);
#77777=ORIENTED_EDGE('',*,*,#53444,.F.);
#77778=ORIENTED_EDGE('',*,*,#53445,.T.);
#77779=ORIENTED_EDGE('',*,*,#53446,.T.);
#77780=ORIENTED_EDGE('',*,*,#53444,.T.);
#77781=ORIENTED_EDGE('',*,*,#53447,.T.);
#77782=ORIENTED_EDGE('',*,*,#53437,.F.);
#77783=ORIENTED_EDGE('',*,*,#53448,.T.);
#77784=ORIENTED_EDGE('',*,*,#53449,.F.);
#77785=ORIENTED_EDGE('',*,*,#53445,.F.);
#77786=ORIENTED_EDGE('',*,*,#53450,.F.);
#77787=ORIENTED_EDGE('',*,*,#53451,.F.);
#77788=ORIENTED_EDGE('',*,*,#53450,.T.);
#77789=ORIENTED_EDGE('',*,*,#53448,.F.);
#77790=ORIENTED_EDGE('',*,*,#53452,.F.);
#77791=ORIENTED_EDGE('',*,*,#53452,.T.);
#77792=ORIENTED_EDGE('',*,*,#53441,.F.);
#77793=ORIENTED_EDGE('',*,*,#53453,.F.);
#77794=ORIENTED_EDGE('',*,*,#53454,.F.);
#77795=ORIENTED_EDGE('',*,*,#53455,.T.);
#77796=ORIENTED_EDGE('',*,*,#53456,.F.);
#77797=ORIENTED_EDGE('',*,*,#53457,.F.);
#77798=ORIENTED_EDGE('',*,*,#50174,.F.);
#77799=ORIENTED_EDGE('',*,*,#53458,.T.);
#77800=ORIENTED_EDGE('',*,*,#53449,.T.);
#77801=ORIENTED_EDGE('',*,*,#53455,.F.);
#77802=ORIENTED_EDGE('',*,*,#50173,.T.);
#77803=ORIENTED_EDGE('',*,*,#53459,.F.);
#77804=ORIENTED_EDGE('',*,*,#53446,.F.);
#77805=ORIENTED_EDGE('',*,*,#53458,.F.);
#77806=ORIENTED_EDGE('',*,*,#50172,.F.);
#77807=ORIENTED_EDGE('',*,*,#53459,.T.);
#77808=ORIENTED_EDGE('',*,*,#50680,.F.);
#77809=ORIENTED_EDGE('',*,*,#53460,.F.);
#77810=ORIENTED_EDGE('',*,*,#53442,.F.);
#77811=ORIENTED_EDGE('',*,*,#53460,.T.);
#77812=ORIENTED_EDGE('',*,*,#49798,.F.);
#77813=ORIENTED_EDGE('',*,*,#53461,.F.);
#77814=ORIENTED_EDGE('',*,*,#53443,.F.);
#77815=ORIENTED_EDGE('',*,*,#53461,.T.);
#77816=ORIENTED_EDGE('',*,*,#49797,.F.);
#77817=ORIENTED_EDGE('',*,*,#53462,.F.);
#77818=ORIENTED_EDGE('',*,*,#53447,.F.);
#77819=ORIENTED_EDGE('',*,*,#53462,.T.);
#77820=ORIENTED_EDGE('',*,*,#49796,.F.);
#77821=ORIENTED_EDGE('',*,*,#53463,.F.);
#77822=ORIENTED_EDGE('',*,*,#53438,.F.);
#77823=ORIENTED_EDGE('',*,*,#53464,.T.);
#77824=ORIENTED_EDGE('',*,*,#53439,.F.);
#77825=ORIENTED_EDGE('',*,*,#53463,.T.);
#77826=ORIENTED_EDGE('',*,*,#50681,.F.);
#77827=ORIENTED_EDGE('',*,*,#53465,.T.);
#77828=ORIENTED_EDGE('',*,*,#53440,.F.);
#77829=ORIENTED_EDGE('',*,*,#53464,.F.);
#77830=ORIENTED_EDGE('',*,*,#50176,.F.);
#77831=ORIENTED_EDGE('',*,*,#53457,.T.);
#77832=ORIENTED_EDGE('',*,*,#53453,.T.);
#77833=ORIENTED_EDGE('',*,*,#53465,.F.);
#77834=ORIENTED_EDGE('',*,*,#50175,.T.);
#77835=ORIENTED_EDGE('',*,*,#53451,.T.);
#77836=ORIENTED_EDGE('',*,*,#53454,.T.);
#77837=ORIENTED_EDGE('',*,*,#53456,.T.);
#77838=ORIENTED_EDGE('',*,*,#53466,.T.);
#77839=ORIENTED_EDGE('',*,*,#53467,.T.);
#77840=ORIENTED_EDGE('',*,*,#53468,.T.);
#77841=ORIENTED_EDGE('',*,*,#53469,.T.);
#77842=ORIENTED_EDGE('',*,*,#53470,.T.);
#77843=ORIENTED_EDGE('',*,*,#53471,.T.);
#77844=ORIENTED_EDGE('',*,*,#53472,.T.);
#77845=ORIENTED_EDGE('',*,*,#53473,.F.);
#77846=ORIENTED_EDGE('',*,*,#53474,.T.);
#77847=ORIENTED_EDGE('',*,*,#53475,.T.);
#77848=ORIENTED_EDGE('',*,*,#53473,.T.);
#77849=ORIENTED_EDGE('',*,*,#53476,.T.);
#77850=ORIENTED_EDGE('',*,*,#53466,.F.);
#77851=ORIENTED_EDGE('',*,*,#53477,.T.);
#77852=ORIENTED_EDGE('',*,*,#53478,.F.);
#77853=ORIENTED_EDGE('',*,*,#53474,.F.);
#77854=ORIENTED_EDGE('',*,*,#53479,.F.);
#77855=ORIENTED_EDGE('',*,*,#53480,.F.);
#77856=ORIENTED_EDGE('',*,*,#53479,.T.);
#77857=ORIENTED_EDGE('',*,*,#53477,.F.);
#77858=ORIENTED_EDGE('',*,*,#53481,.F.);
#77859=ORIENTED_EDGE('',*,*,#53481,.T.);
#77860=ORIENTED_EDGE('',*,*,#53470,.F.);
#77861=ORIENTED_EDGE('',*,*,#53482,.F.);
#77862=ORIENTED_EDGE('',*,*,#53483,.F.);
#77863=ORIENTED_EDGE('',*,*,#53484,.T.);
#77864=ORIENTED_EDGE('',*,*,#53485,.F.);
#77865=ORIENTED_EDGE('',*,*,#53486,.F.);
#77866=ORIENTED_EDGE('',*,*,#50168,.F.);
#77867=ORIENTED_EDGE('',*,*,#53487,.T.);
#77868=ORIENTED_EDGE('',*,*,#53478,.T.);
#77869=ORIENTED_EDGE('',*,*,#53484,.F.);
#77870=ORIENTED_EDGE('',*,*,#50167,.T.);
#77871=ORIENTED_EDGE('',*,*,#53488,.F.);
#77872=ORIENTED_EDGE('',*,*,#53475,.F.);
#77873=ORIENTED_EDGE('',*,*,#53487,.F.);
#77874=ORIENTED_EDGE('',*,*,#50166,.F.);
#77875=ORIENTED_EDGE('',*,*,#53488,.T.);
#77876=ORIENTED_EDGE('',*,*,#50678,.F.);
#77877=ORIENTED_EDGE('',*,*,#53489,.F.);
#77878=ORIENTED_EDGE('',*,*,#53471,.F.);
#77879=ORIENTED_EDGE('',*,*,#53489,.T.);
#77880=ORIENTED_EDGE('',*,*,#49802,.F.);
#77881=ORIENTED_EDGE('',*,*,#53490,.F.);
#77882=ORIENTED_EDGE('',*,*,#53472,.F.);
#77883=ORIENTED_EDGE('',*,*,#53490,.T.);
#77884=ORIENTED_EDGE('',*,*,#49801,.F.);
#77885=ORIENTED_EDGE('',*,*,#53491,.F.);
#77886=ORIENTED_EDGE('',*,*,#53476,.F.);
#77887=ORIENTED_EDGE('',*,*,#53491,.T.);
#77888=ORIENTED_EDGE('',*,*,#49800,.F.);
#77889=ORIENTED_EDGE('',*,*,#53492,.F.);
#77890=ORIENTED_EDGE('',*,*,#53467,.F.);
#77891=ORIENTED_EDGE('',*,*,#53493,.T.);
#77892=ORIENTED_EDGE('',*,*,#53468,.F.);
#77893=ORIENTED_EDGE('',*,*,#53492,.T.);
#77894=ORIENTED_EDGE('',*,*,#50679,.F.);
#77895=ORIENTED_EDGE('',*,*,#53494,.T.);
#77896=ORIENTED_EDGE('',*,*,#53469,.F.);
#77897=ORIENTED_EDGE('',*,*,#53493,.F.);
#77898=ORIENTED_EDGE('',*,*,#50170,.F.);
#77899=ORIENTED_EDGE('',*,*,#53486,.T.);
#77900=ORIENTED_EDGE('',*,*,#53482,.T.);
#77901=ORIENTED_EDGE('',*,*,#53494,.F.);
#77902=ORIENTED_EDGE('',*,*,#50169,.T.);
#77903=ORIENTED_EDGE('',*,*,#53480,.T.);
#77904=ORIENTED_EDGE('',*,*,#53483,.T.);
#77905=ORIENTED_EDGE('',*,*,#53485,.T.);
#77906=ORIENTED_EDGE('',*,*,#53495,.T.);
#77907=ORIENTED_EDGE('',*,*,#53496,.T.);
#77908=ORIENTED_EDGE('',*,*,#53497,.T.);
#77909=ORIENTED_EDGE('',*,*,#53498,.T.);
#77910=ORIENTED_EDGE('',*,*,#53499,.T.);
#77911=ORIENTED_EDGE('',*,*,#53500,.T.);
#77912=ORIENTED_EDGE('',*,*,#53501,.T.);
#77913=ORIENTED_EDGE('',*,*,#53502,.F.);
#77914=ORIENTED_EDGE('',*,*,#53503,.T.);
#77915=ORIENTED_EDGE('',*,*,#53504,.T.);
#77916=ORIENTED_EDGE('',*,*,#53502,.T.);
#77917=ORIENTED_EDGE('',*,*,#53505,.T.);
#77918=ORIENTED_EDGE('',*,*,#53495,.F.);
#77919=ORIENTED_EDGE('',*,*,#53506,.T.);
#77920=ORIENTED_EDGE('',*,*,#53507,.F.);
#77921=ORIENTED_EDGE('',*,*,#53503,.F.);
#77922=ORIENTED_EDGE('',*,*,#53508,.F.);
#77923=ORIENTED_EDGE('',*,*,#53509,.F.);
#77924=ORIENTED_EDGE('',*,*,#53508,.T.);
#77925=ORIENTED_EDGE('',*,*,#53506,.F.);
#77926=ORIENTED_EDGE('',*,*,#53510,.F.);
#77927=ORIENTED_EDGE('',*,*,#53510,.T.);
#77928=ORIENTED_EDGE('',*,*,#53499,.F.);
#77929=ORIENTED_EDGE('',*,*,#53511,.F.);
#77930=ORIENTED_EDGE('',*,*,#53512,.F.);
#77931=ORIENTED_EDGE('',*,*,#53513,.T.);
#77932=ORIENTED_EDGE('',*,*,#53514,.F.);
#77933=ORIENTED_EDGE('',*,*,#53515,.F.);
#77934=ORIENTED_EDGE('',*,*,#50162,.F.);
#77935=ORIENTED_EDGE('',*,*,#53516,.T.);
#77936=ORIENTED_EDGE('',*,*,#53507,.T.);
#77937=ORIENTED_EDGE('',*,*,#53513,.F.);
#77938=ORIENTED_EDGE('',*,*,#50161,.T.);
#77939=ORIENTED_EDGE('',*,*,#53517,.F.);
#77940=ORIENTED_EDGE('',*,*,#53504,.F.);
#77941=ORIENTED_EDGE('',*,*,#53516,.F.);
#77942=ORIENTED_EDGE('',*,*,#50160,.F.);
#77943=ORIENTED_EDGE('',*,*,#53517,.T.);
#77944=ORIENTED_EDGE('',*,*,#50676,.F.);
#77945=ORIENTED_EDGE('',*,*,#53518,.F.);
#77946=ORIENTED_EDGE('',*,*,#53500,.F.);
#77947=ORIENTED_EDGE('',*,*,#53518,.T.);
#77948=ORIENTED_EDGE('',*,*,#49806,.F.);
#77949=ORIENTED_EDGE('',*,*,#53519,.F.);
#77950=ORIENTED_EDGE('',*,*,#53501,.F.);
#77951=ORIENTED_EDGE('',*,*,#53519,.T.);
#77952=ORIENTED_EDGE('',*,*,#49805,.F.);
#77953=ORIENTED_EDGE('',*,*,#53520,.F.);
#77954=ORIENTED_EDGE('',*,*,#53505,.F.);
#77955=ORIENTED_EDGE('',*,*,#53520,.T.);
#77956=ORIENTED_EDGE('',*,*,#49804,.F.);
#77957=ORIENTED_EDGE('',*,*,#53521,.F.);
#77958=ORIENTED_EDGE('',*,*,#53496,.F.);
#77959=ORIENTED_EDGE('',*,*,#53522,.T.);
#77960=ORIENTED_EDGE('',*,*,#53497,.F.);
#77961=ORIENTED_EDGE('',*,*,#53521,.T.);
#77962=ORIENTED_EDGE('',*,*,#50677,.F.);
#77963=ORIENTED_EDGE('',*,*,#53523,.T.);
#77964=ORIENTED_EDGE('',*,*,#53498,.F.);
#77965=ORIENTED_EDGE('',*,*,#53522,.F.);
#77966=ORIENTED_EDGE('',*,*,#50164,.F.);
#77967=ORIENTED_EDGE('',*,*,#53515,.T.);
#77968=ORIENTED_EDGE('',*,*,#53511,.T.);
#77969=ORIENTED_EDGE('',*,*,#53523,.F.);
#77970=ORIENTED_EDGE('',*,*,#50163,.T.);
#77971=ORIENTED_EDGE('',*,*,#53509,.T.);
#77972=ORIENTED_EDGE('',*,*,#53512,.T.);
#77973=ORIENTED_EDGE('',*,*,#53514,.T.);
#77974=ORIENTED_EDGE('',*,*,#53524,.T.);
#77975=ORIENTED_EDGE('',*,*,#53525,.T.);
#77976=ORIENTED_EDGE('',*,*,#53526,.T.);
#77977=ORIENTED_EDGE('',*,*,#53527,.T.);
#77978=ORIENTED_EDGE('',*,*,#53528,.T.);
#77979=ORIENTED_EDGE('',*,*,#53529,.T.);
#77980=ORIENTED_EDGE('',*,*,#53530,.T.);
#77981=ORIENTED_EDGE('',*,*,#53531,.F.);
#77982=ORIENTED_EDGE('',*,*,#53532,.T.);
#77983=ORIENTED_EDGE('',*,*,#53533,.T.);
#77984=ORIENTED_EDGE('',*,*,#53531,.T.);
#77985=ORIENTED_EDGE('',*,*,#53534,.T.);
#77986=ORIENTED_EDGE('',*,*,#53524,.F.);
#77987=ORIENTED_EDGE('',*,*,#53535,.T.);
#77988=ORIENTED_EDGE('',*,*,#53536,.F.);
#77989=ORIENTED_EDGE('',*,*,#53532,.F.);
#77990=ORIENTED_EDGE('',*,*,#53537,.F.);
#77991=ORIENTED_EDGE('',*,*,#53538,.F.);
#77992=ORIENTED_EDGE('',*,*,#53537,.T.);
#77993=ORIENTED_EDGE('',*,*,#53535,.F.);
#77994=ORIENTED_EDGE('',*,*,#53539,.F.);
#77995=ORIENTED_EDGE('',*,*,#53539,.T.);
#77996=ORIENTED_EDGE('',*,*,#53528,.F.);
#77997=ORIENTED_EDGE('',*,*,#53540,.F.);
#77998=ORIENTED_EDGE('',*,*,#53541,.F.);
#77999=ORIENTED_EDGE('',*,*,#53542,.T.);
#78000=ORIENTED_EDGE('',*,*,#53543,.F.);
#78001=ORIENTED_EDGE('',*,*,#53544,.F.);
#78002=ORIENTED_EDGE('',*,*,#50156,.F.);
#78003=ORIENTED_EDGE('',*,*,#53545,.T.);
#78004=ORIENTED_EDGE('',*,*,#53536,.T.);
#78005=ORIENTED_EDGE('',*,*,#53542,.F.);
#78006=ORIENTED_EDGE('',*,*,#50155,.T.);
#78007=ORIENTED_EDGE('',*,*,#53546,.F.);
#78008=ORIENTED_EDGE('',*,*,#53533,.F.);
#78009=ORIENTED_EDGE('',*,*,#53545,.F.);
#78010=ORIENTED_EDGE('',*,*,#50154,.F.);
#78011=ORIENTED_EDGE('',*,*,#53546,.T.);
#78012=ORIENTED_EDGE('',*,*,#50674,.F.);
#78013=ORIENTED_EDGE('',*,*,#53547,.F.);
#78014=ORIENTED_EDGE('',*,*,#53529,.F.);
#78015=ORIENTED_EDGE('',*,*,#53547,.T.);
#78016=ORIENTED_EDGE('',*,*,#49810,.F.);
#78017=ORIENTED_EDGE('',*,*,#53548,.F.);
#78018=ORIENTED_EDGE('',*,*,#53530,.F.);
#78019=ORIENTED_EDGE('',*,*,#53548,.T.);
#78020=ORIENTED_EDGE('',*,*,#49809,.F.);
#78021=ORIENTED_EDGE('',*,*,#53549,.F.);
#78022=ORIENTED_EDGE('',*,*,#53534,.F.);
#78023=ORIENTED_EDGE('',*,*,#53549,.T.);
#78024=ORIENTED_EDGE('',*,*,#49808,.F.);
#78025=ORIENTED_EDGE('',*,*,#53550,.F.);
#78026=ORIENTED_EDGE('',*,*,#53525,.F.);
#78027=ORIENTED_EDGE('',*,*,#53551,.T.);
#78028=ORIENTED_EDGE('',*,*,#53526,.F.);
#78029=ORIENTED_EDGE('',*,*,#53550,.T.);
#78030=ORIENTED_EDGE('',*,*,#50675,.F.);
#78031=ORIENTED_EDGE('',*,*,#53552,.T.);
#78032=ORIENTED_EDGE('',*,*,#53527,.F.);
#78033=ORIENTED_EDGE('',*,*,#53551,.F.);
#78034=ORIENTED_EDGE('',*,*,#50158,.F.);
#78035=ORIENTED_EDGE('',*,*,#53544,.T.);
#78036=ORIENTED_EDGE('',*,*,#53540,.T.);
#78037=ORIENTED_EDGE('',*,*,#53552,.F.);
#78038=ORIENTED_EDGE('',*,*,#50157,.T.);
#78039=ORIENTED_EDGE('',*,*,#53538,.T.);
#78040=ORIENTED_EDGE('',*,*,#53541,.T.);
#78041=ORIENTED_EDGE('',*,*,#53543,.T.);
#78042=ORIENTED_EDGE('',*,*,#53553,.T.);
#78043=ORIENTED_EDGE('',*,*,#53554,.T.);
#78044=ORIENTED_EDGE('',*,*,#53555,.T.);
#78045=ORIENTED_EDGE('',*,*,#53556,.T.);
#78046=ORIENTED_EDGE('',*,*,#53557,.T.);
#78047=ORIENTED_EDGE('',*,*,#53558,.T.);
#78048=ORIENTED_EDGE('',*,*,#53559,.T.);
#78049=ORIENTED_EDGE('',*,*,#53560,.F.);
#78050=ORIENTED_EDGE('',*,*,#53561,.T.);
#78051=ORIENTED_EDGE('',*,*,#53562,.T.);
#78052=ORIENTED_EDGE('',*,*,#53560,.T.);
#78053=ORIENTED_EDGE('',*,*,#53563,.T.);
#78054=ORIENTED_EDGE('',*,*,#53553,.F.);
#78055=ORIENTED_EDGE('',*,*,#53564,.T.);
#78056=ORIENTED_EDGE('',*,*,#53565,.F.);
#78057=ORIENTED_EDGE('',*,*,#53561,.F.);
#78058=ORIENTED_EDGE('',*,*,#53566,.F.);
#78059=ORIENTED_EDGE('',*,*,#53567,.F.);
#78060=ORIENTED_EDGE('',*,*,#53566,.T.);
#78061=ORIENTED_EDGE('',*,*,#53564,.F.);
#78062=ORIENTED_EDGE('',*,*,#53568,.F.);
#78063=ORIENTED_EDGE('',*,*,#53568,.T.);
#78064=ORIENTED_EDGE('',*,*,#53557,.F.);
#78065=ORIENTED_EDGE('',*,*,#53569,.F.);
#78066=ORIENTED_EDGE('',*,*,#53570,.F.);
#78067=ORIENTED_EDGE('',*,*,#53571,.T.);
#78068=ORIENTED_EDGE('',*,*,#53572,.F.);
#78069=ORIENTED_EDGE('',*,*,#53573,.F.);
#78070=ORIENTED_EDGE('',*,*,#50150,.F.);
#78071=ORIENTED_EDGE('',*,*,#53574,.T.);
#78072=ORIENTED_EDGE('',*,*,#53565,.T.);
#78073=ORIENTED_EDGE('',*,*,#53571,.F.);
#78074=ORIENTED_EDGE('',*,*,#50149,.T.);
#78075=ORIENTED_EDGE('',*,*,#53575,.F.);
#78076=ORIENTED_EDGE('',*,*,#53562,.F.);
#78077=ORIENTED_EDGE('',*,*,#53574,.F.);
#78078=ORIENTED_EDGE('',*,*,#50148,.F.);
#78079=ORIENTED_EDGE('',*,*,#53575,.T.);
#78080=ORIENTED_EDGE('',*,*,#50672,.F.);
#78081=ORIENTED_EDGE('',*,*,#53576,.F.);
#78082=ORIENTED_EDGE('',*,*,#53558,.F.);
#78083=ORIENTED_EDGE('',*,*,#53576,.T.);
#78084=ORIENTED_EDGE('',*,*,#49814,.F.);
#78085=ORIENTED_EDGE('',*,*,#53577,.F.);
#78086=ORIENTED_EDGE('',*,*,#53559,.F.);
#78087=ORIENTED_EDGE('',*,*,#53577,.T.);
#78088=ORIENTED_EDGE('',*,*,#49813,.F.);
#78089=ORIENTED_EDGE('',*,*,#53578,.F.);
#78090=ORIENTED_EDGE('',*,*,#53563,.F.);
#78091=ORIENTED_EDGE('',*,*,#53578,.T.);
#78092=ORIENTED_EDGE('',*,*,#49812,.F.);
#78093=ORIENTED_EDGE('',*,*,#53579,.F.);
#78094=ORIENTED_EDGE('',*,*,#53554,.F.);
#78095=ORIENTED_EDGE('',*,*,#53580,.T.);
#78096=ORIENTED_EDGE('',*,*,#53555,.F.);
#78097=ORIENTED_EDGE('',*,*,#53579,.T.);
#78098=ORIENTED_EDGE('',*,*,#50673,.F.);
#78099=ORIENTED_EDGE('',*,*,#53581,.T.);
#78100=ORIENTED_EDGE('',*,*,#53556,.F.);
#78101=ORIENTED_EDGE('',*,*,#53580,.F.);
#78102=ORIENTED_EDGE('',*,*,#50152,.F.);
#78103=ORIENTED_EDGE('',*,*,#53573,.T.);
#78104=ORIENTED_EDGE('',*,*,#53569,.T.);
#78105=ORIENTED_EDGE('',*,*,#53581,.F.);
#78106=ORIENTED_EDGE('',*,*,#50151,.T.);
#78107=ORIENTED_EDGE('',*,*,#53567,.T.);
#78108=ORIENTED_EDGE('',*,*,#53570,.T.);
#78109=ORIENTED_EDGE('',*,*,#53572,.T.);
#78110=ORIENTED_EDGE('',*,*,#53582,.T.);
#78111=ORIENTED_EDGE('',*,*,#53583,.T.);
#78112=ORIENTED_EDGE('',*,*,#53584,.T.);
#78113=ORIENTED_EDGE('',*,*,#53585,.T.);
#78114=ORIENTED_EDGE('',*,*,#53586,.T.);
#78115=ORIENTED_EDGE('',*,*,#53587,.T.);
#78116=ORIENTED_EDGE('',*,*,#53588,.T.);
#78117=ORIENTED_EDGE('',*,*,#53589,.F.);
#78118=ORIENTED_EDGE('',*,*,#53590,.T.);
#78119=ORIENTED_EDGE('',*,*,#53591,.T.);
#78120=ORIENTED_EDGE('',*,*,#53589,.T.);
#78121=ORIENTED_EDGE('',*,*,#53592,.T.);
#78122=ORIENTED_EDGE('',*,*,#53582,.F.);
#78123=ORIENTED_EDGE('',*,*,#53593,.T.);
#78124=ORIENTED_EDGE('',*,*,#53594,.F.);
#78125=ORIENTED_EDGE('',*,*,#53590,.F.);
#78126=ORIENTED_EDGE('',*,*,#53595,.F.);
#78127=ORIENTED_EDGE('',*,*,#53596,.F.);
#78128=ORIENTED_EDGE('',*,*,#53595,.T.);
#78129=ORIENTED_EDGE('',*,*,#53593,.F.);
#78130=ORIENTED_EDGE('',*,*,#53597,.F.);
#78131=ORIENTED_EDGE('',*,*,#53597,.T.);
#78132=ORIENTED_EDGE('',*,*,#53586,.F.);
#78133=ORIENTED_EDGE('',*,*,#53598,.F.);
#78134=ORIENTED_EDGE('',*,*,#53599,.F.);
#78135=ORIENTED_EDGE('',*,*,#53600,.T.);
#78136=ORIENTED_EDGE('',*,*,#53601,.F.);
#78137=ORIENTED_EDGE('',*,*,#53602,.F.);
#78138=ORIENTED_EDGE('',*,*,#50144,.F.);
#78139=ORIENTED_EDGE('',*,*,#53603,.T.);
#78140=ORIENTED_EDGE('',*,*,#53594,.T.);
#78141=ORIENTED_EDGE('',*,*,#53600,.F.);
#78142=ORIENTED_EDGE('',*,*,#50143,.T.);
#78143=ORIENTED_EDGE('',*,*,#53604,.F.);
#78144=ORIENTED_EDGE('',*,*,#53591,.F.);
#78145=ORIENTED_EDGE('',*,*,#53603,.F.);
#78146=ORIENTED_EDGE('',*,*,#50142,.F.);
#78147=ORIENTED_EDGE('',*,*,#53604,.T.);
#78148=ORIENTED_EDGE('',*,*,#50670,.F.);
#78149=ORIENTED_EDGE('',*,*,#53605,.F.);
#78150=ORIENTED_EDGE('',*,*,#53587,.F.);
#78151=ORIENTED_EDGE('',*,*,#53605,.T.);
#78152=ORIENTED_EDGE('',*,*,#49818,.F.);
#78153=ORIENTED_EDGE('',*,*,#53606,.F.);
#78154=ORIENTED_EDGE('',*,*,#53588,.F.);
#78155=ORIENTED_EDGE('',*,*,#53606,.T.);
#78156=ORIENTED_EDGE('',*,*,#49817,.F.);
#78157=ORIENTED_EDGE('',*,*,#53607,.F.);
#78158=ORIENTED_EDGE('',*,*,#53592,.F.);
#78159=ORIENTED_EDGE('',*,*,#53607,.T.);
#78160=ORIENTED_EDGE('',*,*,#49816,.F.);
#78161=ORIENTED_EDGE('',*,*,#53608,.F.);
#78162=ORIENTED_EDGE('',*,*,#53583,.F.);
#78163=ORIENTED_EDGE('',*,*,#53609,.T.);
#78164=ORIENTED_EDGE('',*,*,#53584,.F.);
#78165=ORIENTED_EDGE('',*,*,#53608,.T.);
#78166=ORIENTED_EDGE('',*,*,#50671,.F.);
#78167=ORIENTED_EDGE('',*,*,#53610,.T.);
#78168=ORIENTED_EDGE('',*,*,#53585,.F.);
#78169=ORIENTED_EDGE('',*,*,#53609,.F.);
#78170=ORIENTED_EDGE('',*,*,#50146,.F.);
#78171=ORIENTED_EDGE('',*,*,#53602,.T.);
#78172=ORIENTED_EDGE('',*,*,#53598,.T.);
#78173=ORIENTED_EDGE('',*,*,#53610,.F.);
#78174=ORIENTED_EDGE('',*,*,#50145,.T.);
#78175=ORIENTED_EDGE('',*,*,#53596,.T.);
#78176=ORIENTED_EDGE('',*,*,#53599,.T.);
#78177=ORIENTED_EDGE('',*,*,#53601,.T.);
#78178=ORIENTED_EDGE('',*,*,#53611,.T.);
#78179=ORIENTED_EDGE('',*,*,#53612,.T.);
#78180=ORIENTED_EDGE('',*,*,#53613,.T.);
#78181=ORIENTED_EDGE('',*,*,#53614,.T.);
#78182=ORIENTED_EDGE('',*,*,#53615,.T.);
#78183=ORIENTED_EDGE('',*,*,#53616,.T.);
#78184=ORIENTED_EDGE('',*,*,#53617,.T.);
#78185=ORIENTED_EDGE('',*,*,#53618,.F.);
#78186=ORIENTED_EDGE('',*,*,#53619,.T.);
#78187=ORIENTED_EDGE('',*,*,#53620,.T.);
#78188=ORIENTED_EDGE('',*,*,#53618,.T.);
#78189=ORIENTED_EDGE('',*,*,#53621,.T.);
#78190=ORIENTED_EDGE('',*,*,#53611,.F.);
#78191=ORIENTED_EDGE('',*,*,#53622,.T.);
#78192=ORIENTED_EDGE('',*,*,#53623,.F.);
#78193=ORIENTED_EDGE('',*,*,#53619,.F.);
#78194=ORIENTED_EDGE('',*,*,#53624,.F.);
#78195=ORIENTED_EDGE('',*,*,#53625,.F.);
#78196=ORIENTED_EDGE('',*,*,#53624,.T.);
#78197=ORIENTED_EDGE('',*,*,#53622,.F.);
#78198=ORIENTED_EDGE('',*,*,#53626,.F.);
#78199=ORIENTED_EDGE('',*,*,#53626,.T.);
#78200=ORIENTED_EDGE('',*,*,#53615,.F.);
#78201=ORIENTED_EDGE('',*,*,#53627,.F.);
#78202=ORIENTED_EDGE('',*,*,#53628,.F.);
#78203=ORIENTED_EDGE('',*,*,#53629,.T.);
#78204=ORIENTED_EDGE('',*,*,#53630,.F.);
#78205=ORIENTED_EDGE('',*,*,#53631,.F.);
#78206=ORIENTED_EDGE('',*,*,#50138,.F.);
#78207=ORIENTED_EDGE('',*,*,#53632,.T.);
#78208=ORIENTED_EDGE('',*,*,#53623,.T.);
#78209=ORIENTED_EDGE('',*,*,#53629,.F.);
#78210=ORIENTED_EDGE('',*,*,#50137,.T.);
#78211=ORIENTED_EDGE('',*,*,#53633,.F.);
#78212=ORIENTED_EDGE('',*,*,#53620,.F.);
#78213=ORIENTED_EDGE('',*,*,#53632,.F.);
#78214=ORIENTED_EDGE('',*,*,#50136,.F.);
#78215=ORIENTED_EDGE('',*,*,#53633,.T.);
#78216=ORIENTED_EDGE('',*,*,#50668,.F.);
#78217=ORIENTED_EDGE('',*,*,#53634,.F.);
#78218=ORIENTED_EDGE('',*,*,#53616,.F.);
#78219=ORIENTED_EDGE('',*,*,#53634,.T.);
#78220=ORIENTED_EDGE('',*,*,#49822,.F.);
#78221=ORIENTED_EDGE('',*,*,#53635,.F.);
#78222=ORIENTED_EDGE('',*,*,#53617,.F.);
#78223=ORIENTED_EDGE('',*,*,#53635,.T.);
#78224=ORIENTED_EDGE('',*,*,#49821,.F.);
#78225=ORIENTED_EDGE('',*,*,#53636,.F.);
#78226=ORIENTED_EDGE('',*,*,#53621,.F.);
#78227=ORIENTED_EDGE('',*,*,#53636,.T.);
#78228=ORIENTED_EDGE('',*,*,#49820,.F.);
#78229=ORIENTED_EDGE('',*,*,#53637,.F.);
#78230=ORIENTED_EDGE('',*,*,#53612,.F.);
#78231=ORIENTED_EDGE('',*,*,#53638,.T.);
#78232=ORIENTED_EDGE('',*,*,#53613,.F.);
#78233=ORIENTED_EDGE('',*,*,#53637,.T.);
#78234=ORIENTED_EDGE('',*,*,#50669,.F.);
#78235=ORIENTED_EDGE('',*,*,#53639,.T.);
#78236=ORIENTED_EDGE('',*,*,#53614,.F.);
#78237=ORIENTED_EDGE('',*,*,#53638,.F.);
#78238=ORIENTED_EDGE('',*,*,#50140,.F.);
#78239=ORIENTED_EDGE('',*,*,#53631,.T.);
#78240=ORIENTED_EDGE('',*,*,#53627,.T.);
#78241=ORIENTED_EDGE('',*,*,#53639,.F.);
#78242=ORIENTED_EDGE('',*,*,#50139,.T.);
#78243=ORIENTED_EDGE('',*,*,#53625,.T.);
#78244=ORIENTED_EDGE('',*,*,#53628,.T.);
#78245=ORIENTED_EDGE('',*,*,#53630,.T.);
#78246=ORIENTED_EDGE('',*,*,#53640,.T.);
#78247=ORIENTED_EDGE('',*,*,#53641,.T.);
#78248=ORIENTED_EDGE('',*,*,#53642,.T.);
#78249=ORIENTED_EDGE('',*,*,#53643,.T.);
#78250=ORIENTED_EDGE('',*,*,#53644,.T.);
#78251=ORIENTED_EDGE('',*,*,#53645,.T.);
#78252=ORIENTED_EDGE('',*,*,#53646,.T.);
#78253=ORIENTED_EDGE('',*,*,#53647,.F.);
#78254=ORIENTED_EDGE('',*,*,#53648,.T.);
#78255=ORIENTED_EDGE('',*,*,#53649,.T.);
#78256=ORIENTED_EDGE('',*,*,#53647,.T.);
#78257=ORIENTED_EDGE('',*,*,#53650,.T.);
#78258=ORIENTED_EDGE('',*,*,#53640,.F.);
#78259=ORIENTED_EDGE('',*,*,#53651,.T.);
#78260=ORIENTED_EDGE('',*,*,#53652,.F.);
#78261=ORIENTED_EDGE('',*,*,#53648,.F.);
#78262=ORIENTED_EDGE('',*,*,#53653,.F.);
#78263=ORIENTED_EDGE('',*,*,#53654,.F.);
#78264=ORIENTED_EDGE('',*,*,#53653,.T.);
#78265=ORIENTED_EDGE('',*,*,#53651,.F.);
#78266=ORIENTED_EDGE('',*,*,#53655,.F.);
#78267=ORIENTED_EDGE('',*,*,#53655,.T.);
#78268=ORIENTED_EDGE('',*,*,#53644,.F.);
#78269=ORIENTED_EDGE('',*,*,#53656,.F.);
#78270=ORIENTED_EDGE('',*,*,#53657,.F.);
#78271=ORIENTED_EDGE('',*,*,#53658,.T.);
#78272=ORIENTED_EDGE('',*,*,#53659,.F.);
#78273=ORIENTED_EDGE('',*,*,#53660,.F.);
#78274=ORIENTED_EDGE('',*,*,#50132,.F.);
#78275=ORIENTED_EDGE('',*,*,#53661,.T.);
#78276=ORIENTED_EDGE('',*,*,#53652,.T.);
#78277=ORIENTED_EDGE('',*,*,#53658,.F.);
#78278=ORIENTED_EDGE('',*,*,#50131,.T.);
#78279=ORIENTED_EDGE('',*,*,#53662,.F.);
#78280=ORIENTED_EDGE('',*,*,#53649,.F.);
#78281=ORIENTED_EDGE('',*,*,#53661,.F.);
#78282=ORIENTED_EDGE('',*,*,#50130,.F.);
#78283=ORIENTED_EDGE('',*,*,#53662,.T.);
#78284=ORIENTED_EDGE('',*,*,#50666,.F.);
#78285=ORIENTED_EDGE('',*,*,#53663,.F.);
#78286=ORIENTED_EDGE('',*,*,#53645,.F.);
#78287=ORIENTED_EDGE('',*,*,#53663,.T.);
#78288=ORIENTED_EDGE('',*,*,#49826,.F.);
#78289=ORIENTED_EDGE('',*,*,#53664,.F.);
#78290=ORIENTED_EDGE('',*,*,#53646,.F.);
#78291=ORIENTED_EDGE('',*,*,#53664,.T.);
#78292=ORIENTED_EDGE('',*,*,#49825,.F.);
#78293=ORIENTED_EDGE('',*,*,#53665,.F.);
#78294=ORIENTED_EDGE('',*,*,#53650,.F.);
#78295=ORIENTED_EDGE('',*,*,#53665,.T.);
#78296=ORIENTED_EDGE('',*,*,#49824,.F.);
#78297=ORIENTED_EDGE('',*,*,#53666,.F.);
#78298=ORIENTED_EDGE('',*,*,#53641,.F.);
#78299=ORIENTED_EDGE('',*,*,#53667,.T.);
#78300=ORIENTED_EDGE('',*,*,#53642,.F.);
#78301=ORIENTED_EDGE('',*,*,#53666,.T.);
#78302=ORIENTED_EDGE('',*,*,#50667,.F.);
#78303=ORIENTED_EDGE('',*,*,#53668,.T.);
#78304=ORIENTED_EDGE('',*,*,#53643,.F.);
#78305=ORIENTED_EDGE('',*,*,#53667,.F.);
#78306=ORIENTED_EDGE('',*,*,#50134,.F.);
#78307=ORIENTED_EDGE('',*,*,#53660,.T.);
#78308=ORIENTED_EDGE('',*,*,#53656,.T.);
#78309=ORIENTED_EDGE('',*,*,#53668,.F.);
#78310=ORIENTED_EDGE('',*,*,#50133,.T.);
#78311=ORIENTED_EDGE('',*,*,#53654,.T.);
#78312=ORIENTED_EDGE('',*,*,#53657,.T.);
#78313=ORIENTED_EDGE('',*,*,#53659,.T.);
#78314=ORIENTED_EDGE('',*,*,#53669,.T.);
#78315=ORIENTED_EDGE('',*,*,#53670,.T.);
#78316=ORIENTED_EDGE('',*,*,#53671,.T.);
#78317=ORIENTED_EDGE('',*,*,#53672,.T.);
#78318=ORIENTED_EDGE('',*,*,#53673,.T.);
#78319=ORIENTED_EDGE('',*,*,#53674,.T.);
#78320=ORIENTED_EDGE('',*,*,#53675,.T.);
#78321=ORIENTED_EDGE('',*,*,#53676,.F.);
#78322=ORIENTED_EDGE('',*,*,#53677,.T.);
#78323=ORIENTED_EDGE('',*,*,#53678,.T.);
#78324=ORIENTED_EDGE('',*,*,#53676,.T.);
#78325=ORIENTED_EDGE('',*,*,#53679,.T.);
#78326=ORIENTED_EDGE('',*,*,#53669,.F.);
#78327=ORIENTED_EDGE('',*,*,#53680,.T.);
#78328=ORIENTED_EDGE('',*,*,#53681,.F.);
#78329=ORIENTED_EDGE('',*,*,#53677,.F.);
#78330=ORIENTED_EDGE('',*,*,#53682,.F.);
#78331=ORIENTED_EDGE('',*,*,#53683,.F.);
#78332=ORIENTED_EDGE('',*,*,#53682,.T.);
#78333=ORIENTED_EDGE('',*,*,#53680,.F.);
#78334=ORIENTED_EDGE('',*,*,#53684,.F.);
#78335=ORIENTED_EDGE('',*,*,#53684,.T.);
#78336=ORIENTED_EDGE('',*,*,#53673,.F.);
#78337=ORIENTED_EDGE('',*,*,#53685,.F.);
#78338=ORIENTED_EDGE('',*,*,#53686,.F.);
#78339=ORIENTED_EDGE('',*,*,#53687,.T.);
#78340=ORIENTED_EDGE('',*,*,#53688,.F.);
#78341=ORIENTED_EDGE('',*,*,#53689,.F.);
#78342=ORIENTED_EDGE('',*,*,#50126,.F.);
#78343=ORIENTED_EDGE('',*,*,#53690,.T.);
#78344=ORIENTED_EDGE('',*,*,#53681,.T.);
#78345=ORIENTED_EDGE('',*,*,#53687,.F.);
#78346=ORIENTED_EDGE('',*,*,#50125,.T.);
#78347=ORIENTED_EDGE('',*,*,#53691,.F.);
#78348=ORIENTED_EDGE('',*,*,#53678,.F.);
#78349=ORIENTED_EDGE('',*,*,#53690,.F.);
#78350=ORIENTED_EDGE('',*,*,#50124,.F.);
#78351=ORIENTED_EDGE('',*,*,#53691,.T.);
#78352=ORIENTED_EDGE('',*,*,#50664,.F.);
#78353=ORIENTED_EDGE('',*,*,#53692,.F.);
#78354=ORIENTED_EDGE('',*,*,#53674,.F.);
#78355=ORIENTED_EDGE('',*,*,#53692,.T.);
#78356=ORIENTED_EDGE('',*,*,#49830,.F.);
#78357=ORIENTED_EDGE('',*,*,#53693,.F.);
#78358=ORIENTED_EDGE('',*,*,#53675,.F.);
#78359=ORIENTED_EDGE('',*,*,#53693,.T.);
#78360=ORIENTED_EDGE('',*,*,#49829,.F.);
#78361=ORIENTED_EDGE('',*,*,#53694,.F.);
#78362=ORIENTED_EDGE('',*,*,#53679,.F.);
#78363=ORIENTED_EDGE('',*,*,#53694,.T.);
#78364=ORIENTED_EDGE('',*,*,#49828,.F.);
#78365=ORIENTED_EDGE('',*,*,#53695,.F.);
#78366=ORIENTED_EDGE('',*,*,#53670,.F.);
#78367=ORIENTED_EDGE('',*,*,#53696,.T.);
#78368=ORIENTED_EDGE('',*,*,#53671,.F.);
#78369=ORIENTED_EDGE('',*,*,#53695,.T.);
#78370=ORIENTED_EDGE('',*,*,#50665,.F.);
#78371=ORIENTED_EDGE('',*,*,#53697,.T.);
#78372=ORIENTED_EDGE('',*,*,#53672,.F.);
#78373=ORIENTED_EDGE('',*,*,#53696,.F.);
#78374=ORIENTED_EDGE('',*,*,#50128,.F.);
#78375=ORIENTED_EDGE('',*,*,#53689,.T.);
#78376=ORIENTED_EDGE('',*,*,#53685,.T.);
#78377=ORIENTED_EDGE('',*,*,#53697,.F.);
#78378=ORIENTED_EDGE('',*,*,#50127,.T.);
#78379=ORIENTED_EDGE('',*,*,#53683,.T.);
#78380=ORIENTED_EDGE('',*,*,#53686,.T.);
#78381=ORIENTED_EDGE('',*,*,#53688,.T.);
#78382=ORIENTED_EDGE('',*,*,#53698,.T.);
#78383=ORIENTED_EDGE('',*,*,#53699,.T.);
#78384=ORIENTED_EDGE('',*,*,#53700,.T.);
#78385=ORIENTED_EDGE('',*,*,#53701,.T.);
#78386=ORIENTED_EDGE('',*,*,#53702,.T.);
#78387=ORIENTED_EDGE('',*,*,#53703,.T.);
#78388=ORIENTED_EDGE('',*,*,#53704,.T.);
#78389=ORIENTED_EDGE('',*,*,#53705,.F.);
#78390=ORIENTED_EDGE('',*,*,#53706,.T.);
#78391=ORIENTED_EDGE('',*,*,#53707,.T.);
#78392=ORIENTED_EDGE('',*,*,#53705,.T.);
#78393=ORIENTED_EDGE('',*,*,#53708,.T.);
#78394=ORIENTED_EDGE('',*,*,#53698,.F.);
#78395=ORIENTED_EDGE('',*,*,#53709,.T.);
#78396=ORIENTED_EDGE('',*,*,#53710,.F.);
#78397=ORIENTED_EDGE('',*,*,#53706,.F.);
#78398=ORIENTED_EDGE('',*,*,#53711,.F.);
#78399=ORIENTED_EDGE('',*,*,#53712,.F.);
#78400=ORIENTED_EDGE('',*,*,#53711,.T.);
#78401=ORIENTED_EDGE('',*,*,#53709,.F.);
#78402=ORIENTED_EDGE('',*,*,#53713,.F.);
#78403=ORIENTED_EDGE('',*,*,#53713,.T.);
#78404=ORIENTED_EDGE('',*,*,#53702,.F.);
#78405=ORIENTED_EDGE('',*,*,#53714,.F.);
#78406=ORIENTED_EDGE('',*,*,#53715,.F.);
#78407=ORIENTED_EDGE('',*,*,#53716,.T.);
#78408=ORIENTED_EDGE('',*,*,#53717,.F.);
#78409=ORIENTED_EDGE('',*,*,#53718,.F.);
#78410=ORIENTED_EDGE('',*,*,#50120,.F.);
#78411=ORIENTED_EDGE('',*,*,#53719,.T.);
#78412=ORIENTED_EDGE('',*,*,#53710,.T.);
#78413=ORIENTED_EDGE('',*,*,#53716,.F.);
#78414=ORIENTED_EDGE('',*,*,#50119,.T.);
#78415=ORIENTED_EDGE('',*,*,#53720,.F.);
#78416=ORIENTED_EDGE('',*,*,#53707,.F.);
#78417=ORIENTED_EDGE('',*,*,#53719,.F.);
#78418=ORIENTED_EDGE('',*,*,#50118,.F.);
#78419=ORIENTED_EDGE('',*,*,#53720,.T.);
#78420=ORIENTED_EDGE('',*,*,#50661,.F.);
#78421=ORIENTED_EDGE('',*,*,#53721,.F.);
#78422=ORIENTED_EDGE('',*,*,#53703,.F.);
#78423=ORIENTED_EDGE('',*,*,#53721,.T.);
#78424=ORIENTED_EDGE('',*,*,#49834,.F.);
#78425=ORIENTED_EDGE('',*,*,#53722,.F.);
#78426=ORIENTED_EDGE('',*,*,#53704,.F.);
#78427=ORIENTED_EDGE('',*,*,#53722,.T.);
#78428=ORIENTED_EDGE('',*,*,#49833,.F.);
#78429=ORIENTED_EDGE('',*,*,#53723,.F.);
#78430=ORIENTED_EDGE('',*,*,#53708,.F.);
#78431=ORIENTED_EDGE('',*,*,#53723,.T.);
#78432=ORIENTED_EDGE('',*,*,#49832,.F.);
#78433=ORIENTED_EDGE('',*,*,#53724,.F.);
#78434=ORIENTED_EDGE('',*,*,#53699,.F.);
#78435=ORIENTED_EDGE('',*,*,#53725,.T.);
#78436=ORIENTED_EDGE('',*,*,#53700,.F.);
#78437=ORIENTED_EDGE('',*,*,#53724,.T.);
#78438=ORIENTED_EDGE('',*,*,#50663,.F.);
#78439=ORIENTED_EDGE('',*,*,#53726,.T.);
#78440=ORIENTED_EDGE('',*,*,#53701,.F.);
#78441=ORIENTED_EDGE('',*,*,#53725,.F.);
#78442=ORIENTED_EDGE('',*,*,#50122,.F.);
#78443=ORIENTED_EDGE('',*,*,#53718,.T.);
#78444=ORIENTED_EDGE('',*,*,#53714,.T.);
#78445=ORIENTED_EDGE('',*,*,#53726,.F.);
#78446=ORIENTED_EDGE('',*,*,#50121,.T.);
#78447=ORIENTED_EDGE('',*,*,#53712,.T.);
#78448=ORIENTED_EDGE('',*,*,#53715,.T.);
#78449=ORIENTED_EDGE('',*,*,#53717,.T.);
#78450=ORIENTED_EDGE('',*,*,#53727,.F.);
#78451=ORIENTED_EDGE('',*,*,#53728,.F.);
#78452=ORIENTED_EDGE('',*,*,#53729,.T.);
#78453=ORIENTED_EDGE('',*,*,#53730,.F.);
#78454=ORIENTED_EDGE('',*,*,#53731,.F.);
#78455=ORIENTED_EDGE('',*,*,#53727,.T.);
#78456=ORIENTED_EDGE('',*,*,#53732,.T.);
#78457=ORIENTED_EDGE('',*,*,#53733,.F.);
#78458=ORIENTED_EDGE('',*,*,#53734,.F.);
#78459=ORIENTED_EDGE('',*,*,#53730,.T.);
#78460=ORIENTED_EDGE('',*,*,#53735,.T.);
#78461=ORIENTED_EDGE('',*,*,#53736,.F.);
#78462=ORIENTED_EDGE('',*,*,#53737,.F.);
#78463=ORIENTED_EDGE('',*,*,#53733,.T.);
#78464=ORIENTED_EDGE('',*,*,#53738,.T.);
#78465=ORIENTED_EDGE('',*,*,#53739,.F.);
#78466=ORIENTED_EDGE('',*,*,#53740,.F.);
#78467=ORIENTED_EDGE('',*,*,#53736,.T.);
#78468=ORIENTED_EDGE('',*,*,#53741,.T.);
#78469=ORIENTED_EDGE('',*,*,#53742,.F.);
#78470=ORIENTED_EDGE('',*,*,#53743,.F.);
#78471=ORIENTED_EDGE('',*,*,#53739,.T.);
#78472=ORIENTED_EDGE('',*,*,#53744,.T.);
#78473=ORIENTED_EDGE('',*,*,#53745,.F.);
#78474=ORIENTED_EDGE('',*,*,#53746,.F.);
#78475=ORIENTED_EDGE('',*,*,#53742,.T.);
#78476=ORIENTED_EDGE('',*,*,#53747,.T.);
#78477=ORIENTED_EDGE('',*,*,#53748,.F.);
#78478=ORIENTED_EDGE('',*,*,#53749,.F.);
#78479=ORIENTED_EDGE('',*,*,#53745,.T.);
#78480=ORIENTED_EDGE('',*,*,#53750,.T.);
#78481=ORIENTED_EDGE('',*,*,#53751,.F.);
#78482=ORIENTED_EDGE('',*,*,#53752,.F.);
#78483=ORIENTED_EDGE('',*,*,#53748,.T.);
#78484=ORIENTED_EDGE('',*,*,#53753,.T.);
#78485=ORIENTED_EDGE('',*,*,#53754,.F.);
#78486=ORIENTED_EDGE('',*,*,#53755,.F.);
#78487=ORIENTED_EDGE('',*,*,#53751,.T.);
#78488=ORIENTED_EDGE('',*,*,#53756,.T.);
#78489=ORIENTED_EDGE('',*,*,#53757,.F.);
#78490=ORIENTED_EDGE('',*,*,#53758,.F.);
#78491=ORIENTED_EDGE('',*,*,#53754,.T.);
#78492=ORIENTED_EDGE('',*,*,#53759,.T.);
#78493=ORIENTED_EDGE('',*,*,#53760,.F.);
#78494=ORIENTED_EDGE('',*,*,#53761,.F.);
#78495=ORIENTED_EDGE('',*,*,#53757,.T.);
#78496=ORIENTED_EDGE('',*,*,#53762,.T.);
#78497=ORIENTED_EDGE('',*,*,#53763,.F.);
#78498=ORIENTED_EDGE('',*,*,#53764,.F.);
#78499=ORIENTED_EDGE('',*,*,#53760,.T.);
#78500=ORIENTED_EDGE('',*,*,#53765,.T.);
#78501=ORIENTED_EDGE('',*,*,#53766,.F.);
#78502=ORIENTED_EDGE('',*,*,#53767,.F.);
#78503=ORIENTED_EDGE('',*,*,#53763,.T.);
#78504=ORIENTED_EDGE('',*,*,#53768,.T.);
#78505=ORIENTED_EDGE('',*,*,#53769,.F.);
#78506=ORIENTED_EDGE('',*,*,#53770,.F.);
#78507=ORIENTED_EDGE('',*,*,#53766,.T.);
#78508=ORIENTED_EDGE('',*,*,#53771,.T.);
#78509=ORIENTED_EDGE('',*,*,#53772,.F.);
#78510=ORIENTED_EDGE('',*,*,#53773,.F.);
#78511=ORIENTED_EDGE('',*,*,#53769,.T.);
#78512=ORIENTED_EDGE('',*,*,#53774,.T.);
#78513=ORIENTED_EDGE('',*,*,#53775,.F.);
#78514=ORIENTED_EDGE('',*,*,#53776,.F.);
#78515=ORIENTED_EDGE('',*,*,#53772,.T.);
#78516=ORIENTED_EDGE('',*,*,#53777,.T.);
#78517=ORIENTED_EDGE('',*,*,#53778,.F.);
#78518=ORIENTED_EDGE('',*,*,#53779,.F.);
#78519=ORIENTED_EDGE('',*,*,#53775,.T.);
#78520=ORIENTED_EDGE('',*,*,#53780,.T.);
#78521=ORIENTED_EDGE('',*,*,#53781,.F.);
#78522=ORIENTED_EDGE('',*,*,#53782,.F.);
#78523=ORIENTED_EDGE('',*,*,#53778,.T.);
#78524=ORIENTED_EDGE('',*,*,#53783,.T.);
#78525=ORIENTED_EDGE('',*,*,#53784,.F.);
#78526=ORIENTED_EDGE('',*,*,#53785,.F.);
#78527=ORIENTED_EDGE('',*,*,#53781,.T.);
#78528=ORIENTED_EDGE('',*,*,#53786,.T.);
#78529=ORIENTED_EDGE('',*,*,#53787,.F.);
#78530=ORIENTED_EDGE('',*,*,#53788,.F.);
#78531=ORIENTED_EDGE('',*,*,#53784,.T.);
#78532=ORIENTED_EDGE('',*,*,#53789,.T.);
#78533=ORIENTED_EDGE('',*,*,#53790,.F.);
#78534=ORIENTED_EDGE('',*,*,#53791,.F.);
#78535=ORIENTED_EDGE('',*,*,#53787,.T.);
#78536=ORIENTED_EDGE('',*,*,#53792,.T.);
#78537=ORIENTED_EDGE('',*,*,#53793,.F.);
#78538=ORIENTED_EDGE('',*,*,#53794,.F.);
#78539=ORIENTED_EDGE('',*,*,#53790,.T.);
#78540=ORIENTED_EDGE('',*,*,#53795,.T.);
#78541=ORIENTED_EDGE('',*,*,#53796,.F.);
#78542=ORIENTED_EDGE('',*,*,#53797,.F.);
#78543=ORIENTED_EDGE('',*,*,#53793,.T.);
#78544=ORIENTED_EDGE('',*,*,#53798,.T.);
#78545=ORIENTED_EDGE('',*,*,#53799,.F.);
#78546=ORIENTED_EDGE('',*,*,#53800,.F.);
#78547=ORIENTED_EDGE('',*,*,#53796,.T.);
#78548=ORIENTED_EDGE('',*,*,#53801,.T.);
#78549=ORIENTED_EDGE('',*,*,#53802,.F.);
#78550=ORIENTED_EDGE('',*,*,#53803,.F.);
#78551=ORIENTED_EDGE('',*,*,#53799,.T.);
#78552=ORIENTED_EDGE('',*,*,#53804,.T.);
#78553=ORIENTED_EDGE('',*,*,#53805,.F.);
#78554=ORIENTED_EDGE('',*,*,#53806,.F.);
#78555=ORIENTED_EDGE('',*,*,#53802,.T.);
#78556=ORIENTED_EDGE('',*,*,#53807,.T.);
#78557=ORIENTED_EDGE('',*,*,#53808,.F.);
#78558=ORIENTED_EDGE('',*,*,#53809,.F.);
#78559=ORIENTED_EDGE('',*,*,#53805,.T.);
#78560=ORIENTED_EDGE('',*,*,#53810,.T.);
#78561=ORIENTED_EDGE('',*,*,#53811,.F.);
#78562=ORIENTED_EDGE('',*,*,#53812,.F.);
#78563=ORIENTED_EDGE('',*,*,#53808,.T.);
#78564=ORIENTED_EDGE('',*,*,#53813,.T.);
#78565=ORIENTED_EDGE('',*,*,#53814,.F.);
#78566=ORIENTED_EDGE('',*,*,#53815,.F.);
#78567=ORIENTED_EDGE('',*,*,#53811,.T.);
#78568=ORIENTED_EDGE('',*,*,#53816,.T.);
#78569=ORIENTED_EDGE('',*,*,#53817,.F.);
#78570=ORIENTED_EDGE('',*,*,#53818,.F.);
#78571=ORIENTED_EDGE('',*,*,#53814,.T.);
#78572=ORIENTED_EDGE('',*,*,#53819,.T.);
#78573=ORIENTED_EDGE('',*,*,#53820,.F.);
#78574=ORIENTED_EDGE('',*,*,#53821,.F.);
#78575=ORIENTED_EDGE('',*,*,#53817,.T.);
#78576=ORIENTED_EDGE('',*,*,#53822,.T.);
#78577=ORIENTED_EDGE('',*,*,#53823,.F.);
#78578=ORIENTED_EDGE('',*,*,#53824,.F.);
#78579=ORIENTED_EDGE('',*,*,#53820,.T.);
#78580=ORIENTED_EDGE('',*,*,#53825,.T.);
#78581=ORIENTED_EDGE('',*,*,#53826,.F.);
#78582=ORIENTED_EDGE('',*,*,#53827,.F.);
#78583=ORIENTED_EDGE('',*,*,#53823,.T.);
#78584=ORIENTED_EDGE('',*,*,#53828,.T.);
#78585=ORIENTED_EDGE('',*,*,#53829,.F.);
#78586=ORIENTED_EDGE('',*,*,#53830,.F.);
#78587=ORIENTED_EDGE('',*,*,#53826,.T.);
#78588=ORIENTED_EDGE('',*,*,#53831,.T.);
#78589=ORIENTED_EDGE('',*,*,#53832,.F.);
#78590=ORIENTED_EDGE('',*,*,#53833,.F.);
#78591=ORIENTED_EDGE('',*,*,#53829,.T.);
#78592=ORIENTED_EDGE('',*,*,#53834,.T.);
#78593=ORIENTED_EDGE('',*,*,#53835,.F.);
#78594=ORIENTED_EDGE('',*,*,#53836,.T.);
#78595=ORIENTED_EDGE('',*,*,#53837,.T.);
#78596=ORIENTED_EDGE('',*,*,#53838,.T.);
#78597=ORIENTED_EDGE('',*,*,#53839,.F.);
#78598=ORIENTED_EDGE('',*,*,#53840,.F.);
#78599=ORIENTED_EDGE('',*,*,#53841,.T.);
#78600=ORIENTED_EDGE('',*,*,#53842,.F.);
#78601=ORIENTED_EDGE('',*,*,#53843,.F.);
#78602=ORIENTED_EDGE('',*,*,#53844,.T.);
#78603=ORIENTED_EDGE('',*,*,#53845,.F.);
#78604=ORIENTED_EDGE('',*,*,#53846,.F.);
#78605=ORIENTED_EDGE('',*,*,#53847,.F.);
#78606=ORIENTED_EDGE('',*,*,#53842,.T.);
#78607=ORIENTED_EDGE('',*,*,#53848,.F.);
#78608=ORIENTED_EDGE('',*,*,#53849,.F.);
#78609=ORIENTED_EDGE('',*,*,#53850,.F.);
#78610=ORIENTED_EDGE('',*,*,#53846,.T.);
#78611=ORIENTED_EDGE('',*,*,#53851,.F.);
#78612=ORIENTED_EDGE('',*,*,#53852,.F.);
#78613=ORIENTED_EDGE('',*,*,#53853,.F.);
#78614=ORIENTED_EDGE('',*,*,#53849,.T.);
#78615=ORIENTED_EDGE('',*,*,#53854,.F.);
#78616=ORIENTED_EDGE('',*,*,#53855,.F.);
#78617=ORIENTED_EDGE('',*,*,#53856,.F.);
#78618=ORIENTED_EDGE('',*,*,#53852,.T.);
#78619=ORIENTED_EDGE('',*,*,#53857,.F.);
#78620=ORIENTED_EDGE('',*,*,#53858,.F.);
#78621=ORIENTED_EDGE('',*,*,#53859,.F.);
#78622=ORIENTED_EDGE('',*,*,#53855,.T.);
#78623=ORIENTED_EDGE('',*,*,#53860,.F.);
#78624=ORIENTED_EDGE('',*,*,#53861,.F.);
#78625=ORIENTED_EDGE('',*,*,#53862,.F.);
#78626=ORIENTED_EDGE('',*,*,#53858,.T.);
#78627=ORIENTED_EDGE('',*,*,#53863,.F.);
#78628=ORIENTED_EDGE('',*,*,#53864,.F.);
#78629=ORIENTED_EDGE('',*,*,#53865,.F.);
#78630=ORIENTED_EDGE('',*,*,#53861,.T.);
#78631=ORIENTED_EDGE('',*,*,#53866,.F.);
#78632=ORIENTED_EDGE('',*,*,#53867,.F.);
#78633=ORIENTED_EDGE('',*,*,#53868,.F.);
#78634=ORIENTED_EDGE('',*,*,#53864,.T.);
#78635=ORIENTED_EDGE('',*,*,#53869,.F.);
#78636=ORIENTED_EDGE('',*,*,#53870,.F.);
#78637=ORIENTED_EDGE('',*,*,#53871,.F.);
#78638=ORIENTED_EDGE('',*,*,#53867,.T.);
#78639=ORIENTED_EDGE('',*,*,#53872,.F.);
#78640=ORIENTED_EDGE('',*,*,#53873,.F.);
#78641=ORIENTED_EDGE('',*,*,#53874,.F.);
#78642=ORIENTED_EDGE('',*,*,#53870,.T.);
#78643=ORIENTED_EDGE('',*,*,#53875,.F.);
#78644=ORIENTED_EDGE('',*,*,#53876,.F.);
#78645=ORIENTED_EDGE('',*,*,#53877,.F.);
#78646=ORIENTED_EDGE('',*,*,#53873,.T.);
#78647=ORIENTED_EDGE('',*,*,#53878,.F.);
#78648=ORIENTED_EDGE('',*,*,#53879,.F.);
#78649=ORIENTED_EDGE('',*,*,#53880,.F.);
#78650=ORIENTED_EDGE('',*,*,#53876,.T.);
#78651=ORIENTED_EDGE('',*,*,#53881,.F.);
#78652=ORIENTED_EDGE('',*,*,#53882,.F.);
#78653=ORIENTED_EDGE('',*,*,#53883,.F.);
#78654=ORIENTED_EDGE('',*,*,#53879,.T.);
#78655=ORIENTED_EDGE('',*,*,#53884,.F.);
#78656=ORIENTED_EDGE('',*,*,#53885,.F.);
#78657=ORIENTED_EDGE('',*,*,#53886,.F.);
#78658=ORIENTED_EDGE('',*,*,#53882,.T.);
#78659=ORIENTED_EDGE('',*,*,#53887,.F.);
#78660=ORIENTED_EDGE('',*,*,#53888,.F.);
#78661=ORIENTED_EDGE('',*,*,#53889,.F.);
#78662=ORIENTED_EDGE('',*,*,#53885,.T.);
#78663=ORIENTED_EDGE('',*,*,#53890,.F.);
#78664=ORIENTED_EDGE('',*,*,#53891,.F.);
#78665=ORIENTED_EDGE('',*,*,#53892,.F.);
#78666=ORIENTED_EDGE('',*,*,#53888,.T.);
#78667=ORIENTED_EDGE('',*,*,#53893,.F.);
#78668=ORIENTED_EDGE('',*,*,#53894,.F.);
#78669=ORIENTED_EDGE('',*,*,#53895,.F.);
#78670=ORIENTED_EDGE('',*,*,#53891,.T.);
#78671=ORIENTED_EDGE('',*,*,#53896,.F.);
#78672=ORIENTED_EDGE('',*,*,#53897,.F.);
#78673=ORIENTED_EDGE('',*,*,#53898,.F.);
#78674=ORIENTED_EDGE('',*,*,#53894,.T.);
#78675=ORIENTED_EDGE('',*,*,#53899,.F.);
#78676=ORIENTED_EDGE('',*,*,#53900,.F.);
#78677=ORIENTED_EDGE('',*,*,#53901,.F.);
#78678=ORIENTED_EDGE('',*,*,#53897,.T.);
#78679=ORIENTED_EDGE('',*,*,#53902,.F.);
#78680=ORIENTED_EDGE('',*,*,#53903,.F.);
#78681=ORIENTED_EDGE('',*,*,#53904,.F.);
#78682=ORIENTED_EDGE('',*,*,#53900,.T.);
#78683=ORIENTED_EDGE('',*,*,#53905,.F.);
#78684=ORIENTED_EDGE('',*,*,#53906,.F.);
#78685=ORIENTED_EDGE('',*,*,#53907,.F.);
#78686=ORIENTED_EDGE('',*,*,#53903,.T.);
#78687=ORIENTED_EDGE('',*,*,#53908,.F.);
#78688=ORIENTED_EDGE('',*,*,#53909,.F.);
#78689=ORIENTED_EDGE('',*,*,#53910,.F.);
#78690=ORIENTED_EDGE('',*,*,#53906,.T.);
#78691=ORIENTED_EDGE('',*,*,#53911,.F.);
#78692=ORIENTED_EDGE('',*,*,#53912,.F.);
#78693=ORIENTED_EDGE('',*,*,#53913,.F.);
#78694=ORIENTED_EDGE('',*,*,#53909,.T.);
#78695=ORIENTED_EDGE('',*,*,#53914,.F.);
#78696=ORIENTED_EDGE('',*,*,#53915,.F.);
#78697=ORIENTED_EDGE('',*,*,#53916,.F.);
#78698=ORIENTED_EDGE('',*,*,#53912,.T.);
#78699=ORIENTED_EDGE('',*,*,#53917,.F.);
#78700=ORIENTED_EDGE('',*,*,#53918,.F.);
#78701=ORIENTED_EDGE('',*,*,#53919,.F.);
#78702=ORIENTED_EDGE('',*,*,#53915,.T.);
#78703=ORIENTED_EDGE('',*,*,#53920,.F.);
#78704=ORIENTED_EDGE('',*,*,#53921,.F.);
#78705=ORIENTED_EDGE('',*,*,#53922,.F.);
#78706=ORIENTED_EDGE('',*,*,#53918,.T.);
#78707=ORIENTED_EDGE('',*,*,#53923,.F.);
#78708=ORIENTED_EDGE('',*,*,#53924,.F.);
#78709=ORIENTED_EDGE('',*,*,#53925,.F.);
#78710=ORIENTED_EDGE('',*,*,#53921,.T.);
#78711=ORIENTED_EDGE('',*,*,#53926,.F.);
#78712=ORIENTED_EDGE('',*,*,#53927,.F.);
#78713=ORIENTED_EDGE('',*,*,#53928,.F.);
#78714=ORIENTED_EDGE('',*,*,#53924,.T.);
#78715=ORIENTED_EDGE('',*,*,#53929,.F.);
#78716=ORIENTED_EDGE('',*,*,#53930,.F.);
#78717=ORIENTED_EDGE('',*,*,#53931,.F.);
#78718=ORIENTED_EDGE('',*,*,#53927,.T.);
#78719=ORIENTED_EDGE('',*,*,#53932,.F.);
#78720=ORIENTED_EDGE('',*,*,#53933,.F.);
#78721=ORIENTED_EDGE('',*,*,#53934,.F.);
#78722=ORIENTED_EDGE('',*,*,#53930,.T.);
#78723=ORIENTED_EDGE('',*,*,#53935,.F.);
#78724=ORIENTED_EDGE('',*,*,#53936,.F.);
#78725=ORIENTED_EDGE('',*,*,#53937,.F.);
#78726=ORIENTED_EDGE('',*,*,#53933,.T.);
#78727=ORIENTED_EDGE('',*,*,#53938,.F.);
#78728=ORIENTED_EDGE('',*,*,#53939,.F.);
#78729=ORIENTED_EDGE('',*,*,#53940,.F.);
#78730=ORIENTED_EDGE('',*,*,#53941,.F.);
#78731=ORIENTED_EDGE('',*,*,#53936,.T.);
#78732=ORIENTED_EDGE('',*,*,#53942,.F.);
#78733=ORIENTED_EDGE('',*,*,#53943,.F.);
#78734=ORIENTED_EDGE('',*,*,#53944,.F.);
#78735=ORIENTED_EDGE('',*,*,#53940,.T.);
#78736=ORIENTED_EDGE('',*,*,#53945,.F.);
#78737=ORIENTED_EDGE('',*,*,#53946,.T.);
#78738=ORIENTED_EDGE('',*,*,#53947,.T.);
#78739=ORIENTED_EDGE('',*,*,#53948,.F.);
#78740=ORIENTED_EDGE('',*,*,#53949,.F.);
#78741=ORIENTED_EDGE('',*,*,#53950,.T.);
#78742=ORIENTED_EDGE('',*,*,#53951,.F.);
#78743=ORIENTED_EDGE('',*,*,#53947,.F.);
#78744=ORIENTED_EDGE('',*,*,#53952,.F.);
#78745=ORIENTED_EDGE('',*,*,#53953,.F.);
#78746=ORIENTED_EDGE('',*,*,#53954,.F.);
#78747=ORIENTED_EDGE('',*,*,#53955,.T.);
#78748=ORIENTED_EDGE('',*,*,#53956,.F.);
#78749=ORIENTED_EDGE('',*,*,#53957,.F.);
#78750=ORIENTED_EDGE('',*,*,#53958,.F.);
#78751=ORIENTED_EDGE('',*,*,#53959,.T.);
#78752=ORIENTED_EDGE('',*,*,#53960,.F.);
#78753=ORIENTED_EDGE('',*,*,#53961,.F.);
#78754=ORIENTED_EDGE('',*,*,#53962,.F.);
#78755=ORIENTED_EDGE('',*,*,#53963,.T.);
#78756=ORIENTED_EDGE('',*,*,#53964,.F.);
#78757=ORIENTED_EDGE('',*,*,#53965,.F.);
#78758=ORIENTED_EDGE('',*,*,#53966,.F.);
#78759=ORIENTED_EDGE('',*,*,#53967,.T.);
#78760=ORIENTED_EDGE('',*,*,#53968,.F.);
#78761=ORIENTED_EDGE('',*,*,#53969,.F.);
#78762=ORIENTED_EDGE('',*,*,#53970,.F.);
#78763=ORIENTED_EDGE('',*,*,#53971,.T.);
#78764=ORIENTED_EDGE('',*,*,#53972,.F.);
#78765=ORIENTED_EDGE('',*,*,#53973,.F.);
#78766=ORIENTED_EDGE('',*,*,#53974,.F.);
#78767=ORIENTED_EDGE('',*,*,#53975,.T.);
#78768=ORIENTED_EDGE('',*,*,#53976,.F.);
#78769=ORIENTED_EDGE('',*,*,#53977,.F.);
#78770=ORIENTED_EDGE('',*,*,#53978,.F.);
#78771=ORIENTED_EDGE('',*,*,#53979,.T.);
#78772=ORIENTED_EDGE('',*,*,#53980,.F.);
#78773=ORIENTED_EDGE('',*,*,#53981,.F.);
#78774=ORIENTED_EDGE('',*,*,#53982,.F.);
#78775=ORIENTED_EDGE('',*,*,#53983,.T.);
#78776=ORIENTED_EDGE('',*,*,#53984,.F.);
#78777=ORIENTED_EDGE('',*,*,#53985,.F.);
#78778=ORIENTED_EDGE('',*,*,#53986,.F.);
#78779=ORIENTED_EDGE('',*,*,#53987,.T.);
#78780=ORIENTED_EDGE('',*,*,#53988,.F.);
#78781=ORIENTED_EDGE('',*,*,#53989,.F.);
#78782=ORIENTED_EDGE('',*,*,#53990,.F.);
#78783=ORIENTED_EDGE('',*,*,#53991,.T.);
#78784=ORIENTED_EDGE('',*,*,#53992,.F.);
#78785=ORIENTED_EDGE('',*,*,#53993,.F.);
#78786=ORIENTED_EDGE('',*,*,#53994,.F.);
#78787=ORIENTED_EDGE('',*,*,#53995,.T.);
#78788=ORIENTED_EDGE('',*,*,#53996,.F.);
#78789=ORIENTED_EDGE('',*,*,#53997,.F.);
#78790=ORIENTED_EDGE('',*,*,#53998,.F.);
#78791=ORIENTED_EDGE('',*,*,#53999,.T.);
#78792=ORIENTED_EDGE('',*,*,#54000,.F.);
#78793=ORIENTED_EDGE('',*,*,#54001,.F.);
#78794=ORIENTED_EDGE('',*,*,#54002,.F.);
#78795=ORIENTED_EDGE('',*,*,#54003,.T.);
#78796=ORIENTED_EDGE('',*,*,#54004,.F.);
#78797=ORIENTED_EDGE('',*,*,#54005,.F.);
#78798=ORIENTED_EDGE('',*,*,#54006,.F.);
#78799=ORIENTED_EDGE('',*,*,#54007,.T.);
#78800=ORIENTED_EDGE('',*,*,#54008,.F.);
#78801=ORIENTED_EDGE('',*,*,#54009,.F.);
#78802=ORIENTED_EDGE('',*,*,#54010,.F.);
#78803=ORIENTED_EDGE('',*,*,#54011,.T.);
#78804=ORIENTED_EDGE('',*,*,#54012,.F.);
#78805=ORIENTED_EDGE('',*,*,#54013,.F.);
#78806=ORIENTED_EDGE('',*,*,#54014,.F.);
#78807=ORIENTED_EDGE('',*,*,#54015,.T.);
#78808=ORIENTED_EDGE('',*,*,#54016,.F.);
#78809=ORIENTED_EDGE('',*,*,#54017,.F.);
#78810=ORIENTED_EDGE('',*,*,#54018,.F.);
#78811=ORIENTED_EDGE('',*,*,#54019,.T.);
#78812=ORIENTED_EDGE('',*,*,#54020,.F.);
#78813=ORIENTED_EDGE('',*,*,#54021,.F.);
#78814=ORIENTED_EDGE('',*,*,#54022,.F.);
#78815=ORIENTED_EDGE('',*,*,#54023,.T.);
#78816=ORIENTED_EDGE('',*,*,#54024,.F.);
#78817=ORIENTED_EDGE('',*,*,#54025,.F.);
#78818=ORIENTED_EDGE('',*,*,#54026,.F.);
#78819=ORIENTED_EDGE('',*,*,#54027,.T.);
#78820=ORIENTED_EDGE('',*,*,#54028,.F.);
#78821=ORIENTED_EDGE('',*,*,#54029,.F.);
#78822=ORIENTED_EDGE('',*,*,#54030,.F.);
#78823=ORIENTED_EDGE('',*,*,#54031,.T.);
#78824=ORIENTED_EDGE('',*,*,#54032,.F.);
#78825=ORIENTED_EDGE('',*,*,#54033,.F.);
#78826=ORIENTED_EDGE('',*,*,#54034,.F.);
#78827=ORIENTED_EDGE('',*,*,#54035,.T.);
#78828=ORIENTED_EDGE('',*,*,#54036,.F.);
#78829=ORIENTED_EDGE('',*,*,#54037,.F.);
#78830=ORIENTED_EDGE('',*,*,#54038,.F.);
#78831=ORIENTED_EDGE('',*,*,#54039,.T.);
#78832=ORIENTED_EDGE('',*,*,#54040,.F.);
#78833=ORIENTED_EDGE('',*,*,#54041,.F.);
#78834=ORIENTED_EDGE('',*,*,#54042,.F.);
#78835=ORIENTED_EDGE('',*,*,#54043,.T.);
#78836=ORIENTED_EDGE('',*,*,#54044,.F.);
#78837=ORIENTED_EDGE('',*,*,#54045,.F.);
#78838=ORIENTED_EDGE('',*,*,#54046,.F.);
#78839=ORIENTED_EDGE('',*,*,#54047,.T.);
#78840=ORIENTED_EDGE('',*,*,#54048,.F.);
#78841=ORIENTED_EDGE('',*,*,#54049,.F.);
#78842=ORIENTED_EDGE('',*,*,#54050,.F.);
#78843=ORIENTED_EDGE('',*,*,#54051,.T.);
#78844=ORIENTED_EDGE('',*,*,#54052,.F.);
#78845=ORIENTED_EDGE('',*,*,#54053,.F.);
#78846=ORIENTED_EDGE('',*,*,#54054,.F.);
#78847=ORIENTED_EDGE('',*,*,#54055,.T.);
#78848=ORIENTED_EDGE('',*,*,#54056,.F.);
#78849=ORIENTED_EDGE('',*,*,#54057,.F.);
#78850=ORIENTED_EDGE('',*,*,#54058,.F.);
#78851=ORIENTED_EDGE('',*,*,#54059,.T.);
#78852=ORIENTED_EDGE('',*,*,#54060,.F.);
#78853=ORIENTED_EDGE('',*,*,#54061,.F.);
#78854=ORIENTED_EDGE('',*,*,#54062,.F.);
#78855=ORIENTED_EDGE('',*,*,#54063,.T.);
#78856=ORIENTED_EDGE('',*,*,#54064,.F.);
#78857=ORIENTED_EDGE('',*,*,#54065,.F.);
#78858=ORIENTED_EDGE('',*,*,#54066,.F.);
#78859=ORIENTED_EDGE('',*,*,#54067,.T.);
#78860=ORIENTED_EDGE('',*,*,#54068,.F.);
#78861=ORIENTED_EDGE('',*,*,#54069,.F.);
#78862=ORIENTED_EDGE('',*,*,#54070,.F.);
#78863=ORIENTED_EDGE('',*,*,#54071,.T.);
#78864=ORIENTED_EDGE('',*,*,#54072,.F.);
#78865=ORIENTED_EDGE('',*,*,#54073,.F.);
#78866=ORIENTED_EDGE('',*,*,#54074,.F.);
#78867=ORIENTED_EDGE('',*,*,#54075,.T.);
#78868=ORIENTED_EDGE('',*,*,#54076,.F.);
#78869=ORIENTED_EDGE('',*,*,#54077,.F.);
#78870=ORIENTED_EDGE('',*,*,#54078,.F.);
#78871=ORIENTED_EDGE('',*,*,#54079,.T.);
#78872=ORIENTED_EDGE('',*,*,#54080,.F.);
#78873=ORIENTED_EDGE('',*,*,#54081,.F.);
#78874=ORIENTED_EDGE('',*,*,#54082,.F.);
#78875=ORIENTED_EDGE('',*,*,#54083,.T.);
#78876=ORIENTED_EDGE('',*,*,#54084,.F.);
#78877=ORIENTED_EDGE('',*,*,#54085,.F.);
#78878=ORIENTED_EDGE('',*,*,#54086,.F.);
#78879=ORIENTED_EDGE('',*,*,#54087,.T.);
#78880=ORIENTED_EDGE('',*,*,#54088,.F.);
#78881=ORIENTED_EDGE('',*,*,#54089,.F.);
#78882=ORIENTED_EDGE('',*,*,#54090,.F.);
#78883=ORIENTED_EDGE('',*,*,#54091,.T.);
#78884=ORIENTED_EDGE('',*,*,#54092,.F.);
#78885=ORIENTED_EDGE('',*,*,#54093,.F.);
#78886=ORIENTED_EDGE('',*,*,#54094,.F.);
#78887=ORIENTED_EDGE('',*,*,#54095,.T.);
#78888=ORIENTED_EDGE('',*,*,#54096,.F.);
#78889=ORIENTED_EDGE('',*,*,#54097,.F.);
#78890=ORIENTED_EDGE('',*,*,#54098,.F.);
#78891=ORIENTED_EDGE('',*,*,#54099,.T.);
#78892=ORIENTED_EDGE('',*,*,#54100,.F.);
#78893=ORIENTED_EDGE('',*,*,#54101,.F.);
#78894=ORIENTED_EDGE('',*,*,#54102,.F.);
#78895=ORIENTED_EDGE('',*,*,#54103,.T.);
#78896=ORIENTED_EDGE('',*,*,#54104,.F.);
#78897=ORIENTED_EDGE('',*,*,#54105,.F.);
#78898=ORIENTED_EDGE('',*,*,#54106,.F.);
#78899=ORIENTED_EDGE('',*,*,#54107,.T.);
#78900=ORIENTED_EDGE('',*,*,#54108,.F.);
#78901=ORIENTED_EDGE('',*,*,#54109,.F.);
#78902=ORIENTED_EDGE('',*,*,#54110,.F.);
#78903=ORIENTED_EDGE('',*,*,#54111,.T.);
#78904=ORIENTED_EDGE('',*,*,#54112,.F.);
#78905=ORIENTED_EDGE('',*,*,#54113,.F.);
#78906=ORIENTED_EDGE('',*,*,#54114,.F.);
#78907=ORIENTED_EDGE('',*,*,#54115,.T.);
#78908=ORIENTED_EDGE('',*,*,#54116,.F.);
#78909=ORIENTED_EDGE('',*,*,#54117,.F.);
#78910=ORIENTED_EDGE('',*,*,#54118,.F.);
#78911=ORIENTED_EDGE('',*,*,#54119,.T.);
#78912=ORIENTED_EDGE('',*,*,#54120,.F.);
#78913=ORIENTED_EDGE('',*,*,#54121,.F.);
#78914=ORIENTED_EDGE('',*,*,#54122,.F.);
#78915=ORIENTED_EDGE('',*,*,#54123,.T.);
#78916=ORIENTED_EDGE('',*,*,#54124,.F.);
#78917=ORIENTED_EDGE('',*,*,#54125,.F.);
#78918=ORIENTED_EDGE('',*,*,#54126,.F.);
#78919=ORIENTED_EDGE('',*,*,#54127,.T.);
#78920=ORIENTED_EDGE('',*,*,#54128,.F.);
#78921=ORIENTED_EDGE('',*,*,#54129,.F.);
#78922=ORIENTED_EDGE('',*,*,#54130,.F.);
#78923=ORIENTED_EDGE('',*,*,#54131,.T.);
#78924=ORIENTED_EDGE('',*,*,#54132,.F.);
#78925=ORIENTED_EDGE('',*,*,#54133,.F.);
#78926=ORIENTED_EDGE('',*,*,#54134,.F.);
#78927=ORIENTED_EDGE('',*,*,#54135,.T.);
#78928=ORIENTED_EDGE('',*,*,#54136,.F.);
#78929=ORIENTED_EDGE('',*,*,#54137,.F.);
#78930=ORIENTED_EDGE('',*,*,#54138,.F.);
#78931=ORIENTED_EDGE('',*,*,#54139,.T.);
#78932=ORIENTED_EDGE('',*,*,#54140,.F.);
#78933=ORIENTED_EDGE('',*,*,#54141,.F.);
#78934=ORIENTED_EDGE('',*,*,#54142,.F.);
#78935=ORIENTED_EDGE('',*,*,#54143,.T.);
#78936=ORIENTED_EDGE('',*,*,#54144,.F.);
#78937=ORIENTED_EDGE('',*,*,#54145,.F.);
#78938=ORIENTED_EDGE('',*,*,#54146,.F.);
#78939=ORIENTED_EDGE('',*,*,#54147,.T.);
#78940=ORIENTED_EDGE('',*,*,#54148,.F.);
#78941=ORIENTED_EDGE('',*,*,#54149,.F.);
#78942=ORIENTED_EDGE('',*,*,#54150,.F.);
#78943=ORIENTED_EDGE('',*,*,#54151,.T.);
#78944=ORIENTED_EDGE('',*,*,#54152,.F.);
#78945=ORIENTED_EDGE('',*,*,#54153,.F.);
#78946=ORIENTED_EDGE('',*,*,#54154,.F.);
#78947=ORIENTED_EDGE('',*,*,#54155,.T.);
#78948=ORIENTED_EDGE('',*,*,#54156,.F.);
#78949=ORIENTED_EDGE('',*,*,#54157,.F.);
#78950=ORIENTED_EDGE('',*,*,#54158,.F.);
#78951=ORIENTED_EDGE('',*,*,#54159,.T.);
#78952=ORIENTED_EDGE('',*,*,#54160,.F.);
#78953=ORIENTED_EDGE('',*,*,#54161,.F.);
#78954=ORIENTED_EDGE('',*,*,#54162,.F.);
#78955=ORIENTED_EDGE('',*,*,#54163,.T.);
#78956=ORIENTED_EDGE('',*,*,#54164,.F.);
#78957=ORIENTED_EDGE('',*,*,#54165,.F.);
#78958=ORIENTED_EDGE('',*,*,#54166,.F.);
#78959=ORIENTED_EDGE('',*,*,#54167,.T.);
#78960=ORIENTED_EDGE('',*,*,#54168,.F.);
#78961=ORIENTED_EDGE('',*,*,#54169,.F.);
#78962=ORIENTED_EDGE('',*,*,#54170,.F.);
#78963=ORIENTED_EDGE('',*,*,#54171,.T.);
#78964=ORIENTED_EDGE('',*,*,#54172,.F.);
#78965=ORIENTED_EDGE('',*,*,#54173,.F.);
#78966=ORIENTED_EDGE('',*,*,#54174,.F.);
#78967=ORIENTED_EDGE('',*,*,#54175,.T.);
#78968=ORIENTED_EDGE('',*,*,#54176,.F.);
#78969=ORIENTED_EDGE('',*,*,#54177,.F.);
#78970=ORIENTED_EDGE('',*,*,#54178,.F.);
#78971=ORIENTED_EDGE('',*,*,#54179,.T.);
#78972=ORIENTED_EDGE('',*,*,#54180,.F.);
#78973=ORIENTED_EDGE('',*,*,#54181,.F.);
#78974=ORIENTED_EDGE('',*,*,#54182,.F.);
#78975=ORIENTED_EDGE('',*,*,#54183,.T.);
#78976=ORIENTED_EDGE('',*,*,#54184,.F.);
#78977=ORIENTED_EDGE('',*,*,#54185,.F.);
#78978=ORIENTED_EDGE('',*,*,#54186,.F.);
#78979=ORIENTED_EDGE('',*,*,#54187,.T.);
#78980=ORIENTED_EDGE('',*,*,#54188,.F.);
#78981=ORIENTED_EDGE('',*,*,#54189,.F.);
#78982=ORIENTED_EDGE('',*,*,#54190,.F.);
#78983=ORIENTED_EDGE('',*,*,#54191,.T.);
#78984=ORIENTED_EDGE('',*,*,#54192,.F.);
#78985=ORIENTED_EDGE('',*,*,#54193,.F.);
#78986=ORIENTED_EDGE('',*,*,#54194,.F.);
#78987=ORIENTED_EDGE('',*,*,#54195,.T.);
#78988=ORIENTED_EDGE('',*,*,#54196,.F.);
#78989=ORIENTED_EDGE('',*,*,#54197,.F.);
#78990=ORIENTED_EDGE('',*,*,#54198,.F.);
#78991=ORIENTED_EDGE('',*,*,#54199,.T.);
#78992=ORIENTED_EDGE('',*,*,#54200,.F.);
#78993=ORIENTED_EDGE('',*,*,#54201,.F.);
#78994=ORIENTED_EDGE('',*,*,#54202,.F.);
#78995=ORIENTED_EDGE('',*,*,#54203,.T.);
#78996=ORIENTED_EDGE('',*,*,#54204,.F.);
#78997=ORIENTED_EDGE('',*,*,#54205,.F.);
#78998=ORIENTED_EDGE('',*,*,#54206,.F.);
#78999=ORIENTED_EDGE('',*,*,#54207,.T.);
#79000=ORIENTED_EDGE('',*,*,#54208,.F.);
#79001=ORIENTED_EDGE('',*,*,#54209,.F.);
#79002=ORIENTED_EDGE('',*,*,#54210,.F.);
#79003=ORIENTED_EDGE('',*,*,#54211,.T.);
#79004=ORIENTED_EDGE('',*,*,#54212,.F.);
#79005=ORIENTED_EDGE('',*,*,#54213,.F.);
#79006=ORIENTED_EDGE('',*,*,#54214,.F.);
#79007=ORIENTED_EDGE('',*,*,#54215,.T.);
#79008=ORIENTED_EDGE('',*,*,#54216,.F.);
#79009=ORIENTED_EDGE('',*,*,#54217,.F.);
#79010=ORIENTED_EDGE('',*,*,#54218,.F.);
#79011=ORIENTED_EDGE('',*,*,#54219,.T.);
#79012=ORIENTED_EDGE('',*,*,#54220,.F.);
#79013=ORIENTED_EDGE('',*,*,#54221,.F.);
#79014=ORIENTED_EDGE('',*,*,#54222,.F.);
#79015=ORIENTED_EDGE('',*,*,#54223,.T.);
#79016=ORIENTED_EDGE('',*,*,#54224,.F.);
#79017=ORIENTED_EDGE('',*,*,#54225,.F.);
#79018=ORIENTED_EDGE('',*,*,#54226,.F.);
#79019=ORIENTED_EDGE('',*,*,#54227,.T.);
#79020=ORIENTED_EDGE('',*,*,#54228,.F.);
#79021=ORIENTED_EDGE('',*,*,#54229,.F.);
#79022=ORIENTED_EDGE('',*,*,#54230,.F.);
#79023=ORIENTED_EDGE('',*,*,#54231,.T.);
#79024=ORIENTED_EDGE('',*,*,#54232,.F.);
#79025=ORIENTED_EDGE('',*,*,#54233,.F.);
#79026=ORIENTED_EDGE('',*,*,#54234,.F.);
#79027=ORIENTED_EDGE('',*,*,#54235,.T.);
#79028=ORIENTED_EDGE('',*,*,#54236,.F.);
#79029=ORIENTED_EDGE('',*,*,#54237,.F.);
#79030=ORIENTED_EDGE('',*,*,#54238,.F.);
#79031=ORIENTED_EDGE('',*,*,#54239,.T.);
#79032=ORIENTED_EDGE('',*,*,#54240,.F.);
#79033=ORIENTED_EDGE('',*,*,#54241,.F.);
#79034=ORIENTED_EDGE('',*,*,#54242,.F.);
#79035=ORIENTED_EDGE('',*,*,#54243,.T.);
#79036=ORIENTED_EDGE('',*,*,#54244,.F.);
#79037=ORIENTED_EDGE('',*,*,#54245,.F.);
#79038=ORIENTED_EDGE('',*,*,#54246,.F.);
#79039=ORIENTED_EDGE('',*,*,#54247,.T.);
#79040=ORIENTED_EDGE('',*,*,#54248,.F.);
#79041=ORIENTED_EDGE('',*,*,#54249,.F.);
#79042=ORIENTED_EDGE('',*,*,#54250,.F.);
#79043=ORIENTED_EDGE('',*,*,#54251,.T.);
#79044=ORIENTED_EDGE('',*,*,#54252,.F.);
#79045=ORIENTED_EDGE('',*,*,#54253,.F.);
#79046=ORIENTED_EDGE('',*,*,#54254,.F.);
#79047=ORIENTED_EDGE('',*,*,#54255,.T.);
#79048=ORIENTED_EDGE('',*,*,#54256,.F.);
#79049=ORIENTED_EDGE('',*,*,#54257,.F.);
#79050=ORIENTED_EDGE('',*,*,#54258,.F.);
#79051=ORIENTED_EDGE('',*,*,#54259,.F.);
#79052=ORIENTED_EDGE('',*,*,#54260,.T.);
#79053=ORIENTED_EDGE('',*,*,#53950,.F.);
#79054=ORIENTED_EDGE('',*,*,#54261,.F.);
#79055=ORIENTED_EDGE('',*,*,#53943,.T.);
#79056=ORIENTED_EDGE('',*,*,#54262,.F.);
#79057=ORIENTED_EDGE('',*,*,#53839,.T.);
#79058=ORIENTED_EDGE('',*,*,#54263,.T.);
#79059=ORIENTED_EDGE('',*,*,#54264,.F.);
#79060=ORIENTED_EDGE('',*,*,#53844,.F.);
#79061=ORIENTED_EDGE('',*,*,#54265,.F.);
#79062=ORIENTED_EDGE('',*,*,#54266,.T.);
#79063=ORIENTED_EDGE('',*,*,#54267,.T.);
#79064=ORIENTED_EDGE('',*,*,#53946,.F.);
#79065=ORIENTED_EDGE('',*,*,#54267,.F.);
#79066=ORIENTED_EDGE('',*,*,#53835,.T.);
#79067=ORIENTED_EDGE('',*,*,#54268,.T.);
#79068=ORIENTED_EDGE('',*,*,#53948,.T.);
#79069=ORIENTED_EDGE('',*,*,#54269,.T.);
#79070=ORIENTED_EDGE('',*,*,#54270,.F.);
#79071=ORIENTED_EDGE('',*,*,#54271,.F.);
#79072=ORIENTED_EDGE('',*,*,#54272,.F.);
#79073=ORIENTED_EDGE('',*,*,#54273,.T.);
#79074=ORIENTED_EDGE('',*,*,#54274,.F.);
#79075=ORIENTED_EDGE('',*,*,#54275,.F.);
#79076=ORIENTED_EDGE('',*,*,#54269,.F.);
#79077=ORIENTED_EDGE('',*,*,#54276,.T.);
#79078=ORIENTED_EDGE('',*,*,#54277,.T.);
#79079=ORIENTED_EDGE('',*,*,#54278,.F.);
#79080=ORIENTED_EDGE('',*,*,#54279,.T.);
#79081=ORIENTED_EDGE('',*,*,#54280,.T.);
#79082=ORIENTED_EDGE('',*,*,#54279,.F.);
#79083=ORIENTED_EDGE('',*,*,#54281,.F.);
#79084=ORIENTED_EDGE('',*,*,#54282,.T.);
#79085=ORIENTED_EDGE('',*,*,#54278,.T.);
#79086=ORIENTED_EDGE('',*,*,#54282,.F.);
#79087=ORIENTED_EDGE('',*,*,#54283,.F.);
#79088=ORIENTED_EDGE('',*,*,#54284,.T.);
#79089=ORIENTED_EDGE('',*,*,#54281,.T.);
#79090=ORIENTED_EDGE('',*,*,#54284,.F.);
#79091=ORIENTED_EDGE('',*,*,#54285,.T.);
#79092=ORIENTED_EDGE('',*,*,#54286,.T.);
#79093=ORIENTED_EDGE('',*,*,#54287,.T.);
#79094=ORIENTED_EDGE('',*,*,#54288,.T.);
#79095=ORIENTED_EDGE('',*,*,#54289,.T.);
#79096=ORIENTED_EDGE('',*,*,#54290,.T.);
#79097=ORIENTED_EDGE('',*,*,#54291,.T.);
#79098=ORIENTED_EDGE('',*,*,#54292,.T.);
#79099=ORIENTED_EDGE('',*,*,#54293,.T.);
#79100=ORIENTED_EDGE('',*,*,#54294,.T.);
#79101=ORIENTED_EDGE('',*,*,#54295,.T.);
#79102=ORIENTED_EDGE('',*,*,#54296,.T.);
#79103=ORIENTED_EDGE('',*,*,#54297,.T.);
#79104=ORIENTED_EDGE('',*,*,#54298,.T.);
#79105=ORIENTED_EDGE('',*,*,#54299,.T.);
#79106=ORIENTED_EDGE('',*,*,#54300,.T.);
#79107=ORIENTED_EDGE('',*,*,#54301,.T.);
#79108=ORIENTED_EDGE('',*,*,#54302,.T.);
#79109=ORIENTED_EDGE('',*,*,#54303,.T.);
#79110=ORIENTED_EDGE('',*,*,#54304,.T.);
#79111=ORIENTED_EDGE('',*,*,#54305,.T.);
#79112=ORIENTED_EDGE('',*,*,#54306,.T.);
#79113=ORIENTED_EDGE('',*,*,#54307,.T.);
#79114=ORIENTED_EDGE('',*,*,#54308,.T.);
#79115=ORIENTED_EDGE('',*,*,#54309,.T.);
#79116=ORIENTED_EDGE('',*,*,#54310,.T.);
#79117=ORIENTED_EDGE('',*,*,#54311,.T.);
#79118=ORIENTED_EDGE('',*,*,#54312,.T.);
#79119=ORIENTED_EDGE('',*,*,#54313,.T.);
#79120=ORIENTED_EDGE('',*,*,#54314,.T.);
#79121=ORIENTED_EDGE('',*,*,#54315,.T.);
#79122=ORIENTED_EDGE('',*,*,#54316,.T.);
#79123=ORIENTED_EDGE('',*,*,#54317,.T.);
#79124=ORIENTED_EDGE('',*,*,#54318,.T.);
#79125=ORIENTED_EDGE('',*,*,#54319,.T.);
#79126=ORIENTED_EDGE('',*,*,#54320,.T.);
#79127=ORIENTED_EDGE('',*,*,#54321,.T.);
#79128=ORIENTED_EDGE('',*,*,#54322,.T.);
#79129=ORIENTED_EDGE('',*,*,#54323,.T.);
#79130=ORIENTED_EDGE('',*,*,#54324,.T.);
#79131=ORIENTED_EDGE('',*,*,#54325,.T.);
#79132=ORIENTED_EDGE('',*,*,#54326,.T.);
#79133=ORIENTED_EDGE('',*,*,#54327,.T.);
#79134=ORIENTED_EDGE('',*,*,#54328,.T.);
#79135=ORIENTED_EDGE('',*,*,#54329,.T.);
#79136=ORIENTED_EDGE('',*,*,#54330,.T.);
#79137=ORIENTED_EDGE('',*,*,#54331,.T.);
#79138=ORIENTED_EDGE('',*,*,#54332,.T.);
#79139=ORIENTED_EDGE('',*,*,#54333,.T.);
#79140=ORIENTED_EDGE('',*,*,#54334,.T.);
#79141=ORIENTED_EDGE('',*,*,#54335,.T.);
#79142=ORIENTED_EDGE('',*,*,#54336,.T.);
#79143=ORIENTED_EDGE('',*,*,#54337,.T.);
#79144=ORIENTED_EDGE('',*,*,#54338,.T.);
#79145=ORIENTED_EDGE('',*,*,#54339,.T.);
#79146=ORIENTED_EDGE('',*,*,#54340,.T.);
#79147=ORIENTED_EDGE('',*,*,#54341,.T.);
#79148=ORIENTED_EDGE('',*,*,#54342,.T.);
#79149=ORIENTED_EDGE('',*,*,#54343,.T.);
#79150=ORIENTED_EDGE('',*,*,#54344,.T.);
#79151=ORIENTED_EDGE('',*,*,#54345,.T.);
#79152=ORIENTED_EDGE('',*,*,#54346,.T.);
#79153=ORIENTED_EDGE('',*,*,#54347,.T.);
#79154=ORIENTED_EDGE('',*,*,#54348,.T.);
#79155=ORIENTED_EDGE('',*,*,#54349,.T.);
#79156=ORIENTED_EDGE('',*,*,#54350,.T.);
#79157=ORIENTED_EDGE('',*,*,#54351,.T.);
#79158=ORIENTED_EDGE('',*,*,#54352,.T.);
#79159=ORIENTED_EDGE('',*,*,#54353,.T.);
#79160=ORIENTED_EDGE('',*,*,#54354,.T.);
#79161=ORIENTED_EDGE('',*,*,#54355,.T.);
#79162=ORIENTED_EDGE('',*,*,#54356,.T.);
#79163=ORIENTED_EDGE('',*,*,#54357,.T.);
#79164=ORIENTED_EDGE('',*,*,#54358,.T.);
#79165=ORIENTED_EDGE('',*,*,#54359,.T.);
#79166=ORIENTED_EDGE('',*,*,#54360,.T.);
#79167=ORIENTED_EDGE('',*,*,#54361,.T.);
#79168=ORIENTED_EDGE('',*,*,#54362,.T.);
#79169=ORIENTED_EDGE('',*,*,#54363,.T.);
#79170=ORIENTED_EDGE('',*,*,#54364,.T.);
#79171=ORIENTED_EDGE('',*,*,#54365,.T.);
#79172=ORIENTED_EDGE('',*,*,#54366,.T.);
#79173=ORIENTED_EDGE('',*,*,#54367,.T.);
#79174=ORIENTED_EDGE('',*,*,#54368,.T.);
#79175=ORIENTED_EDGE('',*,*,#54369,.T.);
#79176=ORIENTED_EDGE('',*,*,#54370,.T.);
#79177=ORIENTED_EDGE('',*,*,#54371,.T.);
#79178=ORIENTED_EDGE('',*,*,#54372,.T.);
#79179=ORIENTED_EDGE('',*,*,#54373,.T.);
#79180=ORIENTED_EDGE('',*,*,#54374,.T.);
#79181=ORIENTED_EDGE('',*,*,#54375,.T.);
#79182=ORIENTED_EDGE('',*,*,#54376,.T.);
#79183=ORIENTED_EDGE('',*,*,#54377,.T.);
#79184=ORIENTED_EDGE('',*,*,#54378,.T.);
#79185=ORIENTED_EDGE('',*,*,#54379,.T.);
#79186=ORIENTED_EDGE('',*,*,#54380,.T.);
#79187=ORIENTED_EDGE('',*,*,#54381,.T.);
#79188=ORIENTED_EDGE('',*,*,#54382,.T.);
#79189=ORIENTED_EDGE('',*,*,#54383,.T.);
#79190=ORIENTED_EDGE('',*,*,#54384,.T.);
#79191=ORIENTED_EDGE('',*,*,#54385,.T.);
#79192=ORIENTED_EDGE('',*,*,#54386,.T.);
#79193=ORIENTED_EDGE('',*,*,#54387,.T.);
#79194=ORIENTED_EDGE('',*,*,#54388,.T.);
#79195=ORIENTED_EDGE('',*,*,#54389,.T.);
#79196=ORIENTED_EDGE('',*,*,#54390,.T.);
#79197=ORIENTED_EDGE('',*,*,#54391,.T.);
#79198=ORIENTED_EDGE('',*,*,#54392,.T.);
#79199=ORIENTED_EDGE('',*,*,#54393,.T.);
#79200=ORIENTED_EDGE('',*,*,#54394,.T.);
#79201=ORIENTED_EDGE('',*,*,#54395,.T.);
#79202=ORIENTED_EDGE('',*,*,#54396,.T.);
#79203=ORIENTED_EDGE('',*,*,#54397,.T.);
#79204=ORIENTED_EDGE('',*,*,#54398,.T.);
#79205=ORIENTED_EDGE('',*,*,#54399,.T.);
#79206=ORIENTED_EDGE('',*,*,#54400,.T.);
#79207=ORIENTED_EDGE('',*,*,#54401,.T.);
#79208=ORIENTED_EDGE('',*,*,#54402,.T.);
#79209=ORIENTED_EDGE('',*,*,#54403,.T.);
#79210=ORIENTED_EDGE('',*,*,#54404,.T.);
#79211=ORIENTED_EDGE('',*,*,#54405,.T.);
#79212=ORIENTED_EDGE('',*,*,#54406,.T.);
#79213=ORIENTED_EDGE('',*,*,#54407,.T.);
#79214=ORIENTED_EDGE('',*,*,#54408,.T.);
#79215=ORIENTED_EDGE('',*,*,#54409,.T.);
#79216=ORIENTED_EDGE('',*,*,#54410,.T.);
#79217=ORIENTED_EDGE('',*,*,#54411,.T.);
#79218=ORIENTED_EDGE('',*,*,#54412,.T.);
#79219=ORIENTED_EDGE('',*,*,#54413,.T.);
#79220=ORIENTED_EDGE('',*,*,#54414,.T.);
#79221=ORIENTED_EDGE('',*,*,#54415,.T.);
#79222=ORIENTED_EDGE('',*,*,#54416,.T.);
#79223=ORIENTED_EDGE('',*,*,#54417,.T.);
#79224=ORIENTED_EDGE('',*,*,#54418,.T.);
#79225=ORIENTED_EDGE('',*,*,#54419,.T.);
#79226=ORIENTED_EDGE('',*,*,#54420,.T.);
#79227=ORIENTED_EDGE('',*,*,#54421,.T.);
#79228=ORIENTED_EDGE('',*,*,#54422,.T.);
#79229=ORIENTED_EDGE('',*,*,#54423,.T.);
#79230=ORIENTED_EDGE('',*,*,#54424,.T.);
#79231=ORIENTED_EDGE('',*,*,#54425,.T.);
#79232=ORIENTED_EDGE('',*,*,#54426,.T.);
#79233=ORIENTED_EDGE('',*,*,#54427,.T.);
#79234=ORIENTED_EDGE('',*,*,#54428,.T.);
#79235=ORIENTED_EDGE('',*,*,#54429,.T.);
#79236=ORIENTED_EDGE('',*,*,#54430,.T.);
#79237=ORIENTED_EDGE('',*,*,#54431,.T.);
#79238=ORIENTED_EDGE('',*,*,#54432,.T.);
#79239=ORIENTED_EDGE('',*,*,#54433,.T.);
#79240=ORIENTED_EDGE('',*,*,#54434,.T.);
#79241=ORIENTED_EDGE('',*,*,#54435,.T.);
#79242=ORIENTED_EDGE('',*,*,#54436,.T.);
#79243=ORIENTED_EDGE('',*,*,#54437,.T.);
#79244=ORIENTED_EDGE('',*,*,#54438,.T.);
#79245=ORIENTED_EDGE('',*,*,#54439,.T.);
#79246=ORIENTED_EDGE('',*,*,#54440,.T.);
#79247=ORIENTED_EDGE('',*,*,#54441,.F.);
#79248=ORIENTED_EDGE('',*,*,#54442,.F.);
#79249=ORIENTED_EDGE('',*,*,#54440,.F.);
#79250=ORIENTED_EDGE('',*,*,#54443,.T.);
#79251=ORIENTED_EDGE('',*,*,#54444,.T.);
#79252=ORIENTED_EDGE('',*,*,#54445,.T.);
#79253=ORIENTED_EDGE('',*,*,#54446,.T.);
#79254=ORIENTED_EDGE('',*,*,#54447,.T.);
#79255=ORIENTED_EDGE('',*,*,#54448,.T.);
#79256=ORIENTED_EDGE('',*,*,#54449,.T.);
#79257=ORIENTED_EDGE('',*,*,#54450,.T.);
#79258=ORIENTED_EDGE('',*,*,#54451,.T.);
#79259=ORIENTED_EDGE('',*,*,#54452,.T.);
#79260=ORIENTED_EDGE('',*,*,#54453,.T.);
#79261=ORIENTED_EDGE('',*,*,#54454,.T.);
#79262=ORIENTED_EDGE('',*,*,#54455,.T.);
#79263=ORIENTED_EDGE('',*,*,#54456,.T.);
#79264=ORIENTED_EDGE('',*,*,#54457,.T.);
#79265=ORIENTED_EDGE('',*,*,#54458,.T.);
#79266=ORIENTED_EDGE('',*,*,#54459,.T.);
#79267=ORIENTED_EDGE('',*,*,#54460,.T.);
#79268=ORIENTED_EDGE('',*,*,#54461,.T.);
#79269=ORIENTED_EDGE('',*,*,#54462,.T.);
#79270=ORIENTED_EDGE('',*,*,#54463,.T.);
#79271=ORIENTED_EDGE('',*,*,#54464,.T.);
#79272=ORIENTED_EDGE('',*,*,#54465,.T.);
#79273=ORIENTED_EDGE('',*,*,#54466,.T.);
#79274=ORIENTED_EDGE('',*,*,#54467,.T.);
#79275=ORIENTED_EDGE('',*,*,#54468,.T.);
#79276=ORIENTED_EDGE('',*,*,#54469,.T.);
#79277=ORIENTED_EDGE('',*,*,#54470,.T.);
#79278=ORIENTED_EDGE('',*,*,#54471,.T.);
#79279=ORIENTED_EDGE('',*,*,#54472,.T.);
#79280=ORIENTED_EDGE('',*,*,#54473,.T.);
#79281=ORIENTED_EDGE('',*,*,#54474,.T.);
#79282=ORIENTED_EDGE('',*,*,#54475,.T.);
#79283=ORIENTED_EDGE('',*,*,#54476,.T.);
#79284=ORIENTED_EDGE('',*,*,#54477,.T.);
#79285=ORIENTED_EDGE('',*,*,#54478,.T.);
#79286=ORIENTED_EDGE('',*,*,#54479,.T.);
#79287=ORIENTED_EDGE('',*,*,#54480,.T.);
#79288=ORIENTED_EDGE('',*,*,#54481,.T.);
#79289=ORIENTED_EDGE('',*,*,#54482,.T.);
#79290=ORIENTED_EDGE('',*,*,#54483,.T.);
#79291=ORIENTED_EDGE('',*,*,#54484,.T.);
#79292=ORIENTED_EDGE('',*,*,#54485,.T.);
#79293=ORIENTED_EDGE('',*,*,#54486,.T.);
#79294=ORIENTED_EDGE('',*,*,#54487,.T.);
#79295=ORIENTED_EDGE('',*,*,#54488,.T.);
#79296=ORIENTED_EDGE('',*,*,#54489,.T.);
#79297=ORIENTED_EDGE('',*,*,#54490,.T.);
#79298=ORIENTED_EDGE('',*,*,#54491,.T.);
#79299=ORIENTED_EDGE('',*,*,#54492,.T.);
#79300=ORIENTED_EDGE('',*,*,#54493,.T.);
#79301=ORIENTED_EDGE('',*,*,#54494,.T.);
#79302=ORIENTED_EDGE('',*,*,#54495,.T.);
#79303=ORIENTED_EDGE('',*,*,#54496,.T.);
#79304=ORIENTED_EDGE('',*,*,#54497,.T.);
#79305=ORIENTED_EDGE('',*,*,#54498,.T.);
#79306=ORIENTED_EDGE('',*,*,#54499,.T.);
#79307=ORIENTED_EDGE('',*,*,#54500,.T.);
#79308=ORIENTED_EDGE('',*,*,#54501,.T.);
#79309=ORIENTED_EDGE('',*,*,#54502,.T.);
#79310=ORIENTED_EDGE('',*,*,#54503,.T.);
#79311=ORIENTED_EDGE('',*,*,#54504,.T.);
#79312=ORIENTED_EDGE('',*,*,#54505,.T.);
#79313=ORIENTED_EDGE('',*,*,#54506,.T.);
#79314=ORIENTED_EDGE('',*,*,#54507,.T.);
#79315=ORIENTED_EDGE('',*,*,#54508,.T.);
#79316=ORIENTED_EDGE('',*,*,#54509,.T.);
#79317=ORIENTED_EDGE('',*,*,#54510,.T.);
#79318=ORIENTED_EDGE('',*,*,#54511,.T.);
#79319=ORIENTED_EDGE('',*,*,#54512,.T.);
#79320=ORIENTED_EDGE('',*,*,#54513,.T.);
#79321=ORIENTED_EDGE('',*,*,#54514,.T.);
#79322=ORIENTED_EDGE('',*,*,#54515,.T.);
#79323=ORIENTED_EDGE('',*,*,#54516,.T.);
#79324=ORIENTED_EDGE('',*,*,#54517,.T.);
#79325=ORIENTED_EDGE('',*,*,#54518,.T.);
#79326=ORIENTED_EDGE('',*,*,#54519,.T.);
#79327=ORIENTED_EDGE('',*,*,#54520,.T.);
#79328=ORIENTED_EDGE('',*,*,#54521,.T.);
#79329=ORIENTED_EDGE('',*,*,#54522,.T.);
#79330=ORIENTED_EDGE('',*,*,#54523,.T.);
#79331=ORIENTED_EDGE('',*,*,#54524,.T.);
#79332=ORIENTED_EDGE('',*,*,#54525,.T.);
#79333=ORIENTED_EDGE('',*,*,#54526,.T.);
#79334=ORIENTED_EDGE('',*,*,#54527,.T.);
#79335=ORIENTED_EDGE('',*,*,#54528,.T.);
#79336=ORIENTED_EDGE('',*,*,#54529,.T.);
#79337=ORIENTED_EDGE('',*,*,#54530,.T.);
#79338=ORIENTED_EDGE('',*,*,#54531,.T.);
#79339=ORIENTED_EDGE('',*,*,#54532,.T.);
#79340=ORIENTED_EDGE('',*,*,#54533,.T.);
#79341=ORIENTED_EDGE('',*,*,#54534,.T.);
#79342=ORIENTED_EDGE('',*,*,#54535,.T.);
#79343=ORIENTED_EDGE('',*,*,#54536,.T.);
#79344=ORIENTED_EDGE('',*,*,#54537,.T.);
#79345=ORIENTED_EDGE('',*,*,#54538,.T.);
#79346=ORIENTED_EDGE('',*,*,#54539,.T.);
#79347=ORIENTED_EDGE('',*,*,#54540,.T.);
#79348=ORIENTED_EDGE('',*,*,#54541,.T.);
#79349=ORIENTED_EDGE('',*,*,#54542,.T.);
#79350=ORIENTED_EDGE('',*,*,#54543,.T.);
#79351=ORIENTED_EDGE('',*,*,#54544,.T.);
#79352=ORIENTED_EDGE('',*,*,#54545,.T.);
#79353=ORIENTED_EDGE('',*,*,#54546,.T.);
#79354=ORIENTED_EDGE('',*,*,#54547,.T.);
#79355=ORIENTED_EDGE('',*,*,#54548,.T.);
#79356=ORIENTED_EDGE('',*,*,#54549,.T.);
#79357=ORIENTED_EDGE('',*,*,#54550,.T.);
#79358=ORIENTED_EDGE('',*,*,#54551,.T.);
#79359=ORIENTED_EDGE('',*,*,#54552,.T.);
#79360=ORIENTED_EDGE('',*,*,#54553,.T.);
#79361=ORIENTED_EDGE('',*,*,#54554,.T.);
#79362=ORIENTED_EDGE('',*,*,#54555,.T.);
#79363=ORIENTED_EDGE('',*,*,#54556,.T.);
#79364=ORIENTED_EDGE('',*,*,#54557,.T.);
#79365=ORIENTED_EDGE('',*,*,#54558,.T.);
#79366=ORIENTED_EDGE('',*,*,#54559,.T.);
#79367=ORIENTED_EDGE('',*,*,#54560,.T.);
#79368=ORIENTED_EDGE('',*,*,#54561,.T.);
#79369=ORIENTED_EDGE('',*,*,#54562,.T.);
#79370=ORIENTED_EDGE('',*,*,#54563,.T.);
#79371=ORIENTED_EDGE('',*,*,#54564,.T.);
#79372=ORIENTED_EDGE('',*,*,#54565,.T.);
#79373=ORIENTED_EDGE('',*,*,#54566,.T.);
#79374=ORIENTED_EDGE('',*,*,#54567,.T.);
#79375=ORIENTED_EDGE('',*,*,#54568,.T.);
#79376=ORIENTED_EDGE('',*,*,#54569,.T.);
#79377=ORIENTED_EDGE('',*,*,#54570,.T.);
#79378=ORIENTED_EDGE('',*,*,#54571,.T.);
#79379=ORIENTED_EDGE('',*,*,#54572,.T.);
#79380=ORIENTED_EDGE('',*,*,#54573,.T.);
#79381=ORIENTED_EDGE('',*,*,#54574,.T.);
#79382=ORIENTED_EDGE('',*,*,#54575,.T.);
#79383=ORIENTED_EDGE('',*,*,#54576,.T.);
#79384=ORIENTED_EDGE('',*,*,#54577,.T.);
#79385=ORIENTED_EDGE('',*,*,#54578,.T.);
#79386=ORIENTED_EDGE('',*,*,#54579,.T.);
#79387=ORIENTED_EDGE('',*,*,#54580,.T.);
#79388=ORIENTED_EDGE('',*,*,#54581,.T.);
#79389=ORIENTED_EDGE('',*,*,#54582,.T.);
#79390=ORIENTED_EDGE('',*,*,#54583,.T.);
#79391=ORIENTED_EDGE('',*,*,#54584,.T.);
#79392=ORIENTED_EDGE('',*,*,#54585,.T.);
#79393=ORIENTED_EDGE('',*,*,#54586,.T.);
#79394=ORIENTED_EDGE('',*,*,#54587,.T.);
#79395=ORIENTED_EDGE('',*,*,#54588,.T.);
#79396=ORIENTED_EDGE('',*,*,#54589,.T.);
#79397=ORIENTED_EDGE('',*,*,#54590,.T.);
#79398=ORIENTED_EDGE('',*,*,#54591,.T.);
#79399=ORIENTED_EDGE('',*,*,#54592,.T.);
#79400=ORIENTED_EDGE('',*,*,#54593,.T.);
#79401=ORIENTED_EDGE('',*,*,#54594,.T.);
#79402=ORIENTED_EDGE('',*,*,#54595,.T.);
#79403=ORIENTED_EDGE('',*,*,#54596,.T.);
#79404=ORIENTED_EDGE('',*,*,#54597,.T.);
#79405=ORIENTED_EDGE('',*,*,#54598,.F.);
#79406=ORIENTED_EDGE('',*,*,#54599,.T.);
#79407=ORIENTED_EDGE('',*,*,#54441,.T.);
#79408=ORIENTED_EDGE('',*,*,#54442,.T.);
#79409=ORIENTED_EDGE('',*,*,#54599,.F.);
#79410=ORIENTED_EDGE('',*,*,#54600,.F.);
#79411=ORIENTED_EDGE('',*,*,#54601,.T.);
#79412=ORIENTED_EDGE('',*,*,#54602,.F.);
#79413=ORIENTED_EDGE('',*,*,#54062,.T.);
#79414=ORIENTED_EDGE('',*,*,#54603,.F.);
#79415=ORIENTED_EDGE('',*,*,#54604,.T.);
#79416=ORIENTED_EDGE('',*,*,#54605,.F.);
#79417=ORIENTED_EDGE('',*,*,#54606,.T.);
#79418=ORIENTED_EDGE('',*,*,#54607,.F.);
#79419=ORIENTED_EDGE('',*,*,#54066,.T.);
#79420=ORIENTED_EDGE('',*,*,#54608,.F.);
#79421=ORIENTED_EDGE('',*,*,#54609,.T.);
#79422=ORIENTED_EDGE('',*,*,#54610,.F.);
#79423=ORIENTED_EDGE('',*,*,#54611,.T.);
#79424=ORIENTED_EDGE('',*,*,#54612,.F.);
#79425=ORIENTED_EDGE('',*,*,#54070,.T.);
#79426=ORIENTED_EDGE('',*,*,#54613,.F.);
#79427=ORIENTED_EDGE('',*,*,#54614,.T.);
#79428=ORIENTED_EDGE('',*,*,#54615,.F.);
#79429=ORIENTED_EDGE('',*,*,#54616,.T.);
#79430=ORIENTED_EDGE('',*,*,#54617,.F.);
#79431=ORIENTED_EDGE('',*,*,#54074,.T.);
#79432=ORIENTED_EDGE('',*,*,#54618,.F.);
#79433=ORIENTED_EDGE('',*,*,#54619,.T.);
#79434=ORIENTED_EDGE('',*,*,#54620,.F.);
#79435=ORIENTED_EDGE('',*,*,#54621,.T.);
#79436=ORIENTED_EDGE('',*,*,#54622,.F.);
#79437=ORIENTED_EDGE('',*,*,#54078,.T.);
#79438=ORIENTED_EDGE('',*,*,#54623,.F.);
#79439=ORIENTED_EDGE('',*,*,#54624,.T.);
#79440=ORIENTED_EDGE('',*,*,#54625,.F.);
#79441=ORIENTED_EDGE('',*,*,#54626,.T.);
#79442=ORIENTED_EDGE('',*,*,#54627,.F.);
#79443=ORIENTED_EDGE('',*,*,#54082,.T.);
#79444=ORIENTED_EDGE('',*,*,#54628,.F.);
#79445=ORIENTED_EDGE('',*,*,#54629,.T.);
#79446=ORIENTED_EDGE('',*,*,#54630,.F.);
#79447=ORIENTED_EDGE('',*,*,#54631,.T.);
#79448=ORIENTED_EDGE('',*,*,#54632,.F.);
#79449=ORIENTED_EDGE('',*,*,#54086,.T.);
#79450=ORIENTED_EDGE('',*,*,#54633,.F.);
#79451=ORIENTED_EDGE('',*,*,#54634,.T.);
#79452=ORIENTED_EDGE('',*,*,#54635,.F.);
#79453=ORIENTED_EDGE('',*,*,#54636,.T.);
#79454=ORIENTED_EDGE('',*,*,#54637,.F.);
#79455=ORIENTED_EDGE('',*,*,#54090,.T.);
#79456=ORIENTED_EDGE('',*,*,#54638,.F.);
#79457=ORIENTED_EDGE('',*,*,#54639,.T.);
#79458=ORIENTED_EDGE('',*,*,#54640,.F.);
#79459=ORIENTED_EDGE('',*,*,#54641,.T.);
#79460=ORIENTED_EDGE('',*,*,#54642,.F.);
#79461=ORIENTED_EDGE('',*,*,#54094,.T.);
#79462=ORIENTED_EDGE('',*,*,#54643,.F.);
#79463=ORIENTED_EDGE('',*,*,#54644,.T.);
#79464=ORIENTED_EDGE('',*,*,#54645,.F.);
#79465=ORIENTED_EDGE('',*,*,#54646,.T.);
#79466=ORIENTED_EDGE('',*,*,#54647,.F.);
#79467=ORIENTED_EDGE('',*,*,#54098,.T.);
#79468=ORIENTED_EDGE('',*,*,#54648,.F.);
#79469=ORIENTED_EDGE('',*,*,#54649,.T.);
#79470=ORIENTED_EDGE('',*,*,#54650,.F.);
#79471=ORIENTED_EDGE('',*,*,#54651,.T.);
#79472=ORIENTED_EDGE('',*,*,#54652,.F.);
#79473=ORIENTED_EDGE('',*,*,#54102,.T.);
#79474=ORIENTED_EDGE('',*,*,#54653,.F.);
#79475=ORIENTED_EDGE('',*,*,#54654,.T.);
#79476=ORIENTED_EDGE('',*,*,#54655,.F.);
#79477=ORIENTED_EDGE('',*,*,#54656,.T.);
#79478=ORIENTED_EDGE('',*,*,#54657,.F.);
#79479=ORIENTED_EDGE('',*,*,#54106,.T.);
#79480=ORIENTED_EDGE('',*,*,#54658,.F.);
#79481=ORIENTED_EDGE('',*,*,#54659,.T.);
#79482=ORIENTED_EDGE('',*,*,#54660,.F.);
#79483=ORIENTED_EDGE('',*,*,#54661,.T.);
#79484=ORIENTED_EDGE('',*,*,#54662,.F.);
#79485=ORIENTED_EDGE('',*,*,#54110,.T.);
#79486=ORIENTED_EDGE('',*,*,#54663,.F.);
#79487=ORIENTED_EDGE('',*,*,#54664,.T.);
#79488=ORIENTED_EDGE('',*,*,#54665,.F.);
#79489=ORIENTED_EDGE('',*,*,#54666,.T.);
#79490=ORIENTED_EDGE('',*,*,#54667,.F.);
#79491=ORIENTED_EDGE('',*,*,#54114,.T.);
#79492=ORIENTED_EDGE('',*,*,#54668,.F.);
#79493=ORIENTED_EDGE('',*,*,#54669,.T.);
#79494=ORIENTED_EDGE('',*,*,#54670,.F.);
#79495=ORIENTED_EDGE('',*,*,#54671,.T.);
#79496=ORIENTED_EDGE('',*,*,#54672,.F.);
#79497=ORIENTED_EDGE('',*,*,#54118,.T.);
#79498=ORIENTED_EDGE('',*,*,#54673,.F.);
#79499=ORIENTED_EDGE('',*,*,#54674,.T.);
#79500=ORIENTED_EDGE('',*,*,#54675,.F.);
#79501=ORIENTED_EDGE('',*,*,#54676,.T.);
#79502=ORIENTED_EDGE('',*,*,#54677,.F.);
#79503=ORIENTED_EDGE('',*,*,#54122,.T.);
#79504=ORIENTED_EDGE('',*,*,#54678,.F.);
#79505=ORIENTED_EDGE('',*,*,#54679,.T.);
#79506=ORIENTED_EDGE('',*,*,#54680,.F.);
#79507=ORIENTED_EDGE('',*,*,#54681,.T.);
#79508=ORIENTED_EDGE('',*,*,#54682,.F.);
#79509=ORIENTED_EDGE('',*,*,#54126,.T.);
#79510=ORIENTED_EDGE('',*,*,#54683,.F.);
#79511=ORIENTED_EDGE('',*,*,#54684,.T.);
#79512=ORIENTED_EDGE('',*,*,#54685,.F.);
#79513=ORIENTED_EDGE('',*,*,#54686,.T.);
#79514=ORIENTED_EDGE('',*,*,#54687,.F.);
#79515=ORIENTED_EDGE('',*,*,#54130,.T.);
#79516=ORIENTED_EDGE('',*,*,#54688,.F.);
#79517=ORIENTED_EDGE('',*,*,#54689,.T.);
#79518=ORIENTED_EDGE('',*,*,#54690,.F.);
#79519=ORIENTED_EDGE('',*,*,#54691,.T.);
#79520=ORIENTED_EDGE('',*,*,#54692,.F.);
#79521=ORIENTED_EDGE('',*,*,#54134,.T.);
#79522=ORIENTED_EDGE('',*,*,#54693,.F.);
#79523=ORIENTED_EDGE('',*,*,#54694,.T.);
#79524=ORIENTED_EDGE('',*,*,#54695,.F.);
#79525=ORIENTED_EDGE('',*,*,#54696,.T.);
#79526=ORIENTED_EDGE('',*,*,#54697,.F.);
#79527=ORIENTED_EDGE('',*,*,#54138,.T.);
#79528=ORIENTED_EDGE('',*,*,#54698,.F.);
#79529=ORIENTED_EDGE('',*,*,#54699,.T.);
#79530=ORIENTED_EDGE('',*,*,#54700,.F.);
#79531=ORIENTED_EDGE('',*,*,#54701,.T.);
#79532=ORIENTED_EDGE('',*,*,#54702,.F.);
#79533=ORIENTED_EDGE('',*,*,#54142,.T.);
#79534=ORIENTED_EDGE('',*,*,#54703,.F.);
#79535=ORIENTED_EDGE('',*,*,#54704,.T.);
#79536=ORIENTED_EDGE('',*,*,#54705,.F.);
#79537=ORIENTED_EDGE('',*,*,#54706,.T.);
#79538=ORIENTED_EDGE('',*,*,#54707,.F.);
#79539=ORIENTED_EDGE('',*,*,#54146,.T.);
#79540=ORIENTED_EDGE('',*,*,#54708,.F.);
#79541=ORIENTED_EDGE('',*,*,#54709,.T.);
#79542=ORIENTED_EDGE('',*,*,#54710,.F.);
#79543=ORIENTED_EDGE('',*,*,#54711,.T.);
#79544=ORIENTED_EDGE('',*,*,#54712,.F.);
#79545=ORIENTED_EDGE('',*,*,#54150,.T.);
#79546=ORIENTED_EDGE('',*,*,#54713,.F.);
#79547=ORIENTED_EDGE('',*,*,#54714,.T.);
#79548=ORIENTED_EDGE('',*,*,#54715,.F.);
#79549=ORIENTED_EDGE('',*,*,#54716,.T.);
#79550=ORIENTED_EDGE('',*,*,#54717,.F.);
#79551=ORIENTED_EDGE('',*,*,#54154,.T.);
#79552=ORIENTED_EDGE('',*,*,#54718,.F.);
#79553=ORIENTED_EDGE('',*,*,#54719,.T.);
#79554=ORIENTED_EDGE('',*,*,#54720,.F.);
#79555=ORIENTED_EDGE('',*,*,#54721,.T.);
#79556=ORIENTED_EDGE('',*,*,#54722,.F.);
#79557=ORIENTED_EDGE('',*,*,#54158,.T.);
#79558=ORIENTED_EDGE('',*,*,#54723,.F.);
#79559=ORIENTED_EDGE('',*,*,#54724,.T.);
#79560=ORIENTED_EDGE('',*,*,#54725,.F.);
#79561=ORIENTED_EDGE('',*,*,#54726,.T.);
#79562=ORIENTED_EDGE('',*,*,#54727,.F.);
#79563=ORIENTED_EDGE('',*,*,#54162,.T.);
#79564=ORIENTED_EDGE('',*,*,#54728,.F.);
#79565=ORIENTED_EDGE('',*,*,#54729,.T.);
#79566=ORIENTED_EDGE('',*,*,#54730,.F.);
#79567=ORIENTED_EDGE('',*,*,#54731,.T.);
#79568=ORIENTED_EDGE('',*,*,#54732,.F.);
#79569=ORIENTED_EDGE('',*,*,#54166,.T.);
#79570=ORIENTED_EDGE('',*,*,#54733,.F.);
#79571=ORIENTED_EDGE('',*,*,#54734,.T.);
#79572=ORIENTED_EDGE('',*,*,#54735,.F.);
#79573=ORIENTED_EDGE('',*,*,#54736,.T.);
#79574=ORIENTED_EDGE('',*,*,#54737,.F.);
#79575=ORIENTED_EDGE('',*,*,#54170,.T.);
#79576=ORIENTED_EDGE('',*,*,#54738,.F.);
#79577=ORIENTED_EDGE('',*,*,#54739,.T.);
#79578=ORIENTED_EDGE('',*,*,#54740,.F.);
#79579=ORIENTED_EDGE('',*,*,#54741,.T.);
#79580=ORIENTED_EDGE('',*,*,#54742,.F.);
#79581=ORIENTED_EDGE('',*,*,#54174,.T.);
#79582=ORIENTED_EDGE('',*,*,#54743,.F.);
#79583=ORIENTED_EDGE('',*,*,#54744,.T.);
#79584=ORIENTED_EDGE('',*,*,#54745,.F.);
#79585=ORIENTED_EDGE('',*,*,#54746,.T.);
#79586=ORIENTED_EDGE('',*,*,#54747,.F.);
#79587=ORIENTED_EDGE('',*,*,#54178,.T.);
#79588=ORIENTED_EDGE('',*,*,#54748,.F.);
#79589=ORIENTED_EDGE('',*,*,#54749,.T.);
#79590=ORIENTED_EDGE('',*,*,#54750,.F.);
#79591=ORIENTED_EDGE('',*,*,#54751,.T.);
#79592=ORIENTED_EDGE('',*,*,#54752,.F.);
#79593=ORIENTED_EDGE('',*,*,#54182,.T.);
#79594=ORIENTED_EDGE('',*,*,#54753,.F.);
#79595=ORIENTED_EDGE('',*,*,#54754,.T.);
#79596=ORIENTED_EDGE('',*,*,#54755,.F.);
#79597=ORIENTED_EDGE('',*,*,#54756,.T.);
#79598=ORIENTED_EDGE('',*,*,#54757,.F.);
#79599=ORIENTED_EDGE('',*,*,#54186,.T.);
#79600=ORIENTED_EDGE('',*,*,#54758,.F.);
#79601=ORIENTED_EDGE('',*,*,#54759,.T.);
#79602=ORIENTED_EDGE('',*,*,#54760,.F.);
#79603=ORIENTED_EDGE('',*,*,#54761,.T.);
#79604=ORIENTED_EDGE('',*,*,#54762,.F.);
#79605=ORIENTED_EDGE('',*,*,#54190,.T.);
#79606=ORIENTED_EDGE('',*,*,#54763,.F.);
#79607=ORIENTED_EDGE('',*,*,#54764,.T.);
#79608=ORIENTED_EDGE('',*,*,#54765,.F.);
#79609=ORIENTED_EDGE('',*,*,#54766,.T.);
#79610=ORIENTED_EDGE('',*,*,#54767,.F.);
#79611=ORIENTED_EDGE('',*,*,#54194,.T.);
#79612=ORIENTED_EDGE('',*,*,#54768,.F.);
#79613=ORIENTED_EDGE('',*,*,#54769,.T.);
#79614=ORIENTED_EDGE('',*,*,#54770,.F.);
#79615=ORIENTED_EDGE('',*,*,#54771,.T.);
#79616=ORIENTED_EDGE('',*,*,#54772,.F.);
#79617=ORIENTED_EDGE('',*,*,#54198,.T.);
#79618=ORIENTED_EDGE('',*,*,#54773,.F.);
#79619=ORIENTED_EDGE('',*,*,#54774,.T.);
#79620=ORIENTED_EDGE('',*,*,#54775,.F.);
#79621=ORIENTED_EDGE('',*,*,#54776,.T.);
#79622=ORIENTED_EDGE('',*,*,#54777,.F.);
#79623=ORIENTED_EDGE('',*,*,#54202,.T.);
#79624=ORIENTED_EDGE('',*,*,#54778,.F.);
#79625=ORIENTED_EDGE('',*,*,#54779,.T.);
#79626=ORIENTED_EDGE('',*,*,#54780,.F.);
#79627=ORIENTED_EDGE('',*,*,#54781,.T.);
#79628=ORIENTED_EDGE('',*,*,#54782,.F.);
#79629=ORIENTED_EDGE('',*,*,#54206,.T.);
#79630=ORIENTED_EDGE('',*,*,#54783,.F.);
#79631=ORIENTED_EDGE('',*,*,#54784,.T.);
#79632=ORIENTED_EDGE('',*,*,#54785,.F.);
#79633=ORIENTED_EDGE('',*,*,#54786,.T.);
#79634=ORIENTED_EDGE('',*,*,#54787,.F.);
#79635=ORIENTED_EDGE('',*,*,#54254,.T.);
#79636=ORIENTED_EDGE('',*,*,#54788,.F.);
#79637=ORIENTED_EDGE('',*,*,#54789,.T.);
#79638=ORIENTED_EDGE('',*,*,#54790,.F.);
#79639=ORIENTED_EDGE('',*,*,#54791,.T.);
#79640=ORIENTED_EDGE('',*,*,#54792,.F.);
#79641=ORIENTED_EDGE('',*,*,#54259,.T.);
#79642=ORIENTED_EDGE('',*,*,#54793,.T.);
#79643=ORIENTED_EDGE('',*,*,#54283,.T.);
#79644=ORIENTED_EDGE('',*,*,#54793,.F.);
#79645=ORIENTED_EDGE('',*,*,#54258,.T.);
#79646=ORIENTED_EDGE('',*,*,#54794,.F.);
#79647=ORIENTED_EDGE('',*,*,#54795,.T.);
#79648=ORIENTED_EDGE('',*,*,#54796,.F.);
#79649=ORIENTED_EDGE('',*,*,#54797,.T.);
#79650=ORIENTED_EDGE('',*,*,#54798,.F.);
#79651=ORIENTED_EDGE('',*,*,#54250,.T.);
#79652=ORIENTED_EDGE('',*,*,#54799,.F.);
#79653=ORIENTED_EDGE('',*,*,#54800,.T.);
#79654=ORIENTED_EDGE('',*,*,#54801,.F.);
#79655=ORIENTED_EDGE('',*,*,#54802,.T.);
#79656=ORIENTED_EDGE('',*,*,#54803,.F.);
#79657=ORIENTED_EDGE('',*,*,#54246,.T.);
#79658=ORIENTED_EDGE('',*,*,#54804,.F.);
#79659=ORIENTED_EDGE('',*,*,#54805,.T.);
#79660=ORIENTED_EDGE('',*,*,#54806,.F.);
#79661=ORIENTED_EDGE('',*,*,#54807,.T.);
#79662=ORIENTED_EDGE('',*,*,#54808,.F.);
#79663=ORIENTED_EDGE('',*,*,#54242,.T.);
#79664=ORIENTED_EDGE('',*,*,#54809,.F.);
#79665=ORIENTED_EDGE('',*,*,#54810,.T.);
#79666=ORIENTED_EDGE('',*,*,#54811,.F.);
#79667=ORIENTED_EDGE('',*,*,#54812,.T.);
#79668=ORIENTED_EDGE('',*,*,#54813,.F.);
#79669=ORIENTED_EDGE('',*,*,#54238,.T.);
#79670=ORIENTED_EDGE('',*,*,#54814,.F.);
#79671=ORIENTED_EDGE('',*,*,#54815,.T.);
#79672=ORIENTED_EDGE('',*,*,#54816,.F.);
#79673=ORIENTED_EDGE('',*,*,#54817,.T.);
#79674=ORIENTED_EDGE('',*,*,#54818,.F.);
#79675=ORIENTED_EDGE('',*,*,#54234,.T.);
#79676=ORIENTED_EDGE('',*,*,#54819,.F.);
#79677=ORIENTED_EDGE('',*,*,#54820,.T.);
#79678=ORIENTED_EDGE('',*,*,#54821,.F.);
#79679=ORIENTED_EDGE('',*,*,#54822,.T.);
#79680=ORIENTED_EDGE('',*,*,#54823,.F.);
#79681=ORIENTED_EDGE('',*,*,#54230,.T.);
#79682=ORIENTED_EDGE('',*,*,#54824,.F.);
#79683=ORIENTED_EDGE('',*,*,#54825,.T.);
#79684=ORIENTED_EDGE('',*,*,#54826,.F.);
#79685=ORIENTED_EDGE('',*,*,#54827,.T.);
#79686=ORIENTED_EDGE('',*,*,#54828,.F.);
#79687=ORIENTED_EDGE('',*,*,#54226,.T.);
#79688=ORIENTED_EDGE('',*,*,#54829,.F.);
#79689=ORIENTED_EDGE('',*,*,#54830,.T.);
#79690=ORIENTED_EDGE('',*,*,#54831,.F.);
#79691=ORIENTED_EDGE('',*,*,#54832,.T.);
#79692=ORIENTED_EDGE('',*,*,#54833,.F.);
#79693=ORIENTED_EDGE('',*,*,#54222,.T.);
#79694=ORIENTED_EDGE('',*,*,#54834,.F.);
#79695=ORIENTED_EDGE('',*,*,#54835,.T.);
#79696=ORIENTED_EDGE('',*,*,#54836,.F.);
#79697=ORIENTED_EDGE('',*,*,#54837,.T.);
#79698=ORIENTED_EDGE('',*,*,#54838,.F.);
#79699=ORIENTED_EDGE('',*,*,#54218,.T.);
#79700=ORIENTED_EDGE('',*,*,#54839,.F.);
#79701=ORIENTED_EDGE('',*,*,#54840,.T.);
#79702=ORIENTED_EDGE('',*,*,#54841,.F.);
#79703=ORIENTED_EDGE('',*,*,#54842,.T.);
#79704=ORIENTED_EDGE('',*,*,#54843,.F.);
#79705=ORIENTED_EDGE('',*,*,#54214,.T.);
#79706=ORIENTED_EDGE('',*,*,#54844,.F.);
#79707=ORIENTED_EDGE('',*,*,#54845,.T.);
#79708=ORIENTED_EDGE('',*,*,#54846,.F.);
#79709=ORIENTED_EDGE('',*,*,#54847,.T.);
#79710=ORIENTED_EDGE('',*,*,#54848,.F.);
#79711=ORIENTED_EDGE('',*,*,#54210,.T.);
#79712=ORIENTED_EDGE('',*,*,#54849,.F.);
#79713=ORIENTED_EDGE('',*,*,#54850,.T.);
#79714=ORIENTED_EDGE('',*,*,#54851,.F.);
#79715=ORIENTED_EDGE('',*,*,#54852,.T.);
#79716=ORIENTED_EDGE('',*,*,#54853,.F.);
#79717=ORIENTED_EDGE('',*,*,#53954,.T.);
#79718=ORIENTED_EDGE('',*,*,#54854,.F.);
#79719=ORIENTED_EDGE('',*,*,#54855,.T.);
#79720=ORIENTED_EDGE('',*,*,#54856,.F.);
#79721=ORIENTED_EDGE('',*,*,#54857,.T.);
#79722=ORIENTED_EDGE('',*,*,#54858,.F.);
#79723=ORIENTED_EDGE('',*,*,#53958,.T.);
#79724=ORIENTED_EDGE('',*,*,#54859,.F.);
#79725=ORIENTED_EDGE('',*,*,#54860,.T.);
#79726=ORIENTED_EDGE('',*,*,#54861,.F.);
#79727=ORIENTED_EDGE('',*,*,#54862,.T.);
#79728=ORIENTED_EDGE('',*,*,#54863,.F.);
#79729=ORIENTED_EDGE('',*,*,#53962,.T.);
#79730=ORIENTED_EDGE('',*,*,#54864,.F.);
#79731=ORIENTED_EDGE('',*,*,#54865,.T.);
#79732=ORIENTED_EDGE('',*,*,#54866,.F.);
#79733=ORIENTED_EDGE('',*,*,#54867,.T.);
#79734=ORIENTED_EDGE('',*,*,#54868,.F.);
#79735=ORIENTED_EDGE('',*,*,#53966,.T.);
#79736=ORIENTED_EDGE('',*,*,#54869,.F.);
#79737=ORIENTED_EDGE('',*,*,#54870,.T.);
#79738=ORIENTED_EDGE('',*,*,#54871,.F.);
#79739=ORIENTED_EDGE('',*,*,#54872,.T.);
#79740=ORIENTED_EDGE('',*,*,#54873,.F.);
#79741=ORIENTED_EDGE('',*,*,#53970,.T.);
#79742=ORIENTED_EDGE('',*,*,#54874,.F.);
#79743=ORIENTED_EDGE('',*,*,#54875,.T.);
#79744=ORIENTED_EDGE('',*,*,#54876,.F.);
#79745=ORIENTED_EDGE('',*,*,#54877,.T.);
#79746=ORIENTED_EDGE('',*,*,#54878,.F.);
#79747=ORIENTED_EDGE('',*,*,#53974,.T.);
#79748=ORIENTED_EDGE('',*,*,#54879,.F.);
#79749=ORIENTED_EDGE('',*,*,#54880,.T.);
#79750=ORIENTED_EDGE('',*,*,#54881,.F.);
#79751=ORIENTED_EDGE('',*,*,#54882,.T.);
#79752=ORIENTED_EDGE('',*,*,#54883,.F.);
#79753=ORIENTED_EDGE('',*,*,#53978,.T.);
#79754=ORIENTED_EDGE('',*,*,#54884,.F.);
#79755=ORIENTED_EDGE('',*,*,#54885,.T.);
#79756=ORIENTED_EDGE('',*,*,#54886,.F.);
#79757=ORIENTED_EDGE('',*,*,#54887,.T.);
#79758=ORIENTED_EDGE('',*,*,#54888,.F.);
#79759=ORIENTED_EDGE('',*,*,#53982,.T.);
#79760=ORIENTED_EDGE('',*,*,#54889,.F.);
#79761=ORIENTED_EDGE('',*,*,#54890,.T.);
#79762=ORIENTED_EDGE('',*,*,#54891,.F.);
#79763=ORIENTED_EDGE('',*,*,#54892,.T.);
#79764=ORIENTED_EDGE('',*,*,#54893,.F.);
#79765=ORIENTED_EDGE('',*,*,#53986,.T.);
#79766=ORIENTED_EDGE('',*,*,#54894,.F.);
#79767=ORIENTED_EDGE('',*,*,#54895,.T.);
#79768=ORIENTED_EDGE('',*,*,#54896,.F.);
#79769=ORIENTED_EDGE('',*,*,#54897,.T.);
#79770=ORIENTED_EDGE('',*,*,#54898,.F.);
#79771=ORIENTED_EDGE('',*,*,#53990,.T.);
#79772=ORIENTED_EDGE('',*,*,#54899,.F.);
#79773=ORIENTED_EDGE('',*,*,#54900,.T.);
#79774=ORIENTED_EDGE('',*,*,#54901,.F.);
#79775=ORIENTED_EDGE('',*,*,#54902,.T.);
#79776=ORIENTED_EDGE('',*,*,#54903,.F.);
#79777=ORIENTED_EDGE('',*,*,#53994,.T.);
#79778=ORIENTED_EDGE('',*,*,#54904,.F.);
#79779=ORIENTED_EDGE('',*,*,#54905,.T.);
#79780=ORIENTED_EDGE('',*,*,#54906,.F.);
#79781=ORIENTED_EDGE('',*,*,#54907,.T.);
#79782=ORIENTED_EDGE('',*,*,#54908,.F.);
#79783=ORIENTED_EDGE('',*,*,#53998,.T.);
#79784=ORIENTED_EDGE('',*,*,#54909,.F.);
#79785=ORIENTED_EDGE('',*,*,#54910,.T.);
#79786=ORIENTED_EDGE('',*,*,#54911,.F.);
#79787=ORIENTED_EDGE('',*,*,#54912,.T.);
#79788=ORIENTED_EDGE('',*,*,#54913,.F.);
#79789=ORIENTED_EDGE('',*,*,#54002,.T.);
#79790=ORIENTED_EDGE('',*,*,#54914,.F.);
#79791=ORIENTED_EDGE('',*,*,#54915,.T.);
#79792=ORIENTED_EDGE('',*,*,#54916,.F.);
#79793=ORIENTED_EDGE('',*,*,#54917,.T.);
#79794=ORIENTED_EDGE('',*,*,#54918,.F.);
#79795=ORIENTED_EDGE('',*,*,#54006,.T.);
#79796=ORIENTED_EDGE('',*,*,#54919,.F.);
#79797=ORIENTED_EDGE('',*,*,#54920,.T.);
#79798=ORIENTED_EDGE('',*,*,#54921,.F.);
#79799=ORIENTED_EDGE('',*,*,#54922,.T.);
#79800=ORIENTED_EDGE('',*,*,#54923,.F.);
#79801=ORIENTED_EDGE('',*,*,#54010,.T.);
#79802=ORIENTED_EDGE('',*,*,#54924,.F.);
#79803=ORIENTED_EDGE('',*,*,#54925,.T.);
#79804=ORIENTED_EDGE('',*,*,#54926,.F.);
#79805=ORIENTED_EDGE('',*,*,#54927,.T.);
#79806=ORIENTED_EDGE('',*,*,#54928,.F.);
#79807=ORIENTED_EDGE('',*,*,#54014,.T.);
#79808=ORIENTED_EDGE('',*,*,#54929,.F.);
#79809=ORIENTED_EDGE('',*,*,#54930,.T.);
#79810=ORIENTED_EDGE('',*,*,#54931,.F.);
#79811=ORIENTED_EDGE('',*,*,#54932,.T.);
#79812=ORIENTED_EDGE('',*,*,#54933,.F.);
#79813=ORIENTED_EDGE('',*,*,#54018,.T.);
#79814=ORIENTED_EDGE('',*,*,#54934,.F.);
#79815=ORIENTED_EDGE('',*,*,#54935,.T.);
#79816=ORIENTED_EDGE('',*,*,#54936,.F.);
#79817=ORIENTED_EDGE('',*,*,#54937,.T.);
#79818=ORIENTED_EDGE('',*,*,#54938,.F.);
#79819=ORIENTED_EDGE('',*,*,#54022,.T.);
#79820=ORIENTED_EDGE('',*,*,#54939,.F.);
#79821=ORIENTED_EDGE('',*,*,#54940,.T.);
#79822=ORIENTED_EDGE('',*,*,#54941,.F.);
#79823=ORIENTED_EDGE('',*,*,#54942,.T.);
#79824=ORIENTED_EDGE('',*,*,#54943,.F.);
#79825=ORIENTED_EDGE('',*,*,#54026,.T.);
#79826=ORIENTED_EDGE('',*,*,#54944,.F.);
#79827=ORIENTED_EDGE('',*,*,#54945,.T.);
#79828=ORIENTED_EDGE('',*,*,#54946,.F.);
#79829=ORIENTED_EDGE('',*,*,#54947,.T.);
#79830=ORIENTED_EDGE('',*,*,#54948,.F.);
#79831=ORIENTED_EDGE('',*,*,#54030,.T.);
#79832=ORIENTED_EDGE('',*,*,#54949,.F.);
#79833=ORIENTED_EDGE('',*,*,#54950,.T.);
#79834=ORIENTED_EDGE('',*,*,#54951,.F.);
#79835=ORIENTED_EDGE('',*,*,#54952,.T.);
#79836=ORIENTED_EDGE('',*,*,#54953,.F.);
#79837=ORIENTED_EDGE('',*,*,#54034,.T.);
#79838=ORIENTED_EDGE('',*,*,#54954,.F.);
#79839=ORIENTED_EDGE('',*,*,#54955,.T.);
#79840=ORIENTED_EDGE('',*,*,#54956,.F.);
#79841=ORIENTED_EDGE('',*,*,#54957,.T.);
#79842=ORIENTED_EDGE('',*,*,#54958,.F.);
#79843=ORIENTED_EDGE('',*,*,#54038,.T.);
#79844=ORIENTED_EDGE('',*,*,#54959,.F.);
#79845=ORIENTED_EDGE('',*,*,#54960,.T.);
#79846=ORIENTED_EDGE('',*,*,#54961,.F.);
#79847=ORIENTED_EDGE('',*,*,#54962,.T.);
#79848=ORIENTED_EDGE('',*,*,#54963,.F.);
#79849=ORIENTED_EDGE('',*,*,#54042,.T.);
#79850=ORIENTED_EDGE('',*,*,#54964,.F.);
#79851=ORIENTED_EDGE('',*,*,#54965,.T.);
#79852=ORIENTED_EDGE('',*,*,#54966,.F.);
#79853=ORIENTED_EDGE('',*,*,#54967,.T.);
#79854=ORIENTED_EDGE('',*,*,#54968,.F.);
#79855=ORIENTED_EDGE('',*,*,#54046,.T.);
#79856=ORIENTED_EDGE('',*,*,#54969,.F.);
#79857=ORIENTED_EDGE('',*,*,#54970,.T.);
#79858=ORIENTED_EDGE('',*,*,#54971,.F.);
#79859=ORIENTED_EDGE('',*,*,#54972,.T.);
#79860=ORIENTED_EDGE('',*,*,#54973,.F.);
#79861=ORIENTED_EDGE('',*,*,#54050,.T.);
#79862=ORIENTED_EDGE('',*,*,#54974,.F.);
#79863=ORIENTED_EDGE('',*,*,#54975,.T.);
#79864=ORIENTED_EDGE('',*,*,#54976,.F.);
#79865=ORIENTED_EDGE('',*,*,#54977,.T.);
#79866=ORIENTED_EDGE('',*,*,#54978,.F.);
#79867=ORIENTED_EDGE('',*,*,#54054,.T.);
#79868=ORIENTED_EDGE('',*,*,#54979,.F.);
#79869=ORIENTED_EDGE('',*,*,#54980,.T.);
#79870=ORIENTED_EDGE('',*,*,#54981,.F.);
#79871=ORIENTED_EDGE('',*,*,#54982,.T.);
#79872=ORIENTED_EDGE('',*,*,#54983,.F.);
#79873=ORIENTED_EDGE('',*,*,#54058,.T.);
#79874=ORIENTED_EDGE('',*,*,#54984,.F.);
#79875=ORIENTED_EDGE('',*,*,#54985,.T.);
#79876=ORIENTED_EDGE('',*,*,#54600,.T.);
#79877=ORIENTED_EDGE('',*,*,#54986,.T.);
#79878=ORIENTED_EDGE('',*,*,#54443,.F.);
#79879=ORIENTED_EDGE('',*,*,#54439,.F.);
#79880=ORIENTED_EDGE('',*,*,#54987,.T.);
#79881=ORIENTED_EDGE('',*,*,#54551,.F.);
#79882=ORIENTED_EDGE('',*,*,#54988,.T.);
#79883=ORIENTED_EDGE('',*,*,#54851,.T.);
#79884=ORIENTED_EDGE('',*,*,#54989,.T.);
#79885=ORIENTED_EDGE('',*,*,#54856,.T.);
#79886=ORIENTED_EDGE('',*,*,#54990,.T.);
#79887=ORIENTED_EDGE('',*,*,#54547,.F.);
#79888=ORIENTED_EDGE('',*,*,#54991,.T.);
#79889=ORIENTED_EDGE('',*,*,#54861,.T.);
#79890=ORIENTED_EDGE('',*,*,#54992,.T.);
#79891=ORIENTED_EDGE('',*,*,#54543,.F.);
#79892=ORIENTED_EDGE('',*,*,#54993,.T.);
#79893=ORIENTED_EDGE('',*,*,#54866,.T.);
#79894=ORIENTED_EDGE('',*,*,#54994,.T.);
#79895=ORIENTED_EDGE('',*,*,#54539,.F.);
#79896=ORIENTED_EDGE('',*,*,#54995,.T.);
#79897=ORIENTED_EDGE('',*,*,#54871,.T.);
#79898=ORIENTED_EDGE('',*,*,#54996,.T.);
#79899=ORIENTED_EDGE('',*,*,#54535,.F.);
#79900=ORIENTED_EDGE('',*,*,#54997,.T.);
#79901=ORIENTED_EDGE('',*,*,#54876,.T.);
#79902=ORIENTED_EDGE('',*,*,#54998,.T.);
#79903=ORIENTED_EDGE('',*,*,#54531,.F.);
#79904=ORIENTED_EDGE('',*,*,#54999,.T.);
#79905=ORIENTED_EDGE('',*,*,#54881,.T.);
#79906=ORIENTED_EDGE('',*,*,#55000,.T.);
#79907=ORIENTED_EDGE('',*,*,#54527,.F.);
#79908=ORIENTED_EDGE('',*,*,#55001,.T.);
#79909=ORIENTED_EDGE('',*,*,#54886,.T.);
#79910=ORIENTED_EDGE('',*,*,#55002,.T.);
#79911=ORIENTED_EDGE('',*,*,#54523,.F.);
#79912=ORIENTED_EDGE('',*,*,#55003,.T.);
#79913=ORIENTED_EDGE('',*,*,#54891,.T.);
#79914=ORIENTED_EDGE('',*,*,#55004,.T.);
#79915=ORIENTED_EDGE('',*,*,#54519,.F.);
#79916=ORIENTED_EDGE('',*,*,#55005,.T.);
#79917=ORIENTED_EDGE('',*,*,#54896,.T.);
#79918=ORIENTED_EDGE('',*,*,#55006,.T.);
#79919=ORIENTED_EDGE('',*,*,#54515,.F.);
#79920=ORIENTED_EDGE('',*,*,#55007,.T.);
#79921=ORIENTED_EDGE('',*,*,#54901,.T.);
#79922=ORIENTED_EDGE('',*,*,#55008,.T.);
#79923=ORIENTED_EDGE('',*,*,#54511,.F.);
#79924=ORIENTED_EDGE('',*,*,#55009,.T.);
#79925=ORIENTED_EDGE('',*,*,#54906,.T.);
#79926=ORIENTED_EDGE('',*,*,#55010,.T.);
#79927=ORIENTED_EDGE('',*,*,#54507,.F.);
#79928=ORIENTED_EDGE('',*,*,#55011,.T.);
#79929=ORIENTED_EDGE('',*,*,#54911,.T.);
#79930=ORIENTED_EDGE('',*,*,#55012,.T.);
#79931=ORIENTED_EDGE('',*,*,#54503,.F.);
#79932=ORIENTED_EDGE('',*,*,#55013,.T.);
#79933=ORIENTED_EDGE('',*,*,#54916,.T.);
#79934=ORIENTED_EDGE('',*,*,#55014,.T.);
#79935=ORIENTED_EDGE('',*,*,#54499,.F.);
#79936=ORIENTED_EDGE('',*,*,#55015,.T.);
#79937=ORIENTED_EDGE('',*,*,#54921,.T.);
#79938=ORIENTED_EDGE('',*,*,#55016,.T.);
#79939=ORIENTED_EDGE('',*,*,#54495,.F.);
#79940=ORIENTED_EDGE('',*,*,#55017,.T.);
#79941=ORIENTED_EDGE('',*,*,#54926,.T.);
#79942=ORIENTED_EDGE('',*,*,#55018,.T.);
#79943=ORIENTED_EDGE('',*,*,#54491,.F.);
#79944=ORIENTED_EDGE('',*,*,#55019,.T.);
#79945=ORIENTED_EDGE('',*,*,#54931,.T.);
#79946=ORIENTED_EDGE('',*,*,#55020,.T.);
#79947=ORIENTED_EDGE('',*,*,#54487,.F.);
#79948=ORIENTED_EDGE('',*,*,#55021,.T.);
#79949=ORIENTED_EDGE('',*,*,#54936,.T.);
#79950=ORIENTED_EDGE('',*,*,#55022,.T.);
#79951=ORIENTED_EDGE('',*,*,#54483,.F.);
#79952=ORIENTED_EDGE('',*,*,#55023,.T.);
#79953=ORIENTED_EDGE('',*,*,#54941,.T.);
#79954=ORIENTED_EDGE('',*,*,#55024,.T.);
#79955=ORIENTED_EDGE('',*,*,#54479,.F.);
#79956=ORIENTED_EDGE('',*,*,#55025,.T.);
#79957=ORIENTED_EDGE('',*,*,#54946,.T.);
#79958=ORIENTED_EDGE('',*,*,#55026,.T.);
#79959=ORIENTED_EDGE('',*,*,#54475,.F.);
#79960=ORIENTED_EDGE('',*,*,#55027,.T.);
#79961=ORIENTED_EDGE('',*,*,#54951,.T.);
#79962=ORIENTED_EDGE('',*,*,#55028,.T.);
#79963=ORIENTED_EDGE('',*,*,#54471,.F.);
#79964=ORIENTED_EDGE('',*,*,#55029,.T.);
#79965=ORIENTED_EDGE('',*,*,#54956,.T.);
#79966=ORIENTED_EDGE('',*,*,#55030,.T.);
#79967=ORIENTED_EDGE('',*,*,#54467,.F.);
#79968=ORIENTED_EDGE('',*,*,#55031,.T.);
#79969=ORIENTED_EDGE('',*,*,#54961,.T.);
#79970=ORIENTED_EDGE('',*,*,#55032,.T.);
#79971=ORIENTED_EDGE('',*,*,#54463,.F.);
#79972=ORIENTED_EDGE('',*,*,#55033,.T.);
#79973=ORIENTED_EDGE('',*,*,#54966,.T.);
#79974=ORIENTED_EDGE('',*,*,#55034,.T.);
#79975=ORIENTED_EDGE('',*,*,#54459,.F.);
#79976=ORIENTED_EDGE('',*,*,#55035,.T.);
#79977=ORIENTED_EDGE('',*,*,#54971,.T.);
#79978=ORIENTED_EDGE('',*,*,#55036,.T.);
#79979=ORIENTED_EDGE('',*,*,#54455,.F.);
#79980=ORIENTED_EDGE('',*,*,#55037,.T.);
#79981=ORIENTED_EDGE('',*,*,#54976,.T.);
#79982=ORIENTED_EDGE('',*,*,#55038,.T.);
#79983=ORIENTED_EDGE('',*,*,#54451,.F.);
#79984=ORIENTED_EDGE('',*,*,#55039,.T.);
#79985=ORIENTED_EDGE('',*,*,#54981,.T.);
#79986=ORIENTED_EDGE('',*,*,#55040,.T.);
#79987=ORIENTED_EDGE('',*,*,#54447,.F.);
#79988=ORIENTED_EDGE('',*,*,#55041,.T.);
#79989=ORIENTED_EDGE('',*,*,#54605,.T.);
#79990=ORIENTED_EDGE('',*,*,#55042,.T.);
#79991=ORIENTED_EDGE('',*,*,#54435,.F.);
#79992=ORIENTED_EDGE('',*,*,#55043,.T.);
#79993=ORIENTED_EDGE('',*,*,#54610,.T.);
#79994=ORIENTED_EDGE('',*,*,#55044,.T.);
#79995=ORIENTED_EDGE('',*,*,#54431,.F.);
#79996=ORIENTED_EDGE('',*,*,#55045,.T.);
#79997=ORIENTED_EDGE('',*,*,#54615,.T.);
#79998=ORIENTED_EDGE('',*,*,#55046,.T.);
#79999=ORIENTED_EDGE('',*,*,#54427,.F.);
#80000=ORIENTED_EDGE('',*,*,#55047,.T.);
#80001=ORIENTED_EDGE('',*,*,#54620,.T.);
#80002=ORIENTED_EDGE('',*,*,#55048,.T.);
#80003=ORIENTED_EDGE('',*,*,#54423,.F.);
#80004=ORIENTED_EDGE('',*,*,#55049,.T.);
#80005=ORIENTED_EDGE('',*,*,#54625,.T.);
#80006=ORIENTED_EDGE('',*,*,#55050,.T.);
#80007=ORIENTED_EDGE('',*,*,#54419,.F.);
#80008=ORIENTED_EDGE('',*,*,#55051,.T.);
#80009=ORIENTED_EDGE('',*,*,#54630,.T.);
#80010=ORIENTED_EDGE('',*,*,#55052,.T.);
#80011=ORIENTED_EDGE('',*,*,#54415,.F.);
#80012=ORIENTED_EDGE('',*,*,#55053,.T.);
#80013=ORIENTED_EDGE('',*,*,#54635,.T.);
#80014=ORIENTED_EDGE('',*,*,#55054,.T.);
#80015=ORIENTED_EDGE('',*,*,#54411,.F.);
#80016=ORIENTED_EDGE('',*,*,#55055,.T.);
#80017=ORIENTED_EDGE('',*,*,#54640,.T.);
#80018=ORIENTED_EDGE('',*,*,#55056,.T.);
#80019=ORIENTED_EDGE('',*,*,#54407,.F.);
#80020=ORIENTED_EDGE('',*,*,#55057,.T.);
#80021=ORIENTED_EDGE('',*,*,#54645,.T.);
#80022=ORIENTED_EDGE('',*,*,#55058,.T.);
#80023=ORIENTED_EDGE('',*,*,#54403,.F.);
#80024=ORIENTED_EDGE('',*,*,#55059,.T.);
#80025=ORIENTED_EDGE('',*,*,#54650,.T.);
#80026=ORIENTED_EDGE('',*,*,#55060,.T.);
#80027=ORIENTED_EDGE('',*,*,#54399,.F.);
#80028=ORIENTED_EDGE('',*,*,#55061,.T.);
#80029=ORIENTED_EDGE('',*,*,#54655,.T.);
#80030=ORIENTED_EDGE('',*,*,#55062,.T.);
#80031=ORIENTED_EDGE('',*,*,#54395,.F.);
#80032=ORIENTED_EDGE('',*,*,#55063,.T.);
#80033=ORIENTED_EDGE('',*,*,#54660,.T.);
#80034=ORIENTED_EDGE('',*,*,#55064,.T.);
#80035=ORIENTED_EDGE('',*,*,#54391,.F.);
#80036=ORIENTED_EDGE('',*,*,#55065,.T.);
#80037=ORIENTED_EDGE('',*,*,#54665,.T.);
#80038=ORIENTED_EDGE('',*,*,#55066,.T.);
#80039=ORIENTED_EDGE('',*,*,#54387,.F.);
#80040=ORIENTED_EDGE('',*,*,#55067,.T.);
#80041=ORIENTED_EDGE('',*,*,#54670,.T.);
#80042=ORIENTED_EDGE('',*,*,#55068,.T.);
#80043=ORIENTED_EDGE('',*,*,#54383,.F.);
#80044=ORIENTED_EDGE('',*,*,#55069,.T.);
#80045=ORIENTED_EDGE('',*,*,#54675,.T.);
#80046=ORIENTED_EDGE('',*,*,#55070,.T.);
#80047=ORIENTED_EDGE('',*,*,#54379,.F.);
#80048=ORIENTED_EDGE('',*,*,#55071,.T.);
#80049=ORIENTED_EDGE('',*,*,#54680,.T.);
#80050=ORIENTED_EDGE('',*,*,#55072,.T.);
#80051=ORIENTED_EDGE('',*,*,#54375,.F.);
#80052=ORIENTED_EDGE('',*,*,#55073,.T.);
#80053=ORIENTED_EDGE('',*,*,#54685,.T.);
#80054=ORIENTED_EDGE('',*,*,#55074,.T.);
#80055=ORIENTED_EDGE('',*,*,#54371,.F.);
#80056=ORIENTED_EDGE('',*,*,#55075,.T.);
#80057=ORIENTED_EDGE('',*,*,#54690,.T.);
#80058=ORIENTED_EDGE('',*,*,#55076,.T.);
#80059=ORIENTED_EDGE('',*,*,#54367,.F.);
#80060=ORIENTED_EDGE('',*,*,#55077,.T.);
#80061=ORIENTED_EDGE('',*,*,#54695,.T.);
#80062=ORIENTED_EDGE('',*,*,#55078,.T.);
#80063=ORIENTED_EDGE('',*,*,#54363,.F.);
#80064=ORIENTED_EDGE('',*,*,#55079,.T.);
#80065=ORIENTED_EDGE('',*,*,#54700,.T.);
#80066=ORIENTED_EDGE('',*,*,#55080,.T.);
#80067=ORIENTED_EDGE('',*,*,#54359,.F.);
#80068=ORIENTED_EDGE('',*,*,#55081,.T.);
#80069=ORIENTED_EDGE('',*,*,#54705,.T.);
#80070=ORIENTED_EDGE('',*,*,#55082,.T.);
#80071=ORIENTED_EDGE('',*,*,#54355,.F.);
#80072=ORIENTED_EDGE('',*,*,#55083,.T.);
#80073=ORIENTED_EDGE('',*,*,#54710,.T.);
#80074=ORIENTED_EDGE('',*,*,#55084,.T.);
#80075=ORIENTED_EDGE('',*,*,#54351,.F.);
#80076=ORIENTED_EDGE('',*,*,#55085,.T.);
#80077=ORIENTED_EDGE('',*,*,#54715,.T.);
#80078=ORIENTED_EDGE('',*,*,#55086,.T.);
#80079=ORIENTED_EDGE('',*,*,#54347,.F.);
#80080=ORIENTED_EDGE('',*,*,#55087,.T.);
#80081=ORIENTED_EDGE('',*,*,#54720,.T.);
#80082=ORIENTED_EDGE('',*,*,#55088,.T.);
#80083=ORIENTED_EDGE('',*,*,#54343,.F.);
#80084=ORIENTED_EDGE('',*,*,#55089,.T.);
#80085=ORIENTED_EDGE('',*,*,#54725,.T.);
#80086=ORIENTED_EDGE('',*,*,#55090,.T.);
#80087=ORIENTED_EDGE('',*,*,#54339,.F.);
#80088=ORIENTED_EDGE('',*,*,#55091,.T.);
#80089=ORIENTED_EDGE('',*,*,#54730,.T.);
#80090=ORIENTED_EDGE('',*,*,#55092,.T.);
#80091=ORIENTED_EDGE('',*,*,#54335,.F.);
#80092=ORIENTED_EDGE('',*,*,#55093,.T.);
#80093=ORIENTED_EDGE('',*,*,#54735,.T.);
#80094=ORIENTED_EDGE('',*,*,#55094,.T.);
#80095=ORIENTED_EDGE('',*,*,#54331,.F.);
#80096=ORIENTED_EDGE('',*,*,#55095,.T.);
#80097=ORIENTED_EDGE('',*,*,#54740,.T.);
#80098=ORIENTED_EDGE('',*,*,#55096,.T.);
#80099=ORIENTED_EDGE('',*,*,#54327,.F.);
#80100=ORIENTED_EDGE('',*,*,#55097,.T.);
#80101=ORIENTED_EDGE('',*,*,#54745,.T.);
#80102=ORIENTED_EDGE('',*,*,#55098,.T.);
#80103=ORIENTED_EDGE('',*,*,#54323,.F.);
#80104=ORIENTED_EDGE('',*,*,#55099,.T.);
#80105=ORIENTED_EDGE('',*,*,#54750,.T.);
#80106=ORIENTED_EDGE('',*,*,#55100,.T.);
#80107=ORIENTED_EDGE('',*,*,#54319,.F.);
#80108=ORIENTED_EDGE('',*,*,#55101,.T.);
#80109=ORIENTED_EDGE('',*,*,#54755,.T.);
#80110=ORIENTED_EDGE('',*,*,#55102,.T.);
#80111=ORIENTED_EDGE('',*,*,#54315,.F.);
#80112=ORIENTED_EDGE('',*,*,#55103,.T.);
#80113=ORIENTED_EDGE('',*,*,#54760,.T.);
#80114=ORIENTED_EDGE('',*,*,#55104,.T.);
#80115=ORIENTED_EDGE('',*,*,#54311,.F.);
#80116=ORIENTED_EDGE('',*,*,#55105,.T.);
#80117=ORIENTED_EDGE('',*,*,#54765,.T.);
#80118=ORIENTED_EDGE('',*,*,#55106,.T.);
#80119=ORIENTED_EDGE('',*,*,#54307,.F.);
#80120=ORIENTED_EDGE('',*,*,#55107,.T.);
#80121=ORIENTED_EDGE('',*,*,#54770,.T.);
#80122=ORIENTED_EDGE('',*,*,#55108,.T.);
#80123=ORIENTED_EDGE('',*,*,#54303,.F.);
#80124=ORIENTED_EDGE('',*,*,#55109,.T.);
#80125=ORIENTED_EDGE('',*,*,#54775,.T.);
#80126=ORIENTED_EDGE('',*,*,#55110,.T.);
#80127=ORIENTED_EDGE('',*,*,#54299,.F.);
#80128=ORIENTED_EDGE('',*,*,#55111,.T.);
#80129=ORIENTED_EDGE('',*,*,#54780,.T.);
#80130=ORIENTED_EDGE('',*,*,#55112,.T.);
#80131=ORIENTED_EDGE('',*,*,#54295,.F.);
#80132=ORIENTED_EDGE('',*,*,#55113,.T.);
#80133=ORIENTED_EDGE('',*,*,#54555,.F.);
#80134=ORIENTED_EDGE('',*,*,#55114,.T.);
#80135=ORIENTED_EDGE('',*,*,#54846,.T.);
#80136=ORIENTED_EDGE('',*,*,#55115,.T.);
#80137=ORIENTED_EDGE('',*,*,#54559,.F.);
#80138=ORIENTED_EDGE('',*,*,#55116,.T.);
#80139=ORIENTED_EDGE('',*,*,#54841,.T.);
#80140=ORIENTED_EDGE('',*,*,#55117,.T.);
#80141=ORIENTED_EDGE('',*,*,#54563,.F.);
#80142=ORIENTED_EDGE('',*,*,#55118,.T.);
#80143=ORIENTED_EDGE('',*,*,#54836,.T.);
#80144=ORIENTED_EDGE('',*,*,#55119,.T.);
#80145=ORIENTED_EDGE('',*,*,#54567,.F.);
#80146=ORIENTED_EDGE('',*,*,#55120,.T.);
#80147=ORIENTED_EDGE('',*,*,#54831,.T.);
#80148=ORIENTED_EDGE('',*,*,#55121,.T.);
#80149=ORIENTED_EDGE('',*,*,#54571,.F.);
#80150=ORIENTED_EDGE('',*,*,#55122,.T.);
#80151=ORIENTED_EDGE('',*,*,#54826,.T.);
#80152=ORIENTED_EDGE('',*,*,#55123,.T.);
#80153=ORIENTED_EDGE('',*,*,#54575,.F.);
#80154=ORIENTED_EDGE('',*,*,#55124,.T.);
#80155=ORIENTED_EDGE('',*,*,#54821,.T.);
#80156=ORIENTED_EDGE('',*,*,#55125,.T.);
#80157=ORIENTED_EDGE('',*,*,#54579,.F.);
#80158=ORIENTED_EDGE('',*,*,#55126,.T.);
#80159=ORIENTED_EDGE('',*,*,#54816,.T.);
#80160=ORIENTED_EDGE('',*,*,#55127,.T.);
#80161=ORIENTED_EDGE('',*,*,#54583,.F.);
#80162=ORIENTED_EDGE('',*,*,#55128,.T.);
#80163=ORIENTED_EDGE('',*,*,#54811,.T.);
#80164=ORIENTED_EDGE('',*,*,#55129,.T.);
#80165=ORIENTED_EDGE('',*,*,#54587,.F.);
#80166=ORIENTED_EDGE('',*,*,#55130,.T.);
#80167=ORIENTED_EDGE('',*,*,#54806,.T.);
#80168=ORIENTED_EDGE('',*,*,#55131,.T.);
#80169=ORIENTED_EDGE('',*,*,#54591,.F.);
#80170=ORIENTED_EDGE('',*,*,#55132,.T.);
#80171=ORIENTED_EDGE('',*,*,#54801,.T.);
#80172=ORIENTED_EDGE('',*,*,#55133,.T.);
#80173=ORIENTED_EDGE('',*,*,#54595,.F.);
#80174=ORIENTED_EDGE('',*,*,#55134,.T.);
#80175=ORIENTED_EDGE('',*,*,#54796,.T.);
#80176=ORIENTED_EDGE('',*,*,#55135,.T.);
#80177=ORIENTED_EDGE('',*,*,#54785,.T.);
#80178=ORIENTED_EDGE('',*,*,#55136,.T.);
#80179=ORIENTED_EDGE('',*,*,#54291,.F.);
#80180=ORIENTED_EDGE('',*,*,#55137,.T.);
#80181=ORIENTED_EDGE('',*,*,#55138,.T.);
#80182=ORIENTED_EDGE('',*,*,#55139,.T.);
#80183=ORIENTED_EDGE('',*,*,#55140,.T.);
#80184=ORIENTED_EDGE('',*,*,#55141,.F.);
#80185=ORIENTED_EDGE('',*,*,#55142,.T.);
#80186=ORIENTED_EDGE('',*,*,#55143,.T.);
#80187=ORIENTED_EDGE('',*,*,#55144,.T.);
#80188=ORIENTED_EDGE('',*,*,#55145,.T.);
#80189=ORIENTED_EDGE('',*,*,#55138,.F.);
#80190=ORIENTED_EDGE('',*,*,#55146,.T.);
#80191=ORIENTED_EDGE('',*,*,#55147,.T.);
#80192=ORIENTED_EDGE('',*,*,#55141,.T.);
#80193=ORIENTED_EDGE('',*,*,#55148,.T.);
#80194=ORIENTED_EDGE('',*,*,#55149,.T.);
#80195=ORIENTED_EDGE('',*,*,#55150,.T.);
#80196=ORIENTED_EDGE('',*,*,#55151,.T.);
#80197=ORIENTED_EDGE('',*,*,#54280,.F.);
#80198=ORIENTED_EDGE('',*,*,#54266,.F.);
#80199=ORIENTED_EDGE('',*,*,#55152,.T.);
#80200=ORIENTED_EDGE('',*,*,#54273,.F.);
#80201=ORIENTED_EDGE('',*,*,#55153,.T.);
#80202=ORIENTED_EDGE('',*,*,#55154,.T.);
#80203=ORIENTED_EDGE('',*,*,#54272,.T.);
#80204=ORIENTED_EDGE('',*,*,#55155,.T.);
#80205=ORIENTED_EDGE('',*,*,#55156,.T.);
#80206=ORIENTED_EDGE('',*,*,#54271,.T.);
#80207=ORIENTED_EDGE('',*,*,#55157,.T.);
#80208=ORIENTED_EDGE('',*,*,#55158,.T.);
#80209=ORIENTED_EDGE('',*,*,#54270,.T.);
#80210=ORIENTED_EDGE('',*,*,#55159,.T.);
#80211=ORIENTED_EDGE('',*,*,#55160,.T.);
#80212=ORIENTED_EDGE('',*,*,#54275,.T.);
#80213=ORIENTED_EDGE('',*,*,#55161,.T.);
#80214=ORIENTED_EDGE('',*,*,#54598,.T.);
#80215=ORIENTED_EDGE('',*,*,#55162,.F.);
#80216=ORIENTED_EDGE('',*,*,#55163,.F.);
#80217=ORIENTED_EDGE('',*,*,#54277,.F.);
#80218=ORIENTED_EDGE('',*,*,#55164,.F.);
#80219=ORIENTED_EDGE('',*,*,#55165,.F.);
#80220=ORIENTED_EDGE('',*,*,#55166,.F.);
#80221=ORIENTED_EDGE('',*,*,#54790,.T.);
#80222=ORIENTED_EDGE('',*,*,#55167,.T.);
#80223=ORIENTED_EDGE('',*,*,#54287,.F.);
#80224=ORIENTED_EDGE('',*,*,#55168,.T.);
#80225=ORIENTED_EDGE('',*,*,#55169,.T.);
#80226=ORIENTED_EDGE('',*,*,#55170,.F.);
#80227=ORIENTED_EDGE('',*,*,#55171,.F.);
#80228=ORIENTED_EDGE('',*,*,#55172,.F.);
#80229=ORIENTED_EDGE('',*,*,#55152,.F.);
#80230=ORIENTED_EDGE('',*,*,#55173,.T.);
#80231=ORIENTED_EDGE('',*,*,#54276,.F.);
#80232=ORIENTED_EDGE('',*,*,#55169,.F.);
#80233=ORIENTED_EDGE('',*,*,#55153,.F.);
#80234=ORIENTED_EDGE('',*,*,#55154,.F.);
#80235=ORIENTED_EDGE('',*,*,#55174,.T.);
#80236=ORIENTED_EDGE('',*,*,#55175,.F.);
#80237=ORIENTED_EDGE('',*,*,#55173,.F.);
#80238=ORIENTED_EDGE('',*,*,#55155,.F.);
#80239=ORIENTED_EDGE('',*,*,#55156,.F.);
#80240=ORIENTED_EDGE('',*,*,#55176,.T.);
#80241=ORIENTED_EDGE('',*,*,#55177,.F.);
#80242=ORIENTED_EDGE('',*,*,#55174,.F.);
#80243=ORIENTED_EDGE('',*,*,#55157,.F.);
#80244=ORIENTED_EDGE('',*,*,#55158,.F.);
#80245=ORIENTED_EDGE('',*,*,#55178,.T.);
#80246=ORIENTED_EDGE('',*,*,#55179,.F.);
#80247=ORIENTED_EDGE('',*,*,#55176,.F.);
#80248=ORIENTED_EDGE('',*,*,#55159,.F.);
#80249=ORIENTED_EDGE('',*,*,#55160,.F.);
#80250=ORIENTED_EDGE('',*,*,#55171,.T.);
#80251=ORIENTED_EDGE('',*,*,#55180,.F.);
#80252=ORIENTED_EDGE('',*,*,#55178,.F.);
#80253=ORIENTED_EDGE('',*,*,#55161,.F.);
#80254=ORIENTED_EDGE('',*,*,#55181,.F.);
#80255=ORIENTED_EDGE('',*,*,#55181,.T.);
#80256=ORIENTED_EDGE('',*,*,#54274,.T.);
#80257=ORIENTED_EDGE('',*,*,#55172,.T.);
#80258=ORIENTED_EDGE('',*,*,#55180,.T.);
#80259=ORIENTED_EDGE('',*,*,#55162,.T.);
#80260=ORIENTED_EDGE('',*,*,#55177,.T.);
#80261=ORIENTED_EDGE('',*,*,#55165,.T.);
#80262=ORIENTED_EDGE('',*,*,#55175,.T.);
#80263=ORIENTED_EDGE('',*,*,#55164,.T.);
#80264=ORIENTED_EDGE('',*,*,#55179,.T.);
#80265=ORIENTED_EDGE('',*,*,#55166,.T.);
#80266=ORIENTED_EDGE('',*,*,#55170,.T.);
#80267=ORIENTED_EDGE('',*,*,#55163,.T.);
#80268=ORIENTED_EDGE('',*,*,#53841,.F.);
#80269=ORIENTED_EDGE('',*,*,#53729,.F.);
#80270=ORIENTED_EDGE('',*,*,#54263,.F.);
#80271=ORIENTED_EDGE('',*,*,#53836,.F.);
#80272=ORIENTED_EDGE('',*,*,#53951,.T.);
#80273=ORIENTED_EDGE('',*,*,#54262,.T.);
#80274=ORIENTED_EDGE('',*,*,#53945,.T.);
#80275=ORIENTED_EDGE('',*,*,#53942,.T.);
#80276=ORIENTED_EDGE('',*,*,#53939,.T.);
#80277=ORIENTED_EDGE('',*,*,#53938,.T.);
#80278=ORIENTED_EDGE('',*,*,#53935,.T.);
#80279=ORIENTED_EDGE('',*,*,#53932,.T.);
#80280=ORIENTED_EDGE('',*,*,#53929,.T.);
#80281=ORIENTED_EDGE('',*,*,#53926,.T.);
#80282=ORIENTED_EDGE('',*,*,#53923,.T.);
#80283=ORIENTED_EDGE('',*,*,#53920,.T.);
#80284=ORIENTED_EDGE('',*,*,#53917,.T.);
#80285=ORIENTED_EDGE('',*,*,#53914,.T.);
#80286=ORIENTED_EDGE('',*,*,#53911,.T.);
#80287=ORIENTED_EDGE('',*,*,#53908,.T.);
#80288=ORIENTED_EDGE('',*,*,#53905,.T.);
#80289=ORIENTED_EDGE('',*,*,#53902,.T.);
#80290=ORIENTED_EDGE('',*,*,#53899,.T.);
#80291=ORIENTED_EDGE('',*,*,#53896,.T.);
#80292=ORIENTED_EDGE('',*,*,#53893,.T.);
#80293=ORIENTED_EDGE('',*,*,#53890,.T.);
#80294=ORIENTED_EDGE('',*,*,#53887,.T.);
#80295=ORIENTED_EDGE('',*,*,#53884,.T.);
#80296=ORIENTED_EDGE('',*,*,#53881,.T.);
#80297=ORIENTED_EDGE('',*,*,#53878,.T.);
#80298=ORIENTED_EDGE('',*,*,#53875,.T.);
#80299=ORIENTED_EDGE('',*,*,#53872,.T.);
#80300=ORIENTED_EDGE('',*,*,#53869,.T.);
#80301=ORIENTED_EDGE('',*,*,#53866,.T.);
#80302=ORIENTED_EDGE('',*,*,#53863,.T.);
#80303=ORIENTED_EDGE('',*,*,#53860,.T.);
#80304=ORIENTED_EDGE('',*,*,#53857,.T.);
#80305=ORIENTED_EDGE('',*,*,#53854,.T.);
#80306=ORIENTED_EDGE('',*,*,#53851,.T.);
#80307=ORIENTED_EDGE('',*,*,#53848,.T.);
#80308=ORIENTED_EDGE('',*,*,#53845,.T.);
#80309=ORIENTED_EDGE('',*,*,#54264,.T.);
#80310=ORIENTED_EDGE('',*,*,#53728,.T.);
#80311=ORIENTED_EDGE('',*,*,#53731,.T.);
#80312=ORIENTED_EDGE('',*,*,#53734,.T.);
#80313=ORIENTED_EDGE('',*,*,#53737,.T.);
#80314=ORIENTED_EDGE('',*,*,#53740,.T.);
#80315=ORIENTED_EDGE('',*,*,#53743,.T.);
#80316=ORIENTED_EDGE('',*,*,#53746,.T.);
#80317=ORIENTED_EDGE('',*,*,#53749,.T.);
#80318=ORIENTED_EDGE('',*,*,#53752,.T.);
#80319=ORIENTED_EDGE('',*,*,#53755,.T.);
#80320=ORIENTED_EDGE('',*,*,#53758,.T.);
#80321=ORIENTED_EDGE('',*,*,#53761,.T.);
#80322=ORIENTED_EDGE('',*,*,#53764,.T.);
#80323=ORIENTED_EDGE('',*,*,#53767,.T.);
#80324=ORIENTED_EDGE('',*,*,#53770,.T.);
#80325=ORIENTED_EDGE('',*,*,#53773,.T.);
#80326=ORIENTED_EDGE('',*,*,#53776,.T.);
#80327=ORIENTED_EDGE('',*,*,#53779,.T.);
#80328=ORIENTED_EDGE('',*,*,#53782,.T.);
#80329=ORIENTED_EDGE('',*,*,#53785,.T.);
#80330=ORIENTED_EDGE('',*,*,#53788,.T.);
#80331=ORIENTED_EDGE('',*,*,#53791,.T.);
#80332=ORIENTED_EDGE('',*,*,#53794,.T.);
#80333=ORIENTED_EDGE('',*,*,#53797,.T.);
#80334=ORIENTED_EDGE('',*,*,#53800,.T.);
#80335=ORIENTED_EDGE('',*,*,#53803,.T.);
#80336=ORIENTED_EDGE('',*,*,#53806,.T.);
#80337=ORIENTED_EDGE('',*,*,#53809,.T.);
#80338=ORIENTED_EDGE('',*,*,#53812,.T.);
#80339=ORIENTED_EDGE('',*,*,#53815,.T.);
#80340=ORIENTED_EDGE('',*,*,#53818,.T.);
#80341=ORIENTED_EDGE('',*,*,#53821,.T.);
#80342=ORIENTED_EDGE('',*,*,#53824,.T.);
#80343=ORIENTED_EDGE('',*,*,#53827,.T.);
#80344=ORIENTED_EDGE('',*,*,#53830,.T.);
#80345=ORIENTED_EDGE('',*,*,#53833,.T.);
#80346=ORIENTED_EDGE('',*,*,#55182,.T.);
#80347=ORIENTED_EDGE('',*,*,#53832,.T.);
#80348=ORIENTED_EDGE('',*,*,#55183,.T.);
#80349=ORIENTED_EDGE('',*,*,#53837,.F.);
#80350=ORIENTED_EDGE('',*,*,#55182,.F.);
#80351=ORIENTED_EDGE('',*,*,#53838,.F.);
#80352=ORIENTED_EDGE('',*,*,#55183,.F.);
#80353=ORIENTED_EDGE('',*,*,#53834,.F.);
#80354=ORIENTED_EDGE('',*,*,#53831,.F.);
#80355=ORIENTED_EDGE('',*,*,#53828,.F.);
#80356=ORIENTED_EDGE('',*,*,#53825,.F.);
#80357=ORIENTED_EDGE('',*,*,#53822,.F.);
#80358=ORIENTED_EDGE('',*,*,#53819,.F.);
#80359=ORIENTED_EDGE('',*,*,#53816,.F.);
#80360=ORIENTED_EDGE('',*,*,#53813,.F.);
#80361=ORIENTED_EDGE('',*,*,#53810,.F.);
#80362=ORIENTED_EDGE('',*,*,#53807,.F.);
#80363=ORIENTED_EDGE('',*,*,#53804,.F.);
#80364=ORIENTED_EDGE('',*,*,#53801,.F.);
#80365=ORIENTED_EDGE('',*,*,#53798,.F.);
#80366=ORIENTED_EDGE('',*,*,#53795,.F.);
#80367=ORIENTED_EDGE('',*,*,#53792,.F.);
#80368=ORIENTED_EDGE('',*,*,#53789,.F.);
#80369=ORIENTED_EDGE('',*,*,#53786,.F.);
#80370=ORIENTED_EDGE('',*,*,#53783,.F.);
#80371=ORIENTED_EDGE('',*,*,#53780,.F.);
#80372=ORIENTED_EDGE('',*,*,#53777,.F.);
#80373=ORIENTED_EDGE('',*,*,#53774,.F.);
#80374=ORIENTED_EDGE('',*,*,#53771,.F.);
#80375=ORIENTED_EDGE('',*,*,#53768,.F.);
#80376=ORIENTED_EDGE('',*,*,#53765,.F.);
#80377=ORIENTED_EDGE('',*,*,#53762,.F.);
#80378=ORIENTED_EDGE('',*,*,#53759,.F.);
#80379=ORIENTED_EDGE('',*,*,#53756,.F.);
#80380=ORIENTED_EDGE('',*,*,#53753,.F.);
#80381=ORIENTED_EDGE('',*,*,#53750,.F.);
#80382=ORIENTED_EDGE('',*,*,#53747,.F.);
#80383=ORIENTED_EDGE('',*,*,#53744,.F.);
#80384=ORIENTED_EDGE('',*,*,#53741,.F.);
#80385=ORIENTED_EDGE('',*,*,#53738,.F.);
#80386=ORIENTED_EDGE('',*,*,#53735,.F.);
#80387=ORIENTED_EDGE('',*,*,#53732,.F.);
#80388=ORIENTED_EDGE('',*,*,#53840,.T.);
#80389=ORIENTED_EDGE('',*,*,#54265,.T.);
#80390=ORIENTED_EDGE('',*,*,#53843,.T.);
#80391=ORIENTED_EDGE('',*,*,#53847,.T.);
#80392=ORIENTED_EDGE('',*,*,#53850,.T.);
#80393=ORIENTED_EDGE('',*,*,#53853,.T.);
#80394=ORIENTED_EDGE('',*,*,#53856,.T.);
#80395=ORIENTED_EDGE('',*,*,#53859,.T.);
#80396=ORIENTED_EDGE('',*,*,#53862,.T.);
#80397=ORIENTED_EDGE('',*,*,#53865,.T.);
#80398=ORIENTED_EDGE('',*,*,#53868,.T.);
#80399=ORIENTED_EDGE('',*,*,#53871,.T.);
#80400=ORIENTED_EDGE('',*,*,#53874,.T.);
#80401=ORIENTED_EDGE('',*,*,#53877,.T.);
#80402=ORIENTED_EDGE('',*,*,#53880,.T.);
#80403=ORIENTED_EDGE('',*,*,#53883,.T.);
#80404=ORIENTED_EDGE('',*,*,#53886,.T.);
#80405=ORIENTED_EDGE('',*,*,#53889,.T.);
#80406=ORIENTED_EDGE('',*,*,#53892,.T.);
#80407=ORIENTED_EDGE('',*,*,#53895,.T.);
#80408=ORIENTED_EDGE('',*,*,#53898,.T.);
#80409=ORIENTED_EDGE('',*,*,#53901,.T.);
#80410=ORIENTED_EDGE('',*,*,#53904,.T.);
#80411=ORIENTED_EDGE('',*,*,#53907,.T.);
#80412=ORIENTED_EDGE('',*,*,#53910,.T.);
#80413=ORIENTED_EDGE('',*,*,#53913,.T.);
#80414=ORIENTED_EDGE('',*,*,#53916,.T.);
#80415=ORIENTED_EDGE('',*,*,#53919,.T.);
#80416=ORIENTED_EDGE('',*,*,#53922,.T.);
#80417=ORIENTED_EDGE('',*,*,#53925,.T.);
#80418=ORIENTED_EDGE('',*,*,#53928,.T.);
#80419=ORIENTED_EDGE('',*,*,#53931,.T.);
#80420=ORIENTED_EDGE('',*,*,#53934,.T.);
#80421=ORIENTED_EDGE('',*,*,#53937,.T.);
#80422=ORIENTED_EDGE('',*,*,#53941,.T.);
#80423=ORIENTED_EDGE('',*,*,#53944,.T.);
#80424=ORIENTED_EDGE('',*,*,#54261,.T.);
#80425=ORIENTED_EDGE('',*,*,#53949,.T.);
#80426=ORIENTED_EDGE('',*,*,#54268,.F.);
#80427=ORIENTED_EDGE('',*,*,#55184,.T.);
#80428=ORIENTED_EDGE('',*,*,#55185,.T.);
#80429=ORIENTED_EDGE('',*,*,#54256,.T.);
#80430=ORIENTED_EDGE('',*,*,#55186,.T.);
#80431=ORIENTED_EDGE('',*,*,#55187,.F.);
#80432=ORIENTED_EDGE('',*,*,#55146,.F.);
#80433=ORIENTED_EDGE('',*,*,#55188,.F.);
#80434=ORIENTED_EDGE('',*,*,#55186,.F.);
#80435=ORIENTED_EDGE('',*,*,#55189,.F.);
#80436=ORIENTED_EDGE('',*,*,#55147,.F.);
#80437=ORIENTED_EDGE('',*,*,#55190,.F.);
#80438=ORIENTED_EDGE('',*,*,#54791,.F.);
#80439=ORIENTED_EDGE('',*,*,#55188,.T.);
#80440=ORIENTED_EDGE('',*,*,#55143,.F.);
#80441=ORIENTED_EDGE('',*,*,#55142,.F.);
#80442=ORIENTED_EDGE('',*,*,#55191,.F.);
#80443=ORIENTED_EDGE('',*,*,#55184,.F.);
#80444=ORIENTED_EDGE('',*,*,#55190,.T.);
#80445=ORIENTED_EDGE('',*,*,#55187,.T.);
#80446=ORIENTED_EDGE('',*,*,#54260,.F.);
#80447=ORIENTED_EDGE('',*,*,#54792,.T.);
#80448=ORIENTED_EDGE('',*,*,#55189,.T.);
#80449=ORIENTED_EDGE('',*,*,#55168,.F.);
#80450=ORIENTED_EDGE('',*,*,#55192,.F.);
#80451=ORIENTED_EDGE('',*,*,#55144,.F.);
#80452=ORIENTED_EDGE('',*,*,#55191,.T.);
#80453=ORIENTED_EDGE('',*,*,#55151,.F.);
#80454=ORIENTED_EDGE('',*,*,#55193,.F.);
#80455=ORIENTED_EDGE('',*,*,#55185,.F.);
#80456=ORIENTED_EDGE('',*,*,#55192,.T.);
#80457=ORIENTED_EDGE('',*,*,#54286,.F.);
#80458=ORIENTED_EDGE('',*,*,#55194,.F.);
#80459=ORIENTED_EDGE('',*,*,#55145,.F.);
#80460=ORIENTED_EDGE('',*,*,#54257,.T.);
#80461=ORIENTED_EDGE('',*,*,#55193,.T.);
#80462=ORIENTED_EDGE('',*,*,#55195,.F.);
#80463=ORIENTED_EDGE('',*,*,#54794,.T.);
#80464=ORIENTED_EDGE('',*,*,#55194,.T.);
#80465=ORIENTED_EDGE('',*,*,#54285,.F.);
#80466=ORIENTED_EDGE('',*,*,#54597,.F.);
#80467=ORIENTED_EDGE('',*,*,#55196,.F.);
#80468=ORIENTED_EDGE('',*,*,#55140,.F.);
#80469=ORIENTED_EDGE('',*,*,#55139,.F.);
#80470=ORIENTED_EDGE('',*,*,#55195,.T.);
#80471=ORIENTED_EDGE('',*,*,#55150,.F.);
#80472=ORIENTED_EDGE('',*,*,#55197,.F.);
#80473=ORIENTED_EDGE('',*,*,#54795,.F.);
#80474=ORIENTED_EDGE('',*,*,#55196,.T.);
#80475=ORIENTED_EDGE('',*,*,#54596,.F.);
#80476=ORIENTED_EDGE('',*,*,#55198,.F.);
#80477=ORIENTED_EDGE('',*,*,#55148,.F.);
#80478=ORIENTED_EDGE('',*,*,#55197,.T.);
#80479=ORIENTED_EDGE('',*,*,#55149,.F.);
#80480=ORIENTED_EDGE('',*,*,#55198,.T.);
#80481=ORIENTED_EDGE('',*,*,#55135,.F.);
#80482=ORIENTED_EDGE('',*,*,#55199,.T.);
#80483=ORIENTED_EDGE('',*,*,#55200,.T.);
#80484=ORIENTED_EDGE('',*,*,#55201,.T.);
#80485=ORIENTED_EDGE('',*,*,#55202,.T.);
#80486=ORIENTED_EDGE('',*,*,#55203,.T.);
#80487=ORIENTED_EDGE('',*,*,#55204,.T.);
#80488=ORIENTED_EDGE('',*,*,#55205,.T.);
#80489=ORIENTED_EDGE('',*,*,#55206,.F.);
#80490=ORIENTED_EDGE('',*,*,#55207,.T.);
#80491=ORIENTED_EDGE('',*,*,#55208,.T.);
#80492=ORIENTED_EDGE('',*,*,#55206,.T.);
#80493=ORIENTED_EDGE('',*,*,#55209,.T.);
#80494=ORIENTED_EDGE('',*,*,#55210,.T.);
#80495=ORIENTED_EDGE('',*,*,#55199,.F.);
#80496=ORIENTED_EDGE('',*,*,#55211,.T.);
#80497=ORIENTED_EDGE('',*,*,#55212,.T.);
#80498=ORIENTED_EDGE('',*,*,#55213,.F.);
#80499=ORIENTED_EDGE('',*,*,#55207,.F.);
#80500=ORIENTED_EDGE('',*,*,#55214,.F.);
#80501=ORIENTED_EDGE('',*,*,#55215,.F.);
#80502=ORIENTED_EDGE('',*,*,#55214,.T.);
#80503=ORIENTED_EDGE('',*,*,#55212,.F.);
#80504=ORIENTED_EDGE('',*,*,#55211,.F.);
#80505=ORIENTED_EDGE('',*,*,#55216,.F.);
#80506=ORIENTED_EDGE('',*,*,#55217,.F.);
#80507=ORIENTED_EDGE('',*,*,#55216,.T.);
#80508=ORIENTED_EDGE('',*,*,#55203,.F.);
#80509=ORIENTED_EDGE('',*,*,#55218,.F.);
#80510=ORIENTED_EDGE('',*,*,#55219,.F.);
#80511=ORIENTED_EDGE('',*,*,#55220,.T.);
#80512=ORIENTED_EDGE('',*,*,#55213,.T.);
#80513=ORIENTED_EDGE('',*,*,#54255,.F.);
#80514=ORIENTED_EDGE('',*,*,#54787,.T.);
#80515=ORIENTED_EDGE('',*,*,#55221,.F.);
#80516=ORIENTED_EDGE('',*,*,#55208,.F.);
#80517=ORIENTED_EDGE('',*,*,#55220,.F.);
#80518=ORIENTED_EDGE('',*,*,#54786,.F.);
#80519=ORIENTED_EDGE('',*,*,#55221,.T.);
#80520=ORIENTED_EDGE('',*,*,#55137,.F.);
#80521=ORIENTED_EDGE('',*,*,#55222,.F.);
#80522=ORIENTED_EDGE('',*,*,#55204,.F.);
#80523=ORIENTED_EDGE('',*,*,#55222,.T.);
#80524=ORIENTED_EDGE('',*,*,#54290,.F.);
#80525=ORIENTED_EDGE('',*,*,#55223,.F.);
#80526=ORIENTED_EDGE('',*,*,#55205,.F.);
#80527=ORIENTED_EDGE('',*,*,#55223,.T.);
#80528=ORIENTED_EDGE('',*,*,#54289,.F.);
#80529=ORIENTED_EDGE('',*,*,#55224,.F.);
#80530=ORIENTED_EDGE('',*,*,#55210,.F.);
#80531=ORIENTED_EDGE('',*,*,#55209,.F.);
#80532=ORIENTED_EDGE('',*,*,#55224,.T.);
#80533=ORIENTED_EDGE('',*,*,#54288,.F.);
#80534=ORIENTED_EDGE('',*,*,#55225,.F.);
#80535=ORIENTED_EDGE('',*,*,#55200,.F.);
#80536=ORIENTED_EDGE('',*,*,#55226,.T.);
#80537=ORIENTED_EDGE('',*,*,#55201,.F.);
#80538=ORIENTED_EDGE('',*,*,#55225,.T.);
#80539=ORIENTED_EDGE('',*,*,#55167,.F.);
#80540=ORIENTED_EDGE('',*,*,#55227,.T.);
#80541=ORIENTED_EDGE('',*,*,#55202,.F.);
#80542=ORIENTED_EDGE('',*,*,#55226,.F.);
#80543=ORIENTED_EDGE('',*,*,#54789,.F.);
#80544=ORIENTED_EDGE('',*,*,#54253,.T.);
#80545=ORIENTED_EDGE('',*,*,#55218,.T.);
#80546=ORIENTED_EDGE('',*,*,#55227,.F.);
#80547=ORIENTED_EDGE('',*,*,#54788,.T.);
#80548=ORIENTED_EDGE('',*,*,#55217,.T.);
#80549=ORIENTED_EDGE('',*,*,#55219,.T.);
#80550=ORIENTED_EDGE('',*,*,#54252,.T.);
#80551=ORIENTED_EDGE('',*,*,#55215,.T.);
#80552=ORIENTED_EDGE('',*,*,#55228,.T.);
#80553=ORIENTED_EDGE('',*,*,#55229,.T.);
#80554=ORIENTED_EDGE('',*,*,#55230,.T.);
#80555=ORIENTED_EDGE('',*,*,#55231,.T.);
#80556=ORIENTED_EDGE('',*,*,#55232,.T.);
#80557=ORIENTED_EDGE('',*,*,#55233,.T.);
#80558=ORIENTED_EDGE('',*,*,#55234,.T.);
#80559=ORIENTED_EDGE('',*,*,#55235,.F.);
#80560=ORIENTED_EDGE('',*,*,#55236,.T.);
#80561=ORIENTED_EDGE('',*,*,#55237,.T.);
#80562=ORIENTED_EDGE('',*,*,#55235,.T.);
#80563=ORIENTED_EDGE('',*,*,#55238,.T.);
#80564=ORIENTED_EDGE('',*,*,#55239,.T.);
#80565=ORIENTED_EDGE('',*,*,#55228,.F.);
#80566=ORIENTED_EDGE('',*,*,#55240,.T.);
#80567=ORIENTED_EDGE('',*,*,#55241,.T.);
#80568=ORIENTED_EDGE('',*,*,#55242,.F.);
#80569=ORIENTED_EDGE('',*,*,#55236,.F.);
#80570=ORIENTED_EDGE('',*,*,#55243,.F.);
#80571=ORIENTED_EDGE('',*,*,#55244,.F.);
#80572=ORIENTED_EDGE('',*,*,#55243,.T.);
#80573=ORIENTED_EDGE('',*,*,#55241,.F.);
#80574=ORIENTED_EDGE('',*,*,#55240,.F.);
#80575=ORIENTED_EDGE('',*,*,#55245,.F.);
#80576=ORIENTED_EDGE('',*,*,#55246,.F.);
#80577=ORIENTED_EDGE('',*,*,#55245,.T.);
#80578=ORIENTED_EDGE('',*,*,#55232,.F.);
#80579=ORIENTED_EDGE('',*,*,#55247,.F.);
#80580=ORIENTED_EDGE('',*,*,#55248,.F.);
#80581=ORIENTED_EDGE('',*,*,#55249,.T.);
#80582=ORIENTED_EDGE('',*,*,#55242,.T.);
#80583=ORIENTED_EDGE('',*,*,#54251,.F.);
#80584=ORIENTED_EDGE('',*,*,#54798,.T.);
#80585=ORIENTED_EDGE('',*,*,#55250,.F.);
#80586=ORIENTED_EDGE('',*,*,#55237,.F.);
#80587=ORIENTED_EDGE('',*,*,#55249,.F.);
#80588=ORIENTED_EDGE('',*,*,#54797,.F.);
#80589=ORIENTED_EDGE('',*,*,#55250,.T.);
#80590=ORIENTED_EDGE('',*,*,#55134,.F.);
#80591=ORIENTED_EDGE('',*,*,#55251,.F.);
#80592=ORIENTED_EDGE('',*,*,#55233,.F.);
#80593=ORIENTED_EDGE('',*,*,#55251,.T.);
#80594=ORIENTED_EDGE('',*,*,#54594,.F.);
#80595=ORIENTED_EDGE('',*,*,#55252,.F.);
#80596=ORIENTED_EDGE('',*,*,#55234,.F.);
#80597=ORIENTED_EDGE('',*,*,#55252,.T.);
#80598=ORIENTED_EDGE('',*,*,#54593,.F.);
#80599=ORIENTED_EDGE('',*,*,#55253,.F.);
#80600=ORIENTED_EDGE('',*,*,#55239,.F.);
#80601=ORIENTED_EDGE('',*,*,#55238,.F.);
#80602=ORIENTED_EDGE('',*,*,#55253,.T.);
#80603=ORIENTED_EDGE('',*,*,#54592,.F.);
#80604=ORIENTED_EDGE('',*,*,#55254,.F.);
#80605=ORIENTED_EDGE('',*,*,#55229,.F.);
#80606=ORIENTED_EDGE('',*,*,#55255,.T.);
#80607=ORIENTED_EDGE('',*,*,#55230,.F.);
#80608=ORIENTED_EDGE('',*,*,#55254,.T.);
#80609=ORIENTED_EDGE('',*,*,#55133,.F.);
#80610=ORIENTED_EDGE('',*,*,#55256,.T.);
#80611=ORIENTED_EDGE('',*,*,#55231,.F.);
#80612=ORIENTED_EDGE('',*,*,#55255,.F.);
#80613=ORIENTED_EDGE('',*,*,#54800,.F.);
#80614=ORIENTED_EDGE('',*,*,#54249,.T.);
#80615=ORIENTED_EDGE('',*,*,#55247,.T.);
#80616=ORIENTED_EDGE('',*,*,#55256,.F.);
#80617=ORIENTED_EDGE('',*,*,#54799,.T.);
#80618=ORIENTED_EDGE('',*,*,#55246,.T.);
#80619=ORIENTED_EDGE('',*,*,#55248,.T.);
#80620=ORIENTED_EDGE('',*,*,#54248,.T.);
#80621=ORIENTED_EDGE('',*,*,#55244,.T.);
#80622=ORIENTED_EDGE('',*,*,#55257,.T.);
#80623=ORIENTED_EDGE('',*,*,#55258,.T.);
#80624=ORIENTED_EDGE('',*,*,#55259,.T.);
#80625=ORIENTED_EDGE('',*,*,#55260,.T.);
#80626=ORIENTED_EDGE('',*,*,#55261,.T.);
#80627=ORIENTED_EDGE('',*,*,#55262,.T.);
#80628=ORIENTED_EDGE('',*,*,#55263,.T.);
#80629=ORIENTED_EDGE('',*,*,#55264,.F.);
#80630=ORIENTED_EDGE('',*,*,#55265,.T.);
#80631=ORIENTED_EDGE('',*,*,#55266,.T.);
#80632=ORIENTED_EDGE('',*,*,#55264,.T.);
#80633=ORIENTED_EDGE('',*,*,#55267,.T.);
#80634=ORIENTED_EDGE('',*,*,#55268,.T.);
#80635=ORIENTED_EDGE('',*,*,#55257,.F.);
#80636=ORIENTED_EDGE('',*,*,#55269,.T.);
#80637=ORIENTED_EDGE('',*,*,#55270,.T.);
#80638=ORIENTED_EDGE('',*,*,#55271,.F.);
#80639=ORIENTED_EDGE('',*,*,#55265,.F.);
#80640=ORIENTED_EDGE('',*,*,#55272,.F.);
#80641=ORIENTED_EDGE('',*,*,#55273,.F.);
#80642=ORIENTED_EDGE('',*,*,#55272,.T.);
#80643=ORIENTED_EDGE('',*,*,#55270,.F.);
#80644=ORIENTED_EDGE('',*,*,#55269,.F.);
#80645=ORIENTED_EDGE('',*,*,#55274,.F.);
#80646=ORIENTED_EDGE('',*,*,#55275,.F.);
#80647=ORIENTED_EDGE('',*,*,#55274,.T.);
#80648=ORIENTED_EDGE('',*,*,#55261,.F.);
#80649=ORIENTED_EDGE('',*,*,#55276,.F.);
#80650=ORIENTED_EDGE('',*,*,#55277,.F.);
#80651=ORIENTED_EDGE('',*,*,#55278,.T.);
#80652=ORIENTED_EDGE('',*,*,#55271,.T.);
#80653=ORIENTED_EDGE('',*,*,#54247,.F.);
#80654=ORIENTED_EDGE('',*,*,#54803,.T.);
#80655=ORIENTED_EDGE('',*,*,#55279,.F.);
#80656=ORIENTED_EDGE('',*,*,#55266,.F.);
#80657=ORIENTED_EDGE('',*,*,#55278,.F.);
#80658=ORIENTED_EDGE('',*,*,#54802,.F.);
#80659=ORIENTED_EDGE('',*,*,#55279,.T.);
#80660=ORIENTED_EDGE('',*,*,#55132,.F.);
#80661=ORIENTED_EDGE('',*,*,#55280,.F.);
#80662=ORIENTED_EDGE('',*,*,#55262,.F.);
#80663=ORIENTED_EDGE('',*,*,#55280,.T.);
#80664=ORIENTED_EDGE('',*,*,#54590,.F.);
#80665=ORIENTED_EDGE('',*,*,#55281,.F.);
#80666=ORIENTED_EDGE('',*,*,#55263,.F.);
#80667=ORIENTED_EDGE('',*,*,#55281,.T.);
#80668=ORIENTED_EDGE('',*,*,#54589,.F.);
#80669=ORIENTED_EDGE('',*,*,#55282,.F.);
#80670=ORIENTED_EDGE('',*,*,#55268,.F.);
#80671=ORIENTED_EDGE('',*,*,#55267,.F.);
#80672=ORIENTED_EDGE('',*,*,#55282,.T.);
#80673=ORIENTED_EDGE('',*,*,#54588,.F.);
#80674=ORIENTED_EDGE('',*,*,#55283,.F.);
#80675=ORIENTED_EDGE('',*,*,#55258,.F.);
#80676=ORIENTED_EDGE('',*,*,#55284,.T.);
#80677=ORIENTED_EDGE('',*,*,#55259,.F.);
#80678=ORIENTED_EDGE('',*,*,#55283,.T.);
#80679=ORIENTED_EDGE('',*,*,#55131,.F.);
#80680=ORIENTED_EDGE('',*,*,#55285,.T.);
#80681=ORIENTED_EDGE('',*,*,#55260,.F.);
#80682=ORIENTED_EDGE('',*,*,#55284,.F.);
#80683=ORIENTED_EDGE('',*,*,#54805,.F.);
#80684=ORIENTED_EDGE('',*,*,#54245,.T.);
#80685=ORIENTED_EDGE('',*,*,#55276,.T.);
#80686=ORIENTED_EDGE('',*,*,#55285,.F.);
#80687=ORIENTED_EDGE('',*,*,#54804,.T.);
#80688=ORIENTED_EDGE('',*,*,#55275,.T.);
#80689=ORIENTED_EDGE('',*,*,#55277,.T.);
#80690=ORIENTED_EDGE('',*,*,#54244,.T.);
#80691=ORIENTED_EDGE('',*,*,#55273,.T.);
#80692=ORIENTED_EDGE('',*,*,#55286,.T.);
#80693=ORIENTED_EDGE('',*,*,#55287,.T.);
#80694=ORIENTED_EDGE('',*,*,#55288,.T.);
#80695=ORIENTED_EDGE('',*,*,#55289,.T.);
#80696=ORIENTED_EDGE('',*,*,#55290,.T.);
#80697=ORIENTED_EDGE('',*,*,#55291,.T.);
#80698=ORIENTED_EDGE('',*,*,#55292,.T.);
#80699=ORIENTED_EDGE('',*,*,#55293,.F.);
#80700=ORIENTED_EDGE('',*,*,#55294,.T.);
#80701=ORIENTED_EDGE('',*,*,#55295,.T.);
#80702=ORIENTED_EDGE('',*,*,#55293,.T.);
#80703=ORIENTED_EDGE('',*,*,#55296,.T.);
#80704=ORIENTED_EDGE('',*,*,#55297,.T.);
#80705=ORIENTED_EDGE('',*,*,#55286,.F.);
#80706=ORIENTED_EDGE('',*,*,#55298,.T.);
#80707=ORIENTED_EDGE('',*,*,#55299,.T.);
#80708=ORIENTED_EDGE('',*,*,#55300,.F.);
#80709=ORIENTED_EDGE('',*,*,#55294,.F.);
#80710=ORIENTED_EDGE('',*,*,#55301,.F.);
#80711=ORIENTED_EDGE('',*,*,#55302,.F.);
#80712=ORIENTED_EDGE('',*,*,#55301,.T.);
#80713=ORIENTED_EDGE('',*,*,#55299,.F.);
#80714=ORIENTED_EDGE('',*,*,#55298,.F.);
#80715=ORIENTED_EDGE('',*,*,#55303,.F.);
#80716=ORIENTED_EDGE('',*,*,#55304,.F.);
#80717=ORIENTED_EDGE('',*,*,#55303,.T.);
#80718=ORIENTED_EDGE('',*,*,#55290,.F.);
#80719=ORIENTED_EDGE('',*,*,#55305,.F.);
#80720=ORIENTED_EDGE('',*,*,#55306,.F.);
#80721=ORIENTED_EDGE('',*,*,#55307,.T.);
#80722=ORIENTED_EDGE('',*,*,#55300,.T.);
#80723=ORIENTED_EDGE('',*,*,#54243,.F.);
#80724=ORIENTED_EDGE('',*,*,#54808,.T.);
#80725=ORIENTED_EDGE('',*,*,#55308,.F.);
#80726=ORIENTED_EDGE('',*,*,#55295,.F.);
#80727=ORIENTED_EDGE('',*,*,#55307,.F.);
#80728=ORIENTED_EDGE('',*,*,#54807,.F.);
#80729=ORIENTED_EDGE('',*,*,#55308,.T.);
#80730=ORIENTED_EDGE('',*,*,#55130,.F.);
#80731=ORIENTED_EDGE('',*,*,#55309,.F.);
#80732=ORIENTED_EDGE('',*,*,#55291,.F.);
#80733=ORIENTED_EDGE('',*,*,#55309,.T.);
#80734=ORIENTED_EDGE('',*,*,#54586,.F.);
#80735=ORIENTED_EDGE('',*,*,#55310,.F.);
#80736=ORIENTED_EDGE('',*,*,#55292,.F.);
#80737=ORIENTED_EDGE('',*,*,#55310,.T.);
#80738=ORIENTED_EDGE('',*,*,#54585,.F.);
#80739=ORIENTED_EDGE('',*,*,#55311,.F.);
#80740=ORIENTED_EDGE('',*,*,#55297,.F.);
#80741=ORIENTED_EDGE('',*,*,#55296,.F.);
#80742=ORIENTED_EDGE('',*,*,#55311,.T.);
#80743=ORIENTED_EDGE('',*,*,#54584,.F.);
#80744=ORIENTED_EDGE('',*,*,#55312,.F.);
#80745=ORIENTED_EDGE('',*,*,#55287,.F.);
#80746=ORIENTED_EDGE('',*,*,#55313,.T.);
#80747=ORIENTED_EDGE('',*,*,#55288,.F.);
#80748=ORIENTED_EDGE('',*,*,#55312,.T.);
#80749=ORIENTED_EDGE('',*,*,#55129,.F.);
#80750=ORIENTED_EDGE('',*,*,#55314,.T.);
#80751=ORIENTED_EDGE('',*,*,#55289,.F.);
#80752=ORIENTED_EDGE('',*,*,#55313,.F.);
#80753=ORIENTED_EDGE('',*,*,#54810,.F.);
#80754=ORIENTED_EDGE('',*,*,#54241,.T.);
#80755=ORIENTED_EDGE('',*,*,#55305,.T.);
#80756=ORIENTED_EDGE('',*,*,#55314,.F.);
#80757=ORIENTED_EDGE('',*,*,#54809,.T.);
#80758=ORIENTED_EDGE('',*,*,#55304,.T.);
#80759=ORIENTED_EDGE('',*,*,#55306,.T.);
#80760=ORIENTED_EDGE('',*,*,#54240,.T.);
#80761=ORIENTED_EDGE('',*,*,#55302,.T.);
#80762=ORIENTED_EDGE('',*,*,#55315,.T.);
#80763=ORIENTED_EDGE('',*,*,#55316,.T.);
#80764=ORIENTED_EDGE('',*,*,#55317,.T.);
#80765=ORIENTED_EDGE('',*,*,#55318,.T.);
#80766=ORIENTED_EDGE('',*,*,#55319,.T.);
#80767=ORIENTED_EDGE('',*,*,#55320,.T.);
#80768=ORIENTED_EDGE('',*,*,#55321,.T.);
#80769=ORIENTED_EDGE('',*,*,#55322,.F.);
#80770=ORIENTED_EDGE('',*,*,#55323,.T.);
#80771=ORIENTED_EDGE('',*,*,#55324,.T.);
#80772=ORIENTED_EDGE('',*,*,#55322,.T.);
#80773=ORIENTED_EDGE('',*,*,#55325,.T.);
#80774=ORIENTED_EDGE('',*,*,#55326,.T.);
#80775=ORIENTED_EDGE('',*,*,#55315,.F.);
#80776=ORIENTED_EDGE('',*,*,#55327,.T.);
#80777=ORIENTED_EDGE('',*,*,#55328,.T.);
#80778=ORIENTED_EDGE('',*,*,#55329,.F.);
#80779=ORIENTED_EDGE('',*,*,#55323,.F.);
#80780=ORIENTED_EDGE('',*,*,#55330,.F.);
#80781=ORIENTED_EDGE('',*,*,#55331,.F.);
#80782=ORIENTED_EDGE('',*,*,#55330,.T.);
#80783=ORIENTED_EDGE('',*,*,#55328,.F.);
#80784=ORIENTED_EDGE('',*,*,#55327,.F.);
#80785=ORIENTED_EDGE('',*,*,#55332,.F.);
#80786=ORIENTED_EDGE('',*,*,#55333,.F.);
#80787=ORIENTED_EDGE('',*,*,#55332,.T.);
#80788=ORIENTED_EDGE('',*,*,#55319,.F.);
#80789=ORIENTED_EDGE('',*,*,#55334,.F.);
#80790=ORIENTED_EDGE('',*,*,#55335,.F.);
#80791=ORIENTED_EDGE('',*,*,#55336,.T.);
#80792=ORIENTED_EDGE('',*,*,#55329,.T.);
#80793=ORIENTED_EDGE('',*,*,#54239,.F.);
#80794=ORIENTED_EDGE('',*,*,#54813,.T.);
#80795=ORIENTED_EDGE('',*,*,#55337,.F.);
#80796=ORIENTED_EDGE('',*,*,#55324,.F.);
#80797=ORIENTED_EDGE('',*,*,#55336,.F.);
#80798=ORIENTED_EDGE('',*,*,#54812,.F.);
#80799=ORIENTED_EDGE('',*,*,#55337,.T.);
#80800=ORIENTED_EDGE('',*,*,#55128,.F.);
#80801=ORIENTED_EDGE('',*,*,#55338,.F.);
#80802=ORIENTED_EDGE('',*,*,#55320,.F.);
#80803=ORIENTED_EDGE('',*,*,#55338,.T.);
#80804=ORIENTED_EDGE('',*,*,#54582,.F.);
#80805=ORIENTED_EDGE('',*,*,#55339,.F.);
#80806=ORIENTED_EDGE('',*,*,#55321,.F.);
#80807=ORIENTED_EDGE('',*,*,#55339,.T.);
#80808=ORIENTED_EDGE('',*,*,#54581,.F.);
#80809=ORIENTED_EDGE('',*,*,#55340,.F.);
#80810=ORIENTED_EDGE('',*,*,#55326,.F.);
#80811=ORIENTED_EDGE('',*,*,#55325,.F.);
#80812=ORIENTED_EDGE('',*,*,#55340,.T.);
#80813=ORIENTED_EDGE('',*,*,#54580,.F.);
#80814=ORIENTED_EDGE('',*,*,#55341,.F.);
#80815=ORIENTED_EDGE('',*,*,#55316,.F.);
#80816=ORIENTED_EDGE('',*,*,#55342,.T.);
#80817=ORIENTED_EDGE('',*,*,#55317,.F.);
#80818=ORIENTED_EDGE('',*,*,#55341,.T.);
#80819=ORIENTED_EDGE('',*,*,#55127,.F.);
#80820=ORIENTED_EDGE('',*,*,#55343,.T.);
#80821=ORIENTED_EDGE('',*,*,#55318,.F.);
#80822=ORIENTED_EDGE('',*,*,#55342,.F.);
#80823=ORIENTED_EDGE('',*,*,#54815,.F.);
#80824=ORIENTED_EDGE('',*,*,#54237,.T.);
#80825=ORIENTED_EDGE('',*,*,#55334,.T.);
#80826=ORIENTED_EDGE('',*,*,#55343,.F.);
#80827=ORIENTED_EDGE('',*,*,#54814,.T.);
#80828=ORIENTED_EDGE('',*,*,#55333,.T.);
#80829=ORIENTED_EDGE('',*,*,#55335,.T.);
#80830=ORIENTED_EDGE('',*,*,#54236,.T.);
#80831=ORIENTED_EDGE('',*,*,#55331,.T.);
#80832=ORIENTED_EDGE('',*,*,#55344,.T.);
#80833=ORIENTED_EDGE('',*,*,#55345,.T.);
#80834=ORIENTED_EDGE('',*,*,#55346,.T.);
#80835=ORIENTED_EDGE('',*,*,#55347,.T.);
#80836=ORIENTED_EDGE('',*,*,#55348,.T.);
#80837=ORIENTED_EDGE('',*,*,#55349,.T.);
#80838=ORIENTED_EDGE('',*,*,#55350,.T.);
#80839=ORIENTED_EDGE('',*,*,#55351,.F.);
#80840=ORIENTED_EDGE('',*,*,#55352,.T.);
#80841=ORIENTED_EDGE('',*,*,#55353,.T.);
#80842=ORIENTED_EDGE('',*,*,#55351,.T.);
#80843=ORIENTED_EDGE('',*,*,#55354,.T.);
#80844=ORIENTED_EDGE('',*,*,#55355,.T.);
#80845=ORIENTED_EDGE('',*,*,#55344,.F.);
#80846=ORIENTED_EDGE('',*,*,#55356,.T.);
#80847=ORIENTED_EDGE('',*,*,#55357,.T.);
#80848=ORIENTED_EDGE('',*,*,#55358,.F.);
#80849=ORIENTED_EDGE('',*,*,#55352,.F.);
#80850=ORIENTED_EDGE('',*,*,#55359,.F.);
#80851=ORIENTED_EDGE('',*,*,#55360,.F.);
#80852=ORIENTED_EDGE('',*,*,#55359,.T.);
#80853=ORIENTED_EDGE('',*,*,#55357,.F.);
#80854=ORIENTED_EDGE('',*,*,#55356,.F.);
#80855=ORIENTED_EDGE('',*,*,#55361,.F.);
#80856=ORIENTED_EDGE('',*,*,#55362,.F.);
#80857=ORIENTED_EDGE('',*,*,#55361,.T.);
#80858=ORIENTED_EDGE('',*,*,#55348,.F.);
#80859=ORIENTED_EDGE('',*,*,#55363,.F.);
#80860=ORIENTED_EDGE('',*,*,#55364,.F.);
#80861=ORIENTED_EDGE('',*,*,#55365,.T.);
#80862=ORIENTED_EDGE('',*,*,#55358,.T.);
#80863=ORIENTED_EDGE('',*,*,#54235,.F.);
#80864=ORIENTED_EDGE('',*,*,#54818,.T.);
#80865=ORIENTED_EDGE('',*,*,#55366,.F.);
#80866=ORIENTED_EDGE('',*,*,#55353,.F.);
#80867=ORIENTED_EDGE('',*,*,#55365,.F.);
#80868=ORIENTED_EDGE('',*,*,#54817,.F.);
#80869=ORIENTED_EDGE('',*,*,#55366,.T.);
#80870=ORIENTED_EDGE('',*,*,#55126,.F.);
#80871=ORIENTED_EDGE('',*,*,#55367,.F.);
#80872=ORIENTED_EDGE('',*,*,#55349,.F.);
#80873=ORIENTED_EDGE('',*,*,#55367,.T.);
#80874=ORIENTED_EDGE('',*,*,#54578,.F.);
#80875=ORIENTED_EDGE('',*,*,#55368,.F.);
#80876=ORIENTED_EDGE('',*,*,#55350,.F.);
#80877=ORIENTED_EDGE('',*,*,#55368,.T.);
#80878=ORIENTED_EDGE('',*,*,#54577,.F.);
#80879=ORIENTED_EDGE('',*,*,#55369,.F.);
#80880=ORIENTED_EDGE('',*,*,#55355,.F.);
#80881=ORIENTED_EDGE('',*,*,#55354,.F.);
#80882=ORIENTED_EDGE('',*,*,#55369,.T.);
#80883=ORIENTED_EDGE('',*,*,#54576,.F.);
#80884=ORIENTED_EDGE('',*,*,#55370,.F.);
#80885=ORIENTED_EDGE('',*,*,#55345,.F.);
#80886=ORIENTED_EDGE('',*,*,#55371,.T.);
#80887=ORIENTED_EDGE('',*,*,#55346,.F.);
#80888=ORIENTED_EDGE('',*,*,#55370,.T.);
#80889=ORIENTED_EDGE('',*,*,#55125,.F.);
#80890=ORIENTED_EDGE('',*,*,#55372,.T.);
#80891=ORIENTED_EDGE('',*,*,#55347,.F.);
#80892=ORIENTED_EDGE('',*,*,#55371,.F.);
#80893=ORIENTED_EDGE('',*,*,#54820,.F.);
#80894=ORIENTED_EDGE('',*,*,#54233,.T.);
#80895=ORIENTED_EDGE('',*,*,#55363,.T.);
#80896=ORIENTED_EDGE('',*,*,#55372,.F.);
#80897=ORIENTED_EDGE('',*,*,#54819,.T.);
#80898=ORIENTED_EDGE('',*,*,#55362,.T.);
#80899=ORIENTED_EDGE('',*,*,#55364,.T.);
#80900=ORIENTED_EDGE('',*,*,#54232,.T.);
#80901=ORIENTED_EDGE('',*,*,#55360,.T.);
#80902=ORIENTED_EDGE('',*,*,#55373,.T.);
#80903=ORIENTED_EDGE('',*,*,#55374,.T.);
#80904=ORIENTED_EDGE('',*,*,#55375,.T.);
#80905=ORIENTED_EDGE('',*,*,#55376,.T.);
#80906=ORIENTED_EDGE('',*,*,#55377,.T.);
#80907=ORIENTED_EDGE('',*,*,#55378,.T.);
#80908=ORIENTED_EDGE('',*,*,#55379,.T.);
#80909=ORIENTED_EDGE('',*,*,#55380,.F.);
#80910=ORIENTED_EDGE('',*,*,#55381,.T.);
#80911=ORIENTED_EDGE('',*,*,#55382,.T.);
#80912=ORIENTED_EDGE('',*,*,#55380,.T.);
#80913=ORIENTED_EDGE('',*,*,#55383,.T.);
#80914=ORIENTED_EDGE('',*,*,#55384,.T.);
#80915=ORIENTED_EDGE('',*,*,#55373,.F.);
#80916=ORIENTED_EDGE('',*,*,#55385,.T.);
#80917=ORIENTED_EDGE('',*,*,#55386,.T.);
#80918=ORIENTED_EDGE('',*,*,#55387,.F.);
#80919=ORIENTED_EDGE('',*,*,#55381,.F.);
#80920=ORIENTED_EDGE('',*,*,#55388,.F.);
#80921=ORIENTED_EDGE('',*,*,#55389,.F.);
#80922=ORIENTED_EDGE('',*,*,#55388,.T.);
#80923=ORIENTED_EDGE('',*,*,#55386,.F.);
#80924=ORIENTED_EDGE('',*,*,#55385,.F.);
#80925=ORIENTED_EDGE('',*,*,#55390,.F.);
#80926=ORIENTED_EDGE('',*,*,#55391,.F.);
#80927=ORIENTED_EDGE('',*,*,#55390,.T.);
#80928=ORIENTED_EDGE('',*,*,#55377,.F.);
#80929=ORIENTED_EDGE('',*,*,#55392,.F.);
#80930=ORIENTED_EDGE('',*,*,#55393,.F.);
#80931=ORIENTED_EDGE('',*,*,#55394,.T.);
#80932=ORIENTED_EDGE('',*,*,#55387,.T.);
#80933=ORIENTED_EDGE('',*,*,#54231,.F.);
#80934=ORIENTED_EDGE('',*,*,#54823,.T.);
#80935=ORIENTED_EDGE('',*,*,#55395,.F.);
#80936=ORIENTED_EDGE('',*,*,#55382,.F.);
#80937=ORIENTED_EDGE('',*,*,#55394,.F.);
#80938=ORIENTED_EDGE('',*,*,#54822,.F.);
#80939=ORIENTED_EDGE('',*,*,#55395,.T.);
#80940=ORIENTED_EDGE('',*,*,#55124,.F.);
#80941=ORIENTED_EDGE('',*,*,#55396,.F.);
#80942=ORIENTED_EDGE('',*,*,#55378,.F.);
#80943=ORIENTED_EDGE('',*,*,#55396,.T.);
#80944=ORIENTED_EDGE('',*,*,#54574,.F.);
#80945=ORIENTED_EDGE('',*,*,#55397,.F.);
#80946=ORIENTED_EDGE('',*,*,#55379,.F.);
#80947=ORIENTED_EDGE('',*,*,#55397,.T.);
#80948=ORIENTED_EDGE('',*,*,#54573,.F.);
#80949=ORIENTED_EDGE('',*,*,#55398,.F.);
#80950=ORIENTED_EDGE('',*,*,#55384,.F.);
#80951=ORIENTED_EDGE('',*,*,#55383,.F.);
#80952=ORIENTED_EDGE('',*,*,#55398,.T.);
#80953=ORIENTED_EDGE('',*,*,#54572,.F.);
#80954=ORIENTED_EDGE('',*,*,#55399,.F.);
#80955=ORIENTED_EDGE('',*,*,#55374,.F.);
#80956=ORIENTED_EDGE('',*,*,#55400,.T.);
#80957=ORIENTED_EDGE('',*,*,#55375,.F.);
#80958=ORIENTED_EDGE('',*,*,#55399,.T.);
#80959=ORIENTED_EDGE('',*,*,#55123,.F.);
#80960=ORIENTED_EDGE('',*,*,#55401,.T.);
#80961=ORIENTED_EDGE('',*,*,#55376,.F.);
#80962=ORIENTED_EDGE('',*,*,#55400,.F.);
#80963=ORIENTED_EDGE('',*,*,#54825,.F.);
#80964=ORIENTED_EDGE('',*,*,#54229,.T.);
#80965=ORIENTED_EDGE('',*,*,#55392,.T.);
#80966=ORIENTED_EDGE('',*,*,#55401,.F.);
#80967=ORIENTED_EDGE('',*,*,#54824,.T.);
#80968=ORIENTED_EDGE('',*,*,#55391,.T.);
#80969=ORIENTED_EDGE('',*,*,#55393,.T.);
#80970=ORIENTED_EDGE('',*,*,#54228,.T.);
#80971=ORIENTED_EDGE('',*,*,#55389,.T.);
#80972=ORIENTED_EDGE('',*,*,#55402,.T.);
#80973=ORIENTED_EDGE('',*,*,#55403,.T.);
#80974=ORIENTED_EDGE('',*,*,#55404,.T.);
#80975=ORIENTED_EDGE('',*,*,#55405,.T.);
#80976=ORIENTED_EDGE('',*,*,#55406,.T.);
#80977=ORIENTED_EDGE('',*,*,#55407,.T.);
#80978=ORIENTED_EDGE('',*,*,#55408,.T.);
#80979=ORIENTED_EDGE('',*,*,#55409,.F.);
#80980=ORIENTED_EDGE('',*,*,#55410,.T.);
#80981=ORIENTED_EDGE('',*,*,#55411,.T.);
#80982=ORIENTED_EDGE('',*,*,#55409,.T.);
#80983=ORIENTED_EDGE('',*,*,#55412,.T.);
#80984=ORIENTED_EDGE('',*,*,#55413,.T.);
#80985=ORIENTED_EDGE('',*,*,#55402,.F.);
#80986=ORIENTED_EDGE('',*,*,#55414,.T.);
#80987=ORIENTED_EDGE('',*,*,#55415,.T.);
#80988=ORIENTED_EDGE('',*,*,#55416,.F.);
#80989=ORIENTED_EDGE('',*,*,#55410,.F.);
#80990=ORIENTED_EDGE('',*,*,#55417,.F.);
#80991=ORIENTED_EDGE('',*,*,#55418,.F.);
#80992=ORIENTED_EDGE('',*,*,#55417,.T.);
#80993=ORIENTED_EDGE('',*,*,#55415,.F.);
#80994=ORIENTED_EDGE('',*,*,#55414,.F.);
#80995=ORIENTED_EDGE('',*,*,#55419,.F.);
#80996=ORIENTED_EDGE('',*,*,#55420,.F.);
#80997=ORIENTED_EDGE('',*,*,#55419,.T.);
#80998=ORIENTED_EDGE('',*,*,#55406,.F.);
#80999=ORIENTED_EDGE('',*,*,#55421,.F.);
#81000=ORIENTED_EDGE('',*,*,#55422,.F.);
#81001=ORIENTED_EDGE('',*,*,#55423,.T.);
#81002=ORIENTED_EDGE('',*,*,#55416,.T.);
#81003=ORIENTED_EDGE('',*,*,#54227,.F.);
#81004=ORIENTED_EDGE('',*,*,#54828,.T.);
#81005=ORIENTED_EDGE('',*,*,#55424,.F.);
#81006=ORIENTED_EDGE('',*,*,#55411,.F.);
#81007=ORIENTED_EDGE('',*,*,#55423,.F.);
#81008=ORIENTED_EDGE('',*,*,#54827,.F.);
#81009=ORIENTED_EDGE('',*,*,#55424,.T.);
#81010=ORIENTED_EDGE('',*,*,#55122,.F.);
#81011=ORIENTED_EDGE('',*,*,#55425,.F.);
#81012=ORIENTED_EDGE('',*,*,#55407,.F.);
#81013=ORIENTED_EDGE('',*,*,#55425,.T.);
#81014=ORIENTED_EDGE('',*,*,#54570,.F.);
#81015=ORIENTED_EDGE('',*,*,#55426,.F.);
#81016=ORIENTED_EDGE('',*,*,#55408,.F.);
#81017=ORIENTED_EDGE('',*,*,#55426,.T.);
#81018=ORIENTED_EDGE('',*,*,#54569,.F.);
#81019=ORIENTED_EDGE('',*,*,#55427,.F.);
#81020=ORIENTED_EDGE('',*,*,#55413,.F.);
#81021=ORIENTED_EDGE('',*,*,#55412,.F.);
#81022=ORIENTED_EDGE('',*,*,#55427,.T.);
#81023=ORIENTED_EDGE('',*,*,#54568,.F.);
#81024=ORIENTED_EDGE('',*,*,#55428,.F.);
#81025=ORIENTED_EDGE('',*,*,#55403,.F.);
#81026=ORIENTED_EDGE('',*,*,#55429,.T.);
#81027=ORIENTED_EDGE('',*,*,#55404,.F.);
#81028=ORIENTED_EDGE('',*,*,#55428,.T.);
#81029=ORIENTED_EDGE('',*,*,#55121,.F.);
#81030=ORIENTED_EDGE('',*,*,#55430,.T.);
#81031=ORIENTED_EDGE('',*,*,#55405,.F.);
#81032=ORIENTED_EDGE('',*,*,#55429,.F.);
#81033=ORIENTED_EDGE('',*,*,#54830,.F.);
#81034=ORIENTED_EDGE('',*,*,#54225,.T.);
#81035=ORIENTED_EDGE('',*,*,#55421,.T.);
#81036=ORIENTED_EDGE('',*,*,#55430,.F.);
#81037=ORIENTED_EDGE('',*,*,#54829,.T.);
#81038=ORIENTED_EDGE('',*,*,#55420,.T.);
#81039=ORIENTED_EDGE('',*,*,#55422,.T.);
#81040=ORIENTED_EDGE('',*,*,#54224,.T.);
#81041=ORIENTED_EDGE('',*,*,#55418,.T.);
#81042=ORIENTED_EDGE('',*,*,#55431,.T.);
#81043=ORIENTED_EDGE('',*,*,#55432,.T.);
#81044=ORIENTED_EDGE('',*,*,#55433,.T.);
#81045=ORIENTED_EDGE('',*,*,#55434,.T.);
#81046=ORIENTED_EDGE('',*,*,#55435,.T.);
#81047=ORIENTED_EDGE('',*,*,#55436,.T.);
#81048=ORIENTED_EDGE('',*,*,#55437,.T.);
#81049=ORIENTED_EDGE('',*,*,#55438,.F.);
#81050=ORIENTED_EDGE('',*,*,#55439,.T.);
#81051=ORIENTED_EDGE('',*,*,#55440,.T.);
#81052=ORIENTED_EDGE('',*,*,#55438,.T.);
#81053=ORIENTED_EDGE('',*,*,#55441,.T.);
#81054=ORIENTED_EDGE('',*,*,#55442,.T.);
#81055=ORIENTED_EDGE('',*,*,#55431,.F.);
#81056=ORIENTED_EDGE('',*,*,#55443,.T.);
#81057=ORIENTED_EDGE('',*,*,#55444,.T.);
#81058=ORIENTED_EDGE('',*,*,#55445,.F.);
#81059=ORIENTED_EDGE('',*,*,#55439,.F.);
#81060=ORIENTED_EDGE('',*,*,#55446,.F.);
#81061=ORIENTED_EDGE('',*,*,#55447,.F.);
#81062=ORIENTED_EDGE('',*,*,#55446,.T.);
#81063=ORIENTED_EDGE('',*,*,#55444,.F.);
#81064=ORIENTED_EDGE('',*,*,#55443,.F.);
#81065=ORIENTED_EDGE('',*,*,#55448,.F.);
#81066=ORIENTED_EDGE('',*,*,#55449,.F.);
#81067=ORIENTED_EDGE('',*,*,#55448,.T.);
#81068=ORIENTED_EDGE('',*,*,#55435,.F.);
#81069=ORIENTED_EDGE('',*,*,#55450,.F.);
#81070=ORIENTED_EDGE('',*,*,#55451,.F.);
#81071=ORIENTED_EDGE('',*,*,#55452,.T.);
#81072=ORIENTED_EDGE('',*,*,#55445,.T.);
#81073=ORIENTED_EDGE('',*,*,#54223,.F.);
#81074=ORIENTED_EDGE('',*,*,#54833,.T.);
#81075=ORIENTED_EDGE('',*,*,#55453,.F.);
#81076=ORIENTED_EDGE('',*,*,#55440,.F.);
#81077=ORIENTED_EDGE('',*,*,#55452,.F.);
#81078=ORIENTED_EDGE('',*,*,#54832,.F.);
#81079=ORIENTED_EDGE('',*,*,#55453,.T.);
#81080=ORIENTED_EDGE('',*,*,#55120,.F.);
#81081=ORIENTED_EDGE('',*,*,#55454,.F.);
#81082=ORIENTED_EDGE('',*,*,#55436,.F.);
#81083=ORIENTED_EDGE('',*,*,#55454,.T.);
#81084=ORIENTED_EDGE('',*,*,#54566,.F.);
#81085=ORIENTED_EDGE('',*,*,#55455,.F.);
#81086=ORIENTED_EDGE('',*,*,#55437,.F.);
#81087=ORIENTED_EDGE('',*,*,#55455,.T.);
#81088=ORIENTED_EDGE('',*,*,#54565,.F.);
#81089=ORIENTED_EDGE('',*,*,#55456,.F.);
#81090=ORIENTED_EDGE('',*,*,#55442,.F.);
#81091=ORIENTED_EDGE('',*,*,#55441,.F.);
#81092=ORIENTED_EDGE('',*,*,#55456,.T.);
#81093=ORIENTED_EDGE('',*,*,#54564,.F.);
#81094=ORIENTED_EDGE('',*,*,#55457,.F.);
#81095=ORIENTED_EDGE('',*,*,#55432,.F.);
#81096=ORIENTED_EDGE('',*,*,#55458,.T.);
#81097=ORIENTED_EDGE('',*,*,#55433,.F.);
#81098=ORIENTED_EDGE('',*,*,#55457,.T.);
#81099=ORIENTED_EDGE('',*,*,#55119,.F.);
#81100=ORIENTED_EDGE('',*,*,#55459,.T.);
#81101=ORIENTED_EDGE('',*,*,#55434,.F.);
#81102=ORIENTED_EDGE('',*,*,#55458,.F.);
#81103=ORIENTED_EDGE('',*,*,#54835,.F.);
#81104=ORIENTED_EDGE('',*,*,#54221,.T.);
#81105=ORIENTED_EDGE('',*,*,#55450,.T.);
#81106=ORIENTED_EDGE('',*,*,#55459,.F.);
#81107=ORIENTED_EDGE('',*,*,#54834,.T.);
#81108=ORIENTED_EDGE('',*,*,#55449,.T.);
#81109=ORIENTED_EDGE('',*,*,#55451,.T.);
#81110=ORIENTED_EDGE('',*,*,#54220,.T.);
#81111=ORIENTED_EDGE('',*,*,#55447,.T.);
#81112=ORIENTED_EDGE('',*,*,#55460,.T.);
#81113=ORIENTED_EDGE('',*,*,#55461,.T.);
#81114=ORIENTED_EDGE('',*,*,#55462,.T.);
#81115=ORIENTED_EDGE('',*,*,#55463,.T.);
#81116=ORIENTED_EDGE('',*,*,#55464,.T.);
#81117=ORIENTED_EDGE('',*,*,#55465,.T.);
#81118=ORIENTED_EDGE('',*,*,#55466,.T.);
#81119=ORIENTED_EDGE('',*,*,#55467,.F.);
#81120=ORIENTED_EDGE('',*,*,#55468,.T.);
#81121=ORIENTED_EDGE('',*,*,#55469,.T.);
#81122=ORIENTED_EDGE('',*,*,#55467,.T.);
#81123=ORIENTED_EDGE('',*,*,#55470,.T.);
#81124=ORIENTED_EDGE('',*,*,#55471,.T.);
#81125=ORIENTED_EDGE('',*,*,#55460,.F.);
#81126=ORIENTED_EDGE('',*,*,#55472,.T.);
#81127=ORIENTED_EDGE('',*,*,#55473,.T.);
#81128=ORIENTED_EDGE('',*,*,#55474,.F.);
#81129=ORIENTED_EDGE('',*,*,#55468,.F.);
#81130=ORIENTED_EDGE('',*,*,#55475,.F.);
#81131=ORIENTED_EDGE('',*,*,#55476,.F.);
#81132=ORIENTED_EDGE('',*,*,#55475,.T.);
#81133=ORIENTED_EDGE('',*,*,#55473,.F.);
#81134=ORIENTED_EDGE('',*,*,#55472,.F.);
#81135=ORIENTED_EDGE('',*,*,#55477,.F.);
#81136=ORIENTED_EDGE('',*,*,#55478,.F.);
#81137=ORIENTED_EDGE('',*,*,#55477,.T.);
#81138=ORIENTED_EDGE('',*,*,#55464,.F.);
#81139=ORIENTED_EDGE('',*,*,#55479,.F.);
#81140=ORIENTED_EDGE('',*,*,#55480,.F.);
#81141=ORIENTED_EDGE('',*,*,#55481,.T.);
#81142=ORIENTED_EDGE('',*,*,#55474,.T.);
#81143=ORIENTED_EDGE('',*,*,#54219,.F.);
#81144=ORIENTED_EDGE('',*,*,#54838,.T.);
#81145=ORIENTED_EDGE('',*,*,#55482,.F.);
#81146=ORIENTED_EDGE('',*,*,#55469,.F.);
#81147=ORIENTED_EDGE('',*,*,#55481,.F.);
#81148=ORIENTED_EDGE('',*,*,#54837,.F.);
#81149=ORIENTED_EDGE('',*,*,#55482,.T.);
#81150=ORIENTED_EDGE('',*,*,#55118,.F.);
#81151=ORIENTED_EDGE('',*,*,#55483,.F.);
#81152=ORIENTED_EDGE('',*,*,#55465,.F.);
#81153=ORIENTED_EDGE('',*,*,#55483,.T.);
#81154=ORIENTED_EDGE('',*,*,#54562,.F.);
#81155=ORIENTED_EDGE('',*,*,#55484,.F.);
#81156=ORIENTED_EDGE('',*,*,#55466,.F.);
#81157=ORIENTED_EDGE('',*,*,#55484,.T.);
#81158=ORIENTED_EDGE('',*,*,#54561,.F.);
#81159=ORIENTED_EDGE('',*,*,#55485,.F.);
#81160=ORIENTED_EDGE('',*,*,#55471,.F.);
#81161=ORIENTED_EDGE('',*,*,#55470,.F.);
#81162=ORIENTED_EDGE('',*,*,#55485,.T.);
#81163=ORIENTED_EDGE('',*,*,#54560,.F.);
#81164=ORIENTED_EDGE('',*,*,#55486,.F.);
#81165=ORIENTED_EDGE('',*,*,#55461,.F.);
#81166=ORIENTED_EDGE('',*,*,#55487,.T.);
#81167=ORIENTED_EDGE('',*,*,#55462,.F.);
#81168=ORIENTED_EDGE('',*,*,#55486,.T.);
#81169=ORIENTED_EDGE('',*,*,#55117,.F.);
#81170=ORIENTED_EDGE('',*,*,#55488,.T.);
#81171=ORIENTED_EDGE('',*,*,#55463,.F.);
#81172=ORIENTED_EDGE('',*,*,#55487,.F.);
#81173=ORIENTED_EDGE('',*,*,#54840,.F.);
#81174=ORIENTED_EDGE('',*,*,#54217,.T.);
#81175=ORIENTED_EDGE('',*,*,#55479,.T.);
#81176=ORIENTED_EDGE('',*,*,#55488,.F.);
#81177=ORIENTED_EDGE('',*,*,#54839,.T.);
#81178=ORIENTED_EDGE('',*,*,#55478,.T.);
#81179=ORIENTED_EDGE('',*,*,#55480,.T.);
#81180=ORIENTED_EDGE('',*,*,#54216,.T.);
#81181=ORIENTED_EDGE('',*,*,#55476,.T.);
#81182=ORIENTED_EDGE('',*,*,#55489,.T.);
#81183=ORIENTED_EDGE('',*,*,#55490,.T.);
#81184=ORIENTED_EDGE('',*,*,#55491,.T.);
#81185=ORIENTED_EDGE('',*,*,#55492,.T.);
#81186=ORIENTED_EDGE('',*,*,#55493,.T.);
#81187=ORIENTED_EDGE('',*,*,#55494,.T.);
#81188=ORIENTED_EDGE('',*,*,#55495,.T.);
#81189=ORIENTED_EDGE('',*,*,#55496,.F.);
#81190=ORIENTED_EDGE('',*,*,#55497,.T.);
#81191=ORIENTED_EDGE('',*,*,#55498,.T.);
#81192=ORIENTED_EDGE('',*,*,#55496,.T.);
#81193=ORIENTED_EDGE('',*,*,#55499,.T.);
#81194=ORIENTED_EDGE('',*,*,#55500,.T.);
#81195=ORIENTED_EDGE('',*,*,#55489,.F.);
#81196=ORIENTED_EDGE('',*,*,#55501,.T.);
#81197=ORIENTED_EDGE('',*,*,#55502,.T.);
#81198=ORIENTED_EDGE('',*,*,#55503,.F.);
#81199=ORIENTED_EDGE('',*,*,#55497,.F.);
#81200=ORIENTED_EDGE('',*,*,#55504,.F.);
#81201=ORIENTED_EDGE('',*,*,#55505,.F.);
#81202=ORIENTED_EDGE('',*,*,#55504,.T.);
#81203=ORIENTED_EDGE('',*,*,#55502,.F.);
#81204=ORIENTED_EDGE('',*,*,#55501,.F.);
#81205=ORIENTED_EDGE('',*,*,#55506,.F.);
#81206=ORIENTED_EDGE('',*,*,#55507,.F.);
#81207=ORIENTED_EDGE('',*,*,#55506,.T.);
#81208=ORIENTED_EDGE('',*,*,#55493,.F.);
#81209=ORIENTED_EDGE('',*,*,#55508,.F.);
#81210=ORIENTED_EDGE('',*,*,#55509,.F.);
#81211=ORIENTED_EDGE('',*,*,#55510,.T.);
#81212=ORIENTED_EDGE('',*,*,#55503,.T.);
#81213=ORIENTED_EDGE('',*,*,#54215,.F.);
#81214=ORIENTED_EDGE('',*,*,#54843,.T.);
#81215=ORIENTED_EDGE('',*,*,#55511,.F.);
#81216=ORIENTED_EDGE('',*,*,#55498,.F.);
#81217=ORIENTED_EDGE('',*,*,#55510,.F.);
#81218=ORIENTED_EDGE('',*,*,#54842,.F.);
#81219=ORIENTED_EDGE('',*,*,#55511,.T.);
#81220=ORIENTED_EDGE('',*,*,#55116,.F.);
#81221=ORIENTED_EDGE('',*,*,#55512,.F.);
#81222=ORIENTED_EDGE('',*,*,#55494,.F.);
#81223=ORIENTED_EDGE('',*,*,#55512,.T.);
#81224=ORIENTED_EDGE('',*,*,#54558,.F.);
#81225=ORIENTED_EDGE('',*,*,#55513,.F.);
#81226=ORIENTED_EDGE('',*,*,#55495,.F.);
#81227=ORIENTED_EDGE('',*,*,#55513,.T.);
#81228=ORIENTED_EDGE('',*,*,#54557,.F.);
#81229=ORIENTED_EDGE('',*,*,#55514,.F.);
#81230=ORIENTED_EDGE('',*,*,#55500,.F.);
#81231=ORIENTED_EDGE('',*,*,#55499,.F.);
#81232=ORIENTED_EDGE('',*,*,#55514,.T.);
#81233=ORIENTED_EDGE('',*,*,#54556,.F.);
#81234=ORIENTED_EDGE('',*,*,#55515,.F.);
#81235=ORIENTED_EDGE('',*,*,#55490,.F.);
#81236=ORIENTED_EDGE('',*,*,#55516,.T.);
#81237=ORIENTED_EDGE('',*,*,#55491,.F.);
#81238=ORIENTED_EDGE('',*,*,#55515,.T.);
#81239=ORIENTED_EDGE('',*,*,#55115,.F.);
#81240=ORIENTED_EDGE('',*,*,#55517,.T.);
#81241=ORIENTED_EDGE('',*,*,#55492,.F.);
#81242=ORIENTED_EDGE('',*,*,#55516,.F.);
#81243=ORIENTED_EDGE('',*,*,#54845,.F.);
#81244=ORIENTED_EDGE('',*,*,#54213,.T.);
#81245=ORIENTED_EDGE('',*,*,#55508,.T.);
#81246=ORIENTED_EDGE('',*,*,#55517,.F.);
#81247=ORIENTED_EDGE('',*,*,#54844,.T.);
#81248=ORIENTED_EDGE('',*,*,#55507,.T.);
#81249=ORIENTED_EDGE('',*,*,#55509,.T.);
#81250=ORIENTED_EDGE('',*,*,#54212,.T.);
#81251=ORIENTED_EDGE('',*,*,#55505,.T.);
#81252=ORIENTED_EDGE('',*,*,#55518,.T.);
#81253=ORIENTED_EDGE('',*,*,#55519,.T.);
#81254=ORIENTED_EDGE('',*,*,#55520,.T.);
#81255=ORIENTED_EDGE('',*,*,#55521,.T.);
#81256=ORIENTED_EDGE('',*,*,#55522,.T.);
#81257=ORIENTED_EDGE('',*,*,#55523,.T.);
#81258=ORIENTED_EDGE('',*,*,#55524,.T.);
#81259=ORIENTED_EDGE('',*,*,#55525,.F.);
#81260=ORIENTED_EDGE('',*,*,#55526,.T.);
#81261=ORIENTED_EDGE('',*,*,#55527,.T.);
#81262=ORIENTED_EDGE('',*,*,#55525,.T.);
#81263=ORIENTED_EDGE('',*,*,#55528,.T.);
#81264=ORIENTED_EDGE('',*,*,#55529,.T.);
#81265=ORIENTED_EDGE('',*,*,#55518,.F.);
#81266=ORIENTED_EDGE('',*,*,#55530,.T.);
#81267=ORIENTED_EDGE('',*,*,#55531,.T.);
#81268=ORIENTED_EDGE('',*,*,#55532,.F.);
#81269=ORIENTED_EDGE('',*,*,#55526,.F.);
#81270=ORIENTED_EDGE('',*,*,#55533,.F.);
#81271=ORIENTED_EDGE('',*,*,#55534,.F.);
#81272=ORIENTED_EDGE('',*,*,#55533,.T.);
#81273=ORIENTED_EDGE('',*,*,#55531,.F.);
#81274=ORIENTED_EDGE('',*,*,#55530,.F.);
#81275=ORIENTED_EDGE('',*,*,#55535,.F.);
#81276=ORIENTED_EDGE('',*,*,#55536,.F.);
#81277=ORIENTED_EDGE('',*,*,#55535,.T.);
#81278=ORIENTED_EDGE('',*,*,#55522,.F.);
#81279=ORIENTED_EDGE('',*,*,#55537,.F.);
#81280=ORIENTED_EDGE('',*,*,#55538,.F.);
#81281=ORIENTED_EDGE('',*,*,#55539,.T.);
#81282=ORIENTED_EDGE('',*,*,#55532,.T.);
#81283=ORIENTED_EDGE('',*,*,#54211,.F.);
#81284=ORIENTED_EDGE('',*,*,#54848,.T.);
#81285=ORIENTED_EDGE('',*,*,#55540,.F.);
#81286=ORIENTED_EDGE('',*,*,#55527,.F.);
#81287=ORIENTED_EDGE('',*,*,#55539,.F.);
#81288=ORIENTED_EDGE('',*,*,#54847,.F.);
#81289=ORIENTED_EDGE('',*,*,#55540,.T.);
#81290=ORIENTED_EDGE('',*,*,#55114,.F.);
#81291=ORIENTED_EDGE('',*,*,#55541,.F.);
#81292=ORIENTED_EDGE('',*,*,#55523,.F.);
#81293=ORIENTED_EDGE('',*,*,#55541,.T.);
#81294=ORIENTED_EDGE('',*,*,#54554,.F.);
#81295=ORIENTED_EDGE('',*,*,#55542,.F.);
#81296=ORIENTED_EDGE('',*,*,#55524,.F.);
#81297=ORIENTED_EDGE('',*,*,#55542,.T.);
#81298=ORIENTED_EDGE('',*,*,#54553,.F.);
#81299=ORIENTED_EDGE('',*,*,#55543,.F.);
#81300=ORIENTED_EDGE('',*,*,#55529,.F.);
#81301=ORIENTED_EDGE('',*,*,#55528,.F.);
#81302=ORIENTED_EDGE('',*,*,#55543,.T.);
#81303=ORIENTED_EDGE('',*,*,#54552,.F.);
#81304=ORIENTED_EDGE('',*,*,#55544,.F.);
#81305=ORIENTED_EDGE('',*,*,#55519,.F.);
#81306=ORIENTED_EDGE('',*,*,#55545,.T.);
#81307=ORIENTED_EDGE('',*,*,#55520,.F.);
#81308=ORIENTED_EDGE('',*,*,#55544,.T.);
#81309=ORIENTED_EDGE('',*,*,#54989,.F.);
#81310=ORIENTED_EDGE('',*,*,#55546,.T.);
#81311=ORIENTED_EDGE('',*,*,#55521,.F.);
#81312=ORIENTED_EDGE('',*,*,#55545,.F.);
#81313=ORIENTED_EDGE('',*,*,#54850,.F.);
#81314=ORIENTED_EDGE('',*,*,#54209,.T.);
#81315=ORIENTED_EDGE('',*,*,#55537,.T.);
#81316=ORIENTED_EDGE('',*,*,#55546,.F.);
#81317=ORIENTED_EDGE('',*,*,#54849,.T.);
#81318=ORIENTED_EDGE('',*,*,#55536,.T.);
#81319=ORIENTED_EDGE('',*,*,#55538,.T.);
#81320=ORIENTED_EDGE('',*,*,#54208,.T.);
#81321=ORIENTED_EDGE('',*,*,#55534,.T.);
#81322=ORIENTED_EDGE('',*,*,#55547,.T.);
#81323=ORIENTED_EDGE('',*,*,#55548,.T.);
#81324=ORIENTED_EDGE('',*,*,#55549,.T.);
#81325=ORIENTED_EDGE('',*,*,#55550,.T.);
#81326=ORIENTED_EDGE('',*,*,#55551,.T.);
#81327=ORIENTED_EDGE('',*,*,#55552,.T.);
#81328=ORIENTED_EDGE('',*,*,#55553,.T.);
#81329=ORIENTED_EDGE('',*,*,#55554,.F.);
#81330=ORIENTED_EDGE('',*,*,#55555,.T.);
#81331=ORIENTED_EDGE('',*,*,#55556,.T.);
#81332=ORIENTED_EDGE('',*,*,#55554,.T.);
#81333=ORIENTED_EDGE('',*,*,#55557,.T.);
#81334=ORIENTED_EDGE('',*,*,#55558,.T.);
#81335=ORIENTED_EDGE('',*,*,#55547,.F.);
#81336=ORIENTED_EDGE('',*,*,#55559,.T.);
#81337=ORIENTED_EDGE('',*,*,#55560,.T.);
#81338=ORIENTED_EDGE('',*,*,#55561,.F.);
#81339=ORIENTED_EDGE('',*,*,#55555,.F.);
#81340=ORIENTED_EDGE('',*,*,#55562,.F.);
#81341=ORIENTED_EDGE('',*,*,#55563,.F.);
#81342=ORIENTED_EDGE('',*,*,#55562,.T.);
#81343=ORIENTED_EDGE('',*,*,#55560,.F.);
#81344=ORIENTED_EDGE('',*,*,#55559,.F.);
#81345=ORIENTED_EDGE('',*,*,#55564,.F.);
#81346=ORIENTED_EDGE('',*,*,#55565,.F.);
#81347=ORIENTED_EDGE('',*,*,#55564,.T.);
#81348=ORIENTED_EDGE('',*,*,#55551,.F.);
#81349=ORIENTED_EDGE('',*,*,#55566,.F.);
#81350=ORIENTED_EDGE('',*,*,#55567,.F.);
#81351=ORIENTED_EDGE('',*,*,#55568,.T.);
#81352=ORIENTED_EDGE('',*,*,#55561,.T.);
#81353=ORIENTED_EDGE('',*,*,#54207,.F.);
#81354=ORIENTED_EDGE('',*,*,#54782,.T.);
#81355=ORIENTED_EDGE('',*,*,#55569,.F.);
#81356=ORIENTED_EDGE('',*,*,#55556,.F.);
#81357=ORIENTED_EDGE('',*,*,#55568,.F.);
#81358=ORIENTED_EDGE('',*,*,#54781,.F.);
#81359=ORIENTED_EDGE('',*,*,#55569,.T.);
#81360=ORIENTED_EDGE('',*,*,#55113,.F.);
#81361=ORIENTED_EDGE('',*,*,#55570,.F.);
#81362=ORIENTED_EDGE('',*,*,#55552,.F.);
#81363=ORIENTED_EDGE('',*,*,#55570,.T.);
#81364=ORIENTED_EDGE('',*,*,#54294,.F.);
#81365=ORIENTED_EDGE('',*,*,#55571,.F.);
#81366=ORIENTED_EDGE('',*,*,#55553,.F.);
#81367=ORIENTED_EDGE('',*,*,#55571,.T.);
#81368=ORIENTED_EDGE('',*,*,#54293,.F.);
#81369=ORIENTED_EDGE('',*,*,#55572,.F.);
#81370=ORIENTED_EDGE('',*,*,#55558,.F.);
#81371=ORIENTED_EDGE('',*,*,#55557,.F.);
#81372=ORIENTED_EDGE('',*,*,#55572,.T.);
#81373=ORIENTED_EDGE('',*,*,#54292,.F.);
#81374=ORIENTED_EDGE('',*,*,#55573,.F.);
#81375=ORIENTED_EDGE('',*,*,#55548,.F.);
#81376=ORIENTED_EDGE('',*,*,#55574,.T.);
#81377=ORIENTED_EDGE('',*,*,#55549,.F.);
#81378=ORIENTED_EDGE('',*,*,#55573,.T.);
#81379=ORIENTED_EDGE('',*,*,#55136,.F.);
#81380=ORIENTED_EDGE('',*,*,#55575,.T.);
#81381=ORIENTED_EDGE('',*,*,#55550,.F.);
#81382=ORIENTED_EDGE('',*,*,#55574,.F.);
#81383=ORIENTED_EDGE('',*,*,#54784,.F.);
#81384=ORIENTED_EDGE('',*,*,#54205,.T.);
#81385=ORIENTED_EDGE('',*,*,#55566,.T.);
#81386=ORIENTED_EDGE('',*,*,#55575,.F.);
#81387=ORIENTED_EDGE('',*,*,#54783,.T.);
#81388=ORIENTED_EDGE('',*,*,#55565,.T.);
#81389=ORIENTED_EDGE('',*,*,#55567,.T.);
#81390=ORIENTED_EDGE('',*,*,#54204,.T.);
#81391=ORIENTED_EDGE('',*,*,#55563,.T.);
#81392=ORIENTED_EDGE('',*,*,#55576,.T.);
#81393=ORIENTED_EDGE('',*,*,#55577,.T.);
#81394=ORIENTED_EDGE('',*,*,#55578,.T.);
#81395=ORIENTED_EDGE('',*,*,#55579,.T.);
#81396=ORIENTED_EDGE('',*,*,#55580,.T.);
#81397=ORIENTED_EDGE('',*,*,#55581,.T.);
#81398=ORIENTED_EDGE('',*,*,#55582,.T.);
#81399=ORIENTED_EDGE('',*,*,#55583,.F.);
#81400=ORIENTED_EDGE('',*,*,#55584,.T.);
#81401=ORIENTED_EDGE('',*,*,#55585,.T.);
#81402=ORIENTED_EDGE('',*,*,#55583,.T.);
#81403=ORIENTED_EDGE('',*,*,#55586,.T.);
#81404=ORIENTED_EDGE('',*,*,#55587,.T.);
#81405=ORIENTED_EDGE('',*,*,#55576,.F.);
#81406=ORIENTED_EDGE('',*,*,#55588,.T.);
#81407=ORIENTED_EDGE('',*,*,#55589,.T.);
#81408=ORIENTED_EDGE('',*,*,#55590,.F.);
#81409=ORIENTED_EDGE('',*,*,#55584,.F.);
#81410=ORIENTED_EDGE('',*,*,#55591,.F.);
#81411=ORIENTED_EDGE('',*,*,#55592,.F.);
#81412=ORIENTED_EDGE('',*,*,#55591,.T.);
#81413=ORIENTED_EDGE('',*,*,#55589,.F.);
#81414=ORIENTED_EDGE('',*,*,#55588,.F.);
#81415=ORIENTED_EDGE('',*,*,#55593,.F.);
#81416=ORIENTED_EDGE('',*,*,#55594,.F.);
#81417=ORIENTED_EDGE('',*,*,#55593,.T.);
#81418=ORIENTED_EDGE('',*,*,#55580,.F.);
#81419=ORIENTED_EDGE('',*,*,#55595,.F.);
#81420=ORIENTED_EDGE('',*,*,#55596,.F.);
#81421=ORIENTED_EDGE('',*,*,#55597,.T.);
#81422=ORIENTED_EDGE('',*,*,#55590,.T.);
#81423=ORIENTED_EDGE('',*,*,#54203,.F.);
#81424=ORIENTED_EDGE('',*,*,#54777,.T.);
#81425=ORIENTED_EDGE('',*,*,#55598,.F.);
#81426=ORIENTED_EDGE('',*,*,#55585,.F.);
#81427=ORIENTED_EDGE('',*,*,#55597,.F.);
#81428=ORIENTED_EDGE('',*,*,#54776,.F.);
#81429=ORIENTED_EDGE('',*,*,#55598,.T.);
#81430=ORIENTED_EDGE('',*,*,#55111,.F.);
#81431=ORIENTED_EDGE('',*,*,#55599,.F.);
#81432=ORIENTED_EDGE('',*,*,#55581,.F.);
#81433=ORIENTED_EDGE('',*,*,#55599,.T.);
#81434=ORIENTED_EDGE('',*,*,#54298,.F.);
#81435=ORIENTED_EDGE('',*,*,#55600,.F.);
#81436=ORIENTED_EDGE('',*,*,#55582,.F.);
#81437=ORIENTED_EDGE('',*,*,#55600,.T.);
#81438=ORIENTED_EDGE('',*,*,#54297,.F.);
#81439=ORIENTED_EDGE('',*,*,#55601,.F.);
#81440=ORIENTED_EDGE('',*,*,#55587,.F.);
#81441=ORIENTED_EDGE('',*,*,#55586,.F.);
#81442=ORIENTED_EDGE('',*,*,#55601,.T.);
#81443=ORIENTED_EDGE('',*,*,#54296,.F.);
#81444=ORIENTED_EDGE('',*,*,#55602,.F.);
#81445=ORIENTED_EDGE('',*,*,#55577,.F.);
#81446=ORIENTED_EDGE('',*,*,#55603,.T.);
#81447=ORIENTED_EDGE('',*,*,#55578,.F.);
#81448=ORIENTED_EDGE('',*,*,#55602,.T.);
#81449=ORIENTED_EDGE('',*,*,#55112,.F.);
#81450=ORIENTED_EDGE('',*,*,#55604,.T.);
#81451=ORIENTED_EDGE('',*,*,#55579,.F.);
#81452=ORIENTED_EDGE('',*,*,#55603,.F.);
#81453=ORIENTED_EDGE('',*,*,#54779,.F.);
#81454=ORIENTED_EDGE('',*,*,#54201,.T.);
#81455=ORIENTED_EDGE('',*,*,#55595,.T.);
#81456=ORIENTED_EDGE('',*,*,#55604,.F.);
#81457=ORIENTED_EDGE('',*,*,#54778,.T.);
#81458=ORIENTED_EDGE('',*,*,#55594,.T.);
#81459=ORIENTED_EDGE('',*,*,#55596,.T.);
#81460=ORIENTED_EDGE('',*,*,#54200,.T.);
#81461=ORIENTED_EDGE('',*,*,#55592,.T.);
#81462=ORIENTED_EDGE('',*,*,#55605,.T.);
#81463=ORIENTED_EDGE('',*,*,#55606,.T.);
#81464=ORIENTED_EDGE('',*,*,#55607,.T.);
#81465=ORIENTED_EDGE('',*,*,#55608,.T.);
#81466=ORIENTED_EDGE('',*,*,#55609,.T.);
#81467=ORIENTED_EDGE('',*,*,#55610,.T.);
#81468=ORIENTED_EDGE('',*,*,#55611,.T.);
#81469=ORIENTED_EDGE('',*,*,#55612,.F.);
#81470=ORIENTED_EDGE('',*,*,#55613,.T.);
#81471=ORIENTED_EDGE('',*,*,#55614,.T.);
#81472=ORIENTED_EDGE('',*,*,#55612,.T.);
#81473=ORIENTED_EDGE('',*,*,#55615,.T.);
#81474=ORIENTED_EDGE('',*,*,#55616,.T.);
#81475=ORIENTED_EDGE('',*,*,#55605,.F.);
#81476=ORIENTED_EDGE('',*,*,#55617,.T.);
#81477=ORIENTED_EDGE('',*,*,#55618,.T.);
#81478=ORIENTED_EDGE('',*,*,#55619,.F.);
#81479=ORIENTED_EDGE('',*,*,#55613,.F.);
#81480=ORIENTED_EDGE('',*,*,#55620,.F.);
#81481=ORIENTED_EDGE('',*,*,#55621,.F.);
#81482=ORIENTED_EDGE('',*,*,#55620,.T.);
#81483=ORIENTED_EDGE('',*,*,#55618,.F.);
#81484=ORIENTED_EDGE('',*,*,#55617,.F.);
#81485=ORIENTED_EDGE('',*,*,#55622,.F.);
#81486=ORIENTED_EDGE('',*,*,#55623,.F.);
#81487=ORIENTED_EDGE('',*,*,#55622,.T.);
#81488=ORIENTED_EDGE('',*,*,#55609,.F.);
#81489=ORIENTED_EDGE('',*,*,#55624,.F.);
#81490=ORIENTED_EDGE('',*,*,#55625,.F.);
#81491=ORIENTED_EDGE('',*,*,#55626,.T.);
#81492=ORIENTED_EDGE('',*,*,#55619,.T.);
#81493=ORIENTED_EDGE('',*,*,#54199,.F.);
#81494=ORIENTED_EDGE('',*,*,#54772,.T.);
#81495=ORIENTED_EDGE('',*,*,#55627,.F.);
#81496=ORIENTED_EDGE('',*,*,#55614,.F.);
#81497=ORIENTED_EDGE('',*,*,#55626,.F.);
#81498=ORIENTED_EDGE('',*,*,#54771,.F.);
#81499=ORIENTED_EDGE('',*,*,#55627,.T.);
#81500=ORIENTED_EDGE('',*,*,#55109,.F.);
#81501=ORIENTED_EDGE('',*,*,#55628,.F.);
#81502=ORIENTED_EDGE('',*,*,#55610,.F.);
#81503=ORIENTED_EDGE('',*,*,#55628,.T.);
#81504=ORIENTED_EDGE('',*,*,#54302,.F.);
#81505=ORIENTED_EDGE('',*,*,#55629,.F.);
#81506=ORIENTED_EDGE('',*,*,#55611,.F.);
#81507=ORIENTED_EDGE('',*,*,#55629,.T.);
#81508=ORIENTED_EDGE('',*,*,#54301,.F.);
#81509=ORIENTED_EDGE('',*,*,#55630,.F.);
#81510=ORIENTED_EDGE('',*,*,#55616,.F.);
#81511=ORIENTED_EDGE('',*,*,#55615,.F.);
#81512=ORIENTED_EDGE('',*,*,#55630,.T.);
#81513=ORIENTED_EDGE('',*,*,#54300,.F.);
#81514=ORIENTED_EDGE('',*,*,#55631,.F.);
#81515=ORIENTED_EDGE('',*,*,#55606,.F.);
#81516=ORIENTED_EDGE('',*,*,#55632,.T.);
#81517=ORIENTED_EDGE('',*,*,#55607,.F.);
#81518=ORIENTED_EDGE('',*,*,#55631,.T.);
#81519=ORIENTED_EDGE('',*,*,#55110,.F.);
#81520=ORIENTED_EDGE('',*,*,#55633,.T.);
#81521=ORIENTED_EDGE('',*,*,#55608,.F.);
#81522=ORIENTED_EDGE('',*,*,#55632,.F.);
#81523=ORIENTED_EDGE('',*,*,#54774,.F.);
#81524=ORIENTED_EDGE('',*,*,#54197,.T.);
#81525=ORIENTED_EDGE('',*,*,#55624,.T.);
#81526=ORIENTED_EDGE('',*,*,#55633,.F.);
#81527=ORIENTED_EDGE('',*,*,#54773,.T.);
#81528=ORIENTED_EDGE('',*,*,#55623,.T.);
#81529=ORIENTED_EDGE('',*,*,#55625,.T.);
#81530=ORIENTED_EDGE('',*,*,#54196,.T.);
#81531=ORIENTED_EDGE('',*,*,#55621,.T.);
#81532=ORIENTED_EDGE('',*,*,#55634,.T.);
#81533=ORIENTED_EDGE('',*,*,#55635,.T.);
#81534=ORIENTED_EDGE('',*,*,#55636,.T.);
#81535=ORIENTED_EDGE('',*,*,#55637,.T.);
#81536=ORIENTED_EDGE('',*,*,#55638,.T.);
#81537=ORIENTED_EDGE('',*,*,#55639,.T.);
#81538=ORIENTED_EDGE('',*,*,#55640,.T.);
#81539=ORIENTED_EDGE('',*,*,#55641,.F.);
#81540=ORIENTED_EDGE('',*,*,#55642,.T.);
#81541=ORIENTED_EDGE('',*,*,#55643,.T.);
#81542=ORIENTED_EDGE('',*,*,#55641,.T.);
#81543=ORIENTED_EDGE('',*,*,#55644,.T.);
#81544=ORIENTED_EDGE('',*,*,#55645,.T.);
#81545=ORIENTED_EDGE('',*,*,#55634,.F.);
#81546=ORIENTED_EDGE('',*,*,#55646,.T.);
#81547=ORIENTED_EDGE('',*,*,#55647,.T.);
#81548=ORIENTED_EDGE('',*,*,#55648,.F.);
#81549=ORIENTED_EDGE('',*,*,#55642,.F.);
#81550=ORIENTED_EDGE('',*,*,#55649,.F.);
#81551=ORIENTED_EDGE('',*,*,#55650,.F.);
#81552=ORIENTED_EDGE('',*,*,#55649,.T.);
#81553=ORIENTED_EDGE('',*,*,#55647,.F.);
#81554=ORIENTED_EDGE('',*,*,#55646,.F.);
#81555=ORIENTED_EDGE('',*,*,#55651,.F.);
#81556=ORIENTED_EDGE('',*,*,#55652,.F.);
#81557=ORIENTED_EDGE('',*,*,#55651,.T.);
#81558=ORIENTED_EDGE('',*,*,#55638,.F.);
#81559=ORIENTED_EDGE('',*,*,#55653,.F.);
#81560=ORIENTED_EDGE('',*,*,#55654,.F.);
#81561=ORIENTED_EDGE('',*,*,#55655,.T.);
#81562=ORIENTED_EDGE('',*,*,#55648,.T.);
#81563=ORIENTED_EDGE('',*,*,#54195,.F.);
#81564=ORIENTED_EDGE('',*,*,#54767,.T.);
#81565=ORIENTED_EDGE('',*,*,#55656,.F.);
#81566=ORIENTED_EDGE('',*,*,#55643,.F.);
#81567=ORIENTED_EDGE('',*,*,#55655,.F.);
#81568=ORIENTED_EDGE('',*,*,#54766,.F.);
#81569=ORIENTED_EDGE('',*,*,#55656,.T.);
#81570=ORIENTED_EDGE('',*,*,#55107,.F.);
#81571=ORIENTED_EDGE('',*,*,#55657,.F.);
#81572=ORIENTED_EDGE('',*,*,#55639,.F.);
#81573=ORIENTED_EDGE('',*,*,#55657,.T.);
#81574=ORIENTED_EDGE('',*,*,#54306,.F.);
#81575=ORIENTED_EDGE('',*,*,#55658,.F.);
#81576=ORIENTED_EDGE('',*,*,#55640,.F.);
#81577=ORIENTED_EDGE('',*,*,#55658,.T.);
#81578=ORIENTED_EDGE('',*,*,#54305,.F.);
#81579=ORIENTED_EDGE('',*,*,#55659,.F.);
#81580=ORIENTED_EDGE('',*,*,#55645,.F.);
#81581=ORIENTED_EDGE('',*,*,#55644,.F.);
#81582=ORIENTED_EDGE('',*,*,#55659,.T.);
#81583=ORIENTED_EDGE('',*,*,#54304,.F.);
#81584=ORIENTED_EDGE('',*,*,#55660,.F.);
#81585=ORIENTED_EDGE('',*,*,#55635,.F.);
#81586=ORIENTED_EDGE('',*,*,#55661,.T.);
#81587=ORIENTED_EDGE('',*,*,#55636,.F.);
#81588=ORIENTED_EDGE('',*,*,#55660,.T.);
#81589=ORIENTED_EDGE('',*,*,#55108,.F.);
#81590=ORIENTED_EDGE('',*,*,#55662,.T.);
#81591=ORIENTED_EDGE('',*,*,#55637,.F.);
#81592=ORIENTED_EDGE('',*,*,#55661,.F.);
#81593=ORIENTED_EDGE('',*,*,#54769,.F.);
#81594=ORIENTED_EDGE('',*,*,#54193,.T.);
#81595=ORIENTED_EDGE('',*,*,#55653,.T.);
#81596=ORIENTED_EDGE('',*,*,#55662,.F.);
#81597=ORIENTED_EDGE('',*,*,#54768,.T.);
#81598=ORIENTED_EDGE('',*,*,#55652,.T.);
#81599=ORIENTED_EDGE('',*,*,#55654,.T.);
#81600=ORIENTED_EDGE('',*,*,#54192,.T.);
#81601=ORIENTED_EDGE('',*,*,#55650,.T.);
#81602=ORIENTED_EDGE('',*,*,#55663,.T.);
#81603=ORIENTED_EDGE('',*,*,#55664,.T.);
#81604=ORIENTED_EDGE('',*,*,#55665,.T.);
#81605=ORIENTED_EDGE('',*,*,#55666,.T.);
#81606=ORIENTED_EDGE('',*,*,#55667,.T.);
#81607=ORIENTED_EDGE('',*,*,#55668,.T.);
#81608=ORIENTED_EDGE('',*,*,#55669,.T.);
#81609=ORIENTED_EDGE('',*,*,#55670,.F.);
#81610=ORIENTED_EDGE('',*,*,#55671,.T.);
#81611=ORIENTED_EDGE('',*,*,#55672,.T.);
#81612=ORIENTED_EDGE('',*,*,#55670,.T.);
#81613=ORIENTED_EDGE('',*,*,#55673,.T.);
#81614=ORIENTED_EDGE('',*,*,#55674,.T.);
#81615=ORIENTED_EDGE('',*,*,#55663,.F.);
#81616=ORIENTED_EDGE('',*,*,#55675,.T.);
#81617=ORIENTED_EDGE('',*,*,#55676,.T.);
#81618=ORIENTED_EDGE('',*,*,#55677,.F.);
#81619=ORIENTED_EDGE('',*,*,#55671,.F.);
#81620=ORIENTED_EDGE('',*,*,#55678,.F.);
#81621=ORIENTED_EDGE('',*,*,#55679,.F.);
#81622=ORIENTED_EDGE('',*,*,#55678,.T.);
#81623=ORIENTED_EDGE('',*,*,#55676,.F.);
#81624=ORIENTED_EDGE('',*,*,#55675,.F.);
#81625=ORIENTED_EDGE('',*,*,#55680,.F.);
#81626=ORIENTED_EDGE('',*,*,#55681,.F.);
#81627=ORIENTED_EDGE('',*,*,#55680,.T.);
#81628=ORIENTED_EDGE('',*,*,#55667,.F.);
#81629=ORIENTED_EDGE('',*,*,#55682,.F.);
#81630=ORIENTED_EDGE('',*,*,#55683,.F.);
#81631=ORIENTED_EDGE('',*,*,#55684,.T.);
#81632=ORIENTED_EDGE('',*,*,#55677,.T.);
#81633=ORIENTED_EDGE('',*,*,#54191,.F.);
#81634=ORIENTED_EDGE('',*,*,#54762,.T.);
#81635=ORIENTED_EDGE('',*,*,#55685,.F.);
#81636=ORIENTED_EDGE('',*,*,#55672,.F.);
#81637=ORIENTED_EDGE('',*,*,#55684,.F.);
#81638=ORIENTED_EDGE('',*,*,#54761,.F.);
#81639=ORIENTED_EDGE('',*,*,#55685,.T.);
#81640=ORIENTED_EDGE('',*,*,#55105,.F.);
#81641=ORIENTED_EDGE('',*,*,#55686,.F.);
#81642=ORIENTED_EDGE('',*,*,#55668,.F.);
#81643=ORIENTED_EDGE('',*,*,#55686,.T.);
#81644=ORIENTED_EDGE('',*,*,#54310,.F.);
#81645=ORIENTED_EDGE('',*,*,#55687,.F.);
#81646=ORIENTED_EDGE('',*,*,#55669,.F.);
#81647=ORIENTED_EDGE('',*,*,#55687,.T.);
#81648=ORIENTED_EDGE('',*,*,#54309,.F.);
#81649=ORIENTED_EDGE('',*,*,#55688,.F.);
#81650=ORIENTED_EDGE('',*,*,#55674,.F.);
#81651=ORIENTED_EDGE('',*,*,#55673,.F.);
#81652=ORIENTED_EDGE('',*,*,#55688,.T.);
#81653=ORIENTED_EDGE('',*,*,#54308,.F.);
#81654=ORIENTED_EDGE('',*,*,#55689,.F.);
#81655=ORIENTED_EDGE('',*,*,#55664,.F.);
#81656=ORIENTED_EDGE('',*,*,#55690,.T.);
#81657=ORIENTED_EDGE('',*,*,#55665,.F.);
#81658=ORIENTED_EDGE('',*,*,#55689,.T.);
#81659=ORIENTED_EDGE('',*,*,#55106,.F.);
#81660=ORIENTED_EDGE('',*,*,#55691,.T.);
#81661=ORIENTED_EDGE('',*,*,#55666,.F.);
#81662=ORIENTED_EDGE('',*,*,#55690,.F.);
#81663=ORIENTED_EDGE('',*,*,#54764,.F.);
#81664=ORIENTED_EDGE('',*,*,#54189,.T.);
#81665=ORIENTED_EDGE('',*,*,#55682,.T.);
#81666=ORIENTED_EDGE('',*,*,#55691,.F.);
#81667=ORIENTED_EDGE('',*,*,#54763,.T.);
#81668=ORIENTED_EDGE('',*,*,#55681,.T.);
#81669=ORIENTED_EDGE('',*,*,#55683,.T.);
#81670=ORIENTED_EDGE('',*,*,#54188,.T.);
#81671=ORIENTED_EDGE('',*,*,#55679,.T.);
#81672=ORIENTED_EDGE('',*,*,#55692,.T.);
#81673=ORIENTED_EDGE('',*,*,#55693,.T.);
#81674=ORIENTED_EDGE('',*,*,#55694,.T.);
#81675=ORIENTED_EDGE('',*,*,#55695,.T.);
#81676=ORIENTED_EDGE('',*,*,#55696,.T.);
#81677=ORIENTED_EDGE('',*,*,#55697,.T.);
#81678=ORIENTED_EDGE('',*,*,#55698,.T.);
#81679=ORIENTED_EDGE('',*,*,#55699,.F.);
#81680=ORIENTED_EDGE('',*,*,#55700,.T.);
#81681=ORIENTED_EDGE('',*,*,#55701,.T.);
#81682=ORIENTED_EDGE('',*,*,#55699,.T.);
#81683=ORIENTED_EDGE('',*,*,#55702,.T.);
#81684=ORIENTED_EDGE('',*,*,#55703,.T.);
#81685=ORIENTED_EDGE('',*,*,#55692,.F.);
#81686=ORIENTED_EDGE('',*,*,#55704,.T.);
#81687=ORIENTED_EDGE('',*,*,#55705,.T.);
#81688=ORIENTED_EDGE('',*,*,#55706,.F.);
#81689=ORIENTED_EDGE('',*,*,#55700,.F.);
#81690=ORIENTED_EDGE('',*,*,#55707,.F.);
#81691=ORIENTED_EDGE('',*,*,#55708,.F.);
#81692=ORIENTED_EDGE('',*,*,#55707,.T.);
#81693=ORIENTED_EDGE('',*,*,#55705,.F.);
#81694=ORIENTED_EDGE('',*,*,#55704,.F.);
#81695=ORIENTED_EDGE('',*,*,#55709,.F.);
#81696=ORIENTED_EDGE('',*,*,#55710,.F.);
#81697=ORIENTED_EDGE('',*,*,#55709,.T.);
#81698=ORIENTED_EDGE('',*,*,#55696,.F.);
#81699=ORIENTED_EDGE('',*,*,#55711,.F.);
#81700=ORIENTED_EDGE('',*,*,#55712,.F.);
#81701=ORIENTED_EDGE('',*,*,#55713,.T.);
#81702=ORIENTED_EDGE('',*,*,#55706,.T.);
#81703=ORIENTED_EDGE('',*,*,#54187,.F.);
#81704=ORIENTED_EDGE('',*,*,#54757,.T.);
#81705=ORIENTED_EDGE('',*,*,#55714,.F.);
#81706=ORIENTED_EDGE('',*,*,#55701,.F.);
#81707=ORIENTED_EDGE('',*,*,#55713,.F.);
#81708=ORIENTED_EDGE('',*,*,#54756,.F.);
#81709=ORIENTED_EDGE('',*,*,#55714,.T.);
#81710=ORIENTED_EDGE('',*,*,#55103,.F.);
#81711=ORIENTED_EDGE('',*,*,#55715,.F.);
#81712=ORIENTED_EDGE('',*,*,#55697,.F.);
#81713=ORIENTED_EDGE('',*,*,#55715,.T.);
#81714=ORIENTED_EDGE('',*,*,#54314,.F.);
#81715=ORIENTED_EDGE('',*,*,#55716,.F.);
#81716=ORIENTED_EDGE('',*,*,#55698,.F.);
#81717=ORIENTED_EDGE('',*,*,#55716,.T.);
#81718=ORIENTED_EDGE('',*,*,#54313,.F.);
#81719=ORIENTED_EDGE('',*,*,#55717,.F.);
#81720=ORIENTED_EDGE('',*,*,#55703,.F.);
#81721=ORIENTED_EDGE('',*,*,#55702,.F.);
#81722=ORIENTED_EDGE('',*,*,#55717,.T.);
#81723=ORIENTED_EDGE('',*,*,#54312,.F.);
#81724=ORIENTED_EDGE('',*,*,#55718,.F.);
#81725=ORIENTED_EDGE('',*,*,#55693,.F.);
#81726=ORIENTED_EDGE('',*,*,#55719,.T.);
#81727=ORIENTED_EDGE('',*,*,#55694,.F.);
#81728=ORIENTED_EDGE('',*,*,#55718,.T.);
#81729=ORIENTED_EDGE('',*,*,#55104,.F.);
#81730=ORIENTED_EDGE('',*,*,#55720,.T.);
#81731=ORIENTED_EDGE('',*,*,#55695,.F.);
#81732=ORIENTED_EDGE('',*,*,#55719,.F.);
#81733=ORIENTED_EDGE('',*,*,#54759,.F.);
#81734=ORIENTED_EDGE('',*,*,#54185,.T.);
#81735=ORIENTED_EDGE('',*,*,#55711,.T.);
#81736=ORIENTED_EDGE('',*,*,#55720,.F.);
#81737=ORIENTED_EDGE('',*,*,#54758,.T.);
#81738=ORIENTED_EDGE('',*,*,#55710,.T.);
#81739=ORIENTED_EDGE('',*,*,#55712,.T.);
#81740=ORIENTED_EDGE('',*,*,#54184,.T.);
#81741=ORIENTED_EDGE('',*,*,#55708,.T.);
#81742=ORIENTED_EDGE('',*,*,#55721,.T.);
#81743=ORIENTED_EDGE('',*,*,#55722,.T.);
#81744=ORIENTED_EDGE('',*,*,#55723,.T.);
#81745=ORIENTED_EDGE('',*,*,#55724,.T.);
#81746=ORIENTED_EDGE('',*,*,#55725,.T.);
#81747=ORIENTED_EDGE('',*,*,#55726,.T.);
#81748=ORIENTED_EDGE('',*,*,#55727,.T.);
#81749=ORIENTED_EDGE('',*,*,#55728,.F.);
#81750=ORIENTED_EDGE('',*,*,#55729,.T.);
#81751=ORIENTED_EDGE('',*,*,#55730,.T.);
#81752=ORIENTED_EDGE('',*,*,#55728,.T.);
#81753=ORIENTED_EDGE('',*,*,#55731,.T.);
#81754=ORIENTED_EDGE('',*,*,#55732,.T.);
#81755=ORIENTED_EDGE('',*,*,#55721,.F.);
#81756=ORIENTED_EDGE('',*,*,#55733,.T.);
#81757=ORIENTED_EDGE('',*,*,#55734,.T.);
#81758=ORIENTED_EDGE('',*,*,#55735,.F.);
#81759=ORIENTED_EDGE('',*,*,#55729,.F.);
#81760=ORIENTED_EDGE('',*,*,#55736,.F.);
#81761=ORIENTED_EDGE('',*,*,#55737,.F.);
#81762=ORIENTED_EDGE('',*,*,#55736,.T.);
#81763=ORIENTED_EDGE('',*,*,#55734,.F.);
#81764=ORIENTED_EDGE('',*,*,#55733,.F.);
#81765=ORIENTED_EDGE('',*,*,#55738,.F.);
#81766=ORIENTED_EDGE('',*,*,#55739,.F.);
#81767=ORIENTED_EDGE('',*,*,#55738,.T.);
#81768=ORIENTED_EDGE('',*,*,#55725,.F.);
#81769=ORIENTED_EDGE('',*,*,#55740,.F.);
#81770=ORIENTED_EDGE('',*,*,#55741,.F.);
#81771=ORIENTED_EDGE('',*,*,#55742,.T.);
#81772=ORIENTED_EDGE('',*,*,#55735,.T.);
#81773=ORIENTED_EDGE('',*,*,#54183,.F.);
#81774=ORIENTED_EDGE('',*,*,#54752,.T.);
#81775=ORIENTED_EDGE('',*,*,#55743,.F.);
#81776=ORIENTED_EDGE('',*,*,#55730,.F.);
#81777=ORIENTED_EDGE('',*,*,#55742,.F.);
#81778=ORIENTED_EDGE('',*,*,#54751,.F.);
#81779=ORIENTED_EDGE('',*,*,#55743,.T.);
#81780=ORIENTED_EDGE('',*,*,#55101,.F.);
#81781=ORIENTED_EDGE('',*,*,#55744,.F.);
#81782=ORIENTED_EDGE('',*,*,#55726,.F.);
#81783=ORIENTED_EDGE('',*,*,#55744,.T.);
#81784=ORIENTED_EDGE('',*,*,#54318,.F.);
#81785=ORIENTED_EDGE('',*,*,#55745,.F.);
#81786=ORIENTED_EDGE('',*,*,#55727,.F.);
#81787=ORIENTED_EDGE('',*,*,#55745,.T.);
#81788=ORIENTED_EDGE('',*,*,#54317,.F.);
#81789=ORIENTED_EDGE('',*,*,#55746,.F.);
#81790=ORIENTED_EDGE('',*,*,#55732,.F.);
#81791=ORIENTED_EDGE('',*,*,#55731,.F.);
#81792=ORIENTED_EDGE('',*,*,#55746,.T.);
#81793=ORIENTED_EDGE('',*,*,#54316,.F.);
#81794=ORIENTED_EDGE('',*,*,#55747,.F.);
#81795=ORIENTED_EDGE('',*,*,#55722,.F.);
#81796=ORIENTED_EDGE('',*,*,#55748,.T.);
#81797=ORIENTED_EDGE('',*,*,#55723,.F.);
#81798=ORIENTED_EDGE('',*,*,#55747,.T.);
#81799=ORIENTED_EDGE('',*,*,#55102,.F.);
#81800=ORIENTED_EDGE('',*,*,#55749,.T.);
#81801=ORIENTED_EDGE('',*,*,#55724,.F.);
#81802=ORIENTED_EDGE('',*,*,#55748,.F.);
#81803=ORIENTED_EDGE('',*,*,#54754,.F.);
#81804=ORIENTED_EDGE('',*,*,#54181,.T.);
#81805=ORIENTED_EDGE('',*,*,#55740,.T.);
#81806=ORIENTED_EDGE('',*,*,#55749,.F.);
#81807=ORIENTED_EDGE('',*,*,#54753,.T.);
#81808=ORIENTED_EDGE('',*,*,#55739,.T.);
#81809=ORIENTED_EDGE('',*,*,#55741,.T.);
#81810=ORIENTED_EDGE('',*,*,#54180,.T.);
#81811=ORIENTED_EDGE('',*,*,#55737,.T.);
#81812=ORIENTED_EDGE('',*,*,#55750,.T.);
#81813=ORIENTED_EDGE('',*,*,#55751,.T.);
#81814=ORIENTED_EDGE('',*,*,#55752,.T.);
#81815=ORIENTED_EDGE('',*,*,#55753,.T.);
#81816=ORIENTED_EDGE('',*,*,#55754,.T.);
#81817=ORIENTED_EDGE('',*,*,#55755,.T.);
#81818=ORIENTED_EDGE('',*,*,#55756,.T.);
#81819=ORIENTED_EDGE('',*,*,#55757,.F.);
#81820=ORIENTED_EDGE('',*,*,#55758,.T.);
#81821=ORIENTED_EDGE('',*,*,#55759,.T.);
#81822=ORIENTED_EDGE('',*,*,#55757,.T.);
#81823=ORIENTED_EDGE('',*,*,#55760,.T.);
#81824=ORIENTED_EDGE('',*,*,#55761,.T.);
#81825=ORIENTED_EDGE('',*,*,#55750,.F.);
#81826=ORIENTED_EDGE('',*,*,#55762,.T.);
#81827=ORIENTED_EDGE('',*,*,#55763,.T.);
#81828=ORIENTED_EDGE('',*,*,#55764,.F.);
#81829=ORIENTED_EDGE('',*,*,#55758,.F.);
#81830=ORIENTED_EDGE('',*,*,#55765,.F.);
#81831=ORIENTED_EDGE('',*,*,#55766,.F.);
#81832=ORIENTED_EDGE('',*,*,#55765,.T.);
#81833=ORIENTED_EDGE('',*,*,#55763,.F.);
#81834=ORIENTED_EDGE('',*,*,#55762,.F.);
#81835=ORIENTED_EDGE('',*,*,#55767,.F.);
#81836=ORIENTED_EDGE('',*,*,#55768,.F.);
#81837=ORIENTED_EDGE('',*,*,#55767,.T.);
#81838=ORIENTED_EDGE('',*,*,#55754,.F.);
#81839=ORIENTED_EDGE('',*,*,#55769,.F.);
#81840=ORIENTED_EDGE('',*,*,#55770,.F.);
#81841=ORIENTED_EDGE('',*,*,#55771,.T.);
#81842=ORIENTED_EDGE('',*,*,#55764,.T.);
#81843=ORIENTED_EDGE('',*,*,#54179,.F.);
#81844=ORIENTED_EDGE('',*,*,#54747,.T.);
#81845=ORIENTED_EDGE('',*,*,#55772,.F.);
#81846=ORIENTED_EDGE('',*,*,#55759,.F.);
#81847=ORIENTED_EDGE('',*,*,#55771,.F.);
#81848=ORIENTED_EDGE('',*,*,#54746,.F.);
#81849=ORIENTED_EDGE('',*,*,#55772,.T.);
#81850=ORIENTED_EDGE('',*,*,#55099,.F.);
#81851=ORIENTED_EDGE('',*,*,#55773,.F.);
#81852=ORIENTED_EDGE('',*,*,#55755,.F.);
#81853=ORIENTED_EDGE('',*,*,#55773,.T.);
#81854=ORIENTED_EDGE('',*,*,#54322,.F.);
#81855=ORIENTED_EDGE('',*,*,#55774,.F.);
#81856=ORIENTED_EDGE('',*,*,#55756,.F.);
#81857=ORIENTED_EDGE('',*,*,#55774,.T.);
#81858=ORIENTED_EDGE('',*,*,#54321,.F.);
#81859=ORIENTED_EDGE('',*,*,#55775,.F.);
#81860=ORIENTED_EDGE('',*,*,#55761,.F.);
#81861=ORIENTED_EDGE('',*,*,#55760,.F.);
#81862=ORIENTED_EDGE('',*,*,#55775,.T.);
#81863=ORIENTED_EDGE('',*,*,#54320,.F.);
#81864=ORIENTED_EDGE('',*,*,#55776,.F.);
#81865=ORIENTED_EDGE('',*,*,#55751,.F.);
#81866=ORIENTED_EDGE('',*,*,#55777,.T.);
#81867=ORIENTED_EDGE('',*,*,#55752,.F.);
#81868=ORIENTED_EDGE('',*,*,#55776,.T.);
#81869=ORIENTED_EDGE('',*,*,#55100,.F.);
#81870=ORIENTED_EDGE('',*,*,#55778,.T.);
#81871=ORIENTED_EDGE('',*,*,#55753,.F.);
#81872=ORIENTED_EDGE('',*,*,#55777,.F.);
#81873=ORIENTED_EDGE('',*,*,#54749,.F.);
#81874=ORIENTED_EDGE('',*,*,#54177,.T.);
#81875=ORIENTED_EDGE('',*,*,#55769,.T.);
#81876=ORIENTED_EDGE('',*,*,#55778,.F.);
#81877=ORIENTED_EDGE('',*,*,#54748,.T.);
#81878=ORIENTED_EDGE('',*,*,#55768,.T.);
#81879=ORIENTED_EDGE('',*,*,#55770,.T.);
#81880=ORIENTED_EDGE('',*,*,#54176,.T.);
#81881=ORIENTED_EDGE('',*,*,#55766,.T.);
#81882=ORIENTED_EDGE('',*,*,#55779,.T.);
#81883=ORIENTED_EDGE('',*,*,#55780,.T.);
#81884=ORIENTED_EDGE('',*,*,#55781,.T.);
#81885=ORIENTED_EDGE('',*,*,#55782,.T.);
#81886=ORIENTED_EDGE('',*,*,#55783,.T.);
#81887=ORIENTED_EDGE('',*,*,#55784,.T.);
#81888=ORIENTED_EDGE('',*,*,#55785,.T.);
#81889=ORIENTED_EDGE('',*,*,#55786,.F.);
#81890=ORIENTED_EDGE('',*,*,#55787,.T.);
#81891=ORIENTED_EDGE('',*,*,#55788,.T.);
#81892=ORIENTED_EDGE('',*,*,#55786,.T.);
#81893=ORIENTED_EDGE('',*,*,#55789,.T.);
#81894=ORIENTED_EDGE('',*,*,#55790,.T.);
#81895=ORIENTED_EDGE('',*,*,#55779,.F.);
#81896=ORIENTED_EDGE('',*,*,#55791,.T.);
#81897=ORIENTED_EDGE('',*,*,#55792,.T.);
#81898=ORIENTED_EDGE('',*,*,#55793,.F.);
#81899=ORIENTED_EDGE('',*,*,#55787,.F.);
#81900=ORIENTED_EDGE('',*,*,#55794,.F.);
#81901=ORIENTED_EDGE('',*,*,#55795,.F.);
#81902=ORIENTED_EDGE('',*,*,#55794,.T.);
#81903=ORIENTED_EDGE('',*,*,#55792,.F.);
#81904=ORIENTED_EDGE('',*,*,#55791,.F.);
#81905=ORIENTED_EDGE('',*,*,#55796,.F.);
#81906=ORIENTED_EDGE('',*,*,#55797,.F.);
#81907=ORIENTED_EDGE('',*,*,#55796,.T.);
#81908=ORIENTED_EDGE('',*,*,#55783,.F.);
#81909=ORIENTED_EDGE('',*,*,#55798,.F.);
#81910=ORIENTED_EDGE('',*,*,#55799,.F.);
#81911=ORIENTED_EDGE('',*,*,#55800,.T.);
#81912=ORIENTED_EDGE('',*,*,#55793,.T.);
#81913=ORIENTED_EDGE('',*,*,#54175,.F.);
#81914=ORIENTED_EDGE('',*,*,#54742,.T.);
#81915=ORIENTED_EDGE('',*,*,#55801,.F.);
#81916=ORIENTED_EDGE('',*,*,#55788,.F.);
#81917=ORIENTED_EDGE('',*,*,#55800,.F.);
#81918=ORIENTED_EDGE('',*,*,#54741,.F.);
#81919=ORIENTED_EDGE('',*,*,#55801,.T.);
#81920=ORIENTED_EDGE('',*,*,#55097,.F.);
#81921=ORIENTED_EDGE('',*,*,#55802,.F.);
#81922=ORIENTED_EDGE('',*,*,#55784,.F.);
#81923=ORIENTED_EDGE('',*,*,#55802,.T.);
#81924=ORIENTED_EDGE('',*,*,#54326,.F.);
#81925=ORIENTED_EDGE('',*,*,#55803,.F.);
#81926=ORIENTED_EDGE('',*,*,#55785,.F.);
#81927=ORIENTED_EDGE('',*,*,#55803,.T.);
#81928=ORIENTED_EDGE('',*,*,#54325,.F.);
#81929=ORIENTED_EDGE('',*,*,#55804,.F.);
#81930=ORIENTED_EDGE('',*,*,#55790,.F.);
#81931=ORIENTED_EDGE('',*,*,#55789,.F.);
#81932=ORIENTED_EDGE('',*,*,#55804,.T.);
#81933=ORIENTED_EDGE('',*,*,#54324,.F.);
#81934=ORIENTED_EDGE('',*,*,#55805,.F.);
#81935=ORIENTED_EDGE('',*,*,#55780,.F.);
#81936=ORIENTED_EDGE('',*,*,#55806,.T.);
#81937=ORIENTED_EDGE('',*,*,#55781,.F.);
#81938=ORIENTED_EDGE('',*,*,#55805,.T.);
#81939=ORIENTED_EDGE('',*,*,#55098,.F.);
#81940=ORIENTED_EDGE('',*,*,#55807,.T.);
#81941=ORIENTED_EDGE('',*,*,#55782,.F.);
#81942=ORIENTED_EDGE('',*,*,#55806,.F.);
#81943=ORIENTED_EDGE('',*,*,#54744,.F.);
#81944=ORIENTED_EDGE('',*,*,#54173,.T.);
#81945=ORIENTED_EDGE('',*,*,#55798,.T.);
#81946=ORIENTED_EDGE('',*,*,#55807,.F.);
#81947=ORIENTED_EDGE('',*,*,#54743,.T.);
#81948=ORIENTED_EDGE('',*,*,#55797,.T.);
#81949=ORIENTED_EDGE('',*,*,#55799,.T.);
#81950=ORIENTED_EDGE('',*,*,#54172,.T.);
#81951=ORIENTED_EDGE('',*,*,#55795,.T.);
#81952=ORIENTED_EDGE('',*,*,#55808,.T.);
#81953=ORIENTED_EDGE('',*,*,#55809,.T.);
#81954=ORIENTED_EDGE('',*,*,#55810,.T.);
#81955=ORIENTED_EDGE('',*,*,#55811,.T.);
#81956=ORIENTED_EDGE('',*,*,#55812,.T.);
#81957=ORIENTED_EDGE('',*,*,#55813,.T.);
#81958=ORIENTED_EDGE('',*,*,#55814,.T.);
#81959=ORIENTED_EDGE('',*,*,#55815,.F.);
#81960=ORIENTED_EDGE('',*,*,#55816,.T.);
#81961=ORIENTED_EDGE('',*,*,#55817,.T.);
#81962=ORIENTED_EDGE('',*,*,#55815,.T.);
#81963=ORIENTED_EDGE('',*,*,#55818,.T.);
#81964=ORIENTED_EDGE('',*,*,#55819,.T.);
#81965=ORIENTED_EDGE('',*,*,#55808,.F.);
#81966=ORIENTED_EDGE('',*,*,#55820,.T.);
#81967=ORIENTED_EDGE('',*,*,#55821,.T.);
#81968=ORIENTED_EDGE('',*,*,#55822,.F.);
#81969=ORIENTED_EDGE('',*,*,#55816,.F.);
#81970=ORIENTED_EDGE('',*,*,#55823,.F.);
#81971=ORIENTED_EDGE('',*,*,#55824,.F.);
#81972=ORIENTED_EDGE('',*,*,#55823,.T.);
#81973=ORIENTED_EDGE('',*,*,#55821,.F.);
#81974=ORIENTED_EDGE('',*,*,#55820,.F.);
#81975=ORIENTED_EDGE('',*,*,#55825,.F.);
#81976=ORIENTED_EDGE('',*,*,#55826,.F.);
#81977=ORIENTED_EDGE('',*,*,#55825,.T.);
#81978=ORIENTED_EDGE('',*,*,#55812,.F.);
#81979=ORIENTED_EDGE('',*,*,#55827,.F.);
#81980=ORIENTED_EDGE('',*,*,#55828,.F.);
#81981=ORIENTED_EDGE('',*,*,#55829,.T.);
#81982=ORIENTED_EDGE('',*,*,#55822,.T.);
#81983=ORIENTED_EDGE('',*,*,#54171,.F.);
#81984=ORIENTED_EDGE('',*,*,#54737,.T.);
#81985=ORIENTED_EDGE('',*,*,#55830,.F.);
#81986=ORIENTED_EDGE('',*,*,#55817,.F.);
#81987=ORIENTED_EDGE('',*,*,#55829,.F.);
#81988=ORIENTED_EDGE('',*,*,#54736,.F.);
#81989=ORIENTED_EDGE('',*,*,#55830,.T.);
#81990=ORIENTED_EDGE('',*,*,#55095,.F.);
#81991=ORIENTED_EDGE('',*,*,#55831,.F.);
#81992=ORIENTED_EDGE('',*,*,#55813,.F.);
#81993=ORIENTED_EDGE('',*,*,#55831,.T.);
#81994=ORIENTED_EDGE('',*,*,#54330,.F.);
#81995=ORIENTED_EDGE('',*,*,#55832,.F.);
#81996=ORIENTED_EDGE('',*,*,#55814,.F.);
#81997=ORIENTED_EDGE('',*,*,#55832,.T.);
#81998=ORIENTED_EDGE('',*,*,#54329,.F.);
#81999=ORIENTED_EDGE('',*,*,#55833,.F.);
#82000=ORIENTED_EDGE('',*,*,#55819,.F.);
#82001=ORIENTED_EDGE('',*,*,#55818,.F.);
#82002=ORIENTED_EDGE('',*,*,#55833,.T.);
#82003=ORIENTED_EDGE('',*,*,#54328,.F.);
#82004=ORIENTED_EDGE('',*,*,#55834,.F.);
#82005=ORIENTED_EDGE('',*,*,#55809,.F.);
#82006=ORIENTED_EDGE('',*,*,#55835,.T.);
#82007=ORIENTED_EDGE('',*,*,#55810,.F.);
#82008=ORIENTED_EDGE('',*,*,#55834,.T.);
#82009=ORIENTED_EDGE('',*,*,#55096,.F.);
#82010=ORIENTED_EDGE('',*,*,#55836,.T.);
#82011=ORIENTED_EDGE('',*,*,#55811,.F.);
#82012=ORIENTED_EDGE('',*,*,#55835,.F.);
#82013=ORIENTED_EDGE('',*,*,#54739,.F.);
#82014=ORIENTED_EDGE('',*,*,#54169,.T.);
#82015=ORIENTED_EDGE('',*,*,#55827,.T.);
#82016=ORIENTED_EDGE('',*,*,#55836,.F.);
#82017=ORIENTED_EDGE('',*,*,#54738,.T.);
#82018=ORIENTED_EDGE('',*,*,#55826,.T.);
#82019=ORIENTED_EDGE('',*,*,#55828,.T.);
#82020=ORIENTED_EDGE('',*,*,#54168,.T.);
#82021=ORIENTED_EDGE('',*,*,#55824,.T.);
#82022=ORIENTED_EDGE('',*,*,#55837,.T.);
#82023=ORIENTED_EDGE('',*,*,#55838,.T.);
#82024=ORIENTED_EDGE('',*,*,#55839,.T.);
#82025=ORIENTED_EDGE('',*,*,#55840,.T.);
#82026=ORIENTED_EDGE('',*,*,#55841,.T.);
#82027=ORIENTED_EDGE('',*,*,#55842,.T.);
#82028=ORIENTED_EDGE('',*,*,#55843,.T.);
#82029=ORIENTED_EDGE('',*,*,#55844,.F.);
#82030=ORIENTED_EDGE('',*,*,#55845,.T.);
#82031=ORIENTED_EDGE('',*,*,#55846,.T.);
#82032=ORIENTED_EDGE('',*,*,#55844,.T.);
#82033=ORIENTED_EDGE('',*,*,#55847,.T.);
#82034=ORIENTED_EDGE('',*,*,#55848,.T.);
#82035=ORIENTED_EDGE('',*,*,#55837,.F.);
#82036=ORIENTED_EDGE('',*,*,#55849,.T.);
#82037=ORIENTED_EDGE('',*,*,#55850,.T.);
#82038=ORIENTED_EDGE('',*,*,#55851,.F.);
#82039=ORIENTED_EDGE('',*,*,#55845,.F.);
#82040=ORIENTED_EDGE('',*,*,#55852,.F.);
#82041=ORIENTED_EDGE('',*,*,#55853,.F.);
#82042=ORIENTED_EDGE('',*,*,#55852,.T.);
#82043=ORIENTED_EDGE('',*,*,#55850,.F.);
#82044=ORIENTED_EDGE('',*,*,#55849,.F.);
#82045=ORIENTED_EDGE('',*,*,#55854,.F.);
#82046=ORIENTED_EDGE('',*,*,#55855,.F.);
#82047=ORIENTED_EDGE('',*,*,#55854,.T.);
#82048=ORIENTED_EDGE('',*,*,#55841,.F.);
#82049=ORIENTED_EDGE('',*,*,#55856,.F.);
#82050=ORIENTED_EDGE('',*,*,#55857,.F.);
#82051=ORIENTED_EDGE('',*,*,#55858,.T.);
#82052=ORIENTED_EDGE('',*,*,#55851,.T.);
#82053=ORIENTED_EDGE('',*,*,#54167,.F.);
#82054=ORIENTED_EDGE('',*,*,#54732,.T.);
#82055=ORIENTED_EDGE('',*,*,#55859,.F.);
#82056=ORIENTED_EDGE('',*,*,#55846,.F.);
#82057=ORIENTED_EDGE('',*,*,#55858,.F.);
#82058=ORIENTED_EDGE('',*,*,#54731,.F.);
#82059=ORIENTED_EDGE('',*,*,#55859,.T.);
#82060=ORIENTED_EDGE('',*,*,#55093,.F.);
#82061=ORIENTED_EDGE('',*,*,#55860,.F.);
#82062=ORIENTED_EDGE('',*,*,#55842,.F.);
#82063=ORIENTED_EDGE('',*,*,#55860,.T.);
#82064=ORIENTED_EDGE('',*,*,#54334,.F.);
#82065=ORIENTED_EDGE('',*,*,#55861,.F.);
#82066=ORIENTED_EDGE('',*,*,#55843,.F.);
#82067=ORIENTED_EDGE('',*,*,#55861,.T.);
#82068=ORIENTED_EDGE('',*,*,#54333,.F.);
#82069=ORIENTED_EDGE('',*,*,#55862,.F.);
#82070=ORIENTED_EDGE('',*,*,#55848,.F.);
#82071=ORIENTED_EDGE('',*,*,#55847,.F.);
#82072=ORIENTED_EDGE('',*,*,#55862,.T.);
#82073=ORIENTED_EDGE('',*,*,#54332,.F.);
#82074=ORIENTED_EDGE('',*,*,#55863,.F.);
#82075=ORIENTED_EDGE('',*,*,#55838,.F.);
#82076=ORIENTED_EDGE('',*,*,#55864,.T.);
#82077=ORIENTED_EDGE('',*,*,#55839,.F.);
#82078=ORIENTED_EDGE('',*,*,#55863,.T.);
#82079=ORIENTED_EDGE('',*,*,#55094,.F.);
#82080=ORIENTED_EDGE('',*,*,#55865,.T.);
#82081=ORIENTED_EDGE('',*,*,#55840,.F.);
#82082=ORIENTED_EDGE('',*,*,#55864,.F.);
#82083=ORIENTED_EDGE('',*,*,#54734,.F.);
#82084=ORIENTED_EDGE('',*,*,#54165,.T.);
#82085=ORIENTED_EDGE('',*,*,#55856,.T.);
#82086=ORIENTED_EDGE('',*,*,#55865,.F.);
#82087=ORIENTED_EDGE('',*,*,#54733,.T.);
#82088=ORIENTED_EDGE('',*,*,#55855,.T.);
#82089=ORIENTED_EDGE('',*,*,#55857,.T.);
#82090=ORIENTED_EDGE('',*,*,#54164,.T.);
#82091=ORIENTED_EDGE('',*,*,#55853,.T.);
#82092=ORIENTED_EDGE('',*,*,#55866,.T.);
#82093=ORIENTED_EDGE('',*,*,#55867,.T.);
#82094=ORIENTED_EDGE('',*,*,#55868,.T.);
#82095=ORIENTED_EDGE('',*,*,#55869,.T.);
#82096=ORIENTED_EDGE('',*,*,#55870,.T.);
#82097=ORIENTED_EDGE('',*,*,#55871,.T.);
#82098=ORIENTED_EDGE('',*,*,#55872,.T.);
#82099=ORIENTED_EDGE('',*,*,#55873,.F.);
#82100=ORIENTED_EDGE('',*,*,#55874,.T.);
#82101=ORIENTED_EDGE('',*,*,#55875,.T.);
#82102=ORIENTED_EDGE('',*,*,#55873,.T.);
#82103=ORIENTED_EDGE('',*,*,#55876,.T.);
#82104=ORIENTED_EDGE('',*,*,#55877,.T.);
#82105=ORIENTED_EDGE('',*,*,#55866,.F.);
#82106=ORIENTED_EDGE('',*,*,#55878,.T.);
#82107=ORIENTED_EDGE('',*,*,#55879,.T.);
#82108=ORIENTED_EDGE('',*,*,#55880,.F.);
#82109=ORIENTED_EDGE('',*,*,#55874,.F.);
#82110=ORIENTED_EDGE('',*,*,#55881,.F.);
#82111=ORIENTED_EDGE('',*,*,#55882,.F.);
#82112=ORIENTED_EDGE('',*,*,#55881,.T.);
#82113=ORIENTED_EDGE('',*,*,#55879,.F.);
#82114=ORIENTED_EDGE('',*,*,#55878,.F.);
#82115=ORIENTED_EDGE('',*,*,#55883,.F.);
#82116=ORIENTED_EDGE('',*,*,#55884,.F.);
#82117=ORIENTED_EDGE('',*,*,#55883,.T.);
#82118=ORIENTED_EDGE('',*,*,#55870,.F.);
#82119=ORIENTED_EDGE('',*,*,#55885,.F.);
#82120=ORIENTED_EDGE('',*,*,#55886,.F.);
#82121=ORIENTED_EDGE('',*,*,#55887,.T.);
#82122=ORIENTED_EDGE('',*,*,#55880,.T.);
#82123=ORIENTED_EDGE('',*,*,#54163,.F.);
#82124=ORIENTED_EDGE('',*,*,#54727,.T.);
#82125=ORIENTED_EDGE('',*,*,#55888,.F.);
#82126=ORIENTED_EDGE('',*,*,#55875,.F.);
#82127=ORIENTED_EDGE('',*,*,#55887,.F.);
#82128=ORIENTED_EDGE('',*,*,#54726,.F.);
#82129=ORIENTED_EDGE('',*,*,#55888,.T.);
#82130=ORIENTED_EDGE('',*,*,#55091,.F.);
#82131=ORIENTED_EDGE('',*,*,#55889,.F.);
#82132=ORIENTED_EDGE('',*,*,#55871,.F.);
#82133=ORIENTED_EDGE('',*,*,#55889,.T.);
#82134=ORIENTED_EDGE('',*,*,#54338,.F.);
#82135=ORIENTED_EDGE('',*,*,#55890,.F.);
#82136=ORIENTED_EDGE('',*,*,#55872,.F.);
#82137=ORIENTED_EDGE('',*,*,#55890,.T.);
#82138=ORIENTED_EDGE('',*,*,#54337,.F.);
#82139=ORIENTED_EDGE('',*,*,#55891,.F.);
#82140=ORIENTED_EDGE('',*,*,#55877,.F.);
#82141=ORIENTED_EDGE('',*,*,#55876,.F.);
#82142=ORIENTED_EDGE('',*,*,#55891,.T.);
#82143=ORIENTED_EDGE('',*,*,#54336,.F.);
#82144=ORIENTED_EDGE('',*,*,#55892,.F.);
#82145=ORIENTED_EDGE('',*,*,#55867,.F.);
#82146=ORIENTED_EDGE('',*,*,#55893,.T.);
#82147=ORIENTED_EDGE('',*,*,#55868,.F.);
#82148=ORIENTED_EDGE('',*,*,#55892,.T.);
#82149=ORIENTED_EDGE('',*,*,#55092,.F.);
#82150=ORIENTED_EDGE('',*,*,#55894,.T.);
#82151=ORIENTED_EDGE('',*,*,#55869,.F.);
#82152=ORIENTED_EDGE('',*,*,#55893,.F.);
#82153=ORIENTED_EDGE('',*,*,#54729,.F.);
#82154=ORIENTED_EDGE('',*,*,#54161,.T.);
#82155=ORIENTED_EDGE('',*,*,#55885,.T.);
#82156=ORIENTED_EDGE('',*,*,#55894,.F.);
#82157=ORIENTED_EDGE('',*,*,#54728,.T.);
#82158=ORIENTED_EDGE('',*,*,#55884,.T.);
#82159=ORIENTED_EDGE('',*,*,#55886,.T.);
#82160=ORIENTED_EDGE('',*,*,#54160,.T.);
#82161=ORIENTED_EDGE('',*,*,#55882,.T.);
#82162=ORIENTED_EDGE('',*,*,#55895,.T.);
#82163=ORIENTED_EDGE('',*,*,#55896,.T.);
#82164=ORIENTED_EDGE('',*,*,#55897,.T.);
#82165=ORIENTED_EDGE('',*,*,#55898,.T.);
#82166=ORIENTED_EDGE('',*,*,#55899,.T.);
#82167=ORIENTED_EDGE('',*,*,#55900,.T.);
#82168=ORIENTED_EDGE('',*,*,#55901,.T.);
#82169=ORIENTED_EDGE('',*,*,#55902,.F.);
#82170=ORIENTED_EDGE('',*,*,#55903,.T.);
#82171=ORIENTED_EDGE('',*,*,#55904,.T.);
#82172=ORIENTED_EDGE('',*,*,#55902,.T.);
#82173=ORIENTED_EDGE('',*,*,#55905,.T.);
#82174=ORIENTED_EDGE('',*,*,#55906,.T.);
#82175=ORIENTED_EDGE('',*,*,#55895,.F.);
#82176=ORIENTED_EDGE('',*,*,#55907,.T.);
#82177=ORIENTED_EDGE('',*,*,#55908,.T.);
#82178=ORIENTED_EDGE('',*,*,#55909,.F.);
#82179=ORIENTED_EDGE('',*,*,#55903,.F.);
#82180=ORIENTED_EDGE('',*,*,#55910,.F.);
#82181=ORIENTED_EDGE('',*,*,#55911,.F.);
#82182=ORIENTED_EDGE('',*,*,#55910,.T.);
#82183=ORIENTED_EDGE('',*,*,#55908,.F.);
#82184=ORIENTED_EDGE('',*,*,#55907,.F.);
#82185=ORIENTED_EDGE('',*,*,#55912,.F.);
#82186=ORIENTED_EDGE('',*,*,#55913,.F.);
#82187=ORIENTED_EDGE('',*,*,#55912,.T.);
#82188=ORIENTED_EDGE('',*,*,#55899,.F.);
#82189=ORIENTED_EDGE('',*,*,#55914,.F.);
#82190=ORIENTED_EDGE('',*,*,#55915,.F.);
#82191=ORIENTED_EDGE('',*,*,#55916,.T.);
#82192=ORIENTED_EDGE('',*,*,#55909,.T.);
#82193=ORIENTED_EDGE('',*,*,#54159,.F.);
#82194=ORIENTED_EDGE('',*,*,#54722,.T.);
#82195=ORIENTED_EDGE('',*,*,#55917,.F.);
#82196=ORIENTED_EDGE('',*,*,#55904,.F.);
#82197=ORIENTED_EDGE('',*,*,#55916,.F.);
#82198=ORIENTED_EDGE('',*,*,#54721,.F.);
#82199=ORIENTED_EDGE('',*,*,#55917,.T.);
#82200=ORIENTED_EDGE('',*,*,#55089,.F.);
#82201=ORIENTED_EDGE('',*,*,#55918,.F.);
#82202=ORIENTED_EDGE('',*,*,#55900,.F.);
#82203=ORIENTED_EDGE('',*,*,#55918,.T.);
#82204=ORIENTED_EDGE('',*,*,#54342,.F.);
#82205=ORIENTED_EDGE('',*,*,#55919,.F.);
#82206=ORIENTED_EDGE('',*,*,#55901,.F.);
#82207=ORIENTED_EDGE('',*,*,#55919,.T.);
#82208=ORIENTED_EDGE('',*,*,#54341,.F.);
#82209=ORIENTED_EDGE('',*,*,#55920,.F.);
#82210=ORIENTED_EDGE('',*,*,#55906,.F.);
#82211=ORIENTED_EDGE('',*,*,#55905,.F.);
#82212=ORIENTED_EDGE('',*,*,#55920,.T.);
#82213=ORIENTED_EDGE('',*,*,#54340,.F.);
#82214=ORIENTED_EDGE('',*,*,#55921,.F.);
#82215=ORIENTED_EDGE('',*,*,#55896,.F.);
#82216=ORIENTED_EDGE('',*,*,#55922,.T.);
#82217=ORIENTED_EDGE('',*,*,#55897,.F.);
#82218=ORIENTED_EDGE('',*,*,#55921,.T.);
#82219=ORIENTED_EDGE('',*,*,#55090,.F.);
#82220=ORIENTED_EDGE('',*,*,#55923,.T.);
#82221=ORIENTED_EDGE('',*,*,#55898,.F.);
#82222=ORIENTED_EDGE('',*,*,#55922,.F.);
#82223=ORIENTED_EDGE('',*,*,#54724,.F.);
#82224=ORIENTED_EDGE('',*,*,#54157,.T.);
#82225=ORIENTED_EDGE('',*,*,#55914,.T.);
#82226=ORIENTED_EDGE('',*,*,#55923,.F.);
#82227=ORIENTED_EDGE('',*,*,#54723,.T.);
#82228=ORIENTED_EDGE('',*,*,#55913,.T.);
#82229=ORIENTED_EDGE('',*,*,#55915,.T.);
#82230=ORIENTED_EDGE('',*,*,#54156,.T.);
#82231=ORIENTED_EDGE('',*,*,#55911,.T.);
#82232=ORIENTED_EDGE('',*,*,#55924,.T.);
#82233=ORIENTED_EDGE('',*,*,#55925,.T.);
#82234=ORIENTED_EDGE('',*,*,#55926,.T.);
#82235=ORIENTED_EDGE('',*,*,#55927,.T.);
#82236=ORIENTED_EDGE('',*,*,#55928,.T.);
#82237=ORIENTED_EDGE('',*,*,#55929,.T.);
#82238=ORIENTED_EDGE('',*,*,#55930,.T.);
#82239=ORIENTED_EDGE('',*,*,#55931,.F.);
#82240=ORIENTED_EDGE('',*,*,#55932,.T.);
#82241=ORIENTED_EDGE('',*,*,#55933,.T.);
#82242=ORIENTED_EDGE('',*,*,#55931,.T.);
#82243=ORIENTED_EDGE('',*,*,#55934,.T.);
#82244=ORIENTED_EDGE('',*,*,#55935,.T.);
#82245=ORIENTED_EDGE('',*,*,#55924,.F.);
#82246=ORIENTED_EDGE('',*,*,#55936,.T.);
#82247=ORIENTED_EDGE('',*,*,#55937,.T.);
#82248=ORIENTED_EDGE('',*,*,#55938,.F.);
#82249=ORIENTED_EDGE('',*,*,#55932,.F.);
#82250=ORIENTED_EDGE('',*,*,#55939,.F.);
#82251=ORIENTED_EDGE('',*,*,#55940,.F.);
#82252=ORIENTED_EDGE('',*,*,#55939,.T.);
#82253=ORIENTED_EDGE('',*,*,#55937,.F.);
#82254=ORIENTED_EDGE('',*,*,#55936,.F.);
#82255=ORIENTED_EDGE('',*,*,#55941,.F.);
#82256=ORIENTED_EDGE('',*,*,#55942,.F.);
#82257=ORIENTED_EDGE('',*,*,#55941,.T.);
#82258=ORIENTED_EDGE('',*,*,#55928,.F.);
#82259=ORIENTED_EDGE('',*,*,#55943,.F.);
#82260=ORIENTED_EDGE('',*,*,#55944,.F.);
#82261=ORIENTED_EDGE('',*,*,#55945,.T.);
#82262=ORIENTED_EDGE('',*,*,#55938,.T.);
#82263=ORIENTED_EDGE('',*,*,#54155,.F.);
#82264=ORIENTED_EDGE('',*,*,#54717,.T.);
#82265=ORIENTED_EDGE('',*,*,#55946,.F.);
#82266=ORIENTED_EDGE('',*,*,#55933,.F.);
#82267=ORIENTED_EDGE('',*,*,#55945,.F.);
#82268=ORIENTED_EDGE('',*,*,#54716,.F.);
#82269=ORIENTED_EDGE('',*,*,#55946,.T.);
#82270=ORIENTED_EDGE('',*,*,#55087,.F.);
#82271=ORIENTED_EDGE('',*,*,#55947,.F.);
#82272=ORIENTED_EDGE('',*,*,#55929,.F.);
#82273=ORIENTED_EDGE('',*,*,#55947,.T.);
#82274=ORIENTED_EDGE('',*,*,#54346,.F.);
#82275=ORIENTED_EDGE('',*,*,#55948,.F.);
#82276=ORIENTED_EDGE('',*,*,#55930,.F.);
#82277=ORIENTED_EDGE('',*,*,#55948,.T.);
#82278=ORIENTED_EDGE('',*,*,#54345,.F.);
#82279=ORIENTED_EDGE('',*,*,#55949,.F.);
#82280=ORIENTED_EDGE('',*,*,#55935,.F.);
#82281=ORIENTED_EDGE('',*,*,#55934,.F.);
#82282=ORIENTED_EDGE('',*,*,#55949,.T.);
#82283=ORIENTED_EDGE('',*,*,#54344,.F.);
#82284=ORIENTED_EDGE('',*,*,#55950,.F.);
#82285=ORIENTED_EDGE('',*,*,#55925,.F.);
#82286=ORIENTED_EDGE('',*,*,#55951,.T.);
#82287=ORIENTED_EDGE('',*,*,#55926,.F.);
#82288=ORIENTED_EDGE('',*,*,#55950,.T.);
#82289=ORIENTED_EDGE('',*,*,#55088,.F.);
#82290=ORIENTED_EDGE('',*,*,#55952,.T.);
#82291=ORIENTED_EDGE('',*,*,#55927,.F.);
#82292=ORIENTED_EDGE('',*,*,#55951,.F.);
#82293=ORIENTED_EDGE('',*,*,#54719,.F.);
#82294=ORIENTED_EDGE('',*,*,#54153,.T.);
#82295=ORIENTED_EDGE('',*,*,#55943,.T.);
#82296=ORIENTED_EDGE('',*,*,#55952,.F.);
#82297=ORIENTED_EDGE('',*,*,#54718,.T.);
#82298=ORIENTED_EDGE('',*,*,#55942,.T.);
#82299=ORIENTED_EDGE('',*,*,#55944,.T.);
#82300=ORIENTED_EDGE('',*,*,#54152,.T.);
#82301=ORIENTED_EDGE('',*,*,#55940,.T.);
#82302=ORIENTED_EDGE('',*,*,#55953,.T.);
#82303=ORIENTED_EDGE('',*,*,#55954,.T.);
#82304=ORIENTED_EDGE('',*,*,#55955,.T.);
#82305=ORIENTED_EDGE('',*,*,#55956,.T.);
#82306=ORIENTED_EDGE('',*,*,#55957,.T.);
#82307=ORIENTED_EDGE('',*,*,#55958,.T.);
#82308=ORIENTED_EDGE('',*,*,#55959,.T.);
#82309=ORIENTED_EDGE('',*,*,#55960,.F.);
#82310=ORIENTED_EDGE('',*,*,#55961,.T.);
#82311=ORIENTED_EDGE('',*,*,#55962,.T.);
#82312=ORIENTED_EDGE('',*,*,#55960,.T.);
#82313=ORIENTED_EDGE('',*,*,#55963,.T.);
#82314=ORIENTED_EDGE('',*,*,#55964,.T.);
#82315=ORIENTED_EDGE('',*,*,#55953,.F.);
#82316=ORIENTED_EDGE('',*,*,#55965,.T.);
#82317=ORIENTED_EDGE('',*,*,#55966,.T.);
#82318=ORIENTED_EDGE('',*,*,#55967,.F.);
#82319=ORIENTED_EDGE('',*,*,#55961,.F.);
#82320=ORIENTED_EDGE('',*,*,#55968,.F.);
#82321=ORIENTED_EDGE('',*,*,#55969,.F.);
#82322=ORIENTED_EDGE('',*,*,#55968,.T.);
#82323=ORIENTED_EDGE('',*,*,#55966,.F.);
#82324=ORIENTED_EDGE('',*,*,#55965,.F.);
#82325=ORIENTED_EDGE('',*,*,#55970,.F.);
#82326=ORIENTED_EDGE('',*,*,#55971,.F.);
#82327=ORIENTED_EDGE('',*,*,#55970,.T.);
#82328=ORIENTED_EDGE('',*,*,#55957,.F.);
#82329=ORIENTED_EDGE('',*,*,#55972,.F.);
#82330=ORIENTED_EDGE('',*,*,#55973,.F.);
#82331=ORIENTED_EDGE('',*,*,#55974,.T.);
#82332=ORIENTED_EDGE('',*,*,#55967,.T.);
#82333=ORIENTED_EDGE('',*,*,#54151,.F.);
#82334=ORIENTED_EDGE('',*,*,#54712,.T.);
#82335=ORIENTED_EDGE('',*,*,#55975,.F.);
#82336=ORIENTED_EDGE('',*,*,#55962,.F.);
#82337=ORIENTED_EDGE('',*,*,#55974,.F.);
#82338=ORIENTED_EDGE('',*,*,#54711,.F.);
#82339=ORIENTED_EDGE('',*,*,#55975,.T.);
#82340=ORIENTED_EDGE('',*,*,#55085,.F.);
#82341=ORIENTED_EDGE('',*,*,#55976,.F.);
#82342=ORIENTED_EDGE('',*,*,#55958,.F.);
#82343=ORIENTED_EDGE('',*,*,#55976,.T.);
#82344=ORIENTED_EDGE('',*,*,#54350,.F.);
#82345=ORIENTED_EDGE('',*,*,#55977,.F.);
#82346=ORIENTED_EDGE('',*,*,#55959,.F.);
#82347=ORIENTED_EDGE('',*,*,#55977,.T.);
#82348=ORIENTED_EDGE('',*,*,#54349,.F.);
#82349=ORIENTED_EDGE('',*,*,#55978,.F.);
#82350=ORIENTED_EDGE('',*,*,#55964,.F.);
#82351=ORIENTED_EDGE('',*,*,#55963,.F.);
#82352=ORIENTED_EDGE('',*,*,#55978,.T.);
#82353=ORIENTED_EDGE('',*,*,#54348,.F.);
#82354=ORIENTED_EDGE('',*,*,#55979,.F.);
#82355=ORIENTED_EDGE('',*,*,#55954,.F.);
#82356=ORIENTED_EDGE('',*,*,#55980,.T.);
#82357=ORIENTED_EDGE('',*,*,#55955,.F.);
#82358=ORIENTED_EDGE('',*,*,#55979,.T.);
#82359=ORIENTED_EDGE('',*,*,#55086,.F.);
#82360=ORIENTED_EDGE('',*,*,#55981,.T.);
#82361=ORIENTED_EDGE('',*,*,#55956,.F.);
#82362=ORIENTED_EDGE('',*,*,#55980,.F.);
#82363=ORIENTED_EDGE('',*,*,#54714,.F.);
#82364=ORIENTED_EDGE('',*,*,#54149,.T.);
#82365=ORIENTED_EDGE('',*,*,#55972,.T.);
#82366=ORIENTED_EDGE('',*,*,#55981,.F.);
#82367=ORIENTED_EDGE('',*,*,#54713,.T.);
#82368=ORIENTED_EDGE('',*,*,#55971,.T.);
#82369=ORIENTED_EDGE('',*,*,#55973,.T.);
#82370=ORIENTED_EDGE('',*,*,#54148,.T.);
#82371=ORIENTED_EDGE('',*,*,#55969,.T.);
#82372=ORIENTED_EDGE('',*,*,#55982,.T.);
#82373=ORIENTED_EDGE('',*,*,#55983,.T.);
#82374=ORIENTED_EDGE('',*,*,#55984,.T.);
#82375=ORIENTED_EDGE('',*,*,#55985,.T.);
#82376=ORIENTED_EDGE('',*,*,#55986,.T.);
#82377=ORIENTED_EDGE('',*,*,#55987,.T.);
#82378=ORIENTED_EDGE('',*,*,#55988,.T.);
#82379=ORIENTED_EDGE('',*,*,#55989,.F.);
#82380=ORIENTED_EDGE('',*,*,#55990,.T.);
#82381=ORIENTED_EDGE('',*,*,#55991,.T.);
#82382=ORIENTED_EDGE('',*,*,#55989,.T.);
#82383=ORIENTED_EDGE('',*,*,#55992,.T.);
#82384=ORIENTED_EDGE('',*,*,#55993,.T.);
#82385=ORIENTED_EDGE('',*,*,#55982,.F.);
#82386=ORIENTED_EDGE('',*,*,#55994,.T.);
#82387=ORIENTED_EDGE('',*,*,#55995,.T.);
#82388=ORIENTED_EDGE('',*,*,#55996,.F.);
#82389=ORIENTED_EDGE('',*,*,#55990,.F.);
#82390=ORIENTED_EDGE('',*,*,#55997,.F.);
#82391=ORIENTED_EDGE('',*,*,#55998,.F.);
#82392=ORIENTED_EDGE('',*,*,#55997,.T.);
#82393=ORIENTED_EDGE('',*,*,#55995,.F.);
#82394=ORIENTED_EDGE('',*,*,#55994,.F.);
#82395=ORIENTED_EDGE('',*,*,#55999,.F.);
#82396=ORIENTED_EDGE('',*,*,#56000,.F.);
#82397=ORIENTED_EDGE('',*,*,#55999,.T.);
#82398=ORIENTED_EDGE('',*,*,#55986,.F.);
#82399=ORIENTED_EDGE('',*,*,#56001,.F.);
#82400=ORIENTED_EDGE('',*,*,#56002,.F.);
#82401=ORIENTED_EDGE('',*,*,#56003,.T.);
#82402=ORIENTED_EDGE('',*,*,#55996,.T.);
#82403=ORIENTED_EDGE('',*,*,#54147,.F.);
#82404=ORIENTED_EDGE('',*,*,#54707,.T.);
#82405=ORIENTED_EDGE('',*,*,#56004,.F.);
#82406=ORIENTED_EDGE('',*,*,#55991,.F.);
#82407=ORIENTED_EDGE('',*,*,#56003,.F.);
#82408=ORIENTED_EDGE('',*,*,#54706,.F.);
#82409=ORIENTED_EDGE('',*,*,#56004,.T.);
#82410=ORIENTED_EDGE('',*,*,#55083,.F.);
#82411=ORIENTED_EDGE('',*,*,#56005,.F.);
#82412=ORIENTED_EDGE('',*,*,#55987,.F.);
#82413=ORIENTED_EDGE('',*,*,#56005,.T.);
#82414=ORIENTED_EDGE('',*,*,#54354,.F.);
#82415=ORIENTED_EDGE('',*,*,#56006,.F.);
#82416=ORIENTED_EDGE('',*,*,#55988,.F.);
#82417=ORIENTED_EDGE('',*,*,#56006,.T.);
#82418=ORIENTED_EDGE('',*,*,#54353,.F.);
#82419=ORIENTED_EDGE('',*,*,#56007,.F.);
#82420=ORIENTED_EDGE('',*,*,#55993,.F.);
#82421=ORIENTED_EDGE('',*,*,#55992,.F.);
#82422=ORIENTED_EDGE('',*,*,#56007,.T.);
#82423=ORIENTED_EDGE('',*,*,#54352,.F.);
#82424=ORIENTED_EDGE('',*,*,#56008,.F.);
#82425=ORIENTED_EDGE('',*,*,#55983,.F.);
#82426=ORIENTED_EDGE('',*,*,#56009,.T.);
#82427=ORIENTED_EDGE('',*,*,#55984,.F.);
#82428=ORIENTED_EDGE('',*,*,#56008,.T.);
#82429=ORIENTED_EDGE('',*,*,#55084,.F.);
#82430=ORIENTED_EDGE('',*,*,#56010,.T.);
#82431=ORIENTED_EDGE('',*,*,#55985,.F.);
#82432=ORIENTED_EDGE('',*,*,#56009,.F.);
#82433=ORIENTED_EDGE('',*,*,#54709,.F.);
#82434=ORIENTED_EDGE('',*,*,#54145,.T.);
#82435=ORIENTED_EDGE('',*,*,#56001,.T.);
#82436=ORIENTED_EDGE('',*,*,#56010,.F.);
#82437=ORIENTED_EDGE('',*,*,#54708,.T.);
#82438=ORIENTED_EDGE('',*,*,#56000,.T.);
#82439=ORIENTED_EDGE('',*,*,#56002,.T.);
#82440=ORIENTED_EDGE('',*,*,#54144,.T.);
#82441=ORIENTED_EDGE('',*,*,#55998,.T.);
#82442=ORIENTED_EDGE('',*,*,#56011,.T.);
#82443=ORIENTED_EDGE('',*,*,#56012,.T.);
#82444=ORIENTED_EDGE('',*,*,#56013,.T.);
#82445=ORIENTED_EDGE('',*,*,#56014,.T.);
#82446=ORIENTED_EDGE('',*,*,#56015,.T.);
#82447=ORIENTED_EDGE('',*,*,#56016,.T.);
#82448=ORIENTED_EDGE('',*,*,#56017,.T.);
#82449=ORIENTED_EDGE('',*,*,#56018,.F.);
#82450=ORIENTED_EDGE('',*,*,#56019,.T.);
#82451=ORIENTED_EDGE('',*,*,#56020,.T.);
#82452=ORIENTED_EDGE('',*,*,#56018,.T.);
#82453=ORIENTED_EDGE('',*,*,#56021,.T.);
#82454=ORIENTED_EDGE('',*,*,#56022,.T.);
#82455=ORIENTED_EDGE('',*,*,#56011,.F.);
#82456=ORIENTED_EDGE('',*,*,#56023,.T.);
#82457=ORIENTED_EDGE('',*,*,#56024,.T.);
#82458=ORIENTED_EDGE('',*,*,#56025,.F.);
#82459=ORIENTED_EDGE('',*,*,#56019,.F.);
#82460=ORIENTED_EDGE('',*,*,#56026,.F.);
#82461=ORIENTED_EDGE('',*,*,#56027,.F.);
#82462=ORIENTED_EDGE('',*,*,#56026,.T.);
#82463=ORIENTED_EDGE('',*,*,#56024,.F.);
#82464=ORIENTED_EDGE('',*,*,#56023,.F.);
#82465=ORIENTED_EDGE('',*,*,#56028,.F.);
#82466=ORIENTED_EDGE('',*,*,#56029,.F.);
#82467=ORIENTED_EDGE('',*,*,#56028,.T.);
#82468=ORIENTED_EDGE('',*,*,#56015,.F.);
#82469=ORIENTED_EDGE('',*,*,#56030,.F.);
#82470=ORIENTED_EDGE('',*,*,#56031,.F.);
#82471=ORIENTED_EDGE('',*,*,#56032,.T.);
#82472=ORIENTED_EDGE('',*,*,#56025,.T.);
#82473=ORIENTED_EDGE('',*,*,#54143,.F.);
#82474=ORIENTED_EDGE('',*,*,#54702,.T.);
#82475=ORIENTED_EDGE('',*,*,#56033,.F.);
#82476=ORIENTED_EDGE('',*,*,#56020,.F.);
#82477=ORIENTED_EDGE('',*,*,#56032,.F.);
#82478=ORIENTED_EDGE('',*,*,#54701,.F.);
#82479=ORIENTED_EDGE('',*,*,#56033,.T.);
#82480=ORIENTED_EDGE('',*,*,#55081,.F.);
#82481=ORIENTED_EDGE('',*,*,#56034,.F.);
#82482=ORIENTED_EDGE('',*,*,#56016,.F.);
#82483=ORIENTED_EDGE('',*,*,#56034,.T.);
#82484=ORIENTED_EDGE('',*,*,#54358,.F.);
#82485=ORIENTED_EDGE('',*,*,#56035,.F.);
#82486=ORIENTED_EDGE('',*,*,#56017,.F.);
#82487=ORIENTED_EDGE('',*,*,#56035,.T.);
#82488=ORIENTED_EDGE('',*,*,#54357,.F.);
#82489=ORIENTED_EDGE('',*,*,#56036,.F.);
#82490=ORIENTED_EDGE('',*,*,#56022,.F.);
#82491=ORIENTED_EDGE('',*,*,#56021,.F.);
#82492=ORIENTED_EDGE('',*,*,#56036,.T.);
#82493=ORIENTED_EDGE('',*,*,#54356,.F.);
#82494=ORIENTED_EDGE('',*,*,#56037,.F.);
#82495=ORIENTED_EDGE('',*,*,#56012,.F.);
#82496=ORIENTED_EDGE('',*,*,#56038,.T.);
#82497=ORIENTED_EDGE('',*,*,#56013,.F.);
#82498=ORIENTED_EDGE('',*,*,#56037,.T.);
#82499=ORIENTED_EDGE('',*,*,#55082,.F.);
#82500=ORIENTED_EDGE('',*,*,#56039,.T.);
#82501=ORIENTED_EDGE('',*,*,#56014,.F.);
#82502=ORIENTED_EDGE('',*,*,#56038,.F.);
#82503=ORIENTED_EDGE('',*,*,#54704,.F.);
#82504=ORIENTED_EDGE('',*,*,#54141,.T.);
#82505=ORIENTED_EDGE('',*,*,#56030,.T.);
#82506=ORIENTED_EDGE('',*,*,#56039,.F.);
#82507=ORIENTED_EDGE('',*,*,#54703,.T.);
#82508=ORIENTED_EDGE('',*,*,#56029,.T.);
#82509=ORIENTED_EDGE('',*,*,#56031,.T.);
#82510=ORIENTED_EDGE('',*,*,#54140,.T.);
#82511=ORIENTED_EDGE('',*,*,#56027,.T.);
#82512=ORIENTED_EDGE('',*,*,#56040,.T.);
#82513=ORIENTED_EDGE('',*,*,#56041,.T.);
#82514=ORIENTED_EDGE('',*,*,#56042,.T.);
#82515=ORIENTED_EDGE('',*,*,#56043,.T.);
#82516=ORIENTED_EDGE('',*,*,#56044,.T.);
#82517=ORIENTED_EDGE('',*,*,#56045,.T.);
#82518=ORIENTED_EDGE('',*,*,#56046,.T.);
#82519=ORIENTED_EDGE('',*,*,#56047,.F.);
#82520=ORIENTED_EDGE('',*,*,#56048,.T.);
#82521=ORIENTED_EDGE('',*,*,#56049,.T.);
#82522=ORIENTED_EDGE('',*,*,#56047,.T.);
#82523=ORIENTED_EDGE('',*,*,#56050,.T.);
#82524=ORIENTED_EDGE('',*,*,#56051,.T.);
#82525=ORIENTED_EDGE('',*,*,#56040,.F.);
#82526=ORIENTED_EDGE('',*,*,#56052,.T.);
#82527=ORIENTED_EDGE('',*,*,#56053,.T.);
#82528=ORIENTED_EDGE('',*,*,#56054,.F.);
#82529=ORIENTED_EDGE('',*,*,#56048,.F.);
#82530=ORIENTED_EDGE('',*,*,#56055,.F.);
#82531=ORIENTED_EDGE('',*,*,#56056,.F.);
#82532=ORIENTED_EDGE('',*,*,#56055,.T.);
#82533=ORIENTED_EDGE('',*,*,#56053,.F.);
#82534=ORIENTED_EDGE('',*,*,#56052,.F.);
#82535=ORIENTED_EDGE('',*,*,#56057,.F.);
#82536=ORIENTED_EDGE('',*,*,#56058,.F.);
#82537=ORIENTED_EDGE('',*,*,#56057,.T.);
#82538=ORIENTED_EDGE('',*,*,#56044,.F.);
#82539=ORIENTED_EDGE('',*,*,#56059,.F.);
#82540=ORIENTED_EDGE('',*,*,#56060,.F.);
#82541=ORIENTED_EDGE('',*,*,#56061,.T.);
#82542=ORIENTED_EDGE('',*,*,#56054,.T.);
#82543=ORIENTED_EDGE('',*,*,#54139,.F.);
#82544=ORIENTED_EDGE('',*,*,#54697,.T.);
#82545=ORIENTED_EDGE('',*,*,#56062,.F.);
#82546=ORIENTED_EDGE('',*,*,#56049,.F.);
#82547=ORIENTED_EDGE('',*,*,#56061,.F.);
#82548=ORIENTED_EDGE('',*,*,#54696,.F.);
#82549=ORIENTED_EDGE('',*,*,#56062,.T.);
#82550=ORIENTED_EDGE('',*,*,#55079,.F.);
#82551=ORIENTED_EDGE('',*,*,#56063,.F.);
#82552=ORIENTED_EDGE('',*,*,#56045,.F.);
#82553=ORIENTED_EDGE('',*,*,#56063,.T.);
#82554=ORIENTED_EDGE('',*,*,#54362,.F.);
#82555=ORIENTED_EDGE('',*,*,#56064,.F.);
#82556=ORIENTED_EDGE('',*,*,#56046,.F.);
#82557=ORIENTED_EDGE('',*,*,#56064,.T.);
#82558=ORIENTED_EDGE('',*,*,#54361,.F.);
#82559=ORIENTED_EDGE('',*,*,#56065,.F.);
#82560=ORIENTED_EDGE('',*,*,#56051,.F.);
#82561=ORIENTED_EDGE('',*,*,#56050,.F.);
#82562=ORIENTED_EDGE('',*,*,#56065,.T.);
#82563=ORIENTED_EDGE('',*,*,#54360,.F.);
#82564=ORIENTED_EDGE('',*,*,#56066,.F.);
#82565=ORIENTED_EDGE('',*,*,#56041,.F.);
#82566=ORIENTED_EDGE('',*,*,#56067,.T.);
#82567=ORIENTED_EDGE('',*,*,#56042,.F.);
#82568=ORIENTED_EDGE('',*,*,#56066,.T.);
#82569=ORIENTED_EDGE('',*,*,#55080,.F.);
#82570=ORIENTED_EDGE('',*,*,#56068,.T.);
#82571=ORIENTED_EDGE('',*,*,#56043,.F.);
#82572=ORIENTED_EDGE('',*,*,#56067,.F.);
#82573=ORIENTED_EDGE('',*,*,#54699,.F.);
#82574=ORIENTED_EDGE('',*,*,#54137,.T.);
#82575=ORIENTED_EDGE('',*,*,#56059,.T.);
#82576=ORIENTED_EDGE('',*,*,#56068,.F.);
#82577=ORIENTED_EDGE('',*,*,#54698,.T.);
#82578=ORIENTED_EDGE('',*,*,#56058,.T.);
#82579=ORIENTED_EDGE('',*,*,#56060,.T.);
#82580=ORIENTED_EDGE('',*,*,#54136,.T.);
#82581=ORIENTED_EDGE('',*,*,#56056,.T.);
#82582=ORIENTED_EDGE('',*,*,#56069,.T.);
#82583=ORIENTED_EDGE('',*,*,#56070,.T.);
#82584=ORIENTED_EDGE('',*,*,#56071,.T.);
#82585=ORIENTED_EDGE('',*,*,#56072,.T.);
#82586=ORIENTED_EDGE('',*,*,#56073,.T.);
#82587=ORIENTED_EDGE('',*,*,#56074,.T.);
#82588=ORIENTED_EDGE('',*,*,#56075,.T.);
#82589=ORIENTED_EDGE('',*,*,#56076,.F.);
#82590=ORIENTED_EDGE('',*,*,#56077,.T.);
#82591=ORIENTED_EDGE('',*,*,#56078,.T.);
#82592=ORIENTED_EDGE('',*,*,#56076,.T.);
#82593=ORIENTED_EDGE('',*,*,#56079,.T.);
#82594=ORIENTED_EDGE('',*,*,#56080,.T.);
#82595=ORIENTED_EDGE('',*,*,#56069,.F.);
#82596=ORIENTED_EDGE('',*,*,#56081,.T.);
#82597=ORIENTED_EDGE('',*,*,#56082,.T.);
#82598=ORIENTED_EDGE('',*,*,#56083,.F.);
#82599=ORIENTED_EDGE('',*,*,#56077,.F.);
#82600=ORIENTED_EDGE('',*,*,#56084,.F.);
#82601=ORIENTED_EDGE('',*,*,#56085,.F.);
#82602=ORIENTED_EDGE('',*,*,#56084,.T.);
#82603=ORIENTED_EDGE('',*,*,#56082,.F.);
#82604=ORIENTED_EDGE('',*,*,#56081,.F.);
#82605=ORIENTED_EDGE('',*,*,#56086,.F.);
#82606=ORIENTED_EDGE('',*,*,#56087,.F.);
#82607=ORIENTED_EDGE('',*,*,#56086,.T.);
#82608=ORIENTED_EDGE('',*,*,#56073,.F.);
#82609=ORIENTED_EDGE('',*,*,#56088,.F.);
#82610=ORIENTED_EDGE('',*,*,#56089,.F.);
#82611=ORIENTED_EDGE('',*,*,#56090,.T.);
#82612=ORIENTED_EDGE('',*,*,#56083,.T.);
#82613=ORIENTED_EDGE('',*,*,#54135,.F.);
#82614=ORIENTED_EDGE('',*,*,#54692,.T.);
#82615=ORIENTED_EDGE('',*,*,#56091,.F.);
#82616=ORIENTED_EDGE('',*,*,#56078,.F.);
#82617=ORIENTED_EDGE('',*,*,#56090,.F.);
#82618=ORIENTED_EDGE('',*,*,#54691,.F.);
#82619=ORIENTED_EDGE('',*,*,#56091,.T.);
#82620=ORIENTED_EDGE('',*,*,#55077,.F.);
#82621=ORIENTED_EDGE('',*,*,#56092,.F.);
#82622=ORIENTED_EDGE('',*,*,#56074,.F.);
#82623=ORIENTED_EDGE('',*,*,#56092,.T.);
#82624=ORIENTED_EDGE('',*,*,#54366,.F.);
#82625=ORIENTED_EDGE('',*,*,#56093,.F.);
#82626=ORIENTED_EDGE('',*,*,#56075,.F.);
#82627=ORIENTED_EDGE('',*,*,#56093,.T.);
#82628=ORIENTED_EDGE('',*,*,#54365,.F.);
#82629=ORIENTED_EDGE('',*,*,#56094,.F.);
#82630=ORIENTED_EDGE('',*,*,#56080,.F.);
#82631=ORIENTED_EDGE('',*,*,#56079,.F.);
#82632=ORIENTED_EDGE('',*,*,#56094,.T.);
#82633=ORIENTED_EDGE('',*,*,#54364,.F.);
#82634=ORIENTED_EDGE('',*,*,#56095,.F.);
#82635=ORIENTED_EDGE('',*,*,#56070,.F.);
#82636=ORIENTED_EDGE('',*,*,#56096,.T.);
#82637=ORIENTED_EDGE('',*,*,#56071,.F.);
#82638=ORIENTED_EDGE('',*,*,#56095,.T.);
#82639=ORIENTED_EDGE('',*,*,#55078,.F.);
#82640=ORIENTED_EDGE('',*,*,#56097,.T.);
#82641=ORIENTED_EDGE('',*,*,#56072,.F.);
#82642=ORIENTED_EDGE('',*,*,#56096,.F.);
#82643=ORIENTED_EDGE('',*,*,#54694,.F.);
#82644=ORIENTED_EDGE('',*,*,#54133,.T.);
#82645=ORIENTED_EDGE('',*,*,#56088,.T.);
#82646=ORIENTED_EDGE('',*,*,#56097,.F.);
#82647=ORIENTED_EDGE('',*,*,#54693,.T.);
#82648=ORIENTED_EDGE('',*,*,#56087,.T.);
#82649=ORIENTED_EDGE('',*,*,#56089,.T.);
#82650=ORIENTED_EDGE('',*,*,#54132,.T.);
#82651=ORIENTED_EDGE('',*,*,#56085,.T.);
#82652=ORIENTED_EDGE('',*,*,#56098,.T.);
#82653=ORIENTED_EDGE('',*,*,#56099,.T.);
#82654=ORIENTED_EDGE('',*,*,#56100,.T.);
#82655=ORIENTED_EDGE('',*,*,#56101,.T.);
#82656=ORIENTED_EDGE('',*,*,#56102,.T.);
#82657=ORIENTED_EDGE('',*,*,#56103,.T.);
#82658=ORIENTED_EDGE('',*,*,#56104,.T.);
#82659=ORIENTED_EDGE('',*,*,#56105,.F.);
#82660=ORIENTED_EDGE('',*,*,#56106,.T.);
#82661=ORIENTED_EDGE('',*,*,#56107,.T.);
#82662=ORIENTED_EDGE('',*,*,#56105,.T.);
#82663=ORIENTED_EDGE('',*,*,#56108,.T.);
#82664=ORIENTED_EDGE('',*,*,#56109,.T.);
#82665=ORIENTED_EDGE('',*,*,#56098,.F.);
#82666=ORIENTED_EDGE('',*,*,#56110,.T.);
#82667=ORIENTED_EDGE('',*,*,#56111,.T.);
#82668=ORIENTED_EDGE('',*,*,#56112,.F.);
#82669=ORIENTED_EDGE('',*,*,#56106,.F.);
#82670=ORIENTED_EDGE('',*,*,#56113,.F.);
#82671=ORIENTED_EDGE('',*,*,#56114,.F.);
#82672=ORIENTED_EDGE('',*,*,#56113,.T.);
#82673=ORIENTED_EDGE('',*,*,#56111,.F.);
#82674=ORIENTED_EDGE('',*,*,#56110,.F.);
#82675=ORIENTED_EDGE('',*,*,#56115,.F.);
#82676=ORIENTED_EDGE('',*,*,#56116,.F.);
#82677=ORIENTED_EDGE('',*,*,#56115,.T.);
#82678=ORIENTED_EDGE('',*,*,#56102,.F.);
#82679=ORIENTED_EDGE('',*,*,#56117,.F.);
#82680=ORIENTED_EDGE('',*,*,#56118,.F.);
#82681=ORIENTED_EDGE('',*,*,#56119,.T.);
#82682=ORIENTED_EDGE('',*,*,#56112,.T.);
#82683=ORIENTED_EDGE('',*,*,#54131,.F.);
#82684=ORIENTED_EDGE('',*,*,#54687,.T.);
#82685=ORIENTED_EDGE('',*,*,#56120,.F.);
#82686=ORIENTED_EDGE('',*,*,#56107,.F.);
#82687=ORIENTED_EDGE('',*,*,#56119,.F.);
#82688=ORIENTED_EDGE('',*,*,#54686,.F.);
#82689=ORIENTED_EDGE('',*,*,#56120,.T.);
#82690=ORIENTED_EDGE('',*,*,#55075,.F.);
#82691=ORIENTED_EDGE('',*,*,#56121,.F.);
#82692=ORIENTED_EDGE('',*,*,#56103,.F.);
#82693=ORIENTED_EDGE('',*,*,#56121,.T.);
#82694=ORIENTED_EDGE('',*,*,#54370,.F.);
#82695=ORIENTED_EDGE('',*,*,#56122,.F.);
#82696=ORIENTED_EDGE('',*,*,#56104,.F.);
#82697=ORIENTED_EDGE('',*,*,#56122,.T.);
#82698=ORIENTED_EDGE('',*,*,#54369,.F.);
#82699=ORIENTED_EDGE('',*,*,#56123,.F.);
#82700=ORIENTED_EDGE('',*,*,#56109,.F.);
#82701=ORIENTED_EDGE('',*,*,#56108,.F.);
#82702=ORIENTED_EDGE('',*,*,#56123,.T.);
#82703=ORIENTED_EDGE('',*,*,#54368,.F.);
#82704=ORIENTED_EDGE('',*,*,#56124,.F.);
#82705=ORIENTED_EDGE('',*,*,#56099,.F.);
#82706=ORIENTED_EDGE('',*,*,#56125,.T.);
#82707=ORIENTED_EDGE('',*,*,#56100,.F.);
#82708=ORIENTED_EDGE('',*,*,#56124,.T.);
#82709=ORIENTED_EDGE('',*,*,#55076,.F.);
#82710=ORIENTED_EDGE('',*,*,#56126,.T.);
#82711=ORIENTED_EDGE('',*,*,#56101,.F.);
#82712=ORIENTED_EDGE('',*,*,#56125,.F.);
#82713=ORIENTED_EDGE('',*,*,#54689,.F.);
#82714=ORIENTED_EDGE('',*,*,#54129,.T.);
#82715=ORIENTED_EDGE('',*,*,#56117,.T.);
#82716=ORIENTED_EDGE('',*,*,#56126,.F.);
#82717=ORIENTED_EDGE('',*,*,#54688,.T.);
#82718=ORIENTED_EDGE('',*,*,#56116,.T.);
#82719=ORIENTED_EDGE('',*,*,#56118,.T.);
#82720=ORIENTED_EDGE('',*,*,#54128,.T.);
#82721=ORIENTED_EDGE('',*,*,#56114,.T.);
#82722=ORIENTED_EDGE('',*,*,#56127,.T.);
#82723=ORIENTED_EDGE('',*,*,#56128,.T.);
#82724=ORIENTED_EDGE('',*,*,#56129,.T.);
#82725=ORIENTED_EDGE('',*,*,#56130,.T.);
#82726=ORIENTED_EDGE('',*,*,#56131,.T.);
#82727=ORIENTED_EDGE('',*,*,#56132,.T.);
#82728=ORIENTED_EDGE('',*,*,#56133,.T.);
#82729=ORIENTED_EDGE('',*,*,#56134,.F.);
#82730=ORIENTED_EDGE('',*,*,#56135,.T.);
#82731=ORIENTED_EDGE('',*,*,#56136,.T.);
#82732=ORIENTED_EDGE('',*,*,#56134,.T.);
#82733=ORIENTED_EDGE('',*,*,#56137,.T.);
#82734=ORIENTED_EDGE('',*,*,#56138,.T.);
#82735=ORIENTED_EDGE('',*,*,#56127,.F.);
#82736=ORIENTED_EDGE('',*,*,#56139,.T.);
#82737=ORIENTED_EDGE('',*,*,#56140,.T.);
#82738=ORIENTED_EDGE('',*,*,#56141,.F.);
#82739=ORIENTED_EDGE('',*,*,#56135,.F.);
#82740=ORIENTED_EDGE('',*,*,#56142,.F.);
#82741=ORIENTED_EDGE('',*,*,#56143,.F.);
#82742=ORIENTED_EDGE('',*,*,#56142,.T.);
#82743=ORIENTED_EDGE('',*,*,#56140,.F.);
#82744=ORIENTED_EDGE('',*,*,#56139,.F.);
#82745=ORIENTED_EDGE('',*,*,#56144,.F.);
#82746=ORIENTED_EDGE('',*,*,#56145,.F.);
#82747=ORIENTED_EDGE('',*,*,#56144,.T.);
#82748=ORIENTED_EDGE('',*,*,#56131,.F.);
#82749=ORIENTED_EDGE('',*,*,#56146,.F.);
#82750=ORIENTED_EDGE('',*,*,#56147,.F.);
#82751=ORIENTED_EDGE('',*,*,#56148,.T.);
#82752=ORIENTED_EDGE('',*,*,#56141,.T.);
#82753=ORIENTED_EDGE('',*,*,#54127,.F.);
#82754=ORIENTED_EDGE('',*,*,#54682,.T.);
#82755=ORIENTED_EDGE('',*,*,#56149,.F.);
#82756=ORIENTED_EDGE('',*,*,#56136,.F.);
#82757=ORIENTED_EDGE('',*,*,#56148,.F.);
#82758=ORIENTED_EDGE('',*,*,#54681,.F.);
#82759=ORIENTED_EDGE('',*,*,#56149,.T.);
#82760=ORIENTED_EDGE('',*,*,#55073,.F.);
#82761=ORIENTED_EDGE('',*,*,#56150,.F.);
#82762=ORIENTED_EDGE('',*,*,#56132,.F.);
#82763=ORIENTED_EDGE('',*,*,#56150,.T.);
#82764=ORIENTED_EDGE('',*,*,#54374,.F.);
#82765=ORIENTED_EDGE('',*,*,#56151,.F.);
#82766=ORIENTED_EDGE('',*,*,#56133,.F.);
#82767=ORIENTED_EDGE('',*,*,#56151,.T.);
#82768=ORIENTED_EDGE('',*,*,#54373,.F.);
#82769=ORIENTED_EDGE('',*,*,#56152,.F.);
#82770=ORIENTED_EDGE('',*,*,#56138,.F.);
#82771=ORIENTED_EDGE('',*,*,#56137,.F.);
#82772=ORIENTED_EDGE('',*,*,#56152,.T.);
#82773=ORIENTED_EDGE('',*,*,#54372,.F.);
#82774=ORIENTED_EDGE('',*,*,#56153,.F.);
#82775=ORIENTED_EDGE('',*,*,#56128,.F.);
#82776=ORIENTED_EDGE('',*,*,#56154,.T.);
#82777=ORIENTED_EDGE('',*,*,#56129,.F.);
#82778=ORIENTED_EDGE('',*,*,#56153,.T.);
#82779=ORIENTED_EDGE('',*,*,#55074,.F.);
#82780=ORIENTED_EDGE('',*,*,#56155,.T.);
#82781=ORIENTED_EDGE('',*,*,#56130,.F.);
#82782=ORIENTED_EDGE('',*,*,#56154,.F.);
#82783=ORIENTED_EDGE('',*,*,#54684,.F.);
#82784=ORIENTED_EDGE('',*,*,#54125,.T.);
#82785=ORIENTED_EDGE('',*,*,#56146,.T.);
#82786=ORIENTED_EDGE('',*,*,#56155,.F.);
#82787=ORIENTED_EDGE('',*,*,#54683,.T.);
#82788=ORIENTED_EDGE('',*,*,#56145,.T.);
#82789=ORIENTED_EDGE('',*,*,#56147,.T.);
#82790=ORIENTED_EDGE('',*,*,#54124,.T.);
#82791=ORIENTED_EDGE('',*,*,#56143,.T.);
#82792=ORIENTED_EDGE('',*,*,#56156,.T.);
#82793=ORIENTED_EDGE('',*,*,#56157,.T.);
#82794=ORIENTED_EDGE('',*,*,#56158,.T.);
#82795=ORIENTED_EDGE('',*,*,#56159,.T.);
#82796=ORIENTED_EDGE('',*,*,#56160,.T.);
#82797=ORIENTED_EDGE('',*,*,#56161,.T.);
#82798=ORIENTED_EDGE('',*,*,#56162,.T.);
#82799=ORIENTED_EDGE('',*,*,#56163,.F.);
#82800=ORIENTED_EDGE('',*,*,#56164,.T.);
#82801=ORIENTED_EDGE('',*,*,#56165,.T.);
#82802=ORIENTED_EDGE('',*,*,#56163,.T.);
#82803=ORIENTED_EDGE('',*,*,#56166,.T.);
#82804=ORIENTED_EDGE('',*,*,#56167,.T.);
#82805=ORIENTED_EDGE('',*,*,#56156,.F.);
#82806=ORIENTED_EDGE('',*,*,#56168,.T.);
#82807=ORIENTED_EDGE('',*,*,#56169,.T.);
#82808=ORIENTED_EDGE('',*,*,#56170,.F.);
#82809=ORIENTED_EDGE('',*,*,#56164,.F.);
#82810=ORIENTED_EDGE('',*,*,#56171,.F.);
#82811=ORIENTED_EDGE('',*,*,#56172,.F.);
#82812=ORIENTED_EDGE('',*,*,#56171,.T.);
#82813=ORIENTED_EDGE('',*,*,#56169,.F.);
#82814=ORIENTED_EDGE('',*,*,#56168,.F.);
#82815=ORIENTED_EDGE('',*,*,#56173,.F.);
#82816=ORIENTED_EDGE('',*,*,#56174,.F.);
#82817=ORIENTED_EDGE('',*,*,#56173,.T.);
#82818=ORIENTED_EDGE('',*,*,#56160,.F.);
#82819=ORIENTED_EDGE('',*,*,#56175,.F.);
#82820=ORIENTED_EDGE('',*,*,#56176,.F.);
#82821=ORIENTED_EDGE('',*,*,#56177,.T.);
#82822=ORIENTED_EDGE('',*,*,#56170,.T.);
#82823=ORIENTED_EDGE('',*,*,#54123,.F.);
#82824=ORIENTED_EDGE('',*,*,#54677,.T.);
#82825=ORIENTED_EDGE('',*,*,#56178,.F.);
#82826=ORIENTED_EDGE('',*,*,#56165,.F.);
#82827=ORIENTED_EDGE('',*,*,#56177,.F.);
#82828=ORIENTED_EDGE('',*,*,#54676,.F.);
#82829=ORIENTED_EDGE('',*,*,#56178,.T.);
#82830=ORIENTED_EDGE('',*,*,#55071,.F.);
#82831=ORIENTED_EDGE('',*,*,#56179,.F.);
#82832=ORIENTED_EDGE('',*,*,#56161,.F.);
#82833=ORIENTED_EDGE('',*,*,#56179,.T.);
#82834=ORIENTED_EDGE('',*,*,#54378,.F.);
#82835=ORIENTED_EDGE('',*,*,#56180,.F.);
#82836=ORIENTED_EDGE('',*,*,#56162,.F.);
#82837=ORIENTED_EDGE('',*,*,#56180,.T.);
#82838=ORIENTED_EDGE('',*,*,#54377,.F.);
#82839=ORIENTED_EDGE('',*,*,#56181,.F.);
#82840=ORIENTED_EDGE('',*,*,#56167,.F.);
#82841=ORIENTED_EDGE('',*,*,#56166,.F.);
#82842=ORIENTED_EDGE('',*,*,#56181,.T.);
#82843=ORIENTED_EDGE('',*,*,#54376,.F.);
#82844=ORIENTED_EDGE('',*,*,#56182,.F.);
#82845=ORIENTED_EDGE('',*,*,#56157,.F.);
#82846=ORIENTED_EDGE('',*,*,#56183,.T.);
#82847=ORIENTED_EDGE('',*,*,#56158,.F.);
#82848=ORIENTED_EDGE('',*,*,#56182,.T.);
#82849=ORIENTED_EDGE('',*,*,#55072,.F.);
#82850=ORIENTED_EDGE('',*,*,#56184,.T.);
#82851=ORIENTED_EDGE('',*,*,#56159,.F.);
#82852=ORIENTED_EDGE('',*,*,#56183,.F.);
#82853=ORIENTED_EDGE('',*,*,#54679,.F.);
#82854=ORIENTED_EDGE('',*,*,#54121,.T.);
#82855=ORIENTED_EDGE('',*,*,#56175,.T.);
#82856=ORIENTED_EDGE('',*,*,#56184,.F.);
#82857=ORIENTED_EDGE('',*,*,#54678,.T.);
#82858=ORIENTED_EDGE('',*,*,#56174,.T.);
#82859=ORIENTED_EDGE('',*,*,#56176,.T.);
#82860=ORIENTED_EDGE('',*,*,#54120,.T.);
#82861=ORIENTED_EDGE('',*,*,#56172,.T.);
#82862=ORIENTED_EDGE('',*,*,#56185,.T.);
#82863=ORIENTED_EDGE('',*,*,#56186,.T.);
#82864=ORIENTED_EDGE('',*,*,#56187,.T.);
#82865=ORIENTED_EDGE('',*,*,#56188,.T.);
#82866=ORIENTED_EDGE('',*,*,#56189,.T.);
#82867=ORIENTED_EDGE('',*,*,#56190,.T.);
#82868=ORIENTED_EDGE('',*,*,#56191,.T.);
#82869=ORIENTED_EDGE('',*,*,#56192,.F.);
#82870=ORIENTED_EDGE('',*,*,#56193,.T.);
#82871=ORIENTED_EDGE('',*,*,#56194,.T.);
#82872=ORIENTED_EDGE('',*,*,#56192,.T.);
#82873=ORIENTED_EDGE('',*,*,#56195,.T.);
#82874=ORIENTED_EDGE('',*,*,#56196,.T.);
#82875=ORIENTED_EDGE('',*,*,#56185,.F.);
#82876=ORIENTED_EDGE('',*,*,#56197,.T.);
#82877=ORIENTED_EDGE('',*,*,#56198,.T.);
#82878=ORIENTED_EDGE('',*,*,#56199,.F.);
#82879=ORIENTED_EDGE('',*,*,#56193,.F.);
#82880=ORIENTED_EDGE('',*,*,#56200,.F.);
#82881=ORIENTED_EDGE('',*,*,#56201,.F.);
#82882=ORIENTED_EDGE('',*,*,#56200,.T.);
#82883=ORIENTED_EDGE('',*,*,#56198,.F.);
#82884=ORIENTED_EDGE('',*,*,#56197,.F.);
#82885=ORIENTED_EDGE('',*,*,#56202,.F.);
#82886=ORIENTED_EDGE('',*,*,#56203,.F.);
#82887=ORIENTED_EDGE('',*,*,#56202,.T.);
#82888=ORIENTED_EDGE('',*,*,#56189,.F.);
#82889=ORIENTED_EDGE('',*,*,#56204,.F.);
#82890=ORIENTED_EDGE('',*,*,#56205,.F.);
#82891=ORIENTED_EDGE('',*,*,#56206,.T.);
#82892=ORIENTED_EDGE('',*,*,#56199,.T.);
#82893=ORIENTED_EDGE('',*,*,#54119,.F.);
#82894=ORIENTED_EDGE('',*,*,#54672,.T.);
#82895=ORIENTED_EDGE('',*,*,#56207,.F.);
#82896=ORIENTED_EDGE('',*,*,#56194,.F.);
#82897=ORIENTED_EDGE('',*,*,#56206,.F.);
#82898=ORIENTED_EDGE('',*,*,#54671,.F.);
#82899=ORIENTED_EDGE('',*,*,#56207,.T.);
#82900=ORIENTED_EDGE('',*,*,#55069,.F.);
#82901=ORIENTED_EDGE('',*,*,#56208,.F.);
#82902=ORIENTED_EDGE('',*,*,#56190,.F.);
#82903=ORIENTED_EDGE('',*,*,#56208,.T.);
#82904=ORIENTED_EDGE('',*,*,#54382,.F.);
#82905=ORIENTED_EDGE('',*,*,#56209,.F.);
#82906=ORIENTED_EDGE('',*,*,#56191,.F.);
#82907=ORIENTED_EDGE('',*,*,#56209,.T.);
#82908=ORIENTED_EDGE('',*,*,#54381,.F.);
#82909=ORIENTED_EDGE('',*,*,#56210,.F.);
#82910=ORIENTED_EDGE('',*,*,#56196,.F.);
#82911=ORIENTED_EDGE('',*,*,#56195,.F.);
#82912=ORIENTED_EDGE('',*,*,#56210,.T.);
#82913=ORIENTED_EDGE('',*,*,#54380,.F.);
#82914=ORIENTED_EDGE('',*,*,#56211,.F.);
#82915=ORIENTED_EDGE('',*,*,#56186,.F.);
#82916=ORIENTED_EDGE('',*,*,#56212,.T.);
#82917=ORIENTED_EDGE('',*,*,#56187,.F.);
#82918=ORIENTED_EDGE('',*,*,#56211,.T.);
#82919=ORIENTED_EDGE('',*,*,#55070,.F.);
#82920=ORIENTED_EDGE('',*,*,#56213,.T.);
#82921=ORIENTED_EDGE('',*,*,#56188,.F.);
#82922=ORIENTED_EDGE('',*,*,#56212,.F.);
#82923=ORIENTED_EDGE('',*,*,#54674,.F.);
#82924=ORIENTED_EDGE('',*,*,#54117,.T.);
#82925=ORIENTED_EDGE('',*,*,#56204,.T.);
#82926=ORIENTED_EDGE('',*,*,#56213,.F.);
#82927=ORIENTED_EDGE('',*,*,#54673,.T.);
#82928=ORIENTED_EDGE('',*,*,#56203,.T.);
#82929=ORIENTED_EDGE('',*,*,#56205,.T.);
#82930=ORIENTED_EDGE('',*,*,#54116,.T.);
#82931=ORIENTED_EDGE('',*,*,#56201,.T.);
#82932=ORIENTED_EDGE('',*,*,#56214,.T.);
#82933=ORIENTED_EDGE('',*,*,#56215,.T.);
#82934=ORIENTED_EDGE('',*,*,#56216,.T.);
#82935=ORIENTED_EDGE('',*,*,#56217,.T.);
#82936=ORIENTED_EDGE('',*,*,#56218,.T.);
#82937=ORIENTED_EDGE('',*,*,#56219,.T.);
#82938=ORIENTED_EDGE('',*,*,#56220,.T.);
#82939=ORIENTED_EDGE('',*,*,#56221,.F.);
#82940=ORIENTED_EDGE('',*,*,#56222,.T.);
#82941=ORIENTED_EDGE('',*,*,#56223,.T.);
#82942=ORIENTED_EDGE('',*,*,#56221,.T.);
#82943=ORIENTED_EDGE('',*,*,#56224,.T.);
#82944=ORIENTED_EDGE('',*,*,#56225,.T.);
#82945=ORIENTED_EDGE('',*,*,#56214,.F.);
#82946=ORIENTED_EDGE('',*,*,#56226,.T.);
#82947=ORIENTED_EDGE('',*,*,#56227,.T.);
#82948=ORIENTED_EDGE('',*,*,#56228,.F.);
#82949=ORIENTED_EDGE('',*,*,#56222,.F.);
#82950=ORIENTED_EDGE('',*,*,#56229,.F.);
#82951=ORIENTED_EDGE('',*,*,#56230,.F.);
#82952=ORIENTED_EDGE('',*,*,#56229,.T.);
#82953=ORIENTED_EDGE('',*,*,#56227,.F.);
#82954=ORIENTED_EDGE('',*,*,#56226,.F.);
#82955=ORIENTED_EDGE('',*,*,#56231,.F.);
#82956=ORIENTED_EDGE('',*,*,#56232,.F.);
#82957=ORIENTED_EDGE('',*,*,#56231,.T.);
#82958=ORIENTED_EDGE('',*,*,#56218,.F.);
#82959=ORIENTED_EDGE('',*,*,#56233,.F.);
#82960=ORIENTED_EDGE('',*,*,#56234,.F.);
#82961=ORIENTED_EDGE('',*,*,#56235,.T.);
#82962=ORIENTED_EDGE('',*,*,#56228,.T.);
#82963=ORIENTED_EDGE('',*,*,#54115,.F.);
#82964=ORIENTED_EDGE('',*,*,#54667,.T.);
#82965=ORIENTED_EDGE('',*,*,#56236,.F.);
#82966=ORIENTED_EDGE('',*,*,#56223,.F.);
#82967=ORIENTED_EDGE('',*,*,#56235,.F.);
#82968=ORIENTED_EDGE('',*,*,#54666,.F.);
#82969=ORIENTED_EDGE('',*,*,#56236,.T.);
#82970=ORIENTED_EDGE('',*,*,#55067,.F.);
#82971=ORIENTED_EDGE('',*,*,#56237,.F.);
#82972=ORIENTED_EDGE('',*,*,#56219,.F.);
#82973=ORIENTED_EDGE('',*,*,#56237,.T.);
#82974=ORIENTED_EDGE('',*,*,#54386,.F.);
#82975=ORIENTED_EDGE('',*,*,#56238,.F.);
#82976=ORIENTED_EDGE('',*,*,#56220,.F.);
#82977=ORIENTED_EDGE('',*,*,#56238,.T.);
#82978=ORIENTED_EDGE('',*,*,#54385,.F.);
#82979=ORIENTED_EDGE('',*,*,#56239,.F.);
#82980=ORIENTED_EDGE('',*,*,#56225,.F.);
#82981=ORIENTED_EDGE('',*,*,#56224,.F.);
#82982=ORIENTED_EDGE('',*,*,#56239,.T.);
#82983=ORIENTED_EDGE('',*,*,#54384,.F.);
#82984=ORIENTED_EDGE('',*,*,#56240,.F.);
#82985=ORIENTED_EDGE('',*,*,#56215,.F.);
#82986=ORIENTED_EDGE('',*,*,#56241,.T.);
#82987=ORIENTED_EDGE('',*,*,#56216,.F.);
#82988=ORIENTED_EDGE('',*,*,#56240,.T.);
#82989=ORIENTED_EDGE('',*,*,#55068,.F.);
#82990=ORIENTED_EDGE('',*,*,#56242,.T.);
#82991=ORIENTED_EDGE('',*,*,#56217,.F.);
#82992=ORIENTED_EDGE('',*,*,#56241,.F.);
#82993=ORIENTED_EDGE('',*,*,#54669,.F.);
#82994=ORIENTED_EDGE('',*,*,#54113,.T.);
#82995=ORIENTED_EDGE('',*,*,#56233,.T.);
#82996=ORIENTED_EDGE('',*,*,#56242,.F.);
#82997=ORIENTED_EDGE('',*,*,#54668,.T.);
#82998=ORIENTED_EDGE('',*,*,#56232,.T.);
#82999=ORIENTED_EDGE('',*,*,#56234,.T.);
#83000=ORIENTED_EDGE('',*,*,#54112,.T.);
#83001=ORIENTED_EDGE('',*,*,#56230,.T.);
#83002=ORIENTED_EDGE('',*,*,#56243,.T.);
#83003=ORIENTED_EDGE('',*,*,#56244,.T.);
#83004=ORIENTED_EDGE('',*,*,#56245,.T.);
#83005=ORIENTED_EDGE('',*,*,#56246,.T.);
#83006=ORIENTED_EDGE('',*,*,#56247,.T.);
#83007=ORIENTED_EDGE('',*,*,#56248,.T.);
#83008=ORIENTED_EDGE('',*,*,#56249,.T.);
#83009=ORIENTED_EDGE('',*,*,#56250,.F.);
#83010=ORIENTED_EDGE('',*,*,#56251,.T.);
#83011=ORIENTED_EDGE('',*,*,#56252,.T.);
#83012=ORIENTED_EDGE('',*,*,#56250,.T.);
#83013=ORIENTED_EDGE('',*,*,#56253,.T.);
#83014=ORIENTED_EDGE('',*,*,#56254,.T.);
#83015=ORIENTED_EDGE('',*,*,#56243,.F.);
#83016=ORIENTED_EDGE('',*,*,#56255,.T.);
#83017=ORIENTED_EDGE('',*,*,#56256,.T.);
#83018=ORIENTED_EDGE('',*,*,#56257,.F.);
#83019=ORIENTED_EDGE('',*,*,#56251,.F.);
#83020=ORIENTED_EDGE('',*,*,#56258,.F.);
#83021=ORIENTED_EDGE('',*,*,#56259,.F.);
#83022=ORIENTED_EDGE('',*,*,#56258,.T.);
#83023=ORIENTED_EDGE('',*,*,#56256,.F.);
#83024=ORIENTED_EDGE('',*,*,#56255,.F.);
#83025=ORIENTED_EDGE('',*,*,#56260,.F.);
#83026=ORIENTED_EDGE('',*,*,#56261,.F.);
#83027=ORIENTED_EDGE('',*,*,#56260,.T.);
#83028=ORIENTED_EDGE('',*,*,#56247,.F.);
#83029=ORIENTED_EDGE('',*,*,#56262,.F.);
#83030=ORIENTED_EDGE('',*,*,#56263,.F.);
#83031=ORIENTED_EDGE('',*,*,#56264,.T.);
#83032=ORIENTED_EDGE('',*,*,#56257,.T.);
#83033=ORIENTED_EDGE('',*,*,#54111,.F.);
#83034=ORIENTED_EDGE('',*,*,#54662,.T.);
#83035=ORIENTED_EDGE('',*,*,#56265,.F.);
#83036=ORIENTED_EDGE('',*,*,#56252,.F.);
#83037=ORIENTED_EDGE('',*,*,#56264,.F.);
#83038=ORIENTED_EDGE('',*,*,#54661,.F.);
#83039=ORIENTED_EDGE('',*,*,#56265,.T.);
#83040=ORIENTED_EDGE('',*,*,#55065,.F.);
#83041=ORIENTED_EDGE('',*,*,#56266,.F.);
#83042=ORIENTED_EDGE('',*,*,#56248,.F.);
#83043=ORIENTED_EDGE('',*,*,#56266,.T.);
#83044=ORIENTED_EDGE('',*,*,#54390,.F.);
#83045=ORIENTED_EDGE('',*,*,#56267,.F.);
#83046=ORIENTED_EDGE('',*,*,#56249,.F.);
#83047=ORIENTED_EDGE('',*,*,#56267,.T.);
#83048=ORIENTED_EDGE('',*,*,#54389,.F.);
#83049=ORIENTED_EDGE('',*,*,#56268,.F.);
#83050=ORIENTED_EDGE('',*,*,#56254,.F.);
#83051=ORIENTED_EDGE('',*,*,#56253,.F.);
#83052=ORIENTED_EDGE('',*,*,#56268,.T.);
#83053=ORIENTED_EDGE('',*,*,#54388,.F.);
#83054=ORIENTED_EDGE('',*,*,#56269,.F.);
#83055=ORIENTED_EDGE('',*,*,#56244,.F.);
#83056=ORIENTED_EDGE('',*,*,#56270,.T.);
#83057=ORIENTED_EDGE('',*,*,#56245,.F.);
#83058=ORIENTED_EDGE('',*,*,#56269,.T.);
#83059=ORIENTED_EDGE('',*,*,#55066,.F.);
#83060=ORIENTED_EDGE('',*,*,#56271,.T.);
#83061=ORIENTED_EDGE('',*,*,#56246,.F.);
#83062=ORIENTED_EDGE('',*,*,#56270,.F.);
#83063=ORIENTED_EDGE('',*,*,#54664,.F.);
#83064=ORIENTED_EDGE('',*,*,#54109,.T.);
#83065=ORIENTED_EDGE('',*,*,#56262,.T.);
#83066=ORIENTED_EDGE('',*,*,#56271,.F.);
#83067=ORIENTED_EDGE('',*,*,#54663,.T.);
#83068=ORIENTED_EDGE('',*,*,#56261,.T.);
#83069=ORIENTED_EDGE('',*,*,#56263,.T.);
#83070=ORIENTED_EDGE('',*,*,#54108,.T.);
#83071=ORIENTED_EDGE('',*,*,#56259,.T.);
#83072=ORIENTED_EDGE('',*,*,#56272,.T.);
#83073=ORIENTED_EDGE('',*,*,#56273,.T.);
#83074=ORIENTED_EDGE('',*,*,#56274,.T.);
#83075=ORIENTED_EDGE('',*,*,#56275,.T.);
#83076=ORIENTED_EDGE('',*,*,#56276,.T.);
#83077=ORIENTED_EDGE('',*,*,#56277,.T.);
#83078=ORIENTED_EDGE('',*,*,#56278,.T.);
#83079=ORIENTED_EDGE('',*,*,#56279,.F.);
#83080=ORIENTED_EDGE('',*,*,#56280,.T.);
#83081=ORIENTED_EDGE('',*,*,#56281,.T.);
#83082=ORIENTED_EDGE('',*,*,#56279,.T.);
#83083=ORIENTED_EDGE('',*,*,#56282,.T.);
#83084=ORIENTED_EDGE('',*,*,#56283,.T.);
#83085=ORIENTED_EDGE('',*,*,#56272,.F.);
#83086=ORIENTED_EDGE('',*,*,#56284,.T.);
#83087=ORIENTED_EDGE('',*,*,#56285,.T.);
#83088=ORIENTED_EDGE('',*,*,#56286,.F.);
#83089=ORIENTED_EDGE('',*,*,#56280,.F.);
#83090=ORIENTED_EDGE('',*,*,#56287,.F.);
#83091=ORIENTED_EDGE('',*,*,#56288,.F.);
#83092=ORIENTED_EDGE('',*,*,#56287,.T.);
#83093=ORIENTED_EDGE('',*,*,#56285,.F.);
#83094=ORIENTED_EDGE('',*,*,#56284,.F.);
#83095=ORIENTED_EDGE('',*,*,#56289,.F.);
#83096=ORIENTED_EDGE('',*,*,#56290,.F.);
#83097=ORIENTED_EDGE('',*,*,#56289,.T.);
#83098=ORIENTED_EDGE('',*,*,#56276,.F.);
#83099=ORIENTED_EDGE('',*,*,#56291,.F.);
#83100=ORIENTED_EDGE('',*,*,#56292,.F.);
#83101=ORIENTED_EDGE('',*,*,#56293,.T.);
#83102=ORIENTED_EDGE('',*,*,#56286,.T.);
#83103=ORIENTED_EDGE('',*,*,#54107,.F.);
#83104=ORIENTED_EDGE('',*,*,#54657,.T.);
#83105=ORIENTED_EDGE('',*,*,#56294,.F.);
#83106=ORIENTED_EDGE('',*,*,#56281,.F.);
#83107=ORIENTED_EDGE('',*,*,#56293,.F.);
#83108=ORIENTED_EDGE('',*,*,#54656,.F.);
#83109=ORIENTED_EDGE('',*,*,#56294,.T.);
#83110=ORIENTED_EDGE('',*,*,#55063,.F.);
#83111=ORIENTED_EDGE('',*,*,#56295,.F.);
#83112=ORIENTED_EDGE('',*,*,#56277,.F.);
#83113=ORIENTED_EDGE('',*,*,#56295,.T.);
#83114=ORIENTED_EDGE('',*,*,#54394,.F.);
#83115=ORIENTED_EDGE('',*,*,#56296,.F.);
#83116=ORIENTED_EDGE('',*,*,#56278,.F.);
#83117=ORIENTED_EDGE('',*,*,#56296,.T.);
#83118=ORIENTED_EDGE('',*,*,#54393,.F.);
#83119=ORIENTED_EDGE('',*,*,#56297,.F.);
#83120=ORIENTED_EDGE('',*,*,#56283,.F.);
#83121=ORIENTED_EDGE('',*,*,#56282,.F.);
#83122=ORIENTED_EDGE('',*,*,#56297,.T.);
#83123=ORIENTED_EDGE('',*,*,#54392,.F.);
#83124=ORIENTED_EDGE('',*,*,#56298,.F.);
#83125=ORIENTED_EDGE('',*,*,#56273,.F.);
#83126=ORIENTED_EDGE('',*,*,#56299,.T.);
#83127=ORIENTED_EDGE('',*,*,#56274,.F.);
#83128=ORIENTED_EDGE('',*,*,#56298,.T.);
#83129=ORIENTED_EDGE('',*,*,#55064,.F.);
#83130=ORIENTED_EDGE('',*,*,#56300,.T.);
#83131=ORIENTED_EDGE('',*,*,#56275,.F.);
#83132=ORIENTED_EDGE('',*,*,#56299,.F.);
#83133=ORIENTED_EDGE('',*,*,#54659,.F.);
#83134=ORIENTED_EDGE('',*,*,#54105,.T.);
#83135=ORIENTED_EDGE('',*,*,#56291,.T.);
#83136=ORIENTED_EDGE('',*,*,#56300,.F.);
#83137=ORIENTED_EDGE('',*,*,#54658,.T.);
#83138=ORIENTED_EDGE('',*,*,#56290,.T.);
#83139=ORIENTED_EDGE('',*,*,#56292,.T.);
#83140=ORIENTED_EDGE('',*,*,#54104,.T.);
#83141=ORIENTED_EDGE('',*,*,#56288,.T.);
#83142=ORIENTED_EDGE('',*,*,#56301,.T.);
#83143=ORIENTED_EDGE('',*,*,#56302,.T.);
#83144=ORIENTED_EDGE('',*,*,#56303,.T.);
#83145=ORIENTED_EDGE('',*,*,#56304,.T.);
#83146=ORIENTED_EDGE('',*,*,#56305,.T.);
#83147=ORIENTED_EDGE('',*,*,#56306,.T.);
#83148=ORIENTED_EDGE('',*,*,#56307,.T.);
#83149=ORIENTED_EDGE('',*,*,#56308,.F.);
#83150=ORIENTED_EDGE('',*,*,#56309,.T.);
#83151=ORIENTED_EDGE('',*,*,#56310,.T.);
#83152=ORIENTED_EDGE('',*,*,#56308,.T.);
#83153=ORIENTED_EDGE('',*,*,#56311,.T.);
#83154=ORIENTED_EDGE('',*,*,#56312,.T.);
#83155=ORIENTED_EDGE('',*,*,#56301,.F.);
#83156=ORIENTED_EDGE('',*,*,#56313,.T.);
#83157=ORIENTED_EDGE('',*,*,#56314,.T.);
#83158=ORIENTED_EDGE('',*,*,#56315,.F.);
#83159=ORIENTED_EDGE('',*,*,#56309,.F.);
#83160=ORIENTED_EDGE('',*,*,#56316,.F.);
#83161=ORIENTED_EDGE('',*,*,#56317,.F.);
#83162=ORIENTED_EDGE('',*,*,#56316,.T.);
#83163=ORIENTED_EDGE('',*,*,#56314,.F.);
#83164=ORIENTED_EDGE('',*,*,#56313,.F.);
#83165=ORIENTED_EDGE('',*,*,#56318,.F.);
#83166=ORIENTED_EDGE('',*,*,#56319,.F.);
#83167=ORIENTED_EDGE('',*,*,#56318,.T.);
#83168=ORIENTED_EDGE('',*,*,#56305,.F.);
#83169=ORIENTED_EDGE('',*,*,#56320,.F.);
#83170=ORIENTED_EDGE('',*,*,#56321,.F.);
#83171=ORIENTED_EDGE('',*,*,#56322,.T.);
#83172=ORIENTED_EDGE('',*,*,#56315,.T.);
#83173=ORIENTED_EDGE('',*,*,#54103,.F.);
#83174=ORIENTED_EDGE('',*,*,#54652,.T.);
#83175=ORIENTED_EDGE('',*,*,#56323,.F.);
#83176=ORIENTED_EDGE('',*,*,#56310,.F.);
#83177=ORIENTED_EDGE('',*,*,#56322,.F.);
#83178=ORIENTED_EDGE('',*,*,#54651,.F.);
#83179=ORIENTED_EDGE('',*,*,#56323,.T.);
#83180=ORIENTED_EDGE('',*,*,#55061,.F.);
#83181=ORIENTED_EDGE('',*,*,#56324,.F.);
#83182=ORIENTED_EDGE('',*,*,#56306,.F.);
#83183=ORIENTED_EDGE('',*,*,#56324,.T.);
#83184=ORIENTED_EDGE('',*,*,#54398,.F.);
#83185=ORIENTED_EDGE('',*,*,#56325,.F.);
#83186=ORIENTED_EDGE('',*,*,#56307,.F.);
#83187=ORIENTED_EDGE('',*,*,#56325,.T.);
#83188=ORIENTED_EDGE('',*,*,#54397,.F.);
#83189=ORIENTED_EDGE('',*,*,#56326,.F.);
#83190=ORIENTED_EDGE('',*,*,#56312,.F.);
#83191=ORIENTED_EDGE('',*,*,#56311,.F.);
#83192=ORIENTED_EDGE('',*,*,#56326,.T.);
#83193=ORIENTED_EDGE('',*,*,#54396,.F.);
#83194=ORIENTED_EDGE('',*,*,#56327,.F.);
#83195=ORIENTED_EDGE('',*,*,#56302,.F.);
#83196=ORIENTED_EDGE('',*,*,#56328,.T.);
#83197=ORIENTED_EDGE('',*,*,#56303,.F.);
#83198=ORIENTED_EDGE('',*,*,#56327,.T.);
#83199=ORIENTED_EDGE('',*,*,#55062,.F.);
#83200=ORIENTED_EDGE('',*,*,#56329,.T.);
#83201=ORIENTED_EDGE('',*,*,#56304,.F.);
#83202=ORIENTED_EDGE('',*,*,#56328,.F.);
#83203=ORIENTED_EDGE('',*,*,#54654,.F.);
#83204=ORIENTED_EDGE('',*,*,#54101,.T.);
#83205=ORIENTED_EDGE('',*,*,#56320,.T.);
#83206=ORIENTED_EDGE('',*,*,#56329,.F.);
#83207=ORIENTED_EDGE('',*,*,#54653,.T.);
#83208=ORIENTED_EDGE('',*,*,#56319,.T.);
#83209=ORIENTED_EDGE('',*,*,#56321,.T.);
#83210=ORIENTED_EDGE('',*,*,#54100,.T.);
#83211=ORIENTED_EDGE('',*,*,#56317,.T.);
#83212=ORIENTED_EDGE('',*,*,#56330,.T.);
#83213=ORIENTED_EDGE('',*,*,#56331,.T.);
#83214=ORIENTED_EDGE('',*,*,#56332,.T.);
#83215=ORIENTED_EDGE('',*,*,#56333,.T.);
#83216=ORIENTED_EDGE('',*,*,#56334,.T.);
#83217=ORIENTED_EDGE('',*,*,#56335,.T.);
#83218=ORIENTED_EDGE('',*,*,#56336,.T.);
#83219=ORIENTED_EDGE('',*,*,#56337,.F.);
#83220=ORIENTED_EDGE('',*,*,#56338,.T.);
#83221=ORIENTED_EDGE('',*,*,#56339,.T.);
#83222=ORIENTED_EDGE('',*,*,#56337,.T.);
#83223=ORIENTED_EDGE('',*,*,#56340,.T.);
#83224=ORIENTED_EDGE('',*,*,#56341,.T.);
#83225=ORIENTED_EDGE('',*,*,#56330,.F.);
#83226=ORIENTED_EDGE('',*,*,#56342,.T.);
#83227=ORIENTED_EDGE('',*,*,#56343,.T.);
#83228=ORIENTED_EDGE('',*,*,#56344,.F.);
#83229=ORIENTED_EDGE('',*,*,#56338,.F.);
#83230=ORIENTED_EDGE('',*,*,#56345,.F.);
#83231=ORIENTED_EDGE('',*,*,#56346,.F.);
#83232=ORIENTED_EDGE('',*,*,#56345,.T.);
#83233=ORIENTED_EDGE('',*,*,#56343,.F.);
#83234=ORIENTED_EDGE('',*,*,#56342,.F.);
#83235=ORIENTED_EDGE('',*,*,#56347,.F.);
#83236=ORIENTED_EDGE('',*,*,#56348,.F.);
#83237=ORIENTED_EDGE('',*,*,#56347,.T.);
#83238=ORIENTED_EDGE('',*,*,#56334,.F.);
#83239=ORIENTED_EDGE('',*,*,#56349,.F.);
#83240=ORIENTED_EDGE('',*,*,#56350,.F.);
#83241=ORIENTED_EDGE('',*,*,#56351,.T.);
#83242=ORIENTED_EDGE('',*,*,#56344,.T.);
#83243=ORIENTED_EDGE('',*,*,#54099,.F.);
#83244=ORIENTED_EDGE('',*,*,#54647,.T.);
#83245=ORIENTED_EDGE('',*,*,#56352,.F.);
#83246=ORIENTED_EDGE('',*,*,#56339,.F.);
#83247=ORIENTED_EDGE('',*,*,#56351,.F.);
#83248=ORIENTED_EDGE('',*,*,#54646,.F.);
#83249=ORIENTED_EDGE('',*,*,#56352,.T.);
#83250=ORIENTED_EDGE('',*,*,#55059,.F.);
#83251=ORIENTED_EDGE('',*,*,#56353,.F.);
#83252=ORIENTED_EDGE('',*,*,#56335,.F.);
#83253=ORIENTED_EDGE('',*,*,#56353,.T.);
#83254=ORIENTED_EDGE('',*,*,#54402,.F.);
#83255=ORIENTED_EDGE('',*,*,#56354,.F.);
#83256=ORIENTED_EDGE('',*,*,#56336,.F.);
#83257=ORIENTED_EDGE('',*,*,#56354,.T.);
#83258=ORIENTED_EDGE('',*,*,#54401,.F.);
#83259=ORIENTED_EDGE('',*,*,#56355,.F.);
#83260=ORIENTED_EDGE('',*,*,#56341,.F.);
#83261=ORIENTED_EDGE('',*,*,#56340,.F.);
#83262=ORIENTED_EDGE('',*,*,#56355,.T.);
#83263=ORIENTED_EDGE('',*,*,#54400,.F.);
#83264=ORIENTED_EDGE('',*,*,#56356,.F.);
#83265=ORIENTED_EDGE('',*,*,#56331,.F.);
#83266=ORIENTED_EDGE('',*,*,#56357,.T.);
#83267=ORIENTED_EDGE('',*,*,#56332,.F.);
#83268=ORIENTED_EDGE('',*,*,#56356,.T.);
#83269=ORIENTED_EDGE('',*,*,#55060,.F.);
#83270=ORIENTED_EDGE('',*,*,#56358,.T.);
#83271=ORIENTED_EDGE('',*,*,#56333,.F.);
#83272=ORIENTED_EDGE('',*,*,#56357,.F.);
#83273=ORIENTED_EDGE('',*,*,#54649,.F.);
#83274=ORIENTED_EDGE('',*,*,#54097,.T.);
#83275=ORIENTED_EDGE('',*,*,#56349,.T.);
#83276=ORIENTED_EDGE('',*,*,#56358,.F.);
#83277=ORIENTED_EDGE('',*,*,#54648,.T.);
#83278=ORIENTED_EDGE('',*,*,#56348,.T.);
#83279=ORIENTED_EDGE('',*,*,#56350,.T.);
#83280=ORIENTED_EDGE('',*,*,#54096,.T.);
#83281=ORIENTED_EDGE('',*,*,#56346,.T.);
#83282=ORIENTED_EDGE('',*,*,#56359,.T.);
#83283=ORIENTED_EDGE('',*,*,#56360,.T.);
#83284=ORIENTED_EDGE('',*,*,#56361,.T.);
#83285=ORIENTED_EDGE('',*,*,#56362,.T.);
#83286=ORIENTED_EDGE('',*,*,#56363,.T.);
#83287=ORIENTED_EDGE('',*,*,#56364,.T.);
#83288=ORIENTED_EDGE('',*,*,#56365,.T.);
#83289=ORIENTED_EDGE('',*,*,#56366,.F.);
#83290=ORIENTED_EDGE('',*,*,#56367,.T.);
#83291=ORIENTED_EDGE('',*,*,#56368,.T.);
#83292=ORIENTED_EDGE('',*,*,#56366,.T.);
#83293=ORIENTED_EDGE('',*,*,#56369,.T.);
#83294=ORIENTED_EDGE('',*,*,#56370,.T.);
#83295=ORIENTED_EDGE('',*,*,#56359,.F.);
#83296=ORIENTED_EDGE('',*,*,#56371,.T.);
#83297=ORIENTED_EDGE('',*,*,#56372,.T.);
#83298=ORIENTED_EDGE('',*,*,#56373,.F.);
#83299=ORIENTED_EDGE('',*,*,#56367,.F.);
#83300=ORIENTED_EDGE('',*,*,#56374,.F.);
#83301=ORIENTED_EDGE('',*,*,#56375,.F.);
#83302=ORIENTED_EDGE('',*,*,#56374,.T.);
#83303=ORIENTED_EDGE('',*,*,#56372,.F.);
#83304=ORIENTED_EDGE('',*,*,#56371,.F.);
#83305=ORIENTED_EDGE('',*,*,#56376,.F.);
#83306=ORIENTED_EDGE('',*,*,#56377,.F.);
#83307=ORIENTED_EDGE('',*,*,#56376,.T.);
#83308=ORIENTED_EDGE('',*,*,#56363,.F.);
#83309=ORIENTED_EDGE('',*,*,#56378,.F.);
#83310=ORIENTED_EDGE('',*,*,#56379,.F.);
#83311=ORIENTED_EDGE('',*,*,#56380,.T.);
#83312=ORIENTED_EDGE('',*,*,#56373,.T.);
#83313=ORIENTED_EDGE('',*,*,#54095,.F.);
#83314=ORIENTED_EDGE('',*,*,#54642,.T.);
#83315=ORIENTED_EDGE('',*,*,#56381,.F.);
#83316=ORIENTED_EDGE('',*,*,#56368,.F.);
#83317=ORIENTED_EDGE('',*,*,#56380,.F.);
#83318=ORIENTED_EDGE('',*,*,#54641,.F.);
#83319=ORIENTED_EDGE('',*,*,#56381,.T.);
#83320=ORIENTED_EDGE('',*,*,#55057,.F.);
#83321=ORIENTED_EDGE('',*,*,#56382,.F.);
#83322=ORIENTED_EDGE('',*,*,#56364,.F.);
#83323=ORIENTED_EDGE('',*,*,#56382,.T.);
#83324=ORIENTED_EDGE('',*,*,#54406,.F.);
#83325=ORIENTED_EDGE('',*,*,#56383,.F.);
#83326=ORIENTED_EDGE('',*,*,#56365,.F.);
#83327=ORIENTED_EDGE('',*,*,#56383,.T.);
#83328=ORIENTED_EDGE('',*,*,#54405,.F.);
#83329=ORIENTED_EDGE('',*,*,#56384,.F.);
#83330=ORIENTED_EDGE('',*,*,#56370,.F.);
#83331=ORIENTED_EDGE('',*,*,#56369,.F.);
#83332=ORIENTED_EDGE('',*,*,#56384,.T.);
#83333=ORIENTED_EDGE('',*,*,#54404,.F.);
#83334=ORIENTED_EDGE('',*,*,#56385,.F.);
#83335=ORIENTED_EDGE('',*,*,#56360,.F.);
#83336=ORIENTED_EDGE('',*,*,#56386,.T.);
#83337=ORIENTED_EDGE('',*,*,#56361,.F.);
#83338=ORIENTED_EDGE('',*,*,#56385,.T.);
#83339=ORIENTED_EDGE('',*,*,#55058,.F.);
#83340=ORIENTED_EDGE('',*,*,#56387,.T.);
#83341=ORIENTED_EDGE('',*,*,#56362,.F.);
#83342=ORIENTED_EDGE('',*,*,#56386,.F.);
#83343=ORIENTED_EDGE('',*,*,#54644,.F.);
#83344=ORIENTED_EDGE('',*,*,#54093,.T.);
#83345=ORIENTED_EDGE('',*,*,#56378,.T.);
#83346=ORIENTED_EDGE('',*,*,#56387,.F.);
#83347=ORIENTED_EDGE('',*,*,#54643,.T.);
#83348=ORIENTED_EDGE('',*,*,#56377,.T.);
#83349=ORIENTED_EDGE('',*,*,#56379,.T.);
#83350=ORIENTED_EDGE('',*,*,#54092,.T.);
#83351=ORIENTED_EDGE('',*,*,#56375,.T.);
#83352=ORIENTED_EDGE('',*,*,#56388,.T.);
#83353=ORIENTED_EDGE('',*,*,#56389,.T.);
#83354=ORIENTED_EDGE('',*,*,#56390,.T.);
#83355=ORIENTED_EDGE('',*,*,#56391,.T.);
#83356=ORIENTED_EDGE('',*,*,#56392,.T.);
#83357=ORIENTED_EDGE('',*,*,#56393,.T.);
#83358=ORIENTED_EDGE('',*,*,#56394,.T.);
#83359=ORIENTED_EDGE('',*,*,#56395,.F.);
#83360=ORIENTED_EDGE('',*,*,#56396,.T.);
#83361=ORIENTED_EDGE('',*,*,#56397,.T.);
#83362=ORIENTED_EDGE('',*,*,#56395,.T.);
#83363=ORIENTED_EDGE('',*,*,#56398,.T.);
#83364=ORIENTED_EDGE('',*,*,#56399,.T.);
#83365=ORIENTED_EDGE('',*,*,#56388,.F.);
#83366=ORIENTED_EDGE('',*,*,#56400,.T.);
#83367=ORIENTED_EDGE('',*,*,#56401,.T.);
#83368=ORIENTED_EDGE('',*,*,#56402,.F.);
#83369=ORIENTED_EDGE('',*,*,#56396,.F.);
#83370=ORIENTED_EDGE('',*,*,#56403,.F.);
#83371=ORIENTED_EDGE('',*,*,#56404,.F.);
#83372=ORIENTED_EDGE('',*,*,#56403,.T.);
#83373=ORIENTED_EDGE('',*,*,#56401,.F.);
#83374=ORIENTED_EDGE('',*,*,#56400,.F.);
#83375=ORIENTED_EDGE('',*,*,#56405,.F.);
#83376=ORIENTED_EDGE('',*,*,#56406,.F.);
#83377=ORIENTED_EDGE('',*,*,#56405,.T.);
#83378=ORIENTED_EDGE('',*,*,#56392,.F.);
#83379=ORIENTED_EDGE('',*,*,#56407,.F.);
#83380=ORIENTED_EDGE('',*,*,#56408,.F.);
#83381=ORIENTED_EDGE('',*,*,#56409,.T.);
#83382=ORIENTED_EDGE('',*,*,#56402,.T.);
#83383=ORIENTED_EDGE('',*,*,#54091,.F.);
#83384=ORIENTED_EDGE('',*,*,#54637,.T.);
#83385=ORIENTED_EDGE('',*,*,#56410,.F.);
#83386=ORIENTED_EDGE('',*,*,#56397,.F.);
#83387=ORIENTED_EDGE('',*,*,#56409,.F.);
#83388=ORIENTED_EDGE('',*,*,#54636,.F.);
#83389=ORIENTED_EDGE('',*,*,#56410,.T.);
#83390=ORIENTED_EDGE('',*,*,#55055,.F.);
#83391=ORIENTED_EDGE('',*,*,#56411,.F.);
#83392=ORIENTED_EDGE('',*,*,#56393,.F.);
#83393=ORIENTED_EDGE('',*,*,#56411,.T.);
#83394=ORIENTED_EDGE('',*,*,#54410,.F.);
#83395=ORIENTED_EDGE('',*,*,#56412,.F.);
#83396=ORIENTED_EDGE('',*,*,#56394,.F.);
#83397=ORIENTED_EDGE('',*,*,#56412,.T.);
#83398=ORIENTED_EDGE('',*,*,#54409,.F.);
#83399=ORIENTED_EDGE('',*,*,#56413,.F.);
#83400=ORIENTED_EDGE('',*,*,#56399,.F.);
#83401=ORIENTED_EDGE('',*,*,#56398,.F.);
#83402=ORIENTED_EDGE('',*,*,#56413,.T.);
#83403=ORIENTED_EDGE('',*,*,#54408,.F.);
#83404=ORIENTED_EDGE('',*,*,#56414,.F.);
#83405=ORIENTED_EDGE('',*,*,#56389,.F.);
#83406=ORIENTED_EDGE('',*,*,#56415,.T.);
#83407=ORIENTED_EDGE('',*,*,#56390,.F.);
#83408=ORIENTED_EDGE('',*,*,#56414,.T.);
#83409=ORIENTED_EDGE('',*,*,#55056,.F.);
#83410=ORIENTED_EDGE('',*,*,#56416,.T.);
#83411=ORIENTED_EDGE('',*,*,#56391,.F.);
#83412=ORIENTED_EDGE('',*,*,#56415,.F.);
#83413=ORIENTED_EDGE('',*,*,#54639,.F.);
#83414=ORIENTED_EDGE('',*,*,#54089,.T.);
#83415=ORIENTED_EDGE('',*,*,#56407,.T.);
#83416=ORIENTED_EDGE('',*,*,#56416,.F.);
#83417=ORIENTED_EDGE('',*,*,#54638,.T.);
#83418=ORIENTED_EDGE('',*,*,#56406,.T.);
#83419=ORIENTED_EDGE('',*,*,#56408,.T.);
#83420=ORIENTED_EDGE('',*,*,#54088,.T.);
#83421=ORIENTED_EDGE('',*,*,#56404,.T.);
#83422=ORIENTED_EDGE('',*,*,#56417,.T.);
#83423=ORIENTED_EDGE('',*,*,#56418,.T.);
#83424=ORIENTED_EDGE('',*,*,#56419,.T.);
#83425=ORIENTED_EDGE('',*,*,#56420,.T.);
#83426=ORIENTED_EDGE('',*,*,#56421,.T.);
#83427=ORIENTED_EDGE('',*,*,#56422,.T.);
#83428=ORIENTED_EDGE('',*,*,#56423,.T.);
#83429=ORIENTED_EDGE('',*,*,#56424,.F.);
#83430=ORIENTED_EDGE('',*,*,#56425,.T.);
#83431=ORIENTED_EDGE('',*,*,#56426,.T.);
#83432=ORIENTED_EDGE('',*,*,#56424,.T.);
#83433=ORIENTED_EDGE('',*,*,#56427,.T.);
#83434=ORIENTED_EDGE('',*,*,#56428,.T.);
#83435=ORIENTED_EDGE('',*,*,#56417,.F.);
#83436=ORIENTED_EDGE('',*,*,#56429,.T.);
#83437=ORIENTED_EDGE('',*,*,#56430,.T.);
#83438=ORIENTED_EDGE('',*,*,#56431,.F.);
#83439=ORIENTED_EDGE('',*,*,#56425,.F.);
#83440=ORIENTED_EDGE('',*,*,#56432,.F.);
#83441=ORIENTED_EDGE('',*,*,#56433,.F.);
#83442=ORIENTED_EDGE('',*,*,#56432,.T.);
#83443=ORIENTED_EDGE('',*,*,#56430,.F.);
#83444=ORIENTED_EDGE('',*,*,#56429,.F.);
#83445=ORIENTED_EDGE('',*,*,#56434,.F.);
#83446=ORIENTED_EDGE('',*,*,#56435,.F.);
#83447=ORIENTED_EDGE('',*,*,#56434,.T.);
#83448=ORIENTED_EDGE('',*,*,#56421,.F.);
#83449=ORIENTED_EDGE('',*,*,#56436,.F.);
#83450=ORIENTED_EDGE('',*,*,#56437,.F.);
#83451=ORIENTED_EDGE('',*,*,#56438,.T.);
#83452=ORIENTED_EDGE('',*,*,#56431,.T.);
#83453=ORIENTED_EDGE('',*,*,#54087,.F.);
#83454=ORIENTED_EDGE('',*,*,#54632,.T.);
#83455=ORIENTED_EDGE('',*,*,#56439,.F.);
#83456=ORIENTED_EDGE('',*,*,#56426,.F.);
#83457=ORIENTED_EDGE('',*,*,#56438,.F.);
#83458=ORIENTED_EDGE('',*,*,#54631,.F.);
#83459=ORIENTED_EDGE('',*,*,#56439,.T.);
#83460=ORIENTED_EDGE('',*,*,#55053,.F.);
#83461=ORIENTED_EDGE('',*,*,#56440,.F.);
#83462=ORIENTED_EDGE('',*,*,#56422,.F.);
#83463=ORIENTED_EDGE('',*,*,#56440,.T.);
#83464=ORIENTED_EDGE('',*,*,#54414,.F.);
#83465=ORIENTED_EDGE('',*,*,#56441,.F.);
#83466=ORIENTED_EDGE('',*,*,#56423,.F.);
#83467=ORIENTED_EDGE('',*,*,#56441,.T.);
#83468=ORIENTED_EDGE('',*,*,#54413,.F.);
#83469=ORIENTED_EDGE('',*,*,#56442,.F.);
#83470=ORIENTED_EDGE('',*,*,#56428,.F.);
#83471=ORIENTED_EDGE('',*,*,#56427,.F.);
#83472=ORIENTED_EDGE('',*,*,#56442,.T.);
#83473=ORIENTED_EDGE('',*,*,#54412,.F.);
#83474=ORIENTED_EDGE('',*,*,#56443,.F.);
#83475=ORIENTED_EDGE('',*,*,#56418,.F.);
#83476=ORIENTED_EDGE('',*,*,#56444,.T.);
#83477=ORIENTED_EDGE('',*,*,#56419,.F.);
#83478=ORIENTED_EDGE('',*,*,#56443,.T.);
#83479=ORIENTED_EDGE('',*,*,#55054,.F.);
#83480=ORIENTED_EDGE('',*,*,#56445,.T.);
#83481=ORIENTED_EDGE('',*,*,#56420,.F.);
#83482=ORIENTED_EDGE('',*,*,#56444,.F.);
#83483=ORIENTED_EDGE('',*,*,#54634,.F.);
#83484=ORIENTED_EDGE('',*,*,#54085,.T.);
#83485=ORIENTED_EDGE('',*,*,#56436,.T.);
#83486=ORIENTED_EDGE('',*,*,#56445,.F.);
#83487=ORIENTED_EDGE('',*,*,#54633,.T.);
#83488=ORIENTED_EDGE('',*,*,#56435,.T.);
#83489=ORIENTED_EDGE('',*,*,#56437,.T.);
#83490=ORIENTED_EDGE('',*,*,#54084,.T.);
#83491=ORIENTED_EDGE('',*,*,#56433,.T.);
#83492=ORIENTED_EDGE('',*,*,#56446,.T.);
#83493=ORIENTED_EDGE('',*,*,#56447,.T.);
#83494=ORIENTED_EDGE('',*,*,#56448,.T.);
#83495=ORIENTED_EDGE('',*,*,#56449,.T.);
#83496=ORIENTED_EDGE('',*,*,#56450,.T.);
#83497=ORIENTED_EDGE('',*,*,#56451,.T.);
#83498=ORIENTED_EDGE('',*,*,#56452,.T.);
#83499=ORIENTED_EDGE('',*,*,#56453,.F.);
#83500=ORIENTED_EDGE('',*,*,#56454,.T.);
#83501=ORIENTED_EDGE('',*,*,#56455,.T.);
#83502=ORIENTED_EDGE('',*,*,#56453,.T.);
#83503=ORIENTED_EDGE('',*,*,#56456,.T.);
#83504=ORIENTED_EDGE('',*,*,#56457,.T.);
#83505=ORIENTED_EDGE('',*,*,#56446,.F.);
#83506=ORIENTED_EDGE('',*,*,#56458,.T.);
#83507=ORIENTED_EDGE('',*,*,#56459,.T.);
#83508=ORIENTED_EDGE('',*,*,#56460,.F.);
#83509=ORIENTED_EDGE('',*,*,#56454,.F.);
#83510=ORIENTED_EDGE('',*,*,#56461,.F.);
#83511=ORIENTED_EDGE('',*,*,#56462,.F.);
#83512=ORIENTED_EDGE('',*,*,#56461,.T.);
#83513=ORIENTED_EDGE('',*,*,#56459,.F.);
#83514=ORIENTED_EDGE('',*,*,#56458,.F.);
#83515=ORIENTED_EDGE('',*,*,#56463,.F.);
#83516=ORIENTED_EDGE('',*,*,#56464,.F.);
#83517=ORIENTED_EDGE('',*,*,#56463,.T.);
#83518=ORIENTED_EDGE('',*,*,#56450,.F.);
#83519=ORIENTED_EDGE('',*,*,#56465,.F.);
#83520=ORIENTED_EDGE('',*,*,#56466,.F.);
#83521=ORIENTED_EDGE('',*,*,#56467,.T.);
#83522=ORIENTED_EDGE('',*,*,#56460,.T.);
#83523=ORIENTED_EDGE('',*,*,#54083,.F.);
#83524=ORIENTED_EDGE('',*,*,#54627,.T.);
#83525=ORIENTED_EDGE('',*,*,#56468,.F.);
#83526=ORIENTED_EDGE('',*,*,#56455,.F.);
#83527=ORIENTED_EDGE('',*,*,#56467,.F.);
#83528=ORIENTED_EDGE('',*,*,#54626,.F.);
#83529=ORIENTED_EDGE('',*,*,#56468,.T.);
#83530=ORIENTED_EDGE('',*,*,#55051,.F.);
#83531=ORIENTED_EDGE('',*,*,#56469,.F.);
#83532=ORIENTED_EDGE('',*,*,#56451,.F.);
#83533=ORIENTED_EDGE('',*,*,#56469,.T.);
#83534=ORIENTED_EDGE('',*,*,#54418,.F.);
#83535=ORIENTED_EDGE('',*,*,#56470,.F.);
#83536=ORIENTED_EDGE('',*,*,#56452,.F.);
#83537=ORIENTED_EDGE('',*,*,#56470,.T.);
#83538=ORIENTED_EDGE('',*,*,#54417,.F.);
#83539=ORIENTED_EDGE('',*,*,#56471,.F.);
#83540=ORIENTED_EDGE('',*,*,#56457,.F.);
#83541=ORIENTED_EDGE('',*,*,#56456,.F.);
#83542=ORIENTED_EDGE('',*,*,#56471,.T.);
#83543=ORIENTED_EDGE('',*,*,#54416,.F.);
#83544=ORIENTED_EDGE('',*,*,#56472,.F.);
#83545=ORIENTED_EDGE('',*,*,#56447,.F.);
#83546=ORIENTED_EDGE('',*,*,#56473,.T.);
#83547=ORIENTED_EDGE('',*,*,#56448,.F.);
#83548=ORIENTED_EDGE('',*,*,#56472,.T.);
#83549=ORIENTED_EDGE('',*,*,#55052,.F.);
#83550=ORIENTED_EDGE('',*,*,#56474,.T.);
#83551=ORIENTED_EDGE('',*,*,#56449,.F.);
#83552=ORIENTED_EDGE('',*,*,#56473,.F.);
#83553=ORIENTED_EDGE('',*,*,#54629,.F.);
#83554=ORIENTED_EDGE('',*,*,#54081,.T.);
#83555=ORIENTED_EDGE('',*,*,#56465,.T.);
#83556=ORIENTED_EDGE('',*,*,#56474,.F.);
#83557=ORIENTED_EDGE('',*,*,#54628,.T.);
#83558=ORIENTED_EDGE('',*,*,#56464,.T.);
#83559=ORIENTED_EDGE('',*,*,#56466,.T.);
#83560=ORIENTED_EDGE('',*,*,#54080,.T.);
#83561=ORIENTED_EDGE('',*,*,#56462,.T.);
#83562=ORIENTED_EDGE('',*,*,#56475,.T.);
#83563=ORIENTED_EDGE('',*,*,#56476,.T.);
#83564=ORIENTED_EDGE('',*,*,#56477,.T.);
#83565=ORIENTED_EDGE('',*,*,#56478,.T.);
#83566=ORIENTED_EDGE('',*,*,#56479,.T.);
#83567=ORIENTED_EDGE('',*,*,#56480,.T.);
#83568=ORIENTED_EDGE('',*,*,#56481,.T.);
#83569=ORIENTED_EDGE('',*,*,#56482,.F.);
#83570=ORIENTED_EDGE('',*,*,#56483,.T.);
#83571=ORIENTED_EDGE('',*,*,#56484,.T.);
#83572=ORIENTED_EDGE('',*,*,#56482,.T.);
#83573=ORIENTED_EDGE('',*,*,#56485,.T.);
#83574=ORIENTED_EDGE('',*,*,#56486,.T.);
#83575=ORIENTED_EDGE('',*,*,#56475,.F.);
#83576=ORIENTED_EDGE('',*,*,#56487,.T.);
#83577=ORIENTED_EDGE('',*,*,#56488,.T.);
#83578=ORIENTED_EDGE('',*,*,#56489,.F.);
#83579=ORIENTED_EDGE('',*,*,#56483,.F.);
#83580=ORIENTED_EDGE('',*,*,#56490,.F.);
#83581=ORIENTED_EDGE('',*,*,#56491,.F.);
#83582=ORIENTED_EDGE('',*,*,#56490,.T.);
#83583=ORIENTED_EDGE('',*,*,#56488,.F.);
#83584=ORIENTED_EDGE('',*,*,#56487,.F.);
#83585=ORIENTED_EDGE('',*,*,#56492,.F.);
#83586=ORIENTED_EDGE('',*,*,#56493,.F.);
#83587=ORIENTED_EDGE('',*,*,#56492,.T.);
#83588=ORIENTED_EDGE('',*,*,#56479,.F.);
#83589=ORIENTED_EDGE('',*,*,#56494,.F.);
#83590=ORIENTED_EDGE('',*,*,#56495,.F.);
#83591=ORIENTED_EDGE('',*,*,#56496,.T.);
#83592=ORIENTED_EDGE('',*,*,#56489,.T.);
#83593=ORIENTED_EDGE('',*,*,#54079,.F.);
#83594=ORIENTED_EDGE('',*,*,#54622,.T.);
#83595=ORIENTED_EDGE('',*,*,#56497,.F.);
#83596=ORIENTED_EDGE('',*,*,#56484,.F.);
#83597=ORIENTED_EDGE('',*,*,#56496,.F.);
#83598=ORIENTED_EDGE('',*,*,#54621,.F.);
#83599=ORIENTED_EDGE('',*,*,#56497,.T.);
#83600=ORIENTED_EDGE('',*,*,#55049,.F.);
#83601=ORIENTED_EDGE('',*,*,#56498,.F.);
#83602=ORIENTED_EDGE('',*,*,#56480,.F.);
#83603=ORIENTED_EDGE('',*,*,#56498,.T.);
#83604=ORIENTED_EDGE('',*,*,#54422,.F.);
#83605=ORIENTED_EDGE('',*,*,#56499,.F.);
#83606=ORIENTED_EDGE('',*,*,#56481,.F.);
#83607=ORIENTED_EDGE('',*,*,#56499,.T.);
#83608=ORIENTED_EDGE('',*,*,#54421,.F.);
#83609=ORIENTED_EDGE('',*,*,#56500,.F.);
#83610=ORIENTED_EDGE('',*,*,#56486,.F.);
#83611=ORIENTED_EDGE('',*,*,#56485,.F.);
#83612=ORIENTED_EDGE('',*,*,#56500,.T.);
#83613=ORIENTED_EDGE('',*,*,#54420,.F.);
#83614=ORIENTED_EDGE('',*,*,#56501,.F.);
#83615=ORIENTED_EDGE('',*,*,#56476,.F.);
#83616=ORIENTED_EDGE('',*,*,#56502,.T.);
#83617=ORIENTED_EDGE('',*,*,#56477,.F.);
#83618=ORIENTED_EDGE('',*,*,#56501,.T.);
#83619=ORIENTED_EDGE('',*,*,#55050,.F.);
#83620=ORIENTED_EDGE('',*,*,#56503,.T.);
#83621=ORIENTED_EDGE('',*,*,#56478,.F.);
#83622=ORIENTED_EDGE('',*,*,#56502,.F.);
#83623=ORIENTED_EDGE('',*,*,#54624,.F.);
#83624=ORIENTED_EDGE('',*,*,#54077,.T.);
#83625=ORIENTED_EDGE('',*,*,#56494,.T.);
#83626=ORIENTED_EDGE('',*,*,#56503,.F.);
#83627=ORIENTED_EDGE('',*,*,#54623,.T.);
#83628=ORIENTED_EDGE('',*,*,#56493,.T.);
#83629=ORIENTED_EDGE('',*,*,#56495,.T.);
#83630=ORIENTED_EDGE('',*,*,#54076,.T.);
#83631=ORIENTED_EDGE('',*,*,#56491,.T.);
#83632=ORIENTED_EDGE('',*,*,#56504,.T.);
#83633=ORIENTED_EDGE('',*,*,#56505,.T.);
#83634=ORIENTED_EDGE('',*,*,#56506,.T.);
#83635=ORIENTED_EDGE('',*,*,#56507,.T.);
#83636=ORIENTED_EDGE('',*,*,#56508,.T.);
#83637=ORIENTED_EDGE('',*,*,#56509,.T.);
#83638=ORIENTED_EDGE('',*,*,#56510,.T.);
#83639=ORIENTED_EDGE('',*,*,#56511,.F.);
#83640=ORIENTED_EDGE('',*,*,#56512,.T.);
#83641=ORIENTED_EDGE('',*,*,#56513,.T.);
#83642=ORIENTED_EDGE('',*,*,#56511,.T.);
#83643=ORIENTED_EDGE('',*,*,#56514,.T.);
#83644=ORIENTED_EDGE('',*,*,#56515,.T.);
#83645=ORIENTED_EDGE('',*,*,#56504,.F.);
#83646=ORIENTED_EDGE('',*,*,#56516,.T.);
#83647=ORIENTED_EDGE('',*,*,#56517,.T.);
#83648=ORIENTED_EDGE('',*,*,#56518,.F.);
#83649=ORIENTED_EDGE('',*,*,#56512,.F.);
#83650=ORIENTED_EDGE('',*,*,#56519,.F.);
#83651=ORIENTED_EDGE('',*,*,#56520,.F.);
#83652=ORIENTED_EDGE('',*,*,#56519,.T.);
#83653=ORIENTED_EDGE('',*,*,#56517,.F.);
#83654=ORIENTED_EDGE('',*,*,#56516,.F.);
#83655=ORIENTED_EDGE('',*,*,#56521,.F.);
#83656=ORIENTED_EDGE('',*,*,#56522,.F.);
#83657=ORIENTED_EDGE('',*,*,#56521,.T.);
#83658=ORIENTED_EDGE('',*,*,#56508,.F.);
#83659=ORIENTED_EDGE('',*,*,#56523,.F.);
#83660=ORIENTED_EDGE('',*,*,#56524,.F.);
#83661=ORIENTED_EDGE('',*,*,#56525,.T.);
#83662=ORIENTED_EDGE('',*,*,#56518,.T.);
#83663=ORIENTED_EDGE('',*,*,#54075,.F.);
#83664=ORIENTED_EDGE('',*,*,#54617,.T.);
#83665=ORIENTED_EDGE('',*,*,#56526,.F.);
#83666=ORIENTED_EDGE('',*,*,#56513,.F.);
#83667=ORIENTED_EDGE('',*,*,#56525,.F.);
#83668=ORIENTED_EDGE('',*,*,#54616,.F.);
#83669=ORIENTED_EDGE('',*,*,#56526,.T.);
#83670=ORIENTED_EDGE('',*,*,#55047,.F.);
#83671=ORIENTED_EDGE('',*,*,#56527,.F.);
#83672=ORIENTED_EDGE('',*,*,#56509,.F.);
#83673=ORIENTED_EDGE('',*,*,#56527,.T.);
#83674=ORIENTED_EDGE('',*,*,#54426,.F.);
#83675=ORIENTED_EDGE('',*,*,#56528,.F.);
#83676=ORIENTED_EDGE('',*,*,#56510,.F.);
#83677=ORIENTED_EDGE('',*,*,#56528,.T.);
#83678=ORIENTED_EDGE('',*,*,#54425,.F.);
#83679=ORIENTED_EDGE('',*,*,#56529,.F.);
#83680=ORIENTED_EDGE('',*,*,#56515,.F.);
#83681=ORIENTED_EDGE('',*,*,#56514,.F.);
#83682=ORIENTED_EDGE('',*,*,#56529,.T.);
#83683=ORIENTED_EDGE('',*,*,#54424,.F.);
#83684=ORIENTED_EDGE('',*,*,#56530,.F.);
#83685=ORIENTED_EDGE('',*,*,#56505,.F.);
#83686=ORIENTED_EDGE('',*,*,#56531,.T.);
#83687=ORIENTED_EDGE('',*,*,#56506,.F.);
#83688=ORIENTED_EDGE('',*,*,#56530,.T.);
#83689=ORIENTED_EDGE('',*,*,#55048,.F.);
#83690=ORIENTED_EDGE('',*,*,#56532,.T.);
#83691=ORIENTED_EDGE('',*,*,#56507,.F.);
#83692=ORIENTED_EDGE('',*,*,#56531,.F.);
#83693=ORIENTED_EDGE('',*,*,#54619,.F.);
#83694=ORIENTED_EDGE('',*,*,#54073,.T.);
#83695=ORIENTED_EDGE('',*,*,#56523,.T.);
#83696=ORIENTED_EDGE('',*,*,#56532,.F.);
#83697=ORIENTED_EDGE('',*,*,#54618,.T.);
#83698=ORIENTED_EDGE('',*,*,#56522,.T.);
#83699=ORIENTED_EDGE('',*,*,#56524,.T.);
#83700=ORIENTED_EDGE('',*,*,#54072,.T.);
#83701=ORIENTED_EDGE('',*,*,#56520,.T.);
#83702=ORIENTED_EDGE('',*,*,#56533,.T.);
#83703=ORIENTED_EDGE('',*,*,#56534,.T.);
#83704=ORIENTED_EDGE('',*,*,#56535,.T.);
#83705=ORIENTED_EDGE('',*,*,#56536,.T.);
#83706=ORIENTED_EDGE('',*,*,#56537,.T.);
#83707=ORIENTED_EDGE('',*,*,#56538,.T.);
#83708=ORIENTED_EDGE('',*,*,#56539,.T.);
#83709=ORIENTED_EDGE('',*,*,#56540,.F.);
#83710=ORIENTED_EDGE('',*,*,#56541,.T.);
#83711=ORIENTED_EDGE('',*,*,#56542,.T.);
#83712=ORIENTED_EDGE('',*,*,#56540,.T.);
#83713=ORIENTED_EDGE('',*,*,#56543,.T.);
#83714=ORIENTED_EDGE('',*,*,#56544,.T.);
#83715=ORIENTED_EDGE('',*,*,#56533,.F.);
#83716=ORIENTED_EDGE('',*,*,#56545,.T.);
#83717=ORIENTED_EDGE('',*,*,#56546,.T.);
#83718=ORIENTED_EDGE('',*,*,#56547,.F.);
#83719=ORIENTED_EDGE('',*,*,#56541,.F.);
#83720=ORIENTED_EDGE('',*,*,#56548,.F.);
#83721=ORIENTED_EDGE('',*,*,#56549,.F.);
#83722=ORIENTED_EDGE('',*,*,#56548,.T.);
#83723=ORIENTED_EDGE('',*,*,#56546,.F.);
#83724=ORIENTED_EDGE('',*,*,#56545,.F.);
#83725=ORIENTED_EDGE('',*,*,#56550,.F.);
#83726=ORIENTED_EDGE('',*,*,#56551,.F.);
#83727=ORIENTED_EDGE('',*,*,#56550,.T.);
#83728=ORIENTED_EDGE('',*,*,#56537,.F.);
#83729=ORIENTED_EDGE('',*,*,#56552,.F.);
#83730=ORIENTED_EDGE('',*,*,#56553,.F.);
#83731=ORIENTED_EDGE('',*,*,#56554,.T.);
#83732=ORIENTED_EDGE('',*,*,#56547,.T.);
#83733=ORIENTED_EDGE('',*,*,#54071,.F.);
#83734=ORIENTED_EDGE('',*,*,#54612,.T.);
#83735=ORIENTED_EDGE('',*,*,#56555,.F.);
#83736=ORIENTED_EDGE('',*,*,#56542,.F.);
#83737=ORIENTED_EDGE('',*,*,#56554,.F.);
#83738=ORIENTED_EDGE('',*,*,#54611,.F.);
#83739=ORIENTED_EDGE('',*,*,#56555,.T.);
#83740=ORIENTED_EDGE('',*,*,#55045,.F.);
#83741=ORIENTED_EDGE('',*,*,#56556,.F.);
#83742=ORIENTED_EDGE('',*,*,#56538,.F.);
#83743=ORIENTED_EDGE('',*,*,#56556,.T.);
#83744=ORIENTED_EDGE('',*,*,#54430,.F.);
#83745=ORIENTED_EDGE('',*,*,#56557,.F.);
#83746=ORIENTED_EDGE('',*,*,#56539,.F.);
#83747=ORIENTED_EDGE('',*,*,#56557,.T.);
#83748=ORIENTED_EDGE('',*,*,#54429,.F.);
#83749=ORIENTED_EDGE('',*,*,#56558,.F.);
#83750=ORIENTED_EDGE('',*,*,#56544,.F.);
#83751=ORIENTED_EDGE('',*,*,#56543,.F.);
#83752=ORIENTED_EDGE('',*,*,#56558,.T.);
#83753=ORIENTED_EDGE('',*,*,#54428,.F.);
#83754=ORIENTED_EDGE('',*,*,#56559,.F.);
#83755=ORIENTED_EDGE('',*,*,#56534,.F.);
#83756=ORIENTED_EDGE('',*,*,#56560,.T.);
#83757=ORIENTED_EDGE('',*,*,#56535,.F.);
#83758=ORIENTED_EDGE('',*,*,#56559,.T.);
#83759=ORIENTED_EDGE('',*,*,#55046,.F.);
#83760=ORIENTED_EDGE('',*,*,#56561,.T.);
#83761=ORIENTED_EDGE('',*,*,#56536,.F.);
#83762=ORIENTED_EDGE('',*,*,#56560,.F.);
#83763=ORIENTED_EDGE('',*,*,#54614,.F.);
#83764=ORIENTED_EDGE('',*,*,#54069,.T.);
#83765=ORIENTED_EDGE('',*,*,#56552,.T.);
#83766=ORIENTED_EDGE('',*,*,#56561,.F.);
#83767=ORIENTED_EDGE('',*,*,#54613,.T.);
#83768=ORIENTED_EDGE('',*,*,#56551,.T.);
#83769=ORIENTED_EDGE('',*,*,#56553,.T.);
#83770=ORIENTED_EDGE('',*,*,#54068,.T.);
#83771=ORIENTED_EDGE('',*,*,#56549,.T.);
#83772=ORIENTED_EDGE('',*,*,#56562,.T.);
#83773=ORIENTED_EDGE('',*,*,#56563,.T.);
#83774=ORIENTED_EDGE('',*,*,#56564,.T.);
#83775=ORIENTED_EDGE('',*,*,#56565,.T.);
#83776=ORIENTED_EDGE('',*,*,#56566,.T.);
#83777=ORIENTED_EDGE('',*,*,#56567,.T.);
#83778=ORIENTED_EDGE('',*,*,#56568,.T.);
#83779=ORIENTED_EDGE('',*,*,#56569,.F.);
#83780=ORIENTED_EDGE('',*,*,#56570,.T.);
#83781=ORIENTED_EDGE('',*,*,#56571,.T.);
#83782=ORIENTED_EDGE('',*,*,#56569,.T.);
#83783=ORIENTED_EDGE('',*,*,#56572,.T.);
#83784=ORIENTED_EDGE('',*,*,#56573,.T.);
#83785=ORIENTED_EDGE('',*,*,#56562,.F.);
#83786=ORIENTED_EDGE('',*,*,#56574,.T.);
#83787=ORIENTED_EDGE('',*,*,#56575,.T.);
#83788=ORIENTED_EDGE('',*,*,#56576,.F.);
#83789=ORIENTED_EDGE('',*,*,#56570,.F.);
#83790=ORIENTED_EDGE('',*,*,#56577,.F.);
#83791=ORIENTED_EDGE('',*,*,#56578,.F.);
#83792=ORIENTED_EDGE('',*,*,#56577,.T.);
#83793=ORIENTED_EDGE('',*,*,#56575,.F.);
#83794=ORIENTED_EDGE('',*,*,#56574,.F.);
#83795=ORIENTED_EDGE('',*,*,#56579,.F.);
#83796=ORIENTED_EDGE('',*,*,#56580,.F.);
#83797=ORIENTED_EDGE('',*,*,#56579,.T.);
#83798=ORIENTED_EDGE('',*,*,#56566,.F.);
#83799=ORIENTED_EDGE('',*,*,#56581,.F.);
#83800=ORIENTED_EDGE('',*,*,#56582,.F.);
#83801=ORIENTED_EDGE('',*,*,#56583,.T.);
#83802=ORIENTED_EDGE('',*,*,#56576,.T.);
#83803=ORIENTED_EDGE('',*,*,#54067,.F.);
#83804=ORIENTED_EDGE('',*,*,#54607,.T.);
#83805=ORIENTED_EDGE('',*,*,#56584,.F.);
#83806=ORIENTED_EDGE('',*,*,#56571,.F.);
#83807=ORIENTED_EDGE('',*,*,#56583,.F.);
#83808=ORIENTED_EDGE('',*,*,#54606,.F.);
#83809=ORIENTED_EDGE('',*,*,#56584,.T.);
#83810=ORIENTED_EDGE('',*,*,#55043,.F.);
#83811=ORIENTED_EDGE('',*,*,#56585,.F.);
#83812=ORIENTED_EDGE('',*,*,#56567,.F.);
#83813=ORIENTED_EDGE('',*,*,#56585,.T.);
#83814=ORIENTED_EDGE('',*,*,#54434,.F.);
#83815=ORIENTED_EDGE('',*,*,#56586,.F.);
#83816=ORIENTED_EDGE('',*,*,#56568,.F.);
#83817=ORIENTED_EDGE('',*,*,#56586,.T.);
#83818=ORIENTED_EDGE('',*,*,#54433,.F.);
#83819=ORIENTED_EDGE('',*,*,#56587,.F.);
#83820=ORIENTED_EDGE('',*,*,#56573,.F.);
#83821=ORIENTED_EDGE('',*,*,#56572,.F.);
#83822=ORIENTED_EDGE('',*,*,#56587,.T.);
#83823=ORIENTED_EDGE('',*,*,#54432,.F.);
#83824=ORIENTED_EDGE('',*,*,#56588,.F.);
#83825=ORIENTED_EDGE('',*,*,#56563,.F.);
#83826=ORIENTED_EDGE('',*,*,#56589,.T.);
#83827=ORIENTED_EDGE('',*,*,#56564,.F.);
#83828=ORIENTED_EDGE('',*,*,#56588,.T.);
#83829=ORIENTED_EDGE('',*,*,#55044,.F.);
#83830=ORIENTED_EDGE('',*,*,#56590,.T.);
#83831=ORIENTED_EDGE('',*,*,#56565,.F.);
#83832=ORIENTED_EDGE('',*,*,#56589,.F.);
#83833=ORIENTED_EDGE('',*,*,#54609,.F.);
#83834=ORIENTED_EDGE('',*,*,#54065,.T.);
#83835=ORIENTED_EDGE('',*,*,#56581,.T.);
#83836=ORIENTED_EDGE('',*,*,#56590,.F.);
#83837=ORIENTED_EDGE('',*,*,#54608,.T.);
#83838=ORIENTED_EDGE('',*,*,#56580,.T.);
#83839=ORIENTED_EDGE('',*,*,#56582,.T.);
#83840=ORIENTED_EDGE('',*,*,#54064,.T.);
#83841=ORIENTED_EDGE('',*,*,#56578,.T.);
#83842=ORIENTED_EDGE('',*,*,#56591,.T.);
#83843=ORIENTED_EDGE('',*,*,#56592,.T.);
#83844=ORIENTED_EDGE('',*,*,#56593,.T.);
#83845=ORIENTED_EDGE('',*,*,#56594,.T.);
#83846=ORIENTED_EDGE('',*,*,#56595,.T.);
#83847=ORIENTED_EDGE('',*,*,#56596,.T.);
#83848=ORIENTED_EDGE('',*,*,#56597,.T.);
#83849=ORIENTED_EDGE('',*,*,#56598,.F.);
#83850=ORIENTED_EDGE('',*,*,#56599,.T.);
#83851=ORIENTED_EDGE('',*,*,#56600,.T.);
#83852=ORIENTED_EDGE('',*,*,#56598,.T.);
#83853=ORIENTED_EDGE('',*,*,#56601,.T.);
#83854=ORIENTED_EDGE('',*,*,#56602,.T.);
#83855=ORIENTED_EDGE('',*,*,#56591,.F.);
#83856=ORIENTED_EDGE('',*,*,#56603,.T.);
#83857=ORIENTED_EDGE('',*,*,#56604,.T.);
#83858=ORIENTED_EDGE('',*,*,#56605,.F.);
#83859=ORIENTED_EDGE('',*,*,#56599,.F.);
#83860=ORIENTED_EDGE('',*,*,#56606,.F.);
#83861=ORIENTED_EDGE('',*,*,#56607,.F.);
#83862=ORIENTED_EDGE('',*,*,#56606,.T.);
#83863=ORIENTED_EDGE('',*,*,#56604,.F.);
#83864=ORIENTED_EDGE('',*,*,#56603,.F.);
#83865=ORIENTED_EDGE('',*,*,#56608,.F.);
#83866=ORIENTED_EDGE('',*,*,#56609,.F.);
#83867=ORIENTED_EDGE('',*,*,#56608,.T.);
#83868=ORIENTED_EDGE('',*,*,#56595,.F.);
#83869=ORIENTED_EDGE('',*,*,#56610,.F.);
#83870=ORIENTED_EDGE('',*,*,#56611,.F.);
#83871=ORIENTED_EDGE('',*,*,#56612,.T.);
#83872=ORIENTED_EDGE('',*,*,#56605,.T.);
#83873=ORIENTED_EDGE('',*,*,#54063,.F.);
#83874=ORIENTED_EDGE('',*,*,#54602,.T.);
#83875=ORIENTED_EDGE('',*,*,#56613,.F.);
#83876=ORIENTED_EDGE('',*,*,#56600,.F.);
#83877=ORIENTED_EDGE('',*,*,#56612,.F.);
#83878=ORIENTED_EDGE('',*,*,#54601,.F.);
#83879=ORIENTED_EDGE('',*,*,#56613,.T.);
#83880=ORIENTED_EDGE('',*,*,#54987,.F.);
#83881=ORIENTED_EDGE('',*,*,#56614,.F.);
#83882=ORIENTED_EDGE('',*,*,#56596,.F.);
#83883=ORIENTED_EDGE('',*,*,#56614,.T.);
#83884=ORIENTED_EDGE('',*,*,#54438,.F.);
#83885=ORIENTED_EDGE('',*,*,#56615,.F.);
#83886=ORIENTED_EDGE('',*,*,#56597,.F.);
#83887=ORIENTED_EDGE('',*,*,#56615,.T.);
#83888=ORIENTED_EDGE('',*,*,#54437,.F.);
#83889=ORIENTED_EDGE('',*,*,#56616,.F.);
#83890=ORIENTED_EDGE('',*,*,#56602,.F.);
#83891=ORIENTED_EDGE('',*,*,#56601,.F.);
#83892=ORIENTED_EDGE('',*,*,#56616,.T.);
#83893=ORIENTED_EDGE('',*,*,#54436,.F.);
#83894=ORIENTED_EDGE('',*,*,#56617,.F.);
#83895=ORIENTED_EDGE('',*,*,#56592,.F.);
#83896=ORIENTED_EDGE('',*,*,#56618,.T.);
#83897=ORIENTED_EDGE('',*,*,#56593,.F.);
#83898=ORIENTED_EDGE('',*,*,#56617,.T.);
#83899=ORIENTED_EDGE('',*,*,#55042,.F.);
#83900=ORIENTED_EDGE('',*,*,#56619,.T.);
#83901=ORIENTED_EDGE('',*,*,#56594,.F.);
#83902=ORIENTED_EDGE('',*,*,#56618,.F.);
#83903=ORIENTED_EDGE('',*,*,#54604,.F.);
#83904=ORIENTED_EDGE('',*,*,#54061,.T.);
#83905=ORIENTED_EDGE('',*,*,#56610,.T.);
#83906=ORIENTED_EDGE('',*,*,#56619,.F.);
#83907=ORIENTED_EDGE('',*,*,#54603,.T.);
#83908=ORIENTED_EDGE('',*,*,#56609,.T.);
#83909=ORIENTED_EDGE('',*,*,#56611,.T.);
#83910=ORIENTED_EDGE('',*,*,#54060,.T.);
#83911=ORIENTED_EDGE('',*,*,#56607,.T.);
#83912=ORIENTED_EDGE('',*,*,#56620,.T.);
#83913=ORIENTED_EDGE('',*,*,#56621,.T.);
#83914=ORIENTED_EDGE('',*,*,#56622,.T.);
#83915=ORIENTED_EDGE('',*,*,#56623,.T.);
#83916=ORIENTED_EDGE('',*,*,#56624,.T.);
#83917=ORIENTED_EDGE('',*,*,#56625,.T.);
#83918=ORIENTED_EDGE('',*,*,#56626,.T.);
#83919=ORIENTED_EDGE('',*,*,#56627,.F.);
#83920=ORIENTED_EDGE('',*,*,#56628,.T.);
#83921=ORIENTED_EDGE('',*,*,#56629,.T.);
#83922=ORIENTED_EDGE('',*,*,#56627,.T.);
#83923=ORIENTED_EDGE('',*,*,#56630,.T.);
#83924=ORIENTED_EDGE('',*,*,#56631,.T.);
#83925=ORIENTED_EDGE('',*,*,#56620,.F.);
#83926=ORIENTED_EDGE('',*,*,#56632,.T.);
#83927=ORIENTED_EDGE('',*,*,#56633,.T.);
#83928=ORIENTED_EDGE('',*,*,#56634,.F.);
#83929=ORIENTED_EDGE('',*,*,#56628,.F.);
#83930=ORIENTED_EDGE('',*,*,#56635,.F.);
#83931=ORIENTED_EDGE('',*,*,#56636,.F.);
#83932=ORIENTED_EDGE('',*,*,#56635,.T.);
#83933=ORIENTED_EDGE('',*,*,#56633,.F.);
#83934=ORIENTED_EDGE('',*,*,#56632,.F.);
#83935=ORIENTED_EDGE('',*,*,#56637,.F.);
#83936=ORIENTED_EDGE('',*,*,#56638,.F.);
#83937=ORIENTED_EDGE('',*,*,#56637,.T.);
#83938=ORIENTED_EDGE('',*,*,#56624,.F.);
#83939=ORIENTED_EDGE('',*,*,#56639,.F.);
#83940=ORIENTED_EDGE('',*,*,#56640,.F.);
#83941=ORIENTED_EDGE('',*,*,#56641,.T.);
#83942=ORIENTED_EDGE('',*,*,#56634,.T.);
#83943=ORIENTED_EDGE('',*,*,#54059,.F.);
#83944=ORIENTED_EDGE('',*,*,#54983,.T.);
#83945=ORIENTED_EDGE('',*,*,#56642,.F.);
#83946=ORIENTED_EDGE('',*,*,#56629,.F.);
#83947=ORIENTED_EDGE('',*,*,#56641,.F.);
#83948=ORIENTED_EDGE('',*,*,#54982,.F.);
#83949=ORIENTED_EDGE('',*,*,#56642,.T.);
#83950=ORIENTED_EDGE('',*,*,#55041,.F.);
#83951=ORIENTED_EDGE('',*,*,#56643,.F.);
#83952=ORIENTED_EDGE('',*,*,#56625,.F.);
#83953=ORIENTED_EDGE('',*,*,#56643,.T.);
#83954=ORIENTED_EDGE('',*,*,#54446,.F.);
#83955=ORIENTED_EDGE('',*,*,#56644,.F.);
#83956=ORIENTED_EDGE('',*,*,#56626,.F.);
#83957=ORIENTED_EDGE('',*,*,#56644,.T.);
#83958=ORIENTED_EDGE('',*,*,#54445,.F.);
#83959=ORIENTED_EDGE('',*,*,#56645,.F.);
#83960=ORIENTED_EDGE('',*,*,#56631,.F.);
#83961=ORIENTED_EDGE('',*,*,#56630,.F.);
#83962=ORIENTED_EDGE('',*,*,#56645,.T.);
#83963=ORIENTED_EDGE('',*,*,#54444,.F.);
#83964=ORIENTED_EDGE('',*,*,#56646,.F.);
#83965=ORIENTED_EDGE('',*,*,#56621,.F.);
#83966=ORIENTED_EDGE('',*,*,#56647,.T.);
#83967=ORIENTED_EDGE('',*,*,#56622,.F.);
#83968=ORIENTED_EDGE('',*,*,#56646,.T.);
#83969=ORIENTED_EDGE('',*,*,#54986,.F.);
#83970=ORIENTED_EDGE('',*,*,#56648,.T.);
#83971=ORIENTED_EDGE('',*,*,#56623,.F.);
#83972=ORIENTED_EDGE('',*,*,#56647,.F.);
#83973=ORIENTED_EDGE('',*,*,#54985,.F.);
#83974=ORIENTED_EDGE('',*,*,#54057,.T.);
#83975=ORIENTED_EDGE('',*,*,#56639,.T.);
#83976=ORIENTED_EDGE('',*,*,#56648,.F.);
#83977=ORIENTED_EDGE('',*,*,#54984,.T.);
#83978=ORIENTED_EDGE('',*,*,#56638,.T.);
#83979=ORIENTED_EDGE('',*,*,#56640,.T.);
#83980=ORIENTED_EDGE('',*,*,#54056,.T.);
#83981=ORIENTED_EDGE('',*,*,#56636,.T.);
#83982=ORIENTED_EDGE('',*,*,#56649,.T.);
#83983=ORIENTED_EDGE('',*,*,#56650,.T.);
#83984=ORIENTED_EDGE('',*,*,#56651,.T.);
#83985=ORIENTED_EDGE('',*,*,#56652,.T.);
#83986=ORIENTED_EDGE('',*,*,#56653,.T.);
#83987=ORIENTED_EDGE('',*,*,#56654,.T.);
#83988=ORIENTED_EDGE('',*,*,#56655,.T.);
#83989=ORIENTED_EDGE('',*,*,#56656,.F.);
#83990=ORIENTED_EDGE('',*,*,#56657,.T.);
#83991=ORIENTED_EDGE('',*,*,#56658,.T.);
#83992=ORIENTED_EDGE('',*,*,#56656,.T.);
#83993=ORIENTED_EDGE('',*,*,#56659,.T.);
#83994=ORIENTED_EDGE('',*,*,#56660,.T.);
#83995=ORIENTED_EDGE('',*,*,#56649,.F.);
#83996=ORIENTED_EDGE('',*,*,#56661,.T.);
#83997=ORIENTED_EDGE('',*,*,#56662,.T.);
#83998=ORIENTED_EDGE('',*,*,#56663,.F.);
#83999=ORIENTED_EDGE('',*,*,#56657,.F.);
#84000=ORIENTED_EDGE('',*,*,#56664,.F.);
#84001=ORIENTED_EDGE('',*,*,#56665,.F.);
#84002=ORIENTED_EDGE('',*,*,#56664,.T.);
#84003=ORIENTED_EDGE('',*,*,#56662,.F.);
#84004=ORIENTED_EDGE('',*,*,#56661,.F.);
#84005=ORIENTED_EDGE('',*,*,#56666,.F.);
#84006=ORIENTED_EDGE('',*,*,#56667,.F.);
#84007=ORIENTED_EDGE('',*,*,#56666,.T.);
#84008=ORIENTED_EDGE('',*,*,#56653,.F.);
#84009=ORIENTED_EDGE('',*,*,#56668,.F.);
#84010=ORIENTED_EDGE('',*,*,#56669,.F.);
#84011=ORIENTED_EDGE('',*,*,#56670,.T.);
#84012=ORIENTED_EDGE('',*,*,#56663,.T.);
#84013=ORIENTED_EDGE('',*,*,#54055,.F.);
#84014=ORIENTED_EDGE('',*,*,#54978,.T.);
#84015=ORIENTED_EDGE('',*,*,#56671,.F.);
#84016=ORIENTED_EDGE('',*,*,#56658,.F.);
#84017=ORIENTED_EDGE('',*,*,#56670,.F.);
#84018=ORIENTED_EDGE('',*,*,#54977,.F.);
#84019=ORIENTED_EDGE('',*,*,#56671,.T.);
#84020=ORIENTED_EDGE('',*,*,#55039,.F.);
#84021=ORIENTED_EDGE('',*,*,#56672,.F.);
#84022=ORIENTED_EDGE('',*,*,#56654,.F.);
#84023=ORIENTED_EDGE('',*,*,#56672,.T.);
#84024=ORIENTED_EDGE('',*,*,#54450,.F.);
#84025=ORIENTED_EDGE('',*,*,#56673,.F.);
#84026=ORIENTED_EDGE('',*,*,#56655,.F.);
#84027=ORIENTED_EDGE('',*,*,#56673,.T.);
#84028=ORIENTED_EDGE('',*,*,#54449,.F.);
#84029=ORIENTED_EDGE('',*,*,#56674,.F.);
#84030=ORIENTED_EDGE('',*,*,#56660,.F.);
#84031=ORIENTED_EDGE('',*,*,#56659,.F.);
#84032=ORIENTED_EDGE('',*,*,#56674,.T.);
#84033=ORIENTED_EDGE('',*,*,#54448,.F.);
#84034=ORIENTED_EDGE('',*,*,#56675,.F.);
#84035=ORIENTED_EDGE('',*,*,#56650,.F.);
#84036=ORIENTED_EDGE('',*,*,#56676,.T.);
#84037=ORIENTED_EDGE('',*,*,#56651,.F.);
#84038=ORIENTED_EDGE('',*,*,#56675,.T.);
#84039=ORIENTED_EDGE('',*,*,#55040,.F.);
#84040=ORIENTED_EDGE('',*,*,#56677,.T.);
#84041=ORIENTED_EDGE('',*,*,#56652,.F.);
#84042=ORIENTED_EDGE('',*,*,#56676,.F.);
#84043=ORIENTED_EDGE('',*,*,#54980,.F.);
#84044=ORIENTED_EDGE('',*,*,#54053,.T.);
#84045=ORIENTED_EDGE('',*,*,#56668,.T.);
#84046=ORIENTED_EDGE('',*,*,#56677,.F.);
#84047=ORIENTED_EDGE('',*,*,#54979,.T.);
#84048=ORIENTED_EDGE('',*,*,#56667,.T.);
#84049=ORIENTED_EDGE('',*,*,#56669,.T.);
#84050=ORIENTED_EDGE('',*,*,#54052,.T.);
#84051=ORIENTED_EDGE('',*,*,#56665,.T.);
#84052=ORIENTED_EDGE('',*,*,#56678,.T.);
#84053=ORIENTED_EDGE('',*,*,#56679,.T.);
#84054=ORIENTED_EDGE('',*,*,#56680,.T.);
#84055=ORIENTED_EDGE('',*,*,#56681,.T.);
#84056=ORIENTED_EDGE('',*,*,#56682,.T.);
#84057=ORIENTED_EDGE('',*,*,#56683,.T.);
#84058=ORIENTED_EDGE('',*,*,#56684,.T.);
#84059=ORIENTED_EDGE('',*,*,#56685,.F.);
#84060=ORIENTED_EDGE('',*,*,#56686,.T.);
#84061=ORIENTED_EDGE('',*,*,#56687,.T.);
#84062=ORIENTED_EDGE('',*,*,#56685,.T.);
#84063=ORIENTED_EDGE('',*,*,#56688,.T.);
#84064=ORIENTED_EDGE('',*,*,#56689,.T.);
#84065=ORIENTED_EDGE('',*,*,#56678,.F.);
#84066=ORIENTED_EDGE('',*,*,#56690,.T.);
#84067=ORIENTED_EDGE('',*,*,#56691,.T.);
#84068=ORIENTED_EDGE('',*,*,#56692,.F.);
#84069=ORIENTED_EDGE('',*,*,#56686,.F.);
#84070=ORIENTED_EDGE('',*,*,#56693,.F.);
#84071=ORIENTED_EDGE('',*,*,#56694,.F.);
#84072=ORIENTED_EDGE('',*,*,#56693,.T.);
#84073=ORIENTED_EDGE('',*,*,#56691,.F.);
#84074=ORIENTED_EDGE('',*,*,#56690,.F.);
#84075=ORIENTED_EDGE('',*,*,#56695,.F.);
#84076=ORIENTED_EDGE('',*,*,#56696,.F.);
#84077=ORIENTED_EDGE('',*,*,#56695,.T.);
#84078=ORIENTED_EDGE('',*,*,#56682,.F.);
#84079=ORIENTED_EDGE('',*,*,#56697,.F.);
#84080=ORIENTED_EDGE('',*,*,#56698,.F.);
#84081=ORIENTED_EDGE('',*,*,#56699,.T.);
#84082=ORIENTED_EDGE('',*,*,#56692,.T.);
#84083=ORIENTED_EDGE('',*,*,#54051,.F.);
#84084=ORIENTED_EDGE('',*,*,#54973,.T.);
#84085=ORIENTED_EDGE('',*,*,#56700,.F.);
#84086=ORIENTED_EDGE('',*,*,#56687,.F.);
#84087=ORIENTED_EDGE('',*,*,#56699,.F.);
#84088=ORIENTED_EDGE('',*,*,#54972,.F.);
#84089=ORIENTED_EDGE('',*,*,#56700,.T.);
#84090=ORIENTED_EDGE('',*,*,#55037,.F.);
#84091=ORIENTED_EDGE('',*,*,#56701,.F.);
#84092=ORIENTED_EDGE('',*,*,#56683,.F.);
#84093=ORIENTED_EDGE('',*,*,#56701,.T.);
#84094=ORIENTED_EDGE('',*,*,#54454,.F.);
#84095=ORIENTED_EDGE('',*,*,#56702,.F.);
#84096=ORIENTED_EDGE('',*,*,#56684,.F.);
#84097=ORIENTED_EDGE('',*,*,#56702,.T.);
#84098=ORIENTED_EDGE('',*,*,#54453,.F.);
#84099=ORIENTED_EDGE('',*,*,#56703,.F.);
#84100=ORIENTED_EDGE('',*,*,#56689,.F.);
#84101=ORIENTED_EDGE('',*,*,#56688,.F.);
#84102=ORIENTED_EDGE('',*,*,#56703,.T.);
#84103=ORIENTED_EDGE('',*,*,#54452,.F.);
#84104=ORIENTED_EDGE('',*,*,#56704,.F.);
#84105=ORIENTED_EDGE('',*,*,#56679,.F.);
#84106=ORIENTED_EDGE('',*,*,#56705,.T.);
#84107=ORIENTED_EDGE('',*,*,#56680,.F.);
#84108=ORIENTED_EDGE('',*,*,#56704,.T.);
#84109=ORIENTED_EDGE('',*,*,#55038,.F.);
#84110=ORIENTED_EDGE('',*,*,#56706,.T.);
#84111=ORIENTED_EDGE('',*,*,#56681,.F.);
#84112=ORIENTED_EDGE('',*,*,#56705,.F.);
#84113=ORIENTED_EDGE('',*,*,#54975,.F.);
#84114=ORIENTED_EDGE('',*,*,#54049,.T.);
#84115=ORIENTED_EDGE('',*,*,#56697,.T.);
#84116=ORIENTED_EDGE('',*,*,#56706,.F.);
#84117=ORIENTED_EDGE('',*,*,#54974,.T.);
#84118=ORIENTED_EDGE('',*,*,#56696,.T.);
#84119=ORIENTED_EDGE('',*,*,#56698,.T.);
#84120=ORIENTED_EDGE('',*,*,#54048,.T.);
#84121=ORIENTED_EDGE('',*,*,#56694,.T.);
#84122=ORIENTED_EDGE('',*,*,#56707,.T.);
#84123=ORIENTED_EDGE('',*,*,#56708,.T.);
#84124=ORIENTED_EDGE('',*,*,#56709,.T.);
#84125=ORIENTED_EDGE('',*,*,#56710,.T.);
#84126=ORIENTED_EDGE('',*,*,#56711,.T.);
#84127=ORIENTED_EDGE('',*,*,#56712,.T.);
#84128=ORIENTED_EDGE('',*,*,#56713,.T.);
#84129=ORIENTED_EDGE('',*,*,#56714,.F.);
#84130=ORIENTED_EDGE('',*,*,#56715,.T.);
#84131=ORIENTED_EDGE('',*,*,#56716,.T.);
#84132=ORIENTED_EDGE('',*,*,#56714,.T.);
#84133=ORIENTED_EDGE('',*,*,#56717,.T.);
#84134=ORIENTED_EDGE('',*,*,#56718,.T.);
#84135=ORIENTED_EDGE('',*,*,#56707,.F.);
#84136=ORIENTED_EDGE('',*,*,#56719,.T.);
#84137=ORIENTED_EDGE('',*,*,#56720,.T.);
#84138=ORIENTED_EDGE('',*,*,#56721,.F.);
#84139=ORIENTED_EDGE('',*,*,#56715,.F.);
#84140=ORIENTED_EDGE('',*,*,#56722,.F.);
#84141=ORIENTED_EDGE('',*,*,#56723,.F.);
#84142=ORIENTED_EDGE('',*,*,#56722,.T.);
#84143=ORIENTED_EDGE('',*,*,#56720,.F.);
#84144=ORIENTED_EDGE('',*,*,#56719,.F.);
#84145=ORIENTED_EDGE('',*,*,#56724,.F.);
#84146=ORIENTED_EDGE('',*,*,#56725,.F.);
#84147=ORIENTED_EDGE('',*,*,#56724,.T.);
#84148=ORIENTED_EDGE('',*,*,#56711,.F.);
#84149=ORIENTED_EDGE('',*,*,#56726,.F.);
#84150=ORIENTED_EDGE('',*,*,#56727,.F.);
#84151=ORIENTED_EDGE('',*,*,#56728,.T.);
#84152=ORIENTED_EDGE('',*,*,#56721,.T.);
#84153=ORIENTED_EDGE('',*,*,#54047,.F.);
#84154=ORIENTED_EDGE('',*,*,#54968,.T.);
#84155=ORIENTED_EDGE('',*,*,#56729,.F.);
#84156=ORIENTED_EDGE('',*,*,#56716,.F.);
#84157=ORIENTED_EDGE('',*,*,#56728,.F.);
#84158=ORIENTED_EDGE('',*,*,#54967,.F.);
#84159=ORIENTED_EDGE('',*,*,#56729,.T.);
#84160=ORIENTED_EDGE('',*,*,#55035,.F.);
#84161=ORIENTED_EDGE('',*,*,#56730,.F.);
#84162=ORIENTED_EDGE('',*,*,#56712,.F.);
#84163=ORIENTED_EDGE('',*,*,#56730,.T.);
#84164=ORIENTED_EDGE('',*,*,#54458,.F.);
#84165=ORIENTED_EDGE('',*,*,#56731,.F.);
#84166=ORIENTED_EDGE('',*,*,#56713,.F.);
#84167=ORIENTED_EDGE('',*,*,#56731,.T.);
#84168=ORIENTED_EDGE('',*,*,#54457,.F.);
#84169=ORIENTED_EDGE('',*,*,#56732,.F.);
#84170=ORIENTED_EDGE('',*,*,#56718,.F.);
#84171=ORIENTED_EDGE('',*,*,#56717,.F.);
#84172=ORIENTED_EDGE('',*,*,#56732,.T.);
#84173=ORIENTED_EDGE('',*,*,#54456,.F.);
#84174=ORIENTED_EDGE('',*,*,#56733,.F.);
#84175=ORIENTED_EDGE('',*,*,#56708,.F.);
#84176=ORIENTED_EDGE('',*,*,#56734,.T.);
#84177=ORIENTED_EDGE('',*,*,#56709,.F.);
#84178=ORIENTED_EDGE('',*,*,#56733,.T.);
#84179=ORIENTED_EDGE('',*,*,#55036,.F.);
#84180=ORIENTED_EDGE('',*,*,#56735,.T.);
#84181=ORIENTED_EDGE('',*,*,#56710,.F.);
#84182=ORIENTED_EDGE('',*,*,#56734,.F.);
#84183=ORIENTED_EDGE('',*,*,#54970,.F.);
#84184=ORIENTED_EDGE('',*,*,#54045,.T.);
#84185=ORIENTED_EDGE('',*,*,#56726,.T.);
#84186=ORIENTED_EDGE('',*,*,#56735,.F.);
#84187=ORIENTED_EDGE('',*,*,#54969,.T.);
#84188=ORIENTED_EDGE('',*,*,#56725,.T.);
#84189=ORIENTED_EDGE('',*,*,#56727,.T.);
#84190=ORIENTED_EDGE('',*,*,#54044,.T.);
#84191=ORIENTED_EDGE('',*,*,#56723,.T.);
#84192=ORIENTED_EDGE('',*,*,#56736,.T.);
#84193=ORIENTED_EDGE('',*,*,#56737,.T.);
#84194=ORIENTED_EDGE('',*,*,#56738,.T.);
#84195=ORIENTED_EDGE('',*,*,#56739,.T.);
#84196=ORIENTED_EDGE('',*,*,#56740,.T.);
#84197=ORIENTED_EDGE('',*,*,#56741,.T.);
#84198=ORIENTED_EDGE('',*,*,#56742,.T.);
#84199=ORIENTED_EDGE('',*,*,#56743,.F.);
#84200=ORIENTED_EDGE('',*,*,#56744,.T.);
#84201=ORIENTED_EDGE('',*,*,#56745,.T.);
#84202=ORIENTED_EDGE('',*,*,#56743,.T.);
#84203=ORIENTED_EDGE('',*,*,#56746,.T.);
#84204=ORIENTED_EDGE('',*,*,#56747,.T.);
#84205=ORIENTED_EDGE('',*,*,#56736,.F.);
#84206=ORIENTED_EDGE('',*,*,#56748,.T.);
#84207=ORIENTED_EDGE('',*,*,#56749,.T.);
#84208=ORIENTED_EDGE('',*,*,#56750,.F.);
#84209=ORIENTED_EDGE('',*,*,#56744,.F.);
#84210=ORIENTED_EDGE('',*,*,#56751,.F.);
#84211=ORIENTED_EDGE('',*,*,#56752,.F.);
#84212=ORIENTED_EDGE('',*,*,#56751,.T.);
#84213=ORIENTED_EDGE('',*,*,#56749,.F.);
#84214=ORIENTED_EDGE('',*,*,#56748,.F.);
#84215=ORIENTED_EDGE('',*,*,#56753,.F.);
#84216=ORIENTED_EDGE('',*,*,#56754,.F.);
#84217=ORIENTED_EDGE('',*,*,#56753,.T.);
#84218=ORIENTED_EDGE('',*,*,#56740,.F.);
#84219=ORIENTED_EDGE('',*,*,#56755,.F.);
#84220=ORIENTED_EDGE('',*,*,#56756,.F.);
#84221=ORIENTED_EDGE('',*,*,#56757,.T.);
#84222=ORIENTED_EDGE('',*,*,#56750,.T.);
#84223=ORIENTED_EDGE('',*,*,#54043,.F.);
#84224=ORIENTED_EDGE('',*,*,#54963,.T.);
#84225=ORIENTED_EDGE('',*,*,#56758,.F.);
#84226=ORIENTED_EDGE('',*,*,#56745,.F.);
#84227=ORIENTED_EDGE('',*,*,#56757,.F.);
#84228=ORIENTED_EDGE('',*,*,#54962,.F.);
#84229=ORIENTED_EDGE('',*,*,#56758,.T.);
#84230=ORIENTED_EDGE('',*,*,#55033,.F.);
#84231=ORIENTED_EDGE('',*,*,#56759,.F.);
#84232=ORIENTED_EDGE('',*,*,#56741,.F.);
#84233=ORIENTED_EDGE('',*,*,#56759,.T.);
#84234=ORIENTED_EDGE('',*,*,#54462,.F.);
#84235=ORIENTED_EDGE('',*,*,#56760,.F.);
#84236=ORIENTED_EDGE('',*,*,#56742,.F.);
#84237=ORIENTED_EDGE('',*,*,#56760,.T.);
#84238=ORIENTED_EDGE('',*,*,#54461,.F.);
#84239=ORIENTED_EDGE('',*,*,#56761,.F.);
#84240=ORIENTED_EDGE('',*,*,#56747,.F.);
#84241=ORIENTED_EDGE('',*,*,#56746,.F.);
#84242=ORIENTED_EDGE('',*,*,#56761,.T.);
#84243=ORIENTED_EDGE('',*,*,#54460,.F.);
#84244=ORIENTED_EDGE('',*,*,#56762,.F.);
#84245=ORIENTED_EDGE('',*,*,#56737,.F.);
#84246=ORIENTED_EDGE('',*,*,#56763,.T.);
#84247=ORIENTED_EDGE('',*,*,#56738,.F.);
#84248=ORIENTED_EDGE('',*,*,#56762,.T.);
#84249=ORIENTED_EDGE('',*,*,#55034,.F.);
#84250=ORIENTED_EDGE('',*,*,#56764,.T.);
#84251=ORIENTED_EDGE('',*,*,#56739,.F.);
#84252=ORIENTED_EDGE('',*,*,#56763,.F.);
#84253=ORIENTED_EDGE('',*,*,#54965,.F.);
#84254=ORIENTED_EDGE('',*,*,#54041,.T.);
#84255=ORIENTED_EDGE('',*,*,#56755,.T.);
#84256=ORIENTED_EDGE('',*,*,#56764,.F.);
#84257=ORIENTED_EDGE('',*,*,#54964,.T.);
#84258=ORIENTED_EDGE('',*,*,#56754,.T.);
#84259=ORIENTED_EDGE('',*,*,#56756,.T.);
#84260=ORIENTED_EDGE('',*,*,#54040,.T.);
#84261=ORIENTED_EDGE('',*,*,#56752,.T.);
#84262=ORIENTED_EDGE('',*,*,#56765,.T.);
#84263=ORIENTED_EDGE('',*,*,#56766,.T.);
#84264=ORIENTED_EDGE('',*,*,#56767,.T.);
#84265=ORIENTED_EDGE('',*,*,#56768,.T.);
#84266=ORIENTED_EDGE('',*,*,#56769,.T.);
#84267=ORIENTED_EDGE('',*,*,#56770,.T.);
#84268=ORIENTED_EDGE('',*,*,#56771,.T.);
#84269=ORIENTED_EDGE('',*,*,#56772,.F.);
#84270=ORIENTED_EDGE('',*,*,#56773,.T.);
#84271=ORIENTED_EDGE('',*,*,#56774,.T.);
#84272=ORIENTED_EDGE('',*,*,#56772,.T.);
#84273=ORIENTED_EDGE('',*,*,#56775,.T.);
#84274=ORIENTED_EDGE('',*,*,#56776,.T.);
#84275=ORIENTED_EDGE('',*,*,#56765,.F.);
#84276=ORIENTED_EDGE('',*,*,#56777,.T.);
#84277=ORIENTED_EDGE('',*,*,#56778,.T.);
#84278=ORIENTED_EDGE('',*,*,#56779,.F.);
#84279=ORIENTED_EDGE('',*,*,#56773,.F.);
#84280=ORIENTED_EDGE('',*,*,#56780,.F.);
#84281=ORIENTED_EDGE('',*,*,#56781,.F.);
#84282=ORIENTED_EDGE('',*,*,#56780,.T.);
#84283=ORIENTED_EDGE('',*,*,#56778,.F.);
#84284=ORIENTED_EDGE('',*,*,#56777,.F.);
#84285=ORIENTED_EDGE('',*,*,#56782,.F.);
#84286=ORIENTED_EDGE('',*,*,#56783,.F.);
#84287=ORIENTED_EDGE('',*,*,#56782,.T.);
#84288=ORIENTED_EDGE('',*,*,#56769,.F.);
#84289=ORIENTED_EDGE('',*,*,#56784,.F.);
#84290=ORIENTED_EDGE('',*,*,#56785,.F.);
#84291=ORIENTED_EDGE('',*,*,#56786,.T.);
#84292=ORIENTED_EDGE('',*,*,#56779,.T.);
#84293=ORIENTED_EDGE('',*,*,#54039,.F.);
#84294=ORIENTED_EDGE('',*,*,#54958,.T.);
#84295=ORIENTED_EDGE('',*,*,#56787,.F.);
#84296=ORIENTED_EDGE('',*,*,#56774,.F.);
#84297=ORIENTED_EDGE('',*,*,#56786,.F.);
#84298=ORIENTED_EDGE('',*,*,#54957,.F.);
#84299=ORIENTED_EDGE('',*,*,#56787,.T.);
#84300=ORIENTED_EDGE('',*,*,#55031,.F.);
#84301=ORIENTED_EDGE('',*,*,#56788,.F.);
#84302=ORIENTED_EDGE('',*,*,#56770,.F.);
#84303=ORIENTED_EDGE('',*,*,#56788,.T.);
#84304=ORIENTED_EDGE('',*,*,#54466,.F.);
#84305=ORIENTED_EDGE('',*,*,#56789,.F.);
#84306=ORIENTED_EDGE('',*,*,#56771,.F.);
#84307=ORIENTED_EDGE('',*,*,#56789,.T.);
#84308=ORIENTED_EDGE('',*,*,#54465,.F.);
#84309=ORIENTED_EDGE('',*,*,#56790,.F.);
#84310=ORIENTED_EDGE('',*,*,#56776,.F.);
#84311=ORIENTED_EDGE('',*,*,#56775,.F.);
#84312=ORIENTED_EDGE('',*,*,#56790,.T.);
#84313=ORIENTED_EDGE('',*,*,#54464,.F.);
#84314=ORIENTED_EDGE('',*,*,#56791,.F.);
#84315=ORIENTED_EDGE('',*,*,#56766,.F.);
#84316=ORIENTED_EDGE('',*,*,#56792,.T.);
#84317=ORIENTED_EDGE('',*,*,#56767,.F.);
#84318=ORIENTED_EDGE('',*,*,#56791,.T.);
#84319=ORIENTED_EDGE('',*,*,#55032,.F.);
#84320=ORIENTED_EDGE('',*,*,#56793,.T.);
#84321=ORIENTED_EDGE('',*,*,#56768,.F.);
#84322=ORIENTED_EDGE('',*,*,#56792,.F.);
#84323=ORIENTED_EDGE('',*,*,#54960,.F.);
#84324=ORIENTED_EDGE('',*,*,#54037,.T.);
#84325=ORIENTED_EDGE('',*,*,#56784,.T.);
#84326=ORIENTED_EDGE('',*,*,#56793,.F.);
#84327=ORIENTED_EDGE('',*,*,#54959,.T.);
#84328=ORIENTED_EDGE('',*,*,#56783,.T.);
#84329=ORIENTED_EDGE('',*,*,#56785,.T.);
#84330=ORIENTED_EDGE('',*,*,#54036,.T.);
#84331=ORIENTED_EDGE('',*,*,#56781,.T.);
#84332=ORIENTED_EDGE('',*,*,#56794,.T.);
#84333=ORIENTED_EDGE('',*,*,#56795,.T.);
#84334=ORIENTED_EDGE('',*,*,#56796,.T.);
#84335=ORIENTED_EDGE('',*,*,#56797,.T.);
#84336=ORIENTED_EDGE('',*,*,#56798,.T.);
#84337=ORIENTED_EDGE('',*,*,#56799,.T.);
#84338=ORIENTED_EDGE('',*,*,#56800,.T.);
#84339=ORIENTED_EDGE('',*,*,#56801,.F.);
#84340=ORIENTED_EDGE('',*,*,#56802,.T.);
#84341=ORIENTED_EDGE('',*,*,#56803,.T.);
#84342=ORIENTED_EDGE('',*,*,#56801,.T.);
#84343=ORIENTED_EDGE('',*,*,#56804,.T.);
#84344=ORIENTED_EDGE('',*,*,#56805,.T.);
#84345=ORIENTED_EDGE('',*,*,#56794,.F.);
#84346=ORIENTED_EDGE('',*,*,#56806,.T.);
#84347=ORIENTED_EDGE('',*,*,#56807,.T.);
#84348=ORIENTED_EDGE('',*,*,#56808,.F.);
#84349=ORIENTED_EDGE('',*,*,#56802,.F.);
#84350=ORIENTED_EDGE('',*,*,#56809,.F.);
#84351=ORIENTED_EDGE('',*,*,#56810,.F.);
#84352=ORIENTED_EDGE('',*,*,#56809,.T.);
#84353=ORIENTED_EDGE('',*,*,#56807,.F.);
#84354=ORIENTED_EDGE('',*,*,#56806,.F.);
#84355=ORIENTED_EDGE('',*,*,#56811,.F.);
#84356=ORIENTED_EDGE('',*,*,#56812,.F.);
#84357=ORIENTED_EDGE('',*,*,#56811,.T.);
#84358=ORIENTED_EDGE('',*,*,#56798,.F.);
#84359=ORIENTED_EDGE('',*,*,#56813,.F.);
#84360=ORIENTED_EDGE('',*,*,#56814,.F.);
#84361=ORIENTED_EDGE('',*,*,#56815,.T.);
#84362=ORIENTED_EDGE('',*,*,#56808,.T.);
#84363=ORIENTED_EDGE('',*,*,#54035,.F.);
#84364=ORIENTED_EDGE('',*,*,#54953,.T.);
#84365=ORIENTED_EDGE('',*,*,#56816,.F.);
#84366=ORIENTED_EDGE('',*,*,#56803,.F.);
#84367=ORIENTED_EDGE('',*,*,#56815,.F.);
#84368=ORIENTED_EDGE('',*,*,#54952,.F.);
#84369=ORIENTED_EDGE('',*,*,#56816,.T.);
#84370=ORIENTED_EDGE('',*,*,#55029,.F.);
#84371=ORIENTED_EDGE('',*,*,#56817,.F.);
#84372=ORIENTED_EDGE('',*,*,#56799,.F.);
#84373=ORIENTED_EDGE('',*,*,#56817,.T.);
#84374=ORIENTED_EDGE('',*,*,#54470,.F.);
#84375=ORIENTED_EDGE('',*,*,#56818,.F.);
#84376=ORIENTED_EDGE('',*,*,#56800,.F.);
#84377=ORIENTED_EDGE('',*,*,#56818,.T.);
#84378=ORIENTED_EDGE('',*,*,#54469,.F.);
#84379=ORIENTED_EDGE('',*,*,#56819,.F.);
#84380=ORIENTED_EDGE('',*,*,#56805,.F.);
#84381=ORIENTED_EDGE('',*,*,#56804,.F.);
#84382=ORIENTED_EDGE('',*,*,#56819,.T.);
#84383=ORIENTED_EDGE('',*,*,#54468,.F.);
#84384=ORIENTED_EDGE('',*,*,#56820,.F.);
#84385=ORIENTED_EDGE('',*,*,#56795,.F.);
#84386=ORIENTED_EDGE('',*,*,#56821,.T.);
#84387=ORIENTED_EDGE('',*,*,#56796,.F.);
#84388=ORIENTED_EDGE('',*,*,#56820,.T.);
#84389=ORIENTED_EDGE('',*,*,#55030,.F.);
#84390=ORIENTED_EDGE('',*,*,#56822,.T.);
#84391=ORIENTED_EDGE('',*,*,#56797,.F.);
#84392=ORIENTED_EDGE('',*,*,#56821,.F.);
#84393=ORIENTED_EDGE('',*,*,#54955,.F.);
#84394=ORIENTED_EDGE('',*,*,#54033,.T.);
#84395=ORIENTED_EDGE('',*,*,#56813,.T.);
#84396=ORIENTED_EDGE('',*,*,#56822,.F.);
#84397=ORIENTED_EDGE('',*,*,#54954,.T.);
#84398=ORIENTED_EDGE('',*,*,#56812,.T.);
#84399=ORIENTED_EDGE('',*,*,#56814,.T.);
#84400=ORIENTED_EDGE('',*,*,#54032,.T.);
#84401=ORIENTED_EDGE('',*,*,#56810,.T.);
#84402=ORIENTED_EDGE('',*,*,#56823,.T.);
#84403=ORIENTED_EDGE('',*,*,#56824,.T.);
#84404=ORIENTED_EDGE('',*,*,#56825,.T.);
#84405=ORIENTED_EDGE('',*,*,#56826,.T.);
#84406=ORIENTED_EDGE('',*,*,#56827,.T.);
#84407=ORIENTED_EDGE('',*,*,#56828,.T.);
#84408=ORIENTED_EDGE('',*,*,#56829,.T.);
#84409=ORIENTED_EDGE('',*,*,#56830,.F.);
#84410=ORIENTED_EDGE('',*,*,#56831,.T.);
#84411=ORIENTED_EDGE('',*,*,#56832,.T.);
#84412=ORIENTED_EDGE('',*,*,#56830,.T.);
#84413=ORIENTED_EDGE('',*,*,#56833,.T.);
#84414=ORIENTED_EDGE('',*,*,#56834,.T.);
#84415=ORIENTED_EDGE('',*,*,#56823,.F.);
#84416=ORIENTED_EDGE('',*,*,#56835,.T.);
#84417=ORIENTED_EDGE('',*,*,#56836,.T.);
#84418=ORIENTED_EDGE('',*,*,#56837,.F.);
#84419=ORIENTED_EDGE('',*,*,#56831,.F.);
#84420=ORIENTED_EDGE('',*,*,#56838,.F.);
#84421=ORIENTED_EDGE('',*,*,#56839,.F.);
#84422=ORIENTED_EDGE('',*,*,#56838,.T.);
#84423=ORIENTED_EDGE('',*,*,#56836,.F.);
#84424=ORIENTED_EDGE('',*,*,#56835,.F.);
#84425=ORIENTED_EDGE('',*,*,#56840,.F.);
#84426=ORIENTED_EDGE('',*,*,#56841,.F.);
#84427=ORIENTED_EDGE('',*,*,#56840,.T.);
#84428=ORIENTED_EDGE('',*,*,#56827,.F.);
#84429=ORIENTED_EDGE('',*,*,#56842,.F.);
#84430=ORIENTED_EDGE('',*,*,#56843,.F.);
#84431=ORIENTED_EDGE('',*,*,#56844,.T.);
#84432=ORIENTED_EDGE('',*,*,#56837,.T.);
#84433=ORIENTED_EDGE('',*,*,#54031,.F.);
#84434=ORIENTED_EDGE('',*,*,#54948,.T.);
#84435=ORIENTED_EDGE('',*,*,#56845,.F.);
#84436=ORIENTED_EDGE('',*,*,#56832,.F.);
#84437=ORIENTED_EDGE('',*,*,#56844,.F.);
#84438=ORIENTED_EDGE('',*,*,#54947,.F.);
#84439=ORIENTED_EDGE('',*,*,#56845,.T.);
#84440=ORIENTED_EDGE('',*,*,#55027,.F.);
#84441=ORIENTED_EDGE('',*,*,#56846,.F.);
#84442=ORIENTED_EDGE('',*,*,#56828,.F.);
#84443=ORIENTED_EDGE('',*,*,#56846,.T.);
#84444=ORIENTED_EDGE('',*,*,#54474,.F.);
#84445=ORIENTED_EDGE('',*,*,#56847,.F.);
#84446=ORIENTED_EDGE('',*,*,#56829,.F.);
#84447=ORIENTED_EDGE('',*,*,#56847,.T.);
#84448=ORIENTED_EDGE('',*,*,#54473,.F.);
#84449=ORIENTED_EDGE('',*,*,#56848,.F.);
#84450=ORIENTED_EDGE('',*,*,#56834,.F.);
#84451=ORIENTED_EDGE('',*,*,#56833,.F.);
#84452=ORIENTED_EDGE('',*,*,#56848,.T.);
#84453=ORIENTED_EDGE('',*,*,#54472,.F.);
#84454=ORIENTED_EDGE('',*,*,#56849,.F.);
#84455=ORIENTED_EDGE('',*,*,#56824,.F.);
#84456=ORIENTED_EDGE('',*,*,#56850,.T.);
#84457=ORIENTED_EDGE('',*,*,#56825,.F.);
#84458=ORIENTED_EDGE('',*,*,#56849,.T.);
#84459=ORIENTED_EDGE('',*,*,#55028,.F.);
#84460=ORIENTED_EDGE('',*,*,#56851,.T.);
#84461=ORIENTED_EDGE('',*,*,#56826,.F.);
#84462=ORIENTED_EDGE('',*,*,#56850,.F.);
#84463=ORIENTED_EDGE('',*,*,#54950,.F.);
#84464=ORIENTED_EDGE('',*,*,#54029,.T.);
#84465=ORIENTED_EDGE('',*,*,#56842,.T.);
#84466=ORIENTED_EDGE('',*,*,#56851,.F.);
#84467=ORIENTED_EDGE('',*,*,#54949,.T.);
#84468=ORIENTED_EDGE('',*,*,#56841,.T.);
#84469=ORIENTED_EDGE('',*,*,#56843,.T.);
#84470=ORIENTED_EDGE('',*,*,#54028,.T.);
#84471=ORIENTED_EDGE('',*,*,#56839,.T.);
#84472=ORIENTED_EDGE('',*,*,#56852,.T.);
#84473=ORIENTED_EDGE('',*,*,#56853,.T.);
#84474=ORIENTED_EDGE('',*,*,#56854,.T.);
#84475=ORIENTED_EDGE('',*,*,#56855,.T.);
#84476=ORIENTED_EDGE('',*,*,#56856,.T.);
#84477=ORIENTED_EDGE('',*,*,#56857,.T.);
#84478=ORIENTED_EDGE('',*,*,#56858,.T.);
#84479=ORIENTED_EDGE('',*,*,#56859,.F.);
#84480=ORIENTED_EDGE('',*,*,#56860,.T.);
#84481=ORIENTED_EDGE('',*,*,#56861,.T.);
#84482=ORIENTED_EDGE('',*,*,#56859,.T.);
#84483=ORIENTED_EDGE('',*,*,#56862,.T.);
#84484=ORIENTED_EDGE('',*,*,#56863,.T.);
#84485=ORIENTED_EDGE('',*,*,#56852,.F.);
#84486=ORIENTED_EDGE('',*,*,#56864,.T.);
#84487=ORIENTED_EDGE('',*,*,#56865,.T.);
#84488=ORIENTED_EDGE('',*,*,#56866,.F.);
#84489=ORIENTED_EDGE('',*,*,#56860,.F.);
#84490=ORIENTED_EDGE('',*,*,#56867,.F.);
#84491=ORIENTED_EDGE('',*,*,#56868,.F.);
#84492=ORIENTED_EDGE('',*,*,#56867,.T.);
#84493=ORIENTED_EDGE('',*,*,#56865,.F.);
#84494=ORIENTED_EDGE('',*,*,#56864,.F.);
#84495=ORIENTED_EDGE('',*,*,#56869,.F.);
#84496=ORIENTED_EDGE('',*,*,#56870,.F.);
#84497=ORIENTED_EDGE('',*,*,#56869,.T.);
#84498=ORIENTED_EDGE('',*,*,#56856,.F.);
#84499=ORIENTED_EDGE('',*,*,#56871,.F.);
#84500=ORIENTED_EDGE('',*,*,#56872,.F.);
#84501=ORIENTED_EDGE('',*,*,#56873,.T.);
#84502=ORIENTED_EDGE('',*,*,#56866,.T.);
#84503=ORIENTED_EDGE('',*,*,#54027,.F.);
#84504=ORIENTED_EDGE('',*,*,#54943,.T.);
#84505=ORIENTED_EDGE('',*,*,#56874,.F.);
#84506=ORIENTED_EDGE('',*,*,#56861,.F.);
#84507=ORIENTED_EDGE('',*,*,#56873,.F.);
#84508=ORIENTED_EDGE('',*,*,#54942,.F.);
#84509=ORIENTED_EDGE('',*,*,#56874,.T.);
#84510=ORIENTED_EDGE('',*,*,#55025,.F.);
#84511=ORIENTED_EDGE('',*,*,#56875,.F.);
#84512=ORIENTED_EDGE('',*,*,#56857,.F.);
#84513=ORIENTED_EDGE('',*,*,#56875,.T.);
#84514=ORIENTED_EDGE('',*,*,#54478,.F.);
#84515=ORIENTED_EDGE('',*,*,#56876,.F.);
#84516=ORIENTED_EDGE('',*,*,#56858,.F.);
#84517=ORIENTED_EDGE('',*,*,#56876,.T.);
#84518=ORIENTED_EDGE('',*,*,#54477,.F.);
#84519=ORIENTED_EDGE('',*,*,#56877,.F.);
#84520=ORIENTED_EDGE('',*,*,#56863,.F.);
#84521=ORIENTED_EDGE('',*,*,#56862,.F.);
#84522=ORIENTED_EDGE('',*,*,#56877,.T.);
#84523=ORIENTED_EDGE('',*,*,#54476,.F.);
#84524=ORIENTED_EDGE('',*,*,#56878,.F.);
#84525=ORIENTED_EDGE('',*,*,#56853,.F.);
#84526=ORIENTED_EDGE('',*,*,#56879,.T.);
#84527=ORIENTED_EDGE('',*,*,#56854,.F.);
#84528=ORIENTED_EDGE('',*,*,#56878,.T.);
#84529=ORIENTED_EDGE('',*,*,#55026,.F.);
#84530=ORIENTED_EDGE('',*,*,#56880,.T.);
#84531=ORIENTED_EDGE('',*,*,#56855,.F.);
#84532=ORIENTED_EDGE('',*,*,#56879,.F.);
#84533=ORIENTED_EDGE('',*,*,#54945,.F.);
#84534=ORIENTED_EDGE('',*,*,#54025,.T.);
#84535=ORIENTED_EDGE('',*,*,#56871,.T.);
#84536=ORIENTED_EDGE('',*,*,#56880,.F.);
#84537=ORIENTED_EDGE('',*,*,#54944,.T.);
#84538=ORIENTED_EDGE('',*,*,#56870,.T.);
#84539=ORIENTED_EDGE('',*,*,#56872,.T.);
#84540=ORIENTED_EDGE('',*,*,#54024,.T.);
#84541=ORIENTED_EDGE('',*,*,#56868,.T.);
#84542=ORIENTED_EDGE('',*,*,#56881,.T.);
#84543=ORIENTED_EDGE('',*,*,#56882,.T.);
#84544=ORIENTED_EDGE('',*,*,#56883,.T.);
#84545=ORIENTED_EDGE('',*,*,#56884,.T.);
#84546=ORIENTED_EDGE('',*,*,#56885,.T.);
#84547=ORIENTED_EDGE('',*,*,#56886,.T.);
#84548=ORIENTED_EDGE('',*,*,#56887,.T.);
#84549=ORIENTED_EDGE('',*,*,#56888,.F.);
#84550=ORIENTED_EDGE('',*,*,#56889,.T.);
#84551=ORIENTED_EDGE('',*,*,#56890,.T.);
#84552=ORIENTED_EDGE('',*,*,#56888,.T.);
#84553=ORIENTED_EDGE('',*,*,#56891,.T.);
#84554=ORIENTED_EDGE('',*,*,#56892,.T.);
#84555=ORIENTED_EDGE('',*,*,#56881,.F.);
#84556=ORIENTED_EDGE('',*,*,#56893,.T.);
#84557=ORIENTED_EDGE('',*,*,#56894,.T.);
#84558=ORIENTED_EDGE('',*,*,#56895,.F.);
#84559=ORIENTED_EDGE('',*,*,#56889,.F.);
#84560=ORIENTED_EDGE('',*,*,#56896,.F.);
#84561=ORIENTED_EDGE('',*,*,#56897,.F.);
#84562=ORIENTED_EDGE('',*,*,#56896,.T.);
#84563=ORIENTED_EDGE('',*,*,#56894,.F.);
#84564=ORIENTED_EDGE('',*,*,#56893,.F.);
#84565=ORIENTED_EDGE('',*,*,#56898,.F.);
#84566=ORIENTED_EDGE('',*,*,#56899,.F.);
#84567=ORIENTED_EDGE('',*,*,#56898,.T.);
#84568=ORIENTED_EDGE('',*,*,#56885,.F.);
#84569=ORIENTED_EDGE('',*,*,#56900,.F.);
#84570=ORIENTED_EDGE('',*,*,#56901,.F.);
#84571=ORIENTED_EDGE('',*,*,#56902,.T.);
#84572=ORIENTED_EDGE('',*,*,#56895,.T.);
#84573=ORIENTED_EDGE('',*,*,#54023,.F.);
#84574=ORIENTED_EDGE('',*,*,#54938,.T.);
#84575=ORIENTED_EDGE('',*,*,#56903,.F.);
#84576=ORIENTED_EDGE('',*,*,#56890,.F.);
#84577=ORIENTED_EDGE('',*,*,#56902,.F.);
#84578=ORIENTED_EDGE('',*,*,#54937,.F.);
#84579=ORIENTED_EDGE('',*,*,#56903,.T.);
#84580=ORIENTED_EDGE('',*,*,#55023,.F.);
#84581=ORIENTED_EDGE('',*,*,#56904,.F.);
#84582=ORIENTED_EDGE('',*,*,#56886,.F.);
#84583=ORIENTED_EDGE('',*,*,#56904,.T.);
#84584=ORIENTED_EDGE('',*,*,#54482,.F.);
#84585=ORIENTED_EDGE('',*,*,#56905,.F.);
#84586=ORIENTED_EDGE('',*,*,#56887,.F.);
#84587=ORIENTED_EDGE('',*,*,#56905,.T.);
#84588=ORIENTED_EDGE('',*,*,#54481,.F.);
#84589=ORIENTED_EDGE('',*,*,#56906,.F.);
#84590=ORIENTED_EDGE('',*,*,#56892,.F.);
#84591=ORIENTED_EDGE('',*,*,#56891,.F.);
#84592=ORIENTED_EDGE('',*,*,#56906,.T.);
#84593=ORIENTED_EDGE('',*,*,#54480,.F.);
#84594=ORIENTED_EDGE('',*,*,#56907,.F.);
#84595=ORIENTED_EDGE('',*,*,#56882,.F.);
#84596=ORIENTED_EDGE('',*,*,#56908,.T.);
#84597=ORIENTED_EDGE('',*,*,#56883,.F.);
#84598=ORIENTED_EDGE('',*,*,#56907,.T.);
#84599=ORIENTED_EDGE('',*,*,#55024,.F.);
#84600=ORIENTED_EDGE('',*,*,#56909,.T.);
#84601=ORIENTED_EDGE('',*,*,#56884,.F.);
#84602=ORIENTED_EDGE('',*,*,#56908,.F.);
#84603=ORIENTED_EDGE('',*,*,#54940,.F.);
#84604=ORIENTED_EDGE('',*,*,#54021,.T.);
#84605=ORIENTED_EDGE('',*,*,#56900,.T.);
#84606=ORIENTED_EDGE('',*,*,#56909,.F.);
#84607=ORIENTED_EDGE('',*,*,#54939,.T.);
#84608=ORIENTED_EDGE('',*,*,#56899,.T.);
#84609=ORIENTED_EDGE('',*,*,#56901,.T.);
#84610=ORIENTED_EDGE('',*,*,#54020,.T.);
#84611=ORIENTED_EDGE('',*,*,#56897,.T.);
#84612=ORIENTED_EDGE('',*,*,#56910,.T.);
#84613=ORIENTED_EDGE('',*,*,#56911,.T.);
#84614=ORIENTED_EDGE('',*,*,#56912,.T.);
#84615=ORIENTED_EDGE('',*,*,#56913,.T.);
#84616=ORIENTED_EDGE('',*,*,#56914,.T.);
#84617=ORIENTED_EDGE('',*,*,#56915,.T.);
#84618=ORIENTED_EDGE('',*,*,#56916,.T.);
#84619=ORIENTED_EDGE('',*,*,#56917,.F.);
#84620=ORIENTED_EDGE('',*,*,#56918,.T.);
#84621=ORIENTED_EDGE('',*,*,#56919,.T.);
#84622=ORIENTED_EDGE('',*,*,#56917,.T.);
#84623=ORIENTED_EDGE('',*,*,#56920,.T.);
#84624=ORIENTED_EDGE('',*,*,#56921,.T.);
#84625=ORIENTED_EDGE('',*,*,#56910,.F.);
#84626=ORIENTED_EDGE('',*,*,#56922,.T.);
#84627=ORIENTED_EDGE('',*,*,#56923,.T.);
#84628=ORIENTED_EDGE('',*,*,#56924,.F.);
#84629=ORIENTED_EDGE('',*,*,#56918,.F.);
#84630=ORIENTED_EDGE('',*,*,#56925,.F.);
#84631=ORIENTED_EDGE('',*,*,#56926,.F.);
#84632=ORIENTED_EDGE('',*,*,#56925,.T.);
#84633=ORIENTED_EDGE('',*,*,#56923,.F.);
#84634=ORIENTED_EDGE('',*,*,#56922,.F.);
#84635=ORIENTED_EDGE('',*,*,#56927,.F.);
#84636=ORIENTED_EDGE('',*,*,#56928,.F.);
#84637=ORIENTED_EDGE('',*,*,#56927,.T.);
#84638=ORIENTED_EDGE('',*,*,#56914,.F.);
#84639=ORIENTED_EDGE('',*,*,#56929,.F.);
#84640=ORIENTED_EDGE('',*,*,#56930,.F.);
#84641=ORIENTED_EDGE('',*,*,#56931,.T.);
#84642=ORIENTED_EDGE('',*,*,#56924,.T.);
#84643=ORIENTED_EDGE('',*,*,#54019,.F.);
#84644=ORIENTED_EDGE('',*,*,#54933,.T.);
#84645=ORIENTED_EDGE('',*,*,#56932,.F.);
#84646=ORIENTED_EDGE('',*,*,#56919,.F.);
#84647=ORIENTED_EDGE('',*,*,#56931,.F.);
#84648=ORIENTED_EDGE('',*,*,#54932,.F.);
#84649=ORIENTED_EDGE('',*,*,#56932,.T.);
#84650=ORIENTED_EDGE('',*,*,#55021,.F.);
#84651=ORIENTED_EDGE('',*,*,#56933,.F.);
#84652=ORIENTED_EDGE('',*,*,#56915,.F.);
#84653=ORIENTED_EDGE('',*,*,#56933,.T.);
#84654=ORIENTED_EDGE('',*,*,#54486,.F.);
#84655=ORIENTED_EDGE('',*,*,#56934,.F.);
#84656=ORIENTED_EDGE('',*,*,#56916,.F.);
#84657=ORIENTED_EDGE('',*,*,#56934,.T.);
#84658=ORIENTED_EDGE('',*,*,#54485,.F.);
#84659=ORIENTED_EDGE('',*,*,#56935,.F.);
#84660=ORIENTED_EDGE('',*,*,#56921,.F.);
#84661=ORIENTED_EDGE('',*,*,#56920,.F.);
#84662=ORIENTED_EDGE('',*,*,#56935,.T.);
#84663=ORIENTED_EDGE('',*,*,#54484,.F.);
#84664=ORIENTED_EDGE('',*,*,#56936,.F.);
#84665=ORIENTED_EDGE('',*,*,#56911,.F.);
#84666=ORIENTED_EDGE('',*,*,#56937,.T.);
#84667=ORIENTED_EDGE('',*,*,#56912,.F.);
#84668=ORIENTED_EDGE('',*,*,#56936,.T.);
#84669=ORIENTED_EDGE('',*,*,#55022,.F.);
#84670=ORIENTED_EDGE('',*,*,#56938,.T.);
#84671=ORIENTED_EDGE('',*,*,#56913,.F.);
#84672=ORIENTED_EDGE('',*,*,#56937,.F.);
#84673=ORIENTED_EDGE('',*,*,#54935,.F.);
#84674=ORIENTED_EDGE('',*,*,#54017,.T.);
#84675=ORIENTED_EDGE('',*,*,#56929,.T.);
#84676=ORIENTED_EDGE('',*,*,#56938,.F.);
#84677=ORIENTED_EDGE('',*,*,#54934,.T.);
#84678=ORIENTED_EDGE('',*,*,#56928,.T.);
#84679=ORIENTED_EDGE('',*,*,#56930,.T.);
#84680=ORIENTED_EDGE('',*,*,#54016,.T.);
#84681=ORIENTED_EDGE('',*,*,#56926,.T.);
#84682=ORIENTED_EDGE('',*,*,#56939,.T.);
#84683=ORIENTED_EDGE('',*,*,#56940,.T.);
#84684=ORIENTED_EDGE('',*,*,#56941,.T.);
#84685=ORIENTED_EDGE('',*,*,#56942,.T.);
#84686=ORIENTED_EDGE('',*,*,#56943,.T.);
#84687=ORIENTED_EDGE('',*,*,#56944,.T.);
#84688=ORIENTED_EDGE('',*,*,#56945,.T.);
#84689=ORIENTED_EDGE('',*,*,#56946,.F.);
#84690=ORIENTED_EDGE('',*,*,#56947,.T.);
#84691=ORIENTED_EDGE('',*,*,#56948,.T.);
#84692=ORIENTED_EDGE('',*,*,#56946,.T.);
#84693=ORIENTED_EDGE('',*,*,#56949,.T.);
#84694=ORIENTED_EDGE('',*,*,#56950,.T.);
#84695=ORIENTED_EDGE('',*,*,#56939,.F.);
#84696=ORIENTED_EDGE('',*,*,#56951,.T.);
#84697=ORIENTED_EDGE('',*,*,#56952,.T.);
#84698=ORIENTED_EDGE('',*,*,#56953,.F.);
#84699=ORIENTED_EDGE('',*,*,#56947,.F.);
#84700=ORIENTED_EDGE('',*,*,#56954,.F.);
#84701=ORIENTED_EDGE('',*,*,#56955,.F.);
#84702=ORIENTED_EDGE('',*,*,#56954,.T.);
#84703=ORIENTED_EDGE('',*,*,#56952,.F.);
#84704=ORIENTED_EDGE('',*,*,#56951,.F.);
#84705=ORIENTED_EDGE('',*,*,#56956,.F.);
#84706=ORIENTED_EDGE('',*,*,#56957,.F.);
#84707=ORIENTED_EDGE('',*,*,#56956,.T.);
#84708=ORIENTED_EDGE('',*,*,#56943,.F.);
#84709=ORIENTED_EDGE('',*,*,#56958,.F.);
#84710=ORIENTED_EDGE('',*,*,#56959,.F.);
#84711=ORIENTED_EDGE('',*,*,#56960,.T.);
#84712=ORIENTED_EDGE('',*,*,#56953,.T.);
#84713=ORIENTED_EDGE('',*,*,#54015,.F.);
#84714=ORIENTED_EDGE('',*,*,#54928,.T.);
#84715=ORIENTED_EDGE('',*,*,#56961,.F.);
#84716=ORIENTED_EDGE('',*,*,#56948,.F.);
#84717=ORIENTED_EDGE('',*,*,#56960,.F.);
#84718=ORIENTED_EDGE('',*,*,#54927,.F.);
#84719=ORIENTED_EDGE('',*,*,#56961,.T.);
#84720=ORIENTED_EDGE('',*,*,#55019,.F.);
#84721=ORIENTED_EDGE('',*,*,#56962,.F.);
#84722=ORIENTED_EDGE('',*,*,#56944,.F.);
#84723=ORIENTED_EDGE('',*,*,#56962,.T.);
#84724=ORIENTED_EDGE('',*,*,#54490,.F.);
#84725=ORIENTED_EDGE('',*,*,#56963,.F.);
#84726=ORIENTED_EDGE('',*,*,#56945,.F.);
#84727=ORIENTED_EDGE('',*,*,#56963,.T.);
#84728=ORIENTED_EDGE('',*,*,#54489,.F.);
#84729=ORIENTED_EDGE('',*,*,#56964,.F.);
#84730=ORIENTED_EDGE('',*,*,#56950,.F.);
#84731=ORIENTED_EDGE('',*,*,#56949,.F.);
#84732=ORIENTED_EDGE('',*,*,#56964,.T.);
#84733=ORIENTED_EDGE('',*,*,#54488,.F.);
#84734=ORIENTED_EDGE('',*,*,#56965,.F.);
#84735=ORIENTED_EDGE('',*,*,#56940,.F.);
#84736=ORIENTED_EDGE('',*,*,#56966,.T.);
#84737=ORIENTED_EDGE('',*,*,#56941,.F.);
#84738=ORIENTED_EDGE('',*,*,#56965,.T.);
#84739=ORIENTED_EDGE('',*,*,#55020,.F.);
#84740=ORIENTED_EDGE('',*,*,#56967,.T.);
#84741=ORIENTED_EDGE('',*,*,#56942,.F.);
#84742=ORIENTED_EDGE('',*,*,#56966,.F.);
#84743=ORIENTED_EDGE('',*,*,#54930,.F.);
#84744=ORIENTED_EDGE('',*,*,#54013,.T.);
#84745=ORIENTED_EDGE('',*,*,#56958,.T.);
#84746=ORIENTED_EDGE('',*,*,#56967,.F.);
#84747=ORIENTED_EDGE('',*,*,#54929,.T.);
#84748=ORIENTED_EDGE('',*,*,#56957,.T.);
#84749=ORIENTED_EDGE('',*,*,#56959,.T.);
#84750=ORIENTED_EDGE('',*,*,#54012,.T.);
#84751=ORIENTED_EDGE('',*,*,#56955,.T.);
#84752=ORIENTED_EDGE('',*,*,#56968,.T.);
#84753=ORIENTED_EDGE('',*,*,#56969,.T.);
#84754=ORIENTED_EDGE('',*,*,#56970,.T.);
#84755=ORIENTED_EDGE('',*,*,#56971,.T.);
#84756=ORIENTED_EDGE('',*,*,#56972,.T.);
#84757=ORIENTED_EDGE('',*,*,#56973,.T.);
#84758=ORIENTED_EDGE('',*,*,#56974,.T.);
#84759=ORIENTED_EDGE('',*,*,#56975,.F.);
#84760=ORIENTED_EDGE('',*,*,#56976,.T.);
#84761=ORIENTED_EDGE('',*,*,#56977,.T.);
#84762=ORIENTED_EDGE('',*,*,#56975,.T.);
#84763=ORIENTED_EDGE('',*,*,#56978,.T.);
#84764=ORIENTED_EDGE('',*,*,#56979,.T.);
#84765=ORIENTED_EDGE('',*,*,#56968,.F.);
#84766=ORIENTED_EDGE('',*,*,#56980,.T.);
#84767=ORIENTED_EDGE('',*,*,#56981,.T.);
#84768=ORIENTED_EDGE('',*,*,#56982,.F.);
#84769=ORIENTED_EDGE('',*,*,#56976,.F.);
#84770=ORIENTED_EDGE('',*,*,#56983,.F.);
#84771=ORIENTED_EDGE('',*,*,#56984,.F.);
#84772=ORIENTED_EDGE('',*,*,#56983,.T.);
#84773=ORIENTED_EDGE('',*,*,#56981,.F.);
#84774=ORIENTED_EDGE('',*,*,#56980,.F.);
#84775=ORIENTED_EDGE('',*,*,#56985,.F.);
#84776=ORIENTED_EDGE('',*,*,#56986,.F.);
#84777=ORIENTED_EDGE('',*,*,#56985,.T.);
#84778=ORIENTED_EDGE('',*,*,#56972,.F.);
#84779=ORIENTED_EDGE('',*,*,#56987,.F.);
#84780=ORIENTED_EDGE('',*,*,#56988,.F.);
#84781=ORIENTED_EDGE('',*,*,#56989,.T.);
#84782=ORIENTED_EDGE('',*,*,#56982,.T.);
#84783=ORIENTED_EDGE('',*,*,#54011,.F.);
#84784=ORIENTED_EDGE('',*,*,#54923,.T.);
#84785=ORIENTED_EDGE('',*,*,#56990,.F.);
#84786=ORIENTED_EDGE('',*,*,#56977,.F.);
#84787=ORIENTED_EDGE('',*,*,#56989,.F.);
#84788=ORIENTED_EDGE('',*,*,#54922,.F.);
#84789=ORIENTED_EDGE('',*,*,#56990,.T.);
#84790=ORIENTED_EDGE('',*,*,#55017,.F.);
#84791=ORIENTED_EDGE('',*,*,#56991,.F.);
#84792=ORIENTED_EDGE('',*,*,#56973,.F.);
#84793=ORIENTED_EDGE('',*,*,#56991,.T.);
#84794=ORIENTED_EDGE('',*,*,#54494,.F.);
#84795=ORIENTED_EDGE('',*,*,#56992,.F.);
#84796=ORIENTED_EDGE('',*,*,#56974,.F.);
#84797=ORIENTED_EDGE('',*,*,#56992,.T.);
#84798=ORIENTED_EDGE('',*,*,#54493,.F.);
#84799=ORIENTED_EDGE('',*,*,#56993,.F.);
#84800=ORIENTED_EDGE('',*,*,#56979,.F.);
#84801=ORIENTED_EDGE('',*,*,#56978,.F.);
#84802=ORIENTED_EDGE('',*,*,#56993,.T.);
#84803=ORIENTED_EDGE('',*,*,#54492,.F.);
#84804=ORIENTED_EDGE('',*,*,#56994,.F.);
#84805=ORIENTED_EDGE('',*,*,#56969,.F.);
#84806=ORIENTED_EDGE('',*,*,#56995,.T.);
#84807=ORIENTED_EDGE('',*,*,#56970,.F.);
#84808=ORIENTED_EDGE('',*,*,#56994,.T.);
#84809=ORIENTED_EDGE('',*,*,#55018,.F.);
#84810=ORIENTED_EDGE('',*,*,#56996,.T.);
#84811=ORIENTED_EDGE('',*,*,#56971,.F.);
#84812=ORIENTED_EDGE('',*,*,#56995,.F.);
#84813=ORIENTED_EDGE('',*,*,#54925,.F.);
#84814=ORIENTED_EDGE('',*,*,#54009,.T.);
#84815=ORIENTED_EDGE('',*,*,#56987,.T.);
#84816=ORIENTED_EDGE('',*,*,#56996,.F.);
#84817=ORIENTED_EDGE('',*,*,#54924,.T.);
#84818=ORIENTED_EDGE('',*,*,#56986,.T.);
#84819=ORIENTED_EDGE('',*,*,#56988,.T.);
#84820=ORIENTED_EDGE('',*,*,#54008,.T.);
#84821=ORIENTED_EDGE('',*,*,#56984,.T.);
#84822=ORIENTED_EDGE('',*,*,#56997,.T.);
#84823=ORIENTED_EDGE('',*,*,#56998,.T.);
#84824=ORIENTED_EDGE('',*,*,#56999,.T.);
#84825=ORIENTED_EDGE('',*,*,#57000,.T.);
#84826=ORIENTED_EDGE('',*,*,#57001,.T.);
#84827=ORIENTED_EDGE('',*,*,#57002,.T.);
#84828=ORIENTED_EDGE('',*,*,#57003,.T.);
#84829=ORIENTED_EDGE('',*,*,#57004,.F.);
#84830=ORIENTED_EDGE('',*,*,#57005,.T.);
#84831=ORIENTED_EDGE('',*,*,#57006,.T.);
#84832=ORIENTED_EDGE('',*,*,#57004,.T.);
#84833=ORIENTED_EDGE('',*,*,#57007,.T.);
#84834=ORIENTED_EDGE('',*,*,#57008,.T.);
#84835=ORIENTED_EDGE('',*,*,#56997,.F.);
#84836=ORIENTED_EDGE('',*,*,#57009,.T.);
#84837=ORIENTED_EDGE('',*,*,#57010,.T.);
#84838=ORIENTED_EDGE('',*,*,#57011,.F.);
#84839=ORIENTED_EDGE('',*,*,#57005,.F.);
#84840=ORIENTED_EDGE('',*,*,#57012,.F.);
#84841=ORIENTED_EDGE('',*,*,#57013,.F.);
#84842=ORIENTED_EDGE('',*,*,#57012,.T.);
#84843=ORIENTED_EDGE('',*,*,#57010,.F.);
#84844=ORIENTED_EDGE('',*,*,#57009,.F.);
#84845=ORIENTED_EDGE('',*,*,#57014,.F.);
#84846=ORIENTED_EDGE('',*,*,#57015,.F.);
#84847=ORIENTED_EDGE('',*,*,#57014,.T.);
#84848=ORIENTED_EDGE('',*,*,#57001,.F.);
#84849=ORIENTED_EDGE('',*,*,#57016,.F.);
#84850=ORIENTED_EDGE('',*,*,#57017,.F.);
#84851=ORIENTED_EDGE('',*,*,#57018,.T.);
#84852=ORIENTED_EDGE('',*,*,#57011,.T.);
#84853=ORIENTED_EDGE('',*,*,#54007,.F.);
#84854=ORIENTED_EDGE('',*,*,#54918,.T.);
#84855=ORIENTED_EDGE('',*,*,#57019,.F.);
#84856=ORIENTED_EDGE('',*,*,#57006,.F.);
#84857=ORIENTED_EDGE('',*,*,#57018,.F.);
#84858=ORIENTED_EDGE('',*,*,#54917,.F.);
#84859=ORIENTED_EDGE('',*,*,#57019,.T.);
#84860=ORIENTED_EDGE('',*,*,#55015,.F.);
#84861=ORIENTED_EDGE('',*,*,#57020,.F.);
#84862=ORIENTED_EDGE('',*,*,#57002,.F.);
#84863=ORIENTED_EDGE('',*,*,#57020,.T.);
#84864=ORIENTED_EDGE('',*,*,#54498,.F.);
#84865=ORIENTED_EDGE('',*,*,#57021,.F.);
#84866=ORIENTED_EDGE('',*,*,#57003,.F.);
#84867=ORIENTED_EDGE('',*,*,#57021,.T.);
#84868=ORIENTED_EDGE('',*,*,#54497,.F.);
#84869=ORIENTED_EDGE('',*,*,#57022,.F.);
#84870=ORIENTED_EDGE('',*,*,#57008,.F.);
#84871=ORIENTED_EDGE('',*,*,#57007,.F.);
#84872=ORIENTED_EDGE('',*,*,#57022,.T.);
#84873=ORIENTED_EDGE('',*,*,#54496,.F.);
#84874=ORIENTED_EDGE('',*,*,#57023,.F.);
#84875=ORIENTED_EDGE('',*,*,#56998,.F.);
#84876=ORIENTED_EDGE('',*,*,#57024,.T.);
#84877=ORIENTED_EDGE('',*,*,#56999,.F.);
#84878=ORIENTED_EDGE('',*,*,#57023,.T.);
#84879=ORIENTED_EDGE('',*,*,#55016,.F.);
#84880=ORIENTED_EDGE('',*,*,#57025,.T.);
#84881=ORIENTED_EDGE('',*,*,#57000,.F.);
#84882=ORIENTED_EDGE('',*,*,#57024,.F.);
#84883=ORIENTED_EDGE('',*,*,#54920,.F.);
#84884=ORIENTED_EDGE('',*,*,#54005,.T.);
#84885=ORIENTED_EDGE('',*,*,#57016,.T.);
#84886=ORIENTED_EDGE('',*,*,#57025,.F.);
#84887=ORIENTED_EDGE('',*,*,#54919,.T.);
#84888=ORIENTED_EDGE('',*,*,#57015,.T.);
#84889=ORIENTED_EDGE('',*,*,#57017,.T.);
#84890=ORIENTED_EDGE('',*,*,#54004,.T.);
#84891=ORIENTED_EDGE('',*,*,#57013,.T.);
#84892=ORIENTED_EDGE('',*,*,#57026,.T.);
#84893=ORIENTED_EDGE('',*,*,#57027,.T.);
#84894=ORIENTED_EDGE('',*,*,#57028,.T.);
#84895=ORIENTED_EDGE('',*,*,#57029,.T.);
#84896=ORIENTED_EDGE('',*,*,#57030,.T.);
#84897=ORIENTED_EDGE('',*,*,#57031,.T.);
#84898=ORIENTED_EDGE('',*,*,#57032,.T.);
#84899=ORIENTED_EDGE('',*,*,#57033,.F.);
#84900=ORIENTED_EDGE('',*,*,#57034,.T.);
#84901=ORIENTED_EDGE('',*,*,#57035,.T.);
#84902=ORIENTED_EDGE('',*,*,#57033,.T.);
#84903=ORIENTED_EDGE('',*,*,#57036,.T.);
#84904=ORIENTED_EDGE('',*,*,#57037,.T.);
#84905=ORIENTED_EDGE('',*,*,#57026,.F.);
#84906=ORIENTED_EDGE('',*,*,#57038,.T.);
#84907=ORIENTED_EDGE('',*,*,#57039,.T.);
#84908=ORIENTED_EDGE('',*,*,#57040,.F.);
#84909=ORIENTED_EDGE('',*,*,#57034,.F.);
#84910=ORIENTED_EDGE('',*,*,#57041,.F.);
#84911=ORIENTED_EDGE('',*,*,#57042,.F.);
#84912=ORIENTED_EDGE('',*,*,#57041,.T.);
#84913=ORIENTED_EDGE('',*,*,#57039,.F.);
#84914=ORIENTED_EDGE('',*,*,#57038,.F.);
#84915=ORIENTED_EDGE('',*,*,#57043,.F.);
#84916=ORIENTED_EDGE('',*,*,#57044,.F.);
#84917=ORIENTED_EDGE('',*,*,#57043,.T.);
#84918=ORIENTED_EDGE('',*,*,#57030,.F.);
#84919=ORIENTED_EDGE('',*,*,#57045,.F.);
#84920=ORIENTED_EDGE('',*,*,#57046,.F.);
#84921=ORIENTED_EDGE('',*,*,#57047,.T.);
#84922=ORIENTED_EDGE('',*,*,#57040,.T.);
#84923=ORIENTED_EDGE('',*,*,#54003,.F.);
#84924=ORIENTED_EDGE('',*,*,#54913,.T.);
#84925=ORIENTED_EDGE('',*,*,#57048,.F.);
#84926=ORIENTED_EDGE('',*,*,#57035,.F.);
#84927=ORIENTED_EDGE('',*,*,#57047,.F.);
#84928=ORIENTED_EDGE('',*,*,#54912,.F.);
#84929=ORIENTED_EDGE('',*,*,#57048,.T.);
#84930=ORIENTED_EDGE('',*,*,#55013,.F.);
#84931=ORIENTED_EDGE('',*,*,#57049,.F.);
#84932=ORIENTED_EDGE('',*,*,#57031,.F.);
#84933=ORIENTED_EDGE('',*,*,#57049,.T.);
#84934=ORIENTED_EDGE('',*,*,#54502,.F.);
#84935=ORIENTED_EDGE('',*,*,#57050,.F.);
#84936=ORIENTED_EDGE('',*,*,#57032,.F.);
#84937=ORIENTED_EDGE('',*,*,#57050,.T.);
#84938=ORIENTED_EDGE('',*,*,#54501,.F.);
#84939=ORIENTED_EDGE('',*,*,#57051,.F.);
#84940=ORIENTED_EDGE('',*,*,#57037,.F.);
#84941=ORIENTED_EDGE('',*,*,#57036,.F.);
#84942=ORIENTED_EDGE('',*,*,#57051,.T.);
#84943=ORIENTED_EDGE('',*,*,#54500,.F.);
#84944=ORIENTED_EDGE('',*,*,#57052,.F.);
#84945=ORIENTED_EDGE('',*,*,#57027,.F.);
#84946=ORIENTED_EDGE('',*,*,#57053,.T.);
#84947=ORIENTED_EDGE('',*,*,#57028,.F.);
#84948=ORIENTED_EDGE('',*,*,#57052,.T.);
#84949=ORIENTED_EDGE('',*,*,#55014,.F.);
#84950=ORIENTED_EDGE('',*,*,#57054,.T.);
#84951=ORIENTED_EDGE('',*,*,#57029,.F.);
#84952=ORIENTED_EDGE('',*,*,#57053,.F.);
#84953=ORIENTED_EDGE('',*,*,#54915,.F.);
#84954=ORIENTED_EDGE('',*,*,#54001,.T.);
#84955=ORIENTED_EDGE('',*,*,#57045,.T.);
#84956=ORIENTED_EDGE('',*,*,#57054,.F.);
#84957=ORIENTED_EDGE('',*,*,#54914,.T.);
#84958=ORIENTED_EDGE('',*,*,#57044,.T.);
#84959=ORIENTED_EDGE('',*,*,#57046,.T.);
#84960=ORIENTED_EDGE('',*,*,#54000,.T.);
#84961=ORIENTED_EDGE('',*,*,#57042,.T.);
#84962=ORIENTED_EDGE('',*,*,#57055,.T.);
#84963=ORIENTED_EDGE('',*,*,#57056,.T.);
#84964=ORIENTED_EDGE('',*,*,#57057,.T.);
#84965=ORIENTED_EDGE('',*,*,#57058,.T.);
#84966=ORIENTED_EDGE('',*,*,#57059,.T.);
#84967=ORIENTED_EDGE('',*,*,#57060,.T.);
#84968=ORIENTED_EDGE('',*,*,#57061,.T.);
#84969=ORIENTED_EDGE('',*,*,#57062,.F.);
#84970=ORIENTED_EDGE('',*,*,#57063,.T.);
#84971=ORIENTED_EDGE('',*,*,#57064,.T.);
#84972=ORIENTED_EDGE('',*,*,#57062,.T.);
#84973=ORIENTED_EDGE('',*,*,#57065,.T.);
#84974=ORIENTED_EDGE('',*,*,#57066,.T.);
#84975=ORIENTED_EDGE('',*,*,#57055,.F.);
#84976=ORIENTED_EDGE('',*,*,#57067,.T.);
#84977=ORIENTED_EDGE('',*,*,#57068,.T.);
#84978=ORIENTED_EDGE('',*,*,#57069,.F.);
#84979=ORIENTED_EDGE('',*,*,#57063,.F.);
#84980=ORIENTED_EDGE('',*,*,#57070,.F.);
#84981=ORIENTED_EDGE('',*,*,#57071,.F.);
#84982=ORIENTED_EDGE('',*,*,#57070,.T.);
#84983=ORIENTED_EDGE('',*,*,#57068,.F.);
#84984=ORIENTED_EDGE('',*,*,#57067,.F.);
#84985=ORIENTED_EDGE('',*,*,#57072,.F.);
#84986=ORIENTED_EDGE('',*,*,#57073,.F.);
#84987=ORIENTED_EDGE('',*,*,#57072,.T.);
#84988=ORIENTED_EDGE('',*,*,#57059,.F.);
#84989=ORIENTED_EDGE('',*,*,#57074,.F.);
#84990=ORIENTED_EDGE('',*,*,#57075,.F.);
#84991=ORIENTED_EDGE('',*,*,#57076,.T.);
#84992=ORIENTED_EDGE('',*,*,#57069,.T.);
#84993=ORIENTED_EDGE('',*,*,#53999,.F.);
#84994=ORIENTED_EDGE('',*,*,#54908,.T.);
#84995=ORIENTED_EDGE('',*,*,#57077,.F.);
#84996=ORIENTED_EDGE('',*,*,#57064,.F.);
#84997=ORIENTED_EDGE('',*,*,#57076,.F.);
#84998=ORIENTED_EDGE('',*,*,#54907,.F.);
#84999=ORIENTED_EDGE('',*,*,#57077,.T.);
#85000=ORIENTED_EDGE('',*,*,#55011,.F.);
#85001=ORIENTED_EDGE('',*,*,#57078,.F.);
#85002=ORIENTED_EDGE('',*,*,#57060,.F.);
#85003=ORIENTED_EDGE('',*,*,#57078,.T.);
#85004=ORIENTED_EDGE('',*,*,#54506,.F.);
#85005=ORIENTED_EDGE('',*,*,#57079,.F.);
#85006=ORIENTED_EDGE('',*,*,#57061,.F.);
#85007=ORIENTED_EDGE('',*,*,#57079,.T.);
#85008=ORIENTED_EDGE('',*,*,#54505,.F.);
#85009=ORIENTED_EDGE('',*,*,#57080,.F.);
#85010=ORIENTED_EDGE('',*,*,#57066,.F.);
#85011=ORIENTED_EDGE('',*,*,#57065,.F.);
#85012=ORIENTED_EDGE('',*,*,#57080,.T.);
#85013=ORIENTED_EDGE('',*,*,#54504,.F.);
#85014=ORIENTED_EDGE('',*,*,#57081,.F.);
#85015=ORIENTED_EDGE('',*,*,#57056,.F.);
#85016=ORIENTED_EDGE('',*,*,#57082,.T.);
#85017=ORIENTED_EDGE('',*,*,#57057,.F.);
#85018=ORIENTED_EDGE('',*,*,#57081,.T.);
#85019=ORIENTED_EDGE('',*,*,#55012,.F.);
#85020=ORIENTED_EDGE('',*,*,#57083,.T.);
#85021=ORIENTED_EDGE('',*,*,#57058,.F.);
#85022=ORIENTED_EDGE('',*,*,#57082,.F.);
#85023=ORIENTED_EDGE('',*,*,#54910,.F.);
#85024=ORIENTED_EDGE('',*,*,#53997,.T.);
#85025=ORIENTED_EDGE('',*,*,#57074,.T.);
#85026=ORIENTED_EDGE('',*,*,#57083,.F.);
#85027=ORIENTED_EDGE('',*,*,#54909,.T.);
#85028=ORIENTED_EDGE('',*,*,#57073,.T.);
#85029=ORIENTED_EDGE('',*,*,#57075,.T.);
#85030=ORIENTED_EDGE('',*,*,#53996,.T.);
#85031=ORIENTED_EDGE('',*,*,#57071,.T.);
#85032=ORIENTED_EDGE('',*,*,#57084,.T.);
#85033=ORIENTED_EDGE('',*,*,#57085,.T.);
#85034=ORIENTED_EDGE('',*,*,#57086,.T.);
#85035=ORIENTED_EDGE('',*,*,#57087,.T.);
#85036=ORIENTED_EDGE('',*,*,#57088,.T.);
#85037=ORIENTED_EDGE('',*,*,#57089,.T.);
#85038=ORIENTED_EDGE('',*,*,#57090,.T.);
#85039=ORIENTED_EDGE('',*,*,#57091,.F.);
#85040=ORIENTED_EDGE('',*,*,#57092,.T.);
#85041=ORIENTED_EDGE('',*,*,#57093,.T.);
#85042=ORIENTED_EDGE('',*,*,#57091,.T.);
#85043=ORIENTED_EDGE('',*,*,#57094,.T.);
#85044=ORIENTED_EDGE('',*,*,#57095,.T.);
#85045=ORIENTED_EDGE('',*,*,#57084,.F.);
#85046=ORIENTED_EDGE('',*,*,#57096,.T.);
#85047=ORIENTED_EDGE('',*,*,#57097,.T.);
#85048=ORIENTED_EDGE('',*,*,#57098,.F.);
#85049=ORIENTED_EDGE('',*,*,#57092,.F.);
#85050=ORIENTED_EDGE('',*,*,#57099,.F.);
#85051=ORIENTED_EDGE('',*,*,#57100,.F.);
#85052=ORIENTED_EDGE('',*,*,#57099,.T.);
#85053=ORIENTED_EDGE('',*,*,#57097,.F.);
#85054=ORIENTED_EDGE('',*,*,#57096,.F.);
#85055=ORIENTED_EDGE('',*,*,#57101,.F.);
#85056=ORIENTED_EDGE('',*,*,#57102,.F.);
#85057=ORIENTED_EDGE('',*,*,#57101,.T.);
#85058=ORIENTED_EDGE('',*,*,#57088,.F.);
#85059=ORIENTED_EDGE('',*,*,#57103,.F.);
#85060=ORIENTED_EDGE('',*,*,#57104,.F.);
#85061=ORIENTED_EDGE('',*,*,#57105,.T.);
#85062=ORIENTED_EDGE('',*,*,#57098,.T.);
#85063=ORIENTED_EDGE('',*,*,#53995,.F.);
#85064=ORIENTED_EDGE('',*,*,#54903,.T.);
#85065=ORIENTED_EDGE('',*,*,#57106,.F.);
#85066=ORIENTED_EDGE('',*,*,#57093,.F.);
#85067=ORIENTED_EDGE('',*,*,#57105,.F.);
#85068=ORIENTED_EDGE('',*,*,#54902,.F.);
#85069=ORIENTED_EDGE('',*,*,#57106,.T.);
#85070=ORIENTED_EDGE('',*,*,#55009,.F.);
#85071=ORIENTED_EDGE('',*,*,#57107,.F.);
#85072=ORIENTED_EDGE('',*,*,#57089,.F.);
#85073=ORIENTED_EDGE('',*,*,#57107,.T.);
#85074=ORIENTED_EDGE('',*,*,#54510,.F.);
#85075=ORIENTED_EDGE('',*,*,#57108,.F.);
#85076=ORIENTED_EDGE('',*,*,#57090,.F.);
#85077=ORIENTED_EDGE('',*,*,#57108,.T.);
#85078=ORIENTED_EDGE('',*,*,#54509,.F.);
#85079=ORIENTED_EDGE('',*,*,#57109,.F.);
#85080=ORIENTED_EDGE('',*,*,#57095,.F.);
#85081=ORIENTED_EDGE('',*,*,#57094,.F.);
#85082=ORIENTED_EDGE('',*,*,#57109,.T.);
#85083=ORIENTED_EDGE('',*,*,#54508,.F.);
#85084=ORIENTED_EDGE('',*,*,#57110,.F.);
#85085=ORIENTED_EDGE('',*,*,#57085,.F.);
#85086=ORIENTED_EDGE('',*,*,#57111,.T.);
#85087=ORIENTED_EDGE('',*,*,#57086,.F.);
#85088=ORIENTED_EDGE('',*,*,#57110,.T.);
#85089=ORIENTED_EDGE('',*,*,#55010,.F.);
#85090=ORIENTED_EDGE('',*,*,#57112,.T.);
#85091=ORIENTED_EDGE('',*,*,#57087,.F.);
#85092=ORIENTED_EDGE('',*,*,#57111,.F.);
#85093=ORIENTED_EDGE('',*,*,#54905,.F.);
#85094=ORIENTED_EDGE('',*,*,#53993,.T.);
#85095=ORIENTED_EDGE('',*,*,#57103,.T.);
#85096=ORIENTED_EDGE('',*,*,#57112,.F.);
#85097=ORIENTED_EDGE('',*,*,#54904,.T.);
#85098=ORIENTED_EDGE('',*,*,#57102,.T.);
#85099=ORIENTED_EDGE('',*,*,#57104,.T.);
#85100=ORIENTED_EDGE('',*,*,#53992,.T.);
#85101=ORIENTED_EDGE('',*,*,#57100,.T.);
#85102=ORIENTED_EDGE('',*,*,#57113,.T.);
#85103=ORIENTED_EDGE('',*,*,#57114,.T.);
#85104=ORIENTED_EDGE('',*,*,#57115,.T.);
#85105=ORIENTED_EDGE('',*,*,#57116,.T.);
#85106=ORIENTED_EDGE('',*,*,#57117,.T.);
#85107=ORIENTED_EDGE('',*,*,#57118,.T.);
#85108=ORIENTED_EDGE('',*,*,#57119,.T.);
#85109=ORIENTED_EDGE('',*,*,#57120,.F.);
#85110=ORIENTED_EDGE('',*,*,#57121,.T.);
#85111=ORIENTED_EDGE('',*,*,#57122,.T.);
#85112=ORIENTED_EDGE('',*,*,#57120,.T.);
#85113=ORIENTED_EDGE('',*,*,#57123,.T.);
#85114=ORIENTED_EDGE('',*,*,#57124,.T.);
#85115=ORIENTED_EDGE('',*,*,#57113,.F.);
#85116=ORIENTED_EDGE('',*,*,#57125,.T.);
#85117=ORIENTED_EDGE('',*,*,#57126,.T.);
#85118=ORIENTED_EDGE('',*,*,#57127,.F.);
#85119=ORIENTED_EDGE('',*,*,#57121,.F.);
#85120=ORIENTED_EDGE('',*,*,#57128,.F.);
#85121=ORIENTED_EDGE('',*,*,#57129,.F.);
#85122=ORIENTED_EDGE('',*,*,#57128,.T.);
#85123=ORIENTED_EDGE('',*,*,#57126,.F.);
#85124=ORIENTED_EDGE('',*,*,#57125,.F.);
#85125=ORIENTED_EDGE('',*,*,#57130,.F.);
#85126=ORIENTED_EDGE('',*,*,#57131,.F.);
#85127=ORIENTED_EDGE('',*,*,#57130,.T.);
#85128=ORIENTED_EDGE('',*,*,#57117,.F.);
#85129=ORIENTED_EDGE('',*,*,#57132,.F.);
#85130=ORIENTED_EDGE('',*,*,#57133,.F.);
#85131=ORIENTED_EDGE('',*,*,#57134,.T.);
#85132=ORIENTED_EDGE('',*,*,#57127,.T.);
#85133=ORIENTED_EDGE('',*,*,#53991,.F.);
#85134=ORIENTED_EDGE('',*,*,#54898,.T.);
#85135=ORIENTED_EDGE('',*,*,#57135,.F.);
#85136=ORIENTED_EDGE('',*,*,#57122,.F.);
#85137=ORIENTED_EDGE('',*,*,#57134,.F.);
#85138=ORIENTED_EDGE('',*,*,#54897,.F.);
#85139=ORIENTED_EDGE('',*,*,#57135,.T.);
#85140=ORIENTED_EDGE('',*,*,#55007,.F.);
#85141=ORIENTED_EDGE('',*,*,#57136,.F.);
#85142=ORIENTED_EDGE('',*,*,#57118,.F.);
#85143=ORIENTED_EDGE('',*,*,#57136,.T.);
#85144=ORIENTED_EDGE('',*,*,#54514,.F.);
#85145=ORIENTED_EDGE('',*,*,#57137,.F.);
#85146=ORIENTED_EDGE('',*,*,#57119,.F.);
#85147=ORIENTED_EDGE('',*,*,#57137,.T.);
#85148=ORIENTED_EDGE('',*,*,#54513,.F.);
#85149=ORIENTED_EDGE('',*,*,#57138,.F.);
#85150=ORIENTED_EDGE('',*,*,#57124,.F.);
#85151=ORIENTED_EDGE('',*,*,#57123,.F.);
#85152=ORIENTED_EDGE('',*,*,#57138,.T.);
#85153=ORIENTED_EDGE('',*,*,#54512,.F.);
#85154=ORIENTED_EDGE('',*,*,#57139,.F.);
#85155=ORIENTED_EDGE('',*,*,#57114,.F.);
#85156=ORIENTED_EDGE('',*,*,#57140,.T.);
#85157=ORIENTED_EDGE('',*,*,#57115,.F.);
#85158=ORIENTED_EDGE('',*,*,#57139,.T.);
#85159=ORIENTED_EDGE('',*,*,#55008,.F.);
#85160=ORIENTED_EDGE('',*,*,#57141,.T.);
#85161=ORIENTED_EDGE('',*,*,#57116,.F.);
#85162=ORIENTED_EDGE('',*,*,#57140,.F.);
#85163=ORIENTED_EDGE('',*,*,#54900,.F.);
#85164=ORIENTED_EDGE('',*,*,#53989,.T.);
#85165=ORIENTED_EDGE('',*,*,#57132,.T.);
#85166=ORIENTED_EDGE('',*,*,#57141,.F.);
#85167=ORIENTED_EDGE('',*,*,#54899,.T.);
#85168=ORIENTED_EDGE('',*,*,#57131,.T.);
#85169=ORIENTED_EDGE('',*,*,#57133,.T.);
#85170=ORIENTED_EDGE('',*,*,#53988,.T.);
#85171=ORIENTED_EDGE('',*,*,#57129,.T.);
#85172=ORIENTED_EDGE('',*,*,#57142,.T.);
#85173=ORIENTED_EDGE('',*,*,#57143,.T.);
#85174=ORIENTED_EDGE('',*,*,#57144,.T.);
#85175=ORIENTED_EDGE('',*,*,#57145,.T.);
#85176=ORIENTED_EDGE('',*,*,#57146,.T.);
#85177=ORIENTED_EDGE('',*,*,#57147,.T.);
#85178=ORIENTED_EDGE('',*,*,#57148,.T.);
#85179=ORIENTED_EDGE('',*,*,#57149,.F.);
#85180=ORIENTED_EDGE('',*,*,#57150,.T.);
#85181=ORIENTED_EDGE('',*,*,#57151,.T.);
#85182=ORIENTED_EDGE('',*,*,#57149,.T.);
#85183=ORIENTED_EDGE('',*,*,#57152,.T.);
#85184=ORIENTED_EDGE('',*,*,#57153,.T.);
#85185=ORIENTED_EDGE('',*,*,#57142,.F.);
#85186=ORIENTED_EDGE('',*,*,#57154,.T.);
#85187=ORIENTED_EDGE('',*,*,#57155,.T.);
#85188=ORIENTED_EDGE('',*,*,#57156,.F.);
#85189=ORIENTED_EDGE('',*,*,#57150,.F.);
#85190=ORIENTED_EDGE('',*,*,#57157,.F.);
#85191=ORIENTED_EDGE('',*,*,#57158,.F.);
#85192=ORIENTED_EDGE('',*,*,#57157,.T.);
#85193=ORIENTED_EDGE('',*,*,#57155,.F.);
#85194=ORIENTED_EDGE('',*,*,#57154,.F.);
#85195=ORIENTED_EDGE('',*,*,#57159,.F.);
#85196=ORIENTED_EDGE('',*,*,#57160,.F.);
#85197=ORIENTED_EDGE('',*,*,#57159,.T.);
#85198=ORIENTED_EDGE('',*,*,#57146,.F.);
#85199=ORIENTED_EDGE('',*,*,#57161,.F.);
#85200=ORIENTED_EDGE('',*,*,#57162,.F.);
#85201=ORIENTED_EDGE('',*,*,#57163,.T.);
#85202=ORIENTED_EDGE('',*,*,#57156,.T.);
#85203=ORIENTED_EDGE('',*,*,#53987,.F.);
#85204=ORIENTED_EDGE('',*,*,#54893,.T.);
#85205=ORIENTED_EDGE('',*,*,#57164,.F.);
#85206=ORIENTED_EDGE('',*,*,#57151,.F.);
#85207=ORIENTED_EDGE('',*,*,#57163,.F.);
#85208=ORIENTED_EDGE('',*,*,#54892,.F.);
#85209=ORIENTED_EDGE('',*,*,#57164,.T.);
#85210=ORIENTED_EDGE('',*,*,#55005,.F.);
#85211=ORIENTED_EDGE('',*,*,#57165,.F.);
#85212=ORIENTED_EDGE('',*,*,#57147,.F.);
#85213=ORIENTED_EDGE('',*,*,#57165,.T.);
#85214=ORIENTED_EDGE('',*,*,#54518,.F.);
#85215=ORIENTED_EDGE('',*,*,#57166,.F.);
#85216=ORIENTED_EDGE('',*,*,#57148,.F.);
#85217=ORIENTED_EDGE('',*,*,#57166,.T.);
#85218=ORIENTED_EDGE('',*,*,#54517,.F.);
#85219=ORIENTED_EDGE('',*,*,#57167,.F.);
#85220=ORIENTED_EDGE('',*,*,#57153,.F.);
#85221=ORIENTED_EDGE('',*,*,#57152,.F.);
#85222=ORIENTED_EDGE('',*,*,#57167,.T.);
#85223=ORIENTED_EDGE('',*,*,#54516,.F.);
#85224=ORIENTED_EDGE('',*,*,#57168,.F.);
#85225=ORIENTED_EDGE('',*,*,#57143,.F.);
#85226=ORIENTED_EDGE('',*,*,#57169,.T.);
#85227=ORIENTED_EDGE('',*,*,#57144,.F.);
#85228=ORIENTED_EDGE('',*,*,#57168,.T.);
#85229=ORIENTED_EDGE('',*,*,#55006,.F.);
#85230=ORIENTED_EDGE('',*,*,#57170,.T.);
#85231=ORIENTED_EDGE('',*,*,#57145,.F.);
#85232=ORIENTED_EDGE('',*,*,#57169,.F.);
#85233=ORIENTED_EDGE('',*,*,#54895,.F.);
#85234=ORIENTED_EDGE('',*,*,#53985,.T.);
#85235=ORIENTED_EDGE('',*,*,#57161,.T.);
#85236=ORIENTED_EDGE('',*,*,#57170,.F.);
#85237=ORIENTED_EDGE('',*,*,#54894,.T.);
#85238=ORIENTED_EDGE('',*,*,#57160,.T.);
#85239=ORIENTED_EDGE('',*,*,#57162,.T.);
#85240=ORIENTED_EDGE('',*,*,#53984,.T.);
#85241=ORIENTED_EDGE('',*,*,#57158,.T.);
#85242=ORIENTED_EDGE('',*,*,#57171,.T.);
#85243=ORIENTED_EDGE('',*,*,#57172,.T.);
#85244=ORIENTED_EDGE('',*,*,#57173,.T.);
#85245=ORIENTED_EDGE('',*,*,#57174,.T.);
#85246=ORIENTED_EDGE('',*,*,#57175,.T.);
#85247=ORIENTED_EDGE('',*,*,#57176,.T.);
#85248=ORIENTED_EDGE('',*,*,#57177,.T.);
#85249=ORIENTED_EDGE('',*,*,#57178,.F.);
#85250=ORIENTED_EDGE('',*,*,#57179,.T.);
#85251=ORIENTED_EDGE('',*,*,#57180,.T.);
#85252=ORIENTED_EDGE('',*,*,#57178,.T.);
#85253=ORIENTED_EDGE('',*,*,#57181,.T.);
#85254=ORIENTED_EDGE('',*,*,#57182,.T.);
#85255=ORIENTED_EDGE('',*,*,#57171,.F.);
#85256=ORIENTED_EDGE('',*,*,#57183,.T.);
#85257=ORIENTED_EDGE('',*,*,#57184,.T.);
#85258=ORIENTED_EDGE('',*,*,#57185,.F.);
#85259=ORIENTED_EDGE('',*,*,#57179,.F.);
#85260=ORIENTED_EDGE('',*,*,#57186,.F.);
#85261=ORIENTED_EDGE('',*,*,#57187,.F.);
#85262=ORIENTED_EDGE('',*,*,#57186,.T.);
#85263=ORIENTED_EDGE('',*,*,#57184,.F.);
#85264=ORIENTED_EDGE('',*,*,#57183,.F.);
#85265=ORIENTED_EDGE('',*,*,#57188,.F.);
#85266=ORIENTED_EDGE('',*,*,#57189,.F.);
#85267=ORIENTED_EDGE('',*,*,#57188,.T.);
#85268=ORIENTED_EDGE('',*,*,#57175,.F.);
#85269=ORIENTED_EDGE('',*,*,#57190,.F.);
#85270=ORIENTED_EDGE('',*,*,#57191,.F.);
#85271=ORIENTED_EDGE('',*,*,#57192,.T.);
#85272=ORIENTED_EDGE('',*,*,#57185,.T.);
#85273=ORIENTED_EDGE('',*,*,#53983,.F.);
#85274=ORIENTED_EDGE('',*,*,#54888,.T.);
#85275=ORIENTED_EDGE('',*,*,#57193,.F.);
#85276=ORIENTED_EDGE('',*,*,#57180,.F.);
#85277=ORIENTED_EDGE('',*,*,#57192,.F.);
#85278=ORIENTED_EDGE('',*,*,#54887,.F.);
#85279=ORIENTED_EDGE('',*,*,#57193,.T.);
#85280=ORIENTED_EDGE('',*,*,#55003,.F.);
#85281=ORIENTED_EDGE('',*,*,#57194,.F.);
#85282=ORIENTED_EDGE('',*,*,#57176,.F.);
#85283=ORIENTED_EDGE('',*,*,#57194,.T.);
#85284=ORIENTED_EDGE('',*,*,#54522,.F.);
#85285=ORIENTED_EDGE('',*,*,#57195,.F.);
#85286=ORIENTED_EDGE('',*,*,#57177,.F.);
#85287=ORIENTED_EDGE('',*,*,#57195,.T.);
#85288=ORIENTED_EDGE('',*,*,#54521,.F.);
#85289=ORIENTED_EDGE('',*,*,#57196,.F.);
#85290=ORIENTED_EDGE('',*,*,#57182,.F.);
#85291=ORIENTED_EDGE('',*,*,#57181,.F.);
#85292=ORIENTED_EDGE('',*,*,#57196,.T.);
#85293=ORIENTED_EDGE('',*,*,#54520,.F.);
#85294=ORIENTED_EDGE('',*,*,#57197,.F.);
#85295=ORIENTED_EDGE('',*,*,#57172,.F.);
#85296=ORIENTED_EDGE('',*,*,#57198,.T.);
#85297=ORIENTED_EDGE('',*,*,#57173,.F.);
#85298=ORIENTED_EDGE('',*,*,#57197,.T.);
#85299=ORIENTED_EDGE('',*,*,#55004,.F.);
#85300=ORIENTED_EDGE('',*,*,#57199,.T.);
#85301=ORIENTED_EDGE('',*,*,#57174,.F.);
#85302=ORIENTED_EDGE('',*,*,#57198,.F.);
#85303=ORIENTED_EDGE('',*,*,#54890,.F.);
#85304=ORIENTED_EDGE('',*,*,#53981,.T.);
#85305=ORIENTED_EDGE('',*,*,#57190,.T.);
#85306=ORIENTED_EDGE('',*,*,#57199,.F.);
#85307=ORIENTED_EDGE('',*,*,#54889,.T.);
#85308=ORIENTED_EDGE('',*,*,#57189,.T.);
#85309=ORIENTED_EDGE('',*,*,#57191,.T.);
#85310=ORIENTED_EDGE('',*,*,#53980,.T.);
#85311=ORIENTED_EDGE('',*,*,#57187,.T.);
#85312=ORIENTED_EDGE('',*,*,#57200,.T.);
#85313=ORIENTED_EDGE('',*,*,#57201,.T.);
#85314=ORIENTED_EDGE('',*,*,#57202,.T.);
#85315=ORIENTED_EDGE('',*,*,#57203,.T.);
#85316=ORIENTED_EDGE('',*,*,#57204,.T.);
#85317=ORIENTED_EDGE('',*,*,#57205,.T.);
#85318=ORIENTED_EDGE('',*,*,#57206,.T.);
#85319=ORIENTED_EDGE('',*,*,#57207,.F.);
#85320=ORIENTED_EDGE('',*,*,#57208,.T.);
#85321=ORIENTED_EDGE('',*,*,#57209,.T.);
#85322=ORIENTED_EDGE('',*,*,#57207,.T.);
#85323=ORIENTED_EDGE('',*,*,#57210,.T.);
#85324=ORIENTED_EDGE('',*,*,#57211,.T.);
#85325=ORIENTED_EDGE('',*,*,#57200,.F.);
#85326=ORIENTED_EDGE('',*,*,#57212,.T.);
#85327=ORIENTED_EDGE('',*,*,#57213,.T.);
#85328=ORIENTED_EDGE('',*,*,#57214,.F.);
#85329=ORIENTED_EDGE('',*,*,#57208,.F.);
#85330=ORIENTED_EDGE('',*,*,#57215,.F.);
#85331=ORIENTED_EDGE('',*,*,#57216,.F.);
#85332=ORIENTED_EDGE('',*,*,#57215,.T.);
#85333=ORIENTED_EDGE('',*,*,#57213,.F.);
#85334=ORIENTED_EDGE('',*,*,#57212,.F.);
#85335=ORIENTED_EDGE('',*,*,#57217,.F.);
#85336=ORIENTED_EDGE('',*,*,#57218,.F.);
#85337=ORIENTED_EDGE('',*,*,#57217,.T.);
#85338=ORIENTED_EDGE('',*,*,#57204,.F.);
#85339=ORIENTED_EDGE('',*,*,#57219,.F.);
#85340=ORIENTED_EDGE('',*,*,#57220,.F.);
#85341=ORIENTED_EDGE('',*,*,#57221,.T.);
#85342=ORIENTED_EDGE('',*,*,#57214,.T.);
#85343=ORIENTED_EDGE('',*,*,#53979,.F.);
#85344=ORIENTED_EDGE('',*,*,#54883,.T.);
#85345=ORIENTED_EDGE('',*,*,#57222,.F.);
#85346=ORIENTED_EDGE('',*,*,#57209,.F.);
#85347=ORIENTED_EDGE('',*,*,#57221,.F.);
#85348=ORIENTED_EDGE('',*,*,#54882,.F.);
#85349=ORIENTED_EDGE('',*,*,#57222,.T.);
#85350=ORIENTED_EDGE('',*,*,#55001,.F.);
#85351=ORIENTED_EDGE('',*,*,#57223,.F.);
#85352=ORIENTED_EDGE('',*,*,#57205,.F.);
#85353=ORIENTED_EDGE('',*,*,#57223,.T.);
#85354=ORIENTED_EDGE('',*,*,#54526,.F.);
#85355=ORIENTED_EDGE('',*,*,#57224,.F.);
#85356=ORIENTED_EDGE('',*,*,#57206,.F.);
#85357=ORIENTED_EDGE('',*,*,#57224,.T.);
#85358=ORIENTED_EDGE('',*,*,#54525,.F.);
#85359=ORIENTED_EDGE('',*,*,#57225,.F.);
#85360=ORIENTED_EDGE('',*,*,#57211,.F.);
#85361=ORIENTED_EDGE('',*,*,#57210,.F.);
#85362=ORIENTED_EDGE('',*,*,#57225,.T.);
#85363=ORIENTED_EDGE('',*,*,#54524,.F.);
#85364=ORIENTED_EDGE('',*,*,#57226,.F.);
#85365=ORIENTED_EDGE('',*,*,#57201,.F.);
#85366=ORIENTED_EDGE('',*,*,#57227,.T.);
#85367=ORIENTED_EDGE('',*,*,#57202,.F.);
#85368=ORIENTED_EDGE('',*,*,#57226,.T.);
#85369=ORIENTED_EDGE('',*,*,#55002,.F.);
#85370=ORIENTED_EDGE('',*,*,#57228,.T.);
#85371=ORIENTED_EDGE('',*,*,#57203,.F.);
#85372=ORIENTED_EDGE('',*,*,#57227,.F.);
#85373=ORIENTED_EDGE('',*,*,#54885,.F.);
#85374=ORIENTED_EDGE('',*,*,#53977,.T.);
#85375=ORIENTED_EDGE('',*,*,#57219,.T.);
#85376=ORIENTED_EDGE('',*,*,#57228,.F.);
#85377=ORIENTED_EDGE('',*,*,#54884,.T.);
#85378=ORIENTED_EDGE('',*,*,#57218,.T.);
#85379=ORIENTED_EDGE('',*,*,#57220,.T.);
#85380=ORIENTED_EDGE('',*,*,#53976,.T.);
#85381=ORIENTED_EDGE('',*,*,#57216,.T.);
#85382=ORIENTED_EDGE('',*,*,#57229,.T.);
#85383=ORIENTED_EDGE('',*,*,#57230,.T.);
#85384=ORIENTED_EDGE('',*,*,#57231,.T.);
#85385=ORIENTED_EDGE('',*,*,#57232,.T.);
#85386=ORIENTED_EDGE('',*,*,#57233,.T.);
#85387=ORIENTED_EDGE('',*,*,#57234,.T.);
#85388=ORIENTED_EDGE('',*,*,#57235,.T.);
#85389=ORIENTED_EDGE('',*,*,#57236,.F.);
#85390=ORIENTED_EDGE('',*,*,#57237,.T.);
#85391=ORIENTED_EDGE('',*,*,#57238,.T.);
#85392=ORIENTED_EDGE('',*,*,#57236,.T.);
#85393=ORIENTED_EDGE('',*,*,#57239,.T.);
#85394=ORIENTED_EDGE('',*,*,#57240,.T.);
#85395=ORIENTED_EDGE('',*,*,#57229,.F.);
#85396=ORIENTED_EDGE('',*,*,#57241,.T.);
#85397=ORIENTED_EDGE('',*,*,#57242,.T.);
#85398=ORIENTED_EDGE('',*,*,#57243,.F.);
#85399=ORIENTED_EDGE('',*,*,#57237,.F.);
#85400=ORIENTED_EDGE('',*,*,#57244,.F.);
#85401=ORIENTED_EDGE('',*,*,#57245,.F.);
#85402=ORIENTED_EDGE('',*,*,#57244,.T.);
#85403=ORIENTED_EDGE('',*,*,#57242,.F.);
#85404=ORIENTED_EDGE('',*,*,#57241,.F.);
#85405=ORIENTED_EDGE('',*,*,#57246,.F.);
#85406=ORIENTED_EDGE('',*,*,#57247,.F.);
#85407=ORIENTED_EDGE('',*,*,#57246,.T.);
#85408=ORIENTED_EDGE('',*,*,#57233,.F.);
#85409=ORIENTED_EDGE('',*,*,#57248,.F.);
#85410=ORIENTED_EDGE('',*,*,#57249,.F.);
#85411=ORIENTED_EDGE('',*,*,#57250,.T.);
#85412=ORIENTED_EDGE('',*,*,#57243,.T.);
#85413=ORIENTED_EDGE('',*,*,#53975,.F.);
#85414=ORIENTED_EDGE('',*,*,#54878,.T.);
#85415=ORIENTED_EDGE('',*,*,#57251,.F.);
#85416=ORIENTED_EDGE('',*,*,#57238,.F.);
#85417=ORIENTED_EDGE('',*,*,#57250,.F.);
#85418=ORIENTED_EDGE('',*,*,#54877,.F.);
#85419=ORIENTED_EDGE('',*,*,#57251,.T.);
#85420=ORIENTED_EDGE('',*,*,#54999,.F.);
#85421=ORIENTED_EDGE('',*,*,#57252,.F.);
#85422=ORIENTED_EDGE('',*,*,#57234,.F.);
#85423=ORIENTED_EDGE('',*,*,#57252,.T.);
#85424=ORIENTED_EDGE('',*,*,#54530,.F.);
#85425=ORIENTED_EDGE('',*,*,#57253,.F.);
#85426=ORIENTED_EDGE('',*,*,#57235,.F.);
#85427=ORIENTED_EDGE('',*,*,#57253,.T.);
#85428=ORIENTED_EDGE('',*,*,#54529,.F.);
#85429=ORIENTED_EDGE('',*,*,#57254,.F.);
#85430=ORIENTED_EDGE('',*,*,#57240,.F.);
#85431=ORIENTED_EDGE('',*,*,#57239,.F.);
#85432=ORIENTED_EDGE('',*,*,#57254,.T.);
#85433=ORIENTED_EDGE('',*,*,#54528,.F.);
#85434=ORIENTED_EDGE('',*,*,#57255,.F.);
#85435=ORIENTED_EDGE('',*,*,#57230,.F.);
#85436=ORIENTED_EDGE('',*,*,#57256,.T.);
#85437=ORIENTED_EDGE('',*,*,#57231,.F.);
#85438=ORIENTED_EDGE('',*,*,#57255,.T.);
#85439=ORIENTED_EDGE('',*,*,#55000,.F.);
#85440=ORIENTED_EDGE('',*,*,#57257,.T.);
#85441=ORIENTED_EDGE('',*,*,#57232,.F.);
#85442=ORIENTED_EDGE('',*,*,#57256,.F.);
#85443=ORIENTED_EDGE('',*,*,#54880,.F.);
#85444=ORIENTED_EDGE('',*,*,#53973,.T.);
#85445=ORIENTED_EDGE('',*,*,#57248,.T.);
#85446=ORIENTED_EDGE('',*,*,#57257,.F.);
#85447=ORIENTED_EDGE('',*,*,#54879,.T.);
#85448=ORIENTED_EDGE('',*,*,#57247,.T.);
#85449=ORIENTED_EDGE('',*,*,#57249,.T.);
#85450=ORIENTED_EDGE('',*,*,#53972,.T.);
#85451=ORIENTED_EDGE('',*,*,#57245,.T.);
#85452=ORIENTED_EDGE('',*,*,#57258,.T.);
#85453=ORIENTED_EDGE('',*,*,#57259,.T.);
#85454=ORIENTED_EDGE('',*,*,#57260,.T.);
#85455=ORIENTED_EDGE('',*,*,#57261,.T.);
#85456=ORIENTED_EDGE('',*,*,#57262,.T.);
#85457=ORIENTED_EDGE('',*,*,#57263,.T.);
#85458=ORIENTED_EDGE('',*,*,#57264,.T.);
#85459=ORIENTED_EDGE('',*,*,#57265,.F.);
#85460=ORIENTED_EDGE('',*,*,#57266,.T.);
#85461=ORIENTED_EDGE('',*,*,#57267,.T.);
#85462=ORIENTED_EDGE('',*,*,#57265,.T.);
#85463=ORIENTED_EDGE('',*,*,#57268,.T.);
#85464=ORIENTED_EDGE('',*,*,#57269,.T.);
#85465=ORIENTED_EDGE('',*,*,#57258,.F.);
#85466=ORIENTED_EDGE('',*,*,#57270,.T.);
#85467=ORIENTED_EDGE('',*,*,#57271,.T.);
#85468=ORIENTED_EDGE('',*,*,#57272,.F.);
#85469=ORIENTED_EDGE('',*,*,#57266,.F.);
#85470=ORIENTED_EDGE('',*,*,#57273,.F.);
#85471=ORIENTED_EDGE('',*,*,#57274,.F.);
#85472=ORIENTED_EDGE('',*,*,#57273,.T.);
#85473=ORIENTED_EDGE('',*,*,#57271,.F.);
#85474=ORIENTED_EDGE('',*,*,#57270,.F.);
#85475=ORIENTED_EDGE('',*,*,#57275,.F.);
#85476=ORIENTED_EDGE('',*,*,#57276,.F.);
#85477=ORIENTED_EDGE('',*,*,#57275,.T.);
#85478=ORIENTED_EDGE('',*,*,#57262,.F.);
#85479=ORIENTED_EDGE('',*,*,#57277,.F.);
#85480=ORIENTED_EDGE('',*,*,#57278,.F.);
#85481=ORIENTED_EDGE('',*,*,#57279,.T.);
#85482=ORIENTED_EDGE('',*,*,#57272,.T.);
#85483=ORIENTED_EDGE('',*,*,#53971,.F.);
#85484=ORIENTED_EDGE('',*,*,#54873,.T.);
#85485=ORIENTED_EDGE('',*,*,#57280,.F.);
#85486=ORIENTED_EDGE('',*,*,#57267,.F.);
#85487=ORIENTED_EDGE('',*,*,#57279,.F.);
#85488=ORIENTED_EDGE('',*,*,#54872,.F.);
#85489=ORIENTED_EDGE('',*,*,#57280,.T.);
#85490=ORIENTED_EDGE('',*,*,#54997,.F.);
#85491=ORIENTED_EDGE('',*,*,#57281,.F.);
#85492=ORIENTED_EDGE('',*,*,#57263,.F.);
#85493=ORIENTED_EDGE('',*,*,#57281,.T.);
#85494=ORIENTED_EDGE('',*,*,#54534,.F.);
#85495=ORIENTED_EDGE('',*,*,#57282,.F.);
#85496=ORIENTED_EDGE('',*,*,#57264,.F.);
#85497=ORIENTED_EDGE('',*,*,#57282,.T.);
#85498=ORIENTED_EDGE('',*,*,#54533,.F.);
#85499=ORIENTED_EDGE('',*,*,#57283,.F.);
#85500=ORIENTED_EDGE('',*,*,#57269,.F.);
#85501=ORIENTED_EDGE('',*,*,#57268,.F.);
#85502=ORIENTED_EDGE('',*,*,#57283,.T.);
#85503=ORIENTED_EDGE('',*,*,#54532,.F.);
#85504=ORIENTED_EDGE('',*,*,#57284,.F.);
#85505=ORIENTED_EDGE('',*,*,#57259,.F.);
#85506=ORIENTED_EDGE('',*,*,#57285,.T.);
#85507=ORIENTED_EDGE('',*,*,#57260,.F.);
#85508=ORIENTED_EDGE('',*,*,#57284,.T.);
#85509=ORIENTED_EDGE('',*,*,#54998,.F.);
#85510=ORIENTED_EDGE('',*,*,#57286,.T.);
#85511=ORIENTED_EDGE('',*,*,#57261,.F.);
#85512=ORIENTED_EDGE('',*,*,#57285,.F.);
#85513=ORIENTED_EDGE('',*,*,#54875,.F.);
#85514=ORIENTED_EDGE('',*,*,#53969,.T.);
#85515=ORIENTED_EDGE('',*,*,#57277,.T.);
#85516=ORIENTED_EDGE('',*,*,#57286,.F.);
#85517=ORIENTED_EDGE('',*,*,#54874,.T.);
#85518=ORIENTED_EDGE('',*,*,#57276,.T.);
#85519=ORIENTED_EDGE('',*,*,#57278,.T.);
#85520=ORIENTED_EDGE('',*,*,#53968,.T.);
#85521=ORIENTED_EDGE('',*,*,#57274,.T.);
#85522=ORIENTED_EDGE('',*,*,#57287,.T.);
#85523=ORIENTED_EDGE('',*,*,#57288,.T.);
#85524=ORIENTED_EDGE('',*,*,#57289,.T.);
#85525=ORIENTED_EDGE('',*,*,#57290,.T.);
#85526=ORIENTED_EDGE('',*,*,#57291,.T.);
#85527=ORIENTED_EDGE('',*,*,#57292,.T.);
#85528=ORIENTED_EDGE('',*,*,#57293,.T.);
#85529=ORIENTED_EDGE('',*,*,#57294,.F.);
#85530=ORIENTED_EDGE('',*,*,#57295,.T.);
#85531=ORIENTED_EDGE('',*,*,#57296,.T.);
#85532=ORIENTED_EDGE('',*,*,#57294,.T.);
#85533=ORIENTED_EDGE('',*,*,#57297,.T.);
#85534=ORIENTED_EDGE('',*,*,#57298,.T.);
#85535=ORIENTED_EDGE('',*,*,#57287,.F.);
#85536=ORIENTED_EDGE('',*,*,#57299,.T.);
#85537=ORIENTED_EDGE('',*,*,#57300,.T.);
#85538=ORIENTED_EDGE('',*,*,#57301,.F.);
#85539=ORIENTED_EDGE('',*,*,#57295,.F.);
#85540=ORIENTED_EDGE('',*,*,#57302,.F.);
#85541=ORIENTED_EDGE('',*,*,#57303,.F.);
#85542=ORIENTED_EDGE('',*,*,#57302,.T.);
#85543=ORIENTED_EDGE('',*,*,#57300,.F.);
#85544=ORIENTED_EDGE('',*,*,#57299,.F.);
#85545=ORIENTED_EDGE('',*,*,#57304,.F.);
#85546=ORIENTED_EDGE('',*,*,#57305,.F.);
#85547=ORIENTED_EDGE('',*,*,#57304,.T.);
#85548=ORIENTED_EDGE('',*,*,#57291,.F.);
#85549=ORIENTED_EDGE('',*,*,#57306,.F.);
#85550=ORIENTED_EDGE('',*,*,#57307,.F.);
#85551=ORIENTED_EDGE('',*,*,#57308,.T.);
#85552=ORIENTED_EDGE('',*,*,#57301,.T.);
#85553=ORIENTED_EDGE('',*,*,#53967,.F.);
#85554=ORIENTED_EDGE('',*,*,#54868,.T.);
#85555=ORIENTED_EDGE('',*,*,#57309,.F.);
#85556=ORIENTED_EDGE('',*,*,#57296,.F.);
#85557=ORIENTED_EDGE('',*,*,#57308,.F.);
#85558=ORIENTED_EDGE('',*,*,#54867,.F.);
#85559=ORIENTED_EDGE('',*,*,#57309,.T.);
#85560=ORIENTED_EDGE('',*,*,#54995,.F.);
#85561=ORIENTED_EDGE('',*,*,#57310,.F.);
#85562=ORIENTED_EDGE('',*,*,#57292,.F.);
#85563=ORIENTED_EDGE('',*,*,#57310,.T.);
#85564=ORIENTED_EDGE('',*,*,#54538,.F.);
#85565=ORIENTED_EDGE('',*,*,#57311,.F.);
#85566=ORIENTED_EDGE('',*,*,#57293,.F.);
#85567=ORIENTED_EDGE('',*,*,#57311,.T.);
#85568=ORIENTED_EDGE('',*,*,#54537,.F.);
#85569=ORIENTED_EDGE('',*,*,#57312,.F.);
#85570=ORIENTED_EDGE('',*,*,#57298,.F.);
#85571=ORIENTED_EDGE('',*,*,#57297,.F.);
#85572=ORIENTED_EDGE('',*,*,#57312,.T.);
#85573=ORIENTED_EDGE('',*,*,#54536,.F.);
#85574=ORIENTED_EDGE('',*,*,#57313,.F.);
#85575=ORIENTED_EDGE('',*,*,#57288,.F.);
#85576=ORIENTED_EDGE('',*,*,#57314,.T.);
#85577=ORIENTED_EDGE('',*,*,#57289,.F.);
#85578=ORIENTED_EDGE('',*,*,#57313,.T.);
#85579=ORIENTED_EDGE('',*,*,#54996,.F.);
#85580=ORIENTED_EDGE('',*,*,#57315,.T.);
#85581=ORIENTED_EDGE('',*,*,#57290,.F.);
#85582=ORIENTED_EDGE('',*,*,#57314,.F.);
#85583=ORIENTED_EDGE('',*,*,#54870,.F.);
#85584=ORIENTED_EDGE('',*,*,#53965,.T.);
#85585=ORIENTED_EDGE('',*,*,#57306,.T.);
#85586=ORIENTED_EDGE('',*,*,#57315,.F.);
#85587=ORIENTED_EDGE('',*,*,#54869,.T.);
#85588=ORIENTED_EDGE('',*,*,#57305,.T.);
#85589=ORIENTED_EDGE('',*,*,#57307,.T.);
#85590=ORIENTED_EDGE('',*,*,#53964,.T.);
#85591=ORIENTED_EDGE('',*,*,#57303,.T.);
#85592=ORIENTED_EDGE('',*,*,#57316,.T.);
#85593=ORIENTED_EDGE('',*,*,#57317,.T.);
#85594=ORIENTED_EDGE('',*,*,#57318,.T.);
#85595=ORIENTED_EDGE('',*,*,#57319,.T.);
#85596=ORIENTED_EDGE('',*,*,#57320,.T.);
#85597=ORIENTED_EDGE('',*,*,#57321,.T.);
#85598=ORIENTED_EDGE('',*,*,#57322,.T.);
#85599=ORIENTED_EDGE('',*,*,#57323,.F.);
#85600=ORIENTED_EDGE('',*,*,#57324,.T.);
#85601=ORIENTED_EDGE('',*,*,#57325,.T.);
#85602=ORIENTED_EDGE('',*,*,#57323,.T.);
#85603=ORIENTED_EDGE('',*,*,#57326,.T.);
#85604=ORIENTED_EDGE('',*,*,#57327,.T.);
#85605=ORIENTED_EDGE('',*,*,#57316,.F.);
#85606=ORIENTED_EDGE('',*,*,#57328,.T.);
#85607=ORIENTED_EDGE('',*,*,#57329,.T.);
#85608=ORIENTED_EDGE('',*,*,#57330,.F.);
#85609=ORIENTED_EDGE('',*,*,#57324,.F.);
#85610=ORIENTED_EDGE('',*,*,#57331,.F.);
#85611=ORIENTED_EDGE('',*,*,#57332,.F.);
#85612=ORIENTED_EDGE('',*,*,#57331,.T.);
#85613=ORIENTED_EDGE('',*,*,#57329,.F.);
#85614=ORIENTED_EDGE('',*,*,#57328,.F.);
#85615=ORIENTED_EDGE('',*,*,#57333,.F.);
#85616=ORIENTED_EDGE('',*,*,#57334,.F.);
#85617=ORIENTED_EDGE('',*,*,#57333,.T.);
#85618=ORIENTED_EDGE('',*,*,#57320,.F.);
#85619=ORIENTED_EDGE('',*,*,#57335,.F.);
#85620=ORIENTED_EDGE('',*,*,#57336,.F.);
#85621=ORIENTED_EDGE('',*,*,#57337,.T.);
#85622=ORIENTED_EDGE('',*,*,#57330,.T.);
#85623=ORIENTED_EDGE('',*,*,#53963,.F.);
#85624=ORIENTED_EDGE('',*,*,#54863,.T.);
#85625=ORIENTED_EDGE('',*,*,#57338,.F.);
#85626=ORIENTED_EDGE('',*,*,#57325,.F.);
#85627=ORIENTED_EDGE('',*,*,#57337,.F.);
#85628=ORIENTED_EDGE('',*,*,#54862,.F.);
#85629=ORIENTED_EDGE('',*,*,#57338,.T.);
#85630=ORIENTED_EDGE('',*,*,#54993,.F.);
#85631=ORIENTED_EDGE('',*,*,#57339,.F.);
#85632=ORIENTED_EDGE('',*,*,#57321,.F.);
#85633=ORIENTED_EDGE('',*,*,#57339,.T.);
#85634=ORIENTED_EDGE('',*,*,#54542,.F.);
#85635=ORIENTED_EDGE('',*,*,#57340,.F.);
#85636=ORIENTED_EDGE('',*,*,#57322,.F.);
#85637=ORIENTED_EDGE('',*,*,#57340,.T.);
#85638=ORIENTED_EDGE('',*,*,#54541,.F.);
#85639=ORIENTED_EDGE('',*,*,#57341,.F.);
#85640=ORIENTED_EDGE('',*,*,#57327,.F.);
#85641=ORIENTED_EDGE('',*,*,#57326,.F.);
#85642=ORIENTED_EDGE('',*,*,#57341,.T.);
#85643=ORIENTED_EDGE('',*,*,#54540,.F.);
#85644=ORIENTED_EDGE('',*,*,#57342,.F.);
#85645=ORIENTED_EDGE('',*,*,#57317,.F.);
#85646=ORIENTED_EDGE('',*,*,#57343,.T.);
#85647=ORIENTED_EDGE('',*,*,#57318,.F.);
#85648=ORIENTED_EDGE('',*,*,#57342,.T.);
#85649=ORIENTED_EDGE('',*,*,#54994,.F.);
#85650=ORIENTED_EDGE('',*,*,#57344,.T.);
#85651=ORIENTED_EDGE('',*,*,#57319,.F.);
#85652=ORIENTED_EDGE('',*,*,#57343,.F.);
#85653=ORIENTED_EDGE('',*,*,#54865,.F.);
#85654=ORIENTED_EDGE('',*,*,#53961,.T.);
#85655=ORIENTED_EDGE('',*,*,#57335,.T.);
#85656=ORIENTED_EDGE('',*,*,#57344,.F.);
#85657=ORIENTED_EDGE('',*,*,#54864,.T.);
#85658=ORIENTED_EDGE('',*,*,#57334,.T.);
#85659=ORIENTED_EDGE('',*,*,#57336,.T.);
#85660=ORIENTED_EDGE('',*,*,#53960,.T.);
#85661=ORIENTED_EDGE('',*,*,#57332,.T.);
#85662=ORIENTED_EDGE('',*,*,#57345,.T.);
#85663=ORIENTED_EDGE('',*,*,#57346,.T.);
#85664=ORIENTED_EDGE('',*,*,#57347,.T.);
#85665=ORIENTED_EDGE('',*,*,#57348,.T.);
#85666=ORIENTED_EDGE('',*,*,#57349,.T.);
#85667=ORIENTED_EDGE('',*,*,#57350,.T.);
#85668=ORIENTED_EDGE('',*,*,#57351,.T.);
#85669=ORIENTED_EDGE('',*,*,#57352,.F.);
#85670=ORIENTED_EDGE('',*,*,#57353,.T.);
#85671=ORIENTED_EDGE('',*,*,#57354,.T.);
#85672=ORIENTED_EDGE('',*,*,#57352,.T.);
#85673=ORIENTED_EDGE('',*,*,#57355,.T.);
#85674=ORIENTED_EDGE('',*,*,#57356,.T.);
#85675=ORIENTED_EDGE('',*,*,#57345,.F.);
#85676=ORIENTED_EDGE('',*,*,#57357,.T.);
#85677=ORIENTED_EDGE('',*,*,#57358,.T.);
#85678=ORIENTED_EDGE('',*,*,#57359,.F.);
#85679=ORIENTED_EDGE('',*,*,#57353,.F.);
#85680=ORIENTED_EDGE('',*,*,#57360,.F.);
#85681=ORIENTED_EDGE('',*,*,#57361,.F.);
#85682=ORIENTED_EDGE('',*,*,#57360,.T.);
#85683=ORIENTED_EDGE('',*,*,#57358,.F.);
#85684=ORIENTED_EDGE('',*,*,#57357,.F.);
#85685=ORIENTED_EDGE('',*,*,#57362,.F.);
#85686=ORIENTED_EDGE('',*,*,#57363,.F.);
#85687=ORIENTED_EDGE('',*,*,#57362,.T.);
#85688=ORIENTED_EDGE('',*,*,#57349,.F.);
#85689=ORIENTED_EDGE('',*,*,#57364,.F.);
#85690=ORIENTED_EDGE('',*,*,#57365,.F.);
#85691=ORIENTED_EDGE('',*,*,#57366,.T.);
#85692=ORIENTED_EDGE('',*,*,#57359,.T.);
#85693=ORIENTED_EDGE('',*,*,#53959,.F.);
#85694=ORIENTED_EDGE('',*,*,#54858,.T.);
#85695=ORIENTED_EDGE('',*,*,#57367,.F.);
#85696=ORIENTED_EDGE('',*,*,#57354,.F.);
#85697=ORIENTED_EDGE('',*,*,#57366,.F.);
#85698=ORIENTED_EDGE('',*,*,#54857,.F.);
#85699=ORIENTED_EDGE('',*,*,#57367,.T.);
#85700=ORIENTED_EDGE('',*,*,#54991,.F.);
#85701=ORIENTED_EDGE('',*,*,#57368,.F.);
#85702=ORIENTED_EDGE('',*,*,#57350,.F.);
#85703=ORIENTED_EDGE('',*,*,#57368,.T.);
#85704=ORIENTED_EDGE('',*,*,#54546,.F.);
#85705=ORIENTED_EDGE('',*,*,#57369,.F.);
#85706=ORIENTED_EDGE('',*,*,#57351,.F.);
#85707=ORIENTED_EDGE('',*,*,#57369,.T.);
#85708=ORIENTED_EDGE('',*,*,#54545,.F.);
#85709=ORIENTED_EDGE('',*,*,#57370,.F.);
#85710=ORIENTED_EDGE('',*,*,#57356,.F.);
#85711=ORIENTED_EDGE('',*,*,#57355,.F.);
#85712=ORIENTED_EDGE('',*,*,#57370,.T.);
#85713=ORIENTED_EDGE('',*,*,#54544,.F.);
#85714=ORIENTED_EDGE('',*,*,#57371,.F.);
#85715=ORIENTED_EDGE('',*,*,#57346,.F.);
#85716=ORIENTED_EDGE('',*,*,#57372,.T.);
#85717=ORIENTED_EDGE('',*,*,#57347,.F.);
#85718=ORIENTED_EDGE('',*,*,#57371,.T.);
#85719=ORIENTED_EDGE('',*,*,#54992,.F.);
#85720=ORIENTED_EDGE('',*,*,#57373,.T.);
#85721=ORIENTED_EDGE('',*,*,#57348,.F.);
#85722=ORIENTED_EDGE('',*,*,#57372,.F.);
#85723=ORIENTED_EDGE('',*,*,#54860,.F.);
#85724=ORIENTED_EDGE('',*,*,#53957,.T.);
#85725=ORIENTED_EDGE('',*,*,#57364,.T.);
#85726=ORIENTED_EDGE('',*,*,#57373,.F.);
#85727=ORIENTED_EDGE('',*,*,#54859,.T.);
#85728=ORIENTED_EDGE('',*,*,#57363,.T.);
#85729=ORIENTED_EDGE('',*,*,#57365,.T.);
#85730=ORIENTED_EDGE('',*,*,#53956,.T.);
#85731=ORIENTED_EDGE('',*,*,#57361,.T.);
#85732=ORIENTED_EDGE('',*,*,#57374,.T.);
#85733=ORIENTED_EDGE('',*,*,#57375,.T.);
#85734=ORIENTED_EDGE('',*,*,#57376,.T.);
#85735=ORIENTED_EDGE('',*,*,#57377,.T.);
#85736=ORIENTED_EDGE('',*,*,#57378,.T.);
#85737=ORIENTED_EDGE('',*,*,#57379,.T.);
#85738=ORIENTED_EDGE('',*,*,#57380,.T.);
#85739=ORIENTED_EDGE('',*,*,#57381,.F.);
#85740=ORIENTED_EDGE('',*,*,#57382,.T.);
#85741=ORIENTED_EDGE('',*,*,#57383,.T.);
#85742=ORIENTED_EDGE('',*,*,#57381,.T.);
#85743=ORIENTED_EDGE('',*,*,#57384,.T.);
#85744=ORIENTED_EDGE('',*,*,#57385,.T.);
#85745=ORIENTED_EDGE('',*,*,#57374,.F.);
#85746=ORIENTED_EDGE('',*,*,#57386,.T.);
#85747=ORIENTED_EDGE('',*,*,#57387,.T.);
#85748=ORIENTED_EDGE('',*,*,#57388,.F.);
#85749=ORIENTED_EDGE('',*,*,#57382,.F.);
#85750=ORIENTED_EDGE('',*,*,#57389,.F.);
#85751=ORIENTED_EDGE('',*,*,#57390,.F.);
#85752=ORIENTED_EDGE('',*,*,#57389,.T.);
#85753=ORIENTED_EDGE('',*,*,#57387,.F.);
#85754=ORIENTED_EDGE('',*,*,#57386,.F.);
#85755=ORIENTED_EDGE('',*,*,#57391,.F.);
#85756=ORIENTED_EDGE('',*,*,#57392,.F.);
#85757=ORIENTED_EDGE('',*,*,#57391,.T.);
#85758=ORIENTED_EDGE('',*,*,#57378,.F.);
#85759=ORIENTED_EDGE('',*,*,#57393,.F.);
#85760=ORIENTED_EDGE('',*,*,#57394,.F.);
#85761=ORIENTED_EDGE('',*,*,#57395,.T.);
#85762=ORIENTED_EDGE('',*,*,#57388,.T.);
#85763=ORIENTED_EDGE('',*,*,#53955,.F.);
#85764=ORIENTED_EDGE('',*,*,#54853,.T.);
#85765=ORIENTED_EDGE('',*,*,#57396,.F.);
#85766=ORIENTED_EDGE('',*,*,#57383,.F.);
#85767=ORIENTED_EDGE('',*,*,#57395,.F.);
#85768=ORIENTED_EDGE('',*,*,#54852,.F.);
#85769=ORIENTED_EDGE('',*,*,#57396,.T.);
#85770=ORIENTED_EDGE('',*,*,#54988,.F.);
#85771=ORIENTED_EDGE('',*,*,#57397,.F.);
#85772=ORIENTED_EDGE('',*,*,#57379,.F.);
#85773=ORIENTED_EDGE('',*,*,#57397,.T.);
#85774=ORIENTED_EDGE('',*,*,#54550,.F.);
#85775=ORIENTED_EDGE('',*,*,#57398,.F.);
#85776=ORIENTED_EDGE('',*,*,#57380,.F.);
#85777=ORIENTED_EDGE('',*,*,#57398,.T.);
#85778=ORIENTED_EDGE('',*,*,#54549,.F.);
#85779=ORIENTED_EDGE('',*,*,#57399,.F.);
#85780=ORIENTED_EDGE('',*,*,#57385,.F.);
#85781=ORIENTED_EDGE('',*,*,#57384,.F.);
#85782=ORIENTED_EDGE('',*,*,#57399,.T.);
#85783=ORIENTED_EDGE('',*,*,#54548,.F.);
#85784=ORIENTED_EDGE('',*,*,#57400,.F.);
#85785=ORIENTED_EDGE('',*,*,#57375,.F.);
#85786=ORIENTED_EDGE('',*,*,#57401,.T.);
#85787=ORIENTED_EDGE('',*,*,#57376,.F.);
#85788=ORIENTED_EDGE('',*,*,#57400,.T.);
#85789=ORIENTED_EDGE('',*,*,#54990,.F.);
#85790=ORIENTED_EDGE('',*,*,#57402,.T.);
#85791=ORIENTED_EDGE('',*,*,#57377,.F.);
#85792=ORIENTED_EDGE('',*,*,#57401,.F.);
#85793=ORIENTED_EDGE('',*,*,#54855,.F.);
#85794=ORIENTED_EDGE('',*,*,#53953,.T.);
#85795=ORIENTED_EDGE('',*,*,#57393,.T.);
#85796=ORIENTED_EDGE('',*,*,#57402,.F.);
#85797=ORIENTED_EDGE('',*,*,#54854,.T.);
#85798=ORIENTED_EDGE('',*,*,#57392,.T.);
#85799=ORIENTED_EDGE('',*,*,#57394,.T.);
#85800=ORIENTED_EDGE('',*,*,#53952,.T.);
#85801=ORIENTED_EDGE('',*,*,#57390,.T.);
#85802=ORIENTED_EDGE('',*,*,#57403,.T.);
#85803=ORIENTED_EDGE('',*,*,#57404,.F.);
#85804=ORIENTED_EDGE('',*,*,#57405,.T.);
#85805=ORIENTED_EDGE('',*,*,#57406,.T.);
#85806=ORIENTED_EDGE('',*,*,#57407,.T.);
#85807=ORIENTED_EDGE('',*,*,#57408,.F.);
#85808=ORIENTED_EDGE('',*,*,#57403,.F.);
#85809=ORIENTED_EDGE('',*,*,#57409,.T.);
#85810=ORIENTED_EDGE('',*,*,#57410,.T.);
#85811=ORIENTED_EDGE('',*,*,#57411,.T.);
#85812=ORIENTED_EDGE('',*,*,#57406,.F.);
#85813=ORIENTED_EDGE('',*,*,#57412,.T.);
#85814=ORIENTED_EDGE('',*,*,#57413,.T.);
#85815=ORIENTED_EDGE('',*,*,#57414,.T.);
#85816=ORIENTED_EDGE('',*,*,#57410,.F.);
#85817=ORIENTED_EDGE('',*,*,#57415,.T.);
#85818=ORIENTED_EDGE('',*,*,#57416,.T.);
#85819=ORIENTED_EDGE('',*,*,#57417,.T.);
#85820=ORIENTED_EDGE('',*,*,#57413,.F.);
#85821=ORIENTED_EDGE('',*,*,#57418,.T.);
#85822=ORIENTED_EDGE('',*,*,#57419,.T.);
#85823=ORIENTED_EDGE('',*,*,#57420,.T.);
#85824=ORIENTED_EDGE('',*,*,#57416,.F.);
#85825=ORIENTED_EDGE('',*,*,#57421,.T.);
#85826=ORIENTED_EDGE('',*,*,#57422,.T.);
#85827=ORIENTED_EDGE('',*,*,#57423,.T.);
#85828=ORIENTED_EDGE('',*,*,#57419,.F.);
#85829=ORIENTED_EDGE('',*,*,#57424,.T.);
#85830=ORIENTED_EDGE('',*,*,#57425,.F.);
#85831=ORIENTED_EDGE('',*,*,#57426,.T.);
#85832=ORIENTED_EDGE('',*,*,#57427,.F.);
#85833=ORIENTED_EDGE('',*,*,#57428,.T.);
#85834=ORIENTED_EDGE('',*,*,#57429,.T.);
#85835=ORIENTED_EDGE('',*,*,#57430,.T.);
#85836=ORIENTED_EDGE('',*,*,#57431,.F.);
#85837=ORIENTED_EDGE('',*,*,#57432,.F.);
#85838=ORIENTED_EDGE('',*,*,#57433,.T.);
#85839=ORIENTED_EDGE('',*,*,#57434,.T.);
#85840=ORIENTED_EDGE('',*,*,#57429,.F.);
#85841=ORIENTED_EDGE('',*,*,#57435,.F.);
#85842=ORIENTED_EDGE('',*,*,#57436,.T.);
#85843=ORIENTED_EDGE('',*,*,#57437,.T.);
#85844=ORIENTED_EDGE('',*,*,#57433,.F.);
#85845=ORIENTED_EDGE('',*,*,#57438,.F.);
#85846=ORIENTED_EDGE('',*,*,#57439,.T.);
#85847=ORIENTED_EDGE('',*,*,#57440,.T.);
#85848=ORIENTED_EDGE('',*,*,#57436,.F.);
#85849=ORIENTED_EDGE('',*,*,#57441,.F.);
#85850=ORIENTED_EDGE('',*,*,#57442,.T.);
#85851=ORIENTED_EDGE('',*,*,#57443,.T.);
#85852=ORIENTED_EDGE('',*,*,#57439,.F.);
#85853=ORIENTED_EDGE('',*,*,#57444,.F.);
#85854=ORIENTED_EDGE('',*,*,#57445,.T.);
#85855=ORIENTED_EDGE('',*,*,#57446,.T.);
#85856=ORIENTED_EDGE('',*,*,#57442,.F.);
#85857=ORIENTED_EDGE('',*,*,#57447,.F.);
#85858=ORIENTED_EDGE('',*,*,#57448,.T.);
#85859=ORIENTED_EDGE('',*,*,#57449,.T.);
#85860=ORIENTED_EDGE('',*,*,#57445,.F.);
#85861=ORIENTED_EDGE('',*,*,#57450,.F.);
#85862=ORIENTED_EDGE('',*,*,#57451,.F.);
#85863=ORIENTED_EDGE('',*,*,#57452,.F.);
#85864=ORIENTED_EDGE('',*,*,#57453,.F.);
#85865=ORIENTED_EDGE('',*,*,#57454,.T.);
#85866=ORIENTED_EDGE('',*,*,#57455,.T.);
#85867=ORIENTED_EDGE('',*,*,#57456,.F.);
#85868=ORIENTED_EDGE('',*,*,#57457,.T.);
#85869=ORIENTED_EDGE('',*,*,#57458,.T.);
#85870=ORIENTED_EDGE('',*,*,#57459,.T.);
#85871=ORIENTED_EDGE('',*,*,#57460,.F.);
#85872=ORIENTED_EDGE('',*,*,#57455,.F.);
#85873=ORIENTED_EDGE('',*,*,#57461,.T.);
#85874=ORIENTED_EDGE('',*,*,#57462,.T.);
#85875=ORIENTED_EDGE('',*,*,#57463,.T.);
#85876=ORIENTED_EDGE('',*,*,#57458,.F.);
#85877=ORIENTED_EDGE('',*,*,#57464,.T.);
#85878=ORIENTED_EDGE('',*,*,#57465,.T.);
#85879=ORIENTED_EDGE('',*,*,#57466,.T.);
#85880=ORIENTED_EDGE('',*,*,#57462,.F.);
#85881=ORIENTED_EDGE('',*,*,#57467,.T.);
#85882=ORIENTED_EDGE('',*,*,#57468,.T.);
#85883=ORIENTED_EDGE('',*,*,#57469,.T.);
#85884=ORIENTED_EDGE('',*,*,#57465,.F.);
#85885=ORIENTED_EDGE('',*,*,#57470,.T.);
#85886=ORIENTED_EDGE('',*,*,#57471,.T.);
#85887=ORIENTED_EDGE('',*,*,#57472,.T.);
#85888=ORIENTED_EDGE('',*,*,#57468,.F.);
#85889=ORIENTED_EDGE('',*,*,#57473,.T.);
#85890=ORIENTED_EDGE('',*,*,#57474,.T.);
#85891=ORIENTED_EDGE('',*,*,#57475,.T.);
#85892=ORIENTED_EDGE('',*,*,#57471,.F.);
#85893=ORIENTED_EDGE('',*,*,#57476,.T.);
#85894=ORIENTED_EDGE('',*,*,#57477,.F.);
#85895=ORIENTED_EDGE('',*,*,#57478,.T.);
#85896=ORIENTED_EDGE('',*,*,#57479,.F.);
#85897=ORIENTED_EDGE('',*,*,#57480,.T.);
#85898=ORIENTED_EDGE('',*,*,#57481,.T.);
#85899=ORIENTED_EDGE('',*,*,#57482,.T.);
#85900=ORIENTED_EDGE('',*,*,#57483,.F.);
#85901=ORIENTED_EDGE('',*,*,#57484,.F.);
#85902=ORIENTED_EDGE('',*,*,#57485,.T.);
#85903=ORIENTED_EDGE('',*,*,#57486,.T.);
#85904=ORIENTED_EDGE('',*,*,#57481,.F.);
#85905=ORIENTED_EDGE('',*,*,#57487,.F.);
#85906=ORIENTED_EDGE('',*,*,#57488,.T.);
#85907=ORIENTED_EDGE('',*,*,#57489,.T.);
#85908=ORIENTED_EDGE('',*,*,#57485,.F.);
#85909=ORIENTED_EDGE('',*,*,#57490,.F.);
#85910=ORIENTED_EDGE('',*,*,#57491,.T.);
#85911=ORIENTED_EDGE('',*,*,#57492,.T.);
#85912=ORIENTED_EDGE('',*,*,#57488,.F.);
#85913=ORIENTED_EDGE('',*,*,#57493,.F.);
#85914=ORIENTED_EDGE('',*,*,#57494,.T.);
#85915=ORIENTED_EDGE('',*,*,#57495,.T.);
#85916=ORIENTED_EDGE('',*,*,#57491,.F.);
#85917=ORIENTED_EDGE('',*,*,#57496,.F.);
#85918=ORIENTED_EDGE('',*,*,#57497,.T.);
#85919=ORIENTED_EDGE('',*,*,#57498,.T.);
#85920=ORIENTED_EDGE('',*,*,#57494,.F.);
#85921=ORIENTED_EDGE('',*,*,#57499,.F.);
#85922=ORIENTED_EDGE('',*,*,#57500,.T.);
#85923=ORIENTED_EDGE('',*,*,#57501,.T.);
#85924=ORIENTED_EDGE('',*,*,#57497,.F.);
#85925=ORIENTED_EDGE('',*,*,#57502,.F.);
#85926=ORIENTED_EDGE('',*,*,#57503,.F.);
#85927=ORIENTED_EDGE('',*,*,#57504,.F.);
#85928=ORIENTED_EDGE('',*,*,#57505,.F.);
#85929=ORIENTED_EDGE('',*,*,#57506,.T.);
#85930=ORIENTED_EDGE('',*,*,#57507,.T.);
#85931=ORIENTED_EDGE('',*,*,#57508,.F.);
#85932=ORIENTED_EDGE('',*,*,#57509,.T.);
#85933=ORIENTED_EDGE('',*,*,#57510,.T.);
#85934=ORIENTED_EDGE('',*,*,#57511,.T.);
#85935=ORIENTED_EDGE('',*,*,#57512,.F.);
#85936=ORIENTED_EDGE('',*,*,#57507,.F.);
#85937=ORIENTED_EDGE('',*,*,#57513,.T.);
#85938=ORIENTED_EDGE('',*,*,#57514,.T.);
#85939=ORIENTED_EDGE('',*,*,#57515,.T.);
#85940=ORIENTED_EDGE('',*,*,#57510,.F.);
#85941=ORIENTED_EDGE('',*,*,#57516,.T.);
#85942=ORIENTED_EDGE('',*,*,#57517,.T.);
#85943=ORIENTED_EDGE('',*,*,#57518,.T.);
#85944=ORIENTED_EDGE('',*,*,#57514,.F.);
#85945=ORIENTED_EDGE('',*,*,#57519,.T.);
#85946=ORIENTED_EDGE('',*,*,#57520,.T.);
#85947=ORIENTED_EDGE('',*,*,#57521,.T.);
#85948=ORIENTED_EDGE('',*,*,#57517,.F.);
#85949=ORIENTED_EDGE('',*,*,#57522,.T.);
#85950=ORIENTED_EDGE('',*,*,#57523,.T.);
#85951=ORIENTED_EDGE('',*,*,#57524,.T.);
#85952=ORIENTED_EDGE('',*,*,#57520,.F.);
#85953=ORIENTED_EDGE('',*,*,#57525,.T.);
#85954=ORIENTED_EDGE('',*,*,#57526,.T.);
#85955=ORIENTED_EDGE('',*,*,#57527,.T.);
#85956=ORIENTED_EDGE('',*,*,#57523,.F.);
#85957=ORIENTED_EDGE('',*,*,#57528,.T.);
#85958=ORIENTED_EDGE('',*,*,#57529,.F.);
#85959=ORIENTED_EDGE('',*,*,#57530,.T.);
#85960=ORIENTED_EDGE('',*,*,#57531,.F.);
#85961=ORIENTED_EDGE('',*,*,#57532,.T.);
#85962=ORIENTED_EDGE('',*,*,#57533,.T.);
#85963=ORIENTED_EDGE('',*,*,#57534,.T.);
#85964=ORIENTED_EDGE('',*,*,#57535,.F.);
#85965=ORIENTED_EDGE('',*,*,#57536,.F.);
#85966=ORIENTED_EDGE('',*,*,#57537,.T.);
#85967=ORIENTED_EDGE('',*,*,#57538,.T.);
#85968=ORIENTED_EDGE('',*,*,#57533,.F.);
#85969=ORIENTED_EDGE('',*,*,#57539,.F.);
#85970=ORIENTED_EDGE('',*,*,#57540,.T.);
#85971=ORIENTED_EDGE('',*,*,#57541,.T.);
#85972=ORIENTED_EDGE('',*,*,#57537,.F.);
#85973=ORIENTED_EDGE('',*,*,#57542,.F.);
#85974=ORIENTED_EDGE('',*,*,#57543,.T.);
#85975=ORIENTED_EDGE('',*,*,#57544,.T.);
#85976=ORIENTED_EDGE('',*,*,#57540,.F.);
#85977=ORIENTED_EDGE('',*,*,#57545,.F.);
#85978=ORIENTED_EDGE('',*,*,#57546,.T.);
#85979=ORIENTED_EDGE('',*,*,#57547,.T.);
#85980=ORIENTED_EDGE('',*,*,#57543,.F.);
#85981=ORIENTED_EDGE('',*,*,#57548,.F.);
#85982=ORIENTED_EDGE('',*,*,#57549,.T.);
#85983=ORIENTED_EDGE('',*,*,#57550,.T.);
#85984=ORIENTED_EDGE('',*,*,#57546,.F.);
#85985=ORIENTED_EDGE('',*,*,#57551,.F.);
#85986=ORIENTED_EDGE('',*,*,#57552,.T.);
#85987=ORIENTED_EDGE('',*,*,#57553,.T.);
#85988=ORIENTED_EDGE('',*,*,#57549,.F.);
#85989=ORIENTED_EDGE('',*,*,#57554,.F.);
#85990=ORIENTED_EDGE('',*,*,#57555,.F.);
#85991=ORIENTED_EDGE('',*,*,#57556,.F.);
#85992=ORIENTED_EDGE('',*,*,#57557,.F.);
#85993=ORIENTED_EDGE('',*,*,#57558,.T.);
#85994=ORIENTED_EDGE('',*,*,#57559,.T.);
#85995=ORIENTED_EDGE('',*,*,#57560,.F.);
#85996=ORIENTED_EDGE('',*,*,#57561,.T.);
#85997=ORIENTED_EDGE('',*,*,#57562,.T.);
#85998=ORIENTED_EDGE('',*,*,#57563,.T.);
#85999=ORIENTED_EDGE('',*,*,#57564,.F.);
#86000=ORIENTED_EDGE('',*,*,#57559,.F.);
#86001=ORIENTED_EDGE('',*,*,#57565,.T.);
#86002=ORIENTED_EDGE('',*,*,#57566,.T.);
#86003=ORIENTED_EDGE('',*,*,#57567,.T.);
#86004=ORIENTED_EDGE('',*,*,#57562,.F.);
#86005=ORIENTED_EDGE('',*,*,#57568,.T.);
#86006=ORIENTED_EDGE('',*,*,#57569,.T.);
#86007=ORIENTED_EDGE('',*,*,#57570,.T.);
#86008=ORIENTED_EDGE('',*,*,#57566,.F.);
#86009=ORIENTED_EDGE('',*,*,#57571,.T.);
#86010=ORIENTED_EDGE('',*,*,#57572,.T.);
#86011=ORIENTED_EDGE('',*,*,#57573,.T.);
#86012=ORIENTED_EDGE('',*,*,#57569,.F.);
#86013=ORIENTED_EDGE('',*,*,#57574,.T.);
#86014=ORIENTED_EDGE('',*,*,#57575,.T.);
#86015=ORIENTED_EDGE('',*,*,#57576,.T.);
#86016=ORIENTED_EDGE('',*,*,#57572,.F.);
#86017=ORIENTED_EDGE('',*,*,#57577,.T.);
#86018=ORIENTED_EDGE('',*,*,#57578,.T.);
#86019=ORIENTED_EDGE('',*,*,#57579,.T.);
#86020=ORIENTED_EDGE('',*,*,#57575,.F.);
#86021=ORIENTED_EDGE('',*,*,#57580,.T.);
#86022=ORIENTED_EDGE('',*,*,#57581,.F.);
#86023=ORIENTED_EDGE('',*,*,#57582,.T.);
#86024=ORIENTED_EDGE('',*,*,#57583,.F.);
#86025=ORIENTED_EDGE('',*,*,#57584,.T.);
#86026=ORIENTED_EDGE('',*,*,#57585,.T.);
#86027=ORIENTED_EDGE('',*,*,#57586,.T.);
#86028=ORIENTED_EDGE('',*,*,#57587,.F.);
#86029=ORIENTED_EDGE('',*,*,#57588,.F.);
#86030=ORIENTED_EDGE('',*,*,#57589,.T.);
#86031=ORIENTED_EDGE('',*,*,#57590,.T.);
#86032=ORIENTED_EDGE('',*,*,#57585,.F.);
#86033=ORIENTED_EDGE('',*,*,#57591,.F.);
#86034=ORIENTED_EDGE('',*,*,#57592,.T.);
#86035=ORIENTED_EDGE('',*,*,#57593,.T.);
#86036=ORIENTED_EDGE('',*,*,#57589,.F.);
#86037=ORIENTED_EDGE('',*,*,#57594,.F.);
#86038=ORIENTED_EDGE('',*,*,#57595,.T.);
#86039=ORIENTED_EDGE('',*,*,#57596,.T.);
#86040=ORIENTED_EDGE('',*,*,#57592,.F.);
#86041=ORIENTED_EDGE('',*,*,#57597,.F.);
#86042=ORIENTED_EDGE('',*,*,#57598,.T.);
#86043=ORIENTED_EDGE('',*,*,#57599,.T.);
#86044=ORIENTED_EDGE('',*,*,#57595,.F.);
#86045=ORIENTED_EDGE('',*,*,#57600,.F.);
#86046=ORIENTED_EDGE('',*,*,#57601,.T.);
#86047=ORIENTED_EDGE('',*,*,#57602,.T.);
#86048=ORIENTED_EDGE('',*,*,#57598,.F.);
#86049=ORIENTED_EDGE('',*,*,#57603,.F.);
#86050=ORIENTED_EDGE('',*,*,#57604,.T.);
#86051=ORIENTED_EDGE('',*,*,#57605,.T.);
#86052=ORIENTED_EDGE('',*,*,#57601,.F.);
#86053=ORIENTED_EDGE('',*,*,#57606,.F.);
#86054=ORIENTED_EDGE('',*,*,#57607,.F.);
#86055=ORIENTED_EDGE('',*,*,#57608,.F.);
#86056=ORIENTED_EDGE('',*,*,#57609,.F.);
#86057=ORIENTED_EDGE('',*,*,#57610,.T.);
#86058=ORIENTED_EDGE('',*,*,#57611,.T.);
#86059=ORIENTED_EDGE('',*,*,#57612,.T.);
#86060=ORIENTED_EDGE('',*,*,#57613,.T.);
#86061=ORIENTED_EDGE('',*,*,#57612,.F.);
#86062=ORIENTED_EDGE('',*,*,#57614,.T.);
#86063=ORIENTED_EDGE('',*,*,#57615,.T.);
#86064=ORIENTED_EDGE('',*,*,#57616,.T.);
#86065=ORIENTED_EDGE('',*,*,#57613,.F.);
#86066=ORIENTED_EDGE('',*,*,#57616,.F.);
#86067=ORIENTED_EDGE('',*,*,#57617,.F.);
#86068=ORIENTED_EDGE('',*,*,#57618,.T.);
#86069=ORIENTED_EDGE('',*,*,#57583,.T.);
#86070=ORIENTED_EDGE('',*,*,#57619,.T.);
#86071=ORIENTED_EDGE('',*,*,#57609,.T.);
#86072=ORIENTED_EDGE('',*,*,#57557,.T.);
#86073=ORIENTED_EDGE('',*,*,#57620,.T.);
#86074=ORIENTED_EDGE('',*,*,#57531,.T.);
#86075=ORIENTED_EDGE('',*,*,#57621,.T.);
#86076=ORIENTED_EDGE('',*,*,#57505,.T.);
#86077=ORIENTED_EDGE('',*,*,#57622,.T.);
#86078=ORIENTED_EDGE('',*,*,#57479,.T.);
#86079=ORIENTED_EDGE('',*,*,#57623,.T.);
#86080=ORIENTED_EDGE('',*,*,#57453,.T.);
#86081=ORIENTED_EDGE('',*,*,#57624,.T.);
#86082=ORIENTED_EDGE('',*,*,#57427,.T.);
#86083=ORIENTED_EDGE('',*,*,#57625,.T.);
#86084=ORIENTED_EDGE('',*,*,#57611,.F.);
#86085=ORIENTED_EDGE('',*,*,#57607,.T.);
#86086=ORIENTED_EDGE('',*,*,#57626,.T.);
#86087=ORIENTED_EDGE('',*,*,#57604,.F.);
#86088=ORIENTED_EDGE('',*,*,#57627,.F.);
#86089=ORIENTED_EDGE('',*,*,#57628,.F.);
#86090=ORIENTED_EDGE('',*,*,#57586,.F.);
#86091=ORIENTED_EDGE('',*,*,#57590,.F.);
#86092=ORIENTED_EDGE('',*,*,#57593,.F.);
#86093=ORIENTED_EDGE('',*,*,#57596,.F.);
#86094=ORIENTED_EDGE('',*,*,#57599,.F.);
#86095=ORIENTED_EDGE('',*,*,#57602,.F.);
#86096=ORIENTED_EDGE('',*,*,#57605,.F.);
#86097=ORIENTED_EDGE('',*,*,#57626,.F.);
#86098=ORIENTED_EDGE('',*,*,#57610,.F.);
#86099=ORIENTED_EDGE('',*,*,#57619,.F.);
#86100=ORIENTED_EDGE('',*,*,#57582,.F.);
#86101=ORIENTED_EDGE('',*,*,#57629,.F.);
#86102=ORIENTED_EDGE('',*,*,#57580,.F.);
#86103=ORIENTED_EDGE('',*,*,#57577,.F.);
#86104=ORIENTED_EDGE('',*,*,#57574,.F.);
#86105=ORIENTED_EDGE('',*,*,#57571,.F.);
#86106=ORIENTED_EDGE('',*,*,#57568,.F.);
#86107=ORIENTED_EDGE('',*,*,#57565,.F.);
#86108=ORIENTED_EDGE('',*,*,#57561,.F.);
#86109=ORIENTED_EDGE('',*,*,#57630,.F.);
#86110=ORIENTED_EDGE('',*,*,#57563,.F.);
#86111=ORIENTED_EDGE('',*,*,#57567,.F.);
#86112=ORIENTED_EDGE('',*,*,#57570,.F.);
#86113=ORIENTED_EDGE('',*,*,#57573,.F.);
#86114=ORIENTED_EDGE('',*,*,#57576,.F.);
#86115=ORIENTED_EDGE('',*,*,#57579,.F.);
#86116=ORIENTED_EDGE('',*,*,#57631,.F.);
#86117=ORIENTED_EDGE('',*,*,#57584,.F.);
#86118=ORIENTED_EDGE('',*,*,#57618,.F.);
#86119=ORIENTED_EDGE('',*,*,#57608,.T.);
#86120=ORIENTED_EDGE('',*,*,#57627,.T.);
#86121=ORIENTED_EDGE('',*,*,#57606,.T.);
#86122=ORIENTED_EDGE('',*,*,#57603,.T.);
#86123=ORIENTED_EDGE('',*,*,#57600,.T.);
#86124=ORIENTED_EDGE('',*,*,#57597,.T.);
#86125=ORIENTED_EDGE('',*,*,#57594,.T.);
#86126=ORIENTED_EDGE('',*,*,#57591,.T.);
#86127=ORIENTED_EDGE('',*,*,#57588,.T.);
#86128=ORIENTED_EDGE('',*,*,#57632,.T.);
#86129=ORIENTED_EDGE('',*,*,#57431,.T.);
#86130=ORIENTED_EDGE('',*,*,#57633,.T.);
#86131=ORIENTED_EDGE('',*,*,#57404,.T.);
#86132=ORIENTED_EDGE('',*,*,#57408,.T.);
#86133=ORIENTED_EDGE('',*,*,#57634,.T.);
#86134=ORIENTED_EDGE('',*,*,#57483,.T.);
#86135=ORIENTED_EDGE('',*,*,#57635,.T.);
#86136=ORIENTED_EDGE('',*,*,#57456,.T.);
#86137=ORIENTED_EDGE('',*,*,#57460,.T.);
#86138=ORIENTED_EDGE('',*,*,#57636,.T.);
#86139=ORIENTED_EDGE('',*,*,#57535,.T.);
#86140=ORIENTED_EDGE('',*,*,#57637,.T.);
#86141=ORIENTED_EDGE('',*,*,#57508,.T.);
#86142=ORIENTED_EDGE('',*,*,#57512,.T.);
#86143=ORIENTED_EDGE('',*,*,#57638,.T.);
#86144=ORIENTED_EDGE('',*,*,#57639,.F.);
#86145=ORIENTED_EDGE('',*,*,#57630,.T.);
#86146=ORIENTED_EDGE('',*,*,#57587,.T.);
#86147=ORIENTED_EDGE('',*,*,#57628,.T.);
#86148=ORIENTED_EDGE('',*,*,#57560,.T.);
#86149=ORIENTED_EDGE('',*,*,#57564,.T.);
#86150=ORIENTED_EDGE('',*,*,#57581,.T.);
#86151=ORIENTED_EDGE('',*,*,#57631,.T.);
#86152=ORIENTED_EDGE('',*,*,#57578,.F.);
#86153=ORIENTED_EDGE('',*,*,#57629,.T.);
#86154=ORIENTED_EDGE('',*,*,#57640,.F.);
#86155=ORIENTED_EDGE('',*,*,#57641,.T.);
#86156=ORIENTED_EDGE('',*,*,#57642,.F.);
#86157=ORIENTED_EDGE('',*,*,#57641,.F.);
#86158=ORIENTED_EDGE('',*,*,#57614,.F.);
#86159=ORIENTED_EDGE('',*,*,#57615,.F.);
#86160=ORIENTED_EDGE('',*,*,#57643,.T.);
#86161=ORIENTED_EDGE('',*,*,#57644,.F.);
#86162=ORIENTED_EDGE('',*,*,#57643,.F.);
#86163=ORIENTED_EDGE('',*,*,#57644,.T.);
#86164=ORIENTED_EDGE('',*,*,#57645,.T.);
#86165=ORIENTED_EDGE('',*,*,#57646,.T.);
#86166=ORIENTED_EDGE('',*,*,#57645,.F.);
#86167=ORIENTED_EDGE('',*,*,#57647,.F.);
#86168=ORIENTED_EDGE('',*,*,#57648,.T.);
#86169=ORIENTED_EDGE('',*,*,#57617,.T.);
#86170=ORIENTED_EDGE('',*,*,#57648,.F.);
#86171=ORIENTED_EDGE('',*,*,#57632,.F.);
#86172=ORIENTED_EDGE('',*,*,#57649,.T.);
#86173=ORIENTED_EDGE('',*,*,#57650,.T.);
#86174=ORIENTED_EDGE('',*,*,#57649,.F.);
#86175=ORIENTED_EDGE('',*,*,#57651,.F.);
#86176=ORIENTED_EDGE('',*,*,#57652,.T.);
#86177=ORIENTED_EDGE('',*,*,#57639,.T.);
#86178=ORIENTED_EDGE('',*,*,#57652,.F.);
#86179=ORIENTED_EDGE('',*,*,#57653,.F.);
#86180=ORIENTED_EDGE('',*,*,#57654,.T.);
#86181=ORIENTED_EDGE('',*,*,#57655,.T.);
#86182=ORIENTED_EDGE('',*,*,#57654,.F.);
#86183=ORIENTED_EDGE('',*,*,#57656,.F.);
#86184=ORIENTED_EDGE('',*,*,#57657,.T.);
#86185=ORIENTED_EDGE('',*,*,#57658,.T.);
#86186=ORIENTED_EDGE('',*,*,#57657,.F.);
#86187=ORIENTED_EDGE('',*,*,#57659,.F.);
#86188=ORIENTED_EDGE('',*,*,#57660,.T.);
#86189=ORIENTED_EDGE('',*,*,#57661,.T.);
#86190=ORIENTED_EDGE('',*,*,#57660,.F.);
#86191=ORIENTED_EDGE('',*,*,#57662,.F.);
#86192=ORIENTED_EDGE('',*,*,#57663,.T.);
#86193=ORIENTED_EDGE('',*,*,#57664,.T.);
#86194=ORIENTED_EDGE('',*,*,#57663,.F.);
#86195=ORIENTED_EDGE('',*,*,#57665,.F.);
#86196=ORIENTED_EDGE('',*,*,#57666,.T.);
#86197=ORIENTED_EDGE('',*,*,#57667,.T.);
#86198=ORIENTED_EDGE('',*,*,#57666,.F.);
#86199=ORIENTED_EDGE('',*,*,#57668,.F.);
#86200=ORIENTED_EDGE('',*,*,#57669,.T.);
#86201=ORIENTED_EDGE('',*,*,#57670,.T.);
#86202=ORIENTED_EDGE('',*,*,#57669,.F.);
#86203=ORIENTED_EDGE('',*,*,#57671,.F.);
#86204=ORIENTED_EDGE('',*,*,#57672,.T.);
#86205=ORIENTED_EDGE('',*,*,#57673,.T.);
#86206=ORIENTED_EDGE('',*,*,#57672,.F.);
#86207=ORIENTED_EDGE('',*,*,#57674,.F.);
#86208=ORIENTED_EDGE('',*,*,#57675,.T.);
#86209=ORIENTED_EDGE('',*,*,#57676,.T.);
#86210=ORIENTED_EDGE('',*,*,#57675,.F.);
#86211=ORIENTED_EDGE('',*,*,#57677,.F.);
#86212=ORIENTED_EDGE('',*,*,#57678,.T.);
#86213=ORIENTED_EDGE('',*,*,#57679,.T.);
#86214=ORIENTED_EDGE('',*,*,#57678,.F.);
#86215=ORIENTED_EDGE('',*,*,#57680,.F.);
#86216=ORIENTED_EDGE('',*,*,#57681,.T.);
#86217=ORIENTED_EDGE('',*,*,#57682,.T.);
#86218=ORIENTED_EDGE('',*,*,#57681,.F.);
#86219=ORIENTED_EDGE('',*,*,#57683,.F.);
#86220=ORIENTED_EDGE('',*,*,#57684,.T.);
#86221=ORIENTED_EDGE('',*,*,#57685,.T.);
#86222=ORIENTED_EDGE('',*,*,#57684,.F.);
#86223=ORIENTED_EDGE('',*,*,#57686,.F.);
#86224=ORIENTED_EDGE('',*,*,#57687,.T.);
#86225=ORIENTED_EDGE('',*,*,#57688,.T.);
#86226=ORIENTED_EDGE('',*,*,#57687,.F.);
#86227=ORIENTED_EDGE('',*,*,#57689,.F.);
#86228=ORIENTED_EDGE('',*,*,#57690,.T.);
#86229=ORIENTED_EDGE('',*,*,#57691,.T.);
#86230=ORIENTED_EDGE('',*,*,#57690,.F.);
#86231=ORIENTED_EDGE('',*,*,#57692,.F.);
#86232=ORIENTED_EDGE('',*,*,#57693,.T.);
#86233=ORIENTED_EDGE('',*,*,#57694,.T.);
#86234=ORIENTED_EDGE('',*,*,#57693,.F.);
#86235=ORIENTED_EDGE('',*,*,#57695,.F.);
#86236=ORIENTED_EDGE('',*,*,#57696,.T.);
#86237=ORIENTED_EDGE('',*,*,#57697,.T.);
#86238=ORIENTED_EDGE('',*,*,#57696,.F.);
#86239=ORIENTED_EDGE('',*,*,#57698,.F.);
#86240=ORIENTED_EDGE('',*,*,#57699,.T.);
#86241=ORIENTED_EDGE('',*,*,#57700,.T.);
#86242=ORIENTED_EDGE('',*,*,#57699,.F.);
#86243=ORIENTED_EDGE('',*,*,#57701,.F.);
#86244=ORIENTED_EDGE('',*,*,#57702,.T.);
#86245=ORIENTED_EDGE('',*,*,#57703,.T.);
#86246=ORIENTED_EDGE('',*,*,#57702,.F.);
#86247=ORIENTED_EDGE('',*,*,#57701,.T.);
#86248=ORIENTED_EDGE('',*,*,#57646,.F.);
#86249=ORIENTED_EDGE('',*,*,#57703,.F.);
#86250=ORIENTED_EDGE('',*,*,#57698,.T.);
#86251=ORIENTED_EDGE('',*,*,#57695,.T.);
#86252=ORIENTED_EDGE('',*,*,#57700,.F.);
#86253=ORIENTED_EDGE('',*,*,#57697,.F.);
#86254=ORIENTED_EDGE('',*,*,#57692,.T.);
#86255=ORIENTED_EDGE('',*,*,#57689,.T.);
#86256=ORIENTED_EDGE('',*,*,#57694,.F.);
#86257=ORIENTED_EDGE('',*,*,#57691,.F.);
#86258=ORIENTED_EDGE('',*,*,#57686,.T.);
#86259=ORIENTED_EDGE('',*,*,#57683,.T.);
#86260=ORIENTED_EDGE('',*,*,#57688,.F.);
#86261=ORIENTED_EDGE('',*,*,#57685,.F.);
#86262=ORIENTED_EDGE('',*,*,#57680,.T.);
#86263=ORIENTED_EDGE('',*,*,#57677,.T.);
#86264=ORIENTED_EDGE('',*,*,#57682,.F.);
#86265=ORIENTED_EDGE('',*,*,#57679,.F.);
#86266=ORIENTED_EDGE('',*,*,#57674,.T.);
#86267=ORIENTED_EDGE('',*,*,#57671,.T.);
#86268=ORIENTED_EDGE('',*,*,#57676,.F.);
#86269=ORIENTED_EDGE('',*,*,#57673,.F.);
#86270=ORIENTED_EDGE('',*,*,#57668,.T.);
#86271=ORIENTED_EDGE('',*,*,#57665,.T.);
#86272=ORIENTED_EDGE('',*,*,#57670,.F.);
#86273=ORIENTED_EDGE('',*,*,#57667,.F.);
#86274=ORIENTED_EDGE('',*,*,#57662,.T.);
#86275=ORIENTED_EDGE('',*,*,#57659,.T.);
#86276=ORIENTED_EDGE('',*,*,#57664,.F.);
#86277=ORIENTED_EDGE('',*,*,#57661,.F.);
#86278=ORIENTED_EDGE('',*,*,#57656,.T.);
#86279=ORIENTED_EDGE('',*,*,#57653,.T.);
#86280=ORIENTED_EDGE('',*,*,#57658,.F.);
#86281=ORIENTED_EDGE('',*,*,#57655,.F.);
#86282=ORIENTED_EDGE('',*,*,#57651,.T.);
#86283=ORIENTED_EDGE('',*,*,#57650,.F.);
#86284=ORIENTED_EDGE('',*,*,#57640,.T.);
#86285=ORIENTED_EDGE('',*,*,#57647,.T.);
#86286=ORIENTED_EDGE('',*,*,#57642,.T.);
#86287=ORIENTED_EDGE('',*,*,#57555,.T.);
#86288=ORIENTED_EDGE('',*,*,#57704,.T.);
#86289=ORIENTED_EDGE('',*,*,#57552,.F.);
#86290=ORIENTED_EDGE('',*,*,#57705,.F.);
#86291=ORIENTED_EDGE('',*,*,#57637,.F.);
#86292=ORIENTED_EDGE('',*,*,#57534,.F.);
#86293=ORIENTED_EDGE('',*,*,#57538,.F.);
#86294=ORIENTED_EDGE('',*,*,#57541,.F.);
#86295=ORIENTED_EDGE('',*,*,#57544,.F.);
#86296=ORIENTED_EDGE('',*,*,#57547,.F.);
#86297=ORIENTED_EDGE('',*,*,#57550,.F.);
#86298=ORIENTED_EDGE('',*,*,#57553,.F.);
#86299=ORIENTED_EDGE('',*,*,#57704,.F.);
#86300=ORIENTED_EDGE('',*,*,#57558,.F.);
#86301=ORIENTED_EDGE('',*,*,#57621,.F.);
#86302=ORIENTED_EDGE('',*,*,#57530,.F.);
#86303=ORIENTED_EDGE('',*,*,#57706,.F.);
#86304=ORIENTED_EDGE('',*,*,#57528,.F.);
#86305=ORIENTED_EDGE('',*,*,#57525,.F.);
#86306=ORIENTED_EDGE('',*,*,#57522,.F.);
#86307=ORIENTED_EDGE('',*,*,#57519,.F.);
#86308=ORIENTED_EDGE('',*,*,#57516,.F.);
#86309=ORIENTED_EDGE('',*,*,#57513,.F.);
#86310=ORIENTED_EDGE('',*,*,#57509,.F.);
#86311=ORIENTED_EDGE('',*,*,#57638,.F.);
#86312=ORIENTED_EDGE('',*,*,#57511,.F.);
#86313=ORIENTED_EDGE('',*,*,#57515,.F.);
#86314=ORIENTED_EDGE('',*,*,#57518,.F.);
#86315=ORIENTED_EDGE('',*,*,#57521,.F.);
#86316=ORIENTED_EDGE('',*,*,#57524,.F.);
#86317=ORIENTED_EDGE('',*,*,#57527,.F.);
#86318=ORIENTED_EDGE('',*,*,#57707,.F.);
#86319=ORIENTED_EDGE('',*,*,#57532,.F.);
#86320=ORIENTED_EDGE('',*,*,#57620,.F.);
#86321=ORIENTED_EDGE('',*,*,#57556,.T.);
#86322=ORIENTED_EDGE('',*,*,#57705,.T.);
#86323=ORIENTED_EDGE('',*,*,#57554,.T.);
#86324=ORIENTED_EDGE('',*,*,#57551,.T.);
#86325=ORIENTED_EDGE('',*,*,#57548,.T.);
#86326=ORIENTED_EDGE('',*,*,#57545,.T.);
#86327=ORIENTED_EDGE('',*,*,#57542,.T.);
#86328=ORIENTED_EDGE('',*,*,#57539,.T.);
#86329=ORIENTED_EDGE('',*,*,#57536,.T.);
#86330=ORIENTED_EDGE('',*,*,#57529,.T.);
#86331=ORIENTED_EDGE('',*,*,#57707,.T.);
#86332=ORIENTED_EDGE('',*,*,#57526,.F.);
#86333=ORIENTED_EDGE('',*,*,#57706,.T.);
#86334=ORIENTED_EDGE('',*,*,#57503,.T.);
#86335=ORIENTED_EDGE('',*,*,#57708,.T.);
#86336=ORIENTED_EDGE('',*,*,#57500,.F.);
#86337=ORIENTED_EDGE('',*,*,#57709,.F.);
#86338=ORIENTED_EDGE('',*,*,#57635,.F.);
#86339=ORIENTED_EDGE('',*,*,#57482,.F.);
#86340=ORIENTED_EDGE('',*,*,#57486,.F.);
#86341=ORIENTED_EDGE('',*,*,#57489,.F.);
#86342=ORIENTED_EDGE('',*,*,#57492,.F.);
#86343=ORIENTED_EDGE('',*,*,#57495,.F.);
#86344=ORIENTED_EDGE('',*,*,#57498,.F.);
#86345=ORIENTED_EDGE('',*,*,#57501,.F.);
#86346=ORIENTED_EDGE('',*,*,#57708,.F.);
#86347=ORIENTED_EDGE('',*,*,#57506,.F.);
#86348=ORIENTED_EDGE('',*,*,#57623,.F.);
#86349=ORIENTED_EDGE('',*,*,#57478,.F.);
#86350=ORIENTED_EDGE('',*,*,#57710,.F.);
#86351=ORIENTED_EDGE('',*,*,#57476,.F.);
#86352=ORIENTED_EDGE('',*,*,#57473,.F.);
#86353=ORIENTED_EDGE('',*,*,#57470,.F.);
#86354=ORIENTED_EDGE('',*,*,#57467,.F.);
#86355=ORIENTED_EDGE('',*,*,#57464,.F.);
#86356=ORIENTED_EDGE('',*,*,#57461,.F.);
#86357=ORIENTED_EDGE('',*,*,#57457,.F.);
#86358=ORIENTED_EDGE('',*,*,#57636,.F.);
#86359=ORIENTED_EDGE('',*,*,#57459,.F.);
#86360=ORIENTED_EDGE('',*,*,#57463,.F.);
#86361=ORIENTED_EDGE('',*,*,#57466,.F.);
#86362=ORIENTED_EDGE('',*,*,#57469,.F.);
#86363=ORIENTED_EDGE('',*,*,#57472,.F.);
#86364=ORIENTED_EDGE('',*,*,#57475,.F.);
#86365=ORIENTED_EDGE('',*,*,#57711,.F.);
#86366=ORIENTED_EDGE('',*,*,#57480,.F.);
#86367=ORIENTED_EDGE('',*,*,#57622,.F.);
#86368=ORIENTED_EDGE('',*,*,#57504,.T.);
#86369=ORIENTED_EDGE('',*,*,#57709,.T.);
#86370=ORIENTED_EDGE('',*,*,#57502,.T.);
#86371=ORIENTED_EDGE('',*,*,#57499,.T.);
#86372=ORIENTED_EDGE('',*,*,#57496,.T.);
#86373=ORIENTED_EDGE('',*,*,#57493,.T.);
#86374=ORIENTED_EDGE('',*,*,#57490,.T.);
#86375=ORIENTED_EDGE('',*,*,#57487,.T.);
#86376=ORIENTED_EDGE('',*,*,#57484,.T.);
#86377=ORIENTED_EDGE('',*,*,#57477,.T.);
#86378=ORIENTED_EDGE('',*,*,#57711,.T.);
#86379=ORIENTED_EDGE('',*,*,#57474,.F.);
#86380=ORIENTED_EDGE('',*,*,#57710,.T.);
#86381=ORIENTED_EDGE('',*,*,#57451,.T.);
#86382=ORIENTED_EDGE('',*,*,#57712,.T.);
#86383=ORIENTED_EDGE('',*,*,#57448,.F.);
#86384=ORIENTED_EDGE('',*,*,#57713,.F.);
#86385=ORIENTED_EDGE('',*,*,#57633,.F.);
#86386=ORIENTED_EDGE('',*,*,#57430,.F.);
#86387=ORIENTED_EDGE('',*,*,#57434,.F.);
#86388=ORIENTED_EDGE('',*,*,#57437,.F.);
#86389=ORIENTED_EDGE('',*,*,#57440,.F.);
#86390=ORIENTED_EDGE('',*,*,#57443,.F.);
#86391=ORIENTED_EDGE('',*,*,#57446,.F.);
#86392=ORIENTED_EDGE('',*,*,#57449,.F.);
#86393=ORIENTED_EDGE('',*,*,#57712,.F.);
#86394=ORIENTED_EDGE('',*,*,#57454,.F.);
#86395=ORIENTED_EDGE('',*,*,#57625,.F.);
#86396=ORIENTED_EDGE('',*,*,#57426,.F.);
#86397=ORIENTED_EDGE('',*,*,#57714,.F.);
#86398=ORIENTED_EDGE('',*,*,#57424,.F.);
#86399=ORIENTED_EDGE('',*,*,#57421,.F.);
#86400=ORIENTED_EDGE('',*,*,#57418,.F.);
#86401=ORIENTED_EDGE('',*,*,#57415,.F.);
#86402=ORIENTED_EDGE('',*,*,#57412,.F.);
#86403=ORIENTED_EDGE('',*,*,#57409,.F.);
#86404=ORIENTED_EDGE('',*,*,#57405,.F.);
#86405=ORIENTED_EDGE('',*,*,#57634,.F.);
#86406=ORIENTED_EDGE('',*,*,#57407,.F.);
#86407=ORIENTED_EDGE('',*,*,#57411,.F.);
#86408=ORIENTED_EDGE('',*,*,#57414,.F.);
#86409=ORIENTED_EDGE('',*,*,#57417,.F.);
#86410=ORIENTED_EDGE('',*,*,#57420,.F.);
#86411=ORIENTED_EDGE('',*,*,#57423,.F.);
#86412=ORIENTED_EDGE('',*,*,#57715,.F.);
#86413=ORIENTED_EDGE('',*,*,#57428,.F.);
#86414=ORIENTED_EDGE('',*,*,#57624,.F.);
#86415=ORIENTED_EDGE('',*,*,#57452,.T.);
#86416=ORIENTED_EDGE('',*,*,#57713,.T.);
#86417=ORIENTED_EDGE('',*,*,#57450,.T.);
#86418=ORIENTED_EDGE('',*,*,#57447,.T.);
#86419=ORIENTED_EDGE('',*,*,#57444,.T.);
#86420=ORIENTED_EDGE('',*,*,#57441,.T.);
#86421=ORIENTED_EDGE('',*,*,#57438,.T.);
#86422=ORIENTED_EDGE('',*,*,#57435,.T.);
#86423=ORIENTED_EDGE('',*,*,#57432,.T.);
#86424=ORIENTED_EDGE('',*,*,#57425,.T.);
#86425=ORIENTED_EDGE('',*,*,#57715,.T.);
#86426=ORIENTED_EDGE('',*,*,#57422,.F.);
#86427=ORIENTED_EDGE('',*,*,#57714,.T.);
#86428=ORIENTED_EDGE('',*,*,#57716,.F.);
#86429=ORIENTED_EDGE('',*,*,#57717,.T.);
#86430=ORIENTED_EDGE('',*,*,#57718,.T.);
#86431=ORIENTED_EDGE('',*,*,#57719,.T.);
#86432=ORIENTED_EDGE('',*,*,#57720,.F.);
#86433=ORIENTED_EDGE('',*,*,#57721,.T.);
#86434=ORIENTED_EDGE('',*,*,#57716,.T.);
#86435=ORIENTED_EDGE('',*,*,#57722,.T.);
#86436=ORIENTED_EDGE('',*,*,#57723,.F.);
#86437=ORIENTED_EDGE('',*,*,#57724,.T.);
#86438=ORIENTED_EDGE('',*,*,#57720,.T.);
#86439=ORIENTED_EDGE('',*,*,#57725,.T.);
#86440=ORIENTED_EDGE('',*,*,#57726,.F.);
#86441=ORIENTED_EDGE('',*,*,#57727,.T.);
#86442=ORIENTED_EDGE('',*,*,#57723,.T.);
#86443=ORIENTED_EDGE('',*,*,#57728,.T.);
#86444=ORIENTED_EDGE('',*,*,#57729,.F.);
#86445=ORIENTED_EDGE('',*,*,#57730,.T.);
#86446=ORIENTED_EDGE('',*,*,#57726,.T.);
#86447=ORIENTED_EDGE('',*,*,#57731,.T.);
#86448=ORIENTED_EDGE('',*,*,#57732,.F.);
#86449=ORIENTED_EDGE('',*,*,#57733,.T.);
#86450=ORIENTED_EDGE('',*,*,#57729,.T.);
#86451=ORIENTED_EDGE('',*,*,#57734,.T.);
#86452=ORIENTED_EDGE('',*,*,#57735,.F.);
#86453=ORIENTED_EDGE('',*,*,#57736,.T.);
#86454=ORIENTED_EDGE('',*,*,#57732,.T.);
#86455=ORIENTED_EDGE('',*,*,#57737,.T.);
#86456=ORIENTED_EDGE('',*,*,#57738,.F.);
#86457=ORIENTED_EDGE('',*,*,#57739,.T.);
#86458=ORIENTED_EDGE('',*,*,#57735,.T.);
#86459=ORIENTED_EDGE('',*,*,#57740,.T.);
#86460=ORIENTED_EDGE('',*,*,#57741,.F.);
#86461=ORIENTED_EDGE('',*,*,#57742,.T.);
#86462=ORIENTED_EDGE('',*,*,#57738,.T.);
#86463=ORIENTED_EDGE('',*,*,#57743,.T.);
#86464=ORIENTED_EDGE('',*,*,#57744,.F.);
#86465=ORIENTED_EDGE('',*,*,#57745,.T.);
#86466=ORIENTED_EDGE('',*,*,#57741,.T.);
#86467=ORIENTED_EDGE('',*,*,#57746,.T.);
#86468=ORIENTED_EDGE('',*,*,#57747,.F.);
#86469=ORIENTED_EDGE('',*,*,#57748,.T.);
#86470=ORIENTED_EDGE('',*,*,#57749,.F.);
#86471=ORIENTED_EDGE('',*,*,#57750,.F.);
#86472=ORIENTED_EDGE('',*,*,#57751,.T.);
#86473=ORIENTED_EDGE('',*,*,#57747,.T.);
#86474=ORIENTED_EDGE('',*,*,#57752,.F.);
#86475=ORIENTED_EDGE('',*,*,#57753,.F.);
#86476=ORIENTED_EDGE('',*,*,#57754,.F.);
#86477=ORIENTED_EDGE('',*,*,#57755,.T.);
#86478=ORIENTED_EDGE('',*,*,#57750,.T.);
#86479=ORIENTED_EDGE('',*,*,#57756,.F.);
#86480=ORIENTED_EDGE('',*,*,#57757,.F.);
#86481=ORIENTED_EDGE('',*,*,#57758,.T.);
#86482=ORIENTED_EDGE('',*,*,#57754,.T.);
#86483=ORIENTED_EDGE('',*,*,#57759,.F.);
#86484=ORIENTED_EDGE('',*,*,#57760,.F.);
#86485=ORIENTED_EDGE('',*,*,#57761,.T.);
#86486=ORIENTED_EDGE('',*,*,#57757,.T.);
#86487=ORIENTED_EDGE('',*,*,#57762,.F.);
#86488=ORIENTED_EDGE('',*,*,#57763,.F.);
#86489=ORIENTED_EDGE('',*,*,#57764,.T.);
#86490=ORIENTED_EDGE('',*,*,#57760,.T.);
#86491=ORIENTED_EDGE('',*,*,#57765,.F.);
#86492=ORIENTED_EDGE('',*,*,#57766,.F.);
#86493=ORIENTED_EDGE('',*,*,#57767,.T.);
#86494=ORIENTED_EDGE('',*,*,#57763,.T.);
#86495=ORIENTED_EDGE('',*,*,#57768,.F.);
#86496=ORIENTED_EDGE('',*,*,#57769,.F.);
#86497=ORIENTED_EDGE('',*,*,#57770,.T.);
#86498=ORIENTED_EDGE('',*,*,#57766,.T.);
#86499=ORIENTED_EDGE('',*,*,#57771,.F.);
#86500=ORIENTED_EDGE('',*,*,#57772,.F.);
#86501=ORIENTED_EDGE('',*,*,#57773,.T.);
#86502=ORIENTED_EDGE('',*,*,#57769,.T.);
#86503=ORIENTED_EDGE('',*,*,#57774,.F.);
#86504=ORIENTED_EDGE('',*,*,#57775,.F.);
#86505=ORIENTED_EDGE('',*,*,#57776,.T.);
#86506=ORIENTED_EDGE('',*,*,#57772,.T.);
#86507=ORIENTED_EDGE('',*,*,#57777,.F.);
#86508=ORIENTED_EDGE('',*,*,#57778,.F.);
#86509=ORIENTED_EDGE('',*,*,#57779,.T.);
#86510=ORIENTED_EDGE('',*,*,#57780,.F.);
#86511=ORIENTED_EDGE('',*,*,#57781,.T.);
#86512=ORIENTED_EDGE('',*,*,#57782,.F.);
#86513=ORIENTED_EDGE('',*,*,#57783,.T.);
#86514=ORIENTED_EDGE('',*,*,#57778,.T.);
#86515=ORIENTED_EDGE('',*,*,#57784,.T.);
#86516=ORIENTED_EDGE('',*,*,#57785,.F.);
#86517=ORIENTED_EDGE('',*,*,#57786,.T.);
#86518=ORIENTED_EDGE('',*,*,#57782,.T.);
#86519=ORIENTED_EDGE('',*,*,#57787,.T.);
#86520=ORIENTED_EDGE('',*,*,#57788,.F.);
#86521=ORIENTED_EDGE('',*,*,#57789,.T.);
#86522=ORIENTED_EDGE('',*,*,#57785,.T.);
#86523=ORIENTED_EDGE('',*,*,#57790,.T.);
#86524=ORIENTED_EDGE('',*,*,#57791,.F.);
#86525=ORIENTED_EDGE('',*,*,#57792,.T.);
#86526=ORIENTED_EDGE('',*,*,#57788,.T.);
#86527=ORIENTED_EDGE('',*,*,#57793,.T.);
#86528=ORIENTED_EDGE('',*,*,#57794,.F.);
#86529=ORIENTED_EDGE('',*,*,#57795,.T.);
#86530=ORIENTED_EDGE('',*,*,#57796,.F.);
#86531=ORIENTED_EDGE('',*,*,#57797,.F.);
#86532=ORIENTED_EDGE('',*,*,#57798,.F.);
#86533=ORIENTED_EDGE('',*,*,#57799,.T.);
#86534=ORIENTED_EDGE('',*,*,#57794,.T.);
#86535=ORIENTED_EDGE('',*,*,#57800,.F.);
#86536=ORIENTED_EDGE('',*,*,#57801,.F.);
#86537=ORIENTED_EDGE('',*,*,#57802,.T.);
#86538=ORIENTED_EDGE('',*,*,#57798,.T.);
#86539=ORIENTED_EDGE('',*,*,#57803,.F.);
#86540=ORIENTED_EDGE('',*,*,#57804,.F.);
#86541=ORIENTED_EDGE('',*,*,#57805,.T.);
#86542=ORIENTED_EDGE('',*,*,#57801,.T.);
#86543=ORIENTED_EDGE('',*,*,#57806,.F.);
#86544=ORIENTED_EDGE('',*,*,#57807,.F.);
#86545=ORIENTED_EDGE('',*,*,#57808,.T.);
#86546=ORIENTED_EDGE('',*,*,#57804,.T.);
#86547=ORIENTED_EDGE('',*,*,#57809,.F.);
#86548=ORIENTED_EDGE('',*,*,#57810,.F.);
#86549=ORIENTED_EDGE('',*,*,#57811,.F.);
#86550=ORIENTED_EDGE('',*,*,#57793,.F.);
#86551=ORIENTED_EDGE('',*,*,#57790,.F.);
#86552=ORIENTED_EDGE('',*,*,#57787,.F.);
#86553=ORIENTED_EDGE('',*,*,#57784,.F.);
#86554=ORIENTED_EDGE('',*,*,#57781,.F.);
#86555=ORIENTED_EDGE('',*,*,#57812,.F.);
#86556=ORIENTED_EDGE('',*,*,#57813,.T.);
#86557=ORIENTED_EDGE('',*,*,#57809,.T.);
#86558=ORIENTED_EDGE('',*,*,#57806,.T.);
#86559=ORIENTED_EDGE('',*,*,#57803,.T.);
#86560=ORIENTED_EDGE('',*,*,#57800,.T.);
#86561=ORIENTED_EDGE('',*,*,#57797,.T.);
#86562=ORIENTED_EDGE('',*,*,#57807,.T.);
#86563=ORIENTED_EDGE('',*,*,#57813,.F.);
#86564=ORIENTED_EDGE('',*,*,#57814,.F.);
#86565=ORIENTED_EDGE('',*,*,#57815,.T.);
#86566=ORIENTED_EDGE('',*,*,#57816,.F.);
#86567=ORIENTED_EDGE('',*,*,#57795,.F.);
#86568=ORIENTED_EDGE('',*,*,#57799,.F.);
#86569=ORIENTED_EDGE('',*,*,#57802,.F.);
#86570=ORIENTED_EDGE('',*,*,#57805,.F.);
#86571=ORIENTED_EDGE('',*,*,#57808,.F.);
#86572=ORIENTED_EDGE('',*,*,#57815,.F.);
#86573=ORIENTED_EDGE('',*,*,#57817,.F.);
#86574=ORIENTED_EDGE('',*,*,#57779,.F.);
#86575=ORIENTED_EDGE('',*,*,#57783,.F.);
#86576=ORIENTED_EDGE('',*,*,#57786,.F.);
#86577=ORIENTED_EDGE('',*,*,#57789,.F.);
#86578=ORIENTED_EDGE('',*,*,#57792,.F.);
#86579=ORIENTED_EDGE('',*,*,#57818,.F.);
#86580=ORIENTED_EDGE('',*,*,#57810,.T.);
#86581=ORIENTED_EDGE('',*,*,#57796,.T.);
#86582=ORIENTED_EDGE('',*,*,#57816,.T.);
#86583=ORIENTED_EDGE('',*,*,#57819,.T.);
#86584=ORIENTED_EDGE('',*,*,#57820,.F.);
#86585=ORIENTED_EDGE('',*,*,#57791,.T.);
#86586=ORIENTED_EDGE('',*,*,#57811,.T.);
#86587=ORIENTED_EDGE('',*,*,#57819,.F.);
#86588=ORIENTED_EDGE('',*,*,#57818,.T.);
#86589=ORIENTED_EDGE('',*,*,#57821,.F.);
#86590=ORIENTED_EDGE('',*,*,#57822,.T.);
#86591=ORIENTED_EDGE('',*,*,#57752,.T.);
#86592=ORIENTED_EDGE('',*,*,#57749,.T.);
#86593=ORIENTED_EDGE('',*,*,#57823,.T.);
#86594=ORIENTED_EDGE('',*,*,#57824,.F.);
#86595=ORIENTED_EDGE('',*,*,#57825,.F.);
#86596=ORIENTED_EDGE('',*,*,#57826,.F.);
#86597=ORIENTED_EDGE('',*,*,#57746,.F.);
#86598=ORIENTED_EDGE('',*,*,#57743,.F.);
#86599=ORIENTED_EDGE('',*,*,#57740,.F.);
#86600=ORIENTED_EDGE('',*,*,#57737,.F.);
#86601=ORIENTED_EDGE('',*,*,#57734,.F.);
#86602=ORIENTED_EDGE('',*,*,#57731,.F.);
#86603=ORIENTED_EDGE('',*,*,#57728,.F.);
#86604=ORIENTED_EDGE('',*,*,#57725,.F.);
#86605=ORIENTED_EDGE('',*,*,#57722,.F.);
#86606=ORIENTED_EDGE('',*,*,#57719,.F.);
#86607=ORIENTED_EDGE('',*,*,#57827,.F.);
#86608=ORIENTED_EDGE('',*,*,#57828,.T.);
#86609=ORIENTED_EDGE('',*,*,#57777,.T.);
#86610=ORIENTED_EDGE('',*,*,#57774,.T.);
#86611=ORIENTED_EDGE('',*,*,#57771,.T.);
#86612=ORIENTED_EDGE('',*,*,#57768,.T.);
#86613=ORIENTED_EDGE('',*,*,#57765,.T.);
#86614=ORIENTED_EDGE('',*,*,#57762,.T.);
#86615=ORIENTED_EDGE('',*,*,#57759,.T.);
#86616=ORIENTED_EDGE('',*,*,#57756,.T.);
#86617=ORIENTED_EDGE('',*,*,#57753,.T.);
#86618=ORIENTED_EDGE('',*,*,#57822,.F.);
#86619=ORIENTED_EDGE('',*,*,#57775,.T.);
#86620=ORIENTED_EDGE('',*,*,#57828,.F.);
#86621=ORIENTED_EDGE('',*,*,#57829,.F.);
#86622=ORIENTED_EDGE('',*,*,#57830,.T.);
#86623=ORIENTED_EDGE('',*,*,#57823,.F.);
#86624=ORIENTED_EDGE('',*,*,#57748,.F.);
#86625=ORIENTED_EDGE('',*,*,#57751,.F.);
#86626=ORIENTED_EDGE('',*,*,#57755,.F.);
#86627=ORIENTED_EDGE('',*,*,#57758,.F.);
#86628=ORIENTED_EDGE('',*,*,#57761,.F.);
#86629=ORIENTED_EDGE('',*,*,#57764,.F.);
#86630=ORIENTED_EDGE('',*,*,#57767,.F.);
#86631=ORIENTED_EDGE('',*,*,#57770,.F.);
#86632=ORIENTED_EDGE('',*,*,#57773,.F.);
#86633=ORIENTED_EDGE('',*,*,#57776,.F.);
#86634=ORIENTED_EDGE('',*,*,#57830,.F.);
#86635=ORIENTED_EDGE('',*,*,#57831,.F.);
#86636=ORIENTED_EDGE('',*,*,#57717,.F.);
#86637=ORIENTED_EDGE('',*,*,#57721,.F.);
#86638=ORIENTED_EDGE('',*,*,#57724,.F.);
#86639=ORIENTED_EDGE('',*,*,#57727,.F.);
#86640=ORIENTED_EDGE('',*,*,#57730,.F.);
#86641=ORIENTED_EDGE('',*,*,#57733,.F.);
#86642=ORIENTED_EDGE('',*,*,#57736,.F.);
#86643=ORIENTED_EDGE('',*,*,#57739,.F.);
#86644=ORIENTED_EDGE('',*,*,#57742,.F.);
#86645=ORIENTED_EDGE('',*,*,#57745,.F.);
#86646=ORIENTED_EDGE('',*,*,#57832,.F.);
#86647=ORIENTED_EDGE('',*,*,#57833,.F.);
#86648=ORIENTED_EDGE('',*,*,#57834,.F.);
#86649=ORIENTED_EDGE('',*,*,#57835,.F.);
#86650=ORIENTED_EDGE('',*,*,#57836,.T.);
#86651=ORIENTED_EDGE('',*,*,#57837,.F.);
#86652=ORIENTED_EDGE('',*,*,#57836,.F.);
#86653=ORIENTED_EDGE('',*,*,#57838,.F.);
#86654=ORIENTED_EDGE('',*,*,#57839,.T.);
#86655=ORIENTED_EDGE('',*,*,#57820,.T.);
#86656=ORIENTED_EDGE('',*,*,#57839,.F.);
#86657=ORIENTED_EDGE('',*,*,#57744,.T.);
#86658=ORIENTED_EDGE('',*,*,#57826,.T.);
#86659=ORIENTED_EDGE('',*,*,#57840,.F.);
#86660=ORIENTED_EDGE('',*,*,#57832,.T.);
#86661=ORIENTED_EDGE('',*,*,#57834,.T.);
#86662=ORIENTED_EDGE('',*,*,#57835,.T.);
#86663=ORIENTED_EDGE('',*,*,#57841,.T.);
#86664=ORIENTED_EDGE('',*,*,#57824,.T.);
#86665=ORIENTED_EDGE('',*,*,#57842,.T.);
#86666=ORIENTED_EDGE('',*,*,#57821,.T.);
#86667=ORIENTED_EDGE('',*,*,#57841,.F.);
#86668=ORIENTED_EDGE('',*,*,#57843,.F.);
#86669=ORIENTED_EDGE('',*,*,#57844,.T.);
#86670=ORIENTED_EDGE('',*,*,#57845,.T.);
#86671=ORIENTED_EDGE('',*,*,#57844,.F.);
#86672=ORIENTED_EDGE('',*,*,#57846,.F.);
#86673=ORIENTED_EDGE('',*,*,#57847,.T.);
#86674=ORIENTED_EDGE('',*,*,#57843,.T.);
#86675=ORIENTED_EDGE('',*,*,#57847,.F.);
#86676=ORIENTED_EDGE('',*,*,#57848,.F.);
#86677=ORIENTED_EDGE('',*,*,#57849,.T.);
#86678=ORIENTED_EDGE('',*,*,#57846,.T.);
#86679=ORIENTED_EDGE('',*,*,#57849,.F.);
#86680=ORIENTED_EDGE('',*,*,#57837,.T.);
#86681=ORIENTED_EDGE('',*,*,#57845,.F.);
#86682=ORIENTED_EDGE('',*,*,#57825,.T.);
#86683=ORIENTED_EDGE('',*,*,#57842,.F.);
#86684=ORIENTED_EDGE('',*,*,#57833,.T.);
#86685=ORIENTED_EDGE('',*,*,#57840,.T.);
#86686=ORIENTED_EDGE('',*,*,#57827,.T.);
#86687=ORIENTED_EDGE('',*,*,#57718,.F.);
#86688=ORIENTED_EDGE('',*,*,#57831,.T.);
#86689=ORIENTED_EDGE('',*,*,#57829,.T.);
#86690=ORIENTED_EDGE('',*,*,#57838,.T.);
#86691=ORIENTED_EDGE('',*,*,#57812,.T.);
#86692=ORIENTED_EDGE('',*,*,#57780,.T.);
#86693=ORIENTED_EDGE('',*,*,#57817,.T.);
#86694=ORIENTED_EDGE('',*,*,#57814,.T.);
#86695=ORIENTED_EDGE('',*,*,#57848,.T.);
#86696=ORIENTED_EDGE('',*,*,#57850,.T.);
#86697=ORIENTED_EDGE('',*,*,#57851,.T.);
#86698=ORIENTED_EDGE('',*,*,#57852,.F.);
#86699=ORIENTED_EDGE('',*,*,#57853,.T.);
#86700=ORIENTED_EDGE('',*,*,#57851,.F.);
#86701=ORIENTED_EDGE('',*,*,#57853,.F.);
#86702=ORIENTED_EDGE('',*,*,#57854,.F.);
#86703=ORIENTED_EDGE('',*,*,#57855,.T.);
#86704=ORIENTED_EDGE('',*,*,#57850,.F.);
#86705=ORIENTED_EDGE('',*,*,#57855,.F.);
#86706=ORIENTED_EDGE('',*,*,#57854,.T.);
#86707=ORIENTED_EDGE('',*,*,#57852,.T.);
#86708=ORIENTED_EDGE('',*,*,#57856,.F.);
#86709=ORIENTED_EDGE('',*,*,#57857,.T.);
#86710=ORIENTED_EDGE('',*,*,#57858,.T.);
#86711=ORIENTED_EDGE('',*,*,#57859,.T.);
#86712=ORIENTED_EDGE('',*,*,#57860,.F.);
#86713=ORIENTED_EDGE('',*,*,#57861,.T.);
#86714=ORIENTED_EDGE('',*,*,#57856,.T.);
#86715=ORIENTED_EDGE('',*,*,#57862,.T.);
#86716=ORIENTED_EDGE('',*,*,#57863,.F.);
#86717=ORIENTED_EDGE('',*,*,#57864,.T.);
#86718=ORIENTED_EDGE('',*,*,#57860,.T.);
#86719=ORIENTED_EDGE('',*,*,#57865,.T.);
#86720=ORIENTED_EDGE('',*,*,#57866,.F.);
#86721=ORIENTED_EDGE('',*,*,#57867,.T.);
#86722=ORIENTED_EDGE('',*,*,#57863,.T.);
#86723=ORIENTED_EDGE('',*,*,#57868,.T.);
#86724=ORIENTED_EDGE('',*,*,#57869,.F.);
#86725=ORIENTED_EDGE('',*,*,#57870,.T.);
#86726=ORIENTED_EDGE('',*,*,#57866,.T.);
#86727=ORIENTED_EDGE('',*,*,#57871,.T.);
#86728=ORIENTED_EDGE('',*,*,#57872,.F.);
#86729=ORIENTED_EDGE('',*,*,#57873,.T.);
#86730=ORIENTED_EDGE('',*,*,#57869,.T.);
#86731=ORIENTED_EDGE('',*,*,#57874,.T.);
#86732=ORIENTED_EDGE('',*,*,#57875,.F.);
#86733=ORIENTED_EDGE('',*,*,#57876,.T.);
#86734=ORIENTED_EDGE('',*,*,#57877,.F.);
#86735=ORIENTED_EDGE('',*,*,#57878,.F.);
#86736=ORIENTED_EDGE('',*,*,#57879,.F.);
#86737=ORIENTED_EDGE('',*,*,#57880,.T.);
#86738=ORIENTED_EDGE('',*,*,#57875,.T.);
#86739=ORIENTED_EDGE('',*,*,#57881,.F.);
#86740=ORIENTED_EDGE('',*,*,#57882,.F.);
#86741=ORIENTED_EDGE('',*,*,#57883,.T.);
#86742=ORIENTED_EDGE('',*,*,#57879,.T.);
#86743=ORIENTED_EDGE('',*,*,#57884,.F.);
#86744=ORIENTED_EDGE('',*,*,#57885,.F.);
#86745=ORIENTED_EDGE('',*,*,#57886,.T.);
#86746=ORIENTED_EDGE('',*,*,#57882,.T.);
#86747=ORIENTED_EDGE('',*,*,#57887,.F.);
#86748=ORIENTED_EDGE('',*,*,#57888,.F.);
#86749=ORIENTED_EDGE('',*,*,#57889,.T.);
#86750=ORIENTED_EDGE('',*,*,#57885,.T.);
#86751=ORIENTED_EDGE('',*,*,#57890,.F.);
#86752=ORIENTED_EDGE('',*,*,#57891,.F.);
#86753=ORIENTED_EDGE('',*,*,#57892,.T.);
#86754=ORIENTED_EDGE('',*,*,#57888,.T.);
#86755=ORIENTED_EDGE('',*,*,#57893,.F.);
#86756=ORIENTED_EDGE('',*,*,#57894,.F.);
#86757=ORIENTED_EDGE('',*,*,#57895,.F.);
#86758=ORIENTED_EDGE('',*,*,#57874,.F.);
#86759=ORIENTED_EDGE('',*,*,#57871,.F.);
#86760=ORIENTED_EDGE('',*,*,#57868,.F.);
#86761=ORIENTED_EDGE('',*,*,#57865,.F.);
#86762=ORIENTED_EDGE('',*,*,#57862,.F.);
#86763=ORIENTED_EDGE('',*,*,#57859,.F.);
#86764=ORIENTED_EDGE('',*,*,#57896,.F.);
#86765=ORIENTED_EDGE('',*,*,#57897,.F.);
#86766=ORIENTED_EDGE('',*,*,#57898,.T.);
#86767=ORIENTED_EDGE('',*,*,#57893,.T.);
#86768=ORIENTED_EDGE('',*,*,#57890,.T.);
#86769=ORIENTED_EDGE('',*,*,#57887,.T.);
#86770=ORIENTED_EDGE('',*,*,#57884,.T.);
#86771=ORIENTED_EDGE('',*,*,#57881,.T.);
#86772=ORIENTED_EDGE('',*,*,#57878,.T.);
#86773=ORIENTED_EDGE('',*,*,#57899,.T.);
#86774=ORIENTED_EDGE('',*,*,#57900,.T.);
#86775=ORIENTED_EDGE('',*,*,#57901,.T.);
#86776=ORIENTED_EDGE('',*,*,#57897,.T.);
#86777=ORIENTED_EDGE('',*,*,#57891,.T.);
#86778=ORIENTED_EDGE('',*,*,#57898,.F.);
#86779=ORIENTED_EDGE('',*,*,#57901,.F.);
#86780=ORIENTED_EDGE('',*,*,#57902,.T.);
#86781=ORIENTED_EDGE('',*,*,#57903,.F.);
#86782=ORIENTED_EDGE('',*,*,#57876,.F.);
#86783=ORIENTED_EDGE('',*,*,#57880,.F.);
#86784=ORIENTED_EDGE('',*,*,#57883,.F.);
#86785=ORIENTED_EDGE('',*,*,#57886,.F.);
#86786=ORIENTED_EDGE('',*,*,#57889,.F.);
#86787=ORIENTED_EDGE('',*,*,#57892,.F.);
#86788=ORIENTED_EDGE('',*,*,#57902,.F.);
#86789=ORIENTED_EDGE('',*,*,#57900,.F.);
#86790=ORIENTED_EDGE('',*,*,#57904,.F.);
#86791=ORIENTED_EDGE('',*,*,#57857,.F.);
#86792=ORIENTED_EDGE('',*,*,#57861,.F.);
#86793=ORIENTED_EDGE('',*,*,#57864,.F.);
#86794=ORIENTED_EDGE('',*,*,#57867,.F.);
#86795=ORIENTED_EDGE('',*,*,#57870,.F.);
#86796=ORIENTED_EDGE('',*,*,#57873,.F.);
#86797=ORIENTED_EDGE('',*,*,#57905,.F.);
#86798=ORIENTED_EDGE('',*,*,#57896,.T.);
#86799=ORIENTED_EDGE('',*,*,#57858,.F.);
#86800=ORIENTED_EDGE('',*,*,#57904,.T.);
#86801=ORIENTED_EDGE('',*,*,#57906,.T.);
#86802=ORIENTED_EDGE('',*,*,#57907,.T.);
#86803=ORIENTED_EDGE('',*,*,#57894,.T.);
#86804=ORIENTED_EDGE('',*,*,#57877,.T.);
#86805=ORIENTED_EDGE('',*,*,#57903,.T.);
#86806=ORIENTED_EDGE('',*,*,#57908,.T.);
#86807=ORIENTED_EDGE('',*,*,#57909,.F.);
#86808=ORIENTED_EDGE('',*,*,#57872,.T.);
#86809=ORIENTED_EDGE('',*,*,#57895,.T.);
#86810=ORIENTED_EDGE('',*,*,#57908,.F.);
#86811=ORIENTED_EDGE('',*,*,#57905,.T.);
#86812=ORIENTED_EDGE('',*,*,#57910,.F.);
#86813=ORIENTED_EDGE('',*,*,#57911,.T.);
#86814=ORIENTED_EDGE('',*,*,#57912,.T.);
#86815=ORIENTED_EDGE('',*,*,#57913,.T.);
#86816=ORIENTED_EDGE('',*,*,#57911,.F.);
#86817=ORIENTED_EDGE('',*,*,#57914,.F.);
#86818=ORIENTED_EDGE('',*,*,#57915,.T.);
#86819=ORIENTED_EDGE('',*,*,#57910,.T.);
#86820=ORIENTED_EDGE('',*,*,#57915,.F.);
#86821=ORIENTED_EDGE('',*,*,#57916,.F.);
#86822=ORIENTED_EDGE('',*,*,#57917,.T.);
#86823=ORIENTED_EDGE('',*,*,#57914,.T.);
#86824=ORIENTED_EDGE('',*,*,#57917,.F.);
#86825=ORIENTED_EDGE('',*,*,#57918,.T.);
#86826=ORIENTED_EDGE('',*,*,#57919,.T.);
#86827=ORIENTED_EDGE('',*,*,#57920,.T.);
#86828=ORIENTED_EDGE('',*,*,#57919,.F.);
#86829=ORIENTED_EDGE('',*,*,#57906,.F.);
#86830=ORIENTED_EDGE('',*,*,#57899,.F.);
#86831=ORIENTED_EDGE('',*,*,#57907,.F.);
#86832=ORIENTED_EDGE('',*,*,#57921,.T.);
#86833=ORIENTED_EDGE('',*,*,#57922,.T.);
#86834=ORIENTED_EDGE('',*,*,#57921,.F.);
#86835=ORIENTED_EDGE('',*,*,#57923,.F.);
#86836=ORIENTED_EDGE('',*,*,#57924,.F.);
#86837=ORIENTED_EDGE('',*,*,#57925,.T.);
#86838=ORIENTED_EDGE('',*,*,#57909,.T.);
#86839=ORIENTED_EDGE('',*,*,#57925,.F.);
#86840=ORIENTED_EDGE('',*,*,#57923,.T.);
#86841=ORIENTED_EDGE('',*,*,#57924,.T.);
#86842=ORIENTED_EDGE('',*,*,#57926,.T.);
#86843=ORIENTED_EDGE('',*,*,#57912,.F.);
#86844=ORIENTED_EDGE('',*,*,#57913,.F.);
#86845=ORIENTED_EDGE('',*,*,#57926,.F.);
#86846=ORIENTED_EDGE('',*,*,#57927,.F.);
#86847=ORIENTED_EDGE('',*,*,#57928,.T.);
#86848=ORIENTED_EDGE('',*,*,#57916,.T.);
#86849=ORIENTED_EDGE('',*,*,#57928,.F.);
#86850=ORIENTED_EDGE('',*,*,#57929,.F.);
#86851=ORIENTED_EDGE('',*,*,#57930,.F.);
#86852=ORIENTED_EDGE('',*,*,#57931,.F.);
#86853=ORIENTED_EDGE('',*,*,#57932,.F.);
#86854=ORIENTED_EDGE('',*,*,#57933,.F.);
#86855=ORIENTED_EDGE('',*,*,#57934,.F.);
#86856=ORIENTED_EDGE('',*,*,#57918,.F.);
#86857=ORIENTED_EDGE('',*,*,#57935,.T.);
#86858=ORIENTED_EDGE('',*,*,#57936,.T.);
#86859=ORIENTED_EDGE('',*,*,#57937,.T.);
#86860=ORIENTED_EDGE('',*,*,#57938,.T.);
#86861=ORIENTED_EDGE('',*,*,#57939,.T.);
#86862=ORIENTED_EDGE('',*,*,#57940,.T.);
#86863=ORIENTED_EDGE('',*,*,#57922,.F.);
#86864=ORIENTED_EDGE('',*,*,#57929,.T.);
#86865=ORIENTED_EDGE('',*,*,#57941,.F.);
#86866=ORIENTED_EDGE('',*,*,#57935,.F.);
#86867=ORIENTED_EDGE('',*,*,#57942,.T.);
#86868=ORIENTED_EDGE('',*,*,#57934,.T.);
#86869=ORIENTED_EDGE('',*,*,#57943,.F.);
#86870=ORIENTED_EDGE('',*,*,#57936,.F.);
#86871=ORIENTED_EDGE('',*,*,#57941,.T.);
#86872=ORIENTED_EDGE('',*,*,#57933,.T.);
#86873=ORIENTED_EDGE('',*,*,#57944,.F.);
#86874=ORIENTED_EDGE('',*,*,#57937,.F.);
#86875=ORIENTED_EDGE('',*,*,#57943,.T.);
#86876=ORIENTED_EDGE('',*,*,#57932,.T.);
#86877=ORIENTED_EDGE('',*,*,#57945,.F.);
#86878=ORIENTED_EDGE('',*,*,#57938,.F.);
#86879=ORIENTED_EDGE('',*,*,#57944,.T.);
#86880=ORIENTED_EDGE('',*,*,#57931,.T.);
#86881=ORIENTED_EDGE('',*,*,#57946,.F.);
#86882=ORIENTED_EDGE('',*,*,#57939,.F.);
#86883=ORIENTED_EDGE('',*,*,#57945,.T.);
#86884=ORIENTED_EDGE('',*,*,#57930,.T.);
#86885=ORIENTED_EDGE('',*,*,#57942,.F.);
#86886=ORIENTED_EDGE('',*,*,#57940,.F.);
#86887=ORIENTED_EDGE('',*,*,#57946,.T.);
#86888=ORIENTED_EDGE('',*,*,#57920,.F.);
#86889=ORIENTED_EDGE('',*,*,#57927,.T.);
#86890=ORIENTED_EDGE('',*,*,#57947,.F.);
#86891=ORIENTED_EDGE('',*,*,#57948,.T.);
#86892=ORIENTED_EDGE('',*,*,#57949,.T.);
#86893=ORIENTED_EDGE('',*,*,#57948,.F.);
#86894=ORIENTED_EDGE('',*,*,#57950,.F.);
#86895=ORIENTED_EDGE('',*,*,#57951,.T.);
#86896=ORIENTED_EDGE('',*,*,#57952,.F.);
#86897=ORIENTED_EDGE('',*,*,#57951,.F.);
#86898=ORIENTED_EDGE('',*,*,#57953,.F.);
#86899=ORIENTED_EDGE('',*,*,#57954,.T.);
#86900=ORIENTED_EDGE('',*,*,#57955,.T.);
#86901=ORIENTED_EDGE('',*,*,#57954,.F.);
#86902=ORIENTED_EDGE('',*,*,#57956,.F.);
#86903=ORIENTED_EDGE('',*,*,#57957,.T.);
#86904=ORIENTED_EDGE('',*,*,#57958,.T.);
#86905=ORIENTED_EDGE('',*,*,#57957,.F.);
#86906=ORIENTED_EDGE('',*,*,#57959,.F.);
#86907=ORIENTED_EDGE('',*,*,#57960,.T.);
#86908=ORIENTED_EDGE('',*,*,#57961,.T.);
#86909=ORIENTED_EDGE('',*,*,#57960,.F.);
#86910=ORIENTED_EDGE('',*,*,#57962,.F.);
#86911=ORIENTED_EDGE('',*,*,#57963,.T.);
#86912=ORIENTED_EDGE('',*,*,#57964,.T.);
#86913=ORIENTED_EDGE('',*,*,#57965,.F.);
#86914=ORIENTED_EDGE('',*,*,#57966,.T.);
#86915=ORIENTED_EDGE('',*,*,#57967,.T.);
#86916=ORIENTED_EDGE('',*,*,#57968,.F.);
#86917=ORIENTED_EDGE('',*,*,#57969,.T.);
#86918=ORIENTED_EDGE('',*,*,#57970,.T.);
#86919=ORIENTED_EDGE('',*,*,#57971,.T.);
#86920=ORIENTED_EDGE('',*,*,#57972,.T.);
#86921=ORIENTED_EDGE('',*,*,#57973,.T.);
#86922=ORIENTED_EDGE('',*,*,#57974,.F.);
#86923=ORIENTED_EDGE('',*,*,#57975,.T.);
#86924=ORIENTED_EDGE('',*,*,#57976,.T.);
#86925=ORIENTED_EDGE('',*,*,#57977,.T.);
#86926=ORIENTED_EDGE('',*,*,#57978,.T.);
#86927=ORIENTED_EDGE('',*,*,#57979,.T.);
#86928=ORIENTED_EDGE('',*,*,#57980,.F.);
#86929=ORIENTED_EDGE('',*,*,#57964,.F.);
#86930=ORIENTED_EDGE('',*,*,#57958,.F.);
#86931=ORIENTED_EDGE('',*,*,#57961,.F.);
#86932=ORIENTED_EDGE('',*,*,#57981,.T.);
#86933=ORIENTED_EDGE('',*,*,#57982,.T.);
#86934=ORIENTED_EDGE('',*,*,#57983,.T.);
#86935=ORIENTED_EDGE('',*,*,#57984,.T.);
#86936=ORIENTED_EDGE('',*,*,#57985,.T.);
#86937=ORIENTED_EDGE('',*,*,#57986,.T.);
#86938=ORIENTED_EDGE('',*,*,#57987,.T.);
#86939=ORIENTED_EDGE('',*,*,#57962,.T.);
#86940=ORIENTED_EDGE('',*,*,#57988,.T.);
#86941=ORIENTED_EDGE('',*,*,#57989,.T.);
#86942=ORIENTED_EDGE('',*,*,#57990,.T.);
#86943=ORIENTED_EDGE('',*,*,#57991,.T.);
#86944=ORIENTED_EDGE('',*,*,#57992,.T.);
#86945=ORIENTED_EDGE('',*,*,#57993,.T.);
#86946=ORIENTED_EDGE('',*,*,#57994,.T.);
#86947=ORIENTED_EDGE('',*,*,#57995,.T.);
#86948=ORIENTED_EDGE('',*,*,#57949,.F.);
#86949=ORIENTED_EDGE('',*,*,#57955,.F.);
#86950=ORIENTED_EDGE('',*,*,#57996,.T.);
#86951=ORIENTED_EDGE('',*,*,#57997,.T.);
#86952=ORIENTED_EDGE('',*,*,#57998,.T.);
#86953=ORIENTED_EDGE('',*,*,#57999,.T.);
#86954=ORIENTED_EDGE('',*,*,#57947,.T.);
#86955=ORIENTED_EDGE('',*,*,#57950,.T.);
#86956=ORIENTED_EDGE('',*,*,#57968,.T.);
#86957=ORIENTED_EDGE('',*,*,#58000,.T.);
#86958=ORIENTED_EDGE('',*,*,#57974,.T.);
#86959=ORIENTED_EDGE('',*,*,#57963,.F.);
#86960=ORIENTED_EDGE('',*,*,#57987,.F.);
#86961=ORIENTED_EDGE('',*,*,#58001,.T.);
#86962=ORIENTED_EDGE('',*,*,#57952,.T.);
#86963=ORIENTED_EDGE('',*,*,#57980,.T.);
#86964=ORIENTED_EDGE('',*,*,#58002,.T.);
#86965=ORIENTED_EDGE('',*,*,#57970,.F.);
#86966=ORIENTED_EDGE('',*,*,#58003,.T.);
#86967=ORIENTED_EDGE('',*,*,#57988,.F.);
#86968=ORIENTED_EDGE('',*,*,#57965,.T.);
#86969=ORIENTED_EDGE('',*,*,#57953,.T.);
#86970=ORIENTED_EDGE('',*,*,#57959,.T.);
#86971=ORIENTED_EDGE('',*,*,#57956,.T.);
#86972=ORIENTED_EDGE('',*,*,#58003,.F.);
#86973=ORIENTED_EDGE('',*,*,#57973,.F.);
#86974=ORIENTED_EDGE('',*,*,#58004,.F.);
#86975=ORIENTED_EDGE('',*,*,#57989,.F.);
#86976=ORIENTED_EDGE('',*,*,#58001,.F.);
#86977=ORIENTED_EDGE('',*,*,#57986,.F.);
#86978=ORIENTED_EDGE('',*,*,#58005,.F.);
#86979=ORIENTED_EDGE('',*,*,#57969,.F.);
#86980=ORIENTED_EDGE('',*,*,#58006,.F.);
#86981=ORIENTED_EDGE('',*,*,#58004,.T.);
#86982=ORIENTED_EDGE('',*,*,#58007,.F.);
#86983=ORIENTED_EDGE('',*,*,#58008,.F.);
#86984=ORIENTED_EDGE('',*,*,#58005,.T.);
#86985=ORIENTED_EDGE('',*,*,#58009,.F.);
#86986=ORIENTED_EDGE('',*,*,#58002,.F.);
#86987=ORIENTED_EDGE('',*,*,#57979,.F.);
#86988=ORIENTED_EDGE('',*,*,#58010,.F.);
#86989=ORIENTED_EDGE('',*,*,#57971,.F.);
#86990=ORIENTED_EDGE('',*,*,#58007,.T.);
#86991=ORIENTED_EDGE('',*,*,#57972,.F.);
#86992=ORIENTED_EDGE('',*,*,#58011,.F.);
#86993=ORIENTED_EDGE('',*,*,#57995,.F.);
#86994=ORIENTED_EDGE('',*,*,#58006,.T.);
#86995=ORIENTED_EDGE('',*,*,#57994,.F.);
#86996=ORIENTED_EDGE('',*,*,#58012,.F.);
#86997=ORIENTED_EDGE('',*,*,#57990,.F.);
#86998=ORIENTED_EDGE('',*,*,#58013,.F.);
#86999=ORIENTED_EDGE('',*,*,#57991,.F.);
#87000=ORIENTED_EDGE('',*,*,#58014,.F.);
#87001=ORIENTED_EDGE('',*,*,#57984,.F.);
#87002=ORIENTED_EDGE('',*,*,#58009,.T.);
#87003=ORIENTED_EDGE('',*,*,#57985,.F.);
#87004=ORIENTED_EDGE('',*,*,#58015,.F.);
#87005=ORIENTED_EDGE('',*,*,#57996,.F.);
#87006=ORIENTED_EDGE('',*,*,#58008,.T.);
#87007=ORIENTED_EDGE('',*,*,#57999,.F.);
#87008=ORIENTED_EDGE('',*,*,#58016,.F.);
#87009=ORIENTED_EDGE('',*,*,#57966,.F.);
#87010=ORIENTED_EDGE('',*,*,#58000,.F.);
#87011=ORIENTED_EDGE('',*,*,#57967,.F.);
#87012=ORIENTED_EDGE('',*,*,#58017,.F.);
#87013=ORIENTED_EDGE('',*,*,#57975,.F.);
#87014=ORIENTED_EDGE('',*,*,#58011,.T.);
#87015=ORIENTED_EDGE('',*,*,#58010,.T.);
#87016=ORIENTED_EDGE('',*,*,#58018,.F.);
#87017=ORIENTED_EDGE('',*,*,#58014,.T.);
#87018=ORIENTED_EDGE('',*,*,#58012,.T.);
#87019=ORIENTED_EDGE('',*,*,#58019,.F.);
#87020=ORIENTED_EDGE('',*,*,#58015,.T.);
#87021=ORIENTED_EDGE('',*,*,#58013,.T.);
#87022=ORIENTED_EDGE('',*,*,#58020,.F.);
#87023=ORIENTED_EDGE('',*,*,#58017,.T.);
#87024=ORIENTED_EDGE('',*,*,#58016,.T.);
#87025=ORIENTED_EDGE('',*,*,#58021,.F.);
#87026=ORIENTED_EDGE('',*,*,#58018,.T.);
#87027=ORIENTED_EDGE('',*,*,#57978,.F.);
#87028=ORIENTED_EDGE('',*,*,#58022,.F.);
#87029=ORIENTED_EDGE('',*,*,#57992,.F.);
#87030=ORIENTED_EDGE('',*,*,#58019,.T.);
#87031=ORIENTED_EDGE('',*,*,#57993,.F.);
#87032=ORIENTED_EDGE('',*,*,#58023,.F.);
#87033=ORIENTED_EDGE('',*,*,#57981,.F.);
#87034=ORIENTED_EDGE('',*,*,#58020,.T.);
#87035=ORIENTED_EDGE('',*,*,#57983,.F.);
#87036=ORIENTED_EDGE('',*,*,#58024,.F.);
#87037=ORIENTED_EDGE('',*,*,#57997,.F.);
#87038=ORIENTED_EDGE('',*,*,#58021,.T.);
#87039=ORIENTED_EDGE('',*,*,#57998,.F.);
#87040=ORIENTED_EDGE('',*,*,#58025,.F.);
#87041=ORIENTED_EDGE('',*,*,#57976,.F.);
#87042=ORIENTED_EDGE('',*,*,#58023,.T.);
#87043=ORIENTED_EDGE('',*,*,#58022,.T.);
#87044=ORIENTED_EDGE('',*,*,#58026,.F.);
#87045=ORIENTED_EDGE('',*,*,#58025,.T.);
#87046=ORIENTED_EDGE('',*,*,#58024,.T.);
#87047=ORIENTED_EDGE('',*,*,#58027,.F.);
#87048=ORIENTED_EDGE('',*,*,#58026,.T.);
#87049=ORIENTED_EDGE('',*,*,#57977,.F.);
#87050=ORIENTED_EDGE('',*,*,#58027,.T.);
#87051=ORIENTED_EDGE('',*,*,#57982,.F.);
#87052=CYLINDRICAL_SURFACE('',#94907,1.2645);
#87053=CYLINDRICAL_SURFACE('',#94909,1.2645);
#87054=CYLINDRICAL_SURFACE('',#94910,1.2645);
#87055=CYLINDRICAL_SURFACE('',#94911,1.2645);
#87056=CYLINDRICAL_SURFACE('',#94913,1.2645);
#87057=CYLINDRICAL_SURFACE('',#94915,1.2645);
#87058=CYLINDRICAL_SURFACE('',#94916,1.2645);
#87059=CYLINDRICAL_SURFACE('',#94917,1.2645);
#87060=CYLINDRICAL_SURFACE('',#94919,1.543);
#87061=CYLINDRICAL_SURFACE('',#94921,1.543);
#87062=CYLINDRICAL_SURFACE('',#94922,1.543);
#87063=CYLINDRICAL_SURFACE('',#94923,1.543);
#87064=CYLINDRICAL_SURFACE('',#94925,1.543);
#87065=CYLINDRICAL_SURFACE('',#94927,1.543);
#87066=CYLINDRICAL_SURFACE('',#94928,1.543);
#87067=CYLINDRICAL_SURFACE('',#94929,1.543);
#87068=CYLINDRICAL_SURFACE('',#94931,1.543);
#87069=CYLINDRICAL_SURFACE('',#94932,1.543);
#87070=CYLINDRICAL_SURFACE('',#94933,1.2645);
#87071=CYLINDRICAL_SURFACE('',#94934,1.2645);
#87072=CYLINDRICAL_SURFACE('',#94949,8.);
#87073=CYLINDRICAL_SURFACE('',#94957,18.25);
#87074=CYLINDRICAL_SURFACE('',#94966,18.25);
#87075=CYLINDRICAL_SURFACE('',#94975,2.5);
#87076=CYLINDRICAL_SURFACE('',#95020,3.50000000056584);
#87077=CYLINDRICAL_SURFACE('',#95022,1.);
#87078=CYLINDRICAL_SURFACE('',#95023,1.);
#87079=CYLINDRICAL_SURFACE('',#95026,1.);
#87080=CYLINDRICAL_SURFACE('',#95027,1.);
#87081=CYLINDRICAL_SURFACE('',#95032,1.);
#87082=CYLINDRICAL_SURFACE('',#95079,3.);
#87083=CYLINDRICAL_SURFACE('',#95081,1.875);
#87084=CYLINDRICAL_SURFACE('',#95082,1.875);
#87085=CYLINDRICAL_SURFACE('',#95084,3.);
#87086=CYLINDRICAL_SURFACE('',#95086,1.875);
#87087=CYLINDRICAL_SURFACE('',#95088,3.);
#87088=CYLINDRICAL_SURFACE('',#95090,1.875);
#87089=CYLINDRICAL_SURFACE('',#95092,3.);
#87090=CYLINDRICAL_SURFACE('',#95094,1.875);
#87091=CYLINDRICAL_SURFACE('',#95096,3.);
#87092=CYLINDRICAL_SURFACE('',#95098,1.875);
#87093=CYLINDRICAL_SURFACE('',#95100,3.);
#87094=CYLINDRICAL_SURFACE('',#95102,1.875);
#87095=CYLINDRICAL_SURFACE('',#95104,3.);
#87096=CYLINDRICAL_SURFACE('',#95106,1.875);
#87097=CYLINDRICAL_SURFACE('',#95108,3.);
#87098=CYLINDRICAL_SURFACE('',#95110,1.875);
#87099=CYLINDRICAL_SURFACE('',#95112,3.);
#87100=CYLINDRICAL_SURFACE('',#95114,1.875);
#87101=CYLINDRICAL_SURFACE('',#95116,3.);
#87102=CYLINDRICAL_SURFACE('',#95125,17.5);
#87103=CYLINDRICAL_SURFACE('',#95128,17.5);
#87104=CYLINDRICAL_SURFACE('',#95134,17.5);
#87105=CYLINDRICAL_SURFACE('',#95142,17.5);
#87106=CYLINDRICAL_SURFACE('',#95150,17.5);
#87107=CYLINDRICAL_SURFACE('',#95158,17.5);
#87108=CYLINDRICAL_SURFACE('',#95166,17.5);
#87109=CYLINDRICAL_SURFACE('',#95174,17.5);
#87110=CYLINDRICAL_SURFACE('',#95182,17.5);
#87111=CYLINDRICAL_SURFACE('',#95190,17.5);
#87112=CYLINDRICAL_SURFACE('',#95198,17.5);
#87113=CYLINDRICAL_SURFACE('',#95206,17.5);
#87114=CYLINDRICAL_SURFACE('',#95214,17.5);
#87115=CYLINDRICAL_SURFACE('',#95222,17.5);
#87116=CYLINDRICAL_SURFACE('',#95230,3.49999999943895);
#87117=CYLINDRICAL_SURFACE('',#95231,17.5);
#87118=CYLINDRICAL_SURFACE('',#95239,17.5);
#87119=CYLINDRICAL_SURFACE('',#95240,1.5);
#87120=CYLINDRICAL_SURFACE('',#95271,2.);
#87121=CYLINDRICAL_SURFACE('',#95287,3.);
#87122=CYLINDRICAL_SURFACE('',#95296,5.);
#87123=CYLINDRICAL_SURFACE('',#95311,0.4);
#87124=CYLINDRICAL_SURFACE('',#95322,0.4);
#87125=CYLINDRICAL_SURFACE('',#95324,4.75);
#87126=CYLINDRICAL_SURFACE('',#95326,0.4);
#87127=CYLINDRICAL_SURFACE('',#95328,2.9);
#87128=CYLINDRICAL_SURFACE('',#95330,0.4);
#87129=CYLINDRICAL_SURFACE('',#95332,4.75);
#87130=CYLINDRICAL_SURFACE('',#95342,0.4);
#87131=CYLINDRICAL_SURFACE('',#95369,0.4);
#87132=CYLINDRICAL_SURFACE('',#95373,12.);
#87133=CYLINDRICAL_SURFACE('',#95377,0.8);
#87134=CYLINDRICAL_SURFACE('',#95380,0.8);
#87135=CYLINDRICAL_SURFACE('',#95384,0.4);
#87136=CYLINDRICAL_SURFACE('',#95397,0.4);
#87137=CYLINDRICAL_SURFACE('',#95402,0.4);
#87138=CYLINDRICAL_SURFACE('',#95408,0.4);
#87139=CYLINDRICAL_SURFACE('',#95428,0.8);
#87140=CYLINDRICAL_SURFACE('',#95430,13.2);
#87141=CYLINDRICAL_SURFACE('',#95432,0.6);
#87142=CYLINDRICAL_SURFACE('',#95434,3.15);
#87143=CYLINDRICAL_SURFACE('',#95441,0.8);
#87144=CYLINDRICAL_SURFACE('',#95453,0.4);
#87145=CYLINDRICAL_SURFACE('',#95458,0.4);
#87146=CYLINDRICAL_SURFACE('',#95470,0.4);
#87147=CYLINDRICAL_SURFACE('',#95480,0.6);
#87148=CYLINDRICAL_SURFACE('',#95484,0.6);
#87149=CYLINDRICAL_SURFACE('',#95486,0.6);
#87150=CYLINDRICAL_SURFACE('',#95488,9.70000001490116);
#87151=CYLINDRICAL_SURFACE('',#95491,0.4);
#87152=CYLINDRICAL_SURFACE('',#95512,0.4);
#87153=CYLINDRICAL_SURFACE('',#95521,0.4);
#87154=CYLINDRICAL_SURFACE('',#95526,5.40000000000001);
#87155=CYLINDRICAL_SURFACE('',#95528,0.6);
#87156=CYLINDRICAL_SURFACE('',#95531,0.6);
#87157=CYLINDRICAL_SURFACE('',#95554,0.4);
#87158=CYLINDRICAL_SURFACE('',#95560,0.4);
#87159=CYLINDRICAL_SURFACE('',#95565,0.4);
#87160=CYLINDRICAL_SURFACE('',#95577,0.4);
#87161=CYLINDRICAL_SURFACE('',#95578,0.8);
#87162=CYLINDRICAL_SURFACE('',#95581,0.6);
#87163=CYLINDRICAL_SURFACE('',#95583,3.1);
#87164=CYLINDRICAL_SURFACE('',#95585,0.800000000000001);
#87165=CYLINDRICAL_SURFACE('',#95588,4.8);
#87166=CYLINDRICAL_SURFACE('',#95617,0.4);
#87167=CYLINDRICAL_SURFACE('',#95621,17.3949617393671);
#87168=CYLINDRICAL_SURFACE('',#95623,0.8);
#87169=CYLINDRICAL_SURFACE('',#95626,0.8);
#87170=CYLINDRICAL_SURFACE('',#95628,9.3949617393671);
#87171=CYLINDRICAL_SURFACE('',#95654,0.4);
#87172=CYLINDRICAL_SURFACE('',#95659,0.4);
#87173=CYLINDRICAL_SURFACE('',#95664,0.4);
#87174=CYLINDRICAL_SURFACE('',#95682,0.8);
#87175=CYLINDRICAL_SURFACE('',#95685,0.8);
#87176=CYLINDRICAL_SURFACE('',#95687,18.9949617393671);
#87177=CYLINDRICAL_SURFACE('',#95689,0.6);
#87178=CYLINDRICAL_SURFACE('',#95691,9.7);
#87179=CYLINDRICAL_SURFACE('',#95693,0.6);
#87180=CYLINDRICAL_SURFACE('',#95695,3.6);
#87181=CYLINDRICAL_SURFACE('',#95711,0.4);
#87182=CYLINDRICAL_SURFACE('',#95729,12.);
#87183=CYLINDRICAL_SURFACE('',#95733,0.8);
#87184=CYLINDRICAL_SURFACE('',#95735,10.0999999997296);
#87185=CYLINDRICAL_SURFACE('',#95737,0.8);
#87186=CYLINDRICAL_SURFACE('',#95739,4.65);
#87187=CYLINDRICAL_SURFACE('',#95742,0.4);
#87188=CYLINDRICAL_SURFACE('',#95748,0.4);
#87189=CYLINDRICAL_SURFACE('',#95766,0.6);
#87190=CYLINDRICAL_SURFACE('',#95768,13.2);
#87191=CYLINDRICAL_SURFACE('',#95770,0.6);
#87192=CYLINDRICAL_SURFACE('',#95776,0.4);
#87193=CYLINDRICAL_SURFACE('',#95778,8.5);
#87194=CYLINDRICAL_SURFACE('',#95788,0.4);
#87195=CYLINDRICAL_SURFACE('',#95796,0.8);
#87196=CYLINDRICAL_SURFACE('',#95815,4.2);
#87197=CYLINDRICAL_SURFACE('',#95837,0.8);
#87198=CYLINDRICAL_SURFACE('',#95859,0.8);
#87199=CYLINDRICAL_SURFACE('',#95861,0.8);
#87200=CYLINDRICAL_SURFACE('',#95863,0.8);
#87201=CYLINDRICAL_SURFACE('',#95875,0.8);
#87202=CYLINDRICAL_SURFACE('',#95878,0.8);
#87203=CYLINDRICAL_SURFACE('',#95892,0.8);
#87204=CYLINDRICAL_SURFACE('',#95893,0.8);
#87205=CYLINDRICAL_SURFACE('',#95896,5.4);
#87206=CYLINDRICAL_SURFACE('',#95897,7.99496173936711);
#87207=CYLINDRICAL_SURFACE('',#95898,0.8);
#87208=CYLINDRICAL_SURFACE('',#95900,0.8);
#87209=CYLINDRICAL_SURFACE('',#95902,0.6);
#87210=CYLINDRICAL_SURFACE('',#95904,9.7);
#87211=CYLINDRICAL_SURFACE('',#95906,0.6);
#87212=CYLINDRICAL_SURFACE('',#95908,23.7449617393671);
#87213=CYLINDRICAL_SURFACE('',#95910,0.4);
#87214=CYLINDRICAL_SURFACE('',#95912,7.8);
#87215=CYLINDRICAL_SURFACE('',#95914,0.8);
#87216=CYLINDRICAL_SURFACE('',#95916,0.6);
#87217=CYLINDRICAL_SURFACE('',#95921,3.2);
#87218=CYLINDRICAL_SURFACE('',#95922,0.8);
#87219=CYLINDRICAL_SURFACE('',#95924,0.8);
#87220=CYLINDRICAL_SURFACE('',#95926,0.8);
#87221=CYLINDRICAL_SURFACE('',#95927,0.8);
#87222=CYLINDRICAL_SURFACE('',#95928,10.0999999997296);
#87223=CYLINDRICAL_SURFACE('',#95929,0.8);
#87224=CYLINDRICAL_SURFACE('',#95930,0.8);
#87225=CYLINDRICAL_SURFACE('',#95931,4.65);
#87226=CYLINDRICAL_SURFACE('',#95937,3.60000000004514);
#87227=CYLINDRICAL_SURFACE('',#95942,0.6);
#87228=CYLINDRICAL_SURFACE('',#95943,0.6);
#87229=CYLINDRICAL_SURFACE('',#95944,0.6);
#87230=CYLINDRICAL_SURFACE('',#95947,3.43614417320658);
#87231=CYLINDRICAL_SURFACE('',#95949,10.45);
#87232=CYLINDRICAL_SURFACE('',#95953,0.6);
#87233=CYLINDRICAL_SURFACE('',#95954,100.);
#87234=CYLINDRICAL_SURFACE('',#95956,0.8);
#87235=CYLINDRICAL_SURFACE('',#95959,0.6);
#87236=CYLINDRICAL_SURFACE('',#95961,3.6);
#87237=CYLINDRICAL_SURFACE('',#95963,0.6);
#87238=CYLINDRICAL_SURFACE('',#95964,3.7);
#87239=CYLINDRICAL_SURFACE('',#95965,3.6);
#87240=CYLINDRICAL_SURFACE('',#95967,0.6);
#87241=CYLINDRICAL_SURFACE('',#95969,0.6);
#87242=CYLINDRICAL_SURFACE('',#95970,3.2);
#87243=CYLINDRICAL_SURFACE('',#95971,0.8);
#87244=CYLINDRICAL_SURFACE('',#95972,13.4);
#87245=CYLINDRICAL_SURFACE('',#95974,0.8);
#87246=CYLINDRICAL_SURFACE('',#95975,0.6);
#87247=CYLINDRICAL_SURFACE('',#95977,0.6);
#87248=CYLINDRICAL_SURFACE('',#95978,9.70000001490116);
#87249=CYLINDRICAL_SURFACE('',#95979,0.6);
#87250=CYLINDRICAL_SURFACE('',#95980,0.79999999999745);
#87251=CYLINDRICAL_SURFACE('',#95991,4.);
#87252=CYLINDRICAL_SURFACE('',#95992,3.75);
#87253=CYLINDRICAL_SURFACE('',#95994,0.4);
#87254=CYLINDRICAL_SURFACE('',#95996,0.8);
#87255=CYLINDRICAL_SURFACE('',#96000,1.6);
#87256=CYLINDRICAL_SURFACE('',#96004,1.55);
#87257=CYLINDRICAL_SURFACE('',#96005,3.25);
#87258=CYLINDRICAL_SURFACE('',#96008,3.25);
#87259=CYLINDRICAL_SURFACE('',#96010,1.6);
#87260=CYLINDRICAL_SURFACE('',#96013,1.6);
#87261=CYLINDRICAL_SURFACE('',#96018,3.05);
#87262=CYLINDRICAL_SURFACE('',#96019,2.);
#87263=CYLINDRICAL_SURFACE('',#96021,1.58);
#87264=CYLINDRICAL_SURFACE('',#96023,2.);
#87265=CYLINDRICAL_SURFACE('',#96026,10.9);
#87266=CYLINDRICAL_SURFACE('',#96028,4.);
#87267=CYLINDRICAL_SURFACE('',#96029,1.);
#87268=CYLINDRICAL_SURFACE('',#96035,1.6);
#87269=CYLINDRICAL_SURFACE('',#96036,1.55);
#87270=CYLINDRICAL_SURFACE('',#96038,0.4);
#87271=CYLINDRICAL_SURFACE('',#96040,1.);
#87272=CYLINDRICAL_SURFACE('',#96042,2.);
#87273=CYLINDRICAL_SURFACE('',#96045,3.3);
#87274=CYLINDRICAL_SURFACE('',#96050,6.4499999999938);
#87275=CYLINDRICAL_SURFACE('',#96051,11.65);
#87276=CYLINDRICAL_SURFACE('',#96052,0.8);
#87277=CYLINDRICAL_SURFACE('',#96067,5.);
#87278=CYLINDRICAL_SURFACE('',#96069,0.8);
#87279=CYLINDRICAL_SURFACE('',#96080,0.4);
#87280=CYLINDRICAL_SURFACE('',#96085,0.4);
#87281=CYLINDRICAL_SURFACE('',#96096,0.8);
#87282=CYLINDRICAL_SURFACE('',#96098,10.6);
#87283=CYLINDRICAL_SURFACE('',#96100,0.6);
#87284=CYLINDRICAL_SURFACE('',#96102,4.65);
#87285=CYLINDRICAL_SURFACE('',#96114,0.4);
#87286=CYLINDRICAL_SURFACE('',#96129,0.4);
#87287=CYLINDRICAL_SURFACE('',#96130,4.);
#87288=CYLINDRICAL_SURFACE('',#96132,9.3949617393671);
#87289=CYLINDRICAL_SURFACE('',#96135,17.3949617393671);
#87290=CYLINDRICAL_SURFACE('',#96149,11.55);
#87291=CYLINDRICAL_SURFACE('',#96151,0.599999999999999);
#87292=CYLINDRICAL_SURFACE('',#96152,3.8);
#87293=CYLINDRICAL_SURFACE('',#96155,0.4);
#87294=CYLINDRICAL_SURFACE('',#96164,0.4);
#87295=CYLINDRICAL_SURFACE('',#96169,0.6);
#87296=CYLINDRICAL_SURFACE('',#96172,0.4);
#87297=CYLINDRICAL_SURFACE('',#96174,0.4);
#87298=CYLINDRICAL_SURFACE('',#96192,0.4);
#87299=CYLINDRICAL_SURFACE('',#96194,0.4);
#87300=CYLINDRICAL_SURFACE('',#96198,3.8);
#87301=CYLINDRICAL_SURFACE('',#96218,0.4);
#87302=CYLINDRICAL_SURFACE('',#96222,0.4);
#87303=CYLINDRICAL_SURFACE('',#96226,0.4);
#87304=CYLINDRICAL_SURFACE('',#96232,0.600000000000001);
#87305=CYLINDRICAL_SURFACE('',#96234,3.6);
#87306=CYLINDRICAL_SURFACE('',#96236,3.7);
#87307=CYLINDRICAL_SURFACE('',#96239,0.6);
#87308=CYLINDRICAL_SURFACE('',#96242,0.6);
#87309=CYLINDRICAL_SURFACE('',#96245,0.6);
#87310=CYLINDRICAL_SURFACE('',#96247,9.2);
#87311=CYLINDRICAL_SURFACE('',#96261,0.4);
#87312=CYLINDRICAL_SURFACE('',#96267,0.4);
#87313=CYLINDRICAL_SURFACE('',#96284,0.4);
#87314=CYLINDRICAL_SURFACE('',#96292,0.8);
#87315=CYLINDRICAL_SURFACE('',#96295,0.8);
#87316=CYLINDRICAL_SURFACE('',#96297,7.69496173936711);
#87317=CYLINDRICAL_SURFACE('',#96299,5.7);
#87318=CYLINDRICAL_SURFACE('',#96302,0.4);
#87319=CYLINDRICAL_SURFACE('',#96308,0.4);
#87320=CYLINDRICAL_SURFACE('',#96317,0.4);
#87321=CYLINDRICAL_SURFACE('',#96333,0.4);
#87322=CYLINDRICAL_SURFACE('',#96337,0.6);
#87323=CYLINDRICAL_SURFACE('',#96339,19.0949617393671);
#87324=CYLINDRICAL_SURFACE('',#96341,0.8);
#87325=CYLINDRICAL_SURFACE('',#96344,0.8);
#87326=CYLINDRICAL_SURFACE('',#96348,0.4);
#87327=CYLINDRICAL_SURFACE('',#96354,0.4);
#87328=CYLINDRICAL_SURFACE('',#96359,0.4);
#87329=CYLINDRICAL_SURFACE('',#96382,6.6);
#87330=CYLINDRICAL_SURFACE('',#96384,0.6);
#87331=CYLINDRICAL_SURFACE('',#96386,22.5949617393671);
#87332=CYLINDRICAL_SURFACE('',#96389,9.2);
#87333=CYLINDRICAL_SURFACE('',#96393,0.6);
#87334=CYLINDRICAL_SURFACE('',#96411,0.4);
#87335=CYLINDRICAL_SURFACE('',#96413,0.4);
#87336=CYLINDRICAL_SURFACE('',#96415,0.6);
#87337=CYLINDRICAL_SURFACE('',#96421,3.7);
#87338=CYLINDRICAL_SURFACE('',#96423,11.65);
#87339=CYLINDRICAL_SURFACE('',#96426,0.4);
#87340=CYLINDRICAL_SURFACE('',#96433,0.4);
#87341=CYLINDRICAL_SURFACE('',#96445,0.4);
#87342=CYLINDRICAL_SURFACE('',#96458,0.4);
#87343=CYLINDRICAL_SURFACE('',#96462,0.6);
#87344=CYLINDRICAL_SURFACE('',#96464,3.5);
#87345=CYLINDRICAL_SURFACE('',#96471,0.6);
#87346=CYLINDRICAL_SURFACE('',#96474,0.800000000000001);
#87347=CYLINDRICAL_SURFACE('',#96485,0.4);
#87348=CYLINDRICAL_SURFACE('',#96490,0.4);
#87349=CYLINDRICAL_SURFACE('',#96501,0.4);
#87350=CYLINDRICAL_SURFACE('',#96513,0.6);
#87351=CYLINDRICAL_SURFACE('',#96516,9.2);
#87352=CYLINDRICAL_SURFACE('',#96533,0.4);
#87353=CYLINDRICAL_SURFACE('',#96544,0.4);
#87354=CYLINDRICAL_SURFACE('',#96549,0.4);
#87355=CYLINDRICAL_SURFACE('',#96554,0.6);
#87356=CYLINDRICAL_SURFACE('',#96557,0.6);
#87357=CYLINDRICAL_SURFACE('',#96559,9.2);
#87358=CYLINDRICAL_SURFACE('',#96566,0.8);
#87359=CYLINDRICAL_SURFACE('',#96569,0.6);
#87360=CYLINDRICAL_SURFACE('',#96571,0.6);
#87361=CYLINDRICAL_SURFACE('',#96573,3.2);
#87362=CYLINDRICAL_SURFACE('',#96575,0.399999999999999);
#87363=CYLINDRICAL_SURFACE('',#96580,0.4);
#87364=CYLINDRICAL_SURFACE('',#96583,0.6);
#87365=CYLINDRICAL_SURFACE('',#96585,0.8);
#87366=CYLINDRICAL_SURFACE('',#96588,0.8);
#87367=CYLINDRICAL_SURFACE('',#96591,3.43614417320659);
#87368=CYLINDRICAL_SURFACE('',#96595,3.60000000004514);
#87369=CYLINDRICAL_SURFACE('',#96601,1.6);
#87370=CYLINDRICAL_SURFACE('',#96603,2.8);
#87371=CYLINDRICAL_SURFACE('',#96606,0.4);
#87372=CYLINDRICAL_SURFACE('',#96608,4.2);
#87373=CYLINDRICAL_SURFACE('',#96610,0.800000000000001);
#87374=CYLINDRICAL_SURFACE('',#96612,0.4);
#87375=CYLINDRICAL_SURFACE('',#96615,0.8);
#87376=CYLINDRICAL_SURFACE('',#96619,0.6);
#87377=CYLINDRICAL_SURFACE('',#96622,4.);
#87378=CYLINDRICAL_SURFACE('',#96625,0.8);
#87379=CYLINDRICAL_SURFACE('',#96628,4.2);
#87380=CYLINDRICAL_SURFACE('',#96631,1.55);
#87381=CYLINDRICAL_SURFACE('',#96634,0.4);
#87382=CYLINDRICAL_SURFACE('',#96637,0.75);
#87383=CYLINDRICAL_SURFACE('',#96640,2.5);
#87384=CYLINDRICAL_SURFACE('',#96641,2.5);
#87385=CYLINDRICAL_SURFACE('',#96642,1.3);
#87386=CYLINDRICAL_SURFACE('',#96649,1.3);
#87387=CYLINDRICAL_SURFACE('',#96664,2.5);
#87388=CYLINDRICAL_SURFACE('',#96669,2.5);
#87389=CYLINDRICAL_SURFACE('',#96676,2.5);
#87390=CYLINDRICAL_SURFACE('',#96681,2.5);
#87391=CYLINDRICAL_SURFACE('',#96684,1.3);
#87392=CYLINDRICAL_SURFACE('',#96690,1.3);
#87393=CYLINDRICAL_SURFACE('',#96697,3.6);
#87394=CYLINDRICAL_SURFACE('',#96700,0.6);
#87395=CYLINDRICAL_SURFACE('',#96705,3.6);
#87396=CYLINDRICAL_SURFACE('',#96710,2.);
#87397=CYLINDRICAL_SURFACE('',#96715,0.6);
#87398=CYLINDRICAL_SURFACE('',#96719,3.7);
#87399=CYLINDRICAL_SURFACE('',#96720,0.6);
#87400=CYLINDRICAL_SURFACE('',#96726,0.6);
#87401=CYLINDRICAL_SURFACE('',#96728,5.79999999999998);
#87402=CYLINDRICAL_SURFACE('',#96730,0.6);
#87403=CYLINDRICAL_SURFACE('',#96733,1.);
#87404=CYLINDRICAL_SURFACE('',#96735,11.55);
#87405=CYLINDRICAL_SURFACE('',#96737,0.6);
#87406=CYLINDRICAL_SURFACE('',#96740,10.45);
#87407=CYLINDRICAL_SURFACE('',#96745,10.35);
#87408=CYLINDRICAL_SURFACE('',#96749,1.);
#87409=CYLINDRICAL_SURFACE('',#96750,1.);
#87410=CYLINDRICAL_SURFACE('',#96751,1.);
#87411=CYLINDRICAL_SURFACE('',#96754,0.6);
#87412=CYLINDRICAL_SURFACE('',#96756,0.599999999999999);
#87413=CYLINDRICAL_SURFACE('',#96761,2.8);
#87414=CYLINDRICAL_SURFACE('',#96764,3.6);
#87415=CYLINDRICAL_SURFACE('',#96767,0.4);
#87416=CYLINDRICAL_SURFACE('',#96768,24.9449617393673);
#87417=CYLINDRICAL_SURFACE('',#96769,0.6);
#87418=CYLINDRICAL_SURFACE('',#96771,6.44999999999379);
#87419=CYLINDRICAL_SURFACE('',#96773,1.);
#87420=CYLINDRICAL_SURFACE('',#96775,11.65);
#87421=CYLINDRICAL_SURFACE('',#96782,4.15);
#87422=CYLINDRICAL_SURFACE('',#96786,2.8);
#87423=CYLINDRICAL_SURFACE('',#96789,2.85);
#87424=CYLINDRICAL_SURFACE('',#96790,1.6);
#87425=CYLINDRICAL_SURFACE('',#96793,0.6);
#87426=CYLINDRICAL_SURFACE('',#96797,2.);
#87427=CYLINDRICAL_SURFACE('',#96799,0.4);
#87428=CYLINDRICAL_SURFACE('',#96802,10.35);
#87429=CYLINDRICAL_SURFACE('',#96805,0.75);
#87430=CYLINDRICAL_SURFACE('',#96808,10.);
#87431=CYLINDRICAL_SURFACE('',#96811,0.4);
#87432=CYLINDRICAL_SURFACE('',#96813,2.5);
#87433=CYLINDRICAL_SURFACE('',#96815,3.1);
#87434=CYLINDRICAL_SURFACE('',#96819,2.5);
#87435=CYLINDRICAL_SURFACE('',#96821,0.6);
#87436=CYLINDRICAL_SURFACE('',#96827,0.6);
#87437=CYLINDRICAL_SURFACE('',#96834,1.55);
#87438=CYLINDRICAL_SURFACE('',#96836,2.);
#87439=CYLINDRICAL_SURFACE('',#96843,23.7449617393671);
#87440=CYLINDRICAL_SURFACE('',#96846,1.65);
#87441=CYLINDRICAL_SURFACE('',#96862,2.1);
#87442=CYLINDRICAL_SURFACE('',#96863,5.35);
#87443=CYLINDRICAL_SURFACE('',#96867,3.3);
#87444=CYLINDRICAL_SURFACE('',#96874,2.2);
#87445=CYLINDRICAL_SURFACE('',#96877,0.75);
#87446=CYLINDRICAL_SURFACE('',#96882,0.5);
#87447=CYLINDRICAL_SURFACE('',#96887,3.2);
#87448=CYLINDRICAL_SURFACE('',#96889,0.4);
#87449=CYLINDRICAL_SURFACE('',#96894,0.4);
#87450=CYLINDRICAL_SURFACE('',#96899,0.4);
#87451=CYLINDRICAL_SURFACE('',#96903,0.4);
#87452=CYLINDRICAL_SURFACE('',#96905,2.8);
#87453=CYLINDRICAL_SURFACE('',#96907,0.6);
#87454=CYLINDRICAL_SURFACE('',#96908,24.9449617393673);
#87455=CYLINDRICAL_SURFACE('',#96911,0.6);
#87456=CYLINDRICAL_SURFACE('',#96917,0.6);
#87457=CYLINDRICAL_SURFACE('',#96919,4.1);
#87458=CYLINDRICAL_SURFACE('',#96921,0.6);
#87459=CYLINDRICAL_SURFACE('',#96924,1.);
#87460=CYLINDRICAL_SURFACE('',#96927,2.5);
#87461=CYLINDRICAL_SURFACE('',#96931,1.);
#87462=CYLINDRICAL_SURFACE('',#96940,0.6);
#87463=CYLINDRICAL_SURFACE('',#96942,0.8);
#87464=CYLINDRICAL_SURFACE('',#96945,0.8);
#87465=CYLINDRICAL_SURFACE('',#96948,0.8);
#87466=CYLINDRICAL_SURFACE('',#96952,0.8);
#87467=CYLINDRICAL_SURFACE('',#96955,0.8);
#87468=CYLINDRICAL_SURFACE('',#96961,0.8);
#87469=CYLINDRICAL_SURFACE('',#96963,0.8);
#87470=CYLINDRICAL_SURFACE('',#96965,5.25);
#87471=CYLINDRICAL_SURFACE('',#96972,0.4);
#87472=CYLINDRICAL_SURFACE('',#96974,10.45);
#87473=CYLINDRICAL_SURFACE('',#96978,0.4);
#87474=CYLINDRICAL_SURFACE('',#96981,3.05);
#87475=CYLINDRICAL_SURFACE('',#97003,0.6);
#87476=CYLINDRICAL_SURFACE('',#97005,1.);
#87477=CYLINDRICAL_SURFACE('',#97019,0.2);
#87478=CYLINDRICAL_SURFACE('',#97020,0.2);
#87479=CYLINDRICAL_SURFACE('',#97021,0.2);
#87480=CYLINDRICAL_SURFACE('',#97023,0.2);
#87481=CYLINDRICAL_SURFACE('',#97025,0.2);
#87482=CYLINDRICAL_SURFACE('',#97028,0.2);
#87483=CYLINDRICAL_SURFACE('',#97032,0.2);
#87484=CYLINDRICAL_SURFACE('',#97034,0.2);
#87485=CYLINDRICAL_SURFACE('',#97043,0.4);
#87486=CYLINDRICAL_SURFACE('',#97045,0.6);
#87487=CYLINDRICAL_SURFACE('',#97046,0.6);
#87488=CYLINDRICAL_SURFACE('',#97048,0.6);
#87489=CYLINDRICAL_SURFACE('',#97050,0.4);
#87490=CYLINDRICAL_SURFACE('',#97052,10.6);
#87491=CYLINDRICAL_SURFACE('',#97054,0.4);
#87492=CYLINDRICAL_SURFACE('',#97059,0.4);
#87493=CYLINDRICAL_SURFACE('',#97061,0.6);
#87494=CYLINDRICAL_SURFACE('',#97063,0.6);
#87495=CYLINDRICAL_SURFACE('',#97065,0.6);
#87496=CYLINDRICAL_SURFACE('',#97066,4.8);
#87497=CYLINDRICAL_SURFACE('',#97067,3.7);
#87498=CYLINDRICAL_SURFACE('',#97069,7.8);
#87499=CYLINDRICAL_SURFACE('',#97072,0.8);
#87500=CYLINDRICAL_SURFACE('',#97078,0.8);
#87501=CYLINDRICAL_SURFACE('',#97082,4.);
#87502=CYLINDRICAL_SURFACE('',#97084,1.);
#87503=CYLINDRICAL_SURFACE('',#97087,0.8);
#87504=CYLINDRICAL_SURFACE('',#97132,8.);
#87505=CYLINDRICAL_SURFACE('',#97133,4.);
#87506=CYLINDRICAL_SURFACE('',#97135,10.25);
#87507=CYLINDRICAL_SURFACE('',#97141,1.);
#87508=CYLINDRICAL_SURFACE('',#97150,1.);
#87509=CYLINDRICAL_SURFACE('',#97154,1.7);
#87510=CYLINDRICAL_SURFACE('',#97163,3.2);
#87511=CYLINDRICAL_SURFACE('',#97166,3.2);
#87512=CYLINDRICAL_SURFACE('',#97172,1.7);
#87513=CYLINDRICAL_SURFACE('',#97197,8.);
#87514=CYLINDRICAL_SURFACE('',#97198,3.);
#87515=CYLINDRICAL_SURFACE('',#97200,3.);
#87516=CYLINDRICAL_SURFACE('',#97213,5.);
#87517=CYLINDRICAL_SURFACE('',#97214,5.);
#87518=CYLINDRICAL_SURFACE('',#97215,3.);
#87519=CYLINDRICAL_SURFACE('',#97216,1.5);
#87520=CYLINDRICAL_SURFACE('',#97217,3.);
#87521=CYLINDRICAL_SURFACE('',#97220,1.6);
#87522=CYLINDRICAL_SURFACE('',#97221,1.5);
#87523=CYLINDRICAL_SURFACE('',#97222,4.);
#87524=CYLINDRICAL_SURFACE('',#97227,1.5);
#87525=CYLINDRICAL_SURFACE('',#97237,1.5);
#87526=CYLINDRICAL_SURFACE('',#97483,1.5);
#87527=CYLINDRICAL_SURFACE('',#97484,1.5);
#87528=CYLINDRICAL_SURFACE('',#97487,9.);
#87529=CYLINDRICAL_SURFACE('',#97488,3.5);
#87530=CYLINDRICAL_SURFACE('',#97490,2.5);
#87531=CYLINDRICAL_SURFACE('',#97844,1.);
#87532=CYLINDRICAL_SURFACE('',#97847,1.);
#87533=CYLINDRICAL_SURFACE('',#97897,0.4);
#87534=CYLINDRICAL_SURFACE('',#97900,0.4);
#87535=CYLINDRICAL_SURFACE('',#97903,3.5);
#87536=CYLINDRICAL_SURFACE('',#97905,1.5);
#87537=CYLINDRICAL_SURFACE('',#97906,1.5);
#87538=CYLINDRICAL_SURFACE('',#97907,3.);
#87539=CYLINDRICAL_SURFACE('',#97909,3.7);
#87540=CYLINDRICAL_SURFACE('',#97912,3.7);
#87541=CYLINDRICAL_SURFACE('',#97915,3.7);
#87542=CYLINDRICAL_SURFACE('',#97918,3.7);
#87543=CYLINDRICAL_SURFACE('',#97921,1.5);
#87544=CYLINDRICAL_SURFACE('',#98077,9.75);
#87545=CYLINDRICAL_SURFACE('',#98079,9.75);
#87546=CYLINDRICAL_SURFACE('',#98081,9.75);
#87547=CYLINDRICAL_SURFACE('',#98083,9.75);
#87548=CYLINDRICAL_SURFACE('',#98085,9.75);
#87549=CYLINDRICAL_SURFACE('',#98087,9.75);
#87550=CYLINDRICAL_SURFACE('',#98089,9.75);
#87551=CYLINDRICAL_SURFACE('',#98091,9.75);
#87552=CYLINDRICAL_SURFACE('',#98093,9.75);
#87553=CYLINDRICAL_SURFACE('',#98095,9.75);
#87554=CYLINDRICAL_SURFACE('',#98097,9.75);
#87555=CYLINDRICAL_SURFACE('',#98099,9.75);
#87556=CYLINDRICAL_SURFACE('',#98101,9.75);
#87557=CYLINDRICAL_SURFACE('',#98103,9.75);
#87558=CYLINDRICAL_SURFACE('',#98105,9.75);
#87559=CYLINDRICAL_SURFACE('',#98107,9.75);
#87560=CYLINDRICAL_SURFACE('',#98109,9.75);
#87561=CYLINDRICAL_SURFACE('',#98111,9.75);
#87562=CYLINDRICAL_SURFACE('',#98113,9.75);
#87563=CYLINDRICAL_SURFACE('',#98115,9.75);
#87564=CYLINDRICAL_SURFACE('',#98117,9.75);
#87565=CYLINDRICAL_SURFACE('',#98119,9.75);
#87566=CYLINDRICAL_SURFACE('',#98121,9.75);
#87567=CYLINDRICAL_SURFACE('',#98123,9.75);
#87568=CYLINDRICAL_SURFACE('',#98125,9.75);
#87569=CYLINDRICAL_SURFACE('',#98127,9.75);
#87570=CYLINDRICAL_SURFACE('',#98129,9.75);
#87571=CYLINDRICAL_SURFACE('',#98131,9.75);
#87572=CYLINDRICAL_SURFACE('',#98133,9.75);
#87573=CYLINDRICAL_SURFACE('',#98135,9.75);
#87574=CYLINDRICAL_SURFACE('',#98137,9.75);
#87575=CYLINDRICAL_SURFACE('',#98139,9.75);
#87576=CYLINDRICAL_SURFACE('',#98141,9.75);
#87577=CYLINDRICAL_SURFACE('',#98143,9.75);
#87578=CYLINDRICAL_SURFACE('',#98145,9.75);
#87579=CYLINDRICAL_SURFACE('',#98147,9.75);
#87580=CYLINDRICAL_SURFACE('',#98258,9.75);
#87581=CYLINDRICAL_SURFACE('',#98259,3.7);
#87582=CYLINDRICAL_SURFACE('',#98260,3.7);
#87583=CYLINDRICAL_SURFACE('',#98261,8.624);
#87584=CYLINDRICAL_SURFACE('',#98262,3.7);
#87585=CYLINDRICAL_SURFACE('',#98263,3.7);
#87586=CYLINDRICAL_SURFACE('',#98264,8.624);
#87587=CYLINDRICAL_SURFACE('',#98265,3.7);
#87588=CYLINDRICAL_SURFACE('',#98266,3.7);
#87589=CYLINDRICAL_SURFACE('',#98267,8.624);
#87590=CYLINDRICAL_SURFACE('',#98268,3.7);
#87591=CYLINDRICAL_SURFACE('',#98269,3.7);
#87592=CYLINDRICAL_SURFACE('',#98270,8.624);
#87593=CYLINDRICAL_SURFACE('',#98271,3.7);
#87594=CYLINDRICAL_SURFACE('',#98272,3.7);
#87595=CYLINDRICAL_SURFACE('',#98273,8.624);
#87596=CYLINDRICAL_SURFACE('',#98274,3.7);
#87597=CYLINDRICAL_SURFACE('',#98275,3.7);
#87598=CYLINDRICAL_SURFACE('',#98276,8.624);
#87599=CYLINDRICAL_SURFACE('',#98277,3.7);
#87600=CYLINDRICAL_SURFACE('',#98278,3.7);
#87601=CYLINDRICAL_SURFACE('',#98279,8.624);
#87602=CYLINDRICAL_SURFACE('',#98280,3.7);
#87603=CYLINDRICAL_SURFACE('',#98281,3.7);
#87604=CYLINDRICAL_SURFACE('',#98282,8.624);
#87605=CYLINDRICAL_SURFACE('',#98283,3.7);
#87606=CYLINDRICAL_SURFACE('',#98284,3.7);
#87607=CYLINDRICAL_SURFACE('',#98285,8.624);
#87608=CYLINDRICAL_SURFACE('',#98286,3.7);
#87609=CYLINDRICAL_SURFACE('',#98287,3.7);
#87610=CYLINDRICAL_SURFACE('',#98288,8.624);
#87611=CYLINDRICAL_SURFACE('',#98289,3.7);
#87612=CYLINDRICAL_SURFACE('',#98290,3.7);
#87613=CYLINDRICAL_SURFACE('',#98291,8.624);
#87614=CYLINDRICAL_SURFACE('',#98292,3.7);
#87615=CYLINDRICAL_SURFACE('',#98293,3.7);
#87616=CYLINDRICAL_SURFACE('',#98294,8.624);
#87617=CYLINDRICAL_SURFACE('',#98295,3.7);
#87618=CYLINDRICAL_SURFACE('',#98296,3.7);
#87619=CYLINDRICAL_SURFACE('',#98297,8.624);
#87620=CYLINDRICAL_SURFACE('',#98298,3.7);
#87621=CYLINDRICAL_SURFACE('',#98299,3.7);
#87622=CYLINDRICAL_SURFACE('',#98300,8.624);
#87623=CYLINDRICAL_SURFACE('',#98301,3.7);
#87624=CYLINDRICAL_SURFACE('',#98302,3.7);
#87625=CYLINDRICAL_SURFACE('',#98303,8.624);
#87626=CYLINDRICAL_SURFACE('',#98304,3.7);
#87627=CYLINDRICAL_SURFACE('',#98305,3.7);
#87628=CYLINDRICAL_SURFACE('',#98306,8.624);
#87629=CYLINDRICAL_SURFACE('',#98307,3.7);
#87630=CYLINDRICAL_SURFACE('',#98308,3.7);
#87631=CYLINDRICAL_SURFACE('',#98309,8.624);
#87632=CYLINDRICAL_SURFACE('',#98310,3.7);
#87633=CYLINDRICAL_SURFACE('',#98311,3.7);
#87634=CYLINDRICAL_SURFACE('',#98312,8.624);
#87635=CYLINDRICAL_SURFACE('',#98313,3.7);
#87636=CYLINDRICAL_SURFACE('',#98314,3.7);
#87637=CYLINDRICAL_SURFACE('',#98315,8.624);
#87638=CYLINDRICAL_SURFACE('',#98316,3.7);
#87639=CYLINDRICAL_SURFACE('',#98317,3.7);
#87640=CYLINDRICAL_SURFACE('',#98318,8.624);
#87641=CYLINDRICAL_SURFACE('',#98319,3.7);
#87642=CYLINDRICAL_SURFACE('',#98320,3.7);
#87643=CYLINDRICAL_SURFACE('',#98321,8.624);
#87644=CYLINDRICAL_SURFACE('',#98322,3.7);
#87645=CYLINDRICAL_SURFACE('',#98323,3.7);
#87646=CYLINDRICAL_SURFACE('',#98324,8.624);
#87647=CYLINDRICAL_SURFACE('',#98325,3.7);
#87648=CYLINDRICAL_SURFACE('',#98326,3.7);
#87649=CYLINDRICAL_SURFACE('',#98327,8.624);
#87650=CYLINDRICAL_SURFACE('',#98328,3.7);
#87651=CYLINDRICAL_SURFACE('',#98329,3.7);
#87652=CYLINDRICAL_SURFACE('',#98330,8.624);
#87653=CYLINDRICAL_SURFACE('',#98331,3.7);
#87654=CYLINDRICAL_SURFACE('',#98332,3.7);
#87655=CYLINDRICAL_SURFACE('',#98333,8.624);
#87656=CYLINDRICAL_SURFACE('',#98334,3.7);
#87657=CYLINDRICAL_SURFACE('',#98335,8.624);
#87658=CYLINDRICAL_SURFACE('',#98336,3.7);
#87659=CYLINDRICAL_SURFACE('',#98337,8.624);
#87660=CYLINDRICAL_SURFACE('',#98338,3.7);
#87661=CYLINDRICAL_SURFACE('',#98339,3.7);
#87662=CYLINDRICAL_SURFACE('',#98340,8.624);
#87663=CYLINDRICAL_SURFACE('',#98341,3.7);
#87664=CYLINDRICAL_SURFACE('',#98342,3.7);
#87665=CYLINDRICAL_SURFACE('',#98343,8.624);
#87666=CYLINDRICAL_SURFACE('',#98344,3.7);
#87667=CYLINDRICAL_SURFACE('',#98345,3.7);
#87668=CYLINDRICAL_SURFACE('',#98346,8.624);
#87669=CYLINDRICAL_SURFACE('',#98347,3.7);
#87670=CYLINDRICAL_SURFACE('',#98348,3.7);
#87671=CYLINDRICAL_SURFACE('',#98349,8.624);
#87672=CYLINDRICAL_SURFACE('',#98350,3.7);
#87673=CYLINDRICAL_SURFACE('',#98351,8.624);
#87674=CYLINDRICAL_SURFACE('',#98352,3.7);
#87675=CYLINDRICAL_SURFACE('',#98353,8.624);
#87676=CYLINDRICAL_SURFACE('',#98354,3.7);
#87677=CYLINDRICAL_SURFACE('',#98355,3.7);
#87678=CYLINDRICAL_SURFACE('',#98356,8.624);
#87679=CYLINDRICAL_SURFACE('',#98357,3.7);
#87680=CYLINDRICAL_SURFACE('',#98358,3.7);
#87681=CYLINDRICAL_SURFACE('',#98359,8.624);
#87682=CYLINDRICAL_SURFACE('',#98360,3.7);
#87683=CYLINDRICAL_SURFACE('',#98361,3.7);
#87684=CYLINDRICAL_SURFACE('',#98362,8.624);
#87685=CYLINDRICAL_SURFACE('',#98363,3.7);
#87686=CYLINDRICAL_SURFACE('',#98364,3.7);
#87687=CYLINDRICAL_SURFACE('',#98365,8.624);
#87688=CYLINDRICAL_SURFACE('',#98371,0.4);
#87689=CYLINDRICAL_SURFACE('',#98374,5.);
#87690=CYLINDRICAL_SURFACE('',#98377,0.4);
#87691=CYLINDRICAL_SURFACE('',#98381,0.4);
#87692=CYLINDRICAL_SURFACE('',#98383,7.2);
#87693=CYLINDRICAL_SURFACE('',#98387,0.4);
#87694=CYLINDRICAL_SURFACE('',#98391,7.2);
#87695=CYLINDRICAL_SURFACE('',#98394,0.4);
#87696=CYLINDRICAL_SURFACE('',#98397,0.4);
#87697=CYLINDRICAL_SURFACE('',#98400,5.);
#87698=CYLINDRICAL_SURFACE('',#98407,0.2);
#87699=CYLINDRICAL_SURFACE('',#98414,0.2);
#87700=CYLINDRICAL_SURFACE('',#98422,0.2);
#87701=CYLINDRICAL_SURFACE('',#98425,0.2);
#87702=CYLINDRICAL_SURFACE('',#98433,11.5);
#87703=CYLINDRICAL_SURFACE('',#98436,10.375);
#87704=CYLINDRICAL_SURFACE('',#98439,11.5);
#87705=CYLINDRICAL_SURFACE('',#98442,10.375);
#87706=CYLINDRICAL_SURFACE('',#98445,11.5);
#87707=CYLINDRICAL_SURFACE('',#98448,10.375);
#87708=CYLINDRICAL_SURFACE('',#98451,11.5);
#87709=CYLINDRICAL_SURFACE('',#98454,10.375);
#87710=CYLINDRICAL_SURFACE('',#98457,11.5);
#87711=CYLINDRICAL_SURFACE('',#98460,10.375);
#87712=CYLINDRICAL_SURFACE('',#98463,11.5);
#87713=CYLINDRICAL_SURFACE('',#98466,10.375);
#87714=CYLINDRICAL_SURFACE('',#98469,11.5);
#87715=CYLINDRICAL_SURFACE('',#98472,10.375);
#87716=CYLINDRICAL_SURFACE('',#98475,11.5);
#87717=CYLINDRICAL_SURFACE('',#98478,10.375);
#87718=CYLINDRICAL_SURFACE('',#98481,11.5);
#87719=CYLINDRICAL_SURFACE('',#98484,10.375);
#87720=CYLINDRICAL_SURFACE('',#98487,11.5);
#87721=CYLINDRICAL_SURFACE('',#98490,10.375);
#87722=CYLINDRICAL_SURFACE('',#98493,11.5);
#87723=CYLINDRICAL_SURFACE('',#98496,10.375);
#87724=CYLINDRICAL_SURFACE('',#98499,11.5);
#87725=CYLINDRICAL_SURFACE('',#98502,10.375);
#87726=CYLINDRICAL_SURFACE('',#98505,11.5);
#87727=CYLINDRICAL_SURFACE('',#98508,10.375);
#87728=CYLINDRICAL_SURFACE('',#98511,11.5);
#87729=CYLINDRICAL_SURFACE('',#98514,10.375);
#87730=CYLINDRICAL_SURFACE('',#98517,11.5);
#87731=CYLINDRICAL_SURFACE('',#98520,10.375);
#87732=CYLINDRICAL_SURFACE('',#98523,11.5);
#87733=CYLINDRICAL_SURFACE('',#98526,10.375);
#87734=CYLINDRICAL_SURFACE('',#98529,11.5);
#87735=CYLINDRICAL_SURFACE('',#98532,10.375);
#87736=CYLINDRICAL_SURFACE('',#98535,11.5);
#87737=CYLINDRICAL_SURFACE('',#98538,10.375);
#87738=CYLINDRICAL_SURFACE('',#98541,11.5);
#87739=CYLINDRICAL_SURFACE('',#98544,10.375);
#87740=CYLINDRICAL_SURFACE('',#98547,11.5);
#87741=CYLINDRICAL_SURFACE('',#98550,10.375);
#87742=CYLINDRICAL_SURFACE('',#98553,11.5);
#87743=CYLINDRICAL_SURFACE('',#98556,10.375);
#87744=CYLINDRICAL_SURFACE('',#98559,11.5);
#87745=CYLINDRICAL_SURFACE('',#98562,10.375);
#87746=CYLINDRICAL_SURFACE('',#98565,11.5);
#87747=CYLINDRICAL_SURFACE('',#98568,10.375);
#87748=CYLINDRICAL_SURFACE('',#98571,11.5);
#87749=CYLINDRICAL_SURFACE('',#98574,10.375);
#87750=CYLINDRICAL_SURFACE('',#98577,11.5);
#87751=CYLINDRICAL_SURFACE('',#98580,10.375);
#87752=CYLINDRICAL_SURFACE('',#98583,11.5);
#87753=CYLINDRICAL_SURFACE('',#98586,10.375);
#87754=CYLINDRICAL_SURFACE('',#98589,11.5);
#87755=CYLINDRICAL_SURFACE('',#98592,10.375);
#87756=CYLINDRICAL_SURFACE('',#98595,11.5);
#87757=CYLINDRICAL_SURFACE('',#98598,10.375);
#87758=CYLINDRICAL_SURFACE('',#98601,11.5);
#87759=CYLINDRICAL_SURFACE('',#98604,10.375);
#87760=CYLINDRICAL_SURFACE('',#98607,11.5);
#87761=CYLINDRICAL_SURFACE('',#98610,10.375);
#87762=CYLINDRICAL_SURFACE('',#98613,11.5);
#87763=CYLINDRICAL_SURFACE('',#98616,10.375);
#87764=CYLINDRICAL_SURFACE('',#98619,11.5);
#87765=CYLINDRICAL_SURFACE('',#98622,10.375);
#87766=CYLINDRICAL_SURFACE('',#98625,11.5);
#87767=CYLINDRICAL_SURFACE('',#98628,10.375);
#87768=CYLINDRICAL_SURFACE('',#98631,11.5);
#87769=CYLINDRICAL_SURFACE('',#98634,10.375);
#87770=CYLINDRICAL_SURFACE('',#98637,11.5);
#87771=CYLINDRICAL_SURFACE('',#98640,10.375);
#87772=CYLINDRICAL_SURFACE('',#98643,11.5);
#87773=CYLINDRICAL_SURFACE('',#98646,10.375);
#87774=CYLINDRICAL_SURFACE('',#98649,11.5);
#87775=CYLINDRICAL_SURFACE('',#98652,10.375);
#87776=CYLINDRICAL_SURFACE('',#98655,11.5);
#87777=CYLINDRICAL_SURFACE('',#98658,10.375);
#87778=CYLINDRICAL_SURFACE('',#98661,11.5);
#87779=CYLINDRICAL_SURFACE('',#98664,10.375);
#87780=CYLINDRICAL_SURFACE('',#98667,11.5);
#87781=CYLINDRICAL_SURFACE('',#98670,10.375);
#87782=CYLINDRICAL_SURFACE('',#98673,11.5);
#87783=CYLINDRICAL_SURFACE('',#98676,10.375);
#87784=CYLINDRICAL_SURFACE('',#98679,11.5);
#87785=CYLINDRICAL_SURFACE('',#98682,10.375);
#87786=CYLINDRICAL_SURFACE('',#98685,11.5);
#87787=CYLINDRICAL_SURFACE('',#98693,10.375);
#87788=CYLINDRICAL_SURFACE('',#98695,10.375);
#87789=CYLINDRICAL_SURFACE('',#98697,11.5);
#87790=CYLINDRICAL_SURFACE('',#98699,3.5);
#87791=CYLINDRICAL_SURFACE('',#98702,1.5);
#87792=CYLINDRICAL_SURFACE('',#98705,1.5);
#87793=CYLINDRICAL_SURFACE('',#98746,3.);
#87794=CYLINDRICAL_SURFACE('',#98750,4.75);
#87795=CYLINDRICAL_SURFACE('',#98753,3.625);
#87796=CYLINDRICAL_SURFACE('',#98756,4.75);
#87797=CYLINDRICAL_SURFACE('',#98759,3.625);
#87798=CYLINDRICAL_SURFACE('',#98762,4.75);
#87799=CYLINDRICAL_SURFACE('',#98765,3.625);
#87800=CYLINDRICAL_SURFACE('',#98768,4.75);
#87801=CYLINDRICAL_SURFACE('',#98771,3.625);
#87802=CYLINDRICAL_SURFACE('',#98774,4.75);
#87803=CYLINDRICAL_SURFACE('',#98777,3.625);
#87804=CYLINDRICAL_SURFACE('',#98780,4.75);
#87805=CYLINDRICAL_SURFACE('',#98783,3.625);
#87806=CYLINDRICAL_SURFACE('',#98786,4.75);
#87807=CYLINDRICAL_SURFACE('',#98789,3.625);
#87808=CYLINDRICAL_SURFACE('',#98792,4.75);
#87809=CYLINDRICAL_SURFACE('',#98795,3.625);
#87810=CYLINDRICAL_SURFACE('',#98798,4.75);
#87811=CYLINDRICAL_SURFACE('',#98820,3.625);
#87812=CYLINDRICAL_SURFACE('',#98822,4.75);
#87813=CYLINDRICAL_SURFACE('',#98824,3.625);
#87814=CYLINDRICAL_SURFACE('',#98827,4.75);
#87815=CYLINDRICAL_SURFACE('',#98830,4.75);
#87816=CYLINDRICAL_SURFACE('',#98831,3.625);
#87817=CYLINDRICAL_SURFACE('',#98833,4.75);
#87818=CYLINDRICAL_SURFACE('',#98835,3.625);
#87819=CYLINDRICAL_SURFACE('',#98836,3.625);
#87820=CYLINDRICAL_SURFACE('',#98839,4.75);
#87821=CYLINDRICAL_SURFACE('',#98842,4.75);
#87822=CYLINDRICAL_SURFACE('',#98843,3.625);
#87823=CYLINDRICAL_SURFACE('',#98845,4.75);
#87824=CYLINDRICAL_SURFACE('',#98847,3.625);
#87825=CYLINDRICAL_SURFACE('',#98848,3.625);
#87826=CYLINDRICAL_SURFACE('',#98851,4.75);
#87827=CYLINDRICAL_SURFACE('',#98852,3.625);
#87828=CYLINDRICAL_SURFACE('',#98853,3.5);
#87829=CYLINDRICAL_SURFACE('',#98863,1.6);
#87830=CYLINDRICAL_SURFACE('',#98888,2.4);
#87831=CYLINDRICAL_SURFACE('',#98918,0.525);
#87832=CYLINDRICAL_SURFACE('',#98922,0.525);
#87833=CYLINDRICAL_SURFACE('',#98926,0.525);
#87834=CYLINDRICAL_SURFACE('',#98930,0.525);
#87835=CYLINDRICAL_SURFACE('',#98934,0.525);
#87836=CYLINDRICAL_SURFACE('',#98938,0.525);
#87837=CYLINDRICAL_SURFACE('',#98942,0.525);
#87838=CYLINDRICAL_SURFACE('',#98946,0.525);
#87839=CYLINDRICAL_SURFACE('',#98950,0.525);
#87840=CYLINDRICAL_SURFACE('',#98954,0.525);
#87841=CYLINDRICAL_SURFACE('',#98958,0.525);
#87842=CYLINDRICAL_SURFACE('',#98962,0.525);
#87843=CYLINDRICAL_SURFACE('',#98966,0.525);
#87844=CYLINDRICAL_SURFACE('',#98970,0.525);
#87845=CYLINDRICAL_SURFACE('',#98974,0.525);
#87846=CYLINDRICAL_SURFACE('',#98978,0.525);
#87847=CYLINDRICAL_SURFACE('',#98982,0.5);
#87848=CYLINDRICAL_SURFACE('',#98991,0.5);
#87849=CYLINDRICAL_SURFACE('',#99000,0.5);
#87850=CYLINDRICAL_SURFACE('',#99009,0.5);
#87851=CYLINDRICAL_SURFACE('',#99018,0.5);
#87852=CYLINDRICAL_SURFACE('',#99027,0.5);
#87853=CYLINDRICAL_SURFACE('',#99036,0.5);
#87854=CYLINDRICAL_SURFACE('',#99045,0.5);
#87855=CYLINDRICAL_SURFACE('',#99053,1.17524047358084);
#87856=CYLINDRICAL_SURFACE('',#99055,1.17524047358084);
#87857=CYLINDRICAL_SURFACE('',#99056,1.17524047358084);
#87858=CYLINDRICAL_SURFACE('',#99057,1.17524047358084);
#87859=CYLINDRICAL_SURFACE('',#99058,1.17524047358084);
#87860=CYLINDRICAL_SURFACE('',#99059,1.17524047358084);
#87861=CYLINDRICAL_SURFACE('',#99060,1.17524047358084);
#87862=CYLINDRICAL_SURFACE('',#99061,1.17524047358084);
#87863=CYLINDRICAL_SURFACE('',#99062,1.17524047358084);
#87864=CYLINDRICAL_SURFACE('',#99063,1.17524047358084);
#87865=CYLINDRICAL_SURFACE('',#99064,1.17524047358084);
#87866=CYLINDRICAL_SURFACE('',#99065,1.17524047358084);
#87867=CYLINDRICAL_SURFACE('',#99066,1.17524047358084);
#87868=CYLINDRICAL_SURFACE('',#99067,1.17524047358084);
#87869=CYLINDRICAL_SURFACE('',#99068,1.17524047358084);
#87870=CYLINDRICAL_SURFACE('',#99069,1.17524047358084);
#87871=CYLINDRICAL_SURFACE('',#99070,1.17524047358084);
#87872=CYLINDRICAL_SURFACE('',#99071,1.17524047358084);
#87873=CYLINDRICAL_SURFACE('',#99072,1.17524047358084);
#87874=CYLINDRICAL_SURFACE('',#99073,1.17524047358084);
#87875=CYLINDRICAL_SURFACE('',#99074,1.17524047358084);
#87876=CYLINDRICAL_SURFACE('',#99075,1.17524047358084);
#87877=CYLINDRICAL_SURFACE('',#99076,1.17524047358084);
#87878=CYLINDRICAL_SURFACE('',#99077,1.17524047358084);
#87879=CYLINDRICAL_SURFACE('',#99078,1.17524047358084);
#87880=CYLINDRICAL_SURFACE('',#99079,1.17524047358084);
#87881=CYLINDRICAL_SURFACE('',#99080,1.17524047358084);
#87882=CYLINDRICAL_SURFACE('',#99081,1.17524047358084);
#87883=CYLINDRICAL_SURFACE('',#99082,1.17524047358084);
#87884=CYLINDRICAL_SURFACE('',#99083,1.17524047358084);
#87885=CYLINDRICAL_SURFACE('',#99084,1.17524047358084);
#87886=CYLINDRICAL_SURFACE('',#99085,1.17524047358084);
#87887=CYLINDRICAL_SURFACE('',#99087,1.5);
#87888=CYLINDRICAL_SURFACE('',#99089,1.5);
#87889=CYLINDRICAL_SURFACE('',#99090,1.5);
#87890=CYLINDRICAL_SURFACE('',#99091,1.5);
#87891=CYLINDRICAL_SURFACE('',#99092,1.5);
#87892=CYLINDRICAL_SURFACE('',#99093,1.5);
#87893=CYLINDRICAL_SURFACE('',#99094,1.5);
#87894=CYLINDRICAL_SURFACE('',#99095,1.5);
#87895=CYLINDRICAL_SURFACE('',#99096,1.5);
#87896=CYLINDRICAL_SURFACE('',#99097,1.5);
#87897=CYLINDRICAL_SURFACE('',#99098,1.5);
#87898=CYLINDRICAL_SURFACE('',#99099,1.5);
#87899=CYLINDRICAL_SURFACE('',#99100,1.5);
#87900=CYLINDRICAL_SURFACE('',#99101,1.5);
#87901=CYLINDRICAL_SURFACE('',#99102,1.5);
#87902=CYLINDRICAL_SURFACE('',#99103,1.5);
#87903=CYLINDRICAL_SURFACE('',#99104,1.5);
#87904=CYLINDRICAL_SURFACE('',#99105,1.5);
#87905=CYLINDRICAL_SURFACE('',#99106,1.5);
#87906=CYLINDRICAL_SURFACE('',#99107,1.5);
#87907=CYLINDRICAL_SURFACE('',#99108,1.5);
#87908=CYLINDRICAL_SURFACE('',#99109,1.5);
#87909=CYLINDRICAL_SURFACE('',#99110,1.5);
#87910=CYLINDRICAL_SURFACE('',#99111,1.5);
#87911=CYLINDRICAL_SURFACE('',#99112,1.5);
#87912=CYLINDRICAL_SURFACE('',#99113,1.5);
#87913=CYLINDRICAL_SURFACE('',#99114,1.5);
#87914=CYLINDRICAL_SURFACE('',#99115,1.5);
#87915=CYLINDRICAL_SURFACE('',#99116,1.5);
#87916=CYLINDRICAL_SURFACE('',#99117,1.5);
#87917=CYLINDRICAL_SURFACE('',#99118,1.5);
#87918=CYLINDRICAL_SURFACE('',#99124,3.5);
#87919=CYLINDRICAL_SURFACE('',#99131,1.5);
#87920=CYLINDRICAL_SURFACE('',#99153,1.17524047358084);
#87921=CYLINDRICAL_SURFACE('',#99172,2.40384615384615);
#87922=CYLINDRICAL_SURFACE('',#99178,2.40384615384615);
#87923=CYLINDRICAL_SURFACE('',#99183,3.);
#87924=CYLINDRICAL_SURFACE('',#99197,1.5);
#87925=CYLINDRICAL_SURFACE('',#99202,2.09615384615385);
#87926=CYLINDRICAL_SURFACE('',#99204,2.09615384615385);
#87927=CYLINDRICAL_SURFACE('',#99232,2.40384615384615);
#87928=CYLINDRICAL_SURFACE('',#99235,2.09615384615385);
#87929=CYLINDRICAL_SURFACE('',#99240,2.40384615384615);
#87930=CYLINDRICAL_SURFACE('',#99243,2.09615384615385);
#87931=CYLINDRICAL_SURFACE('',#99249,1.17524047358091);
#87932=CYLINDRICAL_SURFACE('',#99251,1.17524047358091);
#87933=CYLINDRICAL_SURFACE('',#99253,1.17524047358091);
#87934=CYLINDRICAL_SURFACE('',#99254,1.17524047358091);
#87935=CYLINDRICAL_SURFACE('',#99255,1.17524047358091);
#87936=CYLINDRICAL_SURFACE('',#99256,1.17524047358091);
#87937=CYLINDRICAL_SURFACE('',#99257,1.17524047358091);
#87938=CYLINDRICAL_SURFACE('',#99258,1.17524047358091);
#87939=CYLINDRICAL_SURFACE('',#99259,1.17524047358091);
#87940=CYLINDRICAL_SURFACE('',#99260,1.17524047358091);
#87941=CYLINDRICAL_SURFACE('',#99261,1.17524047358091);
#87942=CYLINDRICAL_SURFACE('',#99262,1.17524047358091);
#87943=CYLINDRICAL_SURFACE('',#99263,1.17524047358091);
#87944=CYLINDRICAL_SURFACE('',#99264,1.17524047358091);
#87945=CYLINDRICAL_SURFACE('',#99265,1.17524047358091);
#87946=CYLINDRICAL_SURFACE('',#99266,1.17524047358091);
#87947=CYLINDRICAL_SURFACE('',#99267,1.5);
#87948=CYLINDRICAL_SURFACE('',#99269,1.5);
#87949=CYLINDRICAL_SURFACE('',#99270,1.5);
#87950=CYLINDRICAL_SURFACE('',#99271,1.5);
#87951=CYLINDRICAL_SURFACE('',#99272,1.5);
#87952=CYLINDRICAL_SURFACE('',#99273,1.5);
#87953=CYLINDRICAL_SURFACE('',#99274,1.5);
#87954=CYLINDRICAL_SURFACE('',#99275,1.5);
#87955=CYLINDRICAL_SURFACE('',#99276,1.5);
#87956=CYLINDRICAL_SURFACE('',#99277,1.5);
#87957=CYLINDRICAL_SURFACE('',#99278,1.5);
#87958=CYLINDRICAL_SURFACE('',#99279,1.5);
#87959=CYLINDRICAL_SURFACE('',#99280,1.5);
#87960=CYLINDRICAL_SURFACE('',#99281,1.5);
#87961=CYLINDRICAL_SURFACE('',#99282,1.5);
#87962=CYLINDRICAL_SURFACE('',#99288,3.5);
#87963=CYLINDRICAL_SURFACE('',#99294,1.5);
#87964=CYLINDRICAL_SURFACE('',#99317,1.17524047358091);
#87965=CYLINDRICAL_SURFACE('',#99319,0.957716426222737);
#87966=CYLINDRICAL_SURFACE('',#99321,0.957716426222737);
#87967=CYLINDRICAL_SURFACE('',#99322,0.957716426222737);
#87968=CYLINDRICAL_SURFACE('',#99323,0.957716426222737);
#87969=CYLINDRICAL_SURFACE('',#99324,0.957716426222737);
#87970=CYLINDRICAL_SURFACE('',#99325,0.957716426222737);
#87971=CYLINDRICAL_SURFACE('',#99326,0.957716426222737);
#87972=CYLINDRICAL_SURFACE('',#99327,0.957716426222737);
#87973=CYLINDRICAL_SURFACE('',#99328,0.957716426222737);
#87974=CYLINDRICAL_SURFACE('',#99329,0.957716426222737);
#87975=CYLINDRICAL_SURFACE('',#99330,0.957716426222737);
#87976=CYLINDRICAL_SURFACE('',#99331,0.957716426222737);
#87977=CYLINDRICAL_SURFACE('',#99332,0.957716426222737);
#87978=CYLINDRICAL_SURFACE('',#99333,0.957716426222737);
#87979=CYLINDRICAL_SURFACE('',#99334,0.957716426222737);
#87980=CYLINDRICAL_SURFACE('',#99336,1.25000000000001);
#87981=CYLINDRICAL_SURFACE('',#99338,1.25000000000001);
#87982=CYLINDRICAL_SURFACE('',#99339,1.25000000000001);
#87983=CYLINDRICAL_SURFACE('',#99340,1.25000000000001);
#87984=CYLINDRICAL_SURFACE('',#99341,1.25000000000001);
#87985=CYLINDRICAL_SURFACE('',#99342,1.25000000000001);
#87986=CYLINDRICAL_SURFACE('',#99343,1.25000000000001);
#87987=CYLINDRICAL_SURFACE('',#99344,1.25000000000001);
#87988=CYLINDRICAL_SURFACE('',#99345,1.25000000000001);
#87989=CYLINDRICAL_SURFACE('',#99346,1.25000000000001);
#87990=CYLINDRICAL_SURFACE('',#99347,1.25000000000001);
#87991=CYLINDRICAL_SURFACE('',#99348,1.25000000000001);
#87992=CYLINDRICAL_SURFACE('',#99349,1.25000000000001);
#87993=CYLINDRICAL_SURFACE('',#99350,1.25000000000001);
#87994=CYLINDRICAL_SURFACE('',#99354,1.25000000000001);
#87995=CYLINDRICAL_SURFACE('',#99358,2.5);
#87996=CYLINDRICAL_SURFACE('',#99384,0.957716426222737);
#87997=CYLINDRICAL_SURFACE('',#99386,1.17524047358083);
#87998=CYLINDRICAL_SURFACE('',#99388,1.17524047358083);
#87999=CYLINDRICAL_SURFACE('',#99389,1.17524047358083);
#88000=CYLINDRICAL_SURFACE('',#99390,1.17524047358083);
#88001=CYLINDRICAL_SURFACE('',#99391,1.17524047358083);
#88002=CYLINDRICAL_SURFACE('',#99392,1.17524047358083);
#88003=CYLINDRICAL_SURFACE('',#99393,1.17524047358083);
#88004=CYLINDRICAL_SURFACE('',#99394,1.17524047358083);
#88005=CYLINDRICAL_SURFACE('',#99395,1.17524047358083);
#88006=CYLINDRICAL_SURFACE('',#99396,1.17524047358083);
#88007=CYLINDRICAL_SURFACE('',#99397,1.17524047358083);
#88008=CYLINDRICAL_SURFACE('',#99398,1.17524047358083);
#88009=CYLINDRICAL_SURFACE('',#99399,1.17524047358083);
#88010=CYLINDRICAL_SURFACE('',#99400,1.17524047358083);
#88011=CYLINDRICAL_SURFACE('',#99401,1.17524047358083);
#88012=CYLINDRICAL_SURFACE('',#99402,1.17524047358083);
#88013=CYLINDRICAL_SURFACE('',#99403,1.17524047358083);
#88014=CYLINDRICAL_SURFACE('',#99404,1.17524047358083);
#88015=CYLINDRICAL_SURFACE('',#99405,1.17524047358083);
#88016=CYLINDRICAL_SURFACE('',#99406,1.17524047358083);
#88017=CYLINDRICAL_SURFACE('',#99407,1.17524047358083);
#88018=CYLINDRICAL_SURFACE('',#99408,1.17524047358083);
#88019=CYLINDRICAL_SURFACE('',#99409,1.17524047358083);
#88020=CYLINDRICAL_SURFACE('',#99410,1.17524047358083);
#88021=CYLINDRICAL_SURFACE('',#99411,1.17524047358083);
#88022=CYLINDRICAL_SURFACE('',#99412,1.17524047358083);
#88023=CYLINDRICAL_SURFACE('',#99413,1.17524047358083);
#88024=CYLINDRICAL_SURFACE('',#99414,1.17524047358083);
#88025=CYLINDRICAL_SURFACE('',#99415,1.17524047358083);
#88026=CYLINDRICAL_SURFACE('',#99416,1.5);
#88027=CYLINDRICAL_SURFACE('',#99420,1.5);
#88028=CYLINDRICAL_SURFACE('',#99421,1.5);
#88029=CYLINDRICAL_SURFACE('',#99422,1.5);
#88030=CYLINDRICAL_SURFACE('',#99423,1.5);
#88031=CYLINDRICAL_SURFACE('',#99424,1.5);
#88032=CYLINDRICAL_SURFACE('',#99425,1.5);
#88033=CYLINDRICAL_SURFACE('',#99426,1.5);
#88034=CYLINDRICAL_SURFACE('',#99427,1.5);
#88035=CYLINDRICAL_SURFACE('',#99428,1.5);
#88036=CYLINDRICAL_SURFACE('',#99429,1.5);
#88037=CYLINDRICAL_SURFACE('',#99430,1.5);
#88038=CYLINDRICAL_SURFACE('',#99431,1.5);
#88039=CYLINDRICAL_SURFACE('',#99432,1.5);
#88040=CYLINDRICAL_SURFACE('',#99433,1.5);
#88041=CYLINDRICAL_SURFACE('',#99434,1.5);
#88042=CYLINDRICAL_SURFACE('',#99435,1.5);
#88043=CYLINDRICAL_SURFACE('',#99436,1.5);
#88044=CYLINDRICAL_SURFACE('',#99437,1.5);
#88045=CYLINDRICAL_SURFACE('',#99438,1.5);
#88046=CYLINDRICAL_SURFACE('',#99439,1.5);
#88047=CYLINDRICAL_SURFACE('',#99440,1.5);
#88048=CYLINDRICAL_SURFACE('',#99441,1.5);
#88049=CYLINDRICAL_SURFACE('',#99442,1.5);
#88050=CYLINDRICAL_SURFACE('',#99443,1.5);
#88051=CYLINDRICAL_SURFACE('',#99444,1.5);
#88052=CYLINDRICAL_SURFACE('',#99445,1.5);
#88053=CYLINDRICAL_SURFACE('',#99446,1.5);
#88054=CYLINDRICAL_SURFACE('',#99455,1.5);
#88055=CYLINDRICAL_SURFACE('',#99680,2.75);
#88056=CYLINDRICAL_SURFACE('',#100365,0.00687499999999997);
#88057=CYLINDRICAL_SURFACE('',#100399,1.17524047358083);
#88058=CYLINDRICAL_SURFACE('',#100403,0.0125);
#88059=CYLINDRICAL_SURFACE('',#100414,0.0125);
#88060=CYLINDRICAL_SURFACE('',#100421,0.00687499999999996);
#88061=CYLINDRICAL_SURFACE('',#100430,0.0125);
#88062=CYLINDRICAL_SURFACE('',#100437,0.0125);
#88063=CYLINDRICAL_SURFACE('',#100444,0.00687499999999999);
#88064=CYLINDRICAL_SURFACE('',#100453,0.0125);
#88065=CYLINDRICAL_SURFACE('',#100460,0.0125);
#88066=CYLINDRICAL_SURFACE('',#100467,0.00687499999999993);
#88067=CYLINDRICAL_SURFACE('',#100476,0.0125);
#88068=CYLINDRICAL_SURFACE('',#100483,0.0125);
#88069=CYLINDRICAL_SURFACE('',#100490,0.00687499999999995);
#88070=CYLINDRICAL_SURFACE('',#100499,0.0125);
#88071=CYLINDRICAL_SURFACE('',#100506,0.0125);
#88072=CYLINDRICAL_SURFACE('',#100513,0.00687499999999998);
#88073=CYLINDRICAL_SURFACE('',#100522,0.0125000000000001);
#88074=CYLINDRICAL_SURFACE('',#100529,0.0125000000000001);
#88075=CYLINDRICAL_SURFACE('',#100536,0.00687499999999991);
#88076=CYLINDRICAL_SURFACE('',#100545,0.0125);
#88077=CYLINDRICAL_SURFACE('',#100552,0.0125);
#88078=CYLINDRICAL_SURFACE('',#100559,0.00687500000000009);
#88079=CYLINDRICAL_SURFACE('',#100568,0.0125);
#88080=CYLINDRICAL_SURFACE('',#100575,0.0124999999999999);
#88081=CYLINDRICAL_SURFACE('',#100582,0.00687500000000007);
#88082=CYLINDRICAL_SURFACE('',#100591,0.0125000000000001);
#88083=CYLINDRICAL_SURFACE('',#100598,0.0125000000000001);
#88084=CYLINDRICAL_SURFACE('',#100605,0.00687500000000009);
#88085=CYLINDRICAL_SURFACE('',#100614,0.0125000000000001);
#88086=CYLINDRICAL_SURFACE('',#100621,0.0125000000000001);
#88087=CYLINDRICAL_SURFACE('',#100628,0.00687500000000004);
#88088=CYLINDRICAL_SURFACE('',#100637,0.0125000000000001);
#88089=CYLINDRICAL_SURFACE('',#100644,0.0125000000000001);
#88090=CYLINDRICAL_SURFACE('',#100651,0.00687500000000003);
#88091=CYLINDRICAL_SURFACE('',#100660,0.0125);
#88092=CYLINDRICAL_SURFACE('',#100667,0.0125);
#88093=CYLINDRICAL_SURFACE('',#100674,0.00687499999999996);
#88094=CYLINDRICAL_SURFACE('',#100683,0.0125);
#88095=CYLINDRICAL_SURFACE('',#100690,0.0125);
#88096=CYLINDRICAL_SURFACE('',#100697,0.00687499999999994);
#88097=CYLINDRICAL_SURFACE('',#100706,0.0125);
#88098=CYLINDRICAL_SURFACE('',#100713,0.0125000000000001);
#88099=CYLINDRICAL_SURFACE('',#100720,0.00687499999999994);
#88100=CYLINDRICAL_SURFACE('',#100729,0.0124999999999999);
#88101=CYLINDRICAL_SURFACE('',#100736,0.0124999999999999);
#88102=CYLINDRICAL_SURFACE('',#100743,0.00687500000000012);
#88103=CYLINDRICAL_SURFACE('',#100752,0.0125);
#88104=CYLINDRICAL_SURFACE('',#100759,0.0125);
#88105=CYLINDRICAL_SURFACE('',#100766,0.00687499999999988);
#88106=CYLINDRICAL_SURFACE('',#100775,0.0125);
#88107=CYLINDRICAL_SURFACE('',#100782,0.0125);
#88108=CYLINDRICAL_SURFACE('',#100789,0.00687500000000008);
#88109=CYLINDRICAL_SURFACE('',#100798,0.0125000000000001);
#88110=CYLINDRICAL_SURFACE('',#100805,0.0125000000000001);
#88111=CYLINDRICAL_SURFACE('',#100812,0.00687500000000005);
#88112=CYLINDRICAL_SURFACE('',#100821,0.0125);
#88113=CYLINDRICAL_SURFACE('',#100828,0.0125);
#88114=CYLINDRICAL_SURFACE('',#100835,0.00687499999999988);
#88115=CYLINDRICAL_SURFACE('',#100844,0.0125);
#88116=CYLINDRICAL_SURFACE('',#100851,0.0125);
#88117=CYLINDRICAL_SURFACE('',#100858,0.00687499999999997);
#88118=CYLINDRICAL_SURFACE('',#100867,0.0125);
#88119=CYLINDRICAL_SURFACE('',#100874,0.0125);
#88120=CYLINDRICAL_SURFACE('',#100881,0.00687499999999996);
#88121=CYLINDRICAL_SURFACE('',#100890,0.0125);
#88122=CYLINDRICAL_SURFACE('',#100897,0.0125);
#88123=CYLINDRICAL_SURFACE('',#100904,0.00687499999999993);
#88124=CYLINDRICAL_SURFACE('',#100913,0.0125);
#88125=CYLINDRICAL_SURFACE('',#100920,0.0125);
#88126=CYLINDRICAL_SURFACE('',#100927,0.00687500000000001);
#88127=CYLINDRICAL_SURFACE('',#100936,0.0125);
#88128=CYLINDRICAL_SURFACE('',#100943,0.0125);
#88129=CYLINDRICAL_SURFACE('',#100950,0.00687499999999995);
#88130=CYLINDRICAL_SURFACE('',#100959,0.0125);
#88131=CYLINDRICAL_SURFACE('',#100966,0.0125);
#88132=CYLINDRICAL_SURFACE('',#100973,0.00687499999999997);
#88133=CYLINDRICAL_SURFACE('',#100982,0.0125);
#88134=CYLINDRICAL_SURFACE('',#100989,0.0125);
#88135=CYLINDRICAL_SURFACE('',#100996,0.00687499999999996);
#88136=CYLINDRICAL_SURFACE('',#101005,0.0125);
#88137=CYLINDRICAL_SURFACE('',#101012,0.0125);
#88138=CYLINDRICAL_SURFACE('',#101019,0.00687500000000001);
#88139=CYLINDRICAL_SURFACE('',#101028,0.0125);
#88140=CYLINDRICAL_SURFACE('',#101035,0.0125);
#88141=CYLINDRICAL_SURFACE('',#101042,0.00687499999999995);
#88142=CYLINDRICAL_SURFACE('',#101051,0.0125);
#88143=CYLINDRICAL_SURFACE('',#101058,0.0125);
#88144=CYLINDRICAL_SURFACE('',#101065,0.00687499999999993);
#88145=CYLINDRICAL_SURFACE('',#101074,0.0125);
#88146=CYLINDRICAL_SURFACE('',#101081,0.0125);
#88147=CYLINDRICAL_SURFACE('',#101088,0.00687499999999996);
#88148=CYLINDRICAL_SURFACE('',#101097,0.0125000000000001);
#88149=CYLINDRICAL_SURFACE('',#101104,0.0125000000000001);
#88150=CYLINDRICAL_SURFACE('',#101111,0.00687499999999997);
#88151=CYLINDRICAL_SURFACE('',#101120,0.0125000000000001);
#88152=CYLINDRICAL_SURFACE('',#101127,0.0125);
#88153=CYLINDRICAL_SURFACE('',#101134,0.00687499999999988);
#88154=CYLINDRICAL_SURFACE('',#101143,0.0124999999999999);
#88155=CYLINDRICAL_SURFACE('',#101150,0.0124999999999999);
#88156=CYLINDRICAL_SURFACE('',#101157,0.00687500000000005);
#88157=CYLINDRICAL_SURFACE('',#101166,0.0125);
#88158=CYLINDRICAL_SURFACE('',#101173,0.0125);
#88159=CYLINDRICAL_SURFACE('',#101180,0.00687499999999999);
#88160=CYLINDRICAL_SURFACE('',#101189,0.0125);
#88161=CYLINDRICAL_SURFACE('',#101196,0.0125);
#88162=CYLINDRICAL_SURFACE('',#101203,0.00687499999999995);
#88163=CYLINDRICAL_SURFACE('',#101212,0.0125);
#88164=CYLINDRICAL_SURFACE('',#101219,0.0125);
#88165=CYLINDRICAL_SURFACE('',#101226,0.00687499999999988);
#88166=CYLINDRICAL_SURFACE('',#101235,0.0124999999999999);
#88167=CYLINDRICAL_SURFACE('',#101242,0.0124999999999999);
#88168=CYLINDRICAL_SURFACE('',#101249,0.00687499999999991);
#88169=CYLINDRICAL_SURFACE('',#101258,0.0125);
#88170=CYLINDRICAL_SURFACE('',#101265,0.0125);
#88171=CYLINDRICAL_SURFACE('',#101272,0.0068749999999999);
#88172=CYLINDRICAL_SURFACE('',#101281,0.0125000000000001);
#88173=CYLINDRICAL_SURFACE('',#101288,0.0125);
#88174=CYLINDRICAL_SURFACE('',#101295,0.00687499999999987);
#88175=CYLINDRICAL_SURFACE('',#101304,0.0125);
#88176=CYLINDRICAL_SURFACE('',#101311,0.0125);
#88177=CYLINDRICAL_SURFACE('',#101318,0.00687500000000009);
#88178=CYLINDRICAL_SURFACE('',#101327,0.0124999999999999);
#88179=CYLINDRICAL_SURFACE('',#101334,0.0124999999999999);
#88180=CYLINDRICAL_SURFACE('',#101341,0.00687499999999986);
#88181=CYLINDRICAL_SURFACE('',#101350,0.0124999999999999);
#88182=CYLINDRICAL_SURFACE('',#101357,0.0124999999999999);
#88183=CYLINDRICAL_SURFACE('',#101364,0.00687500000000003);
#88184=CYLINDRICAL_SURFACE('',#101373,0.0124999999999999);
#88185=CYLINDRICAL_SURFACE('',#101380,0.0124999999999999);
#88186=CYLINDRICAL_SURFACE('',#101387,0.00687499999999996);
#88187=CYLINDRICAL_SURFACE('',#101396,0.0124999999999998);
#88188=CYLINDRICAL_SURFACE('',#101403,0.0124999999999998);
#88189=CYLINDRICAL_SURFACE('',#101410,0.00687499999999994);
#88190=CYLINDRICAL_SURFACE('',#101419,0.0125);
#88191=CYLINDRICAL_SURFACE('',#101426,0.0125000000000001);
#88192=CYLINDRICAL_SURFACE('',#101433,0.00687499999999994);
#88193=CYLINDRICAL_SURFACE('',#101442,0.0125);
#88194=CYLINDRICAL_SURFACE('',#101449,0.0125);
#88195=CYLINDRICAL_SURFACE('',#101456,0.00687499999999985);
#88196=CYLINDRICAL_SURFACE('',#101465,0.0125);
#88197=CYLINDRICAL_SURFACE('',#101472,0.0125);
#88198=CYLINDRICAL_SURFACE('',#101479,0.00687500000000006);
#88199=CYLINDRICAL_SURFACE('',#101488,0.0125);
#88200=CYLINDRICAL_SURFACE('',#101495,0.0125);
#88201=CYLINDRICAL_SURFACE('',#101502,0.00687500000000008);
#88202=CYLINDRICAL_SURFACE('',#101511,0.0124999999999999);
#88203=CYLINDRICAL_SURFACE('',#101518,0.0124999999999999);
#88204=CYLINDRICAL_SURFACE('',#101525,0.00687500000000005);
#88205=CYLINDRICAL_SURFACE('',#101534,0.0124999999999998);
#88206=CYLINDRICAL_SURFACE('',#101541,0.0124999999999998);
#88207=CYLINDRICAL_SURFACE('',#101548,0.00687499999999988);
#88208=CYLINDRICAL_SURFACE('',#101557,0.0124999999999999);
#88209=CYLINDRICAL_SURFACE('',#101564,0.0124999999999999);
#88210=CYLINDRICAL_SURFACE('',#101571,0.00687499999999997);
#88211=CYLINDRICAL_SURFACE('',#101580,0.0125);
#88212=CYLINDRICAL_SURFACE('',#101587,0.0125);
#88213=CYLINDRICAL_SURFACE('',#101594,0.00687499999999996);
#88214=CYLINDRICAL_SURFACE('',#101603,0.0125);
#88215=CYLINDRICAL_SURFACE('',#101610,0.0125);
#88216=CYLINDRICAL_SURFACE('',#101617,0.00687499999999993);
#88217=CYLINDRICAL_SURFACE('',#101626,0.0125);
#88218=CYLINDRICAL_SURFACE('',#101633,0.0125);
#88219=CYLINDRICAL_SURFACE('',#101640,0.00687499999999995);
#88220=CYLINDRICAL_SURFACE('',#101649,0.0125);
#88221=CYLINDRICAL_SURFACE('',#101656,0.0125);
#88222=CYLINDRICAL_SURFACE('',#101663,0.00687499999999995);
#88223=CYLINDRICAL_SURFACE('',#101672,0.0125);
#88224=CYLINDRICAL_SURFACE('',#101679,0.0125);
#88225=CYLINDRICAL_SURFACE('',#101686,0.00687499999999996);
#88226=CYLINDRICAL_SURFACE('',#101695,0.0125);
#88227=CYLINDRICAL_SURFACE('',#101702,0.0125);
#88228=CYLINDRICAL_SURFACE('',#101709,0.00687499999999996);
#88229=CYLINDRICAL_SURFACE('',#101718,0.0125);
#88230=CYLINDRICAL_SURFACE('',#101725,0.0125);
#88231=CYLINDRICAL_SURFACE('',#101732,0.00687499999999995);
#88232=CYLINDRICAL_SURFACE('',#101741,0.0125);
#88233=CYLINDRICAL_SURFACE('',#101748,0.0125);
#88234=CYLINDRICAL_SURFACE('',#101755,0.00687500000000001);
#88235=CYLINDRICAL_SURFACE('',#101764,0.0125000000000001);
#88236=CYLINDRICAL_SURFACE('',#101771,0.0125000000000001);
#88237=CYLINDRICAL_SURFACE('',#101778,0.00687499999999993);
#88238=CYLINDRICAL_SURFACE('',#101787,0.0125);
#88239=CYLINDRICAL_SURFACE('',#101794,0.0125);
#88240=CYLINDRICAL_SURFACE('',#101801,0.00687499999999996);
#88241=CYLINDRICAL_SURFACE('',#101810,0.0125);
#88242=CYLINDRICAL_SURFACE('',#101817,0.0125);
#88243=CYLINDRICAL_SURFACE('',#101824,0.00687499999999997);
#88244=CYLINDRICAL_SURFACE('',#101833,0.0125);
#88245=CYLINDRICAL_SURFACE('',#101840,0.0125);
#88246=CYLINDRICAL_SURFACE('',#101847,0.00687499999999988);
#88247=CYLINDRICAL_SURFACE('',#101856,0.0125);
#88248=CYLINDRICAL_SURFACE('',#101863,0.0125);
#88249=CYLINDRICAL_SURFACE('',#101870,0.00687500000000005);
#88250=CYLINDRICAL_SURFACE('',#101879,0.0125);
#88251=CYLINDRICAL_SURFACE('',#101886,0.0125);
#88252=CYLINDRICAL_SURFACE('',#101893,0.00687500000000008);
#88253=CYLINDRICAL_SURFACE('',#101902,0.0125000000000001);
#88254=CYLINDRICAL_SURFACE('',#101909,0.0125000000000001);
#88255=CYLINDRICAL_SURFACE('',#101916,0.00687499999999988);
#88256=CYLINDRICAL_SURFACE('',#101925,0.0125);
#88257=CYLINDRICAL_SURFACE('',#101932,0.0125);
#88258=CYLINDRICAL_SURFACE('',#101939,0.00687499999999985);
#88259=CYLINDRICAL_SURFACE('',#101948,0.0125);
#88260=CYLINDRICAL_SURFACE('',#101955,0.0125);
#88261=CYLINDRICAL_SURFACE('',#101962,0.00687499999999994);
#88262=CYLINDRICAL_SURFACE('',#101971,0.0125);
#88263=CYLINDRICAL_SURFACE('',#101978,0.0125);
#88264=CYLINDRICAL_SURFACE('',#101985,0.00687500000000009);
#88265=CYLINDRICAL_SURFACE('',#101994,0.0124999999999998);
#88266=CYLINDRICAL_SURFACE('',#102001,0.0125);
#88267=CYLINDRICAL_SURFACE('',#102008,0.00687499999999996);
#88268=CYLINDRICAL_SURFACE('',#102017,0.0124999999999998);
#88269=CYLINDRICAL_SURFACE('',#102024,0.0124999999999998);
#88270=CYLINDRICAL_SURFACE('',#102031,0.00687500000000003);
#88271=CYLINDRICAL_SURFACE('',#102040,0.0125);
#88272=CYLINDRICAL_SURFACE('',#102047,0.0125);
#88273=CYLINDRICAL_SURFACE('',#102054,0.00687500000000004);
#88274=CYLINDRICAL_SURFACE('',#102063,0.0124999999999999);
#88275=CYLINDRICAL_SURFACE('',#102070,0.0124999999999999);
#88276=CYLINDRICAL_SURFACE('',#102077,0.00687500000000009);
#88277=CYLINDRICAL_SURFACE('',#102086,0.0124999999999999);
#88278=CYLINDRICAL_SURFACE('',#102093,0.0124999999999999);
#88279=CYLINDRICAL_SURFACE('',#102100,0.00687500000000007);
#88280=CYLINDRICAL_SURFACE('',#102109,0.0124999999999999);
#88281=CYLINDRICAL_SURFACE('',#102116,0.0124999999999999);
#88282=CYLINDRICAL_SURFACE('',#102123,0.00687500000000009);
#88283=CYLINDRICAL_SURFACE('',#102132,0.0125);
#88284=CYLINDRICAL_SURFACE('',#102139,0.0125000000000001);
#88285=CYLINDRICAL_SURFACE('',#102146,0.00687499999999991);
#88286=CYLINDRICAL_SURFACE('',#102155,0.0125);
#88287=CYLINDRICAL_SURFACE('',#102162,0.0125);
#88288=CYLINDRICAL_SURFACE('',#102169,0.00687499999999998);
#88289=CYLINDRICAL_SURFACE('',#102178,0.0124999999999999);
#88290=CYLINDRICAL_SURFACE('',#102185,0.0124999999999999);
#88291=CYLINDRICAL_SURFACE('',#102192,0.00687499999999995);
#88292=CYLINDRICAL_SURFACE('',#102201,0.0125);
#88293=CYLINDRICAL_SURFACE('',#102208,0.0125);
#88294=CYLINDRICAL_SURFACE('',#102215,0.00687499999999993);
#88295=CYLINDRICAL_SURFACE('',#102224,0.0125);
#88296=CYLINDRICAL_SURFACE('',#102231,0.0125);
#88297=CYLINDRICAL_SURFACE('',#102238,0.00687499999999999);
#88298=CYLINDRICAL_SURFACE('',#102247,0.0125);
#88299=CYLINDRICAL_SURFACE('',#102254,0.0125);
#88300=CYLINDRICAL_SURFACE('',#102261,0.00687499999999997);
#88301=CYLINDRICAL_SURFACE('',#102270,0.0125);
#88302=CYLINDRICAL_SURFACE('',#102277,0.0125);
#88303=CYLINDRICAL_SURFACE('',#102284,0.00687499999999996);
#88304=CYLINDRICAL_SURFACE('',#102293,0.0125);
#88305=CYLINDRICAL_SURFACE('',#102300,0.0125);
#88306=CYLINDRICAL_SURFACE('',#102307,0.00687499999999999);
#88307=CYLINDRICAL_SURFACE('',#102316,0.0125);
#88308=CYLINDRICAL_SURFACE('',#102323,0.0125);
#88309=CYLINDRICAL_SURFACE('',#102330,0.00687499999999995);
#88310=CYLINDRICAL_SURFACE('',#102339,0.0125);
#88311=CYLINDRICAL_SURFACE('',#102346,0.0125);
#88312=CYLINDRICAL_SURFACE('',#102353,0.00687499999999988);
#88313=CYLINDRICAL_SURFACE('',#102362,0.0125000000000001);
#88314=CYLINDRICAL_SURFACE('',#102369,0.0125000000000001);
#88315=CYLINDRICAL_SURFACE('',#102376,0.00687500000000005);
#88316=CYLINDRICAL_SURFACE('',#102385,0.0125);
#88317=CYLINDRICAL_SURFACE('',#102392,0.0125);
#88318=CYLINDRICAL_SURFACE('',#102399,0.0068749999999999);
#88319=CYLINDRICAL_SURFACE('',#102408,0.0125000000000001);
#88320=CYLINDRICAL_SURFACE('',#102415,0.0125);
#88321=CYLINDRICAL_SURFACE('',#102422,0.00687499999999987);
#88322=CYLINDRICAL_SURFACE('',#102431,0.0125);
#88323=CYLINDRICAL_SURFACE('',#102438,0.0125);
#88324=CYLINDRICAL_SURFACE('',#102445,0.0068749999999999);
#88325=CYLINDRICAL_SURFACE('',#102454,0.0124999999999999);
#88326=CYLINDRICAL_SURFACE('',#102461,0.0124999999999999);
#88327=CYLINDRICAL_SURFACE('',#102468,0.00687499999999986);
#88328=CYLINDRICAL_SURFACE('',#102477,0.0125000000000001);
#88329=CYLINDRICAL_SURFACE('',#102484,0.0125000000000001);
#88330=CYLINDRICAL_SURFACE('',#102491,0.00687499999999985);
#88331=CYLINDRICAL_SURFACE('',#102500,0.0125000000000001);
#88332=CYLINDRICAL_SURFACE('',#102507,0.0125000000000001);
#88333=CYLINDRICAL_SURFACE('',#102514,0.00687499999999996);
#88334=CYLINDRICAL_SURFACE('',#102523,0.0125000000000001);
#88335=CYLINDRICAL_SURFACE('',#102530,0.0125000000000001);
#88336=CYLINDRICAL_SURFACE('',#102537,0.00687499999999994);
#88337=CYLINDRICAL_SURFACE('',#102546,0.0125);
#88338=CYLINDRICAL_SURFACE('',#102553,0.0125000000000001);
#88339=CYLINDRICAL_SURFACE('',#102560,0.00687499999999994);
#88340=CYLINDRICAL_SURFACE('',#102569,0.0125);
#88341=CYLINDRICAL_SURFACE('',#102576,0.0125);
#88342=CYLINDRICAL_SURFACE('',#102583,0.00687499999999985);
#88343=CYLINDRICAL_SURFACE('',#102592,0.0125);
#88344=CYLINDRICAL_SURFACE('',#102599,0.0125);
#88345=CYLINDRICAL_SURFACE('',#102606,0.00687500000000006);
#88346=CYLINDRICAL_SURFACE('',#102615,0.0125);
#88347=CYLINDRICAL_SURFACE('',#102622,0.0125);
#88348=CYLINDRICAL_SURFACE('',#102629,0.00687500000000008);
#88349=CYLINDRICAL_SURFACE('',#102638,0.0124999999999999);
#88350=CYLINDRICAL_SURFACE('',#102645,0.0124999999999999);
#88351=CYLINDRICAL_SURFACE('',#102649,1.17524047358089);
#88352=CYLINDRICAL_SURFACE('',#102651,1.17524047358089);
#88353=CYLINDRICAL_SURFACE('',#102652,1.17524047358089);
#88354=CYLINDRICAL_SURFACE('',#102653,1.17524047358089);
#88355=CYLINDRICAL_SURFACE('',#102654,1.17524047358089);
#88356=CYLINDRICAL_SURFACE('',#102655,1.17524047358089);
#88357=CYLINDRICAL_SURFACE('',#102656,1.17524047358089);
#88358=CYLINDRICAL_SURFACE('',#102657,1.17524047358089);
#88359=CYLINDRICAL_SURFACE('',#102658,1.17524047358089);
#88360=CYLINDRICAL_SURFACE('',#102659,1.17524047358089);
#88361=CYLINDRICAL_SURFACE('',#102660,1.17524047358089);
#88362=CYLINDRICAL_SURFACE('',#102661,1.17524047358089);
#88363=CYLINDRICAL_SURFACE('',#102662,1.17524047358089);
#88364=CYLINDRICAL_SURFACE('',#102663,1.17524047358089);
#88365=CYLINDRICAL_SURFACE('',#102664,1.17524047358089);
#88366=CYLINDRICAL_SURFACE('',#102665,1.17524047358089);
#88367=CYLINDRICAL_SURFACE('',#102666,1.17524047358089);
#88368=CYLINDRICAL_SURFACE('',#102667,1.17524047358089);
#88369=CYLINDRICAL_SURFACE('',#102668,1.17524047358089);
#88370=CYLINDRICAL_SURFACE('',#102669,1.17524047358089);
#88371=CYLINDRICAL_SURFACE('',#102670,1.17524047358089);
#88372=CYLINDRICAL_SURFACE('',#102671,1.17524047358089);
#88373=CYLINDRICAL_SURFACE('',#102672,1.17524047358089);
#88374=CYLINDRICAL_SURFACE('',#102673,1.17524047358089);
#88375=CYLINDRICAL_SURFACE('',#102674,1.17524047358089);
#88376=CYLINDRICAL_SURFACE('',#102675,1.17524047358089);
#88377=CYLINDRICAL_SURFACE('',#102676,1.17524047358089);
#88378=CYLINDRICAL_SURFACE('',#102677,1.17524047358089);
#88379=CYLINDRICAL_SURFACE('',#102678,1.17524047358089);
#88380=CYLINDRICAL_SURFACE('',#102679,1.17524047358089);
#88381=CYLINDRICAL_SURFACE('',#102680,1.17524047358089);
#88382=CYLINDRICAL_SURFACE('',#102681,1.17524047358089);
#88383=CYLINDRICAL_SURFACE('',#102682,1.17524047358089);
#88384=CYLINDRICAL_SURFACE('',#102683,1.17524047358089);
#88385=CYLINDRICAL_SURFACE('',#102684,1.17524047358089);
#88386=CYLINDRICAL_SURFACE('',#102685,1.17524047358089);
#88387=CYLINDRICAL_SURFACE('',#102690,1.50000000000006);
#88388=CYLINDRICAL_SURFACE('',#102692,1.50000000000006);
#88389=CYLINDRICAL_SURFACE('',#102693,1.50000000000006);
#88390=CYLINDRICAL_SURFACE('',#102694,1.50000000000006);
#88391=CYLINDRICAL_SURFACE('',#102695,1.50000000000006);
#88392=CYLINDRICAL_SURFACE('',#102696,1.50000000000006);
#88393=CYLINDRICAL_SURFACE('',#102697,1.50000000000006);
#88394=CYLINDRICAL_SURFACE('',#102698,1.50000000000006);
#88395=CYLINDRICAL_SURFACE('',#102699,1.50000000000006);
#88396=CYLINDRICAL_SURFACE('',#102700,1.50000000000006);
#88397=CYLINDRICAL_SURFACE('',#102701,1.50000000000006);
#88398=CYLINDRICAL_SURFACE('',#102702,1.50000000000006);
#88399=CYLINDRICAL_SURFACE('',#102703,1.50000000000006);
#88400=CYLINDRICAL_SURFACE('',#102704,1.50000000000006);
#88401=CYLINDRICAL_SURFACE('',#102705,1.50000000000006);
#88402=CYLINDRICAL_SURFACE('',#102706,1.50000000000006);
#88403=CYLINDRICAL_SURFACE('',#102707,1.50000000000006);
#88404=CYLINDRICAL_SURFACE('',#102708,1.50000000000006);
#88405=CYLINDRICAL_SURFACE('',#102709,1.50000000000006);
#88406=CYLINDRICAL_SURFACE('',#102710,1.50000000000006);
#88407=CYLINDRICAL_SURFACE('',#102711,1.50000000000006);
#88408=CYLINDRICAL_SURFACE('',#102712,1.50000000000006);
#88409=CYLINDRICAL_SURFACE('',#102713,1.50000000000006);
#88410=CYLINDRICAL_SURFACE('',#102714,1.50000000000006);
#88411=CYLINDRICAL_SURFACE('',#102715,1.50000000000006);
#88412=CYLINDRICAL_SURFACE('',#102716,1.50000000000006);
#88413=CYLINDRICAL_SURFACE('',#102717,1.50000000000006);
#88414=CYLINDRICAL_SURFACE('',#102718,1.50000000000006);
#88415=CYLINDRICAL_SURFACE('',#102719,1.50000000000006);
#88416=CYLINDRICAL_SURFACE('',#102720,1.50000000000006);
#88417=CYLINDRICAL_SURFACE('',#102721,1.50000000000006);
#88418=CYLINDRICAL_SURFACE('',#102722,1.50000000000006);
#88419=CYLINDRICAL_SURFACE('',#102723,1.50000000000006);
#88420=CYLINDRICAL_SURFACE('',#102724,1.50000000000006);
#88421=CYLINDRICAL_SURFACE('',#102725,1.50000000000006);
#88422=CYLINDRICAL_SURFACE('',#103114,1.50000000000006);
#88423=CYLINDRICAL_SURFACE('',#103222,2.75);
#88424=CYLINDRICAL_SURFACE('',#103528,0.0343750000000002);
#88425=CYLINDRICAL_SURFACE('',#103563,1.17524047358089);
#88426=CYLINDRICAL_SURFACE('',#103567,0.0219999999999999);
#88427=CYLINDRICAL_SURFACE('',#103575,0.0219999999999999);
#88428=CYLINDRICAL_SURFACE('',#103582,0.0343750000000002);
#88429=CYLINDRICAL_SURFACE('',#103589,0.0219999999999999);
#88430=CYLINDRICAL_SURFACE('',#103596,0.0219999999999999);
#88431=CYLINDRICAL_SURFACE('',#103603,0.0343750000000002);
#88432=CYLINDRICAL_SURFACE('',#103610,0.0219999999999999);
#88433=CYLINDRICAL_SURFACE('',#103617,0.0219999999999999);
#88434=CYLINDRICAL_SURFACE('',#103624,0.0343750000000002);
#88435=CYLINDRICAL_SURFACE('',#103631,0.0220000000000001);
#88436=CYLINDRICAL_SURFACE('',#103638,0.0220000000000001);
#88437=CYLINDRICAL_SURFACE('',#103645,0.0343750000000002);
#88438=CYLINDRICAL_SURFACE('',#103652,0.022);
#88439=CYLINDRICAL_SURFACE('',#103659,0.022);
#88440=CYLINDRICAL_SURFACE('',#103666,0.0343750000000002);
#88441=CYLINDRICAL_SURFACE('',#103673,0.022);
#88442=CYLINDRICAL_SURFACE('',#103680,0.022);
#88443=CYLINDRICAL_SURFACE('',#103687,0.0343750000000003);
#88444=CYLINDRICAL_SURFACE('',#103694,0.0219999999999999);
#88445=CYLINDRICAL_SURFACE('',#103701,0.0219999999999999);
#88446=CYLINDRICAL_SURFACE('',#103708,0.0343750000000004);
#88447=CYLINDRICAL_SURFACE('',#103715,0.022);
#88448=CYLINDRICAL_SURFACE('',#103722,0.022);
#88449=CYLINDRICAL_SURFACE('',#103729,0.0343750000000001);
#88450=CYLINDRICAL_SURFACE('',#103736,0.0220000000000002);
#88451=CYLINDRICAL_SURFACE('',#103743,0.0220000000000002);
#88452=CYLINDRICAL_SURFACE('',#103750,0.0343750000000003);
#88453=CYLINDRICAL_SURFACE('',#103757,0.0220000000000001);
#88454=CYLINDRICAL_SURFACE('',#103764,0.0220000000000001);
#88455=CYLINDRICAL_SURFACE('',#103771,0.0343750000000003);
#88456=CYLINDRICAL_SURFACE('',#103778,0.022);
#88457=CYLINDRICAL_SURFACE('',#103785,0.022);
#88458=CYLINDRICAL_SURFACE('',#103792,0.0343750000000002);
#88459=CYLINDRICAL_SURFACE('',#103799,0.022);
#88460=CYLINDRICAL_SURFACE('',#103806,0.0219999999999998);
#88461=CYLINDRICAL_SURFACE('',#103813,0.0343750000000002);
#88462=CYLINDRICAL_SURFACE('',#103820,0.0220000000000002);
#88463=CYLINDRICAL_SURFACE('',#103827,0.0220000000000002);
#88464=CYLINDRICAL_SURFACE('',#103834,0.0343750000000002);
#88465=CYLINDRICAL_SURFACE('',#103841,0.0220000000000002);
#88466=CYLINDRICAL_SURFACE('',#103848,0.0220000000000002);
#88467=CYLINDRICAL_SURFACE('',#103855,0.0343750000000002);
#88468=CYLINDRICAL_SURFACE('',#103862,0.0220000000000001);
#88469=CYLINDRICAL_SURFACE('',#103869,0.0220000000000001);
#88470=CYLINDRICAL_SURFACE('',#103876,0.0343750000000002);
#88471=CYLINDRICAL_SURFACE('',#103883,0.0220000000000001);
#88472=CYLINDRICAL_SURFACE('',#103890,0.0220000000000001);
#88473=CYLINDRICAL_SURFACE('',#103897,0.0343750000000002);
#88474=CYLINDRICAL_SURFACE('',#103904,0.022);
#88475=CYLINDRICAL_SURFACE('',#103911,0.022);
#88476=CYLINDRICAL_SURFACE('',#103918,0.0343750000000004);
#88477=CYLINDRICAL_SURFACE('',#103925,0.0220000000000001);
#88478=CYLINDRICAL_SURFACE('',#103932,0.0220000000000001);
#88479=CYLINDRICAL_SURFACE('',#103939,0.0343750000000002);
#88480=CYLINDRICAL_SURFACE('',#103946,0.0219999999999999);
#88481=CYLINDRICAL_SURFACE('',#103953,0.0219999999999999);
#88482=CYLINDRICAL_SURFACE('',#103960,0.0343750000000001);
#88483=CYLINDRICAL_SURFACE('',#103967,0.0220000000000002);
#88484=CYLINDRICAL_SURFACE('',#103974,0.0220000000000002);
#88485=CYLINDRICAL_SURFACE('',#103981,0.0343750000000004);
#88486=CYLINDRICAL_SURFACE('',#103988,0.0220000000000002);
#88487=CYLINDRICAL_SURFACE('',#103995,0.0220000000000002);
#88488=CYLINDRICAL_SURFACE('',#104002,0.0343750000000002);
#88489=CYLINDRICAL_SURFACE('',#104009,0.022);
#88490=CYLINDRICAL_SURFACE('',#104016,0.022);
#88491=CYLINDRICAL_SURFACE('',#104023,0.0343750000000001);
#88492=CYLINDRICAL_SURFACE('',#104030,0.022);
#88493=CYLINDRICAL_SURFACE('',#104037,0.022);
#88494=CYLINDRICAL_SURFACE('',#104044,0.0343750000000002);
#88495=CYLINDRICAL_SURFACE('',#104051,0.0220000000000001);
#88496=CYLINDRICAL_SURFACE('',#104058,0.0220000000000001);
#88497=CYLINDRICAL_SURFACE('',#104065,0.0343750000000001);
#88498=CYLINDRICAL_SURFACE('',#104072,0.0220000000000002);
#88499=CYLINDRICAL_SURFACE('',#104079,0.0220000000000002);
#88500=CYLINDRICAL_SURFACE('',#104086,0.0343750000000003);
#88501=CYLINDRICAL_SURFACE('',#104093,0.022);
#88502=CYLINDRICAL_SURFACE('',#104100,0.022);
#88503=CYLINDRICAL_SURFACE('',#104107,0.0343750000000003);
#88504=CYLINDRICAL_SURFACE('',#104114,0.022);
#88505=CYLINDRICAL_SURFACE('',#104121,0.022);
#88506=CYLINDRICAL_SURFACE('',#104128,0.0343750000000003);
#88507=CYLINDRICAL_SURFACE('',#104135,0.022);
#88508=CYLINDRICAL_SURFACE('',#104142,0.022);
#88509=CYLINDRICAL_SURFACE('',#104149,0.0343750000000003);
#88510=CYLINDRICAL_SURFACE('',#104156,0.022);
#88511=CYLINDRICAL_SURFACE('',#104163,0.022);
#88512=CYLINDRICAL_SURFACE('',#104170,0.0343750000000002);
#88513=CYLINDRICAL_SURFACE('',#104177,0.0220000000000001);
#88514=CYLINDRICAL_SURFACE('',#104184,0.0220000000000001);
#88515=CYLINDRICAL_SURFACE('',#104191,0.0343750000000002);
#88516=CYLINDRICAL_SURFACE('',#104198,0.022);
#88517=CYLINDRICAL_SURFACE('',#104205,0.022);
#88518=CYLINDRICAL_SURFACE('',#104212,0.0343750000000002);
#88519=CYLINDRICAL_SURFACE('',#104219,0.0220000000000002);
#88520=CYLINDRICAL_SURFACE('',#104226,0.0220000000000001);
#88521=CYLINDRICAL_SURFACE('',#104233,0.0343750000000002);
#88522=CYLINDRICAL_SURFACE('',#104240,0.0219999999999999);
#88523=CYLINDRICAL_SURFACE('',#104247,0.0219999999999999);
#88524=CYLINDRICAL_SURFACE('',#104254,0.0343750000000003);
#88525=CYLINDRICAL_SURFACE('',#104261,0.0220000000000001);
#88526=CYLINDRICAL_SURFACE('',#104268,0.0220000000000001);
#88527=CYLINDRICAL_SURFACE('',#104275,0.0343750000000003);
#88528=CYLINDRICAL_SURFACE('',#104282,0.0219999999999999);
#88529=CYLINDRICAL_SURFACE('',#104289,0.0219999999999999);
#88530=CYLINDRICAL_SURFACE('',#104296,0.0343750000000002);
#88531=CYLINDRICAL_SURFACE('',#104303,0.0220000000000002);
#88532=CYLINDRICAL_SURFACE('',#104310,0.0220000000000002);
#88533=CYLINDRICAL_SURFACE('',#104317,0.0343750000000003);
#88534=CYLINDRICAL_SURFACE('',#104324,0.0219999999999999);
#88535=CYLINDRICAL_SURFACE('',#104331,0.0219999999999999);
#88536=CYLINDRICAL_SURFACE('',#104338,0.0343750000000003);
#88537=CYLINDRICAL_SURFACE('',#104345,0.0219999999999999);
#88538=CYLINDRICAL_SURFACE('',#104352,0.0219999999999999);
#88539=CYLINDRICAL_SURFACE('',#104359,0.0343750000000004);
#88540=CYLINDRICAL_SURFACE('',#104366,0.0219999999999999);
#88541=CYLINDRICAL_SURFACE('',#104373,0.0219999999999999);
#88542=CYLINDRICAL_SURFACE('',#104380,0.034375);
#88543=CYLINDRICAL_SURFACE('',#104387,0.0220000000000001);
#88544=CYLINDRICAL_SURFACE('',#104394,0.0220000000000001);
#88545=CYLINDRICAL_SURFACE('',#104401,0.0343750000000003);
#88546=CYLINDRICAL_SURFACE('',#104408,0.0219999999999999);
#88547=CYLINDRICAL_SURFACE('',#104415,0.022);
#88548=CYLINDRICAL_SURFACE('',#104422,0.0343750000000004);
#88549=CYLINDRICAL_SURFACE('',#104429,0.0219999999999999);
#88550=CYLINDRICAL_SURFACE('',#104436,0.0219999999999999);
#88551=CYLINDRICAL_SURFACE('',#104443,0.0343750000000002);
#88552=CYLINDRICAL_SURFACE('',#104450,0.022);
#88553=CYLINDRICAL_SURFACE('',#104457,0.022);
#88554=CYLINDRICAL_SURFACE('',#104464,0.0343750000000003);
#88555=CYLINDRICAL_SURFACE('',#104471,0.022);
#88556=CYLINDRICAL_SURFACE('',#104478,0.022);
#88557=CYLINDRICAL_SURFACE('',#104485,0.0343750000000001);
#88558=CYLINDRICAL_SURFACE('',#104492,0.0219999999999998);
#88559=CYLINDRICAL_SURFACE('',#104499,0.0219999999999998);
#88560=CYLINDRICAL_SURFACE('',#104506,0.0343750000000001);
#88561=CYLINDRICAL_SURFACE('',#104513,0.0220000000000002);
#88562=CYLINDRICAL_SURFACE('',#104520,0.0220000000000001);
#88563=CYLINDRICAL_SURFACE('',#104527,0.0343750000000003);
#88564=CYLINDRICAL_SURFACE('',#104534,0.0219999999999998);
#88565=CYLINDRICAL_SURFACE('',#104541,0.0219999999999998);
#88566=CYLINDRICAL_SURFACE('',#104548,0.0343750000000001);
#88567=CYLINDRICAL_SURFACE('',#104555,0.0219999999999999);
#88568=CYLINDRICAL_SURFACE('',#104562,0.0219999999999999);
#88569=CYLINDRICAL_SURFACE('',#104569,0.0343750000000002);
#88570=CYLINDRICAL_SURFACE('',#104576,0.022);
#88571=CYLINDRICAL_SURFACE('',#104583,0.022);
#88572=CYLINDRICAL_SURFACE('',#104590,0.0343750000000002);
#88573=CYLINDRICAL_SURFACE('',#104597,0.022);
#88574=CYLINDRICAL_SURFACE('',#104604,0.022);
#88575=CYLINDRICAL_SURFACE('',#104611,0.0343750000000002);
#88576=CYLINDRICAL_SURFACE('',#104618,0.022);
#88577=CYLINDRICAL_SURFACE('',#104625,0.022);
#88578=CYLINDRICAL_SURFACE('',#104632,0.0343750000000002);
#88579=CYLINDRICAL_SURFACE('',#104639,0.022);
#88580=CYLINDRICAL_SURFACE('',#104646,0.022);
#88581=CYLINDRICAL_SURFACE('',#104653,0.0343750000000002);
#88582=CYLINDRICAL_SURFACE('',#104660,0.0219999999999999);
#88583=CYLINDRICAL_SURFACE('',#104667,0.0219999999999999);
#88584=CYLINDRICAL_SURFACE('',#104674,0.0343750000000002);
#88585=CYLINDRICAL_SURFACE('',#104681,0.0219999999999999);
#88586=CYLINDRICAL_SURFACE('',#104688,0.0219999999999999);
#88587=CYLINDRICAL_SURFACE('',#104695,0.0343750000000002);
#88588=CYLINDRICAL_SURFACE('',#104702,0.0219999999999999);
#88589=CYLINDRICAL_SURFACE('',#104709,0.0219999999999998);
#88590=CYLINDRICAL_SURFACE('',#104716,0.0343750000000001);
#88591=CYLINDRICAL_SURFACE('',#104723,0.0219999999999999);
#88592=CYLINDRICAL_SURFACE('',#104730,0.0219999999999999);
#88593=CYLINDRICAL_SURFACE('',#104737,0.0343750000000001);
#88594=CYLINDRICAL_SURFACE('',#104744,0.0219999999999999);
#88595=CYLINDRICAL_SURFACE('',#104751,0.0219999999999999);
#88596=CYLINDRICAL_SURFACE('',#104758,0.0343750000000003);
#88597=CYLINDRICAL_SURFACE('',#104765,0.0220000000000001);
#88598=CYLINDRICAL_SURFACE('',#104772,0.0220000000000001);
#88599=CYLINDRICAL_SURFACE('',#104779,0.034375);
#88600=CYLINDRICAL_SURFACE('',#104786,0.0220000000000001);
#88601=CYLINDRICAL_SURFACE('',#104793,0.022);
#88602=CYLINDRICAL_SURFACE('',#104800,0.0343750000000002);
#88603=CYLINDRICAL_SURFACE('',#104807,0.022);
#88604=CYLINDRICAL_SURFACE('',#104814,0.022);
#88605=CYLINDRICAL_SURFACE('',#104821,0.0343750000000004);
#88606=CYLINDRICAL_SURFACE('',#104828,0.022);
#88607=CYLINDRICAL_SURFACE('',#104835,0.022);
#88608=CYLINDRICAL_SURFACE('',#104842,0.0343750000000003);
#88609=CYLINDRICAL_SURFACE('',#104849,0.0220000000000001);
#88610=CYLINDRICAL_SURFACE('',#104856,0.0220000000000001);
#88611=CYLINDRICAL_SURFACE('',#104863,0.0343750000000002);
#88612=CYLINDRICAL_SURFACE('',#104870,0.0220000000000002);
#88613=CYLINDRICAL_SURFACE('',#104877,0.0220000000000002);
#88614=CYLINDRICAL_SURFACE('',#104884,0.0343750000000003);
#88615=CYLINDRICAL_SURFACE('',#104891,0.0220000000000002);
#88616=CYLINDRICAL_SURFACE('',#104898,0.0220000000000002);
#88617=CYLINDRICAL_SURFACE('',#104905,0.0343750000000003);
#88618=CYLINDRICAL_SURFACE('',#104912,0.0220000000000001);
#88619=CYLINDRICAL_SURFACE('',#104919,0.0220000000000001);
#88620=CYLINDRICAL_SURFACE('',#104926,0.0343750000000002);
#88621=CYLINDRICAL_SURFACE('',#104933,0.0219999999999998);
#88622=CYLINDRICAL_SURFACE('',#104940,0.0219999999999998);
#88623=CYLINDRICAL_SURFACE('',#104947,0.0343750000000003);
#88624=CYLINDRICAL_SURFACE('',#104954,0.0220000000000001);
#88625=CYLINDRICAL_SURFACE('',#104961,0.0220000000000001);
#88626=CYLINDRICAL_SURFACE('',#104968,0.0343750000000002);
#88627=CYLINDRICAL_SURFACE('',#104975,0.0219999999999998);
#88628=CYLINDRICAL_SURFACE('',#104982,0.0219999999999998);
#88629=CYLINDRICAL_SURFACE('',#104989,0.0343750000000002);
#88630=CYLINDRICAL_SURFACE('',#104996,0.0220000000000001);
#88631=CYLINDRICAL_SURFACE('',#105003,0.0220000000000001);
#88632=CYLINDRICAL_SURFACE('',#105010,0.0343750000000002);
#88633=CYLINDRICAL_SURFACE('',#105017,0.022);
#88634=CYLINDRICAL_SURFACE('',#105024,0.022);
#88635=CYLINDRICAL_SURFACE('',#105031,0.0343750000000002);
#88636=CYLINDRICAL_SURFACE('',#105038,0.0220000000000001);
#88637=CYLINDRICAL_SURFACE('',#105045,0.0220000000000001);
#88638=CYLINDRICAL_SURFACE('',#105052,0.0343750000000002);
#88639=CYLINDRICAL_SURFACE('',#105059,0.022);
#88640=CYLINDRICAL_SURFACE('',#105066,0.022);
#88641=CYLINDRICAL_SURFACE('',#105073,0.0343750000000003);
#88642=CYLINDRICAL_SURFACE('',#105080,0.0220000000000001);
#88643=CYLINDRICAL_SURFACE('',#105087,0.0220000000000001);
#88644=CYLINDRICAL_SURFACE('',#105094,0.0343750000000002);
#88645=CYLINDRICAL_SURFACE('',#105101,0.0220000000000001);
#88646=CYLINDRICAL_SURFACE('',#105108,0.0220000000000001);
#88647=CYLINDRICAL_SURFACE('',#105115,0.0343750000000003);
#88648=CYLINDRICAL_SURFACE('',#105122,0.0220000000000001);
#88649=CYLINDRICAL_SURFACE('',#105129,0.0220000000000001);
#88650=CYLINDRICAL_SURFACE('',#105136,0.0343750000000001);
#88651=CYLINDRICAL_SURFACE('',#105143,0.0219999999999999);
#88652=CYLINDRICAL_SURFACE('',#105150,0.0219999999999999);
#88653=CYLINDRICAL_SURFACE('',#105157,0.0343750000000003);
#88654=CYLINDRICAL_SURFACE('',#105164,0.0219999999999999);
#88655=CYLINDRICAL_SURFACE('',#105171,0.0219999999999999);
#88656=CYLINDRICAL_SURFACE('',#105176,1.03775);
#88657=CYLINDRICAL_SURFACE('',#105178,1.03775);
#88658=CYLINDRICAL_SURFACE('',#105180,1.03775);
#88659=CYLINDRICAL_SURFACE('',#105181,1.03775);
#88660=CYLINDRICAL_SURFACE('',#105182,1.03775);
#88661=CYLINDRICAL_SURFACE('',#105183,1.03775);
#88662=CYLINDRICAL_SURFACE('',#105184,1.03775);
#88663=CYLINDRICAL_SURFACE('',#105185,1.03775);
#88664=CYLINDRICAL_SURFACE('',#105187,1.29);
#88665=CYLINDRICAL_SURFACE('',#105189,1.29);
#88666=CYLINDRICAL_SURFACE('',#105190,1.29);
#88667=CYLINDRICAL_SURFACE('',#105191,1.29);
#88668=CYLINDRICAL_SURFACE('',#105192,1.29);
#88669=CYLINDRICAL_SURFACE('',#105193,1.29);
#88670=CYLINDRICAL_SURFACE('',#105194,1.29);
#88671=CYLINDRICAL_SURFACE('',#105195,1.29);
#88672=CYLINDRICAL_SURFACE('',#105197,1.03775);
#88673=CYLINDRICAL_SURFACE('',#105199,1.03775);
#88674=CYLINDRICAL_SURFACE('',#105201,1.03775);
#88675=CYLINDRICAL_SURFACE('',#105202,1.03775);
#88676=CYLINDRICAL_SURFACE('',#105203,1.03775);
#88677=CYLINDRICAL_SURFACE('',#105204,1.03775);
#88678=CYLINDRICAL_SURFACE('',#105205,1.03775);
#88679=CYLINDRICAL_SURFACE('',#105206,1.03775);
#88680=CYLINDRICAL_SURFACE('',#105208,1.29);
#88681=CYLINDRICAL_SURFACE('',#105210,1.29);
#88682=CYLINDRICAL_SURFACE('',#105211,1.29);
#88683=CYLINDRICAL_SURFACE('',#105212,1.29);
#88684=CYLINDRICAL_SURFACE('',#105213,1.29);
#88685=CYLINDRICAL_SURFACE('',#105214,1.29);
#88686=CYLINDRICAL_SURFACE('',#105215,1.29);
#88687=CYLINDRICAL_SURFACE('',#105216,1.29);
#88688=CYLINDRICAL_SURFACE('',#105218,1.03775);
#88689=CYLINDRICAL_SURFACE('',#105220,1.03775);
#88690=CYLINDRICAL_SURFACE('',#105222,1.03775);
#88691=CYLINDRICAL_SURFACE('',#105223,1.03775);
#88692=CYLINDRICAL_SURFACE('',#105224,1.03775);
#88693=CYLINDRICAL_SURFACE('',#105225,1.03775);
#88694=CYLINDRICAL_SURFACE('',#105226,1.03775);
#88695=CYLINDRICAL_SURFACE('',#105227,1.03775);
#88696=CYLINDRICAL_SURFACE('',#105229,1.29);
#88697=CYLINDRICAL_SURFACE('',#105231,1.29);
#88698=CYLINDRICAL_SURFACE('',#105232,1.29);
#88699=CYLINDRICAL_SURFACE('',#105233,1.29);
#88700=CYLINDRICAL_SURFACE('',#105234,1.29);
#88701=CYLINDRICAL_SURFACE('',#105235,1.29);
#88702=CYLINDRICAL_SURFACE('',#105236,1.29);
#88703=CYLINDRICAL_SURFACE('',#105237,1.29);
#88704=CYLINDRICAL_SURFACE('',#105239,1.03775);
#88705=CYLINDRICAL_SURFACE('',#105241,1.03775);
#88706=CYLINDRICAL_SURFACE('',#105243,1.03775);
#88707=CYLINDRICAL_SURFACE('',#105244,1.03775);
#88708=CYLINDRICAL_SURFACE('',#105245,1.03775);
#88709=CYLINDRICAL_SURFACE('',#105246,1.03775);
#88710=CYLINDRICAL_SURFACE('',#105247,1.03775);
#88711=CYLINDRICAL_SURFACE('',#105248,1.03775);
#88712=CYLINDRICAL_SURFACE('',#105250,1.29);
#88713=CYLINDRICAL_SURFACE('',#105252,1.29);
#88714=CYLINDRICAL_SURFACE('',#105253,1.29);
#88715=CYLINDRICAL_SURFACE('',#105254,1.29);
#88716=CYLINDRICAL_SURFACE('',#105255,1.29);
#88717=CYLINDRICAL_SURFACE('',#105256,1.29);
#88718=CYLINDRICAL_SURFACE('',#105257,1.29);
#88719=CYLINDRICAL_SURFACE('',#105258,1.29);
#88720=CYLINDRICAL_SURFACE('',#105263,2.1);
#88721=CYLINDRICAL_SURFACE('',#105268,1.29);
#88722=CYLINDRICAL_SURFACE('',#105272,1.03775);
#88723=CYLINDRICAL_SURFACE('',#105273,9.8);
#88724=CYLINDRICAL_SURFACE('',#105278,3.5);
#88725=CYLINDRICAL_SURFACE('',#105280,10.5);
#88726=CYLINDRICAL_SURFACE('',#105282,10.5);
#88727=CYLINDRICAL_SURFACE('',#105284,4.95184441433916);
#88728=CYLINDRICAL_SURFACE('',#105286,10.5);
#88729=CYLINDRICAL_SURFACE('',#105289,5.08286386254677);
#88730=CYLINDRICAL_SURFACE('',#105292,10.5);
#88731=CYLINDRICAL_SURFACE('',#105295,5.21388331075437);
#88732=CYLINDRICAL_SURFACE('',#105298,10.5);
#88733=CYLINDRICAL_SURFACE('',#105301,5.34490275896198);
#88734=CYLINDRICAL_SURFACE('',#105304,10.5);
#88735=CYLINDRICAL_SURFACE('',#105307,5.47592220716958);
#88736=CYLINDRICAL_SURFACE('',#105310,10.5);
#88737=CYLINDRICAL_SURFACE('',#105313,5.60694165537719);
#88738=CYLINDRICAL_SURFACE('',#105316,10.5);
#88739=CYLINDRICAL_SURFACE('',#105319,5.73796110358479);
#88740=CYLINDRICAL_SURFACE('',#105322,10.5);
#88741=CYLINDRICAL_SURFACE('',#105325,5.8689805517924);
#88742=CYLINDRICAL_SURFACE('',#105328,10.5);
#88743=CYLINDRICAL_SURFACE('',#105331,6.);
#88744=CYLINDRICAL_SURFACE('',#105334,10.5);
#88745=CYLINDRICAL_SURFACE('',#105357,1.29);
#88746=CYLINDRICAL_SURFACE('',#105358,1.03775);
#88747=CYLINDRICAL_SURFACE('',#105359,1.29);
#88748=CYLINDRICAL_SURFACE('',#105360,1.03775);
#88749=CYLINDRICAL_SURFACE('',#105361,1.29);
#88750=CYLINDRICAL_SURFACE('',#105362,1.03775);
#88751=CYLINDRICAL_SURFACE('',#105364,3.442);
#88752=CYLINDRICAL_SURFACE('',#105366,3.442);
#88753=CYLINDRICAL_SURFACE('',#105367,3.442);
#88754=CYLINDRICAL_SURFACE('',#105368,3.442);
#88755=CYLINDRICAL_SURFACE('',#105369,3.442);
#88756=CYLINDRICAL_SURFACE('',#105370,3.442);
#88757=CYLINDRICAL_SURFACE('',#105371,3.442);
#88758=CYLINDRICAL_SURFACE('',#105372,3.442);
#88759=CYLINDRICAL_SURFACE('',#105373,3.442);
#88760=CYLINDRICAL_SURFACE('',#105374,3.442);
#88761=CYLINDRICAL_SURFACE('',#105375,2.872);
#88762=CYLINDRICAL_SURFACE('',#105377,2.872);
#88763=CYLINDRICAL_SURFACE('',#105379,2.872);
#88764=CYLINDRICAL_SURFACE('',#105380,2.872);
#88765=CYLINDRICAL_SURFACE('',#105381,2.872);
#88766=CYLINDRICAL_SURFACE('',#105382,2.872);
#88767=CYLINDRICAL_SURFACE('',#105383,2.872);
#88768=CYLINDRICAL_SURFACE('',#105384,2.872);
#88769=CYLINDRICAL_SURFACE('',#105385,2.872);
#88770=CYLINDRICAL_SURFACE('',#105386,2.872);
#88771=CYLINDRICAL_SURFACE('',#105387,2.942);
#88772=CYLINDRICAL_SURFACE('',#105389,2.942);
#88773=CYLINDRICAL_SURFACE('',#105390,2.942);
#88774=CYLINDRICAL_SURFACE('',#105391,2.942);
#88775=CYLINDRICAL_SURFACE('',#105392,2.942);
#88776=CYLINDRICAL_SURFACE('',#105393,2.37175);
#88777=CYLINDRICAL_SURFACE('',#105395,2.37175);
#88778=CYLINDRICAL_SURFACE('',#105396,2.37175);
#88779=CYLINDRICAL_SURFACE('',#105397,2.37175);
#88780=CYLINDRICAL_SURFACE('',#105398,2.37175);
#88781=CYLINDRICAL_SURFACE('',#105399,2.37175);
#88782=CYLINDRICAL_SURFACE('',#105404,2.942);
#88783=CYLINDRICAL_SURFACE('',#105408,2.872);
#88784=CYLINDRICAL_SURFACE('',#105414,1.4);
#88785=CYLINDRICAL_SURFACE('',#105416,3.442);
#88786=CYLINDRICAL_SURFACE('',#105418,3.);
#88787=CYLINDRICAL_SURFACE('',#105420,2.1);
#88788=CYLINDRICAL_SURFACE('',#105425,1.);
#88789=CYLINDRICAL_SURFACE('',#105435,1.);
#88790=CYLINDRICAL_SURFACE('',#105437,2.);
#88791=CYLINDRICAL_SURFACE('',#105441,2.942);
#88792=CYLINDRICAL_SURFACE('',#105443,2.942);
#88793=CYLINDRICAL_SURFACE('',#105444,2.942);
#88794=CYLINDRICAL_SURFACE('',#105445,2.942);
#88795=CYLINDRICAL_SURFACE('',#105446,2.942);
#88796=CYLINDRICAL_SURFACE('',#105447,2.942);
#88797=CYLINDRICAL_SURFACE('',#105448,2.37175);
#88798=CYLINDRICAL_SURFACE('',#105450,2.37175);
#88799=CYLINDRICAL_SURFACE('',#105451,2.37175);
#88800=CYLINDRICAL_SURFACE('',#105452,2.37175);
#88801=CYLINDRICAL_SURFACE('',#105453,2.37175);
#88802=CYLINDRICAL_SURFACE('',#105454,2.37175);
#88803=CYLINDRICAL_SURFACE('',#105458,2.37175);
#88804=CYLINDRICAL_SURFACE('',#105465,2.942);
#88805=CYLINDRICAL_SURFACE('',#105470,0.75);
#88806=CYLINDRICAL_SURFACE('',#105477,2.5);
#88807=CYLINDRICAL_SURFACE('',#105482,1.);
#88808=CYLINDRICAL_SURFACE('',#105483,0.2);
#88809=CYLINDRICAL_SURFACE('',#105495,3.);
#88810=CYLINDRICAL_SURFACE('',#105498,1.5);
#88811=CYLINDRICAL_SURFACE('',#105501,1.5);
#88812=CYLINDRICAL_SURFACE('',#105504,0.750000000000001);
#88813=CYLINDRICAL_SURFACE('',#105507,1.5);
#88814=CYLINDRICAL_SURFACE('',#105510,3.);
#88815=ADVANCED_FACE('',(#6351),#87052,.F.);
#88816=ADVANCED_FACE('',(#6352),#87053,.F.);
#88817=ADVANCED_FACE('',(#6353),#87054,.F.);
#88818=ADVANCED_FACE('',(#6354),#87055,.F.);
#88819=ADVANCED_FACE('',(#6355),#87056,.F.);
#88820=ADVANCED_FACE('',(#6356),#87057,.F.);
#88821=ADVANCED_FACE('',(#6357),#87058,.F.);
#88822=ADVANCED_FACE('',(#6358),#87059,.F.);
#88823=ADVANCED_FACE('',(#6359),#87060,.F.);
#88824=ADVANCED_FACE('',(#6360),#87061,.F.);
#88825=ADVANCED_FACE('',(#6361),#87062,.F.);
#88826=ADVANCED_FACE('',(#6362),#87063,.F.);
#88827=ADVANCED_FACE('',(#6363),#87064,.F.);
#88828=ADVANCED_FACE('',(#6364),#87065,.F.);
#88829=ADVANCED_FACE('',(#6365),#87066,.F.);
#88830=ADVANCED_FACE('',(#6366),#87067,.F.);
#88831=ADVANCED_FACE('',(#6367),#87068,.F.);
#88832=ADVANCED_FACE('',(#6368),#87069,.F.);
#88833=ADVANCED_FACE('',(#6369),#87070,.F.);
#88834=ADVANCED_FACE('',(#6370),#87071,.F.);
#88835=ADVANCED_FACE('',(#6371),#6181,.F.);
#88836=ADVANCED_FACE('',(#6372),#6182,.F.);
#88837=ADVANCED_FACE('',(#6373,#5113),#5278,.T.);
#88838=ADVANCED_FACE('',(#6374),#6183,.F.);
#88839=ADVANCED_FACE('',(#6375),#6184,.F.);
#88840=ADVANCED_FACE('',(#6376,#5114),#5279,.T.);
#88841=ADVANCED_FACE('',(#6377),#4614,.T.);
#88842=ADVANCED_FACE('',(#6378),#87072,.T.);
#88843=ADVANCED_FACE('',(#6379,#5115),#5280,.F.);
#88844=ADVANCED_FACE('',(#6380),#4615,.T.);
#88845=ADVANCED_FACE('',(#6381),#87073,.T.);
#88846=ADVANCED_FACE('',(#6382,#5116),#5281,.F.);
#88847=ADVANCED_FACE('',(#6383),#4616,.T.);
#88848=ADVANCED_FACE('',(#6384),#87074,.T.);
#88849=ADVANCED_FACE('',(#6385,#5117),#5282,.T.);
#88850=ADVANCED_FACE('',(#6386),#4617,.F.);
#88851=ADVANCED_FACE('',(#6387,#5118),#5283,.T.);
#88852=ADVANCED_FACE('',(#6388),#87075,.F.);
#88853=ADVANCED_FACE('',(#6389),#4618,.T.);
#88854=ADVANCED_FACE('',(#6390),#4619,.F.);
#88855=ADVANCED_FACE('',(#6391),#5284,.T.);
#88856=ADVANCED_FACE('',(#6392),#4620,.T.);
#88857=ADVANCED_FACE('',(#6393),#5285,.T.);
#88858=ADVANCED_FACE('',(#6394),#4621,.F.);
#88859=ADVANCED_FACE('',(#6395),#4622,.F.);
#88860=ADVANCED_FACE('',(#6396),#5286,.T.);
#88861=ADVANCED_FACE('',(#6397),#4623,.T.);
#88862=ADVANCED_FACE('',(#6398),#5287,.T.);
#88863=ADVANCED_FACE('',(#6399),#4624,.F.);
#88864=ADVANCED_FACE('',(#6400),#5288,.T.);
#88865=ADVANCED_FACE('',(#6401),#4625,.T.);
#88866=ADVANCED_FACE('',(#6402),#5289,.T.);
#88867=ADVANCED_FACE('',(#6403),#4626,.F.);
#88868=ADVANCED_FACE('',(#6404),#4627,.T.);
#88869=ADVANCED_FACE('',(#6405),#4628,.F.);
#88870=ADVANCED_FACE('',(#6406),#5290,.T.);
#88871=ADVANCED_FACE('',(#6407),#4629,.T.);
#88872=ADVANCED_FACE('',(#6408),#5291,.T.);
#88873=ADVANCED_FACE('',(#6409),#4630,.F.);
#88874=ADVANCED_FACE('',(#6410),#4631,.T.);
#88875=ADVANCED_FACE('',(#6411),#4632,.F.);
#88876=ADVANCED_FACE('',(#6412),#87076,.T.);
#88877=ADVANCED_FACE('',(#6413),#5292,.T.);
#88878=ADVANCED_FACE('',(#6414),#87077,.F.);
#88879=ADVANCED_FACE('',(#6415),#87078,.F.);
#88880=ADVANCED_FACE('',(#6416),#5293,.T.);
#88881=ADVANCED_FACE('',(#6417,#5119,#5120,#5121),#5294,.F.);
#88882=ADVANCED_FACE('',(#6418),#87079,.F.);
#88883=ADVANCED_FACE('',(#6419),#87080,.F.);
#88884=ADVANCED_FACE('',(#6420),#5295,.T.);
#88885=ADVANCED_FACE('',(#6421),#4633,.F.);
#88886=ADVANCED_FACE('',(#6422),#87081,.F.);
#88887=ADVANCED_FACE('',(#6423,#5122),#5296,.T.);
#88888=ADVANCED_FACE('',(#6424),#5297,.T.);
#88889=ADVANCED_FACE('',(#6425,#5123),#5298,.F.);
#88890=ADVANCED_FACE('',(#6426),#5299,.T.);
#88891=ADVANCED_FACE('',(#6427),#6185,.T.);
#88892=ADVANCED_FACE('',(#6428),#87082,.T.);
#88893=ADVANCED_FACE('',(#6429),#6186,.T.);
#88894=ADVANCED_FACE('',(#6430),#5300,.T.);
#88895=ADVANCED_FACE('',(#6431),#87083,.T.);
#88896=ADVANCED_FACE('',(#6432),#87084,.T.);
#88897=ADVANCED_FACE('',(#6433),#5301,.T.);
#88898=ADVANCED_FACE('',(#6434),#6187,.T.);
#88899=ADVANCED_FACE('',(#6435),#87085,.T.);
#88900=ADVANCED_FACE('',(#6436),#6188,.T.);
#88901=ADVANCED_FACE('',(#6437),#5302,.T.);
#88902=ADVANCED_FACE('',(#6438),#87086,.T.);
#88903=ADVANCED_FACE('',(#6439),#5303,.T.);
#88904=ADVANCED_FACE('',(#6440),#6189,.T.);
#88905=ADVANCED_FACE('',(#6441),#87087,.T.);
#88906=ADVANCED_FACE('',(#6442),#6190,.T.);
#88907=ADVANCED_FACE('',(#6443),#5304,.T.);
#88908=ADVANCED_FACE('',(#6444),#87088,.T.);
#88909=ADVANCED_FACE('',(#6445),#5305,.T.);
#88910=ADVANCED_FACE('',(#6446),#6191,.T.);
#88911=ADVANCED_FACE('',(#6447),#87089,.T.);
#88912=ADVANCED_FACE('',(#6448),#6192,.T.);
#88913=ADVANCED_FACE('',(#6449),#5306,.T.);
#88914=ADVANCED_FACE('',(#6450),#87090,.T.);
#88915=ADVANCED_FACE('',(#6451),#5307,.T.);
#88916=ADVANCED_FACE('',(#6452),#6193,.T.);
#88917=ADVANCED_FACE('',(#6453),#87091,.T.);
#88918=ADVANCED_FACE('',(#6454),#6194,.T.);
#88919=ADVANCED_FACE('',(#6455),#5308,.T.);
#88920=ADVANCED_FACE('',(#6456),#87092,.T.);
#88921=ADVANCED_FACE('',(#6457),#5309,.T.);
#88922=ADVANCED_FACE('',(#6458),#6195,.T.);
#88923=ADVANCED_FACE('',(#6459),#87093,.T.);
#88924=ADVANCED_FACE('',(#6460),#6196,.T.);
#88925=ADVANCED_FACE('',(#6461),#5310,.T.);
#88926=ADVANCED_FACE('',(#6462),#87094,.T.);
#88927=ADVANCED_FACE('',(#6463),#5311,.T.);
#88928=ADVANCED_FACE('',(#6464),#6197,.T.);
#88929=ADVANCED_FACE('',(#6465),#87095,.T.);
#88930=ADVANCED_FACE('',(#6466),#6198,.T.);
#88931=ADVANCED_FACE('',(#6467),#5312,.T.);
#88932=ADVANCED_FACE('',(#6468),#87096,.T.);
#88933=ADVANCED_FACE('',(#6469),#5313,.T.);
#88934=ADVANCED_FACE('',(#6470),#6199,.T.);
#88935=ADVANCED_FACE('',(#6471),#87097,.T.);
#88936=ADVANCED_FACE('',(#6472),#6200,.T.);
#88937=ADVANCED_FACE('',(#6473),#5314,.T.);
#88938=ADVANCED_FACE('',(#6474),#87098,.T.);
#88939=ADVANCED_FACE('',(#6475),#5315,.T.);
#88940=ADVANCED_FACE('',(#6476),#6201,.T.);
#88941=ADVANCED_FACE('',(#6477),#87099,.T.);
#88942=ADVANCED_FACE('',(#6478),#6202,.T.);
#88943=ADVANCED_FACE('',(#6479),#5316,.T.);
#88944=ADVANCED_FACE('',(#6480),#87100,.T.);
#88945=ADVANCED_FACE('',(#6481),#5317,.T.);
#88946=ADVANCED_FACE('',(#6482),#6203,.T.);
#88947=ADVANCED_FACE('',(#6483),#87101,.T.);
#88948=ADVANCED_FACE('',(#6484),#6204,.T.);
#88949=ADVANCED_FACE('',(#6485),#5318,.T.);
#88950=ADVANCED_FACE('',(#6486),#4634,.T.);
#88951=ADVANCED_FACE('',(#6487),#4635,.T.);
#88952=ADVANCED_FACE('',(#6488),#87102,.T.);
#88953=ADVANCED_FACE('',(#6489),#87103,.T.);
#88954=ADVANCED_FACE('',(#6490),#4636,.T.);
#88955=ADVANCED_FACE('',(#6491),#4637,.T.);
#88956=ADVANCED_FACE('',(#6492),#87104,.T.);
#88957=ADVANCED_FACE('',(#6493),#4638,.T.);
#88958=ADVANCED_FACE('',(#6494),#4639,.T.);
#88959=ADVANCED_FACE('',(#6495),#87105,.T.);
#88960=ADVANCED_FACE('',(#6496),#4640,.T.);
#88961=ADVANCED_FACE('',(#6497),#4641,.T.);
#88962=ADVANCED_FACE('',(#6498),#87106,.T.);
#88963=ADVANCED_FACE('',(#6499),#4642,.T.);
#88964=ADVANCED_FACE('',(#6500),#4643,.T.);
#88965=ADVANCED_FACE('',(#6501),#87107,.T.);
#88966=ADVANCED_FACE('',(#6502),#4644,.T.);
#88967=ADVANCED_FACE('',(#6503),#4645,.T.);
#88968=ADVANCED_FACE('',(#6504),#87108,.T.);
#88969=ADVANCED_FACE('',(#6505),#4646,.T.);
#88970=ADVANCED_FACE('',(#6506),#4647,.T.);
#88971=ADVANCED_FACE('',(#6507),#87109,.T.);
#88972=ADVANCED_FACE('',(#6508),#4648,.T.);
#88973=ADVANCED_FACE('',(#6509),#4649,.T.);
#88974=ADVANCED_FACE('',(#6510),#87110,.T.);
#88975=ADVANCED_FACE('',(#6511),#4650,.T.);
#88976=ADVANCED_FACE('',(#6512),#4651,.T.);
#88977=ADVANCED_FACE('',(#6513),#87111,.T.);
#88978=ADVANCED_FACE('',(#6514),#4652,.T.);
#88979=ADVANCED_FACE('',(#6515),#4653,.T.);
#88980=ADVANCED_FACE('',(#6516),#87112,.T.);
#88981=ADVANCED_FACE('',(#6517),#4654,.T.);
#88982=ADVANCED_FACE('',(#6518),#4655,.T.);
#88983=ADVANCED_FACE('',(#6519),#87113,.T.);
#88984=ADVANCED_FACE('',(#6520),#4656,.T.);
#88985=ADVANCED_FACE('',(#6521),#4657,.T.);
#88986=ADVANCED_FACE('',(#6522),#87114,.T.);
#88987=ADVANCED_FACE('',(#6523),#4658,.T.);
#88988=ADVANCED_FACE('',(#6524),#4659,.T.);
#88989=ADVANCED_FACE('',(#6525),#87115,.T.);
#88990=ADVANCED_FACE('',(#6526),#4660,.T.);
#88991=ADVANCED_FACE('',(#6527),#4661,.T.);
#88992=ADVANCED_FACE('',(#6528),#87116,.T.);
#88993=ADVANCED_FACE('',(#6529),#87117,.T.);
#88994=ADVANCED_FACE('',(#6530),#4662,.T.);
#88995=ADVANCED_FACE('',(#6531),#4663,.T.);
#88996=ADVANCED_FACE('',(#6532),#87118,.T.);
#88997=ADVANCED_FACE('',(#6533),#87119,.T.);
#88998=ADVANCED_FACE('',(#6534),#5319,.T.);
#88999=ADVANCED_FACE('',(#6535),#5320,.T.);
#89000=ADVANCED_FACE('',(#6536),#5321,.T.);
#89001=ADVANCED_FACE('',(#6537),#5322,.T.);
#89002=ADVANCED_FACE('',(#6538),#5323,.T.);
#89003=ADVANCED_FACE('',(#6539),#4664,.T.);
#89004=ADVANCED_FACE('',(#6540),#4665,.T.);
#89005=ADVANCED_FACE('',(#6541),#4666,.T.);
#89006=ADVANCED_FACE('',(#6542),#4667,.T.);
#89007=ADVANCED_FACE('',(#6543),#4668,.T.);
#89008=ADVANCED_FACE('',(#6544),#4669,.T.);
#89009=ADVANCED_FACE('',(#6545),#5324,.T.);
#89010=ADVANCED_FACE('',(#6546),#5325,.T.);
#89011=ADVANCED_FACE('',(#6547),#5326,.T.);
#89012=ADVANCED_FACE('',(#6548),#87120,.F.);
#89013=ADVANCED_FACE('',(#6549),#5327,.T.);
#89014=ADVANCED_FACE('',(#6550),#4670,.T.);
#89015=ADVANCED_FACE('',(#6551),#4671,.T.);
#89016=ADVANCED_FACE('',(#6552),#5328,.T.);
#89017=ADVANCED_FACE('',(#6553),#87121,.T.);
#89018=ADVANCED_FACE('',(#6554,#5124),#5329,.T.);
#89019=ADVANCED_FACE('',(#6555),#87122,.T.);
#89020=ADVANCED_FACE('',(#6556,#5125),#5330,.T.);
#89021=ADVANCED_FACE('',(#6557),#5331,.F.);
#89022=ADVANCED_FACE('',(#6558),#5332,.F.);
#89023=ADVANCED_FACE('',(#6559),#5333,.T.);
#89024=ADVANCED_FACE('',(#6560),#5334,.F.);
#89025=ADVANCED_FACE('',(#6561),#5335,.F.);
#89026=ADVANCED_FACE('',(#6562),#5336,.T.);
#89027=ADVANCED_FACE('',(#6563),#5337,.F.);
#89028=ADVANCED_FACE('',(#6564),#5338,.F.);
#89029=ADVANCED_FACE('',(#6565),#5339,.T.);
#89030=ADVANCED_FACE('',(#6566),#5340,.F.);
#89031=ADVANCED_FACE('',(#6567),#5341,.F.);
#89032=ADVANCED_FACE('',(#6568),#5342,.T.);
#89033=ADVANCED_FACE('',(#6569),#87123,.T.);
#89034=ADVANCED_FACE('',(#6570),#5343,.T.);
#89035=ADVANCED_FACE('',(#6571),#5344,.F.);
#89036=ADVANCED_FACE('',(#6572),#87124,.T.);
#89037=ADVANCED_FACE('',(#6573),#87125,.T.);
#89038=ADVANCED_FACE('',(#6574),#87126,.T.);
#89039=ADVANCED_FACE('',(#6575),#87127,.F.);
#89040=ADVANCED_FACE('',(#6576),#87128,.T.);
#89041=ADVANCED_FACE('',(#6577),#87129,.T.);
#89042=ADVANCED_FACE('',(#6578),#5345,.T.);
#89043=ADVANCED_FACE('',(#6579),#5346,.T.);
#89044=ADVANCED_FACE('',(#6580),#5347,.T.);
#89045=ADVANCED_FACE('',(#6581),#5348,.T.);
#89046=ADVANCED_FACE('',(#6582),#5349,.T.);
#89047=ADVANCED_FACE('',(#6583),#5350,.T.);
#89048=ADVANCED_FACE('',(#6584),#5351,.T.);
#89049=ADVANCED_FACE('',(#6585),#87130,.F.);
#89050=ADVANCED_FACE('',(#6586),#2221,.T.);
#89051=ADVANCED_FACE('',(#6587),#1621,.F.);
#89052=ADVANCED_FACE('',(#6588),#2222,.T.);
#89053=ADVANCED_FACE('',(#6589),#1622,.F.);
#89054=ADVANCED_FACE('',(#6590),#2223,.T.);
#89055=ADVANCED_FACE('',(#6591),#1623,.F.);
#89056=ADVANCED_FACE('',(#6592),#2224,.T.);
#89057=ADVANCED_FACE('',(#6593),#87131,.F.);
#89058=ADVANCED_FACE('',(#6594),#2225,.T.);
#89059=ADVANCED_FACE('',(#6595),#87132,.F.);
#89060=ADVANCED_FACE('',(#6596),#87133,.F.);
#89061=ADVANCED_FACE('',(#6597),#5352,.T.);
#89062=ADVANCED_FACE('',(#6598),#87134,.F.);
#89063=ADVANCED_FACE('',(#6599),#5353,.T.);
#89064=ADVANCED_FACE('',(#6600),#5354,.T.);
#89065=ADVANCED_FACE('',(#6601),#87135,.F.);
#89066=ADVANCED_FACE('',(#6602),#2226,.T.);
#89067=ADVANCED_FACE('',(#6603),#1624,.F.);
#89068=ADVANCED_FACE('',(#6604),#2227,.T.);
#89069=ADVANCED_FACE('',(#6605),#87136,.F.);
#89070=ADVANCED_FACE('',(#6606),#2228,.T.);
#89071=ADVANCED_FACE('',(#6607),#87137,.F.);
#89072=ADVANCED_FACE('',(#6608),#1625,.F.);
#89073=ADVANCED_FACE('',(#6609),#87138,.F.);
#89074=ADVANCED_FACE('',(#6610),#2229,.T.);
#89075=ADVANCED_FACE('',(#6611),#1626,.F.);
#89076=ADVANCED_FACE('',(#6612),#2230,.T.);
#89077=ADVANCED_FACE('',(#6613),#1627,.F.);
#89078=ADVANCED_FACE('',(#6614),#2231,.T.);
#89079=ADVANCED_FACE('',(#6615),#5355,.T.);
#89080=ADVANCED_FACE('',(#6616),#87139,.F.);
#89081=ADVANCED_FACE('',(#6617),#87140,.T.);
#89082=ADVANCED_FACE('',(#6618),#87141,.F.);
#89083=ADVANCED_FACE('',(#6619),#87142,.T.);
#89084=ADVANCED_FACE('',(#6620),#87143,.F.);
#89085=ADVANCED_FACE('',(#6621),#5356,.F.);
#89086=ADVANCED_FACE('',(#6622),#5357,.F.);
#89087=ADVANCED_FACE('',(#6623),#1628,.F.);
#89088=ADVANCED_FACE('',(#6624),#2232,.T.);
#89089=ADVANCED_FACE('',(#6625),#87144,.F.);
#89090=ADVANCED_FACE('',(#6626),#2233,.T.);
#89091=ADVANCED_FACE('',(#6627),#87145,.F.);
#89092=ADVANCED_FACE('',(#6628),#2234,.T.);
#89093=ADVANCED_FACE('',(#6629),#1629,.F.);
#89094=ADVANCED_FACE('',(#6630),#2235,.T.);
#89095=ADVANCED_FACE('',(#6631),#87146,.F.);
#89096=ADVANCED_FACE('',(#6632),#2236,.T.);
#89097=ADVANCED_FACE('',(#6633),#1630,.F.);
#89098=ADVANCED_FACE('',(#6634),#2237,.T.);
#89099=ADVANCED_FACE('',(#6635),#87147,.F.);
#89100=ADVANCED_FACE('',(#6636),#5358,.F.);
#89101=ADVANCED_FACE('',(#6637),#87148,.F.);
#89102=ADVANCED_FACE('',(#6638),#87149,.F.);
#89103=ADVANCED_FACE('',(#6639),#87150,.T.);
#89104=ADVANCED_FACE('',(#6640),#5359,.F.);
#89105=ADVANCED_FACE('',(#6641),#87151,.F.);
#89106=ADVANCED_FACE('',(#6642),#2238,.T.);
#89107=ADVANCED_FACE('',(#6643),#1631,.F.);
#89108=ADVANCED_FACE('',(#6644),#2239,.T.);
#89109=ADVANCED_FACE('',(#6645),#1632,.F.);
#89110=ADVANCED_FACE('',(#6646),#1633,.F.);
#89111=ADVANCED_FACE('',(#6647),#87152,.F.);
#89112=ADVANCED_FACE('',(#6648),#1634,.F.);
#89113=ADVANCED_FACE('',(#6649),#2240,.T.);
#89114=ADVANCED_FACE('',(#6650),#87153,.F.);
#89115=ADVANCED_FACE('',(#6651),#2241,.T.);
#89116=ADVANCED_FACE('',(#6652),#5360,.F.);
#89117=ADVANCED_FACE('',(#6653),#87154,.T.);
#89118=ADVANCED_FACE('',(#6654),#87155,.F.);
#89119=ADVANCED_FACE('',(#6655),#5361,.F.);
#89120=ADVANCED_FACE('',(#6656),#87156,.F.);
#89121=ADVANCED_FACE('',(#6657),#5362,.F.);
#89122=ADVANCED_FACE('',(#6658),#5363,.T.);
#89123=ADVANCED_FACE('',(#6659),#1635,.F.);
#89124=ADVANCED_FACE('',(#6660),#2242,.T.);
#89125=ADVANCED_FACE('',(#6661),#1636,.F.);
#89126=ADVANCED_FACE('',(#6662),#1637,.F.);
#89127=ADVANCED_FACE('',(#6663),#2243,.T.);
#89128=ADVANCED_FACE('',(#6664),#87157,.F.);
#89129=ADVANCED_FACE('',(#6665),#1638,.F.);
#89130=ADVANCED_FACE('',(#6666),#87158,.F.);
#89131=ADVANCED_FACE('',(#6667),#2244,.T.);
#89132=ADVANCED_FACE('',(#6668),#87159,.F.);
#89133=ADVANCED_FACE('',(#6669),#2245,.T.);
#89134=ADVANCED_FACE('',(#6670),#1639,.F.);
#89135=ADVANCED_FACE('',(#6671),#2246,.T.);
#89136=ADVANCED_FACE('',(#6672),#87160,.F.);
#89137=ADVANCED_FACE('',(#6673),#87161,.F.);
#89138=ADVANCED_FACE('',(#6674),#5364,.F.);
#89139=ADVANCED_FACE('',(#6675),#87162,.F.);
#89140=ADVANCED_FACE('',(#6676),#87163,.T.);
#89141=ADVANCED_FACE('',(#6677),#87164,.F.);
#89142=ADVANCED_FACE('',(#6678),#5365,.F.);
#89143=ADVANCED_FACE('',(#6679),#87165,.T.);
#89144=ADVANCED_FACE('',(#6680),#5366,.T.);
#89145=ADVANCED_FACE('',(#6681),#1640,.F.);
#89146=ADVANCED_FACE('',(#6682),#1641,.F.);
#89147=ADVANCED_FACE('',(#6683),#2247,.T.);
#89148=ADVANCED_FACE('',(#6684),#1642,.F.);
#89149=ADVANCED_FACE('',(#6685),#2248,.T.);
#89150=ADVANCED_FACE('',(#6686),#1643,.F.);
#89151=ADVANCED_FACE('',(#6687),#2249,.T.);
#89152=ADVANCED_FACE('',(#6688),#87166,.F.);
#89153=ADVANCED_FACE('',(#6689),#2250,.T.);
#89154=ADVANCED_FACE('',(#6690),#87167,.F.);
#89155=ADVANCED_FACE('',(#6691),#87168,.F.);
#89156=ADVANCED_FACE('',(#6692),#5367,.T.);
#89157=ADVANCED_FACE('',(#6693),#87169,.F.);
#89158=ADVANCED_FACE('',(#6694),#87170,.T.);
#89159=ADVANCED_FACE('',(#6695),#5368,.T.);
#89160=ADVANCED_FACE('',(#6696),#1644,.F.);
#89161=ADVANCED_FACE('',(#6697),#2251,.T.);
#89162=ADVANCED_FACE('',(#6698),#1645,.F.);
#89163=ADVANCED_FACE('',(#6699),#1646,.F.);
#89164=ADVANCED_FACE('',(#6700),#1647,.F.);
#89165=ADVANCED_FACE('',(#6701),#2252,.T.);
#89166=ADVANCED_FACE('',(#6702),#87171,.F.);
#89167=ADVANCED_FACE('',(#6703),#2253,.T.);
#89168=ADVANCED_FACE('',(#6704),#87172,.F.);
#89169=ADVANCED_FACE('',(#6705),#2254,.T.);
#89170=ADVANCED_FACE('',(#6706),#87173,.F.);
#89171=ADVANCED_FACE('',(#6707),#2255,.T.);
#89172=ADVANCED_FACE('',(#6708),#1648,.F.);
#89173=ADVANCED_FACE('',(#6709),#2256,.T.);
#89174=ADVANCED_FACE('',(#6710),#1649,.F.);
#89175=ADVANCED_FACE('',(#6711),#2257,.T.);
#89176=ADVANCED_FACE('',(#6712),#87174,.F.);
#89177=ADVANCED_FACE('',(#6713),#5369,.T.);
#89178=ADVANCED_FACE('',(#6714),#87175,.F.);
#89179=ADVANCED_FACE('',(#6715),#87176,.T.);
#89180=ADVANCED_FACE('',(#6716),#87177,.F.);
#89181=ADVANCED_FACE('',(#6717),#87178,.T.);
#89182=ADVANCED_FACE('',(#6718),#87179,.F.);
#89183=ADVANCED_FACE('',(#6719),#87180,.T.);
#89184=ADVANCED_FACE('',(#6720),#5370,.T.);
#89185=ADVANCED_FACE('',(#6721),#1650,.F.);
#89186=ADVANCED_FACE('',(#6722),#2258,.T.);
#89187=ADVANCED_FACE('',(#6723),#1651,.F.);
#89188=ADVANCED_FACE('',(#6724),#87181,.F.);
#89189=ADVANCED_FACE('',(#6725),#2259,.T.);
#89190=ADVANCED_FACE('',(#6726),#1652,.F.);
#89191=ADVANCED_FACE('',(#6727),#2260,.T.);
#89192=ADVANCED_FACE('',(#6728),#1653,.F.);
#89193=ADVANCED_FACE('',(#6729),#2261,.T.);
#89194=ADVANCED_FACE('',(#6730),#87182,.F.);
#89195=ADVANCED_FACE('',(#6731),#87183,.F.);
#89196=ADVANCED_FACE('',(#6732),#87184,.T.);
#89197=ADVANCED_FACE('',(#6733),#87185,.F.);
#89198=ADVANCED_FACE('',(#6734),#87186,.T.);
#89199=ADVANCED_FACE('',(#6735),#5371,.T.);
#89200=ADVANCED_FACE('',(#6736),#87187,.F.);
#89201=ADVANCED_FACE('',(#6737),#2262,.T.);
#89202=ADVANCED_FACE('',(#6738),#87188,.F.);
#89203=ADVANCED_FACE('',(#6739),#2263,.T.);
#89204=ADVANCED_FACE('',(#6740),#1654,.F.);
#89205=ADVANCED_FACE('',(#6741),#2264,.T.);
#89206=ADVANCED_FACE('',(#6742),#1655,.F.);
#89207=ADVANCED_FACE('',(#6743),#2265,.T.);
#89208=ADVANCED_FACE('',(#6744),#87189,.F.);
#89209=ADVANCED_FACE('',(#6745),#87190,.T.);
#89210=ADVANCED_FACE('',(#6746),#87191,.F.);
#89211=ADVANCED_FACE('',(#6747),#5372,.F.);
#89212=ADVANCED_FACE('',(#6748),#5373,.T.);
#89213=ADVANCED_FACE('',(#6749),#6205,.T.);
#89214=ADVANCED_FACE('',(#6750),#6206,.T.);
#89215=ADVANCED_FACE('',(#6751),#6207,.T.);
#89216=ADVANCED_FACE('',(#6752),#87192,.T.);
#89217=ADVANCED_FACE('',(#6753),#87193,.F.);
#89218=ADVANCED_FACE('',(#6754),#4672,.T.);
#89219=ADVANCED_FACE('',(#6755),#87194,.T.);
#89220=ADVANCED_FACE('',(#6756),#5374,.T.);
#89221=ADVANCED_FACE('',(#6757),#5375,.F.);
#89222=ADVANCED_FACE('',(#6758),#87195,.T.);
#89223=ADVANCED_FACE('',(#6759,#5126),#5376,.T.);
#89224=ADVANCED_FACE('',(#6760),#87196,.F.);
#89225=ADVANCED_FACE('',(#6761,#5127,#5128),#5377,.T.);
#89226=ADVANCED_FACE('',(#6762),#5378,.T.);
#89227=ADVANCED_FACE('',(#6763),#87197,.T.);
#89228=ADVANCED_FACE('',(#6764),#5379,.F.);
#89229=ADVANCED_FACE('',(#6765,#5129,#5130,#5131,#5132,#5133),#5380,.F.);
#89230=ADVANCED_FACE('',(#6766),#87198,.F.);
#89231=ADVANCED_FACE('',(#6767),#5381,.F.);
#89232=ADVANCED_FACE('',(#6768),#87199,.F.);
#89233=ADVANCED_FACE('',(#6769),#87200,.T.);
#89234=ADVANCED_FACE('',(#6770),#5382,.F.);
#89235=ADVANCED_FACE('',(#6771),#5383,.T.);
#89236=ADVANCED_FACE('',(#6772),#87201,.T.);
#89237=ADVANCED_FACE('',(#6773),#5384,.F.);
#89238=ADVANCED_FACE('',(#6774),#87202,.T.);
#89239=ADVANCED_FACE('',(#6775,#5134),#5385,.T.);
#89240=ADVANCED_FACE('',(#6776),#87203,.F.);
#89241=ADVANCED_FACE('',(#6777),#87204,.T.);
#89242=ADVANCED_FACE('',(#6778),#5386,.F.);
#89243=ADVANCED_FACE('',(#6779),#5387,.F.);
#89244=ADVANCED_FACE('',(#6780),#87205,.T.);
#89245=ADVANCED_FACE('',(#6781),#87206,.F.);
#89246=ADVANCED_FACE('',(#6782),#87207,.F.);
#89247=ADVANCED_FACE('',(#6783),#5388,.T.);
#89248=ADVANCED_FACE('',(#6784),#87208,.T.);
#89249=ADVANCED_FACE('',(#6785),#5389,.T.);
#89250=ADVANCED_FACE('',(#6786),#87209,.F.);
#89251=ADVANCED_FACE('',(#6787),#87210,.T.);
#89252=ADVANCED_FACE('',(#6788),#87211,.F.);
#89253=ADVANCED_FACE('',(#6789),#87212,.F.);
#89254=ADVANCED_FACE('',(#6790),#87213,.T.);
#89255=ADVANCED_FACE('',(#6791),#87214,.T.);
#89256=ADVANCED_FACE('',(#6792),#87215,.F.);
#89257=ADVANCED_FACE('',(#6793),#5390,.F.);
#89258=ADVANCED_FACE('',(#6794),#87216,.F.);
#89259=ADVANCED_FACE('',(#6795),#5391,.F.);
#89260=ADVANCED_FACE('',(#6796),#5392,.T.);
#89261=ADVANCED_FACE('',(#6797),#87217,.T.);
#89262=ADVANCED_FACE('',(#6798),#87218,.F.);
#89263=ADVANCED_FACE('',(#6799),#5393,.T.);
#89264=ADVANCED_FACE('',(#6800),#87219,.F.);
#89265=ADVANCED_FACE('',(#6801),#5394,.T.);
#89266=ADVANCED_FACE('',(#6802),#87220,.T.);
#89267=ADVANCED_FACE('',(#6803),#87221,.F.);
#89268=ADVANCED_FACE('',(#6804),#87222,.T.);
#89269=ADVANCED_FACE('',(#6805),#87223,.F.);
#89270=ADVANCED_FACE('',(#6806),#87224,.F.);
#89271=ADVANCED_FACE('',(#6807),#87225,.T.);
#89272=ADVANCED_FACE('',(#6808),#5395,.F.);
#89273=ADVANCED_FACE('',(#6809),#4673,.F.);
#89274=ADVANCED_FACE('',(#6810),#5396,.T.);
#89275=ADVANCED_FACE('',(#6811),#5397,.T.);
#89276=ADVANCED_FACE('',(#6812),#87226,.T.);
#89277=ADVANCED_FACE('',(#6813),#5398,.T.);
#89278=ADVANCED_FACE('',(#6814),#87227,.F.);
#89279=ADVANCED_FACE('',(#6815),#87228,.F.);
#89280=ADVANCED_FACE('',(#6816),#87229,.F.);
#89281=ADVANCED_FACE('',(#6817,#5135),#5399,.T.);
#89282=ADVANCED_FACE('',(#6818),#87230,.T.);
#89283=ADVANCED_FACE('',(#6819),#87231,.F.);
#89284=ADVANCED_FACE('',(#6820),#5400,.T.);
#89285=ADVANCED_FACE('',(#6821),#87232,.F.);
#89286=ADVANCED_FACE('',(#6822),#87233,.F.);
#89287=ADVANCED_FACE('',(#6823),#87234,.T.);
#89288=ADVANCED_FACE('',(#6824),#5401,.F.);
#89289=ADVANCED_FACE('',(#6825),#87235,.F.);
#89290=ADVANCED_FACE('',(#6826),#87236,.T.);
#89291=ADVANCED_FACE('',(#6827),#87237,.F.);
#89292=ADVANCED_FACE('',(#6828),#87238,.T.);
#89293=ADVANCED_FACE('',(#6829),#87239,.F.);
#89294=ADVANCED_FACE('',(#6830),#5402,.F.);
#89295=ADVANCED_FACE('',(#6831),#87240,.F.);
#89296=ADVANCED_FACE('',(#6832),#5403,.F.);
#89297=ADVANCED_FACE('',(#6833),#87241,.F.);
#89298=ADVANCED_FACE('',(#6834),#87242,.T.);
#89299=ADVANCED_FACE('',(#6835),#87243,.F.);
#89300=ADVANCED_FACE('',(#6836),#87244,.F.);
#89301=ADVANCED_FACE('',(#6837),#5404,.F.);
#89302=ADVANCED_FACE('',(#6838),#87245,.F.);
#89303=ADVANCED_FACE('',(#6839),#87246,.F.);
#89304=ADVANCED_FACE('',(#6840),#87247,.F.);
#89305=ADVANCED_FACE('',(#6841),#87248,.T.);
#89306=ADVANCED_FACE('',(#6842),#87249,.F.);
#89307=ADVANCED_FACE('',(#6843),#87250,.T.);
#89308=ADVANCED_FACE('',(#6844,#5136,#5137),#5405,.T.);
#89309=ADVANCED_FACE('',(#6845),#4674,.F.);
#89310=ADVANCED_FACE('',(#6846),#87251,.F.);
#89311=ADVANCED_FACE('',(#6847),#87252,.T.);
#89312=ADVANCED_FACE('',(#6848),#5406,.F.);
#89313=ADVANCED_FACE('',(#6849),#87253,.T.);
#89314=ADVANCED_FACE('',(#6850),#5407,.F.);
#89315=ADVANCED_FACE('',(#6851),#87254,.F.);
#89316=ADVANCED_FACE('',(#6852),#5408,.T.);
#89317=ADVANCED_FACE('',(#6853),#5409,.T.);
#89318=ADVANCED_FACE('',(#6854),#87255,.F.);
#89319=ADVANCED_FACE('',(#6855,#5138),#5410,.T.);
#89320=ADVANCED_FACE('',(#6856),#87256,.F.);
#89321=ADVANCED_FACE('',(#6857),#87257,.T.);
#89322=ADVANCED_FACE('',(#6858),#5411,.T.);
#89323=ADVANCED_FACE('',(#6859),#87258,.T.);
#89324=ADVANCED_FACE('',(#6860),#87259,.F.);
#89325=ADVANCED_FACE('',(#6861),#5412,.F.);
#89326=ADVANCED_FACE('',(#6862),#87260,.F.);
#89327=ADVANCED_FACE('',(#6863),#5413,.F.);
#89328=ADVANCED_FACE('',(#6864),#5414,.T.);
#89329=ADVANCED_FACE('',(#6865),#87261,.F.);
#89330=ADVANCED_FACE('',(#6866),#87262,.F.);
#89331=ADVANCED_FACE('',(#6867),#87263,.F.);
#89332=ADVANCED_FACE('',(#6868),#87264,.F.);
#89333=ADVANCED_FACE('',(#6869),#5415,.F.);
#89334=ADVANCED_FACE('',(#6870),#87265,.F.);
#89335=ADVANCED_FACE('',(#6871),#87266,.T.);
#89336=ADVANCED_FACE('',(#6872),#87267,.T.);
#89337=ADVANCED_FACE('',(#6873,#5139),#5416,.T.);
#89338=ADVANCED_FACE('',(#6874),#4675,.T.);
#89339=ADVANCED_FACE('',(#6875),#87268,.F.);
#89340=ADVANCED_FACE('',(#6876),#87269,.F.);
#89341=ADVANCED_FACE('',(#6877),#4676,.F.);
#89342=ADVANCED_FACE('',(#6878),#87270,.T.);
#89343=ADVANCED_FACE('',(#6879),#5417,.T.);
#89344=ADVANCED_FACE('',(#6880),#87271,.T.);
#89345=ADVANCED_FACE('',(#6881),#5418,.F.);
#89346=ADVANCED_FACE('',(#6882),#87272,.F.);
#89347=ADVANCED_FACE('',(#6883),#5419,.F.);
#89348=ADVANCED_FACE('',(#6884),#5420,.F.);
#89349=ADVANCED_FACE('',(#6885),#87273,.T.);
#89350=ADVANCED_FACE('',(#6886),#5421,.T.);
#89351=ADVANCED_FACE('',(#6887),#5422,.T.);
#89352=ADVANCED_FACE('',(#6888),#87274,.T.);
#89353=ADVANCED_FACE('',(#6889),#87275,.T.);
#89354=ADVANCED_FACE('',(#6890),#87276,.T.);
#89355=ADVANCED_FACE('',(#6891),#5423,.T.);
#89356=ADVANCED_FACE('',(#6892),#87277,.F.);
#89357=ADVANCED_FACE('',(#6893),#87278,.T.);
#89358=ADVANCED_FACE('',(#6894),#5424,.T.);
#89359=ADVANCED_FACE('',(#6895),#1656,.F.);
#89360=ADVANCED_FACE('',(#6896),#2266,.T.);
#89361=ADVANCED_FACE('',(#6897),#87279,.F.);
#89362=ADVANCED_FACE('',(#6898),#2267,.T.);
#89363=ADVANCED_FACE('',(#6899),#87280,.F.);
#89364=ADVANCED_FACE('',(#6900),#2268,.T.);
#89365=ADVANCED_FACE('',(#6901),#1657,.F.);
#89366=ADVANCED_FACE('',(#6902),#2269,.T.);
#89367=ADVANCED_FACE('',(#6903),#87281,.F.);
#89368=ADVANCED_FACE('',(#6904),#87282,.T.);
#89369=ADVANCED_FACE('',(#6905),#87283,.F.);
#89370=ADVANCED_FACE('',(#6906),#87284,.T.);
#89371=ADVANCED_FACE('',(#6907),#5425,.T.);
#89372=ADVANCED_FACE('',(#6908),#1658,.F.);
#89373=ADVANCED_FACE('',(#6909),#1659,.F.);
#89374=ADVANCED_FACE('',(#6910),#87285,.F.);
#89375=ADVANCED_FACE('',(#6911),#1660,.F.);
#89376=ADVANCED_FACE('',(#6912),#1661,.F.);
#89377=ADVANCED_FACE('',(#6913),#1662,.F.);
#89378=ADVANCED_FACE('',(#6914),#1663,.F.);
#89379=ADVANCED_FACE('',(#6915),#87286,.F.);
#89380=ADVANCED_FACE('',(#6916),#87287,.F.);
#89381=ADVANCED_FACE('',(#6917),#87288,.T.);
#89382=ADVANCED_FACE('',(#6918),#5426,.T.);
#89383=ADVANCED_FACE('',(#6919),#87289,.F.);
#89384=ADVANCED_FACE('',(#6920),#5427,.T.);
#89385=ADVANCED_FACE('',(#6921),#1664,.F.);
#89386=ADVANCED_FACE('',(#6922),#2270,.T.);
#89387=ADVANCED_FACE('',(#6923),#1665,.F.);
#89388=ADVANCED_FACE('',(#6924),#87290,.T.);
#89389=ADVANCED_FACE('',(#6925),#87291,.F.);
#89390=ADVANCED_FACE('',(#6926),#87292,.T.);
#89391=ADVANCED_FACE('',(#6927),#87293,.F.);
#89392=ADVANCED_FACE('',(#6928),#5428,.T.);
#89393=ADVANCED_FACE('',(#6929),#5429,.T.);
#89394=ADVANCED_FACE('',(#6930),#2271,.T.);
#89395=ADVANCED_FACE('',(#6931),#87294,.F.);
#89396=ADVANCED_FACE('',(#6932,#5140),#5430,.F.);
#89397=ADVANCED_FACE('',(#6933),#87295,.F.);
#89398=ADVANCED_FACE('',(#6934),#5431,.F.);
#89399=ADVANCED_FACE('',(#6935),#87296,.F.);
#89400=ADVANCED_FACE('',(#6936),#87297,.F.);
#89401=ADVANCED_FACE('',(#6937),#5432,.T.);
#89402=ADVANCED_FACE('',(#6938),#5433,.T.);
#89403=ADVANCED_FACE('',(#6939),#1666,.F.);
#89404=ADVANCED_FACE('',(#6940),#2272,.T.);
#89405=ADVANCED_FACE('',(#6941),#1667,.F.);
#89406=ADVANCED_FACE('',(#6942),#2273,.T.);
#89407=ADVANCED_FACE('',(#6943),#87298,.F.);
#89408=ADVANCED_FACE('',(#6944),#87299,.F.);
#89409=ADVANCED_FACE('',(#6945),#5434,.F.);
#89410=ADVANCED_FACE('',(#6946),#5435,.T.);
#89411=ADVANCED_FACE('',(#6947),#87300,.T.);
#89412=ADVANCED_FACE('',(#6948),#5436,.T.);
#89413=ADVANCED_FACE('',(#6949),#1668,.F.);
#89414=ADVANCED_FACE('',(#6950),#2274,.T.);
#89415=ADVANCED_FACE('',(#6951),#1669,.F.);
#89416=ADVANCED_FACE('',(#6952),#1670,.F.);
#89417=ADVANCED_FACE('',(#6953),#5437,.T.);
#89418=ADVANCED_FACE('',(#6954),#87301,.F.);
#89419=ADVANCED_FACE('',(#6955),#2275,.T.);
#89420=ADVANCED_FACE('',(#6956),#87302,.F.);
#89421=ADVANCED_FACE('',(#6957),#2276,.T.);
#89422=ADVANCED_FACE('',(#6958),#87303,.F.);
#89423=ADVANCED_FACE('',(#6959),#2277,.T.);
#89424=ADVANCED_FACE('',(#6960),#1671,.F.);
#89425=ADVANCED_FACE('',(#6961),#87304,.F.);
#89426=ADVANCED_FACE('',(#6962),#87305,.F.);
#89427=ADVANCED_FACE('',(#6963),#87306,.T.);
#89428=ADVANCED_FACE('',(#6964),#5438,.F.);
#89429=ADVANCED_FACE('',(#6965),#87307,.F.);
#89430=ADVANCED_FACE('',(#6966),#5439,.F.);
#89431=ADVANCED_FACE('',(#6967),#87308,.F.);
#89432=ADVANCED_FACE('',(#6968),#5440,.T.);
#89433=ADVANCED_FACE('',(#6969),#87309,.F.);
#89434=ADVANCED_FACE('',(#6970),#87310,.F.);
#89435=ADVANCED_FACE('',(#6971),#135,.T.);
#89436=ADVANCED_FACE('',(#6972),#1672,.F.);
#89437=ADVANCED_FACE('',(#6973),#2278,.T.);
#89438=ADVANCED_FACE('',(#6974),#87311,.F.);
#89439=ADVANCED_FACE('',(#6975),#1673,.F.);
#89440=ADVANCED_FACE('',(#6976),#87312,.F.);
#89441=ADVANCED_FACE('',(#6977),#2279,.T.);
#89442=ADVANCED_FACE('',(#6978),#1674,.F.);
#89443=ADVANCED_FACE('',(#6979),#2280,.T.);
#89444=ADVANCED_FACE('',(#6980),#1675,.F.);
#89445=ADVANCED_FACE('',(#6981),#87313,.F.);
#89446=ADVANCED_FACE('',(#6982),#1676,.F.);
#89447=ADVANCED_FACE('',(#6983),#136,.F.);
#89448=ADVANCED_FACE('',(#6984),#5441,.T.);
#89449=ADVANCED_FACE('',(#6985),#87314,.T.);
#89450=ADVANCED_FACE('',(#6986),#5442,.T.);
#89451=ADVANCED_FACE('',(#6987),#87315,.F.);
#89452=ADVANCED_FACE('',(#6988),#87316,.F.);
#89453=ADVANCED_FACE('',(#6989),#87317,.T.);
#89454=ADVANCED_FACE('',(#6990),#5443,.T.);
#89455=ADVANCED_FACE('',(#6991),#87318,.F.);
#89456=ADVANCED_FACE('',(#6992),#2281,.T.);
#89457=ADVANCED_FACE('',(#6993),#87319,.F.);
#89458=ADVANCED_FACE('',(#6994),#1677,.F.);
#89459=ADVANCED_FACE('',(#6995),#2282,.T.);
#89460=ADVANCED_FACE('',(#6996),#87320,.F.);
#89461=ADVANCED_FACE('',(#6997),#1678,.F.);
#89462=ADVANCED_FACE('',(#6998),#2283,.T.);
#89463=ADVANCED_FACE('',(#6999),#1679,.F.);
#89464=ADVANCED_FACE('',(#7000),#2284,.T.);
#89465=ADVANCED_FACE('',(#7001),#87321,.F.);
#89466=ADVANCED_FACE('',(#7002),#2285,.T.);
#89467=ADVANCED_FACE('',(#7003),#87322,.F.);
#89468=ADVANCED_FACE('',(#7004),#87323,.T.);
#89469=ADVANCED_FACE('',(#7005),#87324,.F.);
#89470=ADVANCED_FACE('',(#7006),#5444,.T.);
#89471=ADVANCED_FACE('',(#7007),#87325,.F.);
#89472=ADVANCED_FACE('',(#7008),#5445,.F.);
#89473=ADVANCED_FACE('',(#7009),#5446,.T.);
#89474=ADVANCED_FACE('',(#7010),#87326,.F.);
#89475=ADVANCED_FACE('',(#7011),#2286,.T.);
#89476=ADVANCED_FACE('',(#7012),#87327,.F.);
#89477=ADVANCED_FACE('',(#7013),#2287,.T.);
#89478=ADVANCED_FACE('',(#7014),#87328,.F.);
#89479=ADVANCED_FACE('',(#7015),#1680,.F.);
#89480=ADVANCED_FACE('',(#7016),#1681,.F.);
#89481=ADVANCED_FACE('',(#7017),#2288,.T.);
#89482=ADVANCED_FACE('',(#7018),#1682,.F.);
#89483=ADVANCED_FACE('',(#7019),#1683,.F.);
#89484=ADVANCED_FACE('',(#7020),#2289,.T.);
#89485=ADVANCED_FACE('',(#7021),#87329,.F.);
#89486=ADVANCED_FACE('',(#7022),#87330,.F.);
#89487=ADVANCED_FACE('',(#7023),#87331,.F.);
#89488=ADVANCED_FACE('',(#7024),#87332,.F.);
#89489=ADVANCED_FACE('',(#7025),#87333,.F.);
#89490=ADVANCED_FACE('',(#7026),#5447,.T.);
#89491=ADVANCED_FACE('',(#7027),#5448,.T.);
#89492=ADVANCED_FACE('',(#7028),#1684,.F.);
#89493=ADVANCED_FACE('',(#7029),#2290,.T.);
#89494=ADVANCED_FACE('',(#7030),#1685,.F.);
#89495=ADVANCED_FACE('',(#7031),#2291,.T.);
#89496=ADVANCED_FACE('',(#7032),#87334,.F.);
#89497=ADVANCED_FACE('',(#7033),#87335,.F.);
#89498=ADVANCED_FACE('',(#7034),#87336,.F.);
#89499=ADVANCED_FACE('',(#7035),#5449,.F.);
#89500=ADVANCED_FACE('',(#7036),#87337,.T.);
#89501=ADVANCED_FACE('',(#7037),#5450,.T.);
#89502=ADVANCED_FACE('',(#7038),#87338,.T.);
#89503=ADVANCED_FACE('',(#7039),#87339,.F.);
#89504=ADVANCED_FACE('',(#7040),#1686,.F.);
#89505=ADVANCED_FACE('',(#7041),#87340,.F.);
#89506=ADVANCED_FACE('',(#7042),#2292,.T.);
#89507=ADVANCED_FACE('',(#7043),#1687,.F.);
#89508=ADVANCED_FACE('',(#7044),#2293,.T.);
#89509=ADVANCED_FACE('',(#7045),#87341,.F.);
#89510=ADVANCED_FACE('',(#7046),#2294,.T.);
#89511=ADVANCED_FACE('',(#7047),#1688,.F.);
#89512=ADVANCED_FACE('',(#7048),#2295,.T.);
#89513=ADVANCED_FACE('',(#7049),#87342,.F.);
#89514=ADVANCED_FACE('',(#7050),#2296,.T.);
#89515=ADVANCED_FACE('',(#7051),#87343,.F.);
#89516=ADVANCED_FACE('',(#7052),#87344,.T.);
#89517=ADVANCED_FACE('',(#7053),#87345,.F.);
#89518=ADVANCED_FACE('',(#7054),#5451,.F.);
#89519=ADVANCED_FACE('',(#7055),#87346,.F.);
#89520=ADVANCED_FACE('',(#7056),#5452,.T.);
#89521=ADVANCED_FACE('',(#7057),#5453,.T.);
#89522=ADVANCED_FACE('',(#7058),#1689,.F.);
#89523=ADVANCED_FACE('',(#7059),#2297,.T.);
#89524=ADVANCED_FACE('',(#7060),#87347,.F.);
#89525=ADVANCED_FACE('',(#7061),#2298,.T.);
#89526=ADVANCED_FACE('',(#7062),#87348,.F.);
#89527=ADVANCED_FACE('',(#7063),#2299,.T.);
#89528=ADVANCED_FACE('',(#7064),#1690,.F.);
#89529=ADVANCED_FACE('',(#7065),#2300,.T.);
#89530=ADVANCED_FACE('',(#7066),#87349,.F.);
#89531=ADVANCED_FACE('',(#7067),#2301,.T.);
#89532=ADVANCED_FACE('',(#7068),#1691,.F.);
#89533=ADVANCED_FACE('',(#7069),#1692,.F.);
#89534=ADVANCED_FACE('',(#7070),#5454,.F.);
#89535=ADVANCED_FACE('',(#7071),#87350,.F.);
#89536=ADVANCED_FACE('',(#7072),#137,.T.);
#89537=ADVANCED_FACE('',(#7073),#87351,.F.);
#89538=ADVANCED_FACE('',(#7074),#5455,.T.);
#89539=ADVANCED_FACE('',(#7075),#1693,.F.);
#89540=ADVANCED_FACE('',(#7076),#2302,.T.);
#89541=ADVANCED_FACE('',(#7077),#87352,.F.);
#89542=ADVANCED_FACE('',(#7078),#2303,.T.);
#89543=ADVANCED_FACE('',(#7079),#1694,.F.);
#89544=ADVANCED_FACE('',(#7080),#2304,.T.);
#89545=ADVANCED_FACE('',(#7081),#87353,.F.);
#89546=ADVANCED_FACE('',(#7082),#2305,.T.);
#89547=ADVANCED_FACE('',(#7083),#87354,.F.);
#89548=ADVANCED_FACE('',(#7084),#2306,.T.);
#89549=ADVANCED_FACE('',(#7085),#5456,.F.);
#89550=ADVANCED_FACE('',(#7086),#87355,.F.);
#89551=ADVANCED_FACE('',(#7087),#5457,.T.);
#89552=ADVANCED_FACE('',(#7088),#87356,.F.);
#89553=ADVANCED_FACE('',(#7089),#87357,.F.);
#89554=ADVANCED_FACE('',(#7090),#5458,.T.);
#89555=ADVANCED_FACE('',(#7091),#87358,.T.);
#89556=ADVANCED_FACE('',(#7092),#5459,.T.);
#89557=ADVANCED_FACE('',(#7093),#87359,.F.);
#89558=ADVANCED_FACE('',(#7094),#87360,.F.);
#89559=ADVANCED_FACE('',(#7095),#87361,.T.);
#89560=ADVANCED_FACE('',(#7096),#87362,.T.);
#89561=ADVANCED_FACE('',(#7097),#5460,.F.);
#89562=ADVANCED_FACE('',(#7098),#5461,.T.);
#89563=ADVANCED_FACE('',(#7099),#87363,.T.);
#89564=ADVANCED_FACE('',(#7100),#87364,.F.);
#89565=ADVANCED_FACE('',(#7101),#87365,.T.);
#89566=ADVANCED_FACE('',(#7102),#87366,.F.);
#89567=ADVANCED_FACE('',(#7103),#87367,.T.);
#89568=ADVANCED_FACE('',(#7104),#5462,.F.);
#89569=ADVANCED_FACE('',(#7105),#87368,.T.);
#89570=ADVANCED_FACE('',(#7106,#5141),#5463,.T.);
#89571=ADVANCED_FACE('',(#7107),#87369,.F.);
#89572=ADVANCED_FACE('',(#7108),#87370,.F.);
#89573=ADVANCED_FACE('',(#7109),#5464,.T.);
#89574=ADVANCED_FACE('',(#7110),#87371,.F.);
#89575=ADVANCED_FACE('',(#7111),#87372,.T.);
#89576=ADVANCED_FACE('',(#7112),#87373,.F.);
#89577=ADVANCED_FACE('',(#7113),#87374,.T.);
#89578=ADVANCED_FACE('',(#7114),#87375,.T.);
#89579=ADVANCED_FACE('',(#7115),#5465,.F.);
#89580=ADVANCED_FACE('',(#7116),#87376,.F.);
#89581=ADVANCED_FACE('',(#7117),#5466,.T.);
#89582=ADVANCED_FACE('',(#7118),#87377,.T.);
#89583=ADVANCED_FACE('',(#7119),#87378,.T.);
#89584=ADVANCED_FACE('',(#7120),#87379,.F.);
#89585=ADVANCED_FACE('',(#7121),#87380,.F.);
#89586=ADVANCED_FACE('',(#7122),#87381,.T.);
#89587=ADVANCED_FACE('',(#7123),#87382,.T.);
#89588=ADVANCED_FACE('',(#7124),#87383,.F.);
#89589=ADVANCED_FACE('',(#7125),#87384,.F.);
#89590=ADVANCED_FACE('',(#7126),#87385,.F.);
#89591=ADVANCED_FACE('',(#7127,#5142),#5467,.T.);
#89592=ADVANCED_FACE('',(#7128),#4677,.F.);
#89593=ADVANCED_FACE('',(#7129),#87386,.F.);
#89594=ADVANCED_FACE('',(#7130,#5143),#5468,.T.);
#89595=ADVANCED_FACE('',(#7131),#4678,.F.);
#89596=ADVANCED_FACE('',(#7132),#4679,.T.);
#89597=ADVANCED_FACE('',(#7133),#5469,.T.);
#89598=ADVANCED_FACE('',(#7134),#5470,.T.);
#89599=ADVANCED_FACE('',(#7135),#5471,.F.);
#89600=ADVANCED_FACE('',(#7136),#87387,.F.);
#89601=ADVANCED_FACE('',(#7137),#5472,.F.);
#89602=ADVANCED_FACE('',(#7138),#5473,.F.);
#89603=ADVANCED_FACE('',(#7139),#87388,.F.);
#89604=ADVANCED_FACE('',(#7140),#5474,.F.);
#89605=ADVANCED_FACE('',(#7141),#138,.F.);
#89606=ADVANCED_FACE('',(#7142),#87389,.F.);
#89607=ADVANCED_FACE('',(#7143),#139,.F.);
#89608=ADVANCED_FACE('',(#7144),#87390,.F.);
#89609=ADVANCED_FACE('',(#7145),#5475,.F.);
#89610=ADVANCED_FACE('',(#7146),#87391,.F.);
#89611=ADVANCED_FACE('',(#7147),#5476,.F.);
#89612=ADVANCED_FACE('',(#7148),#4680,.F.);
#89613=ADVANCED_FACE('',(#7149),#5477,.F.);
#89614=ADVANCED_FACE('',(#7150),#87392,.F.);
#89615=ADVANCED_FACE('',(#7151),#5478,.F.);
#89616=ADVANCED_FACE('',(#7152),#4681,.F.);
#89617=ADVANCED_FACE('',(#7153),#5479,.F.);
#89618=ADVANCED_FACE('',(#7154),#5480,.F.);
#89619=ADVANCED_FACE('',(#7155),#87393,.T.);
#89620=ADVANCED_FACE('',(#7156),#5481,.F.);
#89621=ADVANCED_FACE('',(#7157),#5482,.F.);
#89622=ADVANCED_FACE('',(#7158),#87394,.F.);
#89623=ADVANCED_FACE('',(#7159),#5483,.T.);
#89624=ADVANCED_FACE('',(#7160),#5484,.F.);
#89625=ADVANCED_FACE('',(#7161),#87395,.T.);
#89626=ADVANCED_FACE('',(#7162,#5144),#5485,.T.);
#89627=ADVANCED_FACE('',(#7163),#87396,.F.);
#89628=ADVANCED_FACE('',(#7164),#4682,.T.);
#89629=ADVANCED_FACE('',(#7165),#5486,.F.);
#89630=ADVANCED_FACE('',(#7166),#87397,.F.);
#89631=ADVANCED_FACE('',(#7167),#5487,.F.);
#89632=ADVANCED_FACE('',(#7168),#87398,.T.);
#89633=ADVANCED_FACE('',(#7169),#87399,.F.);
#89634=ADVANCED_FACE('',(#7170),#5488,.T.);
#89635=ADVANCED_FACE('',(#7171),#87400,.F.);
#89636=ADVANCED_FACE('',(#7172),#87401,.T.);
#89637=ADVANCED_FACE('',(#7173),#87402,.F.);
#89638=ADVANCED_FACE('',(#7174),#5489,.F.);
#89639=ADVANCED_FACE('',(#7175),#87403,.T.);
#89640=ADVANCED_FACE('',(#7176),#5490,.F.);
#89641=ADVANCED_FACE('',(#7177),#87404,.T.);
#89642=ADVANCED_FACE('',(#7178),#87405,.F.);
#89643=ADVANCED_FACE('',(#7179),#5491,.F.);
#89644=ADVANCED_FACE('',(#7180),#87406,.F.);
#89645=ADVANCED_FACE('',(#7181),#5492,.F.);
#89646=ADVANCED_FACE('',(#7182),#87407,.F.);
#89647=ADVANCED_FACE('',(#7183),#87408,.T.);
#89648=ADVANCED_FACE('',(#7184),#87409,.T.);
#89649=ADVANCED_FACE('',(#7185),#87410,.T.);
#89650=ADVANCED_FACE('',(#7186,#5145),#5493,.T.);
#89651=ADVANCED_FACE('',(#7187,#5146,#5147,#5148),#5494,.T.);
#89652=ADVANCED_FACE('',(#7188),#87411,.F.);
#89653=ADVANCED_FACE('',(#7189),#87412,.F.);
#89654=ADVANCED_FACE('',(#7190),#4683,.T.);
#89655=ADVANCED_FACE('',(#7191),#87413,.T.);
#89656=ADVANCED_FACE('',(#7192),#87414,.T.);
#89657=ADVANCED_FACE('',(#7193),#87415,.F.);
#89658=ADVANCED_FACE('',(#7194),#87416,.T.);
#89659=ADVANCED_FACE('',(#7195),#87417,.F.);
#89660=ADVANCED_FACE('',(#7196),#87418,.T.);
#89661=ADVANCED_FACE('',(#7197),#87419,.F.);
#89662=ADVANCED_FACE('',(#7198),#87420,.T.);
#89663=ADVANCED_FACE('',(#7199),#4684,.F.);
#89664=ADVANCED_FACE('',(#7200,#5149),#5495,.T.);
#89665=ADVANCED_FACE('',(#7201),#87421,.F.);
#89666=ADVANCED_FACE('',(#7202),#4685,.F.);
#89667=ADVANCED_FACE('',(#7203),#87422,.F.);
#89668=ADVANCED_FACE('',(#7204),#87423,.T.);
#89669=ADVANCED_FACE('',(#7205),#87424,.F.);
#89670=ADVANCED_FACE('',(#7206),#87425,.F.);
#89671=ADVANCED_FACE('',(#7207),#4686,.F.);
#89672=ADVANCED_FACE('',(#7208),#87426,.F.);
#89673=ADVANCED_FACE('',(#7209),#87427,.T.);
#89674=ADVANCED_FACE('',(#7210),#87428,.F.);
#89675=ADVANCED_FACE('',(#7211),#87429,.T.);
#89676=ADVANCED_FACE('',(#7212),#87430,.T.);
#89677=ADVANCED_FACE('',(#7213),#5496,.T.);
#89678=ADVANCED_FACE('',(#7214),#87431,.T.);
#89679=ADVANCED_FACE('',(#7215),#87432,.F.);
#89680=ADVANCED_FACE('',(#7216),#87433,.F.);
#89681=ADVANCED_FACE('',(#7217),#5497,.T.);
#89682=ADVANCED_FACE('',(#7218),#87434,.F.);
#89683=ADVANCED_FACE('',(#7219),#87435,.F.);
#89684=ADVANCED_FACE('',(#7220),#4687,.F.);
#89685=ADVANCED_FACE('',(#7221),#4688,.F.);
#89686=ADVANCED_FACE('',(#7222),#87436,.F.);
#89687=ADVANCED_FACE('',(#7223,#5150),#5498,.T.);
#89688=ADVANCED_FACE('',(#7224,#5151),#5499,.T.);
#89689=ADVANCED_FACE('',(#7225),#87437,.F.);
#89690=ADVANCED_FACE('',(#7226),#87438,.F.);
#89691=ADVANCED_FACE('',(#7227),#5500,.F.);
#89692=ADVANCED_FACE('',(#7228),#5501,.T.);
#89693=ADVANCED_FACE('',(#7229),#4689,.T.);
#89694=ADVANCED_FACE('',(#7230),#87439,.F.);
#89695=ADVANCED_FACE('',(#7231),#87440,.F.);
#89696=ADVANCED_FACE('',(#7232,#5152),#5502,.T.);
#89697=ADVANCED_FACE('',(#7233),#4690,.F.);
#89698=ADVANCED_FACE('',(#7234,#5153),#5503,.T.);
#89699=ADVANCED_FACE('',(#7235),#4691,.F.);
#89700=ADVANCED_FACE('',(#7236),#4692,.T.);
#89701=ADVANCED_FACE('',(#7237),#4693,.T.);
#89702=ADVANCED_FACE('',(#7238),#4694,.T.);
#89703=ADVANCED_FACE('',(#7239,#5154),#5504,.T.);
#89704=ADVANCED_FACE('',(#7240),#87441,.F.);
#89705=ADVANCED_FACE('',(#7241),#87442,.T.);
#89706=ADVANCED_FACE('',(#7242),#87443,.T.);
#89707=ADVANCED_FACE('',(#7243),#4695,.T.);
#89708=ADVANCED_FACE('',(#7244),#4696,.T.);
#89709=ADVANCED_FACE('',(#7245),#87444,.T.);
#89710=ADVANCED_FACE('',(#7246),#5505,.F.);
#89711=ADVANCED_FACE('',(#7247),#87445,.F.);
#89712=ADVANCED_FACE('',(#7248),#5506,.T.);
#89713=ADVANCED_FACE('',(#7249),#5507,.T.);
#89714=ADVANCED_FACE('',(#7250),#87446,.T.);
#89715=ADVANCED_FACE('',(#7251),#1695,.F.);
#89716=ADVANCED_FACE('',(#7252),#87447,.T.);
#89717=ADVANCED_FACE('',(#7253),#87448,.F.);
#89718=ADVANCED_FACE('',(#7254),#140,.F.);
#89719=ADVANCED_FACE('',(#7255),#87449,.F.);
#89720=ADVANCED_FACE('',(#7256),#141,.F.);
#89721=ADVANCED_FACE('',(#7257),#87450,.F.);
#89722=ADVANCED_FACE('',(#7258),#6208,.T.);
#89723=ADVANCED_FACE('',(#7259),#1696,.F.);
#89724=ADVANCED_FACE('',(#7260),#87451,.F.);
#89725=ADVANCED_FACE('',(#7261),#87452,.T.);
#89726=ADVANCED_FACE('',(#7262),#87453,.F.);
#89727=ADVANCED_FACE('',(#7263),#87454,.T.);
#89728=ADVANCED_FACE('',(#7264),#4697,.T.);
#89729=ADVANCED_FACE('',(#7265),#87455,.F.);
#89730=ADVANCED_FACE('',(#7266),#6209,.T.);
#89731=ADVANCED_FACE('',(#7267),#1697,.F.);
#89732=ADVANCED_FACE('',(#7268),#5508,.F.);
#89733=ADVANCED_FACE('',(#7269),#87456,.F.);
#89734=ADVANCED_FACE('',(#7270),#87457,.T.);
#89735=ADVANCED_FACE('',(#7271),#87458,.F.);
#89736=ADVANCED_FACE('',(#7272,#5155),#5509,.T.);
#89737=ADVANCED_FACE('',(#7273),#87459,.T.);
#89738=ADVANCED_FACE('',(#7274),#87460,.F.);
#89739=ADVANCED_FACE('',(#7275),#5510,.F.);
#89740=ADVANCED_FACE('',(#7276),#87461,.T.);
#89741=ADVANCED_FACE('',(#7277),#4698,.F.);
#89742=ADVANCED_FACE('',(#7278,#5156),#5511,.F.);
#89743=ADVANCED_FACE('',(#7279),#87462,.F.);
#89744=ADVANCED_FACE('',(#7280),#87463,.F.);
#89745=ADVANCED_FACE('',(#7281),#5512,.T.);
#89746=ADVANCED_FACE('',(#7282),#87464,.F.);
#89747=ADVANCED_FACE('',(#7283),#5513,.F.);
#89748=ADVANCED_FACE('',(#7284),#87465,.F.);
#89749=ADVANCED_FACE('',(#7285),#5514,.F.);
#89750=ADVANCED_FACE('',(#7286),#87466,.T.);
#89751=ADVANCED_FACE('',(#7287),#5515,.F.);
#89752=ADVANCED_FACE('',(#7288),#87467,.T.);
#89753=ADVANCED_FACE('',(#7289),#5516,.F.);
#89754=ADVANCED_FACE('',(#7290),#5517,.T.);
#89755=ADVANCED_FACE('',(#7291),#87468,.T.);
#89756=ADVANCED_FACE('',(#7292),#87469,.F.);
#89757=ADVANCED_FACE('',(#7293),#87470,.F.);
#89758=ADVANCED_FACE('',(#7294,#5157),#5518,.T.);
#89759=ADVANCED_FACE('',(#7295),#87471,.T.);
#89760=ADVANCED_FACE('',(#7296),#87472,.F.);
#89761=ADVANCED_FACE('',(#7297),#87473,.T.);
#89762=ADVANCED_FACE('',(#7298),#87474,.F.);
#89763=ADVANCED_FACE('',(#7299),#5519,.T.);
#89764=ADVANCED_FACE('',(#7300),#4699,.F.);
#89765=ADVANCED_FACE('',(#7301),#5520,.F.);
#89766=ADVANCED_FACE('',(#7302),#5521,.T.);
#89767=ADVANCED_FACE('',(#7303),#87475,.F.);
#89768=ADVANCED_FACE('',(#7304),#87476,.F.);
#89769=ADVANCED_FACE('',(#7305),#5522,.F.);
#89770=ADVANCED_FACE('',(#7306),#5523,.F.);
#89771=ADVANCED_FACE('',(#7307),#5524,.F.);
#89772=ADVANCED_FACE('',(#7308),#5525,.F.);
#89773=ADVANCED_FACE('',(#7309),#5526,.F.);
#89774=ADVANCED_FACE('',(#7310),#87477,.T.);
#89775=ADVANCED_FACE('',(#7311),#87478,.T.);
#89776=ADVANCED_FACE('',(#7312),#87479,.T.);
#89777=ADVANCED_FACE('',(#7313),#87480,.T.);
#89778=ADVANCED_FACE('',(#7314),#87481,.T.);
#89779=ADVANCED_FACE('',(#7315),#87482,.T.);
#89780=ADVANCED_FACE('',(#7316),#5527,.F.);
#89781=ADVANCED_FACE('',(#7317),#87483,.T.);
#89782=ADVANCED_FACE('',(#7318),#87484,.T.);
#89783=ADVANCED_FACE('',(#7319),#5528,.F.);
#89784=ADVANCED_FACE('',(#7320),#6210,.F.);
#89785=ADVANCED_FACE('',(#7321),#6211,.F.);
#89786=ADVANCED_FACE('',(#7322),#6212,.F.);
#89787=ADVANCED_FACE('',(#7323),#6213,.F.);
#89788=ADVANCED_FACE('',(#7324),#5529,.F.);
#89789=ADVANCED_FACE('',(#7325),#6214,.F.);
#89790=ADVANCED_FACE('',(#7326),#87485,.T.);
#89791=ADVANCED_FACE('',(#7327),#87486,.F.);
#89792=ADVANCED_FACE('',(#7328),#87487,.F.);
#89793=ADVANCED_FACE('',(#7329),#5530,.F.);
#89794=ADVANCED_FACE('',(#7330),#87488,.F.);
#89795=ADVANCED_FACE('',(#7331),#87489,.T.);
#89796=ADVANCED_FACE('',(#7332),#87490,.F.);
#89797=ADVANCED_FACE('',(#7333),#87491,.T.);
#89798=ADVANCED_FACE('',(#7334),#5531,.T.);
#89799=ADVANCED_FACE('',(#7335),#87492,.T.);
#89800=ADVANCED_FACE('',(#7336),#87493,.F.);
#89801=ADVANCED_FACE('',(#7337),#5532,.F.);
#89802=ADVANCED_FACE('',(#7338),#87494,.F.);
#89803=ADVANCED_FACE('',(#7339),#5533,.T.);
#89804=ADVANCED_FACE('',(#7340),#87495,.F.);
#89805=ADVANCED_FACE('',(#7341),#87496,.T.);
#89806=ADVANCED_FACE('',(#7342),#87497,.T.);
#89807=ADVANCED_FACE('',(#7343),#5534,.F.);
#89808=ADVANCED_FACE('',(#7344),#87498,.T.);
#89809=ADVANCED_FACE('',(#7345,#5158),#5535,.T.);
#89810=ADVANCED_FACE('',(#7346),#5536,.T.);
#89811=ADVANCED_FACE('',(#7347),#87499,.F.);
#89812=ADVANCED_FACE('',(#7348),#4700,.T.);
#89813=ADVANCED_FACE('',(#7349),#4701,.T.);
#89814=ADVANCED_FACE('',(#7350),#5537,.T.);
#89815=ADVANCED_FACE('',(#7351),#5538,.T.);
#89816=ADVANCED_FACE('',(#7352),#5539,.F.);
#89817=ADVANCED_FACE('',(#7353),#87500,.F.);
#89818=ADVANCED_FACE('',(#7354),#5540,.F.);
#89819=ADVANCED_FACE('',(#7355),#87501,.F.);
#89820=ADVANCED_FACE('',(#7356),#5541,.T.);
#89821=ADVANCED_FACE('',(#7357),#87502,.F.);
#89822=ADVANCED_FACE('',(#7358,#5159,#5160,#5161),#5542,.T.);
#89823=ADVANCED_FACE('',(#7359),#87503,.F.);
#89824=ADVANCED_FACE('',(#7360),#5543,.T.);
#89825=ADVANCED_FACE('',(#7361),#5544,.F.);
#89826=ADVANCED_FACE('',(#7362),#5545,.T.);
#89827=ADVANCED_FACE('',(#7363),#5546,.T.);
#89828=ADVANCED_FACE('',(#7364),#5547,.F.);
#89829=ADVANCED_FACE('',(#7365),#5548,.F.);
#89830=ADVANCED_FACE('',(#7366),#5549,.F.);
#89831=ADVANCED_FACE('',(#7367),#5550,.F.);
#89832=ADVANCED_FACE('',(#7368),#5551,.T.);
#89833=ADVANCED_FACE('',(#7369),#5552,.T.);
#89834=ADVANCED_FACE('',(#7370),#5553,.T.);
#89835=ADVANCED_FACE('',(#7371),#5554,.T.);
#89836=ADVANCED_FACE('',(#7372,#5162),#5555,.T.);
#89837=ADVANCED_FACE('',(#7373),#5556,.F.);
#89838=ADVANCED_FACE('',(#7374),#5557,.F.);
#89839=ADVANCED_FACE('',(#7375),#87504,.F.);
#89840=ADVANCED_FACE('',(#7376),#87505,.T.);
#89841=ADVANCED_FACE('',(#7377),#5558,.T.);
#89842=ADVANCED_FACE('',(#7378),#87506,.F.);
#89843=ADVANCED_FACE('',(#7379),#5559,.F.);
#89844=ADVANCED_FACE('',(#7380),#5560,.F.);
#89845=ADVANCED_FACE('',(#7381),#5561,.F.);
#89846=ADVANCED_FACE('',(#7382),#5562,.T.);
#89847=ADVANCED_FACE('',(#7383),#87507,.T.);
#89848=ADVANCED_FACE('',(#7384),#5563,.T.);
#89849=ADVANCED_FACE('',(#7385),#5564,.F.);
#89850=ADVANCED_FACE('',(#7386),#87508,.T.);
#89851=ADVANCED_FACE('',(#7387),#5565,.F.);
#89852=ADVANCED_FACE('',(#7388),#5566,.F.);
#89853=ADVANCED_FACE('',(#7389),#87509,.F.);
#89854=ADVANCED_FACE('',(#7390),#4702,.F.);
#89855=ADVANCED_FACE('',(#7391),#5567,.T.);
#89856=ADVANCED_FACE('',(#7392),#4703,.F.);
#89857=ADVANCED_FACE('',(#7393),#5568,.T.);
#89858=ADVANCED_FACE('',(#7394),#5569,.F.);
#89859=ADVANCED_FACE('',(#7395),#87510,.F.);
#89860=ADVANCED_FACE('',(#7396),#5570,.F.);
#89861=ADVANCED_FACE('',(#7397),#87511,.F.);
#89862=ADVANCED_FACE('',(#7398,#5163),#5571,.T.);
#89863=ADVANCED_FACE('',(#7399),#5572,.F.);
#89864=ADVANCED_FACE('',(#7400),#5573,.F.);
#89865=ADVANCED_FACE('',(#7401),#87512,.F.);
#89866=ADVANCED_FACE('',(#7402),#4704,.T.);
#89867=ADVANCED_FACE('',(#7403),#4705,.T.);
#89868=ADVANCED_FACE('',(#7404,#5164),#5574,.T.);
#89869=ADVANCED_FACE('',(#7405,#5165),#5575,.T.);
#89870=ADVANCED_FACE('',(#7406),#4706,.T.);
#89871=ADVANCED_FACE('',(#7407),#4707,.T.);
#89872=ADVANCED_FACE('',(#7408,#5166),#5576,.T.);
#89873=ADVANCED_FACE('',(#7409,#5167),#5577,.T.);
#89874=ADVANCED_FACE('',(#7410),#87513,.F.);
#89875=ADVANCED_FACE('',(#7411),#87514,.T.);
#89876=ADVANCED_FACE('',(#7412),#5578,.T.);
#89877=ADVANCED_FACE('',(#7413),#87515,.T.);
#89878=ADVANCED_FACE('',(#7414,#5168),#5579,.T.);
#89879=ADVANCED_FACE('',(#7415),#5580,.F.);
#89880=ADVANCED_FACE('',(#7416,#5169),#5581,.T.);
#89881=ADVANCED_FACE('',(#7417),#5582,.F.);
#89882=ADVANCED_FACE('',(#7418),#5583,.T.);
#89883=ADVANCED_FACE('',(#7419),#5584,.T.);
#89884=ADVANCED_FACE('',(#7420),#87516,.F.);
#89885=ADVANCED_FACE('',(#7421),#87517,.F.);
#89886=ADVANCED_FACE('',(#7422),#87518,.T.);
#89887=ADVANCED_FACE('',(#7423),#87519,.F.);
#89888=ADVANCED_FACE('',(#7424),#87520,.T.);
#89889=ADVANCED_FACE('',(#7425),#5585,.T.);
#89890=ADVANCED_FACE('',(#7426),#5586,.T.);
#89891=ADVANCED_FACE('',(#7427),#87521,.F.);
#89892=ADVANCED_FACE('',(#7428),#87522,.F.);
#89893=ADVANCED_FACE('',(#7429),#87523,.T.);
#89894=ADVANCED_FACE('',(#7430),#4708,.T.);
#89895=ADVANCED_FACE('',(#7431),#87524,.T.);
#89896=ADVANCED_FACE('',(#7432),#5587,.F.);
#89897=ADVANCED_FACE('',(#7433),#4709,.T.);
#89898=ADVANCED_FACE('',(#7434),#5588,.T.);
#89899=ADVANCED_FACE('',(#7435),#4710,.T.);
#89900=ADVANCED_FACE('',(#7436),#87525,.T.);
#89901=ADVANCED_FACE('',(#7437),#5589,.F.);
#89902=ADVANCED_FACE('',(#7438),#4711,.T.);
#89903=ADVANCED_FACE('',(#7439),#5590,.T.);
#89904=ADVANCED_FACE('',(#7440),#1698,.F.);
#89905=ADVANCED_FACE('',(#7441),#1699,.F.);
#89906=ADVANCED_FACE('',(#7442),#1700,.F.);
#89907=ADVANCED_FACE('',(#7443),#1701,.F.);
#89908=ADVANCED_FACE('',(#7444),#1702,.F.);
#89909=ADVANCED_FACE('',(#7445),#1703,.F.);
#89910=ADVANCED_FACE('',(#7446),#1704,.F.);
#89911=ADVANCED_FACE('',(#7447),#1705,.F.);
#89912=ADVANCED_FACE('',(#7448),#1706,.F.);
#89913=ADVANCED_FACE('',(#7449),#1707,.F.);
#89914=ADVANCED_FACE('',(#7450),#1708,.F.);
#89915=ADVANCED_FACE('',(#7451),#1709,.F.);
#89916=ADVANCED_FACE('',(#7452),#1710,.F.);
#89917=ADVANCED_FACE('',(#7453),#1711,.F.);
#89918=ADVANCED_FACE('',(#7454),#1712,.F.);
#89919=ADVANCED_FACE('',(#7455),#1713,.F.);
#89920=ADVANCED_FACE('',(#7456),#1714,.F.);
#89921=ADVANCED_FACE('',(#7457),#1715,.F.);
#89922=ADVANCED_FACE('',(#7458),#1716,.F.);
#89923=ADVANCED_FACE('',(#7459),#1717,.F.);
#89924=ADVANCED_FACE('',(#7460),#1718,.F.);
#89925=ADVANCED_FACE('',(#7461),#1719,.F.);
#89926=ADVANCED_FACE('',(#7462),#1720,.F.);
#89927=ADVANCED_FACE('',(#7463),#1721,.F.);
#89928=ADVANCED_FACE('',(#7464),#1722,.F.);
#89929=ADVANCED_FACE('',(#7465),#1723,.F.);
#89930=ADVANCED_FACE('',(#7466),#1724,.F.);
#89931=ADVANCED_FACE('',(#7467),#1725,.F.);
#89932=ADVANCED_FACE('',(#7468),#1726,.F.);
#89933=ADVANCED_FACE('',(#7469),#1727,.F.);
#89934=ADVANCED_FACE('',(#7470),#1728,.F.);
#89935=ADVANCED_FACE('',(#7471),#1729,.F.);
#89936=ADVANCED_FACE('',(#7472),#1730,.F.);
#89937=ADVANCED_FACE('',(#7473),#1731,.F.);
#89938=ADVANCED_FACE('',(#7474),#1732,.F.);
#89939=ADVANCED_FACE('',(#7475),#1733,.F.);
#89940=ADVANCED_FACE('',(#7476),#1734,.F.);
#89941=ADVANCED_FACE('',(#7477),#1735,.F.);
#89942=ADVANCED_FACE('',(#7478),#1736,.F.);
#89943=ADVANCED_FACE('',(#7479),#1737,.F.);
#89944=ADVANCED_FACE('',(#7480),#1738,.F.);
#89945=ADVANCED_FACE('',(#7481),#1739,.F.);
#89946=ADVANCED_FACE('',(#7482),#1740,.F.);
#89947=ADVANCED_FACE('',(#7483),#1741,.F.);
#89948=ADVANCED_FACE('',(#7484),#1742,.F.);
#89949=ADVANCED_FACE('',(#7485),#1743,.F.);
#89950=ADVANCED_FACE('',(#7486),#1744,.F.);
#89951=ADVANCED_FACE('',(#7487),#1745,.F.);
#89952=ADVANCED_FACE('',(#7488),#1746,.F.);
#89953=ADVANCED_FACE('',(#7489),#1747,.F.);
#89954=ADVANCED_FACE('',(#7490),#1748,.F.);
#89955=ADVANCED_FACE('',(#7491),#1749,.F.);
#89956=ADVANCED_FACE('',(#7492),#1750,.F.);
#89957=ADVANCED_FACE('',(#7493),#1751,.F.);
#89958=ADVANCED_FACE('',(#7494),#1752,.F.);
#89959=ADVANCED_FACE('',(#7495),#1753,.F.);
#89960=ADVANCED_FACE('',(#7496),#1754,.F.);
#89961=ADVANCED_FACE('',(#7497),#1755,.F.);
#89962=ADVANCED_FACE('',(#7498),#1756,.F.);
#89963=ADVANCED_FACE('',(#7499),#1757,.F.);
#89964=ADVANCED_FACE('',(#7500),#1758,.F.);
#89965=ADVANCED_FACE('',(#7501),#1759,.F.);
#89966=ADVANCED_FACE('',(#7502),#1760,.F.);
#89967=ADVANCED_FACE('',(#7503),#1761,.F.);
#89968=ADVANCED_FACE('',(#7504),#1762,.F.);
#89969=ADVANCED_FACE('',(#7505),#1763,.F.);
#89970=ADVANCED_FACE('',(#7506),#1764,.F.);
#89971=ADVANCED_FACE('',(#7507),#1765,.F.);
#89972=ADVANCED_FACE('',(#7508),#1766,.F.);
#89973=ADVANCED_FACE('',(#7509),#1767,.F.);
#89974=ADVANCED_FACE('',(#7510),#4712,.F.);
#89975=ADVANCED_FACE('',(#7511),#4713,.F.);
#89976=ADVANCED_FACE('',(#7512),#4714,.F.);
#89977=ADVANCED_FACE('',(#7513),#4715,.T.);
#89978=ADVANCED_FACE('',(#7514),#4716,.F.);
#89979=ADVANCED_FACE('',(#7515),#4717,.F.);
#89980=ADVANCED_FACE('',(#7516),#4718,.T.);
#89981=ADVANCED_FACE('',(#7517),#4719,.F.);
#89982=ADVANCED_FACE('',(#7518),#87526,.F.);
#89983=ADVANCED_FACE('',(#7519),#87527,.F.);
#89984=ADVANCED_FACE('',(#7520),#4720,.T.);
#89985=ADVANCED_FACE('',(#7521),#87528,.T.);
#89986=ADVANCED_FACE('',(#7522),#87529,.T.);
#89987=ADVANCED_FACE('',(#7523),#87530,.F.);
#89988=ADVANCED_FACE('',(#7524,#5170),#5591,.T.);
#89989=ADVANCED_FACE('',(#7525,#5171,#5172,#5173),#5592,.T.);
#89990=ADVANCED_FACE('',(#7526,#5174,#5175,#5176),#5593,.T.);
#89991=ADVANCED_FACE('',(#7527),#4721,.F.);
#89992=ADVANCED_FACE('',(#7528),#1768,.F.);
#89993=ADVANCED_FACE('',(#7529),#4722,.F.);
#89994=ADVANCED_FACE('',(#7530),#4723,.F.);
#89995=ADVANCED_FACE('',(#7531),#1769,.F.);
#89996=ADVANCED_FACE('',(#7532),#4724,.F.);
#89997=ADVANCED_FACE('',(#7533),#4725,.F.);
#89998=ADVANCED_FACE('',(#7534),#1770,.F.);
#89999=ADVANCED_FACE('',(#7535),#4726,.F.);
#90000=ADVANCED_FACE('',(#7536),#4727,.F.);
#90001=ADVANCED_FACE('',(#7537),#1771,.F.);
#90002=ADVANCED_FACE('',(#7538),#4728,.F.);
#90003=ADVANCED_FACE('',(#7539),#4729,.F.);
#90004=ADVANCED_FACE('',(#7540),#1772,.F.);
#90005=ADVANCED_FACE('',(#7541),#4730,.F.);
#90006=ADVANCED_FACE('',(#7542),#4731,.F.);
#90007=ADVANCED_FACE('',(#7543),#1773,.F.);
#90008=ADVANCED_FACE('',(#7544),#4732,.F.);
#90009=ADVANCED_FACE('',(#7545),#4733,.F.);
#90010=ADVANCED_FACE('',(#7546),#1774,.F.);
#90011=ADVANCED_FACE('',(#7547),#4734,.F.);
#90012=ADVANCED_FACE('',(#7548),#4735,.F.);
#90013=ADVANCED_FACE('',(#7549),#1775,.F.);
#90014=ADVANCED_FACE('',(#7550),#4736,.F.);
#90015=ADVANCED_FACE('',(#7551),#4737,.F.);
#90016=ADVANCED_FACE('',(#7552),#1776,.F.);
#90017=ADVANCED_FACE('',(#7553),#4738,.F.);
#90018=ADVANCED_FACE('',(#7554),#4739,.F.);
#90019=ADVANCED_FACE('',(#7555),#1777,.F.);
#90020=ADVANCED_FACE('',(#7556),#4740,.F.);
#90021=ADVANCED_FACE('',(#7557),#4741,.F.);
#90022=ADVANCED_FACE('',(#7558),#1778,.F.);
#90023=ADVANCED_FACE('',(#7559),#4742,.F.);
#90024=ADVANCED_FACE('',(#7560),#4743,.F.);
#90025=ADVANCED_FACE('',(#7561),#1779,.F.);
#90026=ADVANCED_FACE('',(#7562),#4744,.F.);
#90027=ADVANCED_FACE('',(#7563),#4745,.F.);
#90028=ADVANCED_FACE('',(#7564),#1780,.F.);
#90029=ADVANCED_FACE('',(#7565),#4746,.F.);
#90030=ADVANCED_FACE('',(#7566),#4747,.F.);
#90031=ADVANCED_FACE('',(#7567),#1781,.F.);
#90032=ADVANCED_FACE('',(#7568),#4748,.F.);
#90033=ADVANCED_FACE('',(#7569),#4749,.F.);
#90034=ADVANCED_FACE('',(#7570),#1782,.F.);
#90035=ADVANCED_FACE('',(#7571),#4750,.F.);
#90036=ADVANCED_FACE('',(#7572),#4751,.F.);
#90037=ADVANCED_FACE('',(#7573),#1783,.F.);
#90038=ADVANCED_FACE('',(#7574),#4752,.F.);
#90039=ADVANCED_FACE('',(#7575),#4753,.F.);
#90040=ADVANCED_FACE('',(#7576),#1784,.F.);
#90041=ADVANCED_FACE('',(#7577),#4754,.F.);
#90042=ADVANCED_FACE('',(#7578),#4755,.F.);
#90043=ADVANCED_FACE('',(#7579),#1785,.F.);
#90044=ADVANCED_FACE('',(#7580),#4756,.F.);
#90045=ADVANCED_FACE('',(#7581),#4757,.F.);
#90046=ADVANCED_FACE('',(#7582),#1786,.F.);
#90047=ADVANCED_FACE('',(#7583),#4758,.F.);
#90048=ADVANCED_FACE('',(#7584),#4759,.F.);
#90049=ADVANCED_FACE('',(#7585),#1787,.F.);
#90050=ADVANCED_FACE('',(#7586),#4760,.F.);
#90051=ADVANCED_FACE('',(#7587),#4761,.F.);
#90052=ADVANCED_FACE('',(#7588),#1788,.F.);
#90053=ADVANCED_FACE('',(#7589),#4762,.F.);
#90054=ADVANCED_FACE('',(#7590),#4763,.F.);
#90055=ADVANCED_FACE('',(#7591),#1789,.F.);
#90056=ADVANCED_FACE('',(#7592),#4764,.F.);
#90057=ADVANCED_FACE('',(#7593),#4765,.F.);
#90058=ADVANCED_FACE('',(#7594),#1790,.F.);
#90059=ADVANCED_FACE('',(#7595),#4766,.F.);
#90060=ADVANCED_FACE('',(#7596),#4767,.F.);
#90061=ADVANCED_FACE('',(#7597),#1791,.F.);
#90062=ADVANCED_FACE('',(#7598),#4768,.F.);
#90063=ADVANCED_FACE('',(#7599),#4769,.F.);
#90064=ADVANCED_FACE('',(#7600),#1792,.F.);
#90065=ADVANCED_FACE('',(#7601),#4770,.F.);
#90066=ADVANCED_FACE('',(#7602),#4771,.F.);
#90067=ADVANCED_FACE('',(#7603),#1793,.F.);
#90068=ADVANCED_FACE('',(#7604),#4772,.F.);
#90069=ADVANCED_FACE('',(#7605),#4773,.F.);
#90070=ADVANCED_FACE('',(#7606),#1794,.F.);
#90071=ADVANCED_FACE('',(#7607),#4774,.F.);
#90072=ADVANCED_FACE('',(#7608),#4775,.F.);
#90073=ADVANCED_FACE('',(#7609),#1795,.F.);
#90074=ADVANCED_FACE('',(#7610),#4776,.F.);
#90075=ADVANCED_FACE('',(#7611),#4777,.F.);
#90076=ADVANCED_FACE('',(#7612),#1796,.F.);
#90077=ADVANCED_FACE('',(#7613),#4778,.F.);
#90078=ADVANCED_FACE('',(#7614),#4779,.F.);
#90079=ADVANCED_FACE('',(#7615),#1797,.F.);
#90080=ADVANCED_FACE('',(#7616),#4780,.F.);
#90081=ADVANCED_FACE('',(#7617),#4781,.F.);
#90082=ADVANCED_FACE('',(#7618),#1798,.F.);
#90083=ADVANCED_FACE('',(#7619),#4782,.F.);
#90084=ADVANCED_FACE('',(#7620),#4783,.F.);
#90085=ADVANCED_FACE('',(#7621),#1799,.F.);
#90086=ADVANCED_FACE('',(#7622),#4784,.F.);
#90087=ADVANCED_FACE('',(#7623),#4785,.F.);
#90088=ADVANCED_FACE('',(#7624),#1800,.F.);
#90089=ADVANCED_FACE('',(#7625),#4786,.F.);
#90090=ADVANCED_FACE('',(#7626),#4787,.F.);
#90091=ADVANCED_FACE('',(#7627),#1801,.F.);
#90092=ADVANCED_FACE('',(#7628),#4788,.F.);
#90093=ADVANCED_FACE('',(#7629),#4789,.F.);
#90094=ADVANCED_FACE('',(#7630),#1802,.F.);
#90095=ADVANCED_FACE('',(#7631),#4790,.F.);
#90096=ADVANCED_FACE('',(#7632),#4791,.F.);
#90097=ADVANCED_FACE('',(#7633),#1803,.F.);
#90098=ADVANCED_FACE('',(#7634),#4792,.F.);
#90099=ADVANCED_FACE('',(#7635),#4793,.F.);
#90100=ADVANCED_FACE('',(#7636),#1804,.F.);
#90101=ADVANCED_FACE('',(#7637),#4794,.F.);
#90102=ADVANCED_FACE('',(#7638),#4795,.F.);
#90103=ADVANCED_FACE('',(#7639),#1805,.F.);
#90104=ADVANCED_FACE('',(#7640),#4796,.F.);
#90105=ADVANCED_FACE('',(#7641),#4797,.F.);
#90106=ADVANCED_FACE('',(#7642),#1806,.F.);
#90107=ADVANCED_FACE('',(#7643),#4798,.F.);
#90108=ADVANCED_FACE('',(#7644),#4799,.F.);
#90109=ADVANCED_FACE('',(#7645),#1807,.F.);
#90110=ADVANCED_FACE('',(#7646),#4800,.F.);
#90111=ADVANCED_FACE('',(#7647),#4801,.F.);
#90112=ADVANCED_FACE('',(#7648),#1808,.F.);
#90113=ADVANCED_FACE('',(#7649),#4802,.F.);
#90114=ADVANCED_FACE('',(#7650),#4803,.F.);
#90115=ADVANCED_FACE('',(#7651),#1809,.F.);
#90116=ADVANCED_FACE('',(#7652),#4804,.F.);
#90117=ADVANCED_FACE('',(#7653),#4805,.F.);
#90118=ADVANCED_FACE('',(#7654),#1810,.F.);
#90119=ADVANCED_FACE('',(#7655),#4806,.F.);
#90120=ADVANCED_FACE('',(#7656),#4807,.F.);
#90121=ADVANCED_FACE('',(#7657),#1811,.F.);
#90122=ADVANCED_FACE('',(#7658),#4808,.F.);
#90123=ADVANCED_FACE('',(#7659),#4809,.F.);
#90124=ADVANCED_FACE('',(#7660),#1812,.F.);
#90125=ADVANCED_FACE('',(#7661),#4810,.F.);
#90126=ADVANCED_FACE('',(#7662),#4811,.F.);
#90127=ADVANCED_FACE('',(#7663),#1813,.F.);
#90128=ADVANCED_FACE('',(#7664),#4812,.F.);
#90129=ADVANCED_FACE('',(#7665),#4813,.F.);
#90130=ADVANCED_FACE('',(#7666),#1814,.F.);
#90131=ADVANCED_FACE('',(#7667),#4814,.F.);
#90132=ADVANCED_FACE('',(#7668),#4815,.F.);
#90133=ADVANCED_FACE('',(#7669),#1815,.F.);
#90134=ADVANCED_FACE('',(#7670),#4816,.F.);
#90135=ADVANCED_FACE('',(#7671),#4817,.F.);
#90136=ADVANCED_FACE('',(#7672),#1816,.F.);
#90137=ADVANCED_FACE('',(#7673),#4818,.F.);
#90138=ADVANCED_FACE('',(#7674),#4819,.F.);
#90139=ADVANCED_FACE('',(#7675),#1817,.F.);
#90140=ADVANCED_FACE('',(#7676),#4820,.F.);
#90141=ADVANCED_FACE('',(#7677),#4821,.F.);
#90142=ADVANCED_FACE('',(#7678),#1818,.F.);
#90143=ADVANCED_FACE('',(#7679),#4822,.F.);
#90144=ADVANCED_FACE('',(#7680),#4823,.F.);
#90145=ADVANCED_FACE('',(#7681),#1819,.F.);
#90146=ADVANCED_FACE('',(#7682),#4824,.F.);
#90147=ADVANCED_FACE('',(#7683),#4825,.F.);
#90148=ADVANCED_FACE('',(#7684),#1820,.F.);
#90149=ADVANCED_FACE('',(#7685),#4826,.F.);
#90150=ADVANCED_FACE('',(#7686),#4827,.F.);
#90151=ADVANCED_FACE('',(#7687),#1821,.F.);
#90152=ADVANCED_FACE('',(#7688),#4828,.F.);
#90153=ADVANCED_FACE('',(#7689),#4829,.F.);
#90154=ADVANCED_FACE('',(#7690),#1822,.F.);
#90155=ADVANCED_FACE('',(#7691),#4830,.F.);
#90156=ADVANCED_FACE('',(#7692),#4831,.F.);
#90157=ADVANCED_FACE('',(#7693),#1823,.F.);
#90158=ADVANCED_FACE('',(#7694),#4832,.F.);
#90159=ADVANCED_FACE('',(#7695),#4833,.F.);
#90160=ADVANCED_FACE('',(#7696),#1824,.F.);
#90161=ADVANCED_FACE('',(#7697),#4834,.F.);
#90162=ADVANCED_FACE('',(#7698),#4835,.F.);
#90163=ADVANCED_FACE('',(#7699),#1825,.F.);
#90164=ADVANCED_FACE('',(#7700),#4836,.F.);
#90165=ADVANCED_FACE('',(#7701),#4837,.F.);
#90166=ADVANCED_FACE('',(#7702),#1826,.F.);
#90167=ADVANCED_FACE('',(#7703),#4838,.F.);
#90168=ADVANCED_FACE('',(#7704),#4839,.F.);
#90169=ADVANCED_FACE('',(#7705),#1827,.F.);
#90170=ADVANCED_FACE('',(#7706),#4840,.F.);
#90171=ADVANCED_FACE('',(#7707),#4841,.F.);
#90172=ADVANCED_FACE('',(#7708),#1828,.F.);
#90173=ADVANCED_FACE('',(#7709),#4842,.F.);
#90174=ADVANCED_FACE('',(#7710),#4843,.F.);
#90175=ADVANCED_FACE('',(#7711),#1829,.F.);
#90176=ADVANCED_FACE('',(#7712),#4844,.F.);
#90177=ADVANCED_FACE('',(#7713),#4845,.F.);
#90178=ADVANCED_FACE('',(#7714),#1830,.F.);
#90179=ADVANCED_FACE('',(#7715),#4846,.F.);
#90180=ADVANCED_FACE('',(#7716),#4847,.F.);
#90181=ADVANCED_FACE('',(#7717),#1831,.F.);
#90182=ADVANCED_FACE('',(#7718),#4848,.F.);
#90183=ADVANCED_FACE('',(#7719),#4849,.F.);
#90184=ADVANCED_FACE('',(#7720),#1832,.F.);
#90185=ADVANCED_FACE('',(#7721),#4850,.F.);
#90186=ADVANCED_FACE('',(#7722),#4851,.F.);
#90187=ADVANCED_FACE('',(#7723),#1833,.F.);
#90188=ADVANCED_FACE('',(#7724),#4852,.F.);
#90189=ADVANCED_FACE('',(#7725),#4853,.F.);
#90190=ADVANCED_FACE('',(#7726),#1834,.F.);
#90191=ADVANCED_FACE('',(#7727),#4854,.F.);
#90192=ADVANCED_FACE('',(#7728),#4855,.F.);
#90193=ADVANCED_FACE('',(#7729),#1835,.F.);
#90194=ADVANCED_FACE('',(#7730),#4856,.F.);
#90195=ADVANCED_FACE('',(#7731),#4857,.F.);
#90196=ADVANCED_FACE('',(#7732),#1836,.F.);
#90197=ADVANCED_FACE('',(#7733),#4858,.F.);
#90198=ADVANCED_FACE('',(#7734),#4859,.F.);
#90199=ADVANCED_FACE('',(#7735),#1837,.F.);
#90200=ADVANCED_FACE('',(#7736),#4860,.F.);
#90201=ADVANCED_FACE('',(#7737),#87531,.F.);
#90202=ADVANCED_FACE('',(#7738),#87532,.F.);
#90203=ADVANCED_FACE('',(#7739),#1838,.F.);
#90204=ADVANCED_FACE('',(#7740),#1839,.F.);
#90205=ADVANCED_FACE('',(#7741),#1840,.T.);
#90206=ADVANCED_FACE('',(#7742),#1841,.T.);
#90207=ADVANCED_FACE('',(#7743),#1842,.T.);
#90208=ADVANCED_FACE('',(#7744),#1843,.T.);
#90209=ADVANCED_FACE('',(#7745),#1844,.T.);
#90210=ADVANCED_FACE('',(#7746),#1845,.T.);
#90211=ADVANCED_FACE('',(#7747),#1846,.T.);
#90212=ADVANCED_FACE('',(#7748),#1847,.T.);
#90213=ADVANCED_FACE('',(#7749),#87533,.F.);
#90214=ADVANCED_FACE('',(#7750),#87534,.F.);
#90215=ADVANCED_FACE('',(#7751),#87535,.F.);
#90216=ADVANCED_FACE('',(#7752),#87536,.T.);
#90217=ADVANCED_FACE('',(#7753),#87537,.T.);
#90218=ADVANCED_FACE('',(#7754),#87538,.T.);
#90219=ADVANCED_FACE('',(#7755),#87539,.T.);
#90220=ADVANCED_FACE('',(#7756),#87540,.T.);
#90221=ADVANCED_FACE('',(#7757),#87541,.T.);
#90222=ADVANCED_FACE('',(#7758),#87542,.T.);
#90223=ADVANCED_FACE('',(#7759),#87543,.F.);
#90224=ADVANCED_FACE('',(#7760,#5177,#5178,#5179,#5180,#5181),#5594,.F.);
#90225=ADVANCED_FACE('',(#7761),#87544,.T.);
#90226=ADVANCED_FACE('',(#7762),#87545,.T.);
#90227=ADVANCED_FACE('',(#7763),#87546,.T.);
#90228=ADVANCED_FACE('',(#7764),#87547,.T.);
#90229=ADVANCED_FACE('',(#7765),#87548,.T.);
#90230=ADVANCED_FACE('',(#7766),#87549,.T.);
#90231=ADVANCED_FACE('',(#7767),#87550,.T.);
#90232=ADVANCED_FACE('',(#7768),#87551,.T.);
#90233=ADVANCED_FACE('',(#7769),#87552,.T.);
#90234=ADVANCED_FACE('',(#7770),#87553,.T.);
#90235=ADVANCED_FACE('',(#7771),#87554,.T.);
#90236=ADVANCED_FACE('',(#7772),#87555,.T.);
#90237=ADVANCED_FACE('',(#7773),#87556,.T.);
#90238=ADVANCED_FACE('',(#7774),#87557,.T.);
#90239=ADVANCED_FACE('',(#7775),#87558,.T.);
#90240=ADVANCED_FACE('',(#7776),#87559,.T.);
#90241=ADVANCED_FACE('',(#7777),#87560,.T.);
#90242=ADVANCED_FACE('',(#7778),#87561,.T.);
#90243=ADVANCED_FACE('',(#7779),#87562,.T.);
#90244=ADVANCED_FACE('',(#7780),#87563,.T.);
#90245=ADVANCED_FACE('',(#7781),#87564,.T.);
#90246=ADVANCED_FACE('',(#7782),#87565,.T.);
#90247=ADVANCED_FACE('',(#7783),#87566,.T.);
#90248=ADVANCED_FACE('',(#7784),#87567,.T.);
#90249=ADVANCED_FACE('',(#7785),#87568,.T.);
#90250=ADVANCED_FACE('',(#7786),#87569,.T.);
#90251=ADVANCED_FACE('',(#7787),#87570,.T.);
#90252=ADVANCED_FACE('',(#7788),#87571,.T.);
#90253=ADVANCED_FACE('',(#7789),#87572,.T.);
#90254=ADVANCED_FACE('',(#7790),#87573,.T.);
#90255=ADVANCED_FACE('',(#7791),#87574,.T.);
#90256=ADVANCED_FACE('',(#7792),#87575,.T.);
#90257=ADVANCED_FACE('',(#7793),#87576,.T.);
#90258=ADVANCED_FACE('',(#7794),#87577,.T.);
#90259=ADVANCED_FACE('',(#7795),#87578,.T.);
#90260=ADVANCED_FACE('',(#7796),#87579,.T.);
#90261=ADVANCED_FACE('',(#7797,#5182,#5183,#5184),#5595,.F.);
#90262=ADVANCED_FACE('',(#7798),#87580,.T.);
#90263=ADVANCED_FACE('',(#7799),#87581,.T.);
#90264=ADVANCED_FACE('',(#7800),#87582,.T.);
#90265=ADVANCED_FACE('',(#7801),#87583,.T.);
#90266=ADVANCED_FACE('',(#7802),#87584,.T.);
#90267=ADVANCED_FACE('',(#7803),#87585,.T.);
#90268=ADVANCED_FACE('',(#7804),#87586,.T.);
#90269=ADVANCED_FACE('',(#7805),#87587,.T.);
#90270=ADVANCED_FACE('',(#7806),#87588,.T.);
#90271=ADVANCED_FACE('',(#7807),#87589,.T.);
#90272=ADVANCED_FACE('',(#7808),#87590,.T.);
#90273=ADVANCED_FACE('',(#7809),#87591,.T.);
#90274=ADVANCED_FACE('',(#7810),#87592,.T.);
#90275=ADVANCED_FACE('',(#7811),#87593,.T.);
#90276=ADVANCED_FACE('',(#7812),#87594,.T.);
#90277=ADVANCED_FACE('',(#7813),#87595,.T.);
#90278=ADVANCED_FACE('',(#7814),#87596,.T.);
#90279=ADVANCED_FACE('',(#7815),#87597,.T.);
#90280=ADVANCED_FACE('',(#7816),#87598,.T.);
#90281=ADVANCED_FACE('',(#7817),#87599,.T.);
#90282=ADVANCED_FACE('',(#7818),#87600,.T.);
#90283=ADVANCED_FACE('',(#7819),#87601,.T.);
#90284=ADVANCED_FACE('',(#7820),#87602,.T.);
#90285=ADVANCED_FACE('',(#7821),#87603,.T.);
#90286=ADVANCED_FACE('',(#7822),#87604,.T.);
#90287=ADVANCED_FACE('',(#7823),#87605,.T.);
#90288=ADVANCED_FACE('',(#7824),#87606,.T.);
#90289=ADVANCED_FACE('',(#7825),#87607,.T.);
#90290=ADVANCED_FACE('',(#7826),#87608,.T.);
#90291=ADVANCED_FACE('',(#7827),#87609,.T.);
#90292=ADVANCED_FACE('',(#7828),#87610,.T.);
#90293=ADVANCED_FACE('',(#7829),#87611,.T.);
#90294=ADVANCED_FACE('',(#7830),#87612,.T.);
#90295=ADVANCED_FACE('',(#7831),#87613,.T.);
#90296=ADVANCED_FACE('',(#7832),#87614,.T.);
#90297=ADVANCED_FACE('',(#7833),#87615,.T.);
#90298=ADVANCED_FACE('',(#7834),#87616,.T.);
#90299=ADVANCED_FACE('',(#7835),#87617,.T.);
#90300=ADVANCED_FACE('',(#7836),#87618,.T.);
#90301=ADVANCED_FACE('',(#7837),#87619,.T.);
#90302=ADVANCED_FACE('',(#7838),#87620,.T.);
#90303=ADVANCED_FACE('',(#7839),#87621,.T.);
#90304=ADVANCED_FACE('',(#7840),#87622,.T.);
#90305=ADVANCED_FACE('',(#7841),#87623,.T.);
#90306=ADVANCED_FACE('',(#7842),#87624,.T.);
#90307=ADVANCED_FACE('',(#7843),#87625,.T.);
#90308=ADVANCED_FACE('',(#7844),#87626,.T.);
#90309=ADVANCED_FACE('',(#7845),#87627,.T.);
#90310=ADVANCED_FACE('',(#7846),#87628,.T.);
#90311=ADVANCED_FACE('',(#7847),#87629,.T.);
#90312=ADVANCED_FACE('',(#7848),#87630,.T.);
#90313=ADVANCED_FACE('',(#7849),#87631,.T.);
#90314=ADVANCED_FACE('',(#7850),#87632,.T.);
#90315=ADVANCED_FACE('',(#7851),#87633,.T.);
#90316=ADVANCED_FACE('',(#7852),#87634,.T.);
#90317=ADVANCED_FACE('',(#7853),#87635,.T.);
#90318=ADVANCED_FACE('',(#7854),#87636,.T.);
#90319=ADVANCED_FACE('',(#7855),#87637,.T.);
#90320=ADVANCED_FACE('',(#7856),#87638,.T.);
#90321=ADVANCED_FACE('',(#7857),#87639,.T.);
#90322=ADVANCED_FACE('',(#7858),#87640,.T.);
#90323=ADVANCED_FACE('',(#7859),#87641,.T.);
#90324=ADVANCED_FACE('',(#7860),#87642,.T.);
#90325=ADVANCED_FACE('',(#7861),#87643,.T.);
#90326=ADVANCED_FACE('',(#7862),#87644,.T.);
#90327=ADVANCED_FACE('',(#7863),#87645,.T.);
#90328=ADVANCED_FACE('',(#7864),#87646,.T.);
#90329=ADVANCED_FACE('',(#7865),#87647,.T.);
#90330=ADVANCED_FACE('',(#7866),#87648,.T.);
#90331=ADVANCED_FACE('',(#7867),#87649,.T.);
#90332=ADVANCED_FACE('',(#7868),#87650,.T.);
#90333=ADVANCED_FACE('',(#7869),#87651,.T.);
#90334=ADVANCED_FACE('',(#7870),#87652,.T.);
#90335=ADVANCED_FACE('',(#7871),#87653,.T.);
#90336=ADVANCED_FACE('',(#7872),#87654,.T.);
#90337=ADVANCED_FACE('',(#7873),#87655,.T.);
#90338=ADVANCED_FACE('',(#7874),#87656,.T.);
#90339=ADVANCED_FACE('',(#7875),#87657,.T.);
#90340=ADVANCED_FACE('',(#7876),#87658,.T.);
#90341=ADVANCED_FACE('',(#7877),#87659,.T.);
#90342=ADVANCED_FACE('',(#7878),#87660,.T.);
#90343=ADVANCED_FACE('',(#7879),#87661,.T.);
#90344=ADVANCED_FACE('',(#7880),#87662,.T.);
#90345=ADVANCED_FACE('',(#7881),#87663,.T.);
#90346=ADVANCED_FACE('',(#7882),#87664,.T.);
#90347=ADVANCED_FACE('',(#7883),#87665,.T.);
#90348=ADVANCED_FACE('',(#7884),#87666,.T.);
#90349=ADVANCED_FACE('',(#7885),#87667,.T.);
#90350=ADVANCED_FACE('',(#7886),#87668,.T.);
#90351=ADVANCED_FACE('',(#7887),#87669,.T.);
#90352=ADVANCED_FACE('',(#7888),#87670,.T.);
#90353=ADVANCED_FACE('',(#7889),#87671,.T.);
#90354=ADVANCED_FACE('',(#7890),#87672,.T.);
#90355=ADVANCED_FACE('',(#7891),#87673,.T.);
#90356=ADVANCED_FACE('',(#7892),#87674,.T.);
#90357=ADVANCED_FACE('',(#7893),#87675,.T.);
#90358=ADVANCED_FACE('',(#7894),#87676,.T.);
#90359=ADVANCED_FACE('',(#7895),#87677,.T.);
#90360=ADVANCED_FACE('',(#7896),#87678,.T.);
#90361=ADVANCED_FACE('',(#7897),#87679,.T.);
#90362=ADVANCED_FACE('',(#7898),#87680,.T.);
#90363=ADVANCED_FACE('',(#7899),#87681,.T.);
#90364=ADVANCED_FACE('',(#7900),#87682,.T.);
#90365=ADVANCED_FACE('',(#7901),#87683,.T.);
#90366=ADVANCED_FACE('',(#7902),#87684,.T.);
#90367=ADVANCED_FACE('',(#7903),#87685,.T.);
#90368=ADVANCED_FACE('',(#7904),#87686,.T.);
#90369=ADVANCED_FACE('',(#7905),#87687,.T.);
#90370=ADVANCED_FACE('',(#7906,#5185),#5596,.T.);
#90371=ADVANCED_FACE('',(#7907),#5597,.T.);
#90372=ADVANCED_FACE('',(#7908),#5598,.T.);
#90373=ADVANCED_FACE('',(#7909,#5186),#5599,.T.);
#90374=ADVANCED_FACE('',(#7910),#5600,.T.);
#90375=ADVANCED_FACE('',(#7911),#87688,.F.);
#90376=ADVANCED_FACE('',(#7912),#87689,.T.);
#90377=ADVANCED_FACE('',(#7913),#87690,.F.);
#90378=ADVANCED_FACE('',(#7914),#5601,.T.);
#90379=ADVANCED_FACE('',(#7915),#87691,.F.);
#90380=ADVANCED_FACE('',(#7916),#87692,.F.);
#90381=ADVANCED_FACE('',(#7917),#5602,.F.);
#90382=ADVANCED_FACE('',(#7918),#87693,.F.);
#90383=ADVANCED_FACE('',(#7919),#5603,.T.);
#90384=ADVANCED_FACE('',(#7920),#87694,.F.);
#90385=ADVANCED_FACE('',(#7921),#87695,.F.);
#90386=ADVANCED_FACE('',(#7922),#5604,.T.);
#90387=ADVANCED_FACE('',(#7923),#87696,.F.);
#90388=ADVANCED_FACE('',(#7924),#87697,.T.);
#90389=ADVANCED_FACE('',(#7925),#5605,.T.);
#90390=ADVANCED_FACE('',(#7926),#1848,.T.);
#90391=ADVANCED_FACE('',(#7927),#87698,.T.);
#90392=ADVANCED_FACE('',(#7928),#1849,.T.);
#90393=ADVANCED_FACE('',(#7929),#1850,.T.);
#90394=ADVANCED_FACE('',(#7930),#1851,.T.);
#90395=ADVANCED_FACE('',(#7931),#87699,.T.);
#90396=ADVANCED_FACE('',(#7932),#1852,.T.);
#90397=ADVANCED_FACE('',(#7933),#1853,.T.);
#90398=ADVANCED_FACE('',(#7934),#1854,.T.);
#90399=ADVANCED_FACE('',(#7935),#87700,.T.);
#90400=ADVANCED_FACE('',(#7936),#1855,.T.);
#90401=ADVANCED_FACE('',(#7937),#87701,.T.);
#90402=ADVANCED_FACE('',(#7938),#1856,.T.);
#90403=ADVANCED_FACE('',(#7939),#1857,.T.);
#90404=ADVANCED_FACE('',(#7940),#5606,.T.);
#90405=ADVANCED_FACE('',(#7941),#5607,.T.);
#90406=ADVANCED_FACE('',(#7942),#87702,.T.);
#90407=ADVANCED_FACE('',(#7943),#6215,.T.);
#90408=ADVANCED_FACE('',(#7944),#6216,.T.);
#90409=ADVANCED_FACE('',(#7945),#87703,.T.);
#90410=ADVANCED_FACE('',(#7946),#87704,.T.);
#90411=ADVANCED_FACE('',(#7947),#6217,.T.);
#90412=ADVANCED_FACE('',(#7948),#6218,.T.);
#90413=ADVANCED_FACE('',(#7949),#87705,.T.);
#90414=ADVANCED_FACE('',(#7950),#87706,.T.);
#90415=ADVANCED_FACE('',(#7951),#6219,.T.);
#90416=ADVANCED_FACE('',(#7952),#6220,.T.);
#90417=ADVANCED_FACE('',(#7953),#87707,.T.);
#90418=ADVANCED_FACE('',(#7954),#87708,.T.);
#90419=ADVANCED_FACE('',(#7955),#6221,.T.);
#90420=ADVANCED_FACE('',(#7956),#6222,.T.);
#90421=ADVANCED_FACE('',(#7957),#87709,.T.);
#90422=ADVANCED_FACE('',(#7958),#87710,.T.);
#90423=ADVANCED_FACE('',(#7959),#6223,.T.);
#90424=ADVANCED_FACE('',(#7960),#6224,.T.);
#90425=ADVANCED_FACE('',(#7961),#87711,.T.);
#90426=ADVANCED_FACE('',(#7962),#87712,.T.);
#90427=ADVANCED_FACE('',(#7963),#6225,.T.);
#90428=ADVANCED_FACE('',(#7964),#6226,.T.);
#90429=ADVANCED_FACE('',(#7965),#87713,.T.);
#90430=ADVANCED_FACE('',(#7966),#87714,.T.);
#90431=ADVANCED_FACE('',(#7967),#6227,.T.);
#90432=ADVANCED_FACE('',(#7968),#6228,.T.);
#90433=ADVANCED_FACE('',(#7969),#87715,.T.);
#90434=ADVANCED_FACE('',(#7970),#87716,.T.);
#90435=ADVANCED_FACE('',(#7971),#6229,.T.);
#90436=ADVANCED_FACE('',(#7972),#6230,.T.);
#90437=ADVANCED_FACE('',(#7973),#87717,.T.);
#90438=ADVANCED_FACE('',(#7974),#87718,.T.);
#90439=ADVANCED_FACE('',(#7975),#6231,.T.);
#90440=ADVANCED_FACE('',(#7976),#6232,.T.);
#90441=ADVANCED_FACE('',(#7977),#87719,.T.);
#90442=ADVANCED_FACE('',(#7978),#87720,.T.);
#90443=ADVANCED_FACE('',(#7979),#6233,.T.);
#90444=ADVANCED_FACE('',(#7980),#6234,.T.);
#90445=ADVANCED_FACE('',(#7981),#87721,.T.);
#90446=ADVANCED_FACE('',(#7982),#87722,.T.);
#90447=ADVANCED_FACE('',(#7983),#6235,.T.);
#90448=ADVANCED_FACE('',(#7984),#6236,.T.);
#90449=ADVANCED_FACE('',(#7985),#87723,.T.);
#90450=ADVANCED_FACE('',(#7986),#87724,.T.);
#90451=ADVANCED_FACE('',(#7987),#6237,.T.);
#90452=ADVANCED_FACE('',(#7988),#6238,.T.);
#90453=ADVANCED_FACE('',(#7989),#87725,.T.);
#90454=ADVANCED_FACE('',(#7990),#87726,.T.);
#90455=ADVANCED_FACE('',(#7991),#6239,.T.);
#90456=ADVANCED_FACE('',(#7992),#6240,.T.);
#90457=ADVANCED_FACE('',(#7993),#87727,.T.);
#90458=ADVANCED_FACE('',(#7994),#87728,.T.);
#90459=ADVANCED_FACE('',(#7995),#6241,.T.);
#90460=ADVANCED_FACE('',(#7996),#6242,.T.);
#90461=ADVANCED_FACE('',(#7997),#87729,.T.);
#90462=ADVANCED_FACE('',(#7998),#87730,.T.);
#90463=ADVANCED_FACE('',(#7999),#6243,.T.);
#90464=ADVANCED_FACE('',(#8000),#6244,.T.);
#90465=ADVANCED_FACE('',(#8001),#87731,.T.);
#90466=ADVANCED_FACE('',(#8002),#87732,.T.);
#90467=ADVANCED_FACE('',(#8003),#6245,.T.);
#90468=ADVANCED_FACE('',(#8004),#6246,.T.);
#90469=ADVANCED_FACE('',(#8005),#87733,.T.);
#90470=ADVANCED_FACE('',(#8006),#87734,.T.);
#90471=ADVANCED_FACE('',(#8007),#6247,.T.);
#90472=ADVANCED_FACE('',(#8008),#6248,.T.);
#90473=ADVANCED_FACE('',(#8009),#87735,.T.);
#90474=ADVANCED_FACE('',(#8010),#87736,.T.);
#90475=ADVANCED_FACE('',(#8011),#6249,.T.);
#90476=ADVANCED_FACE('',(#8012),#6250,.T.);
#90477=ADVANCED_FACE('',(#8013),#87737,.T.);
#90478=ADVANCED_FACE('',(#8014),#87738,.T.);
#90479=ADVANCED_FACE('',(#8015),#6251,.T.);
#90480=ADVANCED_FACE('',(#8016),#6252,.T.);
#90481=ADVANCED_FACE('',(#8017),#87739,.T.);
#90482=ADVANCED_FACE('',(#8018),#87740,.T.);
#90483=ADVANCED_FACE('',(#8019),#6253,.T.);
#90484=ADVANCED_FACE('',(#8020),#6254,.T.);
#90485=ADVANCED_FACE('',(#8021),#87741,.T.);
#90486=ADVANCED_FACE('',(#8022),#87742,.T.);
#90487=ADVANCED_FACE('',(#8023),#6255,.T.);
#90488=ADVANCED_FACE('',(#8024),#6256,.T.);
#90489=ADVANCED_FACE('',(#8025),#87743,.T.);
#90490=ADVANCED_FACE('',(#8026),#87744,.T.);
#90491=ADVANCED_FACE('',(#8027),#6257,.T.);
#90492=ADVANCED_FACE('',(#8028),#6258,.T.);
#90493=ADVANCED_FACE('',(#8029),#87745,.T.);
#90494=ADVANCED_FACE('',(#8030),#87746,.T.);
#90495=ADVANCED_FACE('',(#8031),#6259,.T.);
#90496=ADVANCED_FACE('',(#8032),#6260,.T.);
#90497=ADVANCED_FACE('',(#8033),#87747,.T.);
#90498=ADVANCED_FACE('',(#8034),#87748,.T.);
#90499=ADVANCED_FACE('',(#8035),#6261,.T.);
#90500=ADVANCED_FACE('',(#8036),#6262,.T.);
#90501=ADVANCED_FACE('',(#8037),#87749,.T.);
#90502=ADVANCED_FACE('',(#8038),#87750,.T.);
#90503=ADVANCED_FACE('',(#8039),#6263,.T.);
#90504=ADVANCED_FACE('',(#8040),#6264,.T.);
#90505=ADVANCED_FACE('',(#8041),#87751,.T.);
#90506=ADVANCED_FACE('',(#8042),#87752,.T.);
#90507=ADVANCED_FACE('',(#8043),#6265,.T.);
#90508=ADVANCED_FACE('',(#8044),#6266,.T.);
#90509=ADVANCED_FACE('',(#8045),#87753,.T.);
#90510=ADVANCED_FACE('',(#8046),#87754,.T.);
#90511=ADVANCED_FACE('',(#8047),#6267,.T.);
#90512=ADVANCED_FACE('',(#8048),#6268,.T.);
#90513=ADVANCED_FACE('',(#8049),#87755,.T.);
#90514=ADVANCED_FACE('',(#8050),#87756,.T.);
#90515=ADVANCED_FACE('',(#8051),#6269,.T.);
#90516=ADVANCED_FACE('',(#8052),#6270,.T.);
#90517=ADVANCED_FACE('',(#8053),#87757,.T.);
#90518=ADVANCED_FACE('',(#8054),#87758,.T.);
#90519=ADVANCED_FACE('',(#8055),#6271,.T.);
#90520=ADVANCED_FACE('',(#8056),#6272,.T.);
#90521=ADVANCED_FACE('',(#8057),#87759,.T.);
#90522=ADVANCED_FACE('',(#8058),#87760,.T.);
#90523=ADVANCED_FACE('',(#8059),#6273,.T.);
#90524=ADVANCED_FACE('',(#8060),#6274,.T.);
#90525=ADVANCED_FACE('',(#8061),#87761,.T.);
#90526=ADVANCED_FACE('',(#8062),#87762,.T.);
#90527=ADVANCED_FACE('',(#8063),#6275,.T.);
#90528=ADVANCED_FACE('',(#8064),#6276,.T.);
#90529=ADVANCED_FACE('',(#8065),#87763,.T.);
#90530=ADVANCED_FACE('',(#8066),#87764,.T.);
#90531=ADVANCED_FACE('',(#8067),#6277,.T.);
#90532=ADVANCED_FACE('',(#8068),#6278,.T.);
#90533=ADVANCED_FACE('',(#8069),#87765,.T.);
#90534=ADVANCED_FACE('',(#8070),#87766,.T.);
#90535=ADVANCED_FACE('',(#8071),#6279,.T.);
#90536=ADVANCED_FACE('',(#8072),#6280,.T.);
#90537=ADVANCED_FACE('',(#8073),#87767,.T.);
#90538=ADVANCED_FACE('',(#8074),#87768,.T.);
#90539=ADVANCED_FACE('',(#8075),#6281,.T.);
#90540=ADVANCED_FACE('',(#8076),#6282,.T.);
#90541=ADVANCED_FACE('',(#8077),#87769,.T.);
#90542=ADVANCED_FACE('',(#8078),#87770,.T.);
#90543=ADVANCED_FACE('',(#8079),#6283,.T.);
#90544=ADVANCED_FACE('',(#8080),#6284,.T.);
#90545=ADVANCED_FACE('',(#8081),#87771,.T.);
#90546=ADVANCED_FACE('',(#8082),#87772,.T.);
#90547=ADVANCED_FACE('',(#8083),#6285,.T.);
#90548=ADVANCED_FACE('',(#8084),#6286,.T.);
#90549=ADVANCED_FACE('',(#8085),#87773,.T.);
#90550=ADVANCED_FACE('',(#8086),#87774,.T.);
#90551=ADVANCED_FACE('',(#8087),#6287,.T.);
#90552=ADVANCED_FACE('',(#8088),#6288,.T.);
#90553=ADVANCED_FACE('',(#8089),#87775,.T.);
#90554=ADVANCED_FACE('',(#8090),#87776,.T.);
#90555=ADVANCED_FACE('',(#8091),#6289,.T.);
#90556=ADVANCED_FACE('',(#8092),#6290,.T.);
#90557=ADVANCED_FACE('',(#8093),#87777,.T.);
#90558=ADVANCED_FACE('',(#8094),#87778,.T.);
#90559=ADVANCED_FACE('',(#8095),#6291,.T.);
#90560=ADVANCED_FACE('',(#8096),#6292,.T.);
#90561=ADVANCED_FACE('',(#8097),#87779,.T.);
#90562=ADVANCED_FACE('',(#8098),#87780,.T.);
#90563=ADVANCED_FACE('',(#8099),#6293,.T.);
#90564=ADVANCED_FACE('',(#8100),#6294,.T.);
#90565=ADVANCED_FACE('',(#8101),#87781,.T.);
#90566=ADVANCED_FACE('',(#8102),#87782,.T.);
#90567=ADVANCED_FACE('',(#8103),#6295,.T.);
#90568=ADVANCED_FACE('',(#8104),#6296,.T.);
#90569=ADVANCED_FACE('',(#8105),#87783,.T.);
#90570=ADVANCED_FACE('',(#8106),#87784,.T.);
#90571=ADVANCED_FACE('',(#8107),#6297,.T.);
#90572=ADVANCED_FACE('',(#8108),#6298,.T.);
#90573=ADVANCED_FACE('',(#8109),#87785,.T.);
#90574=ADVANCED_FACE('',(#8110),#87786,.T.);
#90575=ADVANCED_FACE('',(#8111),#6299,.T.);
#90576=ADVANCED_FACE('',(#8112),#6300,.T.);
#90577=ADVANCED_FACE('',(#8113,#5187),#5608,.F.);
#90578=ADVANCED_FACE('',(#8114),#87787,.T.);
#90579=ADVANCED_FACE('',(#8115),#87788,.T.);
#90580=ADVANCED_FACE('',(#8116),#87789,.T.);
#90581=ADVANCED_FACE('',(#8117),#6301,.T.);
#90582=ADVANCED_FACE('',(#8118),#6302,.T.);
#90583=ADVANCED_FACE('',(#8119),#87790,.F.);
#90584=ADVANCED_FACE('',(#8120,#5188),#5609,.T.);
#90585=ADVANCED_FACE('',(#8121),#87791,.T.);
#90586=ADVANCED_FACE('',(#8122),#87792,.T.);
#90587=ADVANCED_FACE('',(#8123),#5610,.F.);
#90588=ADVANCED_FACE('',(#8124),#5611,.T.);
#90589=ADVANCED_FACE('',(#8125,#5189),#5612,.T.);
#90590=ADVANCED_FACE('',(#8126),#87793,.T.);
#90591=ADVANCED_FACE('',(#8127,#5190),#5613,.T.);
#90592=ADVANCED_FACE('',(#8128),#87794,.T.);
#90593=ADVANCED_FACE('',(#8129),#6303,.T.);
#90594=ADVANCED_FACE('',(#8130),#5614,.T.);
#90595=ADVANCED_FACE('',(#8131),#87795,.T.);
#90596=ADVANCED_FACE('',(#8132),#5615,.T.);
#90597=ADVANCED_FACE('',(#8133),#6304,.T.);
#90598=ADVANCED_FACE('',(#8134),#87796,.T.);
#90599=ADVANCED_FACE('',(#8135),#6305,.T.);
#90600=ADVANCED_FACE('',(#8136),#5616,.T.);
#90601=ADVANCED_FACE('',(#8137),#87797,.T.);
#90602=ADVANCED_FACE('',(#8138),#5617,.T.);
#90603=ADVANCED_FACE('',(#8139),#6306,.T.);
#90604=ADVANCED_FACE('',(#8140),#87798,.T.);
#90605=ADVANCED_FACE('',(#8141),#6307,.T.);
#90606=ADVANCED_FACE('',(#8142),#5618,.T.);
#90607=ADVANCED_FACE('',(#8143),#87799,.T.);
#90608=ADVANCED_FACE('',(#8144),#5619,.T.);
#90609=ADVANCED_FACE('',(#8145),#6308,.T.);
#90610=ADVANCED_FACE('',(#8146),#87800,.T.);
#90611=ADVANCED_FACE('',(#8147),#6309,.T.);
#90612=ADVANCED_FACE('',(#8148),#5620,.T.);
#90613=ADVANCED_FACE('',(#8149),#87801,.T.);
#90614=ADVANCED_FACE('',(#8150),#5621,.T.);
#90615=ADVANCED_FACE('',(#8151),#6310,.T.);
#90616=ADVANCED_FACE('',(#8152),#87802,.T.);
#90617=ADVANCED_FACE('',(#8153),#6311,.T.);
#90618=ADVANCED_FACE('',(#8154),#5622,.T.);
#90619=ADVANCED_FACE('',(#8155),#87803,.T.);
#90620=ADVANCED_FACE('',(#8156),#5623,.T.);
#90621=ADVANCED_FACE('',(#8157),#6312,.T.);
#90622=ADVANCED_FACE('',(#8158),#87804,.T.);
#90623=ADVANCED_FACE('',(#8159),#6313,.T.);
#90624=ADVANCED_FACE('',(#8160),#5624,.T.);
#90625=ADVANCED_FACE('',(#8161),#87805,.T.);
#90626=ADVANCED_FACE('',(#8162),#5625,.T.);
#90627=ADVANCED_FACE('',(#8163),#6314,.T.);
#90628=ADVANCED_FACE('',(#8164),#87806,.T.);
#90629=ADVANCED_FACE('',(#8165),#6315,.T.);
#90630=ADVANCED_FACE('',(#8166),#5626,.T.);
#90631=ADVANCED_FACE('',(#8167),#87807,.T.);
#90632=ADVANCED_FACE('',(#8168),#5627,.T.);
#90633=ADVANCED_FACE('',(#8169),#6316,.T.);
#90634=ADVANCED_FACE('',(#8170),#87808,.T.);
#90635=ADVANCED_FACE('',(#8171),#6317,.T.);
#90636=ADVANCED_FACE('',(#8172),#5628,.T.);
#90637=ADVANCED_FACE('',(#8173),#87809,.T.);
#90638=ADVANCED_FACE('',(#8174),#5629,.T.);
#90639=ADVANCED_FACE('',(#8175),#6318,.T.);
#90640=ADVANCED_FACE('',(#8176),#87810,.T.);
#90641=ADVANCED_FACE('',(#8177),#6319,.T.);
#90642=ADVANCED_FACE('',(#8178),#5630,.T.);
#90643=ADVANCED_FACE('',(#8179,#5191),#5631,.T.);
#90644=ADVANCED_FACE('',(#8180),#5632,.T.);
#90645=ADVANCED_FACE('',(#8181),#6320,.T.);
#90646=ADVANCED_FACE('',(#8182),#87811,.T.);
#90647=ADVANCED_FACE('',(#8183),#5633,.T.);
#90648=ADVANCED_FACE('',(#8184),#6321,.T.);
#90649=ADVANCED_FACE('',(#8185),#87812,.T.);
#90650=ADVANCED_FACE('',(#8186),#6322,.T.);
#90651=ADVANCED_FACE('',(#8187),#5634,.T.);
#90652=ADVANCED_FACE('',(#8188),#87813,.T.);
#90653=ADVANCED_FACE('',(#8189),#5635,.T.);
#90654=ADVANCED_FACE('',(#8190),#5636,.T.);
#90655=ADVANCED_FACE('',(#8191),#6323,.T.);
#90656=ADVANCED_FACE('',(#8192),#87814,.T.);
#90657=ADVANCED_FACE('',(#8193),#6324,.T.);
#90658=ADVANCED_FACE('',(#8194),#5637,.T.);
#90659=ADVANCED_FACE('',(#8195),#5638,.T.);
#90660=ADVANCED_FACE('',(#8196),#6325,.T.);
#90661=ADVANCED_FACE('',(#8197),#87815,.T.);
#90662=ADVANCED_FACE('',(#8198),#6326,.T.);
#90663=ADVANCED_FACE('',(#8199),#87816,.T.);
#90664=ADVANCED_FACE('',(#8200),#5639,.T.);
#90665=ADVANCED_FACE('',(#8201),#6327,.T.);
#90666=ADVANCED_FACE('',(#8202),#87817,.T.);
#90667=ADVANCED_FACE('',(#8203),#6328,.T.);
#90668=ADVANCED_FACE('',(#8204),#5640,.T.);
#90669=ADVANCED_FACE('',(#8205),#87818,.T.);
#90670=ADVANCED_FACE('',(#8206),#87819,.T.);
#90671=ADVANCED_FACE('',(#8207),#5641,.T.);
#90672=ADVANCED_FACE('',(#8208),#5642,.T.);
#90673=ADVANCED_FACE('',(#8209),#6329,.T.);
#90674=ADVANCED_FACE('',(#8210),#87820,.T.);
#90675=ADVANCED_FACE('',(#8211),#6330,.T.);
#90676=ADVANCED_FACE('',(#8212),#5643,.T.);
#90677=ADVANCED_FACE('',(#8213),#5644,.T.);
#90678=ADVANCED_FACE('',(#8214),#6331,.T.);
#90679=ADVANCED_FACE('',(#8215),#87821,.T.);
#90680=ADVANCED_FACE('',(#8216),#6332,.T.);
#90681=ADVANCED_FACE('',(#8217),#87822,.T.);
#90682=ADVANCED_FACE('',(#8218),#5645,.T.);
#90683=ADVANCED_FACE('',(#8219),#6333,.T.);
#90684=ADVANCED_FACE('',(#8220),#87823,.T.);
#90685=ADVANCED_FACE('',(#8221),#6334,.T.);
#90686=ADVANCED_FACE('',(#8222),#5646,.T.);
#90687=ADVANCED_FACE('',(#8223),#87824,.T.);
#90688=ADVANCED_FACE('',(#8224),#87825,.T.);
#90689=ADVANCED_FACE('',(#8225),#5647,.T.);
#90690=ADVANCED_FACE('',(#8226),#5648,.T.);
#90691=ADVANCED_FACE('',(#8227),#6335,.T.);
#90692=ADVANCED_FACE('',(#8228),#87826,.T.);
#90693=ADVANCED_FACE('',(#8229),#6336,.T.);
#90694=ADVANCED_FACE('',(#8230),#87827,.T.);
#90695=ADVANCED_FACE('',(#8231),#87828,.T.);
#90696=ADVANCED_FACE('',(#8232,#5192),#5649,.T.);
#90697=ADVANCED_FACE('',(#8233),#1858,.T.);
#90698=ADVANCED_FACE('',(#8234,#5193),#5650,.F.);
#90699=ADVANCED_FACE('',(#8235,#5194,#5195,#5196,#5197,#5198,#5199,#5200),
#87829,.F.);
#90700=ADVANCED_FACE('',(#8236),#1859,.T.);
#90701=ADVANCED_FACE('',(#8237,#5201,#5202,#5203,#5204,#5205,#5206,#5207),
#87830,.T.);
#90702=ADVANCED_FACE('',(#8238),#1860,.T.);
#90703=ADVANCED_FACE('',(#8239,#5208),#5651,.T.);
#90704=ADVANCED_FACE('',(#8240),#1861,.T.);
#90705=ADVANCED_FACE('',(#8241),#5652,.F.);
#90706=ADVANCED_FACE('',(#8242),#87831,.F.);
#90707=ADVANCED_FACE('',(#8243),#5653,.T.);
#90708=ADVANCED_FACE('',(#8244),#87832,.F.);
#90709=ADVANCED_FACE('',(#8245),#5654,.F.);
#90710=ADVANCED_FACE('',(#8246),#87833,.F.);
#90711=ADVANCED_FACE('',(#8247),#5655,.T.);
#90712=ADVANCED_FACE('',(#8248),#87834,.F.);
#90713=ADVANCED_FACE('',(#8249),#5656,.F.);
#90714=ADVANCED_FACE('',(#8250),#87835,.F.);
#90715=ADVANCED_FACE('',(#8251),#5657,.T.);
#90716=ADVANCED_FACE('',(#8252),#87836,.F.);
#90717=ADVANCED_FACE('',(#8253),#5658,.F.);
#90718=ADVANCED_FACE('',(#8254),#87837,.F.);
#90719=ADVANCED_FACE('',(#8255),#5659,.T.);
#90720=ADVANCED_FACE('',(#8256),#87838,.F.);
#90721=ADVANCED_FACE('',(#8257),#5660,.F.);
#90722=ADVANCED_FACE('',(#8258),#87839,.F.);
#90723=ADVANCED_FACE('',(#8259),#5661,.T.);
#90724=ADVANCED_FACE('',(#8260),#87840,.F.);
#90725=ADVANCED_FACE('',(#8261),#5662,.F.);
#90726=ADVANCED_FACE('',(#8262),#87841,.F.);
#90727=ADVANCED_FACE('',(#8263),#5663,.T.);
#90728=ADVANCED_FACE('',(#8264),#87842,.F.);
#90729=ADVANCED_FACE('',(#8265),#5664,.F.);
#90730=ADVANCED_FACE('',(#8266),#87843,.F.);
#90731=ADVANCED_FACE('',(#8267),#5665,.T.);
#90732=ADVANCED_FACE('',(#8268),#87844,.F.);
#90733=ADVANCED_FACE('',(#8269),#5666,.F.);
#90734=ADVANCED_FACE('',(#8270),#87845,.F.);
#90735=ADVANCED_FACE('',(#8271),#5667,.T.);
#90736=ADVANCED_FACE('',(#8272),#87846,.F.);
#90737=ADVANCED_FACE('',(#8273),#4861,.T.);
#90738=ADVANCED_FACE('',(#8274),#87847,.T.);
#90739=ADVANCED_FACE('',(#8275),#5668,.F.);
#90740=ADVANCED_FACE('',(#8276),#4862,.T.);
#90741=ADVANCED_FACE('',(#8277),#5669,.T.);
#90742=ADVANCED_FACE('',(#8278),#4863,.T.);
#90743=ADVANCED_FACE('',(#8279),#87848,.T.);
#90744=ADVANCED_FACE('',(#8280),#5670,.F.);
#90745=ADVANCED_FACE('',(#8281),#4864,.T.);
#90746=ADVANCED_FACE('',(#8282),#5671,.T.);
#90747=ADVANCED_FACE('',(#8283),#4865,.T.);
#90748=ADVANCED_FACE('',(#8284),#87849,.T.);
#90749=ADVANCED_FACE('',(#8285),#5672,.F.);
#90750=ADVANCED_FACE('',(#8286),#4866,.T.);
#90751=ADVANCED_FACE('',(#8287),#5673,.T.);
#90752=ADVANCED_FACE('',(#8288),#4867,.T.);
#90753=ADVANCED_FACE('',(#8289),#87850,.T.);
#90754=ADVANCED_FACE('',(#8290),#5674,.F.);
#90755=ADVANCED_FACE('',(#8291),#4868,.T.);
#90756=ADVANCED_FACE('',(#8292),#5675,.T.);
#90757=ADVANCED_FACE('',(#8293),#4869,.T.);
#90758=ADVANCED_FACE('',(#8294),#87851,.T.);
#90759=ADVANCED_FACE('',(#8295),#5676,.F.);
#90760=ADVANCED_FACE('',(#8296),#4870,.T.);
#90761=ADVANCED_FACE('',(#8297),#5677,.T.);
#90762=ADVANCED_FACE('',(#8298),#4871,.T.);
#90763=ADVANCED_FACE('',(#8299),#87852,.T.);
#90764=ADVANCED_FACE('',(#8300),#5678,.F.);
#90765=ADVANCED_FACE('',(#8301),#4872,.T.);
#90766=ADVANCED_FACE('',(#8302),#5679,.T.);
#90767=ADVANCED_FACE('',(#8303),#4873,.T.);
#90768=ADVANCED_FACE('',(#8304),#87853,.T.);
#90769=ADVANCED_FACE('',(#8305),#5680,.F.);
#90770=ADVANCED_FACE('',(#8306),#4874,.T.);
#90771=ADVANCED_FACE('',(#8307),#5681,.T.);
#90772=ADVANCED_FACE('',(#8308),#4875,.T.);
#90773=ADVANCED_FACE('',(#8309),#87854,.T.);
#90774=ADVANCED_FACE('',(#8310),#5682,.F.);
#90775=ADVANCED_FACE('',(#8311),#4876,.T.);
#90776=ADVANCED_FACE('',(#8312),#5683,.T.);
#90777=ADVANCED_FACE('',(#8313),#87855,.T.);
#90778=ADVANCED_FACE('',(#8314),#87856,.T.);
#90779=ADVANCED_FACE('',(#8315),#87857,.T.);
#90780=ADVANCED_FACE('',(#8316),#87858,.T.);
#90781=ADVANCED_FACE('',(#8317),#87859,.T.);
#90782=ADVANCED_FACE('',(#8318),#87860,.T.);
#90783=ADVANCED_FACE('',(#8319),#87861,.T.);
#90784=ADVANCED_FACE('',(#8320),#87862,.T.);
#90785=ADVANCED_FACE('',(#8321),#87863,.T.);
#90786=ADVANCED_FACE('',(#8322),#87864,.T.);
#90787=ADVANCED_FACE('',(#8323),#87865,.T.);
#90788=ADVANCED_FACE('',(#8324),#87866,.T.);
#90789=ADVANCED_FACE('',(#8325),#87867,.T.);
#90790=ADVANCED_FACE('',(#8326),#87868,.T.);
#90791=ADVANCED_FACE('',(#8327),#87869,.T.);
#90792=ADVANCED_FACE('',(#8328),#87870,.T.);
#90793=ADVANCED_FACE('',(#8329),#87871,.T.);
#90794=ADVANCED_FACE('',(#8330),#87872,.T.);
#90795=ADVANCED_FACE('',(#8331),#87873,.T.);
#90796=ADVANCED_FACE('',(#8332),#87874,.T.);
#90797=ADVANCED_FACE('',(#8333),#87875,.T.);
#90798=ADVANCED_FACE('',(#8334),#87876,.T.);
#90799=ADVANCED_FACE('',(#8335),#87877,.T.);
#90800=ADVANCED_FACE('',(#8336),#87878,.T.);
#90801=ADVANCED_FACE('',(#8337),#87879,.T.);
#90802=ADVANCED_FACE('',(#8338),#87880,.T.);
#90803=ADVANCED_FACE('',(#8339),#87881,.T.);
#90804=ADVANCED_FACE('',(#8340),#87882,.T.);
#90805=ADVANCED_FACE('',(#8341),#87883,.T.);
#90806=ADVANCED_FACE('',(#8342),#87884,.T.);
#90807=ADVANCED_FACE('',(#8343),#87885,.T.);
#90808=ADVANCED_FACE('',(#8344),#87886,.T.);
#90809=ADVANCED_FACE('',(#8345),#87887,.T.);
#90810=ADVANCED_FACE('',(#8346),#87888,.T.);
#90811=ADVANCED_FACE('',(#8347),#87889,.T.);
#90812=ADVANCED_FACE('',(#8348),#87890,.T.);
#90813=ADVANCED_FACE('',(#8349),#87891,.T.);
#90814=ADVANCED_FACE('',(#8350),#87892,.T.);
#90815=ADVANCED_FACE('',(#8351),#87893,.T.);
#90816=ADVANCED_FACE('',(#8352),#87894,.T.);
#90817=ADVANCED_FACE('',(#8353),#87895,.T.);
#90818=ADVANCED_FACE('',(#8354),#87896,.T.);
#90819=ADVANCED_FACE('',(#8355),#87897,.T.);
#90820=ADVANCED_FACE('',(#8356),#87898,.T.);
#90821=ADVANCED_FACE('',(#8357),#87899,.T.);
#90822=ADVANCED_FACE('',(#8358),#87900,.T.);
#90823=ADVANCED_FACE('',(#8359),#87901,.T.);
#90824=ADVANCED_FACE('',(#8360),#87902,.T.);
#90825=ADVANCED_FACE('',(#8361),#87903,.T.);
#90826=ADVANCED_FACE('',(#8362),#87904,.T.);
#90827=ADVANCED_FACE('',(#8363),#87905,.T.);
#90828=ADVANCED_FACE('',(#8364),#87906,.T.);
#90829=ADVANCED_FACE('',(#8365),#87907,.T.);
#90830=ADVANCED_FACE('',(#8366),#87908,.T.);
#90831=ADVANCED_FACE('',(#8367),#87909,.T.);
#90832=ADVANCED_FACE('',(#8368),#87910,.T.);
#90833=ADVANCED_FACE('',(#8369),#87911,.T.);
#90834=ADVANCED_FACE('',(#8370),#87912,.T.);
#90835=ADVANCED_FACE('',(#8371),#87913,.T.);
#90836=ADVANCED_FACE('',(#8372),#87914,.T.);
#90837=ADVANCED_FACE('',(#8373),#87915,.T.);
#90838=ADVANCED_FACE('',(#8374),#87916,.T.);
#90839=ADVANCED_FACE('',(#8375),#87917,.T.);
#90840=ADVANCED_FACE('',(#8376),#4877,.F.);
#90841=ADVANCED_FACE('',(#8377,#5209),#142,.T.);
#90842=ADVANCED_FACE('',(#8378),#87918,.T.);
#90843=ADVANCED_FACE('',(#8379),#4878,.T.);
#90844=ADVANCED_FACE('',(#8380),#87919,.T.);
#90845=ADVANCED_FACE('',(#8381),#5684,.T.);
#90846=ADVANCED_FACE('',(#8382,#5210),#5685,.F.);
#90847=ADVANCED_FACE('',(#8383,#5211),#5686,.F.);
#90848=ADVANCED_FACE('',(#8384,#5212),#5687,.F.);
#90849=ADVANCED_FACE('',(#8385),#4879,.F.);
#90850=ADVANCED_FACE('',(#8386),#4880,.F.);
#90851=ADVANCED_FACE('',(#8387),#4881,.F.);
#90852=ADVANCED_FACE('',(#8388),#4882,.F.);
#90853=ADVANCED_FACE('',(#8389),#4883,.F.);
#90854=ADVANCED_FACE('',(#8390),#5688,.T.);
#90855=ADVANCED_FACE('',(#8391),#5689,.F.);
#90856=ADVANCED_FACE('',(#8392),#5690,.F.);
#90857=ADVANCED_FACE('',(#8393),#5691,.F.);
#90858=ADVANCED_FACE('',(#8394),#5692,.F.);
#90859=ADVANCED_FACE('',(#8395),#5693,.F.);
#90860=ADVANCED_FACE('',(#8396),#5694,.F.);
#90861=ADVANCED_FACE('',(#8397),#2307,.T.);
#90862=ADVANCED_FACE('',(#8398),#87920,.T.);
#90863=ADVANCED_FACE('',(#8399),#2308,.T.);
#90864=ADVANCED_FACE('',(#8400),#2309,.F.);
#90865=ADVANCED_FACE('',(#8401),#2310,.T.);
#90866=ADVANCED_FACE('',(#8402),#2311,.F.);
#90867=ADVANCED_FACE('',(#8403),#2312,.F.);
#90868=ADVANCED_FACE('',(#8404),#5695,.T.);
#90869=ADVANCED_FACE('',(#8405),#2313,.T.);
#90870=ADVANCED_FACE('',(#8406),#5696,.T.);
#90871=ADVANCED_FACE('',(#8407),#2314,.F.);
#90872=ADVANCED_FACE('',(#8408),#87921,.F.);
#90873=ADVANCED_FACE('',(#8409),#1862,.F.);
#90874=ADVANCED_FACE('',(#8410),#87922,.F.);
#90875=ADVANCED_FACE('',(#8411),#4884,.T.);
#90876=ADVANCED_FACE('',(#8412),#87923,.T.);
#90877=ADVANCED_FACE('',(#8413),#4885,.T.);
#90878=ADVANCED_FACE('',(#8414,#5213),#5697,.F.);
#90879=ADVANCED_FACE('',(#8415,#5214),#5698,.F.);
#90880=ADVANCED_FACE('',(#8416),#1863,.F.);
#90881=ADVANCED_FACE('',(#8417),#4886,.F.);
#90882=ADVANCED_FACE('',(#8418),#87924,.F.);
#90883=ADVANCED_FACE('',(#8419),#4887,.F.);
#90884=ADVANCED_FACE('',(#8420),#87925,.T.);
#90885=ADVANCED_FACE('',(#8421),#87926,.T.);
#90886=ADVANCED_FACE('',(#8422,#5215),#5699,.F.);
#90887=ADVANCED_FACE('',(#8423,#5216),#5700,.F.);
#90888=ADVANCED_FACE('',(#8424),#143,.T.);
#90889=ADVANCED_FACE('',(#8425),#144,.T.);
#90890=ADVANCED_FACE('',(#8426),#145,.T.);
#90891=ADVANCED_FACE('',(#8427),#146,.T.);
#90892=ADVANCED_FACE('',(#8428),#147,.T.);
#90893=ADVANCED_FACE('',(#8429),#148,.T.);
#90894=ADVANCED_FACE('',(#8430),#149,.T.);
#90895=ADVANCED_FACE('',(#8431),#150,.T.);
#90896=ADVANCED_FACE('',(#8432),#151,.T.);
#90897=ADVANCED_FACE('',(#8433),#152,.T.);
#90898=ADVANCED_FACE('',(#8434),#153,.T.);
#90899=ADVANCED_FACE('',(#8435),#154,.T.);
#90900=ADVANCED_FACE('',(#8436),#87927,.T.);
#90901=ADVANCED_FACE('',(#8437),#87928,.F.);
#90902=ADVANCED_FACE('',(#8438,#5217),#5701,.F.);
#90903=ADVANCED_FACE('',(#8439,#5218),#5702,.F.);
#90904=ADVANCED_FACE('',(#8440),#87929,.T.);
#90905=ADVANCED_FACE('',(#8441),#87930,.F.);
#90906=ADVANCED_FACE('',(#8442,#5219),#5703,.F.);
#90907=ADVANCED_FACE('',(#8443,#5220),#5704,.F.);
#90908=ADVANCED_FACE('',(#8444),#87931,.T.);
#90909=ADVANCED_FACE('',(#8445),#87932,.T.);
#90910=ADVANCED_FACE('',(#8446),#87933,.T.);
#90911=ADVANCED_FACE('',(#8447),#87934,.T.);
#90912=ADVANCED_FACE('',(#8448),#87935,.T.);
#90913=ADVANCED_FACE('',(#8449),#87936,.T.);
#90914=ADVANCED_FACE('',(#8450),#87937,.T.);
#90915=ADVANCED_FACE('',(#8451),#87938,.T.);
#90916=ADVANCED_FACE('',(#8452),#87939,.T.);
#90917=ADVANCED_FACE('',(#8453),#87940,.T.);
#90918=ADVANCED_FACE('',(#8454),#87941,.T.);
#90919=ADVANCED_FACE('',(#8455),#87942,.T.);
#90920=ADVANCED_FACE('',(#8456),#87943,.T.);
#90921=ADVANCED_FACE('',(#8457),#87944,.T.);
#90922=ADVANCED_FACE('',(#8458),#87945,.T.);
#90923=ADVANCED_FACE('',(#8459),#87946,.T.);
#90924=ADVANCED_FACE('',(#8460),#87947,.T.);
#90925=ADVANCED_FACE('',(#8461),#87948,.T.);
#90926=ADVANCED_FACE('',(#8462),#87949,.T.);
#90927=ADVANCED_FACE('',(#8463),#87950,.T.);
#90928=ADVANCED_FACE('',(#8464),#87951,.T.);
#90929=ADVANCED_FACE('',(#8465),#87952,.T.);
#90930=ADVANCED_FACE('',(#8466),#87953,.T.);
#90931=ADVANCED_FACE('',(#8467),#87954,.T.);
#90932=ADVANCED_FACE('',(#8468),#87955,.T.);
#90933=ADVANCED_FACE('',(#8469),#87956,.T.);
#90934=ADVANCED_FACE('',(#8470),#87957,.T.);
#90935=ADVANCED_FACE('',(#8471),#87958,.T.);
#90936=ADVANCED_FACE('',(#8472),#87959,.T.);
#90937=ADVANCED_FACE('',(#8473),#87960,.T.);
#90938=ADVANCED_FACE('',(#8474),#87961,.T.);
#90939=ADVANCED_FACE('',(#8475),#4888,.F.);
#90940=ADVANCED_FACE('',(#8476,#5221),#155,.T.);
#90941=ADVANCED_FACE('',(#8477),#87962,.T.);
#90942=ADVANCED_FACE('',(#8478),#4889,.T.);
#90943=ADVANCED_FACE('',(#8479),#87963,.T.);
#90944=ADVANCED_FACE('',(#8480),#5705,.T.);
#90945=ADVANCED_FACE('',(#8481,#5222),#5706,.F.);
#90946=ADVANCED_FACE('',(#8482,#5223),#5707,.F.);
#90947=ADVANCED_FACE('',(#8483,#5224),#5708,.F.);
#90948=ADVANCED_FACE('',(#8484),#4890,.F.);
#90949=ADVANCED_FACE('',(#8485),#4891,.F.);
#90950=ADVANCED_FACE('',(#8486),#4892,.F.);
#90951=ADVANCED_FACE('',(#8487),#4893,.F.);
#90952=ADVANCED_FACE('',(#8488),#4894,.F.);
#90953=ADVANCED_FACE('',(#8489),#5709,.T.);
#90954=ADVANCED_FACE('',(#8490),#5710,.F.);
#90955=ADVANCED_FACE('',(#8491),#5711,.F.);
#90956=ADVANCED_FACE('',(#8492),#5712,.F.);
#90957=ADVANCED_FACE('',(#8493),#5713,.F.);
#90958=ADVANCED_FACE('',(#8494),#5714,.F.);
#90959=ADVANCED_FACE('',(#8495),#5715,.F.);
#90960=ADVANCED_FACE('',(#8496),#2315,.T.);
#90961=ADVANCED_FACE('',(#8497),#87964,.T.);
#90962=ADVANCED_FACE('',(#8498),#2316,.T.);
#90963=ADVANCED_FACE('',(#8499),#87965,.T.);
#90964=ADVANCED_FACE('',(#8500),#87966,.T.);
#90965=ADVANCED_FACE('',(#8501),#87967,.T.);
#90966=ADVANCED_FACE('',(#8502),#87968,.T.);
#90967=ADVANCED_FACE('',(#8503),#87969,.T.);
#90968=ADVANCED_FACE('',(#8504),#87970,.T.);
#90969=ADVANCED_FACE('',(#8505),#87971,.T.);
#90970=ADVANCED_FACE('',(#8506),#87972,.T.);
#90971=ADVANCED_FACE('',(#8507),#87973,.T.);
#90972=ADVANCED_FACE('',(#8508),#87974,.T.);
#90973=ADVANCED_FACE('',(#8509),#87975,.T.);
#90974=ADVANCED_FACE('',(#8510),#87976,.T.);
#90975=ADVANCED_FACE('',(#8511),#87977,.T.);
#90976=ADVANCED_FACE('',(#8512),#87978,.T.);
#90977=ADVANCED_FACE('',(#8513),#87979,.T.);
#90978=ADVANCED_FACE('',(#8514),#87980,.T.);
#90979=ADVANCED_FACE('',(#8515),#87981,.T.);
#90980=ADVANCED_FACE('',(#8516),#87982,.T.);
#90981=ADVANCED_FACE('',(#8517),#87983,.T.);
#90982=ADVANCED_FACE('',(#8518),#87984,.T.);
#90983=ADVANCED_FACE('',(#8519),#87985,.T.);
#90984=ADVANCED_FACE('',(#8520),#87986,.T.);
#90985=ADVANCED_FACE('',(#8521),#87987,.T.);
#90986=ADVANCED_FACE('',(#8522),#87988,.T.);
#90987=ADVANCED_FACE('',(#8523),#87989,.T.);
#90988=ADVANCED_FACE('',(#8524),#87990,.T.);
#90989=ADVANCED_FACE('',(#8525),#87991,.T.);
#90990=ADVANCED_FACE('',(#8526),#87992,.T.);
#90991=ADVANCED_FACE('',(#8527),#87993,.T.);
#90992=ADVANCED_FACE('',(#8528),#4895,.T.);
#90993=ADVANCED_FACE('',(#8529),#87994,.T.);
#90994=ADVANCED_FACE('',(#8530),#4896,.F.);
#90995=ADVANCED_FACE('',(#8531),#87995,.T.);
#90996=ADVANCED_FACE('',(#8532),#4897,.T.);
#90997=ADVANCED_FACE('',(#8533,#5225),#5716,.F.);
#90998=ADVANCED_FACE('',(#8534),#5717,.T.);
#90999=ADVANCED_FACE('',(#8535),#4898,.F.);
#91000=ADVANCED_FACE('',(#8536),#4899,.F.);
#91001=ADVANCED_FACE('',(#8537),#4900,.F.);
#91002=ADVANCED_FACE('',(#8538),#4901,.F.);
#91003=ADVANCED_FACE('',(#8539),#4902,.F.);
#91004=ADVANCED_FACE('',(#8540),#5718,.T.);
#91005=ADVANCED_FACE('',(#8541),#5719,.F.);
#91006=ADVANCED_FACE('',(#8542),#5720,.F.);
#91007=ADVANCED_FACE('',(#8543),#5721,.F.);
#91008=ADVANCED_FACE('',(#8544),#5722,.F.);
#91009=ADVANCED_FACE('',(#8545),#5723,.F.);
#91010=ADVANCED_FACE('',(#8546),#5724,.F.);
#91011=ADVANCED_FACE('',(#8547),#5725,.F.);
#91012=ADVANCED_FACE('',(#8548),#2317,.T.);
#91013=ADVANCED_FACE('',(#8549),#87996,.T.);
#91014=ADVANCED_FACE('',(#8550),#2318,.T.);
#91015=ADVANCED_FACE('',(#8551),#87997,.T.);
#91016=ADVANCED_FACE('',(#8552),#87998,.T.);
#91017=ADVANCED_FACE('',(#8553),#87999,.T.);
#91018=ADVANCED_FACE('',(#8554),#88000,.T.);
#91019=ADVANCED_FACE('',(#8555),#88001,.T.);
#91020=ADVANCED_FACE('',(#8556),#88002,.T.);
#91021=ADVANCED_FACE('',(#8557),#88003,.T.);
#91022=ADVANCED_FACE('',(#8558),#88004,.T.);
#91023=ADVANCED_FACE('',(#8559),#88005,.T.);
#91024=ADVANCED_FACE('',(#8560),#88006,.T.);
#91025=ADVANCED_FACE('',(#8561),#88007,.T.);
#91026=ADVANCED_FACE('',(#8562),#88008,.T.);
#91027=ADVANCED_FACE('',(#8563),#88009,.T.);
#91028=ADVANCED_FACE('',(#8564),#88010,.T.);
#91029=ADVANCED_FACE('',(#8565),#88011,.T.);
#91030=ADVANCED_FACE('',(#8566),#88012,.T.);
#91031=ADVANCED_FACE('',(#8567),#88013,.T.);
#91032=ADVANCED_FACE('',(#8568),#88014,.T.);
#91033=ADVANCED_FACE('',(#8569),#88015,.T.);
#91034=ADVANCED_FACE('',(#8570),#88016,.T.);
#91035=ADVANCED_FACE('',(#8571),#88017,.T.);
#91036=ADVANCED_FACE('',(#8572),#88018,.T.);
#91037=ADVANCED_FACE('',(#8573),#88019,.T.);
#91038=ADVANCED_FACE('',(#8574),#88020,.T.);
#91039=ADVANCED_FACE('',(#8575),#88021,.T.);
#91040=ADVANCED_FACE('',(#8576),#88022,.T.);
#91041=ADVANCED_FACE('',(#8577),#88023,.T.);
#91042=ADVANCED_FACE('',(#8578),#88024,.T.);
#91043=ADVANCED_FACE('',(#8579),#88025,.T.);
#91044=ADVANCED_FACE('',(#8580),#88026,.T.);
#91045=ADVANCED_FACE('',(#8581),#88027,.T.);
#91046=ADVANCED_FACE('',(#8582),#88028,.T.);
#91047=ADVANCED_FACE('',(#8583),#88029,.T.);
#91048=ADVANCED_FACE('',(#8584),#88030,.T.);
#91049=ADVANCED_FACE('',(#8585),#88031,.T.);
#91050=ADVANCED_FACE('',(#8586),#88032,.T.);
#91051=ADVANCED_FACE('',(#8587),#88033,.T.);
#91052=ADVANCED_FACE('',(#8588),#88034,.T.);
#91053=ADVANCED_FACE('',(#8589),#88035,.T.);
#91054=ADVANCED_FACE('',(#8590),#88036,.T.);
#91055=ADVANCED_FACE('',(#8591),#88037,.T.);
#91056=ADVANCED_FACE('',(#8592),#88038,.T.);
#91057=ADVANCED_FACE('',(#8593),#88039,.T.);
#91058=ADVANCED_FACE('',(#8594),#88040,.T.);
#91059=ADVANCED_FACE('',(#8595),#88041,.T.);
#91060=ADVANCED_FACE('',(#8596),#88042,.T.);
#91061=ADVANCED_FACE('',(#8597),#88043,.T.);
#91062=ADVANCED_FACE('',(#8598),#88044,.T.);
#91063=ADVANCED_FACE('',(#8599),#88045,.T.);
#91064=ADVANCED_FACE('',(#8600),#88046,.T.);
#91065=ADVANCED_FACE('',(#8601),#88047,.T.);
#91066=ADVANCED_FACE('',(#8602),#88048,.T.);
#91067=ADVANCED_FACE('',(#8603),#88049,.T.);
#91068=ADVANCED_FACE('',(#8604),#88050,.T.);
#91069=ADVANCED_FACE('',(#8605),#88051,.T.);
#91070=ADVANCED_FACE('',(#8606),#88052,.T.);
#91071=ADVANCED_FACE('',(#8607),#88053,.T.);
#91072=ADVANCED_FACE('',(#8608),#4903,.T.);
#91073=ADVANCED_FACE('',(#8609),#4904,.T.);
#91074=ADVANCED_FACE('',(#8610),#4905,.T.);
#91075=ADVANCED_FACE('',(#8611),#4906,.T.);
#91076=ADVANCED_FACE('',(#8612),#88054,.T.);
#91077=ADVANCED_FACE('',(#8613),#1864,.F.);
#91078=ADVANCED_FACE('',(#8614),#4907,.F.);
#91079=ADVANCED_FACE('',(#8615),#4908,.F.);
#91080=ADVANCED_FACE('',(#8616),#1865,.T.);
#91081=ADVANCED_FACE('',(#8617),#4909,.T.);
#91082=ADVANCED_FACE('',(#8618),#1866,.T.);
#91083=ADVANCED_FACE('',(#8619),#4910,.T.);
#91084=ADVANCED_FACE('',(#8620),#1867,.T.);
#91085=ADVANCED_FACE('',(#8621),#88055,.T.);
#91086=ADVANCED_FACE('',(#8622),#1868,.T.);
#91087=ADVANCED_FACE('',(#8623),#1869,.T.);
#91088=ADVANCED_FACE('',(#8624),#1870,.T.);
#91089=ADVANCED_FACE('',(#8625),#1871,.T.);
#91090=ADVANCED_FACE('',(#8626),#1872,.T.);
#91091=ADVANCED_FACE('',(#8627),#1873,.T.);
#91092=ADVANCED_FACE('',(#8628),#1874,.T.);
#91093=ADVANCED_FACE('',(#8629),#1875,.T.);
#91094=ADVANCED_FACE('',(#8630),#1876,.T.);
#91095=ADVANCED_FACE('',(#8631),#1877,.T.);
#91096=ADVANCED_FACE('',(#8632),#1878,.T.);
#91097=ADVANCED_FACE('',(#8633),#1879,.T.);
#91098=ADVANCED_FACE('',(#8634),#1880,.T.);
#91099=ADVANCED_FACE('',(#8635),#1881,.T.);
#91100=ADVANCED_FACE('',(#8636),#1882,.T.);
#91101=ADVANCED_FACE('',(#8637),#1883,.T.);
#91102=ADVANCED_FACE('',(#8638),#1884,.T.);
#91103=ADVANCED_FACE('',(#8639),#1885,.T.);
#91104=ADVANCED_FACE('',(#8640),#1886,.T.);
#91105=ADVANCED_FACE('',(#8641),#1887,.T.);
#91106=ADVANCED_FACE('',(#8642),#1888,.T.);
#91107=ADVANCED_FACE('',(#8643),#1889,.T.);
#91108=ADVANCED_FACE('',(#8644),#1890,.T.);
#91109=ADVANCED_FACE('',(#8645),#1891,.T.);
#91110=ADVANCED_FACE('',(#8646),#1892,.T.);
#91111=ADVANCED_FACE('',(#8647),#1893,.T.);
#91112=ADVANCED_FACE('',(#8648),#1894,.T.);
#91113=ADVANCED_FACE('',(#8649),#1895,.T.);
#91114=ADVANCED_FACE('',(#8650),#1896,.T.);
#91115=ADVANCED_FACE('',(#8651),#1897,.T.);
#91116=ADVANCED_FACE('',(#8652),#1898,.T.);
#91117=ADVANCED_FACE('',(#8653),#1899,.T.);
#91118=ADVANCED_FACE('',(#8654),#1900,.T.);
#91119=ADVANCED_FACE('',(#8655),#1901,.T.);
#91120=ADVANCED_FACE('',(#8656),#1902,.T.);
#91121=ADVANCED_FACE('',(#8657),#1903,.T.);
#91122=ADVANCED_FACE('',(#8658),#1904,.T.);
#91123=ADVANCED_FACE('',(#8659),#1905,.T.);
#91124=ADVANCED_FACE('',(#8660),#1906,.T.);
#91125=ADVANCED_FACE('',(#8661),#1907,.T.);
#91126=ADVANCED_FACE('',(#8662),#1908,.T.);
#91127=ADVANCED_FACE('',(#8663),#1909,.T.);
#91128=ADVANCED_FACE('',(#8664),#1910,.T.);
#91129=ADVANCED_FACE('',(#8665),#1911,.T.);
#91130=ADVANCED_FACE('',(#8666),#1912,.T.);
#91131=ADVANCED_FACE('',(#8667),#1913,.T.);
#91132=ADVANCED_FACE('',(#8668),#1914,.T.);
#91133=ADVANCED_FACE('',(#8669),#1915,.T.);
#91134=ADVANCED_FACE('',(#8670),#1916,.T.);
#91135=ADVANCED_FACE('',(#8671),#1917,.T.);
#91136=ADVANCED_FACE('',(#8672),#1918,.T.);
#91137=ADVANCED_FACE('',(#8673),#1919,.T.);
#91138=ADVANCED_FACE('',(#8674),#1920,.T.);
#91139=ADVANCED_FACE('',(#8675),#1921,.T.);
#91140=ADVANCED_FACE('',(#8676),#1922,.T.);
#91141=ADVANCED_FACE('',(#8677),#1923,.T.);
#91142=ADVANCED_FACE('',(#8678),#1924,.T.);
#91143=ADVANCED_FACE('',(#8679),#1925,.T.);
#91144=ADVANCED_FACE('',(#8680),#1926,.T.);
#91145=ADVANCED_FACE('',(#8681),#1927,.T.);
#91146=ADVANCED_FACE('',(#8682),#1928,.T.);
#91147=ADVANCED_FACE('',(#8683),#1929,.T.);
#91148=ADVANCED_FACE('',(#8684),#1930,.T.);
#91149=ADVANCED_FACE('',(#8685),#1931,.T.);
#91150=ADVANCED_FACE('',(#8686),#1932,.T.);
#91151=ADVANCED_FACE('',(#8687),#1933,.T.);
#91152=ADVANCED_FACE('',(#8688),#1934,.T.);
#91153=ADVANCED_FACE('',(#8689),#1935,.T.);
#91154=ADVANCED_FACE('',(#8690),#1936,.T.);
#91155=ADVANCED_FACE('',(#8691),#1937,.T.);
#91156=ADVANCED_FACE('',(#8692),#1938,.T.);
#91157=ADVANCED_FACE('',(#8693),#1939,.T.);
#91158=ADVANCED_FACE('',(#8694),#1940,.T.);
#91159=ADVANCED_FACE('',(#8695),#1941,.T.);
#91160=ADVANCED_FACE('',(#8696),#1942,.T.);
#91161=ADVANCED_FACE('',(#8697),#1943,.T.);
#91162=ADVANCED_FACE('',(#8698),#1944,.T.);
#91163=ADVANCED_FACE('',(#8699),#1945,.T.);
#91164=ADVANCED_FACE('',(#8700),#1946,.T.);
#91165=ADVANCED_FACE('',(#8701),#1947,.T.);
#91166=ADVANCED_FACE('',(#8702),#1948,.T.);
#91167=ADVANCED_FACE('',(#8703),#1949,.T.);
#91168=ADVANCED_FACE('',(#8704),#1950,.T.);
#91169=ADVANCED_FACE('',(#8705),#1951,.T.);
#91170=ADVANCED_FACE('',(#8706),#1952,.T.);
#91171=ADVANCED_FACE('',(#8707),#1953,.T.);
#91172=ADVANCED_FACE('',(#8708),#1954,.T.);
#91173=ADVANCED_FACE('',(#8709),#1955,.T.);
#91174=ADVANCED_FACE('',(#8710),#1956,.T.);
#91175=ADVANCED_FACE('',(#8711),#1957,.T.);
#91176=ADVANCED_FACE('',(#8712),#1958,.T.);
#91177=ADVANCED_FACE('',(#8713),#1959,.T.);
#91178=ADVANCED_FACE('',(#8714),#1960,.T.);
#91179=ADVANCED_FACE('',(#8715),#1961,.T.);
#91180=ADVANCED_FACE('',(#8716),#1962,.T.);
#91181=ADVANCED_FACE('',(#8717),#1963,.T.);
#91182=ADVANCED_FACE('',(#8718),#1964,.T.);
#91183=ADVANCED_FACE('',(#8719),#88056,.F.);
#91184=ADVANCED_FACE('',(#8720),#5726,.F.);
#91185=ADVANCED_FACE('',(#8721),#5727,.F.);
#91186=ADVANCED_FACE('',(#8722),#5728,.F.);
#91187=ADVANCED_FACE('',(#8723),#5729,.F.);
#91188=ADVANCED_FACE('',(#8724),#5730,.F.);
#91189=ADVANCED_FACE('',(#8725),#5731,.F.);
#91190=ADVANCED_FACE('',(#8726),#5732,.F.);
#91191=ADVANCED_FACE('',(#8727,#5226),#5733,.F.);
#91192=ADVANCED_FACE('',(#8728),#1965,.T.);
#91193=ADVANCED_FACE('',(#8729),#5734,.F.);
#91194=ADVANCED_FACE('',(#8730),#5735,.F.);
#91195=ADVANCED_FACE('',(#8731),#5736,.F.);
#91196=ADVANCED_FACE('',(#8732),#5737,.F.);
#91197=ADVANCED_FACE('',(#8733),#5738,.F.);
#91198=ADVANCED_FACE('',(#8734),#5739,.F.);
#91199=ADVANCED_FACE('',(#8735),#5740,.F.);
#91200=ADVANCED_FACE('',(#8736),#4911,.F.);
#91201=ADVANCED_FACE('',(#8737),#4912,.F.);
#91202=ADVANCED_FACE('',(#8738),#4913,.F.);
#91203=ADVANCED_FACE('',(#8739),#4914,.F.);
#91204=ADVANCED_FACE('',(#8740),#4915,.F.);
#91205=ADVANCED_FACE('',(#8741,#5227),#5741,.T.);
#91206=ADVANCED_FACE('',(#8742),#5742,.F.);
#91207=ADVANCED_FACE('',(#8743),#88057,.T.);
#91208=ADVANCED_FACE('',(#8744),#2319,.T.);
#91209=ADVANCED_FACE('',(#8745),#2320,.T.);
#91210=ADVANCED_FACE('',(#8746),#4916,.T.);
#91211=ADVANCED_FACE('',(#8747),#2321,.F.);
#91212=ADVANCED_FACE('',(#8748),#88058,.T.);
#91213=ADVANCED_FACE('',(#8749),#2322,.F.);
#91214=ADVANCED_FACE('',(#8750),#2323,.T.);
#91215=ADVANCED_FACE('',(#8751),#2324,.T.);
#91216=ADVANCED_FACE('',(#8752),#2325,.F.);
#91217=ADVANCED_FACE('',(#8753),#1966,.T.);
#91218=ADVANCED_FACE('',(#8754),#2326,.T.);
#91219=ADVANCED_FACE('',(#8755),#2327,.T.);
#91220=ADVANCED_FACE('',(#8756),#2328,.T.);
#91221=ADVANCED_FACE('',(#8757),#88059,.T.);
#91222=ADVANCED_FACE('',(#8758),#2329,.T.);
#91223=ADVANCED_FACE('',(#8759),#2330,.T.);
#91224=ADVANCED_FACE('',(#8760),#5743,.F.);
#91225=ADVANCED_FACE('',(#8761),#5744,.F.);
#91226=ADVANCED_FACE('',(#8762),#88060,.F.);
#91227=ADVANCED_FACE('',(#8763),#2331,.F.);
#91228=ADVANCED_FACE('',(#8764),#2332,.F.);
#91229=ADVANCED_FACE('',(#8765),#2333,.F.);
#91230=ADVANCED_FACE('',(#8766),#1967,.T.);
#91231=ADVANCED_FACE('',(#8767),#2334,.T.);
#91232=ADVANCED_FACE('',(#8768),#88061,.T.);
#91233=ADVANCED_FACE('',(#8769),#2335,.T.);
#91234=ADVANCED_FACE('',(#8770),#2336,.T.);
#91235=ADVANCED_FACE('',(#8771),#2337,.T.);
#91236=ADVANCED_FACE('',(#8772),#2338,.T.);
#91237=ADVANCED_FACE('',(#8773),#2339,.T.);
#91238=ADVANCED_FACE('',(#8774),#88062,.T.);
#91239=ADVANCED_FACE('',(#8775),#2340,.T.);
#91240=ADVANCED_FACE('',(#8776),#4917,.T.);
#91241=ADVANCED_FACE('',(#8777),#5745,.F.);
#91242=ADVANCED_FACE('',(#8778),#5746,.F.);
#91243=ADVANCED_FACE('',(#8779),#88063,.F.);
#91244=ADVANCED_FACE('',(#8780),#2341,.F.);
#91245=ADVANCED_FACE('',(#8781),#2342,.F.);
#91246=ADVANCED_FACE('',(#8782),#2343,.F.);
#91247=ADVANCED_FACE('',(#8783),#1968,.T.);
#91248=ADVANCED_FACE('',(#8784),#2344,.T.);
#91249=ADVANCED_FACE('',(#8785),#88064,.T.);
#91250=ADVANCED_FACE('',(#8786),#2345,.T.);
#91251=ADVANCED_FACE('',(#8787),#2346,.T.);
#91252=ADVANCED_FACE('',(#8788),#2347,.T.);
#91253=ADVANCED_FACE('',(#8789),#2348,.T.);
#91254=ADVANCED_FACE('',(#8790),#2349,.T.);
#91255=ADVANCED_FACE('',(#8791),#88065,.T.);
#91256=ADVANCED_FACE('',(#8792),#2350,.T.);
#91257=ADVANCED_FACE('',(#8793),#4918,.T.);
#91258=ADVANCED_FACE('',(#8794),#5747,.F.);
#91259=ADVANCED_FACE('',(#8795),#5748,.F.);
#91260=ADVANCED_FACE('',(#8796),#88066,.F.);
#91261=ADVANCED_FACE('',(#8797),#2351,.F.);
#91262=ADVANCED_FACE('',(#8798),#2352,.F.);
#91263=ADVANCED_FACE('',(#8799),#2353,.F.);
#91264=ADVANCED_FACE('',(#8800),#1969,.T.);
#91265=ADVANCED_FACE('',(#8801),#2354,.T.);
#91266=ADVANCED_FACE('',(#8802),#88067,.T.);
#91267=ADVANCED_FACE('',(#8803),#2355,.T.);
#91268=ADVANCED_FACE('',(#8804),#2356,.T.);
#91269=ADVANCED_FACE('',(#8805),#2357,.T.);
#91270=ADVANCED_FACE('',(#8806),#2358,.T.);
#91271=ADVANCED_FACE('',(#8807),#2359,.T.);
#91272=ADVANCED_FACE('',(#8808),#88068,.T.);
#91273=ADVANCED_FACE('',(#8809),#2360,.T.);
#91274=ADVANCED_FACE('',(#8810),#4919,.T.);
#91275=ADVANCED_FACE('',(#8811),#5749,.F.);
#91276=ADVANCED_FACE('',(#8812),#5750,.F.);
#91277=ADVANCED_FACE('',(#8813),#88069,.F.);
#91278=ADVANCED_FACE('',(#8814),#2361,.F.);
#91279=ADVANCED_FACE('',(#8815),#2362,.F.);
#91280=ADVANCED_FACE('',(#8816),#2363,.F.);
#91281=ADVANCED_FACE('',(#8817),#1970,.T.);
#91282=ADVANCED_FACE('',(#8818),#2364,.T.);
#91283=ADVANCED_FACE('',(#8819),#88070,.T.);
#91284=ADVANCED_FACE('',(#8820),#2365,.T.);
#91285=ADVANCED_FACE('',(#8821),#2366,.T.);
#91286=ADVANCED_FACE('',(#8822),#2367,.T.);
#91287=ADVANCED_FACE('',(#8823),#2368,.T.);
#91288=ADVANCED_FACE('',(#8824),#2369,.T.);
#91289=ADVANCED_FACE('',(#8825),#88071,.T.);
#91290=ADVANCED_FACE('',(#8826),#2370,.T.);
#91291=ADVANCED_FACE('',(#8827),#4920,.T.);
#91292=ADVANCED_FACE('',(#8828),#5751,.F.);
#91293=ADVANCED_FACE('',(#8829),#5752,.F.);
#91294=ADVANCED_FACE('',(#8830),#88072,.F.);
#91295=ADVANCED_FACE('',(#8831),#2371,.F.);
#91296=ADVANCED_FACE('',(#8832),#2372,.F.);
#91297=ADVANCED_FACE('',(#8833),#2373,.F.);
#91298=ADVANCED_FACE('',(#8834),#1971,.T.);
#91299=ADVANCED_FACE('',(#8835),#2374,.T.);
#91300=ADVANCED_FACE('',(#8836),#88073,.T.);
#91301=ADVANCED_FACE('',(#8837),#2375,.T.);
#91302=ADVANCED_FACE('',(#8838),#2376,.T.);
#91303=ADVANCED_FACE('',(#8839),#2377,.T.);
#91304=ADVANCED_FACE('',(#8840),#2378,.T.);
#91305=ADVANCED_FACE('',(#8841),#2379,.T.);
#91306=ADVANCED_FACE('',(#8842),#88074,.T.);
#91307=ADVANCED_FACE('',(#8843),#2380,.T.);
#91308=ADVANCED_FACE('',(#8844),#4921,.T.);
#91309=ADVANCED_FACE('',(#8845),#5753,.F.);
#91310=ADVANCED_FACE('',(#8846),#5754,.F.);
#91311=ADVANCED_FACE('',(#8847),#88075,.F.);
#91312=ADVANCED_FACE('',(#8848),#2381,.F.);
#91313=ADVANCED_FACE('',(#8849),#2382,.F.);
#91314=ADVANCED_FACE('',(#8850),#2383,.F.);
#91315=ADVANCED_FACE('',(#8851),#1972,.T.);
#91316=ADVANCED_FACE('',(#8852),#2384,.T.);
#91317=ADVANCED_FACE('',(#8853),#88076,.T.);
#91318=ADVANCED_FACE('',(#8854),#2385,.T.);
#91319=ADVANCED_FACE('',(#8855),#2386,.T.);
#91320=ADVANCED_FACE('',(#8856),#2387,.T.);
#91321=ADVANCED_FACE('',(#8857),#2388,.T.);
#91322=ADVANCED_FACE('',(#8858),#2389,.T.);
#91323=ADVANCED_FACE('',(#8859),#88077,.T.);
#91324=ADVANCED_FACE('',(#8860),#2390,.T.);
#91325=ADVANCED_FACE('',(#8861),#4922,.T.);
#91326=ADVANCED_FACE('',(#8862),#5755,.F.);
#91327=ADVANCED_FACE('',(#8863),#5756,.F.);
#91328=ADVANCED_FACE('',(#8864),#88078,.F.);
#91329=ADVANCED_FACE('',(#8865),#2391,.F.);
#91330=ADVANCED_FACE('',(#8866),#2392,.F.);
#91331=ADVANCED_FACE('',(#8867),#2393,.F.);
#91332=ADVANCED_FACE('',(#8868),#1973,.T.);
#91333=ADVANCED_FACE('',(#8869),#2394,.T.);
#91334=ADVANCED_FACE('',(#8870),#88079,.T.);
#91335=ADVANCED_FACE('',(#8871),#2395,.T.);
#91336=ADVANCED_FACE('',(#8872),#2396,.T.);
#91337=ADVANCED_FACE('',(#8873),#2397,.T.);
#91338=ADVANCED_FACE('',(#8874),#2398,.T.);
#91339=ADVANCED_FACE('',(#8875),#2399,.T.);
#91340=ADVANCED_FACE('',(#8876),#88080,.T.);
#91341=ADVANCED_FACE('',(#8877),#2400,.T.);
#91342=ADVANCED_FACE('',(#8878),#4923,.T.);
#91343=ADVANCED_FACE('',(#8879),#5757,.F.);
#91344=ADVANCED_FACE('',(#8880),#5758,.F.);
#91345=ADVANCED_FACE('',(#8881),#88081,.F.);
#91346=ADVANCED_FACE('',(#8882),#2401,.F.);
#91347=ADVANCED_FACE('',(#8883),#2402,.F.);
#91348=ADVANCED_FACE('',(#8884),#2403,.F.);
#91349=ADVANCED_FACE('',(#8885),#1974,.T.);
#91350=ADVANCED_FACE('',(#8886),#2404,.T.);
#91351=ADVANCED_FACE('',(#8887),#88082,.T.);
#91352=ADVANCED_FACE('',(#8888),#2405,.T.);
#91353=ADVANCED_FACE('',(#8889),#2406,.T.);
#91354=ADVANCED_FACE('',(#8890),#2407,.T.);
#91355=ADVANCED_FACE('',(#8891),#2408,.T.);
#91356=ADVANCED_FACE('',(#8892),#2409,.T.);
#91357=ADVANCED_FACE('',(#8893),#88083,.T.);
#91358=ADVANCED_FACE('',(#8894),#2410,.T.);
#91359=ADVANCED_FACE('',(#8895),#4924,.T.);
#91360=ADVANCED_FACE('',(#8896),#5759,.F.);
#91361=ADVANCED_FACE('',(#8897),#5760,.F.);
#91362=ADVANCED_FACE('',(#8898),#88084,.F.);
#91363=ADVANCED_FACE('',(#8899),#2411,.F.);
#91364=ADVANCED_FACE('',(#8900),#2412,.F.);
#91365=ADVANCED_FACE('',(#8901),#2413,.F.);
#91366=ADVANCED_FACE('',(#8902),#1975,.T.);
#91367=ADVANCED_FACE('',(#8903),#2414,.T.);
#91368=ADVANCED_FACE('',(#8904),#88085,.T.);
#91369=ADVANCED_FACE('',(#8905),#2415,.T.);
#91370=ADVANCED_FACE('',(#8906),#2416,.T.);
#91371=ADVANCED_FACE('',(#8907),#2417,.T.);
#91372=ADVANCED_FACE('',(#8908),#2418,.T.);
#91373=ADVANCED_FACE('',(#8909),#2419,.T.);
#91374=ADVANCED_FACE('',(#8910),#88086,.T.);
#91375=ADVANCED_FACE('',(#8911),#2420,.T.);
#91376=ADVANCED_FACE('',(#8912),#4925,.T.);
#91377=ADVANCED_FACE('',(#8913),#5761,.F.);
#91378=ADVANCED_FACE('',(#8914),#5762,.F.);
#91379=ADVANCED_FACE('',(#8915),#88087,.F.);
#91380=ADVANCED_FACE('',(#8916),#2421,.F.);
#91381=ADVANCED_FACE('',(#8917),#2422,.F.);
#91382=ADVANCED_FACE('',(#8918),#2423,.F.);
#91383=ADVANCED_FACE('',(#8919),#1976,.T.);
#91384=ADVANCED_FACE('',(#8920),#2424,.T.);
#91385=ADVANCED_FACE('',(#8921),#88088,.T.);
#91386=ADVANCED_FACE('',(#8922),#2425,.T.);
#91387=ADVANCED_FACE('',(#8923),#2426,.T.);
#91388=ADVANCED_FACE('',(#8924),#2427,.T.);
#91389=ADVANCED_FACE('',(#8925),#2428,.T.);
#91390=ADVANCED_FACE('',(#8926),#2429,.T.);
#91391=ADVANCED_FACE('',(#8927),#88089,.T.);
#91392=ADVANCED_FACE('',(#8928),#2430,.T.);
#91393=ADVANCED_FACE('',(#8929),#4926,.T.);
#91394=ADVANCED_FACE('',(#8930),#5763,.F.);
#91395=ADVANCED_FACE('',(#8931),#5764,.F.);
#91396=ADVANCED_FACE('',(#8932),#88090,.F.);
#91397=ADVANCED_FACE('',(#8933),#2431,.F.);
#91398=ADVANCED_FACE('',(#8934),#2432,.F.);
#91399=ADVANCED_FACE('',(#8935),#2433,.F.);
#91400=ADVANCED_FACE('',(#8936),#1977,.T.);
#91401=ADVANCED_FACE('',(#8937),#2434,.T.);
#91402=ADVANCED_FACE('',(#8938),#88091,.T.);
#91403=ADVANCED_FACE('',(#8939),#2435,.T.);
#91404=ADVANCED_FACE('',(#8940),#2436,.T.);
#91405=ADVANCED_FACE('',(#8941),#2437,.T.);
#91406=ADVANCED_FACE('',(#8942),#2438,.T.);
#91407=ADVANCED_FACE('',(#8943),#2439,.T.);
#91408=ADVANCED_FACE('',(#8944),#88092,.T.);
#91409=ADVANCED_FACE('',(#8945),#2440,.T.);
#91410=ADVANCED_FACE('',(#8946),#4927,.T.);
#91411=ADVANCED_FACE('',(#8947),#5765,.F.);
#91412=ADVANCED_FACE('',(#8948),#5766,.F.);
#91413=ADVANCED_FACE('',(#8949),#88093,.F.);
#91414=ADVANCED_FACE('',(#8950),#2441,.F.);
#91415=ADVANCED_FACE('',(#8951),#2442,.F.);
#91416=ADVANCED_FACE('',(#8952),#2443,.F.);
#91417=ADVANCED_FACE('',(#8953),#1978,.T.);
#91418=ADVANCED_FACE('',(#8954),#2444,.T.);
#91419=ADVANCED_FACE('',(#8955),#88094,.T.);
#91420=ADVANCED_FACE('',(#8956),#2445,.T.);
#91421=ADVANCED_FACE('',(#8957),#2446,.T.);
#91422=ADVANCED_FACE('',(#8958),#2447,.T.);
#91423=ADVANCED_FACE('',(#8959),#2448,.T.);
#91424=ADVANCED_FACE('',(#8960),#2449,.T.);
#91425=ADVANCED_FACE('',(#8961),#88095,.T.);
#91426=ADVANCED_FACE('',(#8962),#2450,.T.);
#91427=ADVANCED_FACE('',(#8963),#4928,.T.);
#91428=ADVANCED_FACE('',(#8964),#5767,.F.);
#91429=ADVANCED_FACE('',(#8965),#5768,.F.);
#91430=ADVANCED_FACE('',(#8966),#88096,.F.);
#91431=ADVANCED_FACE('',(#8967),#2451,.F.);
#91432=ADVANCED_FACE('',(#8968),#2452,.F.);
#91433=ADVANCED_FACE('',(#8969),#2453,.F.);
#91434=ADVANCED_FACE('',(#8970),#1979,.T.);
#91435=ADVANCED_FACE('',(#8971),#2454,.T.);
#91436=ADVANCED_FACE('',(#8972),#88097,.T.);
#91437=ADVANCED_FACE('',(#8973),#2455,.T.);
#91438=ADVANCED_FACE('',(#8974),#2456,.T.);
#91439=ADVANCED_FACE('',(#8975),#2457,.T.);
#91440=ADVANCED_FACE('',(#8976),#2458,.T.);
#91441=ADVANCED_FACE('',(#8977),#2459,.T.);
#91442=ADVANCED_FACE('',(#8978),#88098,.T.);
#91443=ADVANCED_FACE('',(#8979),#2460,.T.);
#91444=ADVANCED_FACE('',(#8980),#4929,.T.);
#91445=ADVANCED_FACE('',(#8981),#5769,.F.);
#91446=ADVANCED_FACE('',(#8982),#5770,.F.);
#91447=ADVANCED_FACE('',(#8983),#88099,.F.);
#91448=ADVANCED_FACE('',(#8984),#2461,.F.);
#91449=ADVANCED_FACE('',(#8985),#2462,.F.);
#91450=ADVANCED_FACE('',(#8986),#2463,.F.);
#91451=ADVANCED_FACE('',(#8987),#1980,.T.);
#91452=ADVANCED_FACE('',(#8988),#2464,.T.);
#91453=ADVANCED_FACE('',(#8989),#88100,.T.);
#91454=ADVANCED_FACE('',(#8990),#2465,.T.);
#91455=ADVANCED_FACE('',(#8991),#2466,.T.);
#91456=ADVANCED_FACE('',(#8992),#2467,.T.);
#91457=ADVANCED_FACE('',(#8993),#2468,.T.);
#91458=ADVANCED_FACE('',(#8994),#2469,.T.);
#91459=ADVANCED_FACE('',(#8995),#88101,.T.);
#91460=ADVANCED_FACE('',(#8996),#2470,.T.);
#91461=ADVANCED_FACE('',(#8997),#4930,.T.);
#91462=ADVANCED_FACE('',(#8998),#5771,.F.);
#91463=ADVANCED_FACE('',(#8999),#5772,.F.);
#91464=ADVANCED_FACE('',(#9000),#88102,.F.);
#91465=ADVANCED_FACE('',(#9001),#2471,.F.);
#91466=ADVANCED_FACE('',(#9002),#2472,.F.);
#91467=ADVANCED_FACE('',(#9003),#2473,.F.);
#91468=ADVANCED_FACE('',(#9004),#1981,.T.);
#91469=ADVANCED_FACE('',(#9005),#2474,.T.);
#91470=ADVANCED_FACE('',(#9006),#88103,.T.);
#91471=ADVANCED_FACE('',(#9007),#2475,.T.);
#91472=ADVANCED_FACE('',(#9008),#2476,.T.);
#91473=ADVANCED_FACE('',(#9009),#2477,.T.);
#91474=ADVANCED_FACE('',(#9010),#2478,.T.);
#91475=ADVANCED_FACE('',(#9011),#2479,.T.);
#91476=ADVANCED_FACE('',(#9012),#88104,.T.);
#91477=ADVANCED_FACE('',(#9013),#2480,.T.);
#91478=ADVANCED_FACE('',(#9014),#4931,.T.);
#91479=ADVANCED_FACE('',(#9015),#5773,.F.);
#91480=ADVANCED_FACE('',(#9016),#5774,.F.);
#91481=ADVANCED_FACE('',(#9017),#88105,.F.);
#91482=ADVANCED_FACE('',(#9018),#2481,.F.);
#91483=ADVANCED_FACE('',(#9019),#2482,.F.);
#91484=ADVANCED_FACE('',(#9020),#2483,.F.);
#91485=ADVANCED_FACE('',(#9021),#1982,.T.);
#91486=ADVANCED_FACE('',(#9022),#2484,.T.);
#91487=ADVANCED_FACE('',(#9023),#88106,.T.);
#91488=ADVANCED_FACE('',(#9024),#2485,.T.);
#91489=ADVANCED_FACE('',(#9025),#2486,.T.);
#91490=ADVANCED_FACE('',(#9026),#2487,.T.);
#91491=ADVANCED_FACE('',(#9027),#2488,.T.);
#91492=ADVANCED_FACE('',(#9028),#2489,.T.);
#91493=ADVANCED_FACE('',(#9029),#88107,.T.);
#91494=ADVANCED_FACE('',(#9030),#2490,.T.);
#91495=ADVANCED_FACE('',(#9031),#4932,.T.);
#91496=ADVANCED_FACE('',(#9032),#5775,.F.);
#91497=ADVANCED_FACE('',(#9033),#5776,.F.);
#91498=ADVANCED_FACE('',(#9034),#88108,.F.);
#91499=ADVANCED_FACE('',(#9035),#2491,.F.);
#91500=ADVANCED_FACE('',(#9036),#2492,.F.);
#91501=ADVANCED_FACE('',(#9037),#2493,.F.);
#91502=ADVANCED_FACE('',(#9038),#1983,.T.);
#91503=ADVANCED_FACE('',(#9039),#2494,.T.);
#91504=ADVANCED_FACE('',(#9040),#88109,.T.);
#91505=ADVANCED_FACE('',(#9041),#2495,.T.);
#91506=ADVANCED_FACE('',(#9042),#2496,.T.);
#91507=ADVANCED_FACE('',(#9043),#2497,.T.);
#91508=ADVANCED_FACE('',(#9044),#2498,.T.);
#91509=ADVANCED_FACE('',(#9045),#2499,.T.);
#91510=ADVANCED_FACE('',(#9046),#88110,.T.);
#91511=ADVANCED_FACE('',(#9047),#2500,.T.);
#91512=ADVANCED_FACE('',(#9048),#4933,.T.);
#91513=ADVANCED_FACE('',(#9049),#5777,.F.);
#91514=ADVANCED_FACE('',(#9050),#5778,.F.);
#91515=ADVANCED_FACE('',(#9051),#88111,.F.);
#91516=ADVANCED_FACE('',(#9052),#2501,.F.);
#91517=ADVANCED_FACE('',(#9053),#2502,.F.);
#91518=ADVANCED_FACE('',(#9054),#2503,.F.);
#91519=ADVANCED_FACE('',(#9055),#1984,.T.);
#91520=ADVANCED_FACE('',(#9056),#2504,.T.);
#91521=ADVANCED_FACE('',(#9057),#88112,.T.);
#91522=ADVANCED_FACE('',(#9058),#2505,.T.);
#91523=ADVANCED_FACE('',(#9059),#2506,.T.);
#91524=ADVANCED_FACE('',(#9060),#2507,.T.);
#91525=ADVANCED_FACE('',(#9061),#2508,.T.);
#91526=ADVANCED_FACE('',(#9062),#2509,.T.);
#91527=ADVANCED_FACE('',(#9063),#88113,.T.);
#91528=ADVANCED_FACE('',(#9064),#2510,.T.);
#91529=ADVANCED_FACE('',(#9065),#4934,.T.);
#91530=ADVANCED_FACE('',(#9066),#5779,.F.);
#91531=ADVANCED_FACE('',(#9067),#5780,.F.);
#91532=ADVANCED_FACE('',(#9068),#88114,.F.);
#91533=ADVANCED_FACE('',(#9069),#2511,.F.);
#91534=ADVANCED_FACE('',(#9070),#2512,.F.);
#91535=ADVANCED_FACE('',(#9071),#2513,.F.);
#91536=ADVANCED_FACE('',(#9072),#1985,.T.);
#91537=ADVANCED_FACE('',(#9073),#2514,.T.);
#91538=ADVANCED_FACE('',(#9074),#88115,.T.);
#91539=ADVANCED_FACE('',(#9075),#2515,.T.);
#91540=ADVANCED_FACE('',(#9076),#2516,.T.);
#91541=ADVANCED_FACE('',(#9077),#2517,.T.);
#91542=ADVANCED_FACE('',(#9078),#2518,.T.);
#91543=ADVANCED_FACE('',(#9079),#2519,.T.);
#91544=ADVANCED_FACE('',(#9080),#88116,.T.);
#91545=ADVANCED_FACE('',(#9081),#2520,.T.);
#91546=ADVANCED_FACE('',(#9082),#4935,.T.);
#91547=ADVANCED_FACE('',(#9083),#5781,.F.);
#91548=ADVANCED_FACE('',(#9084),#5782,.F.);
#91549=ADVANCED_FACE('',(#9085),#88117,.F.);
#91550=ADVANCED_FACE('',(#9086),#2521,.F.);
#91551=ADVANCED_FACE('',(#9087),#2522,.F.);
#91552=ADVANCED_FACE('',(#9088),#2523,.F.);
#91553=ADVANCED_FACE('',(#9089),#1986,.T.);
#91554=ADVANCED_FACE('',(#9090),#2524,.T.);
#91555=ADVANCED_FACE('',(#9091),#88118,.T.);
#91556=ADVANCED_FACE('',(#9092),#2525,.T.);
#91557=ADVANCED_FACE('',(#9093),#2526,.T.);
#91558=ADVANCED_FACE('',(#9094),#2527,.T.);
#91559=ADVANCED_FACE('',(#9095),#2528,.T.);
#91560=ADVANCED_FACE('',(#9096),#2529,.T.);
#91561=ADVANCED_FACE('',(#9097),#88119,.T.);
#91562=ADVANCED_FACE('',(#9098),#2530,.T.);
#91563=ADVANCED_FACE('',(#9099),#4936,.T.);
#91564=ADVANCED_FACE('',(#9100),#5783,.F.);
#91565=ADVANCED_FACE('',(#9101),#5784,.F.);
#91566=ADVANCED_FACE('',(#9102),#88120,.F.);
#91567=ADVANCED_FACE('',(#9103),#2531,.F.);
#91568=ADVANCED_FACE('',(#9104),#2532,.F.);
#91569=ADVANCED_FACE('',(#9105),#2533,.F.);
#91570=ADVANCED_FACE('',(#9106),#1987,.T.);
#91571=ADVANCED_FACE('',(#9107),#2534,.T.);
#91572=ADVANCED_FACE('',(#9108),#88121,.T.);
#91573=ADVANCED_FACE('',(#9109),#2535,.T.);
#91574=ADVANCED_FACE('',(#9110),#2536,.T.);
#91575=ADVANCED_FACE('',(#9111),#2537,.T.);
#91576=ADVANCED_FACE('',(#9112),#2538,.T.);
#91577=ADVANCED_FACE('',(#9113),#2539,.T.);
#91578=ADVANCED_FACE('',(#9114),#88122,.T.);
#91579=ADVANCED_FACE('',(#9115),#2540,.T.);
#91580=ADVANCED_FACE('',(#9116),#4937,.T.);
#91581=ADVANCED_FACE('',(#9117),#5785,.F.);
#91582=ADVANCED_FACE('',(#9118),#5786,.F.);
#91583=ADVANCED_FACE('',(#9119),#88123,.F.);
#91584=ADVANCED_FACE('',(#9120),#2541,.F.);
#91585=ADVANCED_FACE('',(#9121),#2542,.F.);
#91586=ADVANCED_FACE('',(#9122),#2543,.F.);
#91587=ADVANCED_FACE('',(#9123),#1988,.T.);
#91588=ADVANCED_FACE('',(#9124),#2544,.T.);
#91589=ADVANCED_FACE('',(#9125),#88124,.T.);
#91590=ADVANCED_FACE('',(#9126),#2545,.T.);
#91591=ADVANCED_FACE('',(#9127),#2546,.T.);
#91592=ADVANCED_FACE('',(#9128),#2547,.T.);
#91593=ADVANCED_FACE('',(#9129),#2548,.T.);
#91594=ADVANCED_FACE('',(#9130),#2549,.T.);
#91595=ADVANCED_FACE('',(#9131),#88125,.T.);
#91596=ADVANCED_FACE('',(#9132),#2550,.T.);
#91597=ADVANCED_FACE('',(#9133),#4938,.T.);
#91598=ADVANCED_FACE('',(#9134),#5787,.F.);
#91599=ADVANCED_FACE('',(#9135),#5788,.F.);
#91600=ADVANCED_FACE('',(#9136),#88126,.F.);
#91601=ADVANCED_FACE('',(#9137),#2551,.F.);
#91602=ADVANCED_FACE('',(#9138),#2552,.F.);
#91603=ADVANCED_FACE('',(#9139),#2553,.F.);
#91604=ADVANCED_FACE('',(#9140),#1989,.T.);
#91605=ADVANCED_FACE('',(#9141),#2554,.T.);
#91606=ADVANCED_FACE('',(#9142),#88127,.T.);
#91607=ADVANCED_FACE('',(#9143),#2555,.T.);
#91608=ADVANCED_FACE('',(#9144),#2556,.T.);
#91609=ADVANCED_FACE('',(#9145),#2557,.T.);
#91610=ADVANCED_FACE('',(#9146),#2558,.T.);
#91611=ADVANCED_FACE('',(#9147),#2559,.T.);
#91612=ADVANCED_FACE('',(#9148),#88128,.T.);
#91613=ADVANCED_FACE('',(#9149),#2560,.T.);
#91614=ADVANCED_FACE('',(#9150),#4939,.T.);
#91615=ADVANCED_FACE('',(#9151),#5789,.F.);
#91616=ADVANCED_FACE('',(#9152),#5790,.F.);
#91617=ADVANCED_FACE('',(#9153),#88129,.F.);
#91618=ADVANCED_FACE('',(#9154),#2561,.F.);
#91619=ADVANCED_FACE('',(#9155),#2562,.F.);
#91620=ADVANCED_FACE('',(#9156),#2563,.F.);
#91621=ADVANCED_FACE('',(#9157),#1990,.T.);
#91622=ADVANCED_FACE('',(#9158),#2564,.T.);
#91623=ADVANCED_FACE('',(#9159),#88130,.T.);
#91624=ADVANCED_FACE('',(#9160),#2565,.T.);
#91625=ADVANCED_FACE('',(#9161),#2566,.T.);
#91626=ADVANCED_FACE('',(#9162),#2567,.T.);
#91627=ADVANCED_FACE('',(#9163),#2568,.T.);
#91628=ADVANCED_FACE('',(#9164),#2569,.T.);
#91629=ADVANCED_FACE('',(#9165),#88131,.T.);
#91630=ADVANCED_FACE('',(#9166),#2570,.T.);
#91631=ADVANCED_FACE('',(#9167),#4940,.T.);
#91632=ADVANCED_FACE('',(#9168),#5791,.F.);
#91633=ADVANCED_FACE('',(#9169),#5792,.F.);
#91634=ADVANCED_FACE('',(#9170),#88132,.F.);
#91635=ADVANCED_FACE('',(#9171),#2571,.F.);
#91636=ADVANCED_FACE('',(#9172),#2572,.F.);
#91637=ADVANCED_FACE('',(#9173),#2573,.F.);
#91638=ADVANCED_FACE('',(#9174),#1991,.T.);
#91639=ADVANCED_FACE('',(#9175),#2574,.T.);
#91640=ADVANCED_FACE('',(#9176),#88133,.T.);
#91641=ADVANCED_FACE('',(#9177),#2575,.T.);
#91642=ADVANCED_FACE('',(#9178),#2576,.T.);
#91643=ADVANCED_FACE('',(#9179),#2577,.T.);
#91644=ADVANCED_FACE('',(#9180),#2578,.T.);
#91645=ADVANCED_FACE('',(#9181),#2579,.T.);
#91646=ADVANCED_FACE('',(#9182),#88134,.T.);
#91647=ADVANCED_FACE('',(#9183),#2580,.T.);
#91648=ADVANCED_FACE('',(#9184),#4941,.T.);
#91649=ADVANCED_FACE('',(#9185),#5793,.F.);
#91650=ADVANCED_FACE('',(#9186),#5794,.F.);
#91651=ADVANCED_FACE('',(#9187),#88135,.F.);
#91652=ADVANCED_FACE('',(#9188),#2581,.F.);
#91653=ADVANCED_FACE('',(#9189),#2582,.F.);
#91654=ADVANCED_FACE('',(#9190),#2583,.F.);
#91655=ADVANCED_FACE('',(#9191),#1992,.T.);
#91656=ADVANCED_FACE('',(#9192),#2584,.T.);
#91657=ADVANCED_FACE('',(#9193),#88136,.T.);
#91658=ADVANCED_FACE('',(#9194),#2585,.T.);
#91659=ADVANCED_FACE('',(#9195),#2586,.T.);
#91660=ADVANCED_FACE('',(#9196),#2587,.T.);
#91661=ADVANCED_FACE('',(#9197),#2588,.T.);
#91662=ADVANCED_FACE('',(#9198),#2589,.T.);
#91663=ADVANCED_FACE('',(#9199),#88137,.T.);
#91664=ADVANCED_FACE('',(#9200),#2590,.T.);
#91665=ADVANCED_FACE('',(#9201),#4942,.T.);
#91666=ADVANCED_FACE('',(#9202),#5795,.F.);
#91667=ADVANCED_FACE('',(#9203),#5796,.F.);
#91668=ADVANCED_FACE('',(#9204),#88138,.F.);
#91669=ADVANCED_FACE('',(#9205),#2591,.F.);
#91670=ADVANCED_FACE('',(#9206),#2592,.F.);
#91671=ADVANCED_FACE('',(#9207),#2593,.F.);
#91672=ADVANCED_FACE('',(#9208),#1993,.T.);
#91673=ADVANCED_FACE('',(#9209),#2594,.T.);
#91674=ADVANCED_FACE('',(#9210),#88139,.T.);
#91675=ADVANCED_FACE('',(#9211),#2595,.T.);
#91676=ADVANCED_FACE('',(#9212),#2596,.T.);
#91677=ADVANCED_FACE('',(#9213),#2597,.T.);
#91678=ADVANCED_FACE('',(#9214),#2598,.T.);
#91679=ADVANCED_FACE('',(#9215),#2599,.T.);
#91680=ADVANCED_FACE('',(#9216),#88140,.T.);
#91681=ADVANCED_FACE('',(#9217),#2600,.T.);
#91682=ADVANCED_FACE('',(#9218),#4943,.T.);
#91683=ADVANCED_FACE('',(#9219),#5797,.F.);
#91684=ADVANCED_FACE('',(#9220),#5798,.F.);
#91685=ADVANCED_FACE('',(#9221),#88141,.F.);
#91686=ADVANCED_FACE('',(#9222),#2601,.F.);
#91687=ADVANCED_FACE('',(#9223),#2602,.F.);
#91688=ADVANCED_FACE('',(#9224),#2603,.F.);
#91689=ADVANCED_FACE('',(#9225),#1994,.T.);
#91690=ADVANCED_FACE('',(#9226),#2604,.T.);
#91691=ADVANCED_FACE('',(#9227),#88142,.T.);
#91692=ADVANCED_FACE('',(#9228),#2605,.T.);
#91693=ADVANCED_FACE('',(#9229),#2606,.T.);
#91694=ADVANCED_FACE('',(#9230),#2607,.T.);
#91695=ADVANCED_FACE('',(#9231),#2608,.T.);
#91696=ADVANCED_FACE('',(#9232),#2609,.T.);
#91697=ADVANCED_FACE('',(#9233),#88143,.T.);
#91698=ADVANCED_FACE('',(#9234),#2610,.T.);
#91699=ADVANCED_FACE('',(#9235),#4944,.T.);
#91700=ADVANCED_FACE('',(#9236),#5799,.F.);
#91701=ADVANCED_FACE('',(#9237),#5800,.F.);
#91702=ADVANCED_FACE('',(#9238),#88144,.F.);
#91703=ADVANCED_FACE('',(#9239),#2611,.F.);
#91704=ADVANCED_FACE('',(#9240),#2612,.F.);
#91705=ADVANCED_FACE('',(#9241),#2613,.F.);
#91706=ADVANCED_FACE('',(#9242),#1995,.T.);
#91707=ADVANCED_FACE('',(#9243),#2614,.T.);
#91708=ADVANCED_FACE('',(#9244),#88145,.T.);
#91709=ADVANCED_FACE('',(#9245),#2615,.T.);
#91710=ADVANCED_FACE('',(#9246),#2616,.T.);
#91711=ADVANCED_FACE('',(#9247),#2617,.T.);
#91712=ADVANCED_FACE('',(#9248),#2618,.T.);
#91713=ADVANCED_FACE('',(#9249),#2619,.T.);
#91714=ADVANCED_FACE('',(#9250),#88146,.T.);
#91715=ADVANCED_FACE('',(#9251),#2620,.T.);
#91716=ADVANCED_FACE('',(#9252),#4945,.T.);
#91717=ADVANCED_FACE('',(#9253),#5801,.F.);
#91718=ADVANCED_FACE('',(#9254),#5802,.F.);
#91719=ADVANCED_FACE('',(#9255),#88147,.F.);
#91720=ADVANCED_FACE('',(#9256),#2621,.F.);
#91721=ADVANCED_FACE('',(#9257),#2622,.F.);
#91722=ADVANCED_FACE('',(#9258),#2623,.F.);
#91723=ADVANCED_FACE('',(#9259),#1996,.T.);
#91724=ADVANCED_FACE('',(#9260),#2624,.T.);
#91725=ADVANCED_FACE('',(#9261),#88148,.T.);
#91726=ADVANCED_FACE('',(#9262),#2625,.T.);
#91727=ADVANCED_FACE('',(#9263),#2626,.T.);
#91728=ADVANCED_FACE('',(#9264),#2627,.T.);
#91729=ADVANCED_FACE('',(#9265),#2628,.T.);
#91730=ADVANCED_FACE('',(#9266),#2629,.T.);
#91731=ADVANCED_FACE('',(#9267),#88149,.T.);
#91732=ADVANCED_FACE('',(#9268),#2630,.T.);
#91733=ADVANCED_FACE('',(#9269),#4946,.T.);
#91734=ADVANCED_FACE('',(#9270),#5803,.F.);
#91735=ADVANCED_FACE('',(#9271),#5804,.F.);
#91736=ADVANCED_FACE('',(#9272),#88150,.F.);
#91737=ADVANCED_FACE('',(#9273),#2631,.F.);
#91738=ADVANCED_FACE('',(#9274),#2632,.F.);
#91739=ADVANCED_FACE('',(#9275),#2633,.F.);
#91740=ADVANCED_FACE('',(#9276),#1997,.T.);
#91741=ADVANCED_FACE('',(#9277),#2634,.T.);
#91742=ADVANCED_FACE('',(#9278),#88151,.T.);
#91743=ADVANCED_FACE('',(#9279),#2635,.T.);
#91744=ADVANCED_FACE('',(#9280),#2636,.T.);
#91745=ADVANCED_FACE('',(#9281),#2637,.T.);
#91746=ADVANCED_FACE('',(#9282),#2638,.T.);
#91747=ADVANCED_FACE('',(#9283),#2639,.T.);
#91748=ADVANCED_FACE('',(#9284),#88152,.T.);
#91749=ADVANCED_FACE('',(#9285),#2640,.T.);
#91750=ADVANCED_FACE('',(#9286),#4947,.T.);
#91751=ADVANCED_FACE('',(#9287),#5805,.F.);
#91752=ADVANCED_FACE('',(#9288),#5806,.F.);
#91753=ADVANCED_FACE('',(#9289),#88153,.F.);
#91754=ADVANCED_FACE('',(#9290),#2641,.F.);
#91755=ADVANCED_FACE('',(#9291),#2642,.F.);
#91756=ADVANCED_FACE('',(#9292),#2643,.F.);
#91757=ADVANCED_FACE('',(#9293),#1998,.T.);
#91758=ADVANCED_FACE('',(#9294),#2644,.T.);
#91759=ADVANCED_FACE('',(#9295),#88154,.T.);
#91760=ADVANCED_FACE('',(#9296),#2645,.T.);
#91761=ADVANCED_FACE('',(#9297),#2646,.T.);
#91762=ADVANCED_FACE('',(#9298),#2647,.T.);
#91763=ADVANCED_FACE('',(#9299),#2648,.T.);
#91764=ADVANCED_FACE('',(#9300),#2649,.T.);
#91765=ADVANCED_FACE('',(#9301),#88155,.T.);
#91766=ADVANCED_FACE('',(#9302),#2650,.T.);
#91767=ADVANCED_FACE('',(#9303),#4948,.T.);
#91768=ADVANCED_FACE('',(#9304),#5807,.F.);
#91769=ADVANCED_FACE('',(#9305),#5808,.F.);
#91770=ADVANCED_FACE('',(#9306),#88156,.F.);
#91771=ADVANCED_FACE('',(#9307),#2651,.F.);
#91772=ADVANCED_FACE('',(#9308),#2652,.F.);
#91773=ADVANCED_FACE('',(#9309),#2653,.F.);
#91774=ADVANCED_FACE('',(#9310),#1999,.T.);
#91775=ADVANCED_FACE('',(#9311),#2654,.T.);
#91776=ADVANCED_FACE('',(#9312),#88157,.T.);
#91777=ADVANCED_FACE('',(#9313),#2655,.T.);
#91778=ADVANCED_FACE('',(#9314),#2656,.T.);
#91779=ADVANCED_FACE('',(#9315),#2657,.T.);
#91780=ADVANCED_FACE('',(#9316),#2658,.T.);
#91781=ADVANCED_FACE('',(#9317),#2659,.T.);
#91782=ADVANCED_FACE('',(#9318),#88158,.T.);
#91783=ADVANCED_FACE('',(#9319),#2660,.T.);
#91784=ADVANCED_FACE('',(#9320),#4949,.T.);
#91785=ADVANCED_FACE('',(#9321),#5809,.F.);
#91786=ADVANCED_FACE('',(#9322),#5810,.F.);
#91787=ADVANCED_FACE('',(#9323),#88159,.F.);
#91788=ADVANCED_FACE('',(#9324),#2661,.F.);
#91789=ADVANCED_FACE('',(#9325),#2662,.F.);
#91790=ADVANCED_FACE('',(#9326),#2663,.F.);
#91791=ADVANCED_FACE('',(#9327),#2000,.T.);
#91792=ADVANCED_FACE('',(#9328),#2664,.T.);
#91793=ADVANCED_FACE('',(#9329),#88160,.T.);
#91794=ADVANCED_FACE('',(#9330),#2665,.T.);
#91795=ADVANCED_FACE('',(#9331),#2666,.T.);
#91796=ADVANCED_FACE('',(#9332),#2667,.T.);
#91797=ADVANCED_FACE('',(#9333),#2668,.T.);
#91798=ADVANCED_FACE('',(#9334),#2669,.T.);
#91799=ADVANCED_FACE('',(#9335),#88161,.T.);
#91800=ADVANCED_FACE('',(#9336),#2670,.T.);
#91801=ADVANCED_FACE('',(#9337),#4950,.T.);
#91802=ADVANCED_FACE('',(#9338),#5811,.F.);
#91803=ADVANCED_FACE('',(#9339),#5812,.F.);
#91804=ADVANCED_FACE('',(#9340),#88162,.F.);
#91805=ADVANCED_FACE('',(#9341),#2671,.F.);
#91806=ADVANCED_FACE('',(#9342),#2672,.F.);
#91807=ADVANCED_FACE('',(#9343),#2673,.F.);
#91808=ADVANCED_FACE('',(#9344),#2001,.T.);
#91809=ADVANCED_FACE('',(#9345),#2674,.T.);
#91810=ADVANCED_FACE('',(#9346),#88163,.T.);
#91811=ADVANCED_FACE('',(#9347),#2675,.T.);
#91812=ADVANCED_FACE('',(#9348),#2676,.T.);
#91813=ADVANCED_FACE('',(#9349),#2677,.T.);
#91814=ADVANCED_FACE('',(#9350),#2678,.T.);
#91815=ADVANCED_FACE('',(#9351),#2679,.T.);
#91816=ADVANCED_FACE('',(#9352),#88164,.T.);
#91817=ADVANCED_FACE('',(#9353),#2680,.T.);
#91818=ADVANCED_FACE('',(#9354),#4951,.T.);
#91819=ADVANCED_FACE('',(#9355),#5813,.F.);
#91820=ADVANCED_FACE('',(#9356),#5814,.F.);
#91821=ADVANCED_FACE('',(#9357),#88165,.F.);
#91822=ADVANCED_FACE('',(#9358),#2681,.F.);
#91823=ADVANCED_FACE('',(#9359),#2682,.F.);
#91824=ADVANCED_FACE('',(#9360),#2683,.F.);
#91825=ADVANCED_FACE('',(#9361),#2002,.T.);
#91826=ADVANCED_FACE('',(#9362),#2684,.T.);
#91827=ADVANCED_FACE('',(#9363),#88166,.T.);
#91828=ADVANCED_FACE('',(#9364),#2685,.T.);
#91829=ADVANCED_FACE('',(#9365),#2686,.T.);
#91830=ADVANCED_FACE('',(#9366),#2687,.T.);
#91831=ADVANCED_FACE('',(#9367),#2688,.T.);
#91832=ADVANCED_FACE('',(#9368),#2689,.T.);
#91833=ADVANCED_FACE('',(#9369),#88167,.T.);
#91834=ADVANCED_FACE('',(#9370),#2690,.T.);
#91835=ADVANCED_FACE('',(#9371),#4952,.T.);
#91836=ADVANCED_FACE('',(#9372),#5815,.F.);
#91837=ADVANCED_FACE('',(#9373),#5816,.F.);
#91838=ADVANCED_FACE('',(#9374),#88168,.F.);
#91839=ADVANCED_FACE('',(#9375),#2691,.F.);
#91840=ADVANCED_FACE('',(#9376),#2692,.F.);
#91841=ADVANCED_FACE('',(#9377),#2693,.F.);
#91842=ADVANCED_FACE('',(#9378),#2003,.T.);
#91843=ADVANCED_FACE('',(#9379),#2694,.T.);
#91844=ADVANCED_FACE('',(#9380),#88169,.T.);
#91845=ADVANCED_FACE('',(#9381),#2695,.T.);
#91846=ADVANCED_FACE('',(#9382),#2696,.T.);
#91847=ADVANCED_FACE('',(#9383),#2697,.T.);
#91848=ADVANCED_FACE('',(#9384),#2698,.T.);
#91849=ADVANCED_FACE('',(#9385),#2699,.T.);
#91850=ADVANCED_FACE('',(#9386),#88170,.T.);
#91851=ADVANCED_FACE('',(#9387),#2700,.T.);
#91852=ADVANCED_FACE('',(#9388),#4953,.T.);
#91853=ADVANCED_FACE('',(#9389),#5817,.F.);
#91854=ADVANCED_FACE('',(#9390),#5818,.F.);
#91855=ADVANCED_FACE('',(#9391),#88171,.F.);
#91856=ADVANCED_FACE('',(#9392),#2701,.F.);
#91857=ADVANCED_FACE('',(#9393),#2702,.F.);
#91858=ADVANCED_FACE('',(#9394),#2703,.F.);
#91859=ADVANCED_FACE('',(#9395),#2004,.T.);
#91860=ADVANCED_FACE('',(#9396),#2704,.T.);
#91861=ADVANCED_FACE('',(#9397),#88172,.T.);
#91862=ADVANCED_FACE('',(#9398),#2705,.T.);
#91863=ADVANCED_FACE('',(#9399),#2706,.T.);
#91864=ADVANCED_FACE('',(#9400),#2707,.T.);
#91865=ADVANCED_FACE('',(#9401),#2708,.T.);
#91866=ADVANCED_FACE('',(#9402),#2709,.T.);
#91867=ADVANCED_FACE('',(#9403),#88173,.T.);
#91868=ADVANCED_FACE('',(#9404),#2710,.T.);
#91869=ADVANCED_FACE('',(#9405),#4954,.T.);
#91870=ADVANCED_FACE('',(#9406),#5819,.F.);
#91871=ADVANCED_FACE('',(#9407),#5820,.F.);
#91872=ADVANCED_FACE('',(#9408),#88174,.F.);
#91873=ADVANCED_FACE('',(#9409),#2711,.F.);
#91874=ADVANCED_FACE('',(#9410),#2712,.F.);
#91875=ADVANCED_FACE('',(#9411),#2713,.F.);
#91876=ADVANCED_FACE('',(#9412),#2005,.T.);
#91877=ADVANCED_FACE('',(#9413),#2714,.T.);
#91878=ADVANCED_FACE('',(#9414),#88175,.T.);
#91879=ADVANCED_FACE('',(#9415),#2715,.T.);
#91880=ADVANCED_FACE('',(#9416),#2716,.T.);
#91881=ADVANCED_FACE('',(#9417),#2717,.T.);
#91882=ADVANCED_FACE('',(#9418),#2718,.T.);
#91883=ADVANCED_FACE('',(#9419),#2719,.T.);
#91884=ADVANCED_FACE('',(#9420),#88176,.T.);
#91885=ADVANCED_FACE('',(#9421),#2720,.T.);
#91886=ADVANCED_FACE('',(#9422),#4955,.T.);
#91887=ADVANCED_FACE('',(#9423),#5821,.F.);
#91888=ADVANCED_FACE('',(#9424),#5822,.F.);
#91889=ADVANCED_FACE('',(#9425),#88177,.F.);
#91890=ADVANCED_FACE('',(#9426),#2721,.F.);
#91891=ADVANCED_FACE('',(#9427),#2722,.F.);
#91892=ADVANCED_FACE('',(#9428),#2723,.F.);
#91893=ADVANCED_FACE('',(#9429),#2006,.T.);
#91894=ADVANCED_FACE('',(#9430),#2724,.T.);
#91895=ADVANCED_FACE('',(#9431),#88178,.T.);
#91896=ADVANCED_FACE('',(#9432),#2725,.T.);
#91897=ADVANCED_FACE('',(#9433),#2726,.T.);
#91898=ADVANCED_FACE('',(#9434),#2727,.T.);
#91899=ADVANCED_FACE('',(#9435),#2728,.T.);
#91900=ADVANCED_FACE('',(#9436),#2729,.T.);
#91901=ADVANCED_FACE('',(#9437),#88179,.T.);
#91902=ADVANCED_FACE('',(#9438),#2730,.T.);
#91903=ADVANCED_FACE('',(#9439),#4956,.T.);
#91904=ADVANCED_FACE('',(#9440),#5823,.F.);
#91905=ADVANCED_FACE('',(#9441),#5824,.F.);
#91906=ADVANCED_FACE('',(#9442),#88180,.F.);
#91907=ADVANCED_FACE('',(#9443),#2731,.F.);
#91908=ADVANCED_FACE('',(#9444),#2732,.F.);
#91909=ADVANCED_FACE('',(#9445),#2733,.F.);
#91910=ADVANCED_FACE('',(#9446),#2007,.T.);
#91911=ADVANCED_FACE('',(#9447),#2734,.T.);
#91912=ADVANCED_FACE('',(#9448),#88181,.T.);
#91913=ADVANCED_FACE('',(#9449),#2735,.T.);
#91914=ADVANCED_FACE('',(#9450),#2736,.T.);
#91915=ADVANCED_FACE('',(#9451),#2737,.T.);
#91916=ADVANCED_FACE('',(#9452),#2738,.T.);
#91917=ADVANCED_FACE('',(#9453),#2739,.T.);
#91918=ADVANCED_FACE('',(#9454),#88182,.T.);
#91919=ADVANCED_FACE('',(#9455),#2740,.T.);
#91920=ADVANCED_FACE('',(#9456),#4957,.T.);
#91921=ADVANCED_FACE('',(#9457),#5825,.F.);
#91922=ADVANCED_FACE('',(#9458),#5826,.F.);
#91923=ADVANCED_FACE('',(#9459),#88183,.F.);
#91924=ADVANCED_FACE('',(#9460),#2741,.F.);
#91925=ADVANCED_FACE('',(#9461),#2742,.F.);
#91926=ADVANCED_FACE('',(#9462),#2743,.F.);
#91927=ADVANCED_FACE('',(#9463),#2008,.T.);
#91928=ADVANCED_FACE('',(#9464),#2744,.T.);
#91929=ADVANCED_FACE('',(#9465),#88184,.T.);
#91930=ADVANCED_FACE('',(#9466),#2745,.T.);
#91931=ADVANCED_FACE('',(#9467),#2746,.T.);
#91932=ADVANCED_FACE('',(#9468),#2747,.T.);
#91933=ADVANCED_FACE('',(#9469),#2748,.T.);
#91934=ADVANCED_FACE('',(#9470),#2749,.T.);
#91935=ADVANCED_FACE('',(#9471),#88185,.T.);
#91936=ADVANCED_FACE('',(#9472),#2750,.T.);
#91937=ADVANCED_FACE('',(#9473),#4958,.T.);
#91938=ADVANCED_FACE('',(#9474),#5827,.F.);
#91939=ADVANCED_FACE('',(#9475),#5828,.F.);
#91940=ADVANCED_FACE('',(#9476),#88186,.F.);
#91941=ADVANCED_FACE('',(#9477),#2751,.F.);
#91942=ADVANCED_FACE('',(#9478),#2752,.F.);
#91943=ADVANCED_FACE('',(#9479),#2753,.F.);
#91944=ADVANCED_FACE('',(#9480),#2009,.T.);
#91945=ADVANCED_FACE('',(#9481),#2754,.T.);
#91946=ADVANCED_FACE('',(#9482),#88187,.T.);
#91947=ADVANCED_FACE('',(#9483),#2755,.T.);
#91948=ADVANCED_FACE('',(#9484),#2756,.T.);
#91949=ADVANCED_FACE('',(#9485),#2757,.T.);
#91950=ADVANCED_FACE('',(#9486),#2758,.T.);
#91951=ADVANCED_FACE('',(#9487),#2759,.T.);
#91952=ADVANCED_FACE('',(#9488),#88188,.T.);
#91953=ADVANCED_FACE('',(#9489),#2760,.T.);
#91954=ADVANCED_FACE('',(#9490),#4959,.T.);
#91955=ADVANCED_FACE('',(#9491),#5829,.F.);
#91956=ADVANCED_FACE('',(#9492),#5830,.F.);
#91957=ADVANCED_FACE('',(#9493),#88189,.F.);
#91958=ADVANCED_FACE('',(#9494),#2761,.F.);
#91959=ADVANCED_FACE('',(#9495),#2762,.F.);
#91960=ADVANCED_FACE('',(#9496),#2763,.F.);
#91961=ADVANCED_FACE('',(#9497),#2010,.T.);
#91962=ADVANCED_FACE('',(#9498),#2764,.T.);
#91963=ADVANCED_FACE('',(#9499),#88190,.T.);
#91964=ADVANCED_FACE('',(#9500),#2765,.T.);
#91965=ADVANCED_FACE('',(#9501),#2766,.T.);
#91966=ADVANCED_FACE('',(#9502),#2767,.T.);
#91967=ADVANCED_FACE('',(#9503),#2768,.T.);
#91968=ADVANCED_FACE('',(#9504),#2769,.T.);
#91969=ADVANCED_FACE('',(#9505),#88191,.T.);
#91970=ADVANCED_FACE('',(#9506),#2770,.T.);
#91971=ADVANCED_FACE('',(#9507),#4960,.T.);
#91972=ADVANCED_FACE('',(#9508),#5831,.F.);
#91973=ADVANCED_FACE('',(#9509),#5832,.F.);
#91974=ADVANCED_FACE('',(#9510),#88192,.F.);
#91975=ADVANCED_FACE('',(#9511),#2771,.F.);
#91976=ADVANCED_FACE('',(#9512),#2772,.F.);
#91977=ADVANCED_FACE('',(#9513),#2773,.F.);
#91978=ADVANCED_FACE('',(#9514),#2011,.T.);
#91979=ADVANCED_FACE('',(#9515),#2774,.T.);
#91980=ADVANCED_FACE('',(#9516),#88193,.T.);
#91981=ADVANCED_FACE('',(#9517),#2775,.T.);
#91982=ADVANCED_FACE('',(#9518),#2776,.T.);
#91983=ADVANCED_FACE('',(#9519),#2777,.T.);
#91984=ADVANCED_FACE('',(#9520),#2778,.T.);
#91985=ADVANCED_FACE('',(#9521),#2779,.T.);
#91986=ADVANCED_FACE('',(#9522),#88194,.T.);
#91987=ADVANCED_FACE('',(#9523),#2780,.T.);
#91988=ADVANCED_FACE('',(#9524),#4961,.T.);
#91989=ADVANCED_FACE('',(#9525),#5833,.F.);
#91990=ADVANCED_FACE('',(#9526),#5834,.F.);
#91991=ADVANCED_FACE('',(#9527),#88195,.F.);
#91992=ADVANCED_FACE('',(#9528),#2781,.F.);
#91993=ADVANCED_FACE('',(#9529),#2782,.F.);
#91994=ADVANCED_FACE('',(#9530),#2783,.F.);
#91995=ADVANCED_FACE('',(#9531),#2012,.T.);
#91996=ADVANCED_FACE('',(#9532),#2784,.T.);
#91997=ADVANCED_FACE('',(#9533),#88196,.T.);
#91998=ADVANCED_FACE('',(#9534),#2785,.T.);
#91999=ADVANCED_FACE('',(#9535),#2786,.T.);
#92000=ADVANCED_FACE('',(#9536),#2787,.T.);
#92001=ADVANCED_FACE('',(#9537),#2788,.T.);
#92002=ADVANCED_FACE('',(#9538),#2789,.T.);
#92003=ADVANCED_FACE('',(#9539),#88197,.T.);
#92004=ADVANCED_FACE('',(#9540),#2790,.T.);
#92005=ADVANCED_FACE('',(#9541),#4962,.T.);
#92006=ADVANCED_FACE('',(#9542),#5835,.F.);
#92007=ADVANCED_FACE('',(#9543),#5836,.F.);
#92008=ADVANCED_FACE('',(#9544),#88198,.F.);
#92009=ADVANCED_FACE('',(#9545),#2791,.F.);
#92010=ADVANCED_FACE('',(#9546),#2792,.F.);
#92011=ADVANCED_FACE('',(#9547),#2793,.F.);
#92012=ADVANCED_FACE('',(#9548),#2013,.T.);
#92013=ADVANCED_FACE('',(#9549),#2794,.T.);
#92014=ADVANCED_FACE('',(#9550),#88199,.T.);
#92015=ADVANCED_FACE('',(#9551),#2795,.T.);
#92016=ADVANCED_FACE('',(#9552),#2796,.T.);
#92017=ADVANCED_FACE('',(#9553),#2797,.T.);
#92018=ADVANCED_FACE('',(#9554),#2798,.T.);
#92019=ADVANCED_FACE('',(#9555),#2799,.T.);
#92020=ADVANCED_FACE('',(#9556),#88200,.T.);
#92021=ADVANCED_FACE('',(#9557),#2800,.T.);
#92022=ADVANCED_FACE('',(#9558),#4963,.T.);
#92023=ADVANCED_FACE('',(#9559),#5837,.F.);
#92024=ADVANCED_FACE('',(#9560),#5838,.F.);
#92025=ADVANCED_FACE('',(#9561),#88201,.F.);
#92026=ADVANCED_FACE('',(#9562),#2801,.F.);
#92027=ADVANCED_FACE('',(#9563),#2802,.F.);
#92028=ADVANCED_FACE('',(#9564),#2803,.F.);
#92029=ADVANCED_FACE('',(#9565),#2014,.T.);
#92030=ADVANCED_FACE('',(#9566),#2804,.T.);
#92031=ADVANCED_FACE('',(#9567),#88202,.T.);
#92032=ADVANCED_FACE('',(#9568),#2805,.T.);
#92033=ADVANCED_FACE('',(#9569),#2806,.T.);
#92034=ADVANCED_FACE('',(#9570),#2807,.T.);
#92035=ADVANCED_FACE('',(#9571),#2808,.T.);
#92036=ADVANCED_FACE('',(#9572),#2809,.T.);
#92037=ADVANCED_FACE('',(#9573),#88203,.T.);
#92038=ADVANCED_FACE('',(#9574),#2810,.T.);
#92039=ADVANCED_FACE('',(#9575),#4964,.T.);
#92040=ADVANCED_FACE('',(#9576),#5839,.F.);
#92041=ADVANCED_FACE('',(#9577),#5840,.F.);
#92042=ADVANCED_FACE('',(#9578),#88204,.F.);
#92043=ADVANCED_FACE('',(#9579),#2811,.F.);
#92044=ADVANCED_FACE('',(#9580),#2812,.F.);
#92045=ADVANCED_FACE('',(#9581),#2813,.F.);
#92046=ADVANCED_FACE('',(#9582),#2015,.T.);
#92047=ADVANCED_FACE('',(#9583),#2814,.T.);
#92048=ADVANCED_FACE('',(#9584),#88205,.T.);
#92049=ADVANCED_FACE('',(#9585),#2815,.T.);
#92050=ADVANCED_FACE('',(#9586),#2816,.T.);
#92051=ADVANCED_FACE('',(#9587),#2817,.T.);
#92052=ADVANCED_FACE('',(#9588),#2818,.T.);
#92053=ADVANCED_FACE('',(#9589),#2819,.T.);
#92054=ADVANCED_FACE('',(#9590),#88206,.T.);
#92055=ADVANCED_FACE('',(#9591),#2820,.T.);
#92056=ADVANCED_FACE('',(#9592),#4965,.T.);
#92057=ADVANCED_FACE('',(#9593),#5841,.F.);
#92058=ADVANCED_FACE('',(#9594),#5842,.F.);
#92059=ADVANCED_FACE('',(#9595),#88207,.F.);
#92060=ADVANCED_FACE('',(#9596),#2821,.F.);
#92061=ADVANCED_FACE('',(#9597),#2822,.F.);
#92062=ADVANCED_FACE('',(#9598),#2823,.F.);
#92063=ADVANCED_FACE('',(#9599),#2016,.T.);
#92064=ADVANCED_FACE('',(#9600),#2824,.T.);
#92065=ADVANCED_FACE('',(#9601),#88208,.T.);
#92066=ADVANCED_FACE('',(#9602),#2825,.T.);
#92067=ADVANCED_FACE('',(#9603),#2826,.T.);
#92068=ADVANCED_FACE('',(#9604),#2827,.T.);
#92069=ADVANCED_FACE('',(#9605),#2828,.T.);
#92070=ADVANCED_FACE('',(#9606),#2829,.T.);
#92071=ADVANCED_FACE('',(#9607),#88209,.T.);
#92072=ADVANCED_FACE('',(#9608),#2830,.T.);
#92073=ADVANCED_FACE('',(#9609),#4966,.T.);
#92074=ADVANCED_FACE('',(#9610),#5843,.F.);
#92075=ADVANCED_FACE('',(#9611),#5844,.F.);
#92076=ADVANCED_FACE('',(#9612),#88210,.F.);
#92077=ADVANCED_FACE('',(#9613),#2831,.F.);
#92078=ADVANCED_FACE('',(#9614),#2832,.F.);
#92079=ADVANCED_FACE('',(#9615),#2833,.F.);
#92080=ADVANCED_FACE('',(#9616),#2017,.T.);
#92081=ADVANCED_FACE('',(#9617),#2834,.T.);
#92082=ADVANCED_FACE('',(#9618),#88211,.T.);
#92083=ADVANCED_FACE('',(#9619),#2835,.T.);
#92084=ADVANCED_FACE('',(#9620),#2836,.T.);
#92085=ADVANCED_FACE('',(#9621),#2837,.T.);
#92086=ADVANCED_FACE('',(#9622),#2838,.T.);
#92087=ADVANCED_FACE('',(#9623),#2839,.T.);
#92088=ADVANCED_FACE('',(#9624),#88212,.T.);
#92089=ADVANCED_FACE('',(#9625),#2840,.T.);
#92090=ADVANCED_FACE('',(#9626),#4967,.T.);
#92091=ADVANCED_FACE('',(#9627),#5845,.F.);
#92092=ADVANCED_FACE('',(#9628),#5846,.F.);
#92093=ADVANCED_FACE('',(#9629),#88213,.F.);
#92094=ADVANCED_FACE('',(#9630),#2841,.F.);
#92095=ADVANCED_FACE('',(#9631),#2842,.F.);
#92096=ADVANCED_FACE('',(#9632),#2843,.F.);
#92097=ADVANCED_FACE('',(#9633),#2018,.T.);
#92098=ADVANCED_FACE('',(#9634),#2844,.T.);
#92099=ADVANCED_FACE('',(#9635),#88214,.T.);
#92100=ADVANCED_FACE('',(#9636),#2845,.T.);
#92101=ADVANCED_FACE('',(#9637),#2846,.T.);
#92102=ADVANCED_FACE('',(#9638),#2847,.T.);
#92103=ADVANCED_FACE('',(#9639),#2848,.T.);
#92104=ADVANCED_FACE('',(#9640),#2849,.T.);
#92105=ADVANCED_FACE('',(#9641),#88215,.T.);
#92106=ADVANCED_FACE('',(#9642),#2850,.T.);
#92107=ADVANCED_FACE('',(#9643),#4968,.T.);
#92108=ADVANCED_FACE('',(#9644),#5847,.F.);
#92109=ADVANCED_FACE('',(#9645),#5848,.F.);
#92110=ADVANCED_FACE('',(#9646),#88216,.F.);
#92111=ADVANCED_FACE('',(#9647),#2851,.F.);
#92112=ADVANCED_FACE('',(#9648),#2852,.F.);
#92113=ADVANCED_FACE('',(#9649),#2853,.F.);
#92114=ADVANCED_FACE('',(#9650),#2019,.T.);
#92115=ADVANCED_FACE('',(#9651),#2854,.T.);
#92116=ADVANCED_FACE('',(#9652),#88217,.T.);
#92117=ADVANCED_FACE('',(#9653),#2855,.T.);
#92118=ADVANCED_FACE('',(#9654),#2856,.T.);
#92119=ADVANCED_FACE('',(#9655),#2857,.T.);
#92120=ADVANCED_FACE('',(#9656),#2858,.T.);
#92121=ADVANCED_FACE('',(#9657),#2859,.T.);
#92122=ADVANCED_FACE('',(#9658),#88218,.T.);
#92123=ADVANCED_FACE('',(#9659),#2860,.T.);
#92124=ADVANCED_FACE('',(#9660),#4969,.T.);
#92125=ADVANCED_FACE('',(#9661),#5849,.F.);
#92126=ADVANCED_FACE('',(#9662),#5850,.F.);
#92127=ADVANCED_FACE('',(#9663),#88219,.F.);
#92128=ADVANCED_FACE('',(#9664),#2861,.F.);
#92129=ADVANCED_FACE('',(#9665),#2862,.F.);
#92130=ADVANCED_FACE('',(#9666),#2863,.F.);
#92131=ADVANCED_FACE('',(#9667),#2020,.T.);
#92132=ADVANCED_FACE('',(#9668),#2864,.T.);
#92133=ADVANCED_FACE('',(#9669),#88220,.T.);
#92134=ADVANCED_FACE('',(#9670),#2865,.T.);
#92135=ADVANCED_FACE('',(#9671),#2866,.T.);
#92136=ADVANCED_FACE('',(#9672),#2867,.T.);
#92137=ADVANCED_FACE('',(#9673),#2868,.T.);
#92138=ADVANCED_FACE('',(#9674),#2869,.T.);
#92139=ADVANCED_FACE('',(#9675),#88221,.T.);
#92140=ADVANCED_FACE('',(#9676),#2870,.T.);
#92141=ADVANCED_FACE('',(#9677),#4970,.T.);
#92142=ADVANCED_FACE('',(#9678),#5851,.F.);
#92143=ADVANCED_FACE('',(#9679),#5852,.F.);
#92144=ADVANCED_FACE('',(#9680),#88222,.F.);
#92145=ADVANCED_FACE('',(#9681),#2871,.F.);
#92146=ADVANCED_FACE('',(#9682),#2872,.F.);
#92147=ADVANCED_FACE('',(#9683),#2873,.F.);
#92148=ADVANCED_FACE('',(#9684),#2021,.T.);
#92149=ADVANCED_FACE('',(#9685),#2874,.T.);
#92150=ADVANCED_FACE('',(#9686),#88223,.T.);
#92151=ADVANCED_FACE('',(#9687),#2875,.T.);
#92152=ADVANCED_FACE('',(#9688),#2876,.T.);
#92153=ADVANCED_FACE('',(#9689),#2877,.T.);
#92154=ADVANCED_FACE('',(#9690),#2878,.T.);
#92155=ADVANCED_FACE('',(#9691),#2879,.T.);
#92156=ADVANCED_FACE('',(#9692),#88224,.T.);
#92157=ADVANCED_FACE('',(#9693),#2880,.T.);
#92158=ADVANCED_FACE('',(#9694),#4971,.T.);
#92159=ADVANCED_FACE('',(#9695),#5853,.F.);
#92160=ADVANCED_FACE('',(#9696),#5854,.F.);
#92161=ADVANCED_FACE('',(#9697),#88225,.F.);
#92162=ADVANCED_FACE('',(#9698),#2881,.F.);
#92163=ADVANCED_FACE('',(#9699),#2882,.F.);
#92164=ADVANCED_FACE('',(#9700),#2883,.F.);
#92165=ADVANCED_FACE('',(#9701),#2022,.T.);
#92166=ADVANCED_FACE('',(#9702),#2884,.T.);
#92167=ADVANCED_FACE('',(#9703),#88226,.T.);
#92168=ADVANCED_FACE('',(#9704),#2885,.T.);
#92169=ADVANCED_FACE('',(#9705),#2886,.T.);
#92170=ADVANCED_FACE('',(#9706),#2887,.T.);
#92171=ADVANCED_FACE('',(#9707),#2888,.T.);
#92172=ADVANCED_FACE('',(#9708),#2889,.T.);
#92173=ADVANCED_FACE('',(#9709),#88227,.T.);
#92174=ADVANCED_FACE('',(#9710),#2890,.T.);
#92175=ADVANCED_FACE('',(#9711),#4972,.T.);
#92176=ADVANCED_FACE('',(#9712),#5855,.F.);
#92177=ADVANCED_FACE('',(#9713),#5856,.F.);
#92178=ADVANCED_FACE('',(#9714),#88228,.F.);
#92179=ADVANCED_FACE('',(#9715),#2891,.F.);
#92180=ADVANCED_FACE('',(#9716),#2892,.F.);
#92181=ADVANCED_FACE('',(#9717),#2893,.F.);
#92182=ADVANCED_FACE('',(#9718),#2023,.T.);
#92183=ADVANCED_FACE('',(#9719),#2894,.T.);
#92184=ADVANCED_FACE('',(#9720),#88229,.T.);
#92185=ADVANCED_FACE('',(#9721),#2895,.T.);
#92186=ADVANCED_FACE('',(#9722),#2896,.T.);
#92187=ADVANCED_FACE('',(#9723),#2897,.T.);
#92188=ADVANCED_FACE('',(#9724),#2898,.T.);
#92189=ADVANCED_FACE('',(#9725),#2899,.T.);
#92190=ADVANCED_FACE('',(#9726),#88230,.T.);
#92191=ADVANCED_FACE('',(#9727),#2900,.T.);
#92192=ADVANCED_FACE('',(#9728),#4973,.T.);
#92193=ADVANCED_FACE('',(#9729),#5857,.F.);
#92194=ADVANCED_FACE('',(#9730),#5858,.F.);
#92195=ADVANCED_FACE('',(#9731),#88231,.F.);
#92196=ADVANCED_FACE('',(#9732),#2901,.F.);
#92197=ADVANCED_FACE('',(#9733),#2902,.F.);
#92198=ADVANCED_FACE('',(#9734),#2903,.F.);
#92199=ADVANCED_FACE('',(#9735),#2024,.T.);
#92200=ADVANCED_FACE('',(#9736),#2904,.T.);
#92201=ADVANCED_FACE('',(#9737),#88232,.T.);
#92202=ADVANCED_FACE('',(#9738),#2905,.T.);
#92203=ADVANCED_FACE('',(#9739),#2906,.T.);
#92204=ADVANCED_FACE('',(#9740),#2907,.T.);
#92205=ADVANCED_FACE('',(#9741),#2908,.T.);
#92206=ADVANCED_FACE('',(#9742),#2909,.T.);
#92207=ADVANCED_FACE('',(#9743),#88233,.T.);
#92208=ADVANCED_FACE('',(#9744),#2910,.T.);
#92209=ADVANCED_FACE('',(#9745),#4974,.T.);
#92210=ADVANCED_FACE('',(#9746),#5859,.F.);
#92211=ADVANCED_FACE('',(#9747),#5860,.F.);
#92212=ADVANCED_FACE('',(#9748),#88234,.F.);
#92213=ADVANCED_FACE('',(#9749),#2911,.F.);
#92214=ADVANCED_FACE('',(#9750),#2912,.F.);
#92215=ADVANCED_FACE('',(#9751),#2913,.F.);
#92216=ADVANCED_FACE('',(#9752),#2025,.T.);
#92217=ADVANCED_FACE('',(#9753),#2914,.T.);
#92218=ADVANCED_FACE('',(#9754),#88235,.T.);
#92219=ADVANCED_FACE('',(#9755),#2915,.T.);
#92220=ADVANCED_FACE('',(#9756),#2916,.T.);
#92221=ADVANCED_FACE('',(#9757),#2917,.T.);
#92222=ADVANCED_FACE('',(#9758),#2918,.T.);
#92223=ADVANCED_FACE('',(#9759),#2919,.T.);
#92224=ADVANCED_FACE('',(#9760),#88236,.T.);
#92225=ADVANCED_FACE('',(#9761),#2920,.T.);
#92226=ADVANCED_FACE('',(#9762),#4975,.T.);
#92227=ADVANCED_FACE('',(#9763),#5861,.F.);
#92228=ADVANCED_FACE('',(#9764),#5862,.F.);
#92229=ADVANCED_FACE('',(#9765),#88237,.F.);
#92230=ADVANCED_FACE('',(#9766),#2921,.F.);
#92231=ADVANCED_FACE('',(#9767),#2922,.F.);
#92232=ADVANCED_FACE('',(#9768),#2923,.F.);
#92233=ADVANCED_FACE('',(#9769),#2026,.T.);
#92234=ADVANCED_FACE('',(#9770),#2924,.T.);
#92235=ADVANCED_FACE('',(#9771),#88238,.T.);
#92236=ADVANCED_FACE('',(#9772),#2925,.T.);
#92237=ADVANCED_FACE('',(#9773),#2926,.T.);
#92238=ADVANCED_FACE('',(#9774),#2927,.T.);
#92239=ADVANCED_FACE('',(#9775),#2928,.T.);
#92240=ADVANCED_FACE('',(#9776),#2929,.T.);
#92241=ADVANCED_FACE('',(#9777),#88239,.T.);
#92242=ADVANCED_FACE('',(#9778),#2930,.T.);
#92243=ADVANCED_FACE('',(#9779),#4976,.T.);
#92244=ADVANCED_FACE('',(#9780),#5863,.F.);
#92245=ADVANCED_FACE('',(#9781),#5864,.F.);
#92246=ADVANCED_FACE('',(#9782),#88240,.F.);
#92247=ADVANCED_FACE('',(#9783),#2931,.F.);
#92248=ADVANCED_FACE('',(#9784),#2932,.F.);
#92249=ADVANCED_FACE('',(#9785),#2933,.F.);
#92250=ADVANCED_FACE('',(#9786),#2027,.T.);
#92251=ADVANCED_FACE('',(#9787),#2934,.T.);
#92252=ADVANCED_FACE('',(#9788),#88241,.T.);
#92253=ADVANCED_FACE('',(#9789),#2935,.T.);
#92254=ADVANCED_FACE('',(#9790),#2936,.T.);
#92255=ADVANCED_FACE('',(#9791),#2937,.T.);
#92256=ADVANCED_FACE('',(#9792),#2938,.T.);
#92257=ADVANCED_FACE('',(#9793),#2939,.T.);
#92258=ADVANCED_FACE('',(#9794),#88242,.T.);
#92259=ADVANCED_FACE('',(#9795),#2940,.T.);
#92260=ADVANCED_FACE('',(#9796),#4977,.T.);
#92261=ADVANCED_FACE('',(#9797),#5865,.F.);
#92262=ADVANCED_FACE('',(#9798),#5866,.F.);
#92263=ADVANCED_FACE('',(#9799),#88243,.F.);
#92264=ADVANCED_FACE('',(#9800),#2941,.F.);
#92265=ADVANCED_FACE('',(#9801),#2942,.F.);
#92266=ADVANCED_FACE('',(#9802),#2943,.F.);
#92267=ADVANCED_FACE('',(#9803),#2028,.T.);
#92268=ADVANCED_FACE('',(#9804),#2944,.T.);
#92269=ADVANCED_FACE('',(#9805),#88244,.T.);
#92270=ADVANCED_FACE('',(#9806),#2945,.T.);
#92271=ADVANCED_FACE('',(#9807),#2946,.T.);
#92272=ADVANCED_FACE('',(#9808),#2947,.T.);
#92273=ADVANCED_FACE('',(#9809),#2948,.T.);
#92274=ADVANCED_FACE('',(#9810),#2949,.T.);
#92275=ADVANCED_FACE('',(#9811),#88245,.T.);
#92276=ADVANCED_FACE('',(#9812),#2950,.T.);
#92277=ADVANCED_FACE('',(#9813),#4978,.T.);
#92278=ADVANCED_FACE('',(#9814),#5867,.F.);
#92279=ADVANCED_FACE('',(#9815),#5868,.F.);
#92280=ADVANCED_FACE('',(#9816),#88246,.F.);
#92281=ADVANCED_FACE('',(#9817),#2951,.F.);
#92282=ADVANCED_FACE('',(#9818),#2952,.F.);
#92283=ADVANCED_FACE('',(#9819),#2953,.F.);
#92284=ADVANCED_FACE('',(#9820),#2029,.T.);
#92285=ADVANCED_FACE('',(#9821),#2954,.T.);
#92286=ADVANCED_FACE('',(#9822),#88247,.T.);
#92287=ADVANCED_FACE('',(#9823),#2955,.T.);
#92288=ADVANCED_FACE('',(#9824),#2956,.T.);
#92289=ADVANCED_FACE('',(#9825),#2957,.T.);
#92290=ADVANCED_FACE('',(#9826),#2958,.T.);
#92291=ADVANCED_FACE('',(#9827),#2959,.T.);
#92292=ADVANCED_FACE('',(#9828),#88248,.T.);
#92293=ADVANCED_FACE('',(#9829),#2960,.T.);
#92294=ADVANCED_FACE('',(#9830),#4979,.T.);
#92295=ADVANCED_FACE('',(#9831),#5869,.F.);
#92296=ADVANCED_FACE('',(#9832),#5870,.F.);
#92297=ADVANCED_FACE('',(#9833),#88249,.F.);
#92298=ADVANCED_FACE('',(#9834),#2961,.F.);
#92299=ADVANCED_FACE('',(#9835),#2962,.F.);
#92300=ADVANCED_FACE('',(#9836),#2963,.F.);
#92301=ADVANCED_FACE('',(#9837),#2030,.T.);
#92302=ADVANCED_FACE('',(#9838),#2964,.T.);
#92303=ADVANCED_FACE('',(#9839),#88250,.T.);
#92304=ADVANCED_FACE('',(#9840),#2965,.T.);
#92305=ADVANCED_FACE('',(#9841),#2966,.T.);
#92306=ADVANCED_FACE('',(#9842),#2967,.T.);
#92307=ADVANCED_FACE('',(#9843),#2968,.T.);
#92308=ADVANCED_FACE('',(#9844),#2969,.T.);
#92309=ADVANCED_FACE('',(#9845),#88251,.T.);
#92310=ADVANCED_FACE('',(#9846),#2970,.T.);
#92311=ADVANCED_FACE('',(#9847),#4980,.T.);
#92312=ADVANCED_FACE('',(#9848),#5871,.F.);
#92313=ADVANCED_FACE('',(#9849),#5872,.F.);
#92314=ADVANCED_FACE('',(#9850),#88252,.F.);
#92315=ADVANCED_FACE('',(#9851),#2971,.F.);
#92316=ADVANCED_FACE('',(#9852),#2972,.F.);
#92317=ADVANCED_FACE('',(#9853),#2973,.F.);
#92318=ADVANCED_FACE('',(#9854),#2031,.T.);
#92319=ADVANCED_FACE('',(#9855),#2974,.T.);
#92320=ADVANCED_FACE('',(#9856),#88253,.T.);
#92321=ADVANCED_FACE('',(#9857),#2975,.T.);
#92322=ADVANCED_FACE('',(#9858),#2976,.T.);
#92323=ADVANCED_FACE('',(#9859),#2977,.T.);
#92324=ADVANCED_FACE('',(#9860),#2978,.T.);
#92325=ADVANCED_FACE('',(#9861),#2979,.T.);
#92326=ADVANCED_FACE('',(#9862),#88254,.T.);
#92327=ADVANCED_FACE('',(#9863),#2980,.T.);
#92328=ADVANCED_FACE('',(#9864),#4981,.T.);
#92329=ADVANCED_FACE('',(#9865),#5873,.F.);
#92330=ADVANCED_FACE('',(#9866),#5874,.F.);
#92331=ADVANCED_FACE('',(#9867),#88255,.F.);
#92332=ADVANCED_FACE('',(#9868),#2981,.F.);
#92333=ADVANCED_FACE('',(#9869),#2982,.F.);
#92334=ADVANCED_FACE('',(#9870),#2983,.F.);
#92335=ADVANCED_FACE('',(#9871),#2032,.T.);
#92336=ADVANCED_FACE('',(#9872),#2984,.T.);
#92337=ADVANCED_FACE('',(#9873),#88256,.T.);
#92338=ADVANCED_FACE('',(#9874),#2985,.T.);
#92339=ADVANCED_FACE('',(#9875),#2986,.T.);
#92340=ADVANCED_FACE('',(#9876),#2987,.T.);
#92341=ADVANCED_FACE('',(#9877),#2988,.T.);
#92342=ADVANCED_FACE('',(#9878),#2989,.T.);
#92343=ADVANCED_FACE('',(#9879),#88257,.T.);
#92344=ADVANCED_FACE('',(#9880),#2990,.T.);
#92345=ADVANCED_FACE('',(#9881),#4982,.T.);
#92346=ADVANCED_FACE('',(#9882),#5875,.F.);
#92347=ADVANCED_FACE('',(#9883),#5876,.F.);
#92348=ADVANCED_FACE('',(#9884),#88258,.F.);
#92349=ADVANCED_FACE('',(#9885),#2991,.F.);
#92350=ADVANCED_FACE('',(#9886),#2992,.F.);
#92351=ADVANCED_FACE('',(#9887),#2993,.F.);
#92352=ADVANCED_FACE('',(#9888),#2033,.T.);
#92353=ADVANCED_FACE('',(#9889),#2994,.T.);
#92354=ADVANCED_FACE('',(#9890),#88259,.T.);
#92355=ADVANCED_FACE('',(#9891),#2995,.T.);
#92356=ADVANCED_FACE('',(#9892),#2996,.T.);
#92357=ADVANCED_FACE('',(#9893),#2997,.T.);
#92358=ADVANCED_FACE('',(#9894),#2998,.T.);
#92359=ADVANCED_FACE('',(#9895),#2999,.T.);
#92360=ADVANCED_FACE('',(#9896),#88260,.T.);
#92361=ADVANCED_FACE('',(#9897),#3000,.T.);
#92362=ADVANCED_FACE('',(#9898),#4983,.T.);
#92363=ADVANCED_FACE('',(#9899),#5877,.F.);
#92364=ADVANCED_FACE('',(#9900),#5878,.F.);
#92365=ADVANCED_FACE('',(#9901),#88261,.F.);
#92366=ADVANCED_FACE('',(#9902),#3001,.F.);
#92367=ADVANCED_FACE('',(#9903),#3002,.F.);
#92368=ADVANCED_FACE('',(#9904),#3003,.F.);
#92369=ADVANCED_FACE('',(#9905),#2034,.T.);
#92370=ADVANCED_FACE('',(#9906),#3004,.T.);
#92371=ADVANCED_FACE('',(#9907),#88262,.T.);
#92372=ADVANCED_FACE('',(#9908),#3005,.T.);
#92373=ADVANCED_FACE('',(#9909),#3006,.T.);
#92374=ADVANCED_FACE('',(#9910),#3007,.T.);
#92375=ADVANCED_FACE('',(#9911),#3008,.T.);
#92376=ADVANCED_FACE('',(#9912),#3009,.T.);
#92377=ADVANCED_FACE('',(#9913),#88263,.T.);
#92378=ADVANCED_FACE('',(#9914),#3010,.T.);
#92379=ADVANCED_FACE('',(#9915),#4984,.T.);
#92380=ADVANCED_FACE('',(#9916),#5879,.F.);
#92381=ADVANCED_FACE('',(#9917),#5880,.F.);
#92382=ADVANCED_FACE('',(#9918),#88264,.F.);
#92383=ADVANCED_FACE('',(#9919),#3011,.F.);
#92384=ADVANCED_FACE('',(#9920),#3012,.F.);
#92385=ADVANCED_FACE('',(#9921),#3013,.F.);
#92386=ADVANCED_FACE('',(#9922),#2035,.T.);
#92387=ADVANCED_FACE('',(#9923),#3014,.T.);
#92388=ADVANCED_FACE('',(#9924),#88265,.T.);
#92389=ADVANCED_FACE('',(#9925),#3015,.T.);
#92390=ADVANCED_FACE('',(#9926),#3016,.T.);
#92391=ADVANCED_FACE('',(#9927),#3017,.T.);
#92392=ADVANCED_FACE('',(#9928),#3018,.T.);
#92393=ADVANCED_FACE('',(#9929),#3019,.T.);
#92394=ADVANCED_FACE('',(#9930),#88266,.T.);
#92395=ADVANCED_FACE('',(#9931),#3020,.T.);
#92396=ADVANCED_FACE('',(#9932),#4985,.T.);
#92397=ADVANCED_FACE('',(#9933),#5881,.F.);
#92398=ADVANCED_FACE('',(#9934),#5882,.F.);
#92399=ADVANCED_FACE('',(#9935),#88267,.F.);
#92400=ADVANCED_FACE('',(#9936),#3021,.F.);
#92401=ADVANCED_FACE('',(#9937),#3022,.F.);
#92402=ADVANCED_FACE('',(#9938),#3023,.F.);
#92403=ADVANCED_FACE('',(#9939),#2036,.T.);
#92404=ADVANCED_FACE('',(#9940),#3024,.T.);
#92405=ADVANCED_FACE('',(#9941),#88268,.T.);
#92406=ADVANCED_FACE('',(#9942),#3025,.T.);
#92407=ADVANCED_FACE('',(#9943),#3026,.T.);
#92408=ADVANCED_FACE('',(#9944),#3027,.T.);
#92409=ADVANCED_FACE('',(#9945),#3028,.T.);
#92410=ADVANCED_FACE('',(#9946),#3029,.T.);
#92411=ADVANCED_FACE('',(#9947),#88269,.T.);
#92412=ADVANCED_FACE('',(#9948),#3030,.T.);
#92413=ADVANCED_FACE('',(#9949),#4986,.T.);
#92414=ADVANCED_FACE('',(#9950),#5883,.F.);
#92415=ADVANCED_FACE('',(#9951),#5884,.F.);
#92416=ADVANCED_FACE('',(#9952),#88270,.F.);
#92417=ADVANCED_FACE('',(#9953),#3031,.F.);
#92418=ADVANCED_FACE('',(#9954),#3032,.F.);
#92419=ADVANCED_FACE('',(#9955),#3033,.F.);
#92420=ADVANCED_FACE('',(#9956),#2037,.T.);
#92421=ADVANCED_FACE('',(#9957),#3034,.T.);
#92422=ADVANCED_FACE('',(#9958),#88271,.T.);
#92423=ADVANCED_FACE('',(#9959),#3035,.T.);
#92424=ADVANCED_FACE('',(#9960),#3036,.T.);
#92425=ADVANCED_FACE('',(#9961),#3037,.T.);
#92426=ADVANCED_FACE('',(#9962),#3038,.T.);
#92427=ADVANCED_FACE('',(#9963),#3039,.T.);
#92428=ADVANCED_FACE('',(#9964),#88272,.T.);
#92429=ADVANCED_FACE('',(#9965),#3040,.T.);
#92430=ADVANCED_FACE('',(#9966),#4987,.T.);
#92431=ADVANCED_FACE('',(#9967),#5885,.F.);
#92432=ADVANCED_FACE('',(#9968),#5886,.F.);
#92433=ADVANCED_FACE('',(#9969),#88273,.F.);
#92434=ADVANCED_FACE('',(#9970),#3041,.F.);
#92435=ADVANCED_FACE('',(#9971),#3042,.F.);
#92436=ADVANCED_FACE('',(#9972),#3043,.F.);
#92437=ADVANCED_FACE('',(#9973),#2038,.T.);
#92438=ADVANCED_FACE('',(#9974),#3044,.T.);
#92439=ADVANCED_FACE('',(#9975),#88274,.T.);
#92440=ADVANCED_FACE('',(#9976),#3045,.T.);
#92441=ADVANCED_FACE('',(#9977),#3046,.T.);
#92442=ADVANCED_FACE('',(#9978),#3047,.T.);
#92443=ADVANCED_FACE('',(#9979),#3048,.T.);
#92444=ADVANCED_FACE('',(#9980),#3049,.T.);
#92445=ADVANCED_FACE('',(#9981),#88275,.T.);
#92446=ADVANCED_FACE('',(#9982),#3050,.T.);
#92447=ADVANCED_FACE('',(#9983),#4988,.T.);
#92448=ADVANCED_FACE('',(#9984),#5887,.F.);
#92449=ADVANCED_FACE('',(#9985),#5888,.F.);
#92450=ADVANCED_FACE('',(#9986),#88276,.F.);
#92451=ADVANCED_FACE('',(#9987),#3051,.F.);
#92452=ADVANCED_FACE('',(#9988),#3052,.F.);
#92453=ADVANCED_FACE('',(#9989),#3053,.F.);
#92454=ADVANCED_FACE('',(#9990),#2039,.T.);
#92455=ADVANCED_FACE('',(#9991),#3054,.T.);
#92456=ADVANCED_FACE('',(#9992),#88277,.T.);
#92457=ADVANCED_FACE('',(#9993),#3055,.T.);
#92458=ADVANCED_FACE('',(#9994),#3056,.T.);
#92459=ADVANCED_FACE('',(#9995),#3057,.T.);
#92460=ADVANCED_FACE('',(#9996),#3058,.T.);
#92461=ADVANCED_FACE('',(#9997),#3059,.T.);
#92462=ADVANCED_FACE('',(#9998),#88278,.T.);
#92463=ADVANCED_FACE('',(#9999),#3060,.T.);
#92464=ADVANCED_FACE('',(#10000),#4989,.T.);
#92465=ADVANCED_FACE('',(#10001),#5889,.F.);
#92466=ADVANCED_FACE('',(#10002),#5890,.F.);
#92467=ADVANCED_FACE('',(#10003),#88279,.F.);
#92468=ADVANCED_FACE('',(#10004),#3061,.F.);
#92469=ADVANCED_FACE('',(#10005),#3062,.F.);
#92470=ADVANCED_FACE('',(#10006),#3063,.F.);
#92471=ADVANCED_FACE('',(#10007),#2040,.T.);
#92472=ADVANCED_FACE('',(#10008),#3064,.T.);
#92473=ADVANCED_FACE('',(#10009),#88280,.T.);
#92474=ADVANCED_FACE('',(#10010),#3065,.T.);
#92475=ADVANCED_FACE('',(#10011),#3066,.T.);
#92476=ADVANCED_FACE('',(#10012),#3067,.T.);
#92477=ADVANCED_FACE('',(#10013),#3068,.T.);
#92478=ADVANCED_FACE('',(#10014),#3069,.T.);
#92479=ADVANCED_FACE('',(#10015),#88281,.T.);
#92480=ADVANCED_FACE('',(#10016),#3070,.T.);
#92481=ADVANCED_FACE('',(#10017),#4990,.T.);
#92482=ADVANCED_FACE('',(#10018),#5891,.F.);
#92483=ADVANCED_FACE('',(#10019),#5892,.F.);
#92484=ADVANCED_FACE('',(#10020),#88282,.F.);
#92485=ADVANCED_FACE('',(#10021),#3071,.F.);
#92486=ADVANCED_FACE('',(#10022),#3072,.F.);
#92487=ADVANCED_FACE('',(#10023),#3073,.F.);
#92488=ADVANCED_FACE('',(#10024),#2041,.T.);
#92489=ADVANCED_FACE('',(#10025),#3074,.T.);
#92490=ADVANCED_FACE('',(#10026),#88283,.T.);
#92491=ADVANCED_FACE('',(#10027),#3075,.T.);
#92492=ADVANCED_FACE('',(#10028),#3076,.T.);
#92493=ADVANCED_FACE('',(#10029),#3077,.T.);
#92494=ADVANCED_FACE('',(#10030),#3078,.T.);
#92495=ADVANCED_FACE('',(#10031),#3079,.T.);
#92496=ADVANCED_FACE('',(#10032),#88284,.T.);
#92497=ADVANCED_FACE('',(#10033),#3080,.T.);
#92498=ADVANCED_FACE('',(#10034),#4991,.T.);
#92499=ADVANCED_FACE('',(#10035),#5893,.F.);
#92500=ADVANCED_FACE('',(#10036),#5894,.F.);
#92501=ADVANCED_FACE('',(#10037),#88285,.F.);
#92502=ADVANCED_FACE('',(#10038),#3081,.F.);
#92503=ADVANCED_FACE('',(#10039),#3082,.F.);
#92504=ADVANCED_FACE('',(#10040),#3083,.F.);
#92505=ADVANCED_FACE('',(#10041),#2042,.T.);
#92506=ADVANCED_FACE('',(#10042),#3084,.T.);
#92507=ADVANCED_FACE('',(#10043),#88286,.T.);
#92508=ADVANCED_FACE('',(#10044),#3085,.T.);
#92509=ADVANCED_FACE('',(#10045),#3086,.T.);
#92510=ADVANCED_FACE('',(#10046),#3087,.T.);
#92511=ADVANCED_FACE('',(#10047),#3088,.T.);
#92512=ADVANCED_FACE('',(#10048),#3089,.T.);
#92513=ADVANCED_FACE('',(#10049),#88287,.T.);
#92514=ADVANCED_FACE('',(#10050),#3090,.T.);
#92515=ADVANCED_FACE('',(#10051),#4992,.T.);
#92516=ADVANCED_FACE('',(#10052),#5895,.F.);
#92517=ADVANCED_FACE('',(#10053),#5896,.F.);
#92518=ADVANCED_FACE('',(#10054),#88288,.F.);
#92519=ADVANCED_FACE('',(#10055),#3091,.F.);
#92520=ADVANCED_FACE('',(#10056),#3092,.F.);
#92521=ADVANCED_FACE('',(#10057),#3093,.F.);
#92522=ADVANCED_FACE('',(#10058),#2043,.T.);
#92523=ADVANCED_FACE('',(#10059),#3094,.T.);
#92524=ADVANCED_FACE('',(#10060),#88289,.T.);
#92525=ADVANCED_FACE('',(#10061),#3095,.T.);
#92526=ADVANCED_FACE('',(#10062),#3096,.T.);
#92527=ADVANCED_FACE('',(#10063),#3097,.T.);
#92528=ADVANCED_FACE('',(#10064),#3098,.T.);
#92529=ADVANCED_FACE('',(#10065),#3099,.T.);
#92530=ADVANCED_FACE('',(#10066),#88290,.T.);
#92531=ADVANCED_FACE('',(#10067),#3100,.T.);
#92532=ADVANCED_FACE('',(#10068),#4993,.T.);
#92533=ADVANCED_FACE('',(#10069),#5897,.F.);
#92534=ADVANCED_FACE('',(#10070),#5898,.F.);
#92535=ADVANCED_FACE('',(#10071),#88291,.F.);
#92536=ADVANCED_FACE('',(#10072),#3101,.F.);
#92537=ADVANCED_FACE('',(#10073),#3102,.F.);
#92538=ADVANCED_FACE('',(#10074),#3103,.F.);
#92539=ADVANCED_FACE('',(#10075),#2044,.T.);
#92540=ADVANCED_FACE('',(#10076),#3104,.T.);
#92541=ADVANCED_FACE('',(#10077),#88292,.T.);
#92542=ADVANCED_FACE('',(#10078),#3105,.T.);
#92543=ADVANCED_FACE('',(#10079),#3106,.T.);
#92544=ADVANCED_FACE('',(#10080),#3107,.T.);
#92545=ADVANCED_FACE('',(#10081),#3108,.T.);
#92546=ADVANCED_FACE('',(#10082),#3109,.T.);
#92547=ADVANCED_FACE('',(#10083),#88293,.T.);
#92548=ADVANCED_FACE('',(#10084),#3110,.T.);
#92549=ADVANCED_FACE('',(#10085),#4994,.T.);
#92550=ADVANCED_FACE('',(#10086),#5899,.F.);
#92551=ADVANCED_FACE('',(#10087),#5900,.F.);
#92552=ADVANCED_FACE('',(#10088),#88294,.F.);
#92553=ADVANCED_FACE('',(#10089),#3111,.F.);
#92554=ADVANCED_FACE('',(#10090),#3112,.F.);
#92555=ADVANCED_FACE('',(#10091),#3113,.F.);
#92556=ADVANCED_FACE('',(#10092),#2045,.T.);
#92557=ADVANCED_FACE('',(#10093),#3114,.T.);
#92558=ADVANCED_FACE('',(#10094),#88295,.T.);
#92559=ADVANCED_FACE('',(#10095),#3115,.T.);
#92560=ADVANCED_FACE('',(#10096),#3116,.T.);
#92561=ADVANCED_FACE('',(#10097),#3117,.T.);
#92562=ADVANCED_FACE('',(#10098),#3118,.T.);
#92563=ADVANCED_FACE('',(#10099),#3119,.T.);
#92564=ADVANCED_FACE('',(#10100),#88296,.T.);
#92565=ADVANCED_FACE('',(#10101),#3120,.T.);
#92566=ADVANCED_FACE('',(#10102),#4995,.T.);
#92567=ADVANCED_FACE('',(#10103),#5901,.F.);
#92568=ADVANCED_FACE('',(#10104),#5902,.F.);
#92569=ADVANCED_FACE('',(#10105),#88297,.F.);
#92570=ADVANCED_FACE('',(#10106),#3121,.F.);
#92571=ADVANCED_FACE('',(#10107),#3122,.F.);
#92572=ADVANCED_FACE('',(#10108),#3123,.F.);
#92573=ADVANCED_FACE('',(#10109),#2046,.T.);
#92574=ADVANCED_FACE('',(#10110),#3124,.T.);
#92575=ADVANCED_FACE('',(#10111),#88298,.T.);
#92576=ADVANCED_FACE('',(#10112),#3125,.T.);
#92577=ADVANCED_FACE('',(#10113),#3126,.T.);
#92578=ADVANCED_FACE('',(#10114),#3127,.T.);
#92579=ADVANCED_FACE('',(#10115),#3128,.T.);
#92580=ADVANCED_FACE('',(#10116),#3129,.T.);
#92581=ADVANCED_FACE('',(#10117),#88299,.T.);
#92582=ADVANCED_FACE('',(#10118),#3130,.T.);
#92583=ADVANCED_FACE('',(#10119),#4996,.T.);
#92584=ADVANCED_FACE('',(#10120),#5903,.F.);
#92585=ADVANCED_FACE('',(#10121),#5904,.F.);
#92586=ADVANCED_FACE('',(#10122),#88300,.F.);
#92587=ADVANCED_FACE('',(#10123),#3131,.F.);
#92588=ADVANCED_FACE('',(#10124),#3132,.F.);
#92589=ADVANCED_FACE('',(#10125),#3133,.F.);
#92590=ADVANCED_FACE('',(#10126),#2047,.T.);
#92591=ADVANCED_FACE('',(#10127),#3134,.T.);
#92592=ADVANCED_FACE('',(#10128),#88301,.T.);
#92593=ADVANCED_FACE('',(#10129),#3135,.T.);
#92594=ADVANCED_FACE('',(#10130),#3136,.T.);
#92595=ADVANCED_FACE('',(#10131),#3137,.T.);
#92596=ADVANCED_FACE('',(#10132),#3138,.T.);
#92597=ADVANCED_FACE('',(#10133),#3139,.T.);
#92598=ADVANCED_FACE('',(#10134),#88302,.T.);
#92599=ADVANCED_FACE('',(#10135),#3140,.T.);
#92600=ADVANCED_FACE('',(#10136),#4997,.T.);
#92601=ADVANCED_FACE('',(#10137),#5905,.F.);
#92602=ADVANCED_FACE('',(#10138),#5906,.F.);
#92603=ADVANCED_FACE('',(#10139),#88303,.F.);
#92604=ADVANCED_FACE('',(#10140),#3141,.F.);
#92605=ADVANCED_FACE('',(#10141),#3142,.F.);
#92606=ADVANCED_FACE('',(#10142),#3143,.F.);
#92607=ADVANCED_FACE('',(#10143),#2048,.T.);
#92608=ADVANCED_FACE('',(#10144),#3144,.T.);
#92609=ADVANCED_FACE('',(#10145),#88304,.T.);
#92610=ADVANCED_FACE('',(#10146),#3145,.T.);
#92611=ADVANCED_FACE('',(#10147),#3146,.T.);
#92612=ADVANCED_FACE('',(#10148),#3147,.T.);
#92613=ADVANCED_FACE('',(#10149),#3148,.T.);
#92614=ADVANCED_FACE('',(#10150),#3149,.T.);
#92615=ADVANCED_FACE('',(#10151),#88305,.T.);
#92616=ADVANCED_FACE('',(#10152),#3150,.T.);
#92617=ADVANCED_FACE('',(#10153),#4998,.T.);
#92618=ADVANCED_FACE('',(#10154),#5907,.F.);
#92619=ADVANCED_FACE('',(#10155),#5908,.F.);
#92620=ADVANCED_FACE('',(#10156),#88306,.F.);
#92621=ADVANCED_FACE('',(#10157),#3151,.F.);
#92622=ADVANCED_FACE('',(#10158),#3152,.F.);
#92623=ADVANCED_FACE('',(#10159),#3153,.F.);
#92624=ADVANCED_FACE('',(#10160),#2049,.T.);
#92625=ADVANCED_FACE('',(#10161),#3154,.T.);
#92626=ADVANCED_FACE('',(#10162),#88307,.T.);
#92627=ADVANCED_FACE('',(#10163),#3155,.T.);
#92628=ADVANCED_FACE('',(#10164),#3156,.T.);
#92629=ADVANCED_FACE('',(#10165),#3157,.T.);
#92630=ADVANCED_FACE('',(#10166),#3158,.T.);
#92631=ADVANCED_FACE('',(#10167),#3159,.T.);
#92632=ADVANCED_FACE('',(#10168),#88308,.T.);
#92633=ADVANCED_FACE('',(#10169),#3160,.T.);
#92634=ADVANCED_FACE('',(#10170),#4999,.T.);
#92635=ADVANCED_FACE('',(#10171),#5909,.F.);
#92636=ADVANCED_FACE('',(#10172),#5910,.F.);
#92637=ADVANCED_FACE('',(#10173),#88309,.F.);
#92638=ADVANCED_FACE('',(#10174),#3161,.F.);
#92639=ADVANCED_FACE('',(#10175),#3162,.F.);
#92640=ADVANCED_FACE('',(#10176),#3163,.F.);
#92641=ADVANCED_FACE('',(#10177),#2050,.T.);
#92642=ADVANCED_FACE('',(#10178),#3164,.T.);
#92643=ADVANCED_FACE('',(#10179),#88310,.T.);
#92644=ADVANCED_FACE('',(#10180),#3165,.T.);
#92645=ADVANCED_FACE('',(#10181),#3166,.T.);
#92646=ADVANCED_FACE('',(#10182),#3167,.T.);
#92647=ADVANCED_FACE('',(#10183),#3168,.T.);
#92648=ADVANCED_FACE('',(#10184),#3169,.T.);
#92649=ADVANCED_FACE('',(#10185),#88311,.T.);
#92650=ADVANCED_FACE('',(#10186),#3170,.T.);
#92651=ADVANCED_FACE('',(#10187),#5000,.T.);
#92652=ADVANCED_FACE('',(#10188),#5911,.F.);
#92653=ADVANCED_FACE('',(#10189),#5912,.F.);
#92654=ADVANCED_FACE('',(#10190),#88312,.F.);
#92655=ADVANCED_FACE('',(#10191),#3171,.F.);
#92656=ADVANCED_FACE('',(#10192),#3172,.F.);
#92657=ADVANCED_FACE('',(#10193),#3173,.F.);
#92658=ADVANCED_FACE('',(#10194),#2051,.T.);
#92659=ADVANCED_FACE('',(#10195),#3174,.T.);
#92660=ADVANCED_FACE('',(#10196),#88313,.T.);
#92661=ADVANCED_FACE('',(#10197),#3175,.T.);
#92662=ADVANCED_FACE('',(#10198),#3176,.T.);
#92663=ADVANCED_FACE('',(#10199),#3177,.T.);
#92664=ADVANCED_FACE('',(#10200),#3178,.T.);
#92665=ADVANCED_FACE('',(#10201),#3179,.T.);
#92666=ADVANCED_FACE('',(#10202),#88314,.T.);
#92667=ADVANCED_FACE('',(#10203),#3180,.T.);
#92668=ADVANCED_FACE('',(#10204),#5001,.T.);
#92669=ADVANCED_FACE('',(#10205),#5913,.F.);
#92670=ADVANCED_FACE('',(#10206),#5914,.F.);
#92671=ADVANCED_FACE('',(#10207),#88315,.F.);
#92672=ADVANCED_FACE('',(#10208),#3181,.F.);
#92673=ADVANCED_FACE('',(#10209),#3182,.F.);
#92674=ADVANCED_FACE('',(#10210),#3183,.F.);
#92675=ADVANCED_FACE('',(#10211),#2052,.T.);
#92676=ADVANCED_FACE('',(#10212),#3184,.T.);
#92677=ADVANCED_FACE('',(#10213),#88316,.T.);
#92678=ADVANCED_FACE('',(#10214),#3185,.T.);
#92679=ADVANCED_FACE('',(#10215),#3186,.T.);
#92680=ADVANCED_FACE('',(#10216),#3187,.T.);
#92681=ADVANCED_FACE('',(#10217),#3188,.T.);
#92682=ADVANCED_FACE('',(#10218),#3189,.T.);
#92683=ADVANCED_FACE('',(#10219),#88317,.T.);
#92684=ADVANCED_FACE('',(#10220),#3190,.T.);
#92685=ADVANCED_FACE('',(#10221),#5002,.T.);
#92686=ADVANCED_FACE('',(#10222),#5915,.F.);
#92687=ADVANCED_FACE('',(#10223),#5916,.F.);
#92688=ADVANCED_FACE('',(#10224),#88318,.F.);
#92689=ADVANCED_FACE('',(#10225),#3191,.F.);
#92690=ADVANCED_FACE('',(#10226),#3192,.F.);
#92691=ADVANCED_FACE('',(#10227),#3193,.F.);
#92692=ADVANCED_FACE('',(#10228),#2053,.T.);
#92693=ADVANCED_FACE('',(#10229),#3194,.T.);
#92694=ADVANCED_FACE('',(#10230),#88319,.T.);
#92695=ADVANCED_FACE('',(#10231),#3195,.T.);
#92696=ADVANCED_FACE('',(#10232),#3196,.T.);
#92697=ADVANCED_FACE('',(#10233),#3197,.T.);
#92698=ADVANCED_FACE('',(#10234),#3198,.T.);
#92699=ADVANCED_FACE('',(#10235),#3199,.T.);
#92700=ADVANCED_FACE('',(#10236),#88320,.T.);
#92701=ADVANCED_FACE('',(#10237),#3200,.T.);
#92702=ADVANCED_FACE('',(#10238),#5003,.T.);
#92703=ADVANCED_FACE('',(#10239),#5917,.F.);
#92704=ADVANCED_FACE('',(#10240),#5918,.F.);
#92705=ADVANCED_FACE('',(#10241),#88321,.F.);
#92706=ADVANCED_FACE('',(#10242),#3201,.F.);
#92707=ADVANCED_FACE('',(#10243),#3202,.F.);
#92708=ADVANCED_FACE('',(#10244),#3203,.F.);
#92709=ADVANCED_FACE('',(#10245),#2054,.T.);
#92710=ADVANCED_FACE('',(#10246),#3204,.T.);
#92711=ADVANCED_FACE('',(#10247),#88322,.T.);
#92712=ADVANCED_FACE('',(#10248),#3205,.T.);
#92713=ADVANCED_FACE('',(#10249),#3206,.T.);
#92714=ADVANCED_FACE('',(#10250),#3207,.T.);
#92715=ADVANCED_FACE('',(#10251),#3208,.T.);
#92716=ADVANCED_FACE('',(#10252),#3209,.T.);
#92717=ADVANCED_FACE('',(#10253),#88323,.T.);
#92718=ADVANCED_FACE('',(#10254),#3210,.T.);
#92719=ADVANCED_FACE('',(#10255),#5004,.T.);
#92720=ADVANCED_FACE('',(#10256),#5919,.F.);
#92721=ADVANCED_FACE('',(#10257),#5920,.F.);
#92722=ADVANCED_FACE('',(#10258),#88324,.F.);
#92723=ADVANCED_FACE('',(#10259),#3211,.F.);
#92724=ADVANCED_FACE('',(#10260),#3212,.F.);
#92725=ADVANCED_FACE('',(#10261),#3213,.F.);
#92726=ADVANCED_FACE('',(#10262),#2055,.T.);
#92727=ADVANCED_FACE('',(#10263),#3214,.T.);
#92728=ADVANCED_FACE('',(#10264),#88325,.T.);
#92729=ADVANCED_FACE('',(#10265),#3215,.T.);
#92730=ADVANCED_FACE('',(#10266),#3216,.T.);
#92731=ADVANCED_FACE('',(#10267),#3217,.T.);
#92732=ADVANCED_FACE('',(#10268),#3218,.T.);
#92733=ADVANCED_FACE('',(#10269),#3219,.T.);
#92734=ADVANCED_FACE('',(#10270),#88326,.T.);
#92735=ADVANCED_FACE('',(#10271),#3220,.T.);
#92736=ADVANCED_FACE('',(#10272),#5005,.T.);
#92737=ADVANCED_FACE('',(#10273),#5921,.F.);
#92738=ADVANCED_FACE('',(#10274),#5922,.F.);
#92739=ADVANCED_FACE('',(#10275),#88327,.F.);
#92740=ADVANCED_FACE('',(#10276),#3221,.F.);
#92741=ADVANCED_FACE('',(#10277),#3222,.F.);
#92742=ADVANCED_FACE('',(#10278),#3223,.F.);
#92743=ADVANCED_FACE('',(#10279),#2056,.T.);
#92744=ADVANCED_FACE('',(#10280),#3224,.T.);
#92745=ADVANCED_FACE('',(#10281),#88328,.T.);
#92746=ADVANCED_FACE('',(#10282),#3225,.T.);
#92747=ADVANCED_FACE('',(#10283),#3226,.T.);
#92748=ADVANCED_FACE('',(#10284),#3227,.T.);
#92749=ADVANCED_FACE('',(#10285),#3228,.T.);
#92750=ADVANCED_FACE('',(#10286),#3229,.T.);
#92751=ADVANCED_FACE('',(#10287),#88329,.T.);
#92752=ADVANCED_FACE('',(#10288),#3230,.T.);
#92753=ADVANCED_FACE('',(#10289),#5006,.T.);
#92754=ADVANCED_FACE('',(#10290),#5923,.F.);
#92755=ADVANCED_FACE('',(#10291),#5924,.F.);
#92756=ADVANCED_FACE('',(#10292),#88330,.F.);
#92757=ADVANCED_FACE('',(#10293),#3231,.F.);
#92758=ADVANCED_FACE('',(#10294),#3232,.F.);
#92759=ADVANCED_FACE('',(#10295),#3233,.F.);
#92760=ADVANCED_FACE('',(#10296),#2057,.T.);
#92761=ADVANCED_FACE('',(#10297),#3234,.T.);
#92762=ADVANCED_FACE('',(#10298),#88331,.T.);
#92763=ADVANCED_FACE('',(#10299),#3235,.T.);
#92764=ADVANCED_FACE('',(#10300),#3236,.T.);
#92765=ADVANCED_FACE('',(#10301),#3237,.T.);
#92766=ADVANCED_FACE('',(#10302),#3238,.T.);
#92767=ADVANCED_FACE('',(#10303),#3239,.T.);
#92768=ADVANCED_FACE('',(#10304),#88332,.T.);
#92769=ADVANCED_FACE('',(#10305),#3240,.T.);
#92770=ADVANCED_FACE('',(#10306),#5007,.T.);
#92771=ADVANCED_FACE('',(#10307),#5925,.F.);
#92772=ADVANCED_FACE('',(#10308),#5926,.F.);
#92773=ADVANCED_FACE('',(#10309),#88333,.F.);
#92774=ADVANCED_FACE('',(#10310),#3241,.F.);
#92775=ADVANCED_FACE('',(#10311),#3242,.F.);
#92776=ADVANCED_FACE('',(#10312),#3243,.F.);
#92777=ADVANCED_FACE('',(#10313),#2058,.T.);
#92778=ADVANCED_FACE('',(#10314),#3244,.T.);
#92779=ADVANCED_FACE('',(#10315),#88334,.T.);
#92780=ADVANCED_FACE('',(#10316),#3245,.T.);
#92781=ADVANCED_FACE('',(#10317),#3246,.T.);
#92782=ADVANCED_FACE('',(#10318),#3247,.T.);
#92783=ADVANCED_FACE('',(#10319),#3248,.T.);
#92784=ADVANCED_FACE('',(#10320),#3249,.T.);
#92785=ADVANCED_FACE('',(#10321),#88335,.T.);
#92786=ADVANCED_FACE('',(#10322),#3250,.T.);
#92787=ADVANCED_FACE('',(#10323),#5008,.T.);
#92788=ADVANCED_FACE('',(#10324),#5927,.F.);
#92789=ADVANCED_FACE('',(#10325),#5928,.F.);
#92790=ADVANCED_FACE('',(#10326),#88336,.F.);
#92791=ADVANCED_FACE('',(#10327),#3251,.F.);
#92792=ADVANCED_FACE('',(#10328),#3252,.F.);
#92793=ADVANCED_FACE('',(#10329),#3253,.F.);
#92794=ADVANCED_FACE('',(#10330),#2059,.T.);
#92795=ADVANCED_FACE('',(#10331),#3254,.T.);
#92796=ADVANCED_FACE('',(#10332),#88337,.T.);
#92797=ADVANCED_FACE('',(#10333),#3255,.T.);
#92798=ADVANCED_FACE('',(#10334),#3256,.T.);
#92799=ADVANCED_FACE('',(#10335),#3257,.T.);
#92800=ADVANCED_FACE('',(#10336),#3258,.T.);
#92801=ADVANCED_FACE('',(#10337),#3259,.T.);
#92802=ADVANCED_FACE('',(#10338),#88338,.T.);
#92803=ADVANCED_FACE('',(#10339),#3260,.T.);
#92804=ADVANCED_FACE('',(#10340),#5009,.T.);
#92805=ADVANCED_FACE('',(#10341),#5929,.F.);
#92806=ADVANCED_FACE('',(#10342),#5930,.F.);
#92807=ADVANCED_FACE('',(#10343),#88339,.F.);
#92808=ADVANCED_FACE('',(#10344),#3261,.F.);
#92809=ADVANCED_FACE('',(#10345),#3262,.F.);
#92810=ADVANCED_FACE('',(#10346),#3263,.F.);
#92811=ADVANCED_FACE('',(#10347),#2060,.T.);
#92812=ADVANCED_FACE('',(#10348),#3264,.T.);
#92813=ADVANCED_FACE('',(#10349),#88340,.T.);
#92814=ADVANCED_FACE('',(#10350),#3265,.T.);
#92815=ADVANCED_FACE('',(#10351),#3266,.T.);
#92816=ADVANCED_FACE('',(#10352),#3267,.T.);
#92817=ADVANCED_FACE('',(#10353),#3268,.T.);
#92818=ADVANCED_FACE('',(#10354),#3269,.T.);
#92819=ADVANCED_FACE('',(#10355),#88341,.T.);
#92820=ADVANCED_FACE('',(#10356),#3270,.T.);
#92821=ADVANCED_FACE('',(#10357),#5010,.T.);
#92822=ADVANCED_FACE('',(#10358),#5931,.F.);
#92823=ADVANCED_FACE('',(#10359),#5932,.F.);
#92824=ADVANCED_FACE('',(#10360),#88342,.F.);
#92825=ADVANCED_FACE('',(#10361),#3271,.F.);
#92826=ADVANCED_FACE('',(#10362),#3272,.F.);
#92827=ADVANCED_FACE('',(#10363),#3273,.F.);
#92828=ADVANCED_FACE('',(#10364),#2061,.T.);
#92829=ADVANCED_FACE('',(#10365),#3274,.T.);
#92830=ADVANCED_FACE('',(#10366),#88343,.T.);
#92831=ADVANCED_FACE('',(#10367),#3275,.T.);
#92832=ADVANCED_FACE('',(#10368),#3276,.T.);
#92833=ADVANCED_FACE('',(#10369),#3277,.T.);
#92834=ADVANCED_FACE('',(#10370),#3278,.T.);
#92835=ADVANCED_FACE('',(#10371),#3279,.T.);
#92836=ADVANCED_FACE('',(#10372),#88344,.T.);
#92837=ADVANCED_FACE('',(#10373),#3280,.T.);
#92838=ADVANCED_FACE('',(#10374),#5011,.T.);
#92839=ADVANCED_FACE('',(#10375),#5933,.F.);
#92840=ADVANCED_FACE('',(#10376),#5934,.F.);
#92841=ADVANCED_FACE('',(#10377),#88345,.F.);
#92842=ADVANCED_FACE('',(#10378),#3281,.F.);
#92843=ADVANCED_FACE('',(#10379),#3282,.F.);
#92844=ADVANCED_FACE('',(#10380),#3283,.F.);
#92845=ADVANCED_FACE('',(#10381),#2062,.T.);
#92846=ADVANCED_FACE('',(#10382),#3284,.T.);
#92847=ADVANCED_FACE('',(#10383),#88346,.T.);
#92848=ADVANCED_FACE('',(#10384),#3285,.T.);
#92849=ADVANCED_FACE('',(#10385),#3286,.T.);
#92850=ADVANCED_FACE('',(#10386),#3287,.T.);
#92851=ADVANCED_FACE('',(#10387),#3288,.T.);
#92852=ADVANCED_FACE('',(#10388),#3289,.T.);
#92853=ADVANCED_FACE('',(#10389),#88347,.T.);
#92854=ADVANCED_FACE('',(#10390),#3290,.T.);
#92855=ADVANCED_FACE('',(#10391),#5012,.T.);
#92856=ADVANCED_FACE('',(#10392),#5935,.F.);
#92857=ADVANCED_FACE('',(#10393),#5936,.F.);
#92858=ADVANCED_FACE('',(#10394),#88348,.F.);
#92859=ADVANCED_FACE('',(#10395),#3291,.F.);
#92860=ADVANCED_FACE('',(#10396),#3292,.F.);
#92861=ADVANCED_FACE('',(#10397),#3293,.F.);
#92862=ADVANCED_FACE('',(#10398),#2063,.T.);
#92863=ADVANCED_FACE('',(#10399),#3294,.T.);
#92864=ADVANCED_FACE('',(#10400),#88349,.T.);
#92865=ADVANCED_FACE('',(#10401),#3295,.T.);
#92866=ADVANCED_FACE('',(#10402),#3296,.T.);
#92867=ADVANCED_FACE('',(#10403),#3297,.T.);
#92868=ADVANCED_FACE('',(#10404),#3298,.T.);
#92869=ADVANCED_FACE('',(#10405),#3299,.T.);
#92870=ADVANCED_FACE('',(#10406),#88350,.T.);
#92871=ADVANCED_FACE('',(#10407),#3300,.T.);
#92872=ADVANCED_FACE('',(#10408),#5013,.T.);
#92873=ADVANCED_FACE('',(#10409),#88351,.T.);
#92874=ADVANCED_FACE('',(#10410),#88352,.T.);
#92875=ADVANCED_FACE('',(#10411),#88353,.T.);
#92876=ADVANCED_FACE('',(#10412),#88354,.T.);
#92877=ADVANCED_FACE('',(#10413),#88355,.T.);
#92878=ADVANCED_FACE('',(#10414),#88356,.T.);
#92879=ADVANCED_FACE('',(#10415),#88357,.T.);
#92880=ADVANCED_FACE('',(#10416),#88358,.T.);
#92881=ADVANCED_FACE('',(#10417),#88359,.T.);
#92882=ADVANCED_FACE('',(#10418),#88360,.T.);
#92883=ADVANCED_FACE('',(#10419),#88361,.T.);
#92884=ADVANCED_FACE('',(#10420),#88362,.T.);
#92885=ADVANCED_FACE('',(#10421),#88363,.T.);
#92886=ADVANCED_FACE('',(#10422),#88364,.T.);
#92887=ADVANCED_FACE('',(#10423),#88365,.T.);
#92888=ADVANCED_FACE('',(#10424),#88366,.T.);
#92889=ADVANCED_FACE('',(#10425),#88367,.T.);
#92890=ADVANCED_FACE('',(#10426),#88368,.T.);
#92891=ADVANCED_FACE('',(#10427),#88369,.T.);
#92892=ADVANCED_FACE('',(#10428),#88370,.T.);
#92893=ADVANCED_FACE('',(#10429),#88371,.T.);
#92894=ADVANCED_FACE('',(#10430),#88372,.T.);
#92895=ADVANCED_FACE('',(#10431),#88373,.T.);
#92896=ADVANCED_FACE('',(#10432),#88374,.T.);
#92897=ADVANCED_FACE('',(#10433),#88375,.T.);
#92898=ADVANCED_FACE('',(#10434),#88376,.T.);
#92899=ADVANCED_FACE('',(#10435),#88377,.T.);
#92900=ADVANCED_FACE('',(#10436),#88378,.T.);
#92901=ADVANCED_FACE('',(#10437),#88379,.T.);
#92902=ADVANCED_FACE('',(#10438),#88380,.T.);
#92903=ADVANCED_FACE('',(#10439),#88381,.T.);
#92904=ADVANCED_FACE('',(#10440),#88382,.T.);
#92905=ADVANCED_FACE('',(#10441),#88383,.T.);
#92906=ADVANCED_FACE('',(#10442),#88384,.T.);
#92907=ADVANCED_FACE('',(#10443),#88385,.T.);
#92908=ADVANCED_FACE('',(#10444),#88386,.T.);
#92909=ADVANCED_FACE('',(#10445),#5014,.T.);
#92910=ADVANCED_FACE('',(#10446),#5015,.T.);
#92911=ADVANCED_FACE('',(#10447),#88387,.T.);
#92912=ADVANCED_FACE('',(#10448),#88388,.T.);
#92913=ADVANCED_FACE('',(#10449),#88389,.T.);
#92914=ADVANCED_FACE('',(#10450),#88390,.T.);
#92915=ADVANCED_FACE('',(#10451),#88391,.T.);
#92916=ADVANCED_FACE('',(#10452),#88392,.T.);
#92917=ADVANCED_FACE('',(#10453),#88393,.T.);
#92918=ADVANCED_FACE('',(#10454),#88394,.T.);
#92919=ADVANCED_FACE('',(#10455),#88395,.T.);
#92920=ADVANCED_FACE('',(#10456),#88396,.T.);
#92921=ADVANCED_FACE('',(#10457),#88397,.T.);
#92922=ADVANCED_FACE('',(#10458),#88398,.T.);
#92923=ADVANCED_FACE('',(#10459),#88399,.T.);
#92924=ADVANCED_FACE('',(#10460),#88400,.T.);
#92925=ADVANCED_FACE('',(#10461),#88401,.T.);
#92926=ADVANCED_FACE('',(#10462),#88402,.T.);
#92927=ADVANCED_FACE('',(#10463),#88403,.T.);
#92928=ADVANCED_FACE('',(#10464),#88404,.T.);
#92929=ADVANCED_FACE('',(#10465),#88405,.T.);
#92930=ADVANCED_FACE('',(#10466),#88406,.T.);
#92931=ADVANCED_FACE('',(#10467),#88407,.T.);
#92932=ADVANCED_FACE('',(#10468),#88408,.T.);
#92933=ADVANCED_FACE('',(#10469),#88409,.T.);
#92934=ADVANCED_FACE('',(#10470),#88410,.T.);
#92935=ADVANCED_FACE('',(#10471),#88411,.T.);
#92936=ADVANCED_FACE('',(#10472),#88412,.T.);
#92937=ADVANCED_FACE('',(#10473),#88413,.T.);
#92938=ADVANCED_FACE('',(#10474),#88414,.T.);
#92939=ADVANCED_FACE('',(#10475),#88415,.T.);
#92940=ADVANCED_FACE('',(#10476),#88416,.T.);
#92941=ADVANCED_FACE('',(#10477),#88417,.T.);
#92942=ADVANCED_FACE('',(#10478),#88418,.T.);
#92943=ADVANCED_FACE('',(#10479),#88419,.T.);
#92944=ADVANCED_FACE('',(#10480),#88420,.T.);
#92945=ADVANCED_FACE('',(#10481),#88421,.T.);
#92946=ADVANCED_FACE('',(#10482),#2064,.T.);
#92947=ADVANCED_FACE('',(#10483),#2065,.T.);
#92948=ADVANCED_FACE('',(#10484),#2066,.T.);
#92949=ADVANCED_FACE('',(#10485),#2067,.T.);
#92950=ADVANCED_FACE('',(#10486),#2068,.T.);
#92951=ADVANCED_FACE('',(#10487),#2069,.T.);
#92952=ADVANCED_FACE('',(#10488),#2070,.T.);
#92953=ADVANCED_FACE('',(#10489),#2071,.T.);
#92954=ADVANCED_FACE('',(#10490),#2072,.T.);
#92955=ADVANCED_FACE('',(#10491),#2073,.T.);
#92956=ADVANCED_FACE('',(#10492),#2074,.T.);
#92957=ADVANCED_FACE('',(#10493),#2075,.T.);
#92958=ADVANCED_FACE('',(#10494),#2076,.T.);
#92959=ADVANCED_FACE('',(#10495),#2077,.T.);
#92960=ADVANCED_FACE('',(#10496),#2078,.T.);
#92961=ADVANCED_FACE('',(#10497),#2079,.T.);
#92962=ADVANCED_FACE('',(#10498),#2080,.T.);
#92963=ADVANCED_FACE('',(#10499),#2081,.T.);
#92964=ADVANCED_FACE('',(#10500),#2082,.T.);
#92965=ADVANCED_FACE('',(#10501),#2083,.T.);
#92966=ADVANCED_FACE('',(#10502),#2084,.T.);
#92967=ADVANCED_FACE('',(#10503),#2085,.T.);
#92968=ADVANCED_FACE('',(#10504),#2086,.T.);
#92969=ADVANCED_FACE('',(#10505),#2087,.T.);
#92970=ADVANCED_FACE('',(#10506),#2088,.T.);
#92971=ADVANCED_FACE('',(#10507),#2089,.T.);
#92972=ADVANCED_FACE('',(#10508),#2090,.T.);
#92973=ADVANCED_FACE('',(#10509),#2091,.T.);
#92974=ADVANCED_FACE('',(#10510),#2092,.T.);
#92975=ADVANCED_FACE('',(#10511),#2093,.T.);
#92976=ADVANCED_FACE('',(#10512),#2094,.T.);
#92977=ADVANCED_FACE('',(#10513),#2095,.T.);
#92978=ADVANCED_FACE('',(#10514),#2096,.T.);
#92979=ADVANCED_FACE('',(#10515),#2097,.T.);
#92980=ADVANCED_FACE('',(#10516),#2098,.T.);
#92981=ADVANCED_FACE('',(#10517),#2099,.T.);
#92982=ADVANCED_FACE('',(#10518),#2100,.T.);
#92983=ADVANCED_FACE('',(#10519),#2101,.T.);
#92984=ADVANCED_FACE('',(#10520),#2102,.T.);
#92985=ADVANCED_FACE('',(#10521),#2103,.T.);
#92986=ADVANCED_FACE('',(#10522),#2104,.T.);
#92987=ADVANCED_FACE('',(#10523),#2105,.T.);
#92988=ADVANCED_FACE('',(#10524),#2106,.T.);
#92989=ADVANCED_FACE('',(#10525),#2107,.T.);
#92990=ADVANCED_FACE('',(#10526),#2108,.T.);
#92991=ADVANCED_FACE('',(#10527),#2109,.T.);
#92992=ADVANCED_FACE('',(#10528),#2110,.T.);
#92993=ADVANCED_FACE('',(#10529),#2111,.T.);
#92994=ADVANCED_FACE('',(#10530),#2112,.T.);
#92995=ADVANCED_FACE('',(#10531),#2113,.T.);
#92996=ADVANCED_FACE('',(#10532),#2114,.T.);
#92997=ADVANCED_FACE('',(#10533),#2115,.T.);
#92998=ADVANCED_FACE('',(#10534),#2116,.T.);
#92999=ADVANCED_FACE('',(#10535),#2117,.T.);
#93000=ADVANCED_FACE('',(#10536),#2118,.T.);
#93001=ADVANCED_FACE('',(#10537),#2119,.T.);
#93002=ADVANCED_FACE('',(#10538),#2120,.T.);
#93003=ADVANCED_FACE('',(#10539),#2121,.T.);
#93004=ADVANCED_FACE('',(#10540),#2122,.T.);
#93005=ADVANCED_FACE('',(#10541),#2123,.T.);
#93006=ADVANCED_FACE('',(#10542),#2124,.T.);
#93007=ADVANCED_FACE('',(#10543),#2125,.T.);
#93008=ADVANCED_FACE('',(#10544),#2126,.T.);
#93009=ADVANCED_FACE('',(#10545),#2127,.T.);
#93010=ADVANCED_FACE('',(#10546),#2128,.T.);
#93011=ADVANCED_FACE('',(#10547),#2129,.T.);
#93012=ADVANCED_FACE('',(#10548),#2130,.T.);
#93013=ADVANCED_FACE('',(#10549),#2131,.T.);
#93014=ADVANCED_FACE('',(#10550),#2132,.T.);
#93015=ADVANCED_FACE('',(#10551),#2133,.T.);
#93016=ADVANCED_FACE('',(#10552),#2134,.T.);
#93017=ADVANCED_FACE('',(#10553),#2135,.T.);
#93018=ADVANCED_FACE('',(#10554),#2136,.T.);
#93019=ADVANCED_FACE('',(#10555),#2137,.T.);
#93020=ADVANCED_FACE('',(#10556),#2138,.T.);
#93021=ADVANCED_FACE('',(#10557),#2139,.T.);
#93022=ADVANCED_FACE('',(#10558),#2140,.T.);
#93023=ADVANCED_FACE('',(#10559),#88422,.T.);
#93024=ADVANCED_FACE('',(#10560),#5016,.T.);
#93025=ADVANCED_FACE('',(#10561),#5017,.T.);
#93026=ADVANCED_FACE('',(#10562),#5018,.T.);
#93027=ADVANCED_FACE('',(#10563),#5019,.F.);
#93028=ADVANCED_FACE('',(#10564),#5020,.F.);
#93029=ADVANCED_FACE('',(#10565),#2141,.T.);
#93030=ADVANCED_FACE('',(#10566),#5021,.T.);
#93031=ADVANCED_FACE('',(#10567),#2142,.T.);
#93032=ADVANCED_FACE('',(#10568),#5022,.T.);
#93033=ADVANCED_FACE('',(#10569),#2143,.T.);
#93034=ADVANCED_FACE('',(#10570),#88423,.T.);
#93035=ADVANCED_FACE('',(#10571),#2144,.T.);
#93036=ADVANCED_FACE('',(#10572),#2145,.T.);
#93037=ADVANCED_FACE('',(#10573),#2146,.T.);
#93038=ADVANCED_FACE('',(#10574),#2147,.T.);
#93039=ADVANCED_FACE('',(#10575),#2148,.T.);
#93040=ADVANCED_FACE('',(#10576),#2149,.T.);
#93041=ADVANCED_FACE('',(#10577),#2150,.T.);
#93042=ADVANCED_FACE('',(#10578),#2151,.T.);
#93043=ADVANCED_FACE('',(#10579),#2152,.T.);
#93044=ADVANCED_FACE('',(#10580),#2153,.T.);
#93045=ADVANCED_FACE('',(#10581),#2154,.T.);
#93046=ADVANCED_FACE('',(#10582),#2155,.T.);
#93047=ADVANCED_FACE('',(#10583),#2156,.T.);
#93048=ADVANCED_FACE('',(#10584),#2157,.T.);
#93049=ADVANCED_FACE('',(#10585),#2158,.T.);
#93050=ADVANCED_FACE('',(#10586),#2159,.T.);
#93051=ADVANCED_FACE('',(#10587),#2160,.T.);
#93052=ADVANCED_FACE('',(#10588),#2161,.T.);
#93053=ADVANCED_FACE('',(#10589),#2162,.T.);
#93054=ADVANCED_FACE('',(#10590),#2163,.T.);
#93055=ADVANCED_FACE('',(#10591),#2164,.T.);
#93056=ADVANCED_FACE('',(#10592),#2165,.T.);
#93057=ADVANCED_FACE('',(#10593),#2166,.T.);
#93058=ADVANCED_FACE('',(#10594),#2167,.T.);
#93059=ADVANCED_FACE('',(#10595),#2168,.T.);
#93060=ADVANCED_FACE('',(#10596),#2169,.T.);
#93061=ADVANCED_FACE('',(#10597),#2170,.T.);
#93062=ADVANCED_FACE('',(#10598),#2171,.T.);
#93063=ADVANCED_FACE('',(#10599),#2172,.T.);
#93064=ADVANCED_FACE('',(#10600),#2173,.T.);
#93065=ADVANCED_FACE('',(#10601),#2174,.T.);
#93066=ADVANCED_FACE('',(#10602),#2175,.T.);
#93067=ADVANCED_FACE('',(#10603),#2176,.T.);
#93068=ADVANCED_FACE('',(#10604),#2177,.T.);
#93069=ADVANCED_FACE('',(#10605),#2178,.T.);
#93070=ADVANCED_FACE('',(#10606),#2179,.T.);
#93071=ADVANCED_FACE('',(#10607),#2180,.T.);
#93072=ADVANCED_FACE('',(#10608),#2181,.T.);
#93073=ADVANCED_FACE('',(#10609),#2182,.T.);
#93074=ADVANCED_FACE('',(#10610),#2183,.T.);
#93075=ADVANCED_FACE('',(#10611),#2184,.T.);
#93076=ADVANCED_FACE('',(#10612),#2185,.T.);
#93077=ADVANCED_FACE('',(#10613),#2186,.T.);
#93078=ADVANCED_FACE('',(#10614),#2187,.T.);
#93079=ADVANCED_FACE('',(#10615),#2188,.T.);
#93080=ADVANCED_FACE('',(#10616),#2189,.T.);
#93081=ADVANCED_FACE('',(#10617),#2190,.T.);
#93082=ADVANCED_FACE('',(#10618),#2191,.T.);
#93083=ADVANCED_FACE('',(#10619),#2192,.T.);
#93084=ADVANCED_FACE('',(#10620),#2193,.T.);
#93085=ADVANCED_FACE('',(#10621),#2194,.T.);
#93086=ADVANCED_FACE('',(#10622),#2195,.T.);
#93087=ADVANCED_FACE('',(#10623),#2196,.T.);
#93088=ADVANCED_FACE('',(#10624),#2197,.T.);
#93089=ADVANCED_FACE('',(#10625),#2198,.T.);
#93090=ADVANCED_FACE('',(#10626),#2199,.T.);
#93091=ADVANCED_FACE('',(#10627),#2200,.T.);
#93092=ADVANCED_FACE('',(#10628),#2201,.T.);
#93093=ADVANCED_FACE('',(#10629),#2202,.T.);
#93094=ADVANCED_FACE('',(#10630),#2203,.T.);
#93095=ADVANCED_FACE('',(#10631),#2204,.T.);
#93096=ADVANCED_FACE('',(#10632),#2205,.T.);
#93097=ADVANCED_FACE('',(#10633),#2206,.T.);
#93098=ADVANCED_FACE('',(#10634),#2207,.T.);
#93099=ADVANCED_FACE('',(#10635),#2208,.T.);
#93100=ADVANCED_FACE('',(#10636),#2209,.T.);
#93101=ADVANCED_FACE('',(#10637),#2210,.T.);
#93102=ADVANCED_FACE('',(#10638),#2211,.T.);
#93103=ADVANCED_FACE('',(#10639),#2212,.T.);
#93104=ADVANCED_FACE('',(#10640),#2213,.T.);
#93105=ADVANCED_FACE('',(#10641),#2214,.T.);
#93106=ADVANCED_FACE('',(#10642),#2215,.T.);
#93107=ADVANCED_FACE('',(#10643),#2216,.T.);
#93108=ADVANCED_FACE('',(#10644),#2217,.T.);
#93109=ADVANCED_FACE('',(#10645),#2218,.T.);
#93110=ADVANCED_FACE('',(#10646),#2219,.T.);
#93111=ADVANCED_FACE('',(#10647),#88424,.F.);
#93112=ADVANCED_FACE('',(#10648),#5937,.F.);
#93113=ADVANCED_FACE('',(#10649),#5938,.F.);
#93114=ADVANCED_FACE('',(#10650,#5228),#5939,.F.);
#93115=ADVANCED_FACE('',(#10651),#5940,.F.);
#93116=ADVANCED_FACE('',(#10652),#5941,.F.);
#93117=ADVANCED_FACE('',(#10653),#5942,.F.);
#93118=ADVANCED_FACE('',(#10654),#5943,.F.);
#93119=ADVANCED_FACE('',(#10655),#5944,.F.);
#93120=ADVANCED_FACE('',(#10656,#5229),#5945,.F.);
#93121=ADVANCED_FACE('',(#10657),#2220,.T.);
#93122=ADVANCED_FACE('',(#10658),#5946,.F.);
#93123=ADVANCED_FACE('',(#10659),#5947,.F.);
#93124=ADVANCED_FACE('',(#10660),#5948,.F.);
#93125=ADVANCED_FACE('',(#10661),#5949,.F.);
#93126=ADVANCED_FACE('',(#10662),#5950,.F.);
#93127=ADVANCED_FACE('',(#10663),#5951,.F.);
#93128=ADVANCED_FACE('',(#10664),#5952,.F.);
#93129=ADVANCED_FACE('',(#10665),#5023,.F.);
#93130=ADVANCED_FACE('',(#10666),#5024,.F.);
#93131=ADVANCED_FACE('',(#10667),#5025,.F.);
#93132=ADVANCED_FACE('',(#10668),#5026,.F.);
#93133=ADVANCED_FACE('',(#10669),#5027,.F.);
#93134=ADVANCED_FACE('',(#10670),#5953,.F.);
#93135=ADVANCED_FACE('',(#10671),#3301,.T.);
#93136=ADVANCED_FACE('',(#10672),#88425,.T.);
#93137=ADVANCED_FACE('',(#10673),#3302,.T.);
#93138=ADVANCED_FACE('',(#10674),#5028,.T.);
#93139=ADVANCED_FACE('',(#10675),#3303,.F.);
#93140=ADVANCED_FACE('',(#10676),#88426,.T.);
#93141=ADVANCED_FACE('',(#10677),#3304,.F.);
#93142=ADVANCED_FACE('',(#10678),#3305,.T.);
#93143=ADVANCED_FACE('',(#10679),#3306,.T.);
#93144=ADVANCED_FACE('',(#10680),#3307,.F.);
#93145=ADVANCED_FACE('',(#10681),#3308,.T.);
#93146=ADVANCED_FACE('',(#10682),#3309,.T.);
#93147=ADVANCED_FACE('',(#10683),#3310,.T.);
#93148=ADVANCED_FACE('',(#10684),#88427,.T.);
#93149=ADVANCED_FACE('',(#10685),#3311,.T.);
#93150=ADVANCED_FACE('',(#10686),#3312,.T.);
#93151=ADVANCED_FACE('',(#10687),#5954,.F.);
#93152=ADVANCED_FACE('',(#10688),#5955,.F.);
#93153=ADVANCED_FACE('',(#10689),#88428,.F.);
#93154=ADVANCED_FACE('',(#10690),#3313,.F.);
#93155=ADVANCED_FACE('',(#10691),#3314,.F.);
#93156=ADVANCED_FACE('',(#10692),#3315,.F.);
#93157=ADVANCED_FACE('',(#10693),#3316,.T.);
#93158=ADVANCED_FACE('',(#10694),#88429,.T.);
#93159=ADVANCED_FACE('',(#10695),#3317,.T.);
#93160=ADVANCED_FACE('',(#10696),#3318,.T.);
#93161=ADVANCED_FACE('',(#10697),#3319,.T.);
#93162=ADVANCED_FACE('',(#10698),#3320,.T.);
#93163=ADVANCED_FACE('',(#10699),#3321,.T.);
#93164=ADVANCED_FACE('',(#10700),#88430,.T.);
#93165=ADVANCED_FACE('',(#10701),#3322,.T.);
#93166=ADVANCED_FACE('',(#10702),#5029,.T.);
#93167=ADVANCED_FACE('',(#10703),#5956,.F.);
#93168=ADVANCED_FACE('',(#10704),#5957,.F.);
#93169=ADVANCED_FACE('',(#10705),#88431,.F.);
#93170=ADVANCED_FACE('',(#10706),#3323,.F.);
#93171=ADVANCED_FACE('',(#10707),#3324,.F.);
#93172=ADVANCED_FACE('',(#10708),#3325,.F.);
#93173=ADVANCED_FACE('',(#10709),#3326,.T.);
#93174=ADVANCED_FACE('',(#10710),#88432,.T.);
#93175=ADVANCED_FACE('',(#10711),#3327,.T.);
#93176=ADVANCED_FACE('',(#10712),#3328,.T.);
#93177=ADVANCED_FACE('',(#10713),#3329,.T.);
#93178=ADVANCED_FACE('',(#10714),#3330,.T.);
#93179=ADVANCED_FACE('',(#10715),#3331,.T.);
#93180=ADVANCED_FACE('',(#10716),#88433,.T.);
#93181=ADVANCED_FACE('',(#10717),#3332,.T.);
#93182=ADVANCED_FACE('',(#10718),#5030,.T.);
#93183=ADVANCED_FACE('',(#10719),#5958,.F.);
#93184=ADVANCED_FACE('',(#10720),#5959,.F.);
#93185=ADVANCED_FACE('',(#10721),#88434,.F.);
#93186=ADVANCED_FACE('',(#10722),#3333,.F.);
#93187=ADVANCED_FACE('',(#10723),#3334,.F.);
#93188=ADVANCED_FACE('',(#10724),#3335,.F.);
#93189=ADVANCED_FACE('',(#10725),#3336,.T.);
#93190=ADVANCED_FACE('',(#10726),#88435,.T.);
#93191=ADVANCED_FACE('',(#10727),#3337,.T.);
#93192=ADVANCED_FACE('',(#10728),#3338,.T.);
#93193=ADVANCED_FACE('',(#10729),#3339,.T.);
#93194=ADVANCED_FACE('',(#10730),#3340,.T.);
#93195=ADVANCED_FACE('',(#10731),#3341,.T.);
#93196=ADVANCED_FACE('',(#10732),#88436,.T.);
#93197=ADVANCED_FACE('',(#10733),#3342,.T.);
#93198=ADVANCED_FACE('',(#10734),#5031,.T.);
#93199=ADVANCED_FACE('',(#10735),#5960,.F.);
#93200=ADVANCED_FACE('',(#10736),#5961,.F.);
#93201=ADVANCED_FACE('',(#10737),#88437,.F.);
#93202=ADVANCED_FACE('',(#10738),#3343,.F.);
#93203=ADVANCED_FACE('',(#10739),#3344,.F.);
#93204=ADVANCED_FACE('',(#10740),#3345,.F.);
#93205=ADVANCED_FACE('',(#10741),#3346,.T.);
#93206=ADVANCED_FACE('',(#10742),#88438,.T.);
#93207=ADVANCED_FACE('',(#10743),#3347,.T.);
#93208=ADVANCED_FACE('',(#10744),#3348,.T.);
#93209=ADVANCED_FACE('',(#10745),#3349,.T.);
#93210=ADVANCED_FACE('',(#10746),#3350,.T.);
#93211=ADVANCED_FACE('',(#10747),#3351,.T.);
#93212=ADVANCED_FACE('',(#10748),#88439,.T.);
#93213=ADVANCED_FACE('',(#10749),#3352,.T.);
#93214=ADVANCED_FACE('',(#10750),#5032,.T.);
#93215=ADVANCED_FACE('',(#10751),#5962,.F.);
#93216=ADVANCED_FACE('',(#10752),#5963,.F.);
#93217=ADVANCED_FACE('',(#10753),#88440,.F.);
#93218=ADVANCED_FACE('',(#10754),#3353,.F.);
#93219=ADVANCED_FACE('',(#10755),#3354,.F.);
#93220=ADVANCED_FACE('',(#10756),#3355,.F.);
#93221=ADVANCED_FACE('',(#10757),#3356,.T.);
#93222=ADVANCED_FACE('',(#10758),#88441,.T.);
#93223=ADVANCED_FACE('',(#10759),#3357,.T.);
#93224=ADVANCED_FACE('',(#10760),#3358,.T.);
#93225=ADVANCED_FACE('',(#10761),#3359,.T.);
#93226=ADVANCED_FACE('',(#10762),#3360,.T.);
#93227=ADVANCED_FACE('',(#10763),#3361,.T.);
#93228=ADVANCED_FACE('',(#10764),#88442,.T.);
#93229=ADVANCED_FACE('',(#10765),#3362,.T.);
#93230=ADVANCED_FACE('',(#10766),#5033,.T.);
#93231=ADVANCED_FACE('',(#10767),#5964,.F.);
#93232=ADVANCED_FACE('',(#10768),#5965,.F.);
#93233=ADVANCED_FACE('',(#10769),#88443,.F.);
#93234=ADVANCED_FACE('',(#10770),#3363,.F.);
#93235=ADVANCED_FACE('',(#10771),#3364,.F.);
#93236=ADVANCED_FACE('',(#10772),#3365,.F.);
#93237=ADVANCED_FACE('',(#10773),#3366,.T.);
#93238=ADVANCED_FACE('',(#10774),#88444,.T.);
#93239=ADVANCED_FACE('',(#10775),#3367,.T.);
#93240=ADVANCED_FACE('',(#10776),#3368,.T.);
#93241=ADVANCED_FACE('',(#10777),#3369,.T.);
#93242=ADVANCED_FACE('',(#10778),#3370,.T.);
#93243=ADVANCED_FACE('',(#10779),#3371,.T.);
#93244=ADVANCED_FACE('',(#10780),#88445,.T.);
#93245=ADVANCED_FACE('',(#10781),#3372,.T.);
#93246=ADVANCED_FACE('',(#10782),#5034,.T.);
#93247=ADVANCED_FACE('',(#10783),#5966,.F.);
#93248=ADVANCED_FACE('',(#10784),#5967,.F.);
#93249=ADVANCED_FACE('',(#10785),#88446,.F.);
#93250=ADVANCED_FACE('',(#10786),#3373,.F.);
#93251=ADVANCED_FACE('',(#10787),#3374,.F.);
#93252=ADVANCED_FACE('',(#10788),#3375,.F.);
#93253=ADVANCED_FACE('',(#10789),#3376,.T.);
#93254=ADVANCED_FACE('',(#10790),#88447,.T.);
#93255=ADVANCED_FACE('',(#10791),#3377,.T.);
#93256=ADVANCED_FACE('',(#10792),#3378,.T.);
#93257=ADVANCED_FACE('',(#10793),#3379,.T.);
#93258=ADVANCED_FACE('',(#10794),#3380,.T.);
#93259=ADVANCED_FACE('',(#10795),#3381,.T.);
#93260=ADVANCED_FACE('',(#10796),#88448,.T.);
#93261=ADVANCED_FACE('',(#10797),#3382,.T.);
#93262=ADVANCED_FACE('',(#10798),#5035,.T.);
#93263=ADVANCED_FACE('',(#10799),#5968,.F.);
#93264=ADVANCED_FACE('',(#10800),#5969,.F.);
#93265=ADVANCED_FACE('',(#10801),#88449,.F.);
#93266=ADVANCED_FACE('',(#10802),#3383,.F.);
#93267=ADVANCED_FACE('',(#10803),#3384,.F.);
#93268=ADVANCED_FACE('',(#10804),#3385,.F.);
#93269=ADVANCED_FACE('',(#10805),#3386,.T.);
#93270=ADVANCED_FACE('',(#10806),#88450,.T.);
#93271=ADVANCED_FACE('',(#10807),#3387,.T.);
#93272=ADVANCED_FACE('',(#10808),#3388,.T.);
#93273=ADVANCED_FACE('',(#10809),#3389,.T.);
#93274=ADVANCED_FACE('',(#10810),#3390,.T.);
#93275=ADVANCED_FACE('',(#10811),#3391,.T.);
#93276=ADVANCED_FACE('',(#10812),#88451,.T.);
#93277=ADVANCED_FACE('',(#10813),#3392,.T.);
#93278=ADVANCED_FACE('',(#10814),#5036,.T.);
#93279=ADVANCED_FACE('',(#10815),#5970,.F.);
#93280=ADVANCED_FACE('',(#10816),#5971,.F.);
#93281=ADVANCED_FACE('',(#10817),#88452,.F.);
#93282=ADVANCED_FACE('',(#10818),#3393,.F.);
#93283=ADVANCED_FACE('',(#10819),#3394,.F.);
#93284=ADVANCED_FACE('',(#10820),#3395,.F.);
#93285=ADVANCED_FACE('',(#10821),#3396,.T.);
#93286=ADVANCED_FACE('',(#10822),#88453,.T.);
#93287=ADVANCED_FACE('',(#10823),#3397,.T.);
#93288=ADVANCED_FACE('',(#10824),#3398,.T.);
#93289=ADVANCED_FACE('',(#10825),#3399,.T.);
#93290=ADVANCED_FACE('',(#10826),#3400,.T.);
#93291=ADVANCED_FACE('',(#10827),#3401,.T.);
#93292=ADVANCED_FACE('',(#10828),#88454,.T.);
#93293=ADVANCED_FACE('',(#10829),#3402,.T.);
#93294=ADVANCED_FACE('',(#10830),#5037,.T.);
#93295=ADVANCED_FACE('',(#10831),#5972,.F.);
#93296=ADVANCED_FACE('',(#10832),#5973,.F.);
#93297=ADVANCED_FACE('',(#10833),#88455,.F.);
#93298=ADVANCED_FACE('',(#10834),#3403,.F.);
#93299=ADVANCED_FACE('',(#10835),#3404,.F.);
#93300=ADVANCED_FACE('',(#10836),#3405,.F.);
#93301=ADVANCED_FACE('',(#10837),#3406,.T.);
#93302=ADVANCED_FACE('',(#10838),#88456,.T.);
#93303=ADVANCED_FACE('',(#10839),#3407,.T.);
#93304=ADVANCED_FACE('',(#10840),#3408,.T.);
#93305=ADVANCED_FACE('',(#10841),#3409,.T.);
#93306=ADVANCED_FACE('',(#10842),#3410,.T.);
#93307=ADVANCED_FACE('',(#10843),#3411,.T.);
#93308=ADVANCED_FACE('',(#10844),#88457,.T.);
#93309=ADVANCED_FACE('',(#10845),#3412,.T.);
#93310=ADVANCED_FACE('',(#10846),#5038,.T.);
#93311=ADVANCED_FACE('',(#10847),#5974,.F.);
#93312=ADVANCED_FACE('',(#10848),#5975,.F.);
#93313=ADVANCED_FACE('',(#10849),#88458,.F.);
#93314=ADVANCED_FACE('',(#10850),#3413,.F.);
#93315=ADVANCED_FACE('',(#10851),#3414,.F.);
#93316=ADVANCED_FACE('',(#10852),#3415,.F.);
#93317=ADVANCED_FACE('',(#10853),#3416,.T.);
#93318=ADVANCED_FACE('',(#10854),#88459,.T.);
#93319=ADVANCED_FACE('',(#10855),#3417,.T.);
#93320=ADVANCED_FACE('',(#10856),#3418,.T.);
#93321=ADVANCED_FACE('',(#10857),#3419,.T.);
#93322=ADVANCED_FACE('',(#10858),#3420,.T.);
#93323=ADVANCED_FACE('',(#10859),#3421,.T.);
#93324=ADVANCED_FACE('',(#10860),#88460,.T.);
#93325=ADVANCED_FACE('',(#10861),#3422,.T.);
#93326=ADVANCED_FACE('',(#10862),#5039,.T.);
#93327=ADVANCED_FACE('',(#10863),#5976,.F.);
#93328=ADVANCED_FACE('',(#10864),#5977,.F.);
#93329=ADVANCED_FACE('',(#10865),#88461,.F.);
#93330=ADVANCED_FACE('',(#10866),#3423,.F.);
#93331=ADVANCED_FACE('',(#10867),#3424,.F.);
#93332=ADVANCED_FACE('',(#10868),#3425,.F.);
#93333=ADVANCED_FACE('',(#10869),#3426,.T.);
#93334=ADVANCED_FACE('',(#10870),#88462,.T.);
#93335=ADVANCED_FACE('',(#10871),#3427,.T.);
#93336=ADVANCED_FACE('',(#10872),#3428,.T.);
#93337=ADVANCED_FACE('',(#10873),#3429,.T.);
#93338=ADVANCED_FACE('',(#10874),#3430,.T.);
#93339=ADVANCED_FACE('',(#10875),#3431,.T.);
#93340=ADVANCED_FACE('',(#10876),#88463,.T.);
#93341=ADVANCED_FACE('',(#10877),#3432,.T.);
#93342=ADVANCED_FACE('',(#10878),#5040,.T.);
#93343=ADVANCED_FACE('',(#10879),#5978,.F.);
#93344=ADVANCED_FACE('',(#10880),#5979,.F.);
#93345=ADVANCED_FACE('',(#10881),#88464,.F.);
#93346=ADVANCED_FACE('',(#10882),#3433,.F.);
#93347=ADVANCED_FACE('',(#10883),#3434,.F.);
#93348=ADVANCED_FACE('',(#10884),#3435,.F.);
#93349=ADVANCED_FACE('',(#10885),#3436,.T.);
#93350=ADVANCED_FACE('',(#10886),#88465,.T.);
#93351=ADVANCED_FACE('',(#10887),#3437,.T.);
#93352=ADVANCED_FACE('',(#10888),#3438,.T.);
#93353=ADVANCED_FACE('',(#10889),#3439,.T.);
#93354=ADVANCED_FACE('',(#10890),#3440,.T.);
#93355=ADVANCED_FACE('',(#10891),#3441,.T.);
#93356=ADVANCED_FACE('',(#10892),#88466,.T.);
#93357=ADVANCED_FACE('',(#10893),#3442,.T.);
#93358=ADVANCED_FACE('',(#10894),#5041,.T.);
#93359=ADVANCED_FACE('',(#10895),#5980,.F.);
#93360=ADVANCED_FACE('',(#10896),#5981,.F.);
#93361=ADVANCED_FACE('',(#10897),#88467,.F.);
#93362=ADVANCED_FACE('',(#10898),#3443,.F.);
#93363=ADVANCED_FACE('',(#10899),#3444,.F.);
#93364=ADVANCED_FACE('',(#10900),#3445,.F.);
#93365=ADVANCED_FACE('',(#10901),#3446,.T.);
#93366=ADVANCED_FACE('',(#10902),#88468,.T.);
#93367=ADVANCED_FACE('',(#10903),#3447,.T.);
#93368=ADVANCED_FACE('',(#10904),#3448,.T.);
#93369=ADVANCED_FACE('',(#10905),#3449,.T.);
#93370=ADVANCED_FACE('',(#10906),#3450,.T.);
#93371=ADVANCED_FACE('',(#10907),#3451,.T.);
#93372=ADVANCED_FACE('',(#10908),#88469,.T.);
#93373=ADVANCED_FACE('',(#10909),#3452,.T.);
#93374=ADVANCED_FACE('',(#10910),#5042,.T.);
#93375=ADVANCED_FACE('',(#10911),#5982,.F.);
#93376=ADVANCED_FACE('',(#10912),#5983,.F.);
#93377=ADVANCED_FACE('',(#10913),#88470,.F.);
#93378=ADVANCED_FACE('',(#10914),#3453,.F.);
#93379=ADVANCED_FACE('',(#10915),#3454,.F.);
#93380=ADVANCED_FACE('',(#10916),#3455,.F.);
#93381=ADVANCED_FACE('',(#10917),#3456,.T.);
#93382=ADVANCED_FACE('',(#10918),#88471,.T.);
#93383=ADVANCED_FACE('',(#10919),#3457,.T.);
#93384=ADVANCED_FACE('',(#10920),#3458,.T.);
#93385=ADVANCED_FACE('',(#10921),#3459,.T.);
#93386=ADVANCED_FACE('',(#10922),#3460,.T.);
#93387=ADVANCED_FACE('',(#10923),#3461,.T.);
#93388=ADVANCED_FACE('',(#10924),#88472,.T.);
#93389=ADVANCED_FACE('',(#10925),#3462,.T.);
#93390=ADVANCED_FACE('',(#10926),#5043,.T.);
#93391=ADVANCED_FACE('',(#10927),#5984,.F.);
#93392=ADVANCED_FACE('',(#10928),#5985,.F.);
#93393=ADVANCED_FACE('',(#10929),#88473,.F.);
#93394=ADVANCED_FACE('',(#10930),#3463,.F.);
#93395=ADVANCED_FACE('',(#10931),#3464,.F.);
#93396=ADVANCED_FACE('',(#10932),#3465,.F.);
#93397=ADVANCED_FACE('',(#10933),#3466,.T.);
#93398=ADVANCED_FACE('',(#10934),#88474,.T.);
#93399=ADVANCED_FACE('',(#10935),#3467,.T.);
#93400=ADVANCED_FACE('',(#10936),#3468,.T.);
#93401=ADVANCED_FACE('',(#10937),#3469,.T.);
#93402=ADVANCED_FACE('',(#10938),#3470,.T.);
#93403=ADVANCED_FACE('',(#10939),#3471,.T.);
#93404=ADVANCED_FACE('',(#10940),#88475,.T.);
#93405=ADVANCED_FACE('',(#10941),#3472,.T.);
#93406=ADVANCED_FACE('',(#10942),#5044,.T.);
#93407=ADVANCED_FACE('',(#10943),#5986,.F.);
#93408=ADVANCED_FACE('',(#10944),#5987,.F.);
#93409=ADVANCED_FACE('',(#10945),#88476,.F.);
#93410=ADVANCED_FACE('',(#10946),#3473,.F.);
#93411=ADVANCED_FACE('',(#10947),#3474,.F.);
#93412=ADVANCED_FACE('',(#10948),#3475,.F.);
#93413=ADVANCED_FACE('',(#10949),#3476,.T.);
#93414=ADVANCED_FACE('',(#10950),#88477,.T.);
#93415=ADVANCED_FACE('',(#10951),#3477,.T.);
#93416=ADVANCED_FACE('',(#10952),#3478,.T.);
#93417=ADVANCED_FACE('',(#10953),#3479,.T.);
#93418=ADVANCED_FACE('',(#10954),#3480,.T.);
#93419=ADVANCED_FACE('',(#10955),#3481,.T.);
#93420=ADVANCED_FACE('',(#10956),#88478,.T.);
#93421=ADVANCED_FACE('',(#10957),#3482,.T.);
#93422=ADVANCED_FACE('',(#10958),#5045,.T.);
#93423=ADVANCED_FACE('',(#10959),#5988,.F.);
#93424=ADVANCED_FACE('',(#10960),#5989,.F.);
#93425=ADVANCED_FACE('',(#10961),#88479,.F.);
#93426=ADVANCED_FACE('',(#10962),#3483,.F.);
#93427=ADVANCED_FACE('',(#10963),#3484,.F.);
#93428=ADVANCED_FACE('',(#10964),#3485,.F.);
#93429=ADVANCED_FACE('',(#10965),#3486,.T.);
#93430=ADVANCED_FACE('',(#10966),#88480,.T.);
#93431=ADVANCED_FACE('',(#10967),#3487,.T.);
#93432=ADVANCED_FACE('',(#10968),#3488,.T.);
#93433=ADVANCED_FACE('',(#10969),#3489,.T.);
#93434=ADVANCED_FACE('',(#10970),#3490,.T.);
#93435=ADVANCED_FACE('',(#10971),#3491,.T.);
#93436=ADVANCED_FACE('',(#10972),#88481,.T.);
#93437=ADVANCED_FACE('',(#10973),#3492,.T.);
#93438=ADVANCED_FACE('',(#10974),#5046,.T.);
#93439=ADVANCED_FACE('',(#10975),#5990,.F.);
#93440=ADVANCED_FACE('',(#10976),#5991,.F.);
#93441=ADVANCED_FACE('',(#10977),#88482,.F.);
#93442=ADVANCED_FACE('',(#10978),#3493,.F.);
#93443=ADVANCED_FACE('',(#10979),#3494,.F.);
#93444=ADVANCED_FACE('',(#10980),#3495,.F.);
#93445=ADVANCED_FACE('',(#10981),#3496,.T.);
#93446=ADVANCED_FACE('',(#10982),#88483,.T.);
#93447=ADVANCED_FACE('',(#10983),#3497,.T.);
#93448=ADVANCED_FACE('',(#10984),#3498,.T.);
#93449=ADVANCED_FACE('',(#10985),#3499,.T.);
#93450=ADVANCED_FACE('',(#10986),#3500,.T.);
#93451=ADVANCED_FACE('',(#10987),#3501,.T.);
#93452=ADVANCED_FACE('',(#10988),#88484,.T.);
#93453=ADVANCED_FACE('',(#10989),#3502,.T.);
#93454=ADVANCED_FACE('',(#10990),#5047,.T.);
#93455=ADVANCED_FACE('',(#10991),#5992,.F.);
#93456=ADVANCED_FACE('',(#10992),#5993,.F.);
#93457=ADVANCED_FACE('',(#10993),#88485,.F.);
#93458=ADVANCED_FACE('',(#10994),#3503,.F.);
#93459=ADVANCED_FACE('',(#10995),#3504,.F.);
#93460=ADVANCED_FACE('',(#10996),#3505,.F.);
#93461=ADVANCED_FACE('',(#10997),#3506,.T.);
#93462=ADVANCED_FACE('',(#10998),#88486,.T.);
#93463=ADVANCED_FACE('',(#10999),#3507,.T.);
#93464=ADVANCED_FACE('',(#11000),#3508,.T.);
#93465=ADVANCED_FACE('',(#11001),#3509,.T.);
#93466=ADVANCED_FACE('',(#11002),#3510,.T.);
#93467=ADVANCED_FACE('',(#11003),#3511,.T.);
#93468=ADVANCED_FACE('',(#11004),#88487,.T.);
#93469=ADVANCED_FACE('',(#11005),#3512,.T.);
#93470=ADVANCED_FACE('',(#11006),#5048,.T.);
#93471=ADVANCED_FACE('',(#11007),#5994,.F.);
#93472=ADVANCED_FACE('',(#11008),#5995,.F.);
#93473=ADVANCED_FACE('',(#11009),#88488,.F.);
#93474=ADVANCED_FACE('',(#11010),#3513,.F.);
#93475=ADVANCED_FACE('',(#11011),#3514,.F.);
#93476=ADVANCED_FACE('',(#11012),#3515,.F.);
#93477=ADVANCED_FACE('',(#11013),#3516,.T.);
#93478=ADVANCED_FACE('',(#11014),#88489,.T.);
#93479=ADVANCED_FACE('',(#11015),#3517,.T.);
#93480=ADVANCED_FACE('',(#11016),#3518,.T.);
#93481=ADVANCED_FACE('',(#11017),#3519,.T.);
#93482=ADVANCED_FACE('',(#11018),#3520,.T.);
#93483=ADVANCED_FACE('',(#11019),#3521,.T.);
#93484=ADVANCED_FACE('',(#11020),#88490,.T.);
#93485=ADVANCED_FACE('',(#11021),#3522,.T.);
#93486=ADVANCED_FACE('',(#11022),#5049,.T.);
#93487=ADVANCED_FACE('',(#11023),#5996,.F.);
#93488=ADVANCED_FACE('',(#11024),#5997,.F.);
#93489=ADVANCED_FACE('',(#11025),#88491,.F.);
#93490=ADVANCED_FACE('',(#11026),#3523,.F.);
#93491=ADVANCED_FACE('',(#11027),#3524,.F.);
#93492=ADVANCED_FACE('',(#11028),#3525,.F.);
#93493=ADVANCED_FACE('',(#11029),#3526,.T.);
#93494=ADVANCED_FACE('',(#11030),#88492,.T.);
#93495=ADVANCED_FACE('',(#11031),#3527,.T.);
#93496=ADVANCED_FACE('',(#11032),#3528,.T.);
#93497=ADVANCED_FACE('',(#11033),#3529,.T.);
#93498=ADVANCED_FACE('',(#11034),#3530,.T.);
#93499=ADVANCED_FACE('',(#11035),#3531,.T.);
#93500=ADVANCED_FACE('',(#11036),#88493,.T.);
#93501=ADVANCED_FACE('',(#11037),#3532,.T.);
#93502=ADVANCED_FACE('',(#11038),#5050,.T.);
#93503=ADVANCED_FACE('',(#11039),#5998,.F.);
#93504=ADVANCED_FACE('',(#11040),#5999,.F.);
#93505=ADVANCED_FACE('',(#11041),#88494,.F.);
#93506=ADVANCED_FACE('',(#11042),#3533,.F.);
#93507=ADVANCED_FACE('',(#11043),#3534,.F.);
#93508=ADVANCED_FACE('',(#11044),#3535,.F.);
#93509=ADVANCED_FACE('',(#11045),#3536,.T.);
#93510=ADVANCED_FACE('',(#11046),#88495,.T.);
#93511=ADVANCED_FACE('',(#11047),#3537,.T.);
#93512=ADVANCED_FACE('',(#11048),#3538,.T.);
#93513=ADVANCED_FACE('',(#11049),#3539,.T.);
#93514=ADVANCED_FACE('',(#11050),#3540,.T.);
#93515=ADVANCED_FACE('',(#11051),#3541,.T.);
#93516=ADVANCED_FACE('',(#11052),#88496,.T.);
#93517=ADVANCED_FACE('',(#11053),#3542,.T.);
#93518=ADVANCED_FACE('',(#11054),#5051,.T.);
#93519=ADVANCED_FACE('',(#11055),#6000,.F.);
#93520=ADVANCED_FACE('',(#11056),#6001,.F.);
#93521=ADVANCED_FACE('',(#11057),#88497,.F.);
#93522=ADVANCED_FACE('',(#11058),#3543,.F.);
#93523=ADVANCED_FACE('',(#11059),#3544,.F.);
#93524=ADVANCED_FACE('',(#11060),#3545,.F.);
#93525=ADVANCED_FACE('',(#11061),#3546,.T.);
#93526=ADVANCED_FACE('',(#11062),#88498,.T.);
#93527=ADVANCED_FACE('',(#11063),#3547,.T.);
#93528=ADVANCED_FACE('',(#11064),#3548,.T.);
#93529=ADVANCED_FACE('',(#11065),#3549,.T.);
#93530=ADVANCED_FACE('',(#11066),#3550,.T.);
#93531=ADVANCED_FACE('',(#11067),#3551,.T.);
#93532=ADVANCED_FACE('',(#11068),#88499,.T.);
#93533=ADVANCED_FACE('',(#11069),#3552,.T.);
#93534=ADVANCED_FACE('',(#11070),#5052,.T.);
#93535=ADVANCED_FACE('',(#11071),#6002,.F.);
#93536=ADVANCED_FACE('',(#11072),#6003,.F.);
#93537=ADVANCED_FACE('',(#11073),#88500,.F.);
#93538=ADVANCED_FACE('',(#11074),#3553,.F.);
#93539=ADVANCED_FACE('',(#11075),#3554,.F.);
#93540=ADVANCED_FACE('',(#11076),#3555,.F.);
#93541=ADVANCED_FACE('',(#11077),#3556,.T.);
#93542=ADVANCED_FACE('',(#11078),#88501,.T.);
#93543=ADVANCED_FACE('',(#11079),#3557,.T.);
#93544=ADVANCED_FACE('',(#11080),#3558,.T.);
#93545=ADVANCED_FACE('',(#11081),#3559,.T.);
#93546=ADVANCED_FACE('',(#11082),#3560,.T.);
#93547=ADVANCED_FACE('',(#11083),#3561,.T.);
#93548=ADVANCED_FACE('',(#11084),#88502,.T.);
#93549=ADVANCED_FACE('',(#11085),#3562,.T.);
#93550=ADVANCED_FACE('',(#11086),#5053,.T.);
#93551=ADVANCED_FACE('',(#11087),#6004,.F.);
#93552=ADVANCED_FACE('',(#11088),#6005,.F.);
#93553=ADVANCED_FACE('',(#11089),#88503,.F.);
#93554=ADVANCED_FACE('',(#11090),#3563,.F.);
#93555=ADVANCED_FACE('',(#11091),#3564,.F.);
#93556=ADVANCED_FACE('',(#11092),#3565,.F.);
#93557=ADVANCED_FACE('',(#11093),#3566,.T.);
#93558=ADVANCED_FACE('',(#11094),#88504,.T.);
#93559=ADVANCED_FACE('',(#11095),#3567,.T.);
#93560=ADVANCED_FACE('',(#11096),#3568,.T.);
#93561=ADVANCED_FACE('',(#11097),#3569,.T.);
#93562=ADVANCED_FACE('',(#11098),#3570,.T.);
#93563=ADVANCED_FACE('',(#11099),#3571,.T.);
#93564=ADVANCED_FACE('',(#11100),#88505,.T.);
#93565=ADVANCED_FACE('',(#11101),#3572,.T.);
#93566=ADVANCED_FACE('',(#11102),#5054,.T.);
#93567=ADVANCED_FACE('',(#11103),#6006,.F.);
#93568=ADVANCED_FACE('',(#11104),#6007,.F.);
#93569=ADVANCED_FACE('',(#11105),#88506,.F.);
#93570=ADVANCED_FACE('',(#11106),#3573,.F.);
#93571=ADVANCED_FACE('',(#11107),#3574,.F.);
#93572=ADVANCED_FACE('',(#11108),#3575,.F.);
#93573=ADVANCED_FACE('',(#11109),#3576,.T.);
#93574=ADVANCED_FACE('',(#11110),#88507,.T.);
#93575=ADVANCED_FACE('',(#11111),#3577,.T.);
#93576=ADVANCED_FACE('',(#11112),#3578,.T.);
#93577=ADVANCED_FACE('',(#11113),#3579,.T.);
#93578=ADVANCED_FACE('',(#11114),#3580,.T.);
#93579=ADVANCED_FACE('',(#11115),#3581,.T.);
#93580=ADVANCED_FACE('',(#11116),#88508,.T.);
#93581=ADVANCED_FACE('',(#11117),#3582,.T.);
#93582=ADVANCED_FACE('',(#11118),#5055,.T.);
#93583=ADVANCED_FACE('',(#11119),#6008,.F.);
#93584=ADVANCED_FACE('',(#11120),#6009,.F.);
#93585=ADVANCED_FACE('',(#11121),#88509,.F.);
#93586=ADVANCED_FACE('',(#11122),#3583,.F.);
#93587=ADVANCED_FACE('',(#11123),#3584,.F.);
#93588=ADVANCED_FACE('',(#11124),#3585,.F.);
#93589=ADVANCED_FACE('',(#11125),#3586,.T.);
#93590=ADVANCED_FACE('',(#11126),#88510,.T.);
#93591=ADVANCED_FACE('',(#11127),#3587,.T.);
#93592=ADVANCED_FACE('',(#11128),#3588,.T.);
#93593=ADVANCED_FACE('',(#11129),#3589,.T.);
#93594=ADVANCED_FACE('',(#11130),#3590,.T.);
#93595=ADVANCED_FACE('',(#11131),#3591,.T.);
#93596=ADVANCED_FACE('',(#11132),#88511,.T.);
#93597=ADVANCED_FACE('',(#11133),#3592,.T.);
#93598=ADVANCED_FACE('',(#11134),#5056,.T.);
#93599=ADVANCED_FACE('',(#11135),#6010,.F.);
#93600=ADVANCED_FACE('',(#11136),#6011,.F.);
#93601=ADVANCED_FACE('',(#11137),#88512,.F.);
#93602=ADVANCED_FACE('',(#11138),#3593,.F.);
#93603=ADVANCED_FACE('',(#11139),#3594,.F.);
#93604=ADVANCED_FACE('',(#11140),#3595,.F.);
#93605=ADVANCED_FACE('',(#11141),#3596,.T.);
#93606=ADVANCED_FACE('',(#11142),#88513,.T.);
#93607=ADVANCED_FACE('',(#11143),#3597,.T.);
#93608=ADVANCED_FACE('',(#11144),#3598,.T.);
#93609=ADVANCED_FACE('',(#11145),#3599,.T.);
#93610=ADVANCED_FACE('',(#11146),#3600,.T.);
#93611=ADVANCED_FACE('',(#11147),#3601,.T.);
#93612=ADVANCED_FACE('',(#11148),#88514,.T.);
#93613=ADVANCED_FACE('',(#11149),#3602,.T.);
#93614=ADVANCED_FACE('',(#11150),#5057,.T.);
#93615=ADVANCED_FACE('',(#11151),#6012,.F.);
#93616=ADVANCED_FACE('',(#11152),#6013,.F.);
#93617=ADVANCED_FACE('',(#11153),#88515,.F.);
#93618=ADVANCED_FACE('',(#11154),#3603,.F.);
#93619=ADVANCED_FACE('',(#11155),#3604,.F.);
#93620=ADVANCED_FACE('',(#11156),#3605,.F.);
#93621=ADVANCED_FACE('',(#11157),#3606,.T.);
#93622=ADVANCED_FACE('',(#11158),#88516,.T.);
#93623=ADVANCED_FACE('',(#11159),#3607,.T.);
#93624=ADVANCED_FACE('',(#11160),#3608,.T.);
#93625=ADVANCED_FACE('',(#11161),#3609,.T.);
#93626=ADVANCED_FACE('',(#11162),#3610,.T.);
#93627=ADVANCED_FACE('',(#11163),#3611,.T.);
#93628=ADVANCED_FACE('',(#11164),#88517,.T.);
#93629=ADVANCED_FACE('',(#11165),#3612,.T.);
#93630=ADVANCED_FACE('',(#11166),#5058,.T.);
#93631=ADVANCED_FACE('',(#11167),#6014,.F.);
#93632=ADVANCED_FACE('',(#11168),#6015,.F.);
#93633=ADVANCED_FACE('',(#11169),#88518,.F.);
#93634=ADVANCED_FACE('',(#11170),#3613,.F.);
#93635=ADVANCED_FACE('',(#11171),#3614,.F.);
#93636=ADVANCED_FACE('',(#11172),#3615,.F.);
#93637=ADVANCED_FACE('',(#11173),#3616,.T.);
#93638=ADVANCED_FACE('',(#11174),#88519,.T.);
#93639=ADVANCED_FACE('',(#11175),#3617,.T.);
#93640=ADVANCED_FACE('',(#11176),#3618,.T.);
#93641=ADVANCED_FACE('',(#11177),#3619,.T.);
#93642=ADVANCED_FACE('',(#11178),#3620,.T.);
#93643=ADVANCED_FACE('',(#11179),#3621,.T.);
#93644=ADVANCED_FACE('',(#11180),#88520,.T.);
#93645=ADVANCED_FACE('',(#11181),#3622,.T.);
#93646=ADVANCED_FACE('',(#11182),#5059,.T.);
#93647=ADVANCED_FACE('',(#11183),#6016,.F.);
#93648=ADVANCED_FACE('',(#11184),#6017,.F.);
#93649=ADVANCED_FACE('',(#11185),#88521,.F.);
#93650=ADVANCED_FACE('',(#11186),#3623,.F.);
#93651=ADVANCED_FACE('',(#11187),#3624,.F.);
#93652=ADVANCED_FACE('',(#11188),#3625,.F.);
#93653=ADVANCED_FACE('',(#11189),#3626,.T.);
#93654=ADVANCED_FACE('',(#11190),#88522,.T.);
#93655=ADVANCED_FACE('',(#11191),#3627,.T.);
#93656=ADVANCED_FACE('',(#11192),#3628,.T.);
#93657=ADVANCED_FACE('',(#11193),#3629,.T.);
#93658=ADVANCED_FACE('',(#11194),#3630,.T.);
#93659=ADVANCED_FACE('',(#11195),#3631,.T.);
#93660=ADVANCED_FACE('',(#11196),#88523,.T.);
#93661=ADVANCED_FACE('',(#11197),#3632,.T.);
#93662=ADVANCED_FACE('',(#11198),#5060,.T.);
#93663=ADVANCED_FACE('',(#11199),#6018,.F.);
#93664=ADVANCED_FACE('',(#11200),#6019,.F.);
#93665=ADVANCED_FACE('',(#11201),#88524,.F.);
#93666=ADVANCED_FACE('',(#11202),#3633,.F.);
#93667=ADVANCED_FACE('',(#11203),#3634,.F.);
#93668=ADVANCED_FACE('',(#11204),#3635,.F.);
#93669=ADVANCED_FACE('',(#11205),#3636,.T.);
#93670=ADVANCED_FACE('',(#11206),#88525,.T.);
#93671=ADVANCED_FACE('',(#11207),#3637,.T.);
#93672=ADVANCED_FACE('',(#11208),#3638,.T.);
#93673=ADVANCED_FACE('',(#11209),#3639,.T.);
#93674=ADVANCED_FACE('',(#11210),#3640,.T.);
#93675=ADVANCED_FACE('',(#11211),#3641,.T.);
#93676=ADVANCED_FACE('',(#11212),#88526,.T.);
#93677=ADVANCED_FACE('',(#11213),#3642,.T.);
#93678=ADVANCED_FACE('',(#11214),#5061,.T.);
#93679=ADVANCED_FACE('',(#11215),#6020,.F.);
#93680=ADVANCED_FACE('',(#11216),#6021,.F.);
#93681=ADVANCED_FACE('',(#11217),#88527,.F.);
#93682=ADVANCED_FACE('',(#11218),#3643,.F.);
#93683=ADVANCED_FACE('',(#11219),#3644,.F.);
#93684=ADVANCED_FACE('',(#11220),#3645,.F.);
#93685=ADVANCED_FACE('',(#11221),#3646,.T.);
#93686=ADVANCED_FACE('',(#11222),#88528,.T.);
#93687=ADVANCED_FACE('',(#11223),#3647,.T.);
#93688=ADVANCED_FACE('',(#11224),#3648,.T.);
#93689=ADVANCED_FACE('',(#11225),#3649,.T.);
#93690=ADVANCED_FACE('',(#11226),#3650,.T.);
#93691=ADVANCED_FACE('',(#11227),#3651,.T.);
#93692=ADVANCED_FACE('',(#11228),#88529,.T.);
#93693=ADVANCED_FACE('',(#11229),#3652,.T.);
#93694=ADVANCED_FACE('',(#11230),#5062,.T.);
#93695=ADVANCED_FACE('',(#11231),#6022,.F.);
#93696=ADVANCED_FACE('',(#11232),#6023,.F.);
#93697=ADVANCED_FACE('',(#11233),#88530,.F.);
#93698=ADVANCED_FACE('',(#11234),#3653,.F.);
#93699=ADVANCED_FACE('',(#11235),#3654,.F.);
#93700=ADVANCED_FACE('',(#11236),#3655,.F.);
#93701=ADVANCED_FACE('',(#11237),#3656,.T.);
#93702=ADVANCED_FACE('',(#11238),#88531,.T.);
#93703=ADVANCED_FACE('',(#11239),#3657,.T.);
#93704=ADVANCED_FACE('',(#11240),#3658,.T.);
#93705=ADVANCED_FACE('',(#11241),#3659,.T.);
#93706=ADVANCED_FACE('',(#11242),#3660,.T.);
#93707=ADVANCED_FACE('',(#11243),#3661,.T.);
#93708=ADVANCED_FACE('',(#11244),#88532,.T.);
#93709=ADVANCED_FACE('',(#11245),#3662,.T.);
#93710=ADVANCED_FACE('',(#11246),#5063,.T.);
#93711=ADVANCED_FACE('',(#11247),#6024,.F.);
#93712=ADVANCED_FACE('',(#11248),#6025,.F.);
#93713=ADVANCED_FACE('',(#11249),#88533,.F.);
#93714=ADVANCED_FACE('',(#11250),#3663,.F.);
#93715=ADVANCED_FACE('',(#11251),#3664,.F.);
#93716=ADVANCED_FACE('',(#11252),#3665,.F.);
#93717=ADVANCED_FACE('',(#11253),#3666,.T.);
#93718=ADVANCED_FACE('',(#11254),#88534,.T.);
#93719=ADVANCED_FACE('',(#11255),#3667,.T.);
#93720=ADVANCED_FACE('',(#11256),#3668,.T.);
#93721=ADVANCED_FACE('',(#11257),#3669,.T.);
#93722=ADVANCED_FACE('',(#11258),#3670,.T.);
#93723=ADVANCED_FACE('',(#11259),#3671,.T.);
#93724=ADVANCED_FACE('',(#11260),#88535,.T.);
#93725=ADVANCED_FACE('',(#11261),#3672,.T.);
#93726=ADVANCED_FACE('',(#11262),#5064,.T.);
#93727=ADVANCED_FACE('',(#11263),#6026,.F.);
#93728=ADVANCED_FACE('',(#11264),#6027,.F.);
#93729=ADVANCED_FACE('',(#11265),#88536,.F.);
#93730=ADVANCED_FACE('',(#11266),#3673,.F.);
#93731=ADVANCED_FACE('',(#11267),#3674,.F.);
#93732=ADVANCED_FACE('',(#11268),#3675,.F.);
#93733=ADVANCED_FACE('',(#11269),#3676,.T.);
#93734=ADVANCED_FACE('',(#11270),#88537,.T.);
#93735=ADVANCED_FACE('',(#11271),#3677,.T.);
#93736=ADVANCED_FACE('',(#11272),#3678,.T.);
#93737=ADVANCED_FACE('',(#11273),#3679,.T.);
#93738=ADVANCED_FACE('',(#11274),#3680,.T.);
#93739=ADVANCED_FACE('',(#11275),#3681,.T.);
#93740=ADVANCED_FACE('',(#11276),#88538,.T.);
#93741=ADVANCED_FACE('',(#11277),#3682,.T.);
#93742=ADVANCED_FACE('',(#11278),#5065,.T.);
#93743=ADVANCED_FACE('',(#11279),#6028,.F.);
#93744=ADVANCED_FACE('',(#11280),#6029,.F.);
#93745=ADVANCED_FACE('',(#11281),#88539,.F.);
#93746=ADVANCED_FACE('',(#11282),#3683,.F.);
#93747=ADVANCED_FACE('',(#11283),#3684,.F.);
#93748=ADVANCED_FACE('',(#11284),#3685,.F.);
#93749=ADVANCED_FACE('',(#11285),#3686,.T.);
#93750=ADVANCED_FACE('',(#11286),#88540,.T.);
#93751=ADVANCED_FACE('',(#11287),#3687,.T.);
#93752=ADVANCED_FACE('',(#11288),#3688,.T.);
#93753=ADVANCED_FACE('',(#11289),#3689,.T.);
#93754=ADVANCED_FACE('',(#11290),#3690,.T.);
#93755=ADVANCED_FACE('',(#11291),#3691,.T.);
#93756=ADVANCED_FACE('',(#11292),#88541,.T.);
#93757=ADVANCED_FACE('',(#11293),#3692,.T.);
#93758=ADVANCED_FACE('',(#11294),#5066,.T.);
#93759=ADVANCED_FACE('',(#11295),#6030,.F.);
#93760=ADVANCED_FACE('',(#11296),#6031,.F.);
#93761=ADVANCED_FACE('',(#11297),#88542,.F.);
#93762=ADVANCED_FACE('',(#11298),#3693,.F.);
#93763=ADVANCED_FACE('',(#11299),#3694,.F.);
#93764=ADVANCED_FACE('',(#11300),#3695,.F.);
#93765=ADVANCED_FACE('',(#11301),#3696,.T.);
#93766=ADVANCED_FACE('',(#11302),#88543,.T.);
#93767=ADVANCED_FACE('',(#11303),#3697,.T.);
#93768=ADVANCED_FACE('',(#11304),#3698,.T.);
#93769=ADVANCED_FACE('',(#11305),#3699,.T.);
#93770=ADVANCED_FACE('',(#11306),#3700,.T.);
#93771=ADVANCED_FACE('',(#11307),#3701,.T.);
#93772=ADVANCED_FACE('',(#11308),#88544,.T.);
#93773=ADVANCED_FACE('',(#11309),#3702,.T.);
#93774=ADVANCED_FACE('',(#11310),#5067,.T.);
#93775=ADVANCED_FACE('',(#11311),#6032,.F.);
#93776=ADVANCED_FACE('',(#11312),#6033,.F.);
#93777=ADVANCED_FACE('',(#11313),#88545,.F.);
#93778=ADVANCED_FACE('',(#11314),#3703,.F.);
#93779=ADVANCED_FACE('',(#11315),#3704,.F.);
#93780=ADVANCED_FACE('',(#11316),#3705,.F.);
#93781=ADVANCED_FACE('',(#11317),#3706,.T.);
#93782=ADVANCED_FACE('',(#11318),#88546,.T.);
#93783=ADVANCED_FACE('',(#11319),#3707,.T.);
#93784=ADVANCED_FACE('',(#11320),#3708,.T.);
#93785=ADVANCED_FACE('',(#11321),#3709,.T.);
#93786=ADVANCED_FACE('',(#11322),#3710,.T.);
#93787=ADVANCED_FACE('',(#11323),#3711,.T.);
#93788=ADVANCED_FACE('',(#11324),#88547,.T.);
#93789=ADVANCED_FACE('',(#11325),#3712,.T.);
#93790=ADVANCED_FACE('',(#11326),#5068,.T.);
#93791=ADVANCED_FACE('',(#11327),#6034,.F.);
#93792=ADVANCED_FACE('',(#11328),#6035,.F.);
#93793=ADVANCED_FACE('',(#11329),#88548,.F.);
#93794=ADVANCED_FACE('',(#11330),#3713,.F.);
#93795=ADVANCED_FACE('',(#11331),#3714,.F.);
#93796=ADVANCED_FACE('',(#11332),#3715,.F.);
#93797=ADVANCED_FACE('',(#11333),#3716,.T.);
#93798=ADVANCED_FACE('',(#11334),#88549,.T.);
#93799=ADVANCED_FACE('',(#11335),#3717,.T.);
#93800=ADVANCED_FACE('',(#11336),#3718,.T.);
#93801=ADVANCED_FACE('',(#11337),#3719,.T.);
#93802=ADVANCED_FACE('',(#11338),#3720,.T.);
#93803=ADVANCED_FACE('',(#11339),#3721,.T.);
#93804=ADVANCED_FACE('',(#11340),#88550,.T.);
#93805=ADVANCED_FACE('',(#11341),#3722,.T.);
#93806=ADVANCED_FACE('',(#11342),#5069,.T.);
#93807=ADVANCED_FACE('',(#11343),#6036,.F.);
#93808=ADVANCED_FACE('',(#11344),#6037,.F.);
#93809=ADVANCED_FACE('',(#11345),#88551,.F.);
#93810=ADVANCED_FACE('',(#11346),#3723,.F.);
#93811=ADVANCED_FACE('',(#11347),#3724,.F.);
#93812=ADVANCED_FACE('',(#11348),#3725,.F.);
#93813=ADVANCED_FACE('',(#11349),#3726,.T.);
#93814=ADVANCED_FACE('',(#11350),#88552,.T.);
#93815=ADVANCED_FACE('',(#11351),#3727,.T.);
#93816=ADVANCED_FACE('',(#11352),#3728,.T.);
#93817=ADVANCED_FACE('',(#11353),#3729,.T.);
#93818=ADVANCED_FACE('',(#11354),#3730,.T.);
#93819=ADVANCED_FACE('',(#11355),#3731,.T.);
#93820=ADVANCED_FACE('',(#11356),#88553,.T.);
#93821=ADVANCED_FACE('',(#11357),#3732,.T.);
#93822=ADVANCED_FACE('',(#11358),#5070,.T.);
#93823=ADVANCED_FACE('',(#11359),#6038,.F.);
#93824=ADVANCED_FACE('',(#11360),#6039,.F.);
#93825=ADVANCED_FACE('',(#11361),#88554,.F.);
#93826=ADVANCED_FACE('',(#11362),#3733,.F.);
#93827=ADVANCED_FACE('',(#11363),#3734,.F.);
#93828=ADVANCED_FACE('',(#11364),#3735,.F.);
#93829=ADVANCED_FACE('',(#11365),#3736,.T.);
#93830=ADVANCED_FACE('',(#11366),#88555,.T.);
#93831=ADVANCED_FACE('',(#11367),#3737,.T.);
#93832=ADVANCED_FACE('',(#11368),#3738,.T.);
#93833=ADVANCED_FACE('',(#11369),#3739,.T.);
#93834=ADVANCED_FACE('',(#11370),#3740,.T.);
#93835=ADVANCED_FACE('',(#11371),#3741,.T.);
#93836=ADVANCED_FACE('',(#11372),#88556,.T.);
#93837=ADVANCED_FACE('',(#11373),#3742,.T.);
#93838=ADVANCED_FACE('',(#11374),#5071,.T.);
#93839=ADVANCED_FACE('',(#11375),#6040,.F.);
#93840=ADVANCED_FACE('',(#11376),#6041,.F.);
#93841=ADVANCED_FACE('',(#11377),#88557,.F.);
#93842=ADVANCED_FACE('',(#11378),#3743,.F.);
#93843=ADVANCED_FACE('',(#11379),#3744,.F.);
#93844=ADVANCED_FACE('',(#11380),#3745,.F.);
#93845=ADVANCED_FACE('',(#11381),#3746,.T.);
#93846=ADVANCED_FACE('',(#11382),#88558,.T.);
#93847=ADVANCED_FACE('',(#11383),#3747,.T.);
#93848=ADVANCED_FACE('',(#11384),#3748,.T.);
#93849=ADVANCED_FACE('',(#11385),#3749,.T.);
#93850=ADVANCED_FACE('',(#11386),#3750,.T.);
#93851=ADVANCED_FACE('',(#11387),#3751,.T.);
#93852=ADVANCED_FACE('',(#11388),#88559,.T.);
#93853=ADVANCED_FACE('',(#11389),#3752,.T.);
#93854=ADVANCED_FACE('',(#11390),#5072,.T.);
#93855=ADVANCED_FACE('',(#11391),#6042,.F.);
#93856=ADVANCED_FACE('',(#11392),#6043,.F.);
#93857=ADVANCED_FACE('',(#11393),#88560,.F.);
#93858=ADVANCED_FACE('',(#11394),#3753,.F.);
#93859=ADVANCED_FACE('',(#11395),#3754,.F.);
#93860=ADVANCED_FACE('',(#11396),#3755,.F.);
#93861=ADVANCED_FACE('',(#11397),#3756,.T.);
#93862=ADVANCED_FACE('',(#11398),#88561,.T.);
#93863=ADVANCED_FACE('',(#11399),#3757,.T.);
#93864=ADVANCED_FACE('',(#11400),#3758,.T.);
#93865=ADVANCED_FACE('',(#11401),#3759,.T.);
#93866=ADVANCED_FACE('',(#11402),#3760,.T.);
#93867=ADVANCED_FACE('',(#11403),#3761,.T.);
#93868=ADVANCED_FACE('',(#11404),#88562,.T.);
#93869=ADVANCED_FACE('',(#11405),#3762,.T.);
#93870=ADVANCED_FACE('',(#11406),#5073,.T.);
#93871=ADVANCED_FACE('',(#11407),#6044,.F.);
#93872=ADVANCED_FACE('',(#11408),#6045,.F.);
#93873=ADVANCED_FACE('',(#11409),#88563,.F.);
#93874=ADVANCED_FACE('',(#11410),#3763,.F.);
#93875=ADVANCED_FACE('',(#11411),#3764,.F.);
#93876=ADVANCED_FACE('',(#11412),#3765,.F.);
#93877=ADVANCED_FACE('',(#11413),#3766,.T.);
#93878=ADVANCED_FACE('',(#11414),#88564,.T.);
#93879=ADVANCED_FACE('',(#11415),#3767,.T.);
#93880=ADVANCED_FACE('',(#11416),#3768,.T.);
#93881=ADVANCED_FACE('',(#11417),#3769,.T.);
#93882=ADVANCED_FACE('',(#11418),#3770,.T.);
#93883=ADVANCED_FACE('',(#11419),#3771,.T.);
#93884=ADVANCED_FACE('',(#11420),#88565,.T.);
#93885=ADVANCED_FACE('',(#11421),#3772,.T.);
#93886=ADVANCED_FACE('',(#11422),#5074,.T.);
#93887=ADVANCED_FACE('',(#11423),#6046,.F.);
#93888=ADVANCED_FACE('',(#11424),#6047,.F.);
#93889=ADVANCED_FACE('',(#11425),#88566,.F.);
#93890=ADVANCED_FACE('',(#11426),#3773,.F.);
#93891=ADVANCED_FACE('',(#11427),#3774,.F.);
#93892=ADVANCED_FACE('',(#11428),#3775,.F.);
#93893=ADVANCED_FACE('',(#11429),#3776,.T.);
#93894=ADVANCED_FACE('',(#11430),#88567,.T.);
#93895=ADVANCED_FACE('',(#11431),#3777,.T.);
#93896=ADVANCED_FACE('',(#11432),#3778,.T.);
#93897=ADVANCED_FACE('',(#11433),#3779,.T.);
#93898=ADVANCED_FACE('',(#11434),#3780,.T.);
#93899=ADVANCED_FACE('',(#11435),#3781,.T.);
#93900=ADVANCED_FACE('',(#11436),#88568,.T.);
#93901=ADVANCED_FACE('',(#11437),#3782,.T.);
#93902=ADVANCED_FACE('',(#11438),#5075,.T.);
#93903=ADVANCED_FACE('',(#11439),#6048,.F.);
#93904=ADVANCED_FACE('',(#11440),#6049,.F.);
#93905=ADVANCED_FACE('',(#11441),#88569,.F.);
#93906=ADVANCED_FACE('',(#11442),#3783,.F.);
#93907=ADVANCED_FACE('',(#11443),#3784,.F.);
#93908=ADVANCED_FACE('',(#11444),#3785,.F.);
#93909=ADVANCED_FACE('',(#11445),#3786,.T.);
#93910=ADVANCED_FACE('',(#11446),#88570,.T.);
#93911=ADVANCED_FACE('',(#11447),#3787,.T.);
#93912=ADVANCED_FACE('',(#11448),#3788,.T.);
#93913=ADVANCED_FACE('',(#11449),#3789,.T.);
#93914=ADVANCED_FACE('',(#11450),#3790,.T.);
#93915=ADVANCED_FACE('',(#11451),#3791,.T.);
#93916=ADVANCED_FACE('',(#11452),#88571,.T.);
#93917=ADVANCED_FACE('',(#11453),#3792,.T.);
#93918=ADVANCED_FACE('',(#11454),#5076,.T.);
#93919=ADVANCED_FACE('',(#11455),#6050,.F.);
#93920=ADVANCED_FACE('',(#11456),#6051,.F.);
#93921=ADVANCED_FACE('',(#11457),#88572,.F.);
#93922=ADVANCED_FACE('',(#11458),#3793,.F.);
#93923=ADVANCED_FACE('',(#11459),#3794,.F.);
#93924=ADVANCED_FACE('',(#11460),#3795,.F.);
#93925=ADVANCED_FACE('',(#11461),#3796,.T.);
#93926=ADVANCED_FACE('',(#11462),#88573,.T.);
#93927=ADVANCED_FACE('',(#11463),#3797,.T.);
#93928=ADVANCED_FACE('',(#11464),#3798,.T.);
#93929=ADVANCED_FACE('',(#11465),#3799,.T.);
#93930=ADVANCED_FACE('',(#11466),#3800,.T.);
#93931=ADVANCED_FACE('',(#11467),#3801,.T.);
#93932=ADVANCED_FACE('',(#11468),#88574,.T.);
#93933=ADVANCED_FACE('',(#11469),#3802,.T.);
#93934=ADVANCED_FACE('',(#11470),#5077,.T.);
#93935=ADVANCED_FACE('',(#11471),#6052,.F.);
#93936=ADVANCED_FACE('',(#11472),#6053,.F.);
#93937=ADVANCED_FACE('',(#11473),#88575,.F.);
#93938=ADVANCED_FACE('',(#11474),#3803,.F.);
#93939=ADVANCED_FACE('',(#11475),#3804,.F.);
#93940=ADVANCED_FACE('',(#11476),#3805,.F.);
#93941=ADVANCED_FACE('',(#11477),#3806,.T.);
#93942=ADVANCED_FACE('',(#11478),#88576,.T.);
#93943=ADVANCED_FACE('',(#11479),#3807,.T.);
#93944=ADVANCED_FACE('',(#11480),#3808,.T.);
#93945=ADVANCED_FACE('',(#11481),#3809,.T.);
#93946=ADVANCED_FACE('',(#11482),#3810,.T.);
#93947=ADVANCED_FACE('',(#11483),#3811,.T.);
#93948=ADVANCED_FACE('',(#11484),#88577,.T.);
#93949=ADVANCED_FACE('',(#11485),#3812,.T.);
#93950=ADVANCED_FACE('',(#11486),#5078,.T.);
#93951=ADVANCED_FACE('',(#11487),#6054,.F.);
#93952=ADVANCED_FACE('',(#11488),#6055,.F.);
#93953=ADVANCED_FACE('',(#11489),#88578,.F.);
#93954=ADVANCED_FACE('',(#11490),#3813,.F.);
#93955=ADVANCED_FACE('',(#11491),#3814,.F.);
#93956=ADVANCED_FACE('',(#11492),#3815,.F.);
#93957=ADVANCED_FACE('',(#11493),#3816,.T.);
#93958=ADVANCED_FACE('',(#11494),#88579,.T.);
#93959=ADVANCED_FACE('',(#11495),#3817,.T.);
#93960=ADVANCED_FACE('',(#11496),#3818,.T.);
#93961=ADVANCED_FACE('',(#11497),#3819,.T.);
#93962=ADVANCED_FACE('',(#11498),#3820,.T.);
#93963=ADVANCED_FACE('',(#11499),#3821,.T.);
#93964=ADVANCED_FACE('',(#11500),#88580,.T.);
#93965=ADVANCED_FACE('',(#11501),#3822,.T.);
#93966=ADVANCED_FACE('',(#11502),#5079,.T.);
#93967=ADVANCED_FACE('',(#11503),#6056,.F.);
#93968=ADVANCED_FACE('',(#11504),#6057,.F.);
#93969=ADVANCED_FACE('',(#11505),#88581,.F.);
#93970=ADVANCED_FACE('',(#11506),#3823,.F.);
#93971=ADVANCED_FACE('',(#11507),#3824,.F.);
#93972=ADVANCED_FACE('',(#11508),#3825,.F.);
#93973=ADVANCED_FACE('',(#11509),#3826,.T.);
#93974=ADVANCED_FACE('',(#11510),#88582,.T.);
#93975=ADVANCED_FACE('',(#11511),#3827,.T.);
#93976=ADVANCED_FACE('',(#11512),#3828,.T.);
#93977=ADVANCED_FACE('',(#11513),#3829,.T.);
#93978=ADVANCED_FACE('',(#11514),#3830,.T.);
#93979=ADVANCED_FACE('',(#11515),#3831,.T.);
#93980=ADVANCED_FACE('',(#11516),#88583,.T.);
#93981=ADVANCED_FACE('',(#11517),#3832,.T.);
#93982=ADVANCED_FACE('',(#11518),#5080,.T.);
#93983=ADVANCED_FACE('',(#11519),#6058,.F.);
#93984=ADVANCED_FACE('',(#11520),#6059,.F.);
#93985=ADVANCED_FACE('',(#11521),#88584,.F.);
#93986=ADVANCED_FACE('',(#11522),#3833,.F.);
#93987=ADVANCED_FACE('',(#11523),#3834,.F.);
#93988=ADVANCED_FACE('',(#11524),#3835,.F.);
#93989=ADVANCED_FACE('',(#11525),#3836,.T.);
#93990=ADVANCED_FACE('',(#11526),#88585,.T.);
#93991=ADVANCED_FACE('',(#11527),#3837,.T.);
#93992=ADVANCED_FACE('',(#11528),#3838,.T.);
#93993=ADVANCED_FACE('',(#11529),#3839,.T.);
#93994=ADVANCED_FACE('',(#11530),#3840,.T.);
#93995=ADVANCED_FACE('',(#11531),#3841,.T.);
#93996=ADVANCED_FACE('',(#11532),#88586,.T.);
#93997=ADVANCED_FACE('',(#11533),#3842,.T.);
#93998=ADVANCED_FACE('',(#11534),#5081,.T.);
#93999=ADVANCED_FACE('',(#11535),#6060,.F.);
#94000=ADVANCED_FACE('',(#11536),#6061,.F.);
#94001=ADVANCED_FACE('',(#11537),#88587,.F.);
#94002=ADVANCED_FACE('',(#11538),#3843,.F.);
#94003=ADVANCED_FACE('',(#11539),#3844,.F.);
#94004=ADVANCED_FACE('',(#11540),#3845,.F.);
#94005=ADVANCED_FACE('',(#11541),#3846,.T.);
#94006=ADVANCED_FACE('',(#11542),#88588,.T.);
#94007=ADVANCED_FACE('',(#11543),#3847,.T.);
#94008=ADVANCED_FACE('',(#11544),#3848,.T.);
#94009=ADVANCED_FACE('',(#11545),#3849,.T.);
#94010=ADVANCED_FACE('',(#11546),#3850,.T.);
#94011=ADVANCED_FACE('',(#11547),#3851,.T.);
#94012=ADVANCED_FACE('',(#11548),#88589,.T.);
#94013=ADVANCED_FACE('',(#11549),#3852,.T.);
#94014=ADVANCED_FACE('',(#11550),#5082,.T.);
#94015=ADVANCED_FACE('',(#11551),#6062,.F.);
#94016=ADVANCED_FACE('',(#11552),#6063,.F.);
#94017=ADVANCED_FACE('',(#11553),#88590,.F.);
#94018=ADVANCED_FACE('',(#11554),#3853,.F.);
#94019=ADVANCED_FACE('',(#11555),#3854,.F.);
#94020=ADVANCED_FACE('',(#11556),#3855,.F.);
#94021=ADVANCED_FACE('',(#11557),#3856,.T.);
#94022=ADVANCED_FACE('',(#11558),#88591,.T.);
#94023=ADVANCED_FACE('',(#11559),#3857,.T.);
#94024=ADVANCED_FACE('',(#11560),#3858,.T.);
#94025=ADVANCED_FACE('',(#11561),#3859,.T.);
#94026=ADVANCED_FACE('',(#11562),#3860,.T.);
#94027=ADVANCED_FACE('',(#11563),#3861,.T.);
#94028=ADVANCED_FACE('',(#11564),#88592,.T.);
#94029=ADVANCED_FACE('',(#11565),#3862,.T.);
#94030=ADVANCED_FACE('',(#11566),#5083,.T.);
#94031=ADVANCED_FACE('',(#11567),#6064,.F.);
#94032=ADVANCED_FACE('',(#11568),#6065,.F.);
#94033=ADVANCED_FACE('',(#11569),#88593,.F.);
#94034=ADVANCED_FACE('',(#11570),#3863,.F.);
#94035=ADVANCED_FACE('',(#11571),#3864,.F.);
#94036=ADVANCED_FACE('',(#11572),#3865,.F.);
#94037=ADVANCED_FACE('',(#11573),#3866,.T.);
#94038=ADVANCED_FACE('',(#11574),#88594,.T.);
#94039=ADVANCED_FACE('',(#11575),#3867,.T.);
#94040=ADVANCED_FACE('',(#11576),#3868,.T.);
#94041=ADVANCED_FACE('',(#11577),#3869,.T.);
#94042=ADVANCED_FACE('',(#11578),#3870,.T.);
#94043=ADVANCED_FACE('',(#11579),#3871,.T.);
#94044=ADVANCED_FACE('',(#11580),#88595,.T.);
#94045=ADVANCED_FACE('',(#11581),#3872,.T.);
#94046=ADVANCED_FACE('',(#11582),#5084,.T.);
#94047=ADVANCED_FACE('',(#11583),#6066,.F.);
#94048=ADVANCED_FACE('',(#11584),#6067,.F.);
#94049=ADVANCED_FACE('',(#11585),#88596,.F.);
#94050=ADVANCED_FACE('',(#11586),#3873,.F.);
#94051=ADVANCED_FACE('',(#11587),#3874,.F.);
#94052=ADVANCED_FACE('',(#11588),#3875,.F.);
#94053=ADVANCED_FACE('',(#11589),#3876,.T.);
#94054=ADVANCED_FACE('',(#11590),#88597,.T.);
#94055=ADVANCED_FACE('',(#11591),#3877,.T.);
#94056=ADVANCED_FACE('',(#11592),#3878,.T.);
#94057=ADVANCED_FACE('',(#11593),#3879,.T.);
#94058=ADVANCED_FACE('',(#11594),#3880,.T.);
#94059=ADVANCED_FACE('',(#11595),#3881,.T.);
#94060=ADVANCED_FACE('',(#11596),#88598,.T.);
#94061=ADVANCED_FACE('',(#11597),#3882,.T.);
#94062=ADVANCED_FACE('',(#11598),#5085,.T.);
#94063=ADVANCED_FACE('',(#11599),#6068,.F.);
#94064=ADVANCED_FACE('',(#11600),#6069,.F.);
#94065=ADVANCED_FACE('',(#11601),#88599,.F.);
#94066=ADVANCED_FACE('',(#11602),#3883,.F.);
#94067=ADVANCED_FACE('',(#11603),#3884,.F.);
#94068=ADVANCED_FACE('',(#11604),#3885,.F.);
#94069=ADVANCED_FACE('',(#11605),#3886,.T.);
#94070=ADVANCED_FACE('',(#11606),#88600,.T.);
#94071=ADVANCED_FACE('',(#11607),#3887,.T.);
#94072=ADVANCED_FACE('',(#11608),#3888,.T.);
#94073=ADVANCED_FACE('',(#11609),#3889,.T.);
#94074=ADVANCED_FACE('',(#11610),#3890,.T.);
#94075=ADVANCED_FACE('',(#11611),#3891,.T.);
#94076=ADVANCED_FACE('',(#11612),#88601,.T.);
#94077=ADVANCED_FACE('',(#11613),#3892,.T.);
#94078=ADVANCED_FACE('',(#11614),#5086,.T.);
#94079=ADVANCED_FACE('',(#11615),#6070,.F.);
#94080=ADVANCED_FACE('',(#11616),#6071,.F.);
#94081=ADVANCED_FACE('',(#11617),#88602,.F.);
#94082=ADVANCED_FACE('',(#11618),#3893,.F.);
#94083=ADVANCED_FACE('',(#11619),#3894,.F.);
#94084=ADVANCED_FACE('',(#11620),#3895,.F.);
#94085=ADVANCED_FACE('',(#11621),#3896,.T.);
#94086=ADVANCED_FACE('',(#11622),#88603,.T.);
#94087=ADVANCED_FACE('',(#11623),#3897,.T.);
#94088=ADVANCED_FACE('',(#11624),#3898,.T.);
#94089=ADVANCED_FACE('',(#11625),#3899,.T.);
#94090=ADVANCED_FACE('',(#11626),#3900,.T.);
#94091=ADVANCED_FACE('',(#11627),#3901,.T.);
#94092=ADVANCED_FACE('',(#11628),#88604,.T.);
#94093=ADVANCED_FACE('',(#11629),#3902,.T.);
#94094=ADVANCED_FACE('',(#11630),#5087,.T.);
#94095=ADVANCED_FACE('',(#11631),#6072,.F.);
#94096=ADVANCED_FACE('',(#11632),#6073,.F.);
#94097=ADVANCED_FACE('',(#11633),#88605,.F.);
#94098=ADVANCED_FACE('',(#11634),#3903,.F.);
#94099=ADVANCED_FACE('',(#11635),#3904,.F.);
#94100=ADVANCED_FACE('',(#11636),#3905,.F.);
#94101=ADVANCED_FACE('',(#11637),#3906,.T.);
#94102=ADVANCED_FACE('',(#11638),#88606,.T.);
#94103=ADVANCED_FACE('',(#11639),#3907,.T.);
#94104=ADVANCED_FACE('',(#11640),#3908,.T.);
#94105=ADVANCED_FACE('',(#11641),#3909,.T.);
#94106=ADVANCED_FACE('',(#11642),#3910,.T.);
#94107=ADVANCED_FACE('',(#11643),#3911,.T.);
#94108=ADVANCED_FACE('',(#11644),#88607,.T.);
#94109=ADVANCED_FACE('',(#11645),#3912,.T.);
#94110=ADVANCED_FACE('',(#11646),#5088,.T.);
#94111=ADVANCED_FACE('',(#11647),#6074,.F.);
#94112=ADVANCED_FACE('',(#11648),#6075,.F.);
#94113=ADVANCED_FACE('',(#11649),#88608,.F.);
#94114=ADVANCED_FACE('',(#11650),#3913,.F.);
#94115=ADVANCED_FACE('',(#11651),#3914,.F.);
#94116=ADVANCED_FACE('',(#11652),#3915,.F.);
#94117=ADVANCED_FACE('',(#11653),#3916,.T.);
#94118=ADVANCED_FACE('',(#11654),#88609,.T.);
#94119=ADVANCED_FACE('',(#11655),#3917,.T.);
#94120=ADVANCED_FACE('',(#11656),#3918,.T.);
#94121=ADVANCED_FACE('',(#11657),#3919,.T.);
#94122=ADVANCED_FACE('',(#11658),#3920,.T.);
#94123=ADVANCED_FACE('',(#11659),#3921,.T.);
#94124=ADVANCED_FACE('',(#11660),#88610,.T.);
#94125=ADVANCED_FACE('',(#11661),#3922,.T.);
#94126=ADVANCED_FACE('',(#11662),#5089,.T.);
#94127=ADVANCED_FACE('',(#11663),#6076,.F.);
#94128=ADVANCED_FACE('',(#11664),#6077,.F.);
#94129=ADVANCED_FACE('',(#11665),#88611,.F.);
#94130=ADVANCED_FACE('',(#11666),#3923,.F.);
#94131=ADVANCED_FACE('',(#11667),#3924,.F.);
#94132=ADVANCED_FACE('',(#11668),#3925,.F.);
#94133=ADVANCED_FACE('',(#11669),#3926,.T.);
#94134=ADVANCED_FACE('',(#11670),#88612,.T.);
#94135=ADVANCED_FACE('',(#11671),#3927,.T.);
#94136=ADVANCED_FACE('',(#11672),#3928,.T.);
#94137=ADVANCED_FACE('',(#11673),#3929,.T.);
#94138=ADVANCED_FACE('',(#11674),#3930,.T.);
#94139=ADVANCED_FACE('',(#11675),#3931,.T.);
#94140=ADVANCED_FACE('',(#11676),#88613,.T.);
#94141=ADVANCED_FACE('',(#11677),#3932,.T.);
#94142=ADVANCED_FACE('',(#11678),#5090,.T.);
#94143=ADVANCED_FACE('',(#11679),#6078,.F.);
#94144=ADVANCED_FACE('',(#11680),#6079,.F.);
#94145=ADVANCED_FACE('',(#11681),#88614,.F.);
#94146=ADVANCED_FACE('',(#11682),#3933,.F.);
#94147=ADVANCED_FACE('',(#11683),#3934,.F.);
#94148=ADVANCED_FACE('',(#11684),#3935,.F.);
#94149=ADVANCED_FACE('',(#11685),#3936,.T.);
#94150=ADVANCED_FACE('',(#11686),#88615,.T.);
#94151=ADVANCED_FACE('',(#11687),#3937,.T.);
#94152=ADVANCED_FACE('',(#11688),#3938,.T.);
#94153=ADVANCED_FACE('',(#11689),#3939,.T.);
#94154=ADVANCED_FACE('',(#11690),#3940,.T.);
#94155=ADVANCED_FACE('',(#11691),#3941,.T.);
#94156=ADVANCED_FACE('',(#11692),#88616,.T.);
#94157=ADVANCED_FACE('',(#11693),#3942,.T.);
#94158=ADVANCED_FACE('',(#11694),#5091,.T.);
#94159=ADVANCED_FACE('',(#11695),#6080,.F.);
#94160=ADVANCED_FACE('',(#11696),#6081,.F.);
#94161=ADVANCED_FACE('',(#11697),#88617,.F.);
#94162=ADVANCED_FACE('',(#11698),#3943,.F.);
#94163=ADVANCED_FACE('',(#11699),#3944,.F.);
#94164=ADVANCED_FACE('',(#11700),#3945,.F.);
#94165=ADVANCED_FACE('',(#11701),#3946,.T.);
#94166=ADVANCED_FACE('',(#11702),#88618,.T.);
#94167=ADVANCED_FACE('',(#11703),#3947,.T.);
#94168=ADVANCED_FACE('',(#11704),#3948,.T.);
#94169=ADVANCED_FACE('',(#11705),#3949,.T.);
#94170=ADVANCED_FACE('',(#11706),#3950,.T.);
#94171=ADVANCED_FACE('',(#11707),#3951,.T.);
#94172=ADVANCED_FACE('',(#11708),#88619,.T.);
#94173=ADVANCED_FACE('',(#11709),#3952,.T.);
#94174=ADVANCED_FACE('',(#11710),#5092,.T.);
#94175=ADVANCED_FACE('',(#11711),#6082,.F.);
#94176=ADVANCED_FACE('',(#11712),#6083,.F.);
#94177=ADVANCED_FACE('',(#11713),#88620,.F.);
#94178=ADVANCED_FACE('',(#11714),#3953,.F.);
#94179=ADVANCED_FACE('',(#11715),#3954,.F.);
#94180=ADVANCED_FACE('',(#11716),#3955,.F.);
#94181=ADVANCED_FACE('',(#11717),#3956,.T.);
#94182=ADVANCED_FACE('',(#11718),#88621,.T.);
#94183=ADVANCED_FACE('',(#11719),#3957,.T.);
#94184=ADVANCED_FACE('',(#11720),#3958,.T.);
#94185=ADVANCED_FACE('',(#11721),#3959,.T.);
#94186=ADVANCED_FACE('',(#11722),#3960,.T.);
#94187=ADVANCED_FACE('',(#11723),#3961,.T.);
#94188=ADVANCED_FACE('',(#11724),#88622,.T.);
#94189=ADVANCED_FACE('',(#11725),#3962,.T.);
#94190=ADVANCED_FACE('',(#11726),#5093,.T.);
#94191=ADVANCED_FACE('',(#11727),#6084,.F.);
#94192=ADVANCED_FACE('',(#11728),#6085,.F.);
#94193=ADVANCED_FACE('',(#11729),#88623,.F.);
#94194=ADVANCED_FACE('',(#11730),#3963,.F.);
#94195=ADVANCED_FACE('',(#11731),#3964,.F.);
#94196=ADVANCED_FACE('',(#11732),#3965,.F.);
#94197=ADVANCED_FACE('',(#11733),#3966,.T.);
#94198=ADVANCED_FACE('',(#11734),#88624,.T.);
#94199=ADVANCED_FACE('',(#11735),#3967,.T.);
#94200=ADVANCED_FACE('',(#11736),#3968,.T.);
#94201=ADVANCED_FACE('',(#11737),#3969,.T.);
#94202=ADVANCED_FACE('',(#11738),#3970,.T.);
#94203=ADVANCED_FACE('',(#11739),#3971,.T.);
#94204=ADVANCED_FACE('',(#11740),#88625,.T.);
#94205=ADVANCED_FACE('',(#11741),#3972,.T.);
#94206=ADVANCED_FACE('',(#11742),#5094,.T.);
#94207=ADVANCED_FACE('',(#11743),#6086,.F.);
#94208=ADVANCED_FACE('',(#11744),#6087,.F.);
#94209=ADVANCED_FACE('',(#11745),#88626,.F.);
#94210=ADVANCED_FACE('',(#11746),#3973,.F.);
#94211=ADVANCED_FACE('',(#11747),#3974,.F.);
#94212=ADVANCED_FACE('',(#11748),#3975,.F.);
#94213=ADVANCED_FACE('',(#11749),#3976,.T.);
#94214=ADVANCED_FACE('',(#11750),#88627,.T.);
#94215=ADVANCED_FACE('',(#11751),#3977,.T.);
#94216=ADVANCED_FACE('',(#11752),#3978,.T.);
#94217=ADVANCED_FACE('',(#11753),#3979,.T.);
#94218=ADVANCED_FACE('',(#11754),#3980,.T.);
#94219=ADVANCED_FACE('',(#11755),#3981,.T.);
#94220=ADVANCED_FACE('',(#11756),#88628,.T.);
#94221=ADVANCED_FACE('',(#11757),#3982,.T.);
#94222=ADVANCED_FACE('',(#11758),#5095,.T.);
#94223=ADVANCED_FACE('',(#11759),#6088,.F.);
#94224=ADVANCED_FACE('',(#11760),#6089,.F.);
#94225=ADVANCED_FACE('',(#11761),#88629,.F.);
#94226=ADVANCED_FACE('',(#11762),#3983,.F.);
#94227=ADVANCED_FACE('',(#11763),#3984,.F.);
#94228=ADVANCED_FACE('',(#11764),#3985,.F.);
#94229=ADVANCED_FACE('',(#11765),#3986,.T.);
#94230=ADVANCED_FACE('',(#11766),#88630,.T.);
#94231=ADVANCED_FACE('',(#11767),#3987,.T.);
#94232=ADVANCED_FACE('',(#11768),#3988,.T.);
#94233=ADVANCED_FACE('',(#11769),#3989,.T.);
#94234=ADVANCED_FACE('',(#11770),#3990,.T.);
#94235=ADVANCED_FACE('',(#11771),#3991,.T.);
#94236=ADVANCED_FACE('',(#11772),#88631,.T.);
#94237=ADVANCED_FACE('',(#11773),#3992,.T.);
#94238=ADVANCED_FACE('',(#11774),#5096,.T.);
#94239=ADVANCED_FACE('',(#11775),#6090,.F.);
#94240=ADVANCED_FACE('',(#11776),#6091,.F.);
#94241=ADVANCED_FACE('',(#11777),#88632,.F.);
#94242=ADVANCED_FACE('',(#11778),#3993,.F.);
#94243=ADVANCED_FACE('',(#11779),#3994,.F.);
#94244=ADVANCED_FACE('',(#11780),#3995,.F.);
#94245=ADVANCED_FACE('',(#11781),#3996,.T.);
#94246=ADVANCED_FACE('',(#11782),#88633,.T.);
#94247=ADVANCED_FACE('',(#11783),#3997,.T.);
#94248=ADVANCED_FACE('',(#11784),#3998,.T.);
#94249=ADVANCED_FACE('',(#11785),#3999,.T.);
#94250=ADVANCED_FACE('',(#11786),#4000,.T.);
#94251=ADVANCED_FACE('',(#11787),#4001,.T.);
#94252=ADVANCED_FACE('',(#11788),#88634,.T.);
#94253=ADVANCED_FACE('',(#11789),#4002,.T.);
#94254=ADVANCED_FACE('',(#11790),#5097,.T.);
#94255=ADVANCED_FACE('',(#11791),#6092,.F.);
#94256=ADVANCED_FACE('',(#11792),#6093,.F.);
#94257=ADVANCED_FACE('',(#11793),#88635,.F.);
#94258=ADVANCED_FACE('',(#11794),#4003,.F.);
#94259=ADVANCED_FACE('',(#11795),#4004,.F.);
#94260=ADVANCED_FACE('',(#11796),#4005,.F.);
#94261=ADVANCED_FACE('',(#11797),#4006,.T.);
#94262=ADVANCED_FACE('',(#11798),#88636,.T.);
#94263=ADVANCED_FACE('',(#11799),#4007,.T.);
#94264=ADVANCED_FACE('',(#11800),#4008,.T.);
#94265=ADVANCED_FACE('',(#11801),#4009,.T.);
#94266=ADVANCED_FACE('',(#11802),#4010,.T.);
#94267=ADVANCED_FACE('',(#11803),#4011,.T.);
#94268=ADVANCED_FACE('',(#11804),#88637,.T.);
#94269=ADVANCED_FACE('',(#11805),#4012,.T.);
#94270=ADVANCED_FACE('',(#11806),#5098,.T.);
#94271=ADVANCED_FACE('',(#11807),#6094,.F.);
#94272=ADVANCED_FACE('',(#11808),#6095,.F.);
#94273=ADVANCED_FACE('',(#11809),#88638,.F.);
#94274=ADVANCED_FACE('',(#11810),#4013,.F.);
#94275=ADVANCED_FACE('',(#11811),#4014,.F.);
#94276=ADVANCED_FACE('',(#11812),#4015,.F.);
#94277=ADVANCED_FACE('',(#11813),#4016,.T.);
#94278=ADVANCED_FACE('',(#11814),#88639,.T.);
#94279=ADVANCED_FACE('',(#11815),#4017,.T.);
#94280=ADVANCED_FACE('',(#11816),#4018,.T.);
#94281=ADVANCED_FACE('',(#11817),#4019,.T.);
#94282=ADVANCED_FACE('',(#11818),#4020,.T.);
#94283=ADVANCED_FACE('',(#11819),#4021,.T.);
#94284=ADVANCED_FACE('',(#11820),#88640,.T.);
#94285=ADVANCED_FACE('',(#11821),#4022,.T.);
#94286=ADVANCED_FACE('',(#11822),#5099,.T.);
#94287=ADVANCED_FACE('',(#11823),#6096,.F.);
#94288=ADVANCED_FACE('',(#11824),#6097,.F.);
#94289=ADVANCED_FACE('',(#11825),#88641,.F.);
#94290=ADVANCED_FACE('',(#11826),#4023,.F.);
#94291=ADVANCED_FACE('',(#11827),#4024,.F.);
#94292=ADVANCED_FACE('',(#11828),#4025,.F.);
#94293=ADVANCED_FACE('',(#11829),#4026,.T.);
#94294=ADVANCED_FACE('',(#11830),#88642,.T.);
#94295=ADVANCED_FACE('',(#11831),#4027,.T.);
#94296=ADVANCED_FACE('',(#11832),#4028,.T.);
#94297=ADVANCED_FACE('',(#11833),#4029,.T.);
#94298=ADVANCED_FACE('',(#11834),#4030,.T.);
#94299=ADVANCED_FACE('',(#11835),#4031,.T.);
#94300=ADVANCED_FACE('',(#11836),#88643,.T.);
#94301=ADVANCED_FACE('',(#11837),#4032,.T.);
#94302=ADVANCED_FACE('',(#11838),#5100,.T.);
#94303=ADVANCED_FACE('',(#11839),#6098,.F.);
#94304=ADVANCED_FACE('',(#11840),#6099,.F.);
#94305=ADVANCED_FACE('',(#11841),#88644,.F.);
#94306=ADVANCED_FACE('',(#11842),#4033,.F.);
#94307=ADVANCED_FACE('',(#11843),#4034,.F.);
#94308=ADVANCED_FACE('',(#11844),#4035,.F.);
#94309=ADVANCED_FACE('',(#11845),#4036,.T.);
#94310=ADVANCED_FACE('',(#11846),#88645,.T.);
#94311=ADVANCED_FACE('',(#11847),#4037,.T.);
#94312=ADVANCED_FACE('',(#11848),#4038,.T.);
#94313=ADVANCED_FACE('',(#11849),#4039,.T.);
#94314=ADVANCED_FACE('',(#11850),#4040,.T.);
#94315=ADVANCED_FACE('',(#11851),#4041,.T.);
#94316=ADVANCED_FACE('',(#11852),#88646,.T.);
#94317=ADVANCED_FACE('',(#11853),#4042,.T.);
#94318=ADVANCED_FACE('',(#11854),#5101,.T.);
#94319=ADVANCED_FACE('',(#11855),#6100,.F.);
#94320=ADVANCED_FACE('',(#11856),#6101,.F.);
#94321=ADVANCED_FACE('',(#11857),#88647,.F.);
#94322=ADVANCED_FACE('',(#11858),#4043,.F.);
#94323=ADVANCED_FACE('',(#11859),#4044,.F.);
#94324=ADVANCED_FACE('',(#11860),#4045,.F.);
#94325=ADVANCED_FACE('',(#11861),#4046,.T.);
#94326=ADVANCED_FACE('',(#11862),#88648,.T.);
#94327=ADVANCED_FACE('',(#11863),#4047,.T.);
#94328=ADVANCED_FACE('',(#11864),#4048,.T.);
#94329=ADVANCED_FACE('',(#11865),#4049,.T.);
#94330=ADVANCED_FACE('',(#11866),#4050,.T.);
#94331=ADVANCED_FACE('',(#11867),#4051,.T.);
#94332=ADVANCED_FACE('',(#11868),#88649,.T.);
#94333=ADVANCED_FACE('',(#11869),#4052,.T.);
#94334=ADVANCED_FACE('',(#11870),#5102,.T.);
#94335=ADVANCED_FACE('',(#11871),#6102,.F.);
#94336=ADVANCED_FACE('',(#11872),#6103,.F.);
#94337=ADVANCED_FACE('',(#11873),#88650,.F.);
#94338=ADVANCED_FACE('',(#11874),#4053,.F.);
#94339=ADVANCED_FACE('',(#11875),#4054,.F.);
#94340=ADVANCED_FACE('',(#11876),#4055,.F.);
#94341=ADVANCED_FACE('',(#11877),#4056,.T.);
#94342=ADVANCED_FACE('',(#11878),#88651,.T.);
#94343=ADVANCED_FACE('',(#11879),#4057,.T.);
#94344=ADVANCED_FACE('',(#11880),#4058,.T.);
#94345=ADVANCED_FACE('',(#11881),#4059,.T.);
#94346=ADVANCED_FACE('',(#11882),#4060,.T.);
#94347=ADVANCED_FACE('',(#11883),#4061,.T.);
#94348=ADVANCED_FACE('',(#11884),#88652,.T.);
#94349=ADVANCED_FACE('',(#11885),#4062,.T.);
#94350=ADVANCED_FACE('',(#11886),#5103,.T.);
#94351=ADVANCED_FACE('',(#11887),#6104,.F.);
#94352=ADVANCED_FACE('',(#11888),#6105,.F.);
#94353=ADVANCED_FACE('',(#11889),#88653,.F.);
#94354=ADVANCED_FACE('',(#11890),#4063,.F.);
#94355=ADVANCED_FACE('',(#11891),#4064,.F.);
#94356=ADVANCED_FACE('',(#11892),#4065,.F.);
#94357=ADVANCED_FACE('',(#11893),#4066,.T.);
#94358=ADVANCED_FACE('',(#11894),#88654,.T.);
#94359=ADVANCED_FACE('',(#11895),#4067,.T.);
#94360=ADVANCED_FACE('',(#11896),#4068,.T.);
#94361=ADVANCED_FACE('',(#11897),#4069,.T.);
#94362=ADVANCED_FACE('',(#11898),#4070,.T.);
#94363=ADVANCED_FACE('',(#11899),#4071,.T.);
#94364=ADVANCED_FACE('',(#11900),#88655,.T.);
#94365=ADVANCED_FACE('',(#11901),#4072,.T.);
#94366=ADVANCED_FACE('',(#11902),#5104,.T.);
#94367=ADVANCED_FACE('',(#11903),#88656,.F.);
#94368=ADVANCED_FACE('',(#11904),#88657,.F.);
#94369=ADVANCED_FACE('',(#11905),#88658,.F.);
#94370=ADVANCED_FACE('',(#11906),#88659,.F.);
#94371=ADVANCED_FACE('',(#11907),#88660,.F.);
#94372=ADVANCED_FACE('',(#11908),#88661,.F.);
#94373=ADVANCED_FACE('',(#11909),#88662,.F.);
#94374=ADVANCED_FACE('',(#11910),#88663,.F.);
#94375=ADVANCED_FACE('',(#11911),#88664,.F.);
#94376=ADVANCED_FACE('',(#11912),#88665,.F.);
#94377=ADVANCED_FACE('',(#11913),#88666,.F.);
#94378=ADVANCED_FACE('',(#11914),#88667,.F.);
#94379=ADVANCED_FACE('',(#11915),#88668,.F.);
#94380=ADVANCED_FACE('',(#11916),#88669,.F.);
#94381=ADVANCED_FACE('',(#11917),#88670,.F.);
#94382=ADVANCED_FACE('',(#11918),#88671,.F.);
#94383=ADVANCED_FACE('',(#11919),#88672,.F.);
#94384=ADVANCED_FACE('',(#11920),#88673,.F.);
#94385=ADVANCED_FACE('',(#11921),#88674,.F.);
#94386=ADVANCED_FACE('',(#11922),#88675,.F.);
#94387=ADVANCED_FACE('',(#11923),#88676,.F.);
#94388=ADVANCED_FACE('',(#11924),#88677,.F.);
#94389=ADVANCED_FACE('',(#11925),#88678,.F.);
#94390=ADVANCED_FACE('',(#11926),#88679,.F.);
#94391=ADVANCED_FACE('',(#11927),#88680,.F.);
#94392=ADVANCED_FACE('',(#11928),#88681,.F.);
#94393=ADVANCED_FACE('',(#11929),#88682,.F.);
#94394=ADVANCED_FACE('',(#11930),#88683,.F.);
#94395=ADVANCED_FACE('',(#11931),#88684,.F.);
#94396=ADVANCED_FACE('',(#11932),#88685,.F.);
#94397=ADVANCED_FACE('',(#11933),#88686,.F.);
#94398=ADVANCED_FACE('',(#11934),#88687,.F.);
#94399=ADVANCED_FACE('',(#11935),#88688,.F.);
#94400=ADVANCED_FACE('',(#11936),#88689,.F.);
#94401=ADVANCED_FACE('',(#11937),#88690,.F.);
#94402=ADVANCED_FACE('',(#11938),#88691,.F.);
#94403=ADVANCED_FACE('',(#11939),#88692,.F.);
#94404=ADVANCED_FACE('',(#11940),#88693,.F.);
#94405=ADVANCED_FACE('',(#11941),#88694,.F.);
#94406=ADVANCED_FACE('',(#11942),#88695,.F.);
#94407=ADVANCED_FACE('',(#11943),#88696,.F.);
#94408=ADVANCED_FACE('',(#11944),#88697,.F.);
#94409=ADVANCED_FACE('',(#11945),#88698,.F.);
#94410=ADVANCED_FACE('',(#11946),#88699,.F.);
#94411=ADVANCED_FACE('',(#11947),#88700,.F.);
#94412=ADVANCED_FACE('',(#11948),#88701,.F.);
#94413=ADVANCED_FACE('',(#11949),#88702,.F.);
#94414=ADVANCED_FACE('',(#11950),#88703,.F.);
#94415=ADVANCED_FACE('',(#11951),#88704,.F.);
#94416=ADVANCED_FACE('',(#11952),#88705,.F.);
#94417=ADVANCED_FACE('',(#11953),#88706,.F.);
#94418=ADVANCED_FACE('',(#11954),#88707,.F.);
#94419=ADVANCED_FACE('',(#11955),#88708,.F.);
#94420=ADVANCED_FACE('',(#11956),#88709,.F.);
#94421=ADVANCED_FACE('',(#11957),#88710,.F.);
#94422=ADVANCED_FACE('',(#11958),#88711,.F.);
#94423=ADVANCED_FACE('',(#11959),#88712,.F.);
#94424=ADVANCED_FACE('',(#11960),#88713,.F.);
#94425=ADVANCED_FACE('',(#11961),#88714,.F.);
#94426=ADVANCED_FACE('',(#11962),#88715,.F.);
#94427=ADVANCED_FACE('',(#11963),#88716,.F.);
#94428=ADVANCED_FACE('',(#11964),#88717,.F.);
#94429=ADVANCED_FACE('',(#11965),#88718,.F.);
#94430=ADVANCED_FACE('',(#11966),#88719,.F.);
#94431=ADVANCED_FACE('',(#11967),#5105,.F.);
#94432=ADVANCED_FACE('',(#11968),#88720,.F.);
#94433=ADVANCED_FACE('',(#11969,#5230,#5231,#5232,#5233,#5234),#6106,.T.);
#94434=ADVANCED_FACE('',(#11970),#88721,.F.);
#94435=ADVANCED_FACE('',(#11971),#6337,.F.);
#94436=ADVANCED_FACE('',(#11972),#6338,.F.);
#94437=ADVANCED_FACE('',(#11973,#5235,#5236,#5237,#5238,#5239),#6107,.T.);
#94438=ADVANCED_FACE('',(#11974),#88722,.F.);
#94439=ADVANCED_FACE('',(#11975),#88723,.T.);
#94440=ADVANCED_FACE('',(#11976),#5106,.F.);
#94441=ADVANCED_FACE('',(#11977),#88724,.F.);
#94442=ADVANCED_FACE('',(#11978),#88725,.T.);
#94443=ADVANCED_FACE('',(#11979),#88726,.T.);
#94444=ADVANCED_FACE('',(#11980),#88727,.T.);
#94445=ADVANCED_FACE('',(#11981),#88728,.T.);
#94446=ADVANCED_FACE('',(#11982),#88729,.T.);
#94447=ADVANCED_FACE('',(#11983),#88730,.T.);
#94448=ADVANCED_FACE('',(#11984),#88731,.T.);
#94449=ADVANCED_FACE('',(#11985),#88732,.T.);
#94450=ADVANCED_FACE('',(#11986),#88733,.T.);
#94451=ADVANCED_FACE('',(#11987),#88734,.T.);
#94452=ADVANCED_FACE('',(#11988),#88735,.T.);
#94453=ADVANCED_FACE('',(#11989),#88736,.T.);
#94454=ADVANCED_FACE('',(#11990),#88737,.T.);
#94455=ADVANCED_FACE('',(#11991),#88738,.T.);
#94456=ADVANCED_FACE('',(#11992),#88739,.T.);
#94457=ADVANCED_FACE('',(#11993),#88740,.T.);
#94458=ADVANCED_FACE('',(#11994),#88741,.T.);
#94459=ADVANCED_FACE('',(#11995),#88742,.T.);
#94460=ADVANCED_FACE('',(#11996),#88743,.T.);
#94461=ADVANCED_FACE('',(#11997),#88744,.T.);
#94462=ADVANCED_FACE('',(#11998,#5240),#6108,.T.);
#94463=ADVANCED_FACE('',(#11999,#5241),#6109,.T.);
#94464=ADVANCED_FACE('',(#12000,#5242),#6110,.T.);
#94465=ADVANCED_FACE('',(#12001,#5243),#6111,.T.);
#94466=ADVANCED_FACE('',(#12002,#5244),#6112,.T.);
#94467=ADVANCED_FACE('',(#12003,#5245),#6113,.T.);
#94468=ADVANCED_FACE('',(#12004,#5246),#6114,.T.);
#94469=ADVANCED_FACE('',(#12005,#5247),#6115,.T.);
#94470=ADVANCED_FACE('',(#12006,#5248),#6116,.T.);
#94471=ADVANCED_FACE('',(#12007,#5249),#6117,.T.);
#94472=ADVANCED_FACE('',(#12008,#5250),#6118,.T.);
#94473=ADVANCED_FACE('',(#12009,#5251),#6119,.T.);
#94474=ADVANCED_FACE('',(#12010,#5252),#6120,.T.);
#94475=ADVANCED_FACE('',(#12011,#5253),#6121,.T.);
#94476=ADVANCED_FACE('',(#12012,#5254),#6122,.T.);
#94477=ADVANCED_FACE('',(#12013,#5255),#6123,.T.);
#94478=ADVANCED_FACE('',(#12014,#5256),#6124,.T.);
#94479=ADVANCED_FACE('',(#12015,#5257),#6125,.T.);
#94480=ADVANCED_FACE('',(#12016,#5258),#6126,.T.);
#94481=ADVANCED_FACE('',(#12017,#5259),#6127,.T.);
#94482=ADVANCED_FACE('',(#12018),#88745,.F.);
#94483=ADVANCED_FACE('',(#12019),#6339,.F.);
#94484=ADVANCED_FACE('',(#12020),#6340,.F.);
#94485=ADVANCED_FACE('',(#12021),#88746,.F.);
#94486=ADVANCED_FACE('',(#12022),#88747,.F.);
#94487=ADVANCED_FACE('',(#12023),#6341,.F.);
#94488=ADVANCED_FACE('',(#12024),#6342,.F.);
#94489=ADVANCED_FACE('',(#12025),#88748,.F.);
#94490=ADVANCED_FACE('',(#12026),#88749,.F.);
#94491=ADVANCED_FACE('',(#12027),#6343,.F.);
#94492=ADVANCED_FACE('',(#12028),#6344,.F.);
#94493=ADVANCED_FACE('',(#12029),#88750,.F.);
#94494=ADVANCED_FACE('',(#12030),#88751,.T.);
#94495=ADVANCED_FACE('',(#12031),#88752,.T.);
#94496=ADVANCED_FACE('',(#12032),#88753,.T.);
#94497=ADVANCED_FACE('',(#12033),#88754,.T.);
#94498=ADVANCED_FACE('',(#12034),#88755,.T.);
#94499=ADVANCED_FACE('',(#12035),#88756,.T.);
#94500=ADVANCED_FACE('',(#12036),#88757,.T.);
#94501=ADVANCED_FACE('',(#12037),#88758,.T.);
#94502=ADVANCED_FACE('',(#12038),#88759,.T.);
#94503=ADVANCED_FACE('',(#12039),#88760,.T.);
#94504=ADVANCED_FACE('',(#12040),#88761,.T.);
#94505=ADVANCED_FACE('',(#12041),#88762,.T.);
#94506=ADVANCED_FACE('',(#12042),#88763,.T.);
#94507=ADVANCED_FACE('',(#12043),#88764,.T.);
#94508=ADVANCED_FACE('',(#12044),#88765,.T.);
#94509=ADVANCED_FACE('',(#12045),#88766,.T.);
#94510=ADVANCED_FACE('',(#12046),#88767,.T.);
#94511=ADVANCED_FACE('',(#12047),#88768,.T.);
#94512=ADVANCED_FACE('',(#12048),#88769,.T.);
#94513=ADVANCED_FACE('',(#12049),#88770,.T.);
#94514=ADVANCED_FACE('',(#12050),#88771,.T.);
#94515=ADVANCED_FACE('',(#12051),#88772,.T.);
#94516=ADVANCED_FACE('',(#12052),#88773,.T.);
#94517=ADVANCED_FACE('',(#12053),#88774,.T.);
#94518=ADVANCED_FACE('',(#12054),#88775,.T.);
#94519=ADVANCED_FACE('',(#12055),#88776,.T.);
#94520=ADVANCED_FACE('',(#12056),#88777,.T.);
#94521=ADVANCED_FACE('',(#12057),#88778,.T.);
#94522=ADVANCED_FACE('',(#12058),#88779,.T.);
#94523=ADVANCED_FACE('',(#12059),#88780,.T.);
#94524=ADVANCED_FACE('',(#12060),#6345,.F.);
#94525=ADVANCED_FACE('',(#12061),#88781,.T.);
#94526=ADVANCED_FACE('',(#12062),#6346,.F.);
#94527=ADVANCED_FACE('',(#12063,#5260),#6128,.F.);
#94528=ADVANCED_FACE('',(#12064),#88782,.T.);
#94529=ADVANCED_FACE('',(#12065),#6129,.F.);
#94530=ADVANCED_FACE('',(#12066),#6347,.F.);
#94531=ADVANCED_FACE('',(#12067),#88783,.T.);
#94532=ADVANCED_FACE('',(#12068),#6348,.F.);
#94533=ADVANCED_FACE('',(#12069),#5107,.T.);
#94534=ADVANCED_FACE('',(#12070),#88784,.T.);
#94535=ADVANCED_FACE('',(#12071),#88785,.T.);
#94536=ADVANCED_FACE('',(#12072),#88786,.T.);
#94537=ADVANCED_FACE('',(#12073),#88787,.F.);
#94538=ADVANCED_FACE('',(#12074),#5108,.F.);
#94539=ADVANCED_FACE('',(#12075),#88788,.F.);
#94540=ADVANCED_FACE('',(#12076,#5261),#6130,.F.);
#94541=ADVANCED_FACE('',(#12077),#6131,.F.);
#94542=ADVANCED_FACE('',(#12078,#5262),#6132,.F.);
#94543=ADVANCED_FACE('',(#12079,#5263),#6133,.F.);
#94544=ADVANCED_FACE('',(#12080,#5264),#6134,.F.);
#94545=ADVANCED_FACE('',(#12081),#88789,.F.);
#94546=ADVANCED_FACE('',(#12082),#88790,.T.);
#94547=ADVANCED_FACE('',(#12083,#5265),#6135,.T.);
#94548=ADVANCED_FACE('',(#12084),#88791,.T.);
#94549=ADVANCED_FACE('',(#12085),#88792,.T.);
#94550=ADVANCED_FACE('',(#12086),#88793,.T.);
#94551=ADVANCED_FACE('',(#12087),#88794,.T.);
#94552=ADVANCED_FACE('',(#12088),#88795,.T.);
#94553=ADVANCED_FACE('',(#12089),#88796,.T.);
#94554=ADVANCED_FACE('',(#12090),#88797,.T.);
#94555=ADVANCED_FACE('',(#12091),#88798,.T.);
#94556=ADVANCED_FACE('',(#12092),#88799,.T.);
#94557=ADVANCED_FACE('',(#12093),#88800,.T.);
#94558=ADVANCED_FACE('',(#12094),#88801,.T.);
#94559=ADVANCED_FACE('',(#12095),#88802,.T.);
#94560=ADVANCED_FACE('',(#12096),#6349,.F.);
#94561=ADVANCED_FACE('',(#12097),#6136,.T.);
#94562=ADVANCED_FACE('',(#12098),#88803,.T.);
#94563=ADVANCED_FACE('',(#12099),#6350,.F.);
#94564=ADVANCED_FACE('',(#12100),#6137,.F.);
#94565=ADVANCED_FACE('',(#12101,#5266),#6138,.F.);
#94566=ADVANCED_FACE('',(#12102),#88804,.T.);
#94567=ADVANCED_FACE('',(#12103),#5109,.F.);
#94568=ADVANCED_FACE('',(#12104),#88805,.F.);
#94569=ADVANCED_FACE('',(#12105),#5110,.F.);
#94570=ADVANCED_FACE('',(#12106),#5111,.T.);
#94571=ADVANCED_FACE('',(#12107),#88806,.T.);
#94572=ADVANCED_FACE('',(#12108),#5112,.F.);
#94573=ADVANCED_FACE('',(#12109),#88807,.F.);
#94574=ADVANCED_FACE('',(#12110),#88808,.F.);
#94575=ADVANCED_FACE('',(#12111,#5267),#6139,.F.);
#94576=ADVANCED_FACE('',(#12112,#5268),#6140,.T.);
#94577=ADVANCED_FACE('',(#12113),#6141,.F.);
#94578=ADVANCED_FACE('',(#12114),#6142,.F.);
#94579=ADVANCED_FACE('',(#12115),#6143,.F.);
#94580=ADVANCED_FACE('',(#12116),#6144,.F.);
#94581=ADVANCED_FACE('',(#12117),#6145,.F.);
#94582=ADVANCED_FACE('',(#12118),#6146,.F.);
#94583=ADVANCED_FACE('',(#12119,#5269),#6147,.F.);
#94584=ADVANCED_FACE('',(#12120),#88809,.F.);
#94585=ADVANCED_FACE('',(#12121),#88810,.F.);
#94586=ADVANCED_FACE('',(#12122),#88811,.F.);
#94587=ADVANCED_FACE('',(#12123),#88812,.F.);
#94588=ADVANCED_FACE('',(#12124),#88813,.F.);
#94589=ADVANCED_FACE('',(#12125),#88814,.F.);
#94590=ADVANCED_FACE('',(#12126),#6148,.F.);
#94591=ADVANCED_FACE('',(#12127),#6149,.F.);
#94592=ADVANCED_FACE('',(#12128,#5270,#5271),#6150,.F.);
#94593=ADVANCED_FACE('',(#12129),#6151,.F.);
#94594=ADVANCED_FACE('',(#12130),#6152,.F.);
#94595=ADVANCED_FACE('',(#12131,#5272,#5273),#6153,.T.);
#94596=ADVANCED_FACE('',(#12132,#5274,#5275),#6154,.F.);
#94597=ADVANCED_FACE('',(#12133,#5276),#6155,.F.);
#94598=ADVANCED_FACE('',(#12134,#5277),#6156,.F.);
#94599=ADVANCED_FACE('',(#12135),#6157,.T.);
#94600=ADVANCED_FACE('',(#12136),#6158,.T.);
#94601=ADVANCED_FACE('',(#12137),#6159,.F.);
#94602=ADVANCED_FACE('',(#12138),#6160,.F.);
#94603=ADVANCED_FACE('',(#12139),#6161,.T.);
#94604=ADVANCED_FACE('',(#12140),#6162,.T.);
#94605=ADVANCED_FACE('',(#12141),#6163,.F.);
#94606=ADVANCED_FACE('',(#12142),#6164,.T.);
#94607=ADVANCED_FACE('',(#12143),#6165,.T.);
#94608=ADVANCED_FACE('',(#12144),#6166,.F.);
#94609=ADVANCED_FACE('',(#12145),#6167,.F.);
#94610=ADVANCED_FACE('',(#12146),#6168,.F.);
#94611=ADVANCED_FACE('',(#12147),#6169,.F.);
#94612=ADVANCED_FACE('',(#12148),#6170,.T.);
#94613=ADVANCED_FACE('',(#12149),#6171,.T.);
#94614=ADVANCED_FACE('',(#12150),#6172,.T.);
#94615=ADVANCED_FACE('',(#12151),#6173,.T.);
#94616=ADVANCED_FACE('',(#12152),#6174,.T.);
#94617=ADVANCED_FACE('',(#12153),#6175,.T.);
#94618=ADVANCED_FACE('',(#12154),#6176,.F.);
#94619=ADVANCED_FACE('',(#12155),#6177,.F.);
#94620=ADVANCED_FACE('',(#12156),#6178,.T.);
#94621=ADVANCED_FACE('',(#12157),#6179,.T.);
#94622=ADVANCED_FACE('',(#12158),#6180,.F.);
#94623=CLOSED_SHELL('',(#88815,#88816,#88817,#88818,#88819,#88820,#88821,
#88822,#88823,#88824,#88825,#88826,#88827,#88828,#88829,#88830,#88831,#88832,
#88833,#88834,#88835,#88836,#88837,#88838,#88839,#88840,#88841,#88842,#88843,
#88844,#88845,#88846,#88847,#88848,#88849,#88850,#88851,#88852,#88853,#88854,
#88855,#88856,#88857,#88858,#88859,#88860,#88861,#88862,#88863,#88864,#88865,
#88866,#88867,#88868,#88869,#88870,#88871,#88872,#88873,#88874,#88875,#88876,
#88877,#88878,#88879,#88880,#88881,#88882,#88883,#88884,#88885,#88886,#88887,
#88888,#88889,#88890,#88891,#88892,#88893,#88894,#88895,#88896,#88897,#88898,
#88899,#88900,#88901,#88902,#88903,#88904,#88905,#88906,#88907,#88908,#88909,
#88910,#88911,#88912,#88913,#88914,#88915,#88916,#88917,#88918,#88919,#88920,
#88921,#88922,#88923,#88924,#88925,#88926,#88927,#88928,#88929,#88930,#88931,
#88932,#88933,#88934,#88935,#88936,#88937,#88938,#88939,#88940,#88941,#88942,
#88943,#88944,#88945,#88946,#88947,#88948,#88949,#88950,#88951,#88952,#88953,
#88954,#88955,#88956,#88957,#88958,#88959,#88960,#88961,#88962,#88963,#88964,
#88965,#88966,#88967,#88968,#88969,#88970,#88971,#88972,#88973,#88974,#88975,
#88976,#88977,#88978,#88979,#88980,#88981,#88982,#88983,#88984,#88985,#88986,
#88987,#88988,#88989,#88990,#88991,#88992,#88993,#88994,#88995,#88996,#88997,
#88998,#88999));
#94624=CLOSED_SHELL('',(#89000,#89001,#89002,#89003,#89004,#89005,#89006,
#89007,#89008,#89009,#89010,#89011,#89012,#89013,#89014,#89015,#89016,#89017,
#89018,#89019,#89020,#89021,#89022,#89023,#89024,#89025,#89026,#89027,#89028,
#89029,#89030,#89031,#89032));
#94625=CLOSED_SHELL('',(#89033,#89034,#89035,#89036,#89037,#89038,#89039,
#89040,#89041,#89042,#89043,#89044,#89045,#89046,#89047,#89048));
#94626=CLOSED_SHELL('',(#89049,#89050,#89051,#89052,#89053,#89054,#89055,
#89056,#89057,#89058,#89059,#89060,#89061,#89062,#89063,#89064,#89065,#89066,
#89067,#89068,#89069,#89070,#89071,#89072,#89073,#89074,#89075,#89076,#89077,
#89078,#89079,#89080,#89081,#89082,#89083,#89084,#89085,#89086,#89087,#89088,
#89089,#89090,#89091,#89092,#89093,#89094,#89095,#89096,#89097,#89098,#89099,
#89100,#89101,#89102,#89103,#89104,#89105,#89106,#89107,#89108,#89109,#89110,
#89111,#89112,#89113,#89114,#89115,#89116,#89117,#89118,#89119,#89120,#89121,
#89122,#89123,#89124,#89125,#89126,#89127,#89128,#89129,#89130,#89131,#89132,
#89133,#89134,#89135,#89136,#89137,#89138,#89139,#89140,#89141,#89142,#89143,
#89144,#89145,#89146,#89147,#89148,#89149,#89150,#89151,#89152,#89153,#89154,
#89155,#89156,#89157,#89158,#89159,#89160,#89161,#89162,#89163,#89164,#89165,
#89166,#89167,#89168,#89169,#89170,#89171,#89172,#89173,#89174,#89175,#89176,
#89177,#89178,#89179,#89180,#89181,#89182,#89183,#89184,#89185,#89186,#89187,
#89188,#89189,#89190,#89191,#89192,#89193,#89194,#89195,#89196,#89197,#89198,
#89199,#89200,#89201,#89202,#89203,#89204,#89205,#89206,#89207,#89208,#89209,
#89210,#89211,#89212,#89213,#89214,#89215,#89216,#89217,#89218,#89219,#89220,
#89221,#89222,#89223,#89224,#89225,#89226,#89227,#89228,#89229,#89230,#89231,
#89232,#89233,#89234,#89235,#89236,#89237,#89238,#89239,#89240,#89241,#89242,
#89243,#89244,#89245,#89246,#89247,#89248,#89249,#89250,#89251,#89252,#89253,
#89254,#89255,#89256,#89257,#89258,#89259,#89260,#89261,#89262,#89263,#89264,
#89265,#89266,#89267,#89268,#89269,#89270,#89271,#89272,#89273,#89274,#89275,
#89276,#89277,#89278,#89279,#89280,#89281,#89282,#89283,#89284,#89285,#89286,
#89287,#89288,#89289,#89290,#89291,#89292,#89293,#89294,#89295,#89296,#89297,
#89298,#89299,#89300,#89301,#89302,#89303,#89304,#89305,#89306,#89307,#89308,
#89309,#89310,#89311,#89312,#89313,#89314,#89315,#89316,#89317,#89318,#89319,
#89320,#89321,#89322,#89323,#89324,#89325,#89326,#89327,#89328,#89329,#89330,
#89331,#89332,#89333,#89334,#89335,#89336,#89337,#89338,#89339,#89340,#89341,
#89342,#89343,#89344,#89345,#89346,#89347,#89348));
#94627=CLOSED_SHELL('',(#89349,#89350,#89351,#89352,#89353));
#94628=CLOSED_SHELL('',(#89354,#89355,#89356,#89357,#89358,#89359,#89360,
#89361,#89362,#89363,#89364,#89365,#89366,#89367,#89368,#89369,#89370,#89371,
#89372,#89373,#89374,#89375,#89376,#89377,#89378,#89379,#89380,#89381,#89382,
#89383,#89384,#89385,#89386,#89387,#89388,#89389,#89390,#89391,#89392,#89393,
#89394,#89395,#89396,#89397,#89398,#89399,#89400,#89401,#89402,#89403,#89404,
#89405,#89406,#89407,#89408,#89409,#89410,#89411,#89412,#89413,#89414,#89415,
#89416,#89417,#89418,#89419,#89420,#89421,#89422,#89423,#89424,#89425,#89426,
#89427,#89428,#89429,#89430,#89431,#89432,#89433,#89434,#89435,#89436,#89437,
#89438,#89439,#89440,#89441,#89442,#89443,#89444,#89445,#89446,#89447,#89448,
#89449,#89450,#89451,#89452,#89453,#89454,#89455,#89456,#89457,#89458,#89459,
#89460,#89461,#89462,#89463,#89464,#89465,#89466,#89467,#89468,#89469,#89470,
#89471,#89472,#89473,#89474,#89475,#89476,#89477,#89478,#89479,#89480,#89481,
#89482,#89483,#89484,#89485,#89486,#89487,#89488,#89489,#89490,#89491,#89492,
#89493,#89494,#89495,#89496,#89497,#89498,#89499,#89500,#89501,#89502,#89503,
#89504,#89505,#89506,#89507,#89508,#89509,#89510,#89511,#89512,#89513,#89514,
#89515,#89516,#89517,#89518,#89519,#89520,#89521,#89522,#89523,#89524,#89525,
#89526,#89527,#89528,#89529,#89530,#89531,#89532,#89533,#89534,#89535,#89536,
#89537,#89538,#89539,#89540,#89541,#89542,#89543,#89544,#89545,#89546,#89547,
#89548,#89549,#89550,#89551,#89552,#89553,#89554,#89555,#89556,#89557,#89558,
#89559,#89560,#89561,#89562,#89563,#89564,#89565,#89566,#89567,#89568,#89569,
#89570,#89571,#89572,#89573,#89574,#89575,#89576,#89577,#89578,#89579,#89580,
#89581,#89582,#89583,#89584,#89585,#89586,#89587,#89588,#89589,#89590,#89591,
#89592,#89593,#89594,#89595,#89596,#89597,#89598,#89599,#89600,#89601,#89602,
#89603,#89604,#89605,#89606,#89607,#89608,#89609,#89610,#89611,#89612,#89613,
#89614,#89615,#89616,#89617,#89618,#89619,#89620,#89621,#89622,#89623,#89624,
#89625,#89626,#89627,#89628,#89629,#89630,#89631,#89632,#89633,#89634,#89635,
#89636,#89637,#89638,#89639,#89640,#89641,#89642,#89643,#89644,#89645,#89646,
#89647,#89648,#89649,#89650,#89651,#89652,#89653,#89654,#89655,#89656,#89657,
#89658,#89659,#89660,#89661,#89662,#89663,#89664,#89665,#89666,#89667,#89668,
#89669,#89670,#89671,#89672,#89673,#89674,#89675,#89676,#89677,#89678,#89679,
#89680,#89681,#89682,#89683,#89684,#89685,#89686,#89687,#89688,#89689,#89690,
#89691,#89692,#89693,#89694,#89695,#89696,#89697,#89698,#89699,#89700,#89701,
#89702,#89703,#89704,#89705,#89706,#89707,#89708,#89709,#89710,#89711,#89712,
#89713,#89714,#89715,#89716,#89717,#89718,#89719,#89720,#89721,#89722,#89723,
#89724,#89725,#89726,#89727,#89728,#89729,#89730,#89731,#89732,#89733,#89734,
#89735,#89736,#89737,#89738,#89739,#89740,#89741,#89742,#89743,#89744,#89745,
#89746,#89747,#89748,#89749,#89750,#89751,#89752,#89753,#89754,#89755,#89756,
#89757,#89758,#89759,#89760,#89761,#89762,#89763,#89764,#89765,#89766,#89767,
#89768,#89769,#89770,#89771,#89772,#89773,#89774,#89775,#89776,#89777,#89778,
#89779,#89780,#89781,#89782,#89783,#89784,#89785,#89786,#89787,#89788,#89789,
#89790,#89791,#89792,#89793,#89794,#89795,#89796,#89797,#89798,#89799,#89800,
#89801,#89802,#89803,#89804,#89805,#89806,#89807,#89808,#89809,#89810,#89811,
#89812,#89813,#89814,#89815,#89816,#89817,#89818,#89819,#89820,#89821,#89822,
#89823,#89824,#89825,#89826,#89827));
#94629=CLOSED_SHELL('',(#89828,#89829,#89830,#89831,#89832,#89833,#89834,
#89835,#89836,#89837,#89838,#89839,#89840,#89841,#89842,#89843,#89844,#89845,
#89846,#89847,#89848,#89849,#89850,#89851,#89852,#89853,#89854,#89855,#89856,
#89857,#89858,#89859,#89860,#89861,#89862,#89863,#89864,#89865,#89866,#89867,
#89868,#89869,#89870,#89871,#89872,#89873,#89874,#89875,#89876,#89877,#89878,
#89879,#89880,#89881,#89882,#89883,#89884,#89885,#89886,#89887,#89888,#89889,
#89890,#89891,#89892,#89893));
#94630=CLOSED_SHELL('',(#89894,#89895,#89896,#89897,#89898));
#94631=CLOSED_SHELL('',(#89899,#89900,#89901,#89902,#89903));
#94632=CLOSED_SHELL('',(#89904,#89905,#89906,#89907,#89908,#89909,#89910,
#89911,#89912,#89913,#89914,#89915,#89916,#89917,#89918,#89919,#89920,#89921,
#89922,#89923,#89924,#89925,#89926,#89927,#89928,#89929,#89930,#89931,#89932,
#89933,#89934,#89935,#89936,#89937,#89938,#89939,#89940,#89941,#89942,#89943,
#89944,#89945,#89946,#89947,#89948,#89949,#89950,#89951,#89952,#89953,#89954,
#89955,#89956,#89957,#89958,#89959,#89960,#89961,#89962,#89963,#89964,#89965,
#89966,#89967,#89968,#89969,#89970,#89971,#89972,#89973,#89974,#89975,#89976,
#89977,#89978,#89979,#89980,#89981,#89982,#89983,#89984,#89985,#89986,#89987,
#89988,#89989,#89990,#89991,#89992,#89993,#89994,#89995,#89996,#89997,#89998,
#89999,#90000,#90001,#90002,#90003,#90004,#90005,#90006,#90007,#90008,#90009,
#90010,#90011,#90012,#90013,#90014,#90015,#90016,#90017,#90018,#90019,#90020,
#90021,#90022,#90023,#90024,#90025,#90026,#90027,#90028,#90029,#90030,#90031,
#90032,#90033,#90034,#90035,#90036,#90037,#90038,#90039,#90040,#90041,#90042,
#90043,#90044,#90045,#90046,#90047,#90048,#90049,#90050,#90051,#90052,#90053,
#90054,#90055,#90056,#90057,#90058,#90059,#90060,#90061,#90062,#90063,#90064,
#90065,#90066,#90067,#90068,#90069,#90070,#90071,#90072,#90073,#90074,#90075,
#90076,#90077,#90078,#90079,#90080,#90081,#90082,#90083,#90084,#90085,#90086,
#90087,#90088,#90089,#90090,#90091,#90092,#90093,#90094,#90095,#90096,#90097,
#90098,#90099,#90100,#90101,#90102,#90103,#90104,#90105,#90106,#90107,#90108,
#90109,#90110,#90111,#90112,#90113,#90114,#90115,#90116,#90117,#90118,#90119,
#90120,#90121,#90122,#90123,#90124,#90125,#90126,#90127,#90128,#90129,#90130,
#90131,#90132,#90133,#90134,#90135,#90136,#90137,#90138,#90139,#90140,#90141,
#90142,#90143,#90144,#90145,#90146,#90147,#90148,#90149,#90150,#90151,#90152,
#90153,#90154,#90155,#90156,#90157,#90158,#90159,#90160,#90161,#90162,#90163,
#90164,#90165,#90166,#90167,#90168,#90169,#90170,#90171,#90172,#90173,#90174,
#90175,#90176,#90177,#90178,#90179,#90180,#90181,#90182,#90183,#90184,#90185,
#90186,#90187,#90188,#90189,#90190,#90191,#90192,#90193,#90194,#90195,#90196,
#90197,#90198,#90199,#90200));
#94633=CLOSED_SHELL('',(#90201,#90202,#90203,#90204,#90205,#90206,#90207,
#90208,#90209,#90210,#90211,#90212,#90213,#90214,#90215,#90216,#90217,#90218,
#90219,#90220,#90221,#90222,#90223,#90224,#90225,#90226,#90227,#90228,#90229,
#90230,#90231,#90232,#90233,#90234,#90235,#90236,#90237,#90238,#90239,#90240,
#90241,#90242,#90243,#90244,#90245,#90246,#90247,#90248,#90249,#90250,#90251,
#90252,#90253,#90254,#90255,#90256,#90257,#90258,#90259,#90260,#90261,#90262,
#90263,#90264,#90265,#90266,#90267,#90268,#90269,#90270,#90271,#90272,#90273,
#90274,#90275,#90276,#90277,#90278,#90279,#90280,#90281,#90282,#90283,#90284,
#90285,#90286,#90287,#90288,#90289,#90290,#90291,#90292,#90293,#90294,#90295,
#90296,#90297,#90298,#90299,#90300,#90301,#90302,#90303,#90304,#90305,#90306,
#90307,#90308,#90309,#90310,#90311,#90312,#90313,#90314,#90315,#90316,#90317,
#90318,#90319,#90320,#90321,#90322,#90323,#90324,#90325,#90326,#90327,#90328,
#90329,#90330,#90331,#90332,#90333,#90334,#90335,#90336,#90337,#90338,#90339,
#90340,#90341,#90342,#90343,#90344,#90345,#90346,#90347,#90348,#90349,#90350,
#90351,#90352,#90353,#90354,#90355,#90356,#90357,#90358,#90359,#90360,#90361,
#90362,#90363,#90364,#90365,#90366,#90367,#90368,#90369,#90370,#90371,#90372,
#90373,#90374,#90375,#90376,#90377,#90378,#90379,#90380,#90381,#90382,#90383,
#90384,#90385,#90386,#90387,#90388,#90389,#90390,#90391,#90392,#90393,#90394,
#90395,#90396,#90397,#90398,#90399,#90400,#90401,#90402,#90403,#90404,#90405));
#94634=CLOSED_SHELL('',(#90406,#90407,#90408,#90409,#90410,#90411,#90412,
#90413,#90414,#90415,#90416,#90417,#90418,#90419,#90420,#90421,#90422,#90423,
#90424,#90425,#90426,#90427,#90428,#90429,#90430,#90431,#90432,#90433,#90434,
#90435,#90436,#90437,#90438,#90439,#90440,#90441,#90442,#90443,#90444,#90445,
#90446,#90447,#90448,#90449,#90450,#90451,#90452,#90453,#90454,#90455,#90456,
#90457,#90458,#90459,#90460,#90461,#90462,#90463,#90464,#90465,#90466,#90467,
#90468,#90469,#90470,#90471,#90472,#90473,#90474,#90475,#90476,#90477,#90478,
#90479,#90480,#90481,#90482,#90483,#90484,#90485,#90486,#90487,#90488,#90489,
#90490,#90491,#90492,#90493,#90494,#90495,#90496,#90497,#90498,#90499,#90500,
#90501,#90502,#90503,#90504,#90505,#90506,#90507,#90508,#90509,#90510,#90511,
#90512,#90513,#90514,#90515,#90516,#90517,#90518,#90519,#90520,#90521,#90522,
#90523,#90524,#90525,#90526,#90527,#90528,#90529,#90530,#90531,#90532,#90533,
#90534,#90535,#90536,#90537,#90538,#90539,#90540,#90541,#90542,#90543,#90544,
#90545,#90546,#90547,#90548,#90549,#90550,#90551,#90552,#90553,#90554,#90555,
#90556,#90557,#90558,#90559,#90560,#90561,#90562,#90563,#90564,#90565,#90566,
#90567,#90568,#90569,#90570,#90571,#90572,#90573,#90574,#90575,#90576,#90577,
#90578,#90579,#90580,#90581,#90582,#90583,#90584));
#94635=CLOSED_SHELL('',(#90585,#90586,#90587,#90588,#90589,#90590,#90591,
#90592,#90593,#90594,#90595,#90596,#90597,#90598,#90599,#90600,#90601,#90602,
#90603,#90604,#90605,#90606,#90607,#90608,#90609,#90610,#90611,#90612,#90613,
#90614,#90615,#90616,#90617,#90618,#90619,#90620,#90621,#90622,#90623,#90624,
#90625,#90626,#90627,#90628,#90629,#90630,#90631,#90632,#90633,#90634,#90635,
#90636,#90637,#90638,#90639,#90640,#90641,#90642,#90643,#90644,#90645,#90646,
#90647,#90648,#90649,#90650,#90651,#90652,#90653,#90654,#90655,#90656,#90657,
#90658,#90659,#90660,#90661,#90662,#90663,#90664,#90665,#90666,#90667,#90668,
#90669,#90670,#90671,#90672,#90673,#90674,#90675,#90676,#90677,#90678,#90679,
#90680,#90681,#90682,#90683,#90684,#90685,#90686,#90687,#90688,#90689,#90690,
#90691,#90692,#90693,#90694,#90695,#90696));
#94636=CLOSED_SHELL('',(#90697,#90698,#90699,#90700,#90701,#90702,#90703,
#90704,#90705,#90706,#90707,#90708,#90709,#90710,#90711,#90712,#90713,#90714,
#90715,#90716,#90717,#90718,#90719,#90720,#90721,#90722,#90723,#90724,#90725,
#90726,#90727,#90728,#90729,#90730,#90731,#90732,#90733,#90734,#90735,#90736));
#94637=CLOSED_SHELL('',(#90737,#90738,#90739,#90740,#90741));
#94638=CLOSED_SHELL('',(#90742,#90743,#90744,#90745,#90746));
#94639=CLOSED_SHELL('',(#90747,#90748,#90749,#90750,#90751));
#94640=CLOSED_SHELL('',(#90752,#90753,#90754,#90755,#90756));
#94641=CLOSED_SHELL('',(#90757,#90758,#90759,#90760,#90761));
#94642=CLOSED_SHELL('',(#90762,#90763,#90764,#90765,#90766));
#94643=CLOSED_SHELL('',(#90767,#90768,#90769,#90770,#90771));
#94644=CLOSED_SHELL('',(#90772,#90773,#90774,#90775,#90776));
#94645=CLOSED_SHELL('',(#90777,#90778,#90779,#90780,#90781,#90782,#90783,
#90784,#90785,#90786,#90787,#90788,#90789,#90790,#90791,#90792,#90793,#90794,
#90795,#90796,#90797,#90798,#90799,#90800,#90801,#90802,#90803,#90804,#90805,
#90806,#90807,#90808,#90809,#90810,#90811,#90812,#90813,#90814,#90815,#90816,
#90817,#90818,#90819,#90820,#90821,#90822,#90823,#90824,#90825,#90826,#90827,
#90828,#90829,#90830,#90831,#90832,#90833,#90834,#90835,#90836,#90837,#90838,
#90839,#90840,#90841,#90842,#90843,#90844,#90845,#90846,#90847,#90848,#90849,
#90850,#90851,#90852,#90853,#90854,#90855,#90856,#90857,#90858,#90859,#90860,
#90861,#90862,#90863));
#94646=CLOSED_SHELL('',(#90864,#90865,#90866,#90867,#90868,#90869,#90870,
#90871));
#94647=CLOSED_SHELL('',(#90872,#90873,#90874,#90875,#90876,#90877,#90878,
#90879));
#94648=CLOSED_SHELL('',(#90880,#90881,#90882,#90883,#90884,#90885,#90886,
#90887));
#94649=CLOSED_SHELL('',(#90888));
#94650=CLOSED_SHELL('',(#90889));
#94651=CLOSED_SHELL('',(#90890));
#94652=CLOSED_SHELL('',(#90891));
#94653=CLOSED_SHELL('',(#90892));
#94654=CLOSED_SHELL('',(#90893));
#94655=CLOSED_SHELL('',(#90894));
#94656=CLOSED_SHELL('',(#90895));
#94657=CLOSED_SHELL('',(#90896));
#94658=CLOSED_SHELL('',(#90897));
#94659=CLOSED_SHELL('',(#90898));
#94660=CLOSED_SHELL('',(#90899));
#94661=CLOSED_SHELL('',(#90900,#90901,#90902,#90903));
#94662=CLOSED_SHELL('',(#90904,#90905,#90906,#90907));
#94663=CLOSED_SHELL('',(#90908,#90909,#90910,#90911,#90912,#90913,#90914,
#90915,#90916,#90917,#90918,#90919,#90920,#90921,#90922,#90923,#90924,#90925,
#90926,#90927,#90928,#90929,#90930,#90931,#90932,#90933,#90934,#90935,#90936,
#90937,#90938,#90939,#90940,#90941,#90942,#90943,#90944,#90945,#90946,#90947,
#90948,#90949,#90950,#90951,#90952,#90953,#90954,#90955,#90956,#90957,#90958,
#90959,#90960,#90961,#90962));
#94664=CLOSED_SHELL('',(#90963,#90964,#90965,#90966,#90967,#90968,#90969,
#90970,#90971,#90972,#90973,#90974,#90975,#90976,#90977,#90978,#90979,#90980,
#90981,#90982,#90983,#90984,#90985,#90986,#90987,#90988,#90989,#90990,#90991,
#90992,#90993,#90994,#90995,#90996,#90997,#90998,#90999,#91000,#91001,#91002,
#91003,#91004,#91005,#91006,#91007,#91008,#91009,#91010,#91011,#91012,#91013,
#91014));
#94665=CLOSED_SHELL('',(#91015,#91016,#91017,#91018,#91019,#91020,#91021,
#91022,#91023,#91024,#91025,#91026,#91027,#91028,#91029,#91030,#91031,#91032,
#91033,#91034,#91035,#91036,#91037,#91038,#91039,#91040,#91041,#91042,#91043,
#91044,#91045,#91046,#91047,#91048,#91049,#91050,#91051,#91052,#91053,#91054,
#91055,#91056,#91057,#91058,#91059,#91060,#91061,#91062,#91063,#91064,#91065,
#91066,#91067,#91068,#91069,#91070,#91071,#91072,#91073,#91074,#91075,#91076,
#91077,#91078,#91079,#91080,#91081,#91082,#91083,#91084,#91085,#91086,#91087,
#91088,#91089,#91090,#91091,#91092,#91093,#91094,#91095,#91096,#91097,#91098,
#91099,#91100,#91101,#91102,#91103,#91104,#91105,#91106,#91107,#91108,#91109,
#91110,#91111,#91112,#91113,#91114,#91115,#91116,#91117,#91118,#91119,#91120,
#91121,#91122,#91123,#91124,#91125,#91126,#91127,#91128,#91129,#91130,#91131,
#91132,#91133,#91134,#91135,#91136,#91137,#91138,#91139,#91140,#91141,#91142,
#91143,#91144,#91145,#91146,#91147,#91148,#91149,#91150,#91151,#91152,#91153,
#91154,#91155,#91156,#91157,#91158,#91159,#91160,#91161,#91162,#91163,#91164,
#91165,#91166,#91167,#91168,#91169,#91170,#91171,#91172,#91173,#91174,#91175,
#91176,#91177,#91178,#91179,#91180,#91181,#91182,#91183,#91184,#91185,#91186,
#91187,#91188,#91189,#91190,#91191,#91192,#91193,#91194,#91195,#91196,#91197,
#91198,#91199,#91200,#91201,#91202,#91203,#91204,#91205,#91206,#91207,#91208,
#91209,#91210,#91211,#91212,#91213,#91214,#91215,#91216,#91217,#91218,#91219,
#91220,#91221,#91222,#91223,#91224,#91225,#91226,#91227,#91228,#91229,#91230,
#91231,#91232,#91233,#91234,#91235,#91236,#91237,#91238,#91239,#91240,#91241,
#91242,#91243,#91244,#91245,#91246,#91247,#91248,#91249,#91250,#91251,#91252,
#91253,#91254,#91255,#91256,#91257,#91258,#91259,#91260,#91261,#91262,#91263,
#91264,#91265,#91266,#91267,#91268,#91269,#91270,#91271,#91272,#91273,#91274,
#91275,#91276,#91277,#91278,#91279,#91280,#91281,#91282,#91283,#91284,#91285,
#91286,#91287,#91288,#91289,#91290,#91291,#91292,#91293,#91294,#91295,#91296,
#91297,#91298,#91299,#91300,#91301,#91302,#91303,#91304,#91305,#91306,#91307,
#91308,#91309,#91310,#91311,#91312,#91313,#91314,#91315,#91316,#91317,#91318,
#91319,#91320,#91321,#91322,#91323,#91324,#91325,#91326,#91327,#91328,#91329,
#91330,#91331,#91332,#91333,#91334,#91335,#91336,#91337,#91338,#91339,#91340,
#91341,#91342,#91343,#91344,#91345,#91346,#91347,#91348,#91349,#91350,#91351,
#91352,#91353,#91354,#91355,#91356,#91357,#91358,#91359,#91360,#91361,#91362,
#91363,#91364,#91365,#91366,#91367,#91368,#91369,#91370,#91371,#91372,#91373,
#91374,#91375,#91376,#91377,#91378,#91379,#91380,#91381,#91382,#91383,#91384,
#91385,#91386,#91387,#91388,#91389,#91390,#91391,#91392,#91393,#91394,#91395,
#91396,#91397,#91398,#91399,#91400,#91401,#91402,#91403,#91404,#91405,#91406,
#91407,#91408,#91409,#91410,#91411,#91412,#91413,#91414,#91415,#91416,#91417,
#91418,#91419,#91420,#91421,#91422,#91423,#91424,#91425,#91426,#91427,#91428,
#91429,#91430,#91431,#91432,#91433,#91434,#91435,#91436,#91437,#91438,#91439,
#91440,#91441,#91442,#91443,#91444,#91445,#91446,#91447,#91448,#91449,#91450,
#91451,#91452,#91453,#91454,#91455,#91456,#91457,#91458,#91459,#91460,#91461,
#91462,#91463,#91464,#91465,#91466,#91467,#91468,#91469,#91470,#91471,#91472,
#91473,#91474,#91475,#91476,#91477,#91478,#91479,#91480,#91481,#91482,#91483,
#91484,#91485,#91486,#91487,#91488,#91489,#91490,#91491,#91492,#91493,#91494,
#91495,#91496,#91497,#91498,#91499,#91500,#91501,#91502,#91503,#91504,#91505,
#91506,#91507,#91508,#91509,#91510,#91511,#91512,#91513,#91514,#91515,#91516,
#91517,#91518,#91519,#91520,#91521,#91522,#91523,#91524,#91525,#91526,#91527,
#91528,#91529,#91530,#91531,#91532,#91533,#91534,#91535,#91536,#91537,#91538,
#91539,#91540,#91541,#91542,#91543,#91544,#91545,#91546,#91547,#91548,#91549,
#91550,#91551,#91552,#91553,#91554,#91555,#91556,#91557,#91558,#91559,#91560,
#91561,#91562,#91563,#91564,#91565,#91566,#91567,#91568,#91569,#91570,#91571,
#91572,#91573,#91574,#91575,#91576,#91577,#91578,#91579,#91580,#91581,#91582,
#91583,#91584,#91585,#91586,#91587,#91588,#91589,#91590,#91591,#91592,#91593,
#91594,#91595,#91596,#91597,#91598,#91599,#91600,#91601,#91602,#91603,#91604,
#91605,#91606,#91607,#91608,#91609,#91610,#91611,#91612,#91613,#91614,#91615,
#91616,#91617,#91618,#91619,#91620,#91621,#91622,#91623,#91624,#91625,#91626,
#91627,#91628,#91629,#91630,#91631,#91632,#91633,#91634,#91635,#91636,#91637,
#91638,#91639,#91640,#91641,#91642,#91643,#91644,#91645,#91646,#91647,#91648,
#91649,#91650,#91651,#91652,#91653,#91654,#91655,#91656,#91657,#91658,#91659,
#91660,#91661,#91662,#91663,#91664,#91665,#91666,#91667,#91668,#91669,#91670,
#91671,#91672,#91673,#91674,#91675,#91676,#91677,#91678,#91679,#91680,#91681,
#91682,#91683,#91684,#91685,#91686,#91687,#91688,#91689,#91690,#91691,#91692,
#91693,#91694,#91695,#91696,#91697,#91698,#91699,#91700,#91701,#91702,#91703,
#91704,#91705,#91706,#91707,#91708,#91709,#91710,#91711,#91712,#91713,#91714,
#91715,#91716,#91717,#91718,#91719,#91720,#91721,#91722,#91723,#91724,#91725,
#91726,#91727,#91728,#91729,#91730,#91731,#91732,#91733,#91734,#91735,#91736,
#91737,#91738,#91739,#91740,#91741,#91742,#91743,#91744,#91745,#91746,#91747,
#91748,#91749,#91750,#91751,#91752,#91753,#91754,#91755,#91756,#91757,#91758,
#91759,#91760,#91761,#91762,#91763,#91764,#91765,#91766,#91767,#91768,#91769,
#91770,#91771,#91772,#91773,#91774,#91775,#91776,#91777,#91778,#91779,#91780,
#91781,#91782,#91783,#91784,#91785,#91786,#91787,#91788,#91789,#91790,#91791,
#91792,#91793,#91794,#91795,#91796,#91797,#91798,#91799,#91800,#91801,#91802,
#91803,#91804,#91805,#91806,#91807,#91808,#91809,#91810,#91811,#91812,#91813,
#91814,#91815,#91816,#91817,#91818,#91819,#91820,#91821,#91822,#91823,#91824,
#91825,#91826,#91827,#91828,#91829,#91830,#91831,#91832,#91833,#91834,#91835,
#91836,#91837,#91838,#91839,#91840,#91841,#91842,#91843,#91844,#91845,#91846,
#91847,#91848,#91849,#91850,#91851,#91852,#91853,#91854,#91855,#91856,#91857,
#91858,#91859,#91860,#91861,#91862,#91863,#91864,#91865,#91866,#91867,#91868,
#91869,#91870,#91871,#91872,#91873,#91874,#91875,#91876,#91877,#91878,#91879,
#91880,#91881,#91882,#91883,#91884,#91885,#91886,#91887,#91888,#91889,#91890,
#91891,#91892,#91893,#91894,#91895,#91896,#91897,#91898,#91899,#91900,#91901,
#91902,#91903,#91904,#91905,#91906,#91907,#91908,#91909,#91910,#91911,#91912,
#91913,#91914,#91915,#91916,#91917,#91918,#91919,#91920,#91921,#91922,#91923,
#91924,#91925,#91926,#91927,#91928,#91929,#91930,#91931,#91932,#91933,#91934,
#91935,#91936,#91937,#91938,#91939,#91940,#91941,#91942,#91943,#91944,#91945,
#91946,#91947,#91948,#91949,#91950,#91951,#91952,#91953,#91954,#91955,#91956,
#91957,#91958,#91959,#91960,#91961,#91962,#91963,#91964,#91965,#91966,#91967,
#91968,#91969,#91970,#91971,#91972,#91973,#91974,#91975,#91976,#91977,#91978,
#91979,#91980,#91981,#91982,#91983,#91984,#91985,#91986,#91987,#91988,#91989,
#91990,#91991,#91992,#91993,#91994,#91995,#91996,#91997,#91998,#91999,#92000,
#92001,#92002,#92003,#92004,#92005,#92006,#92007,#92008,#92009,#92010,#92011,
#92012,#92013,#92014,#92015,#92016,#92017,#92018,#92019,#92020,#92021,#92022,
#92023,#92024,#92025,#92026,#92027,#92028,#92029,#92030,#92031,#92032,#92033,
#92034,#92035,#92036,#92037,#92038,#92039,#92040,#92041,#92042,#92043,#92044,
#92045,#92046,#92047,#92048,#92049,#92050,#92051,#92052,#92053,#92054,#92055,
#92056,#92057,#92058,#92059,#92060,#92061,#92062,#92063,#92064,#92065,#92066,
#92067,#92068,#92069,#92070,#92071,#92072,#92073,#92074,#92075,#92076,#92077,
#92078,#92079,#92080,#92081,#92082,#92083,#92084,#92085,#92086,#92087,#92088,
#92089,#92090,#92091,#92092,#92093,#92094,#92095,#92096,#92097,#92098,#92099,
#92100,#92101,#92102,#92103,#92104,#92105,#92106,#92107,#92108,#92109,#92110,
#92111,#92112,#92113,#92114,#92115,#92116,#92117,#92118,#92119,#92120,#92121,
#92122,#92123,#92124,#92125,#92126,#92127,#92128,#92129,#92130,#92131,#92132,
#92133,#92134,#92135,#92136,#92137,#92138,#92139,#92140,#92141,#92142,#92143,
#92144,#92145,#92146,#92147,#92148,#92149,#92150,#92151,#92152,#92153,#92154,
#92155,#92156,#92157,#92158,#92159,#92160,#92161,#92162,#92163,#92164,#92165,
#92166,#92167,#92168,#92169,#92170,#92171,#92172,#92173,#92174,#92175,#92176,
#92177,#92178,#92179,#92180,#92181,#92182,#92183,#92184,#92185,#92186,#92187,
#92188,#92189,#92190,#92191,#92192,#92193,#92194,#92195,#92196,#92197,#92198,
#92199,#92200,#92201,#92202,#92203,#92204,#92205,#92206,#92207,#92208,#92209,
#92210,#92211,#92212,#92213,#92214,#92215,#92216,#92217,#92218,#92219,#92220,
#92221,#92222,#92223,#92224,#92225,#92226,#92227,#92228,#92229,#92230,#92231,
#92232,#92233,#92234,#92235,#92236,#92237,#92238,#92239,#92240,#92241,#92242,
#92243,#92244,#92245,#92246,#92247,#92248,#92249,#92250,#92251,#92252,#92253,
#92254,#92255,#92256,#92257,#92258,#92259,#92260,#92261,#92262,#92263,#92264,
#92265,#92266,#92267,#92268,#92269,#92270,#92271,#92272,#92273,#92274,#92275,
#92276,#92277,#92278,#92279,#92280,#92281,#92282,#92283,#92284,#92285,#92286,
#92287,#92288,#92289,#92290,#92291,#92292,#92293,#92294,#92295,#92296,#92297,
#92298,#92299,#92300,#92301,#92302,#92303,#92304,#92305,#92306,#92307,#92308,
#92309,#92310,#92311,#92312,#92313,#92314,#92315,#92316,#92317,#92318,#92319,
#92320,#92321,#92322,#92323,#92324,#92325,#92326,#92327,#92328,#92329,#92330,
#92331,#92332,#92333,#92334,#92335,#92336,#92337,#92338,#92339,#92340,#92341,
#92342,#92343,#92344,#92345,#92346,#92347,#92348,#92349,#92350,#92351,#92352,
#92353,#92354,#92355,#92356,#92357,#92358,#92359,#92360,#92361,#92362,#92363,
#92364,#92365,#92366,#92367,#92368,#92369,#92370,#92371,#92372,#92373,#92374,
#92375,#92376,#92377,#92378,#92379,#92380,#92381,#92382,#92383,#92384,#92385,
#92386,#92387,#92388,#92389,#92390,#92391,#92392,#92393,#92394,#92395,#92396,
#92397,#92398,#92399,#92400,#92401,#92402,#92403,#92404,#92405,#92406,#92407,
#92408,#92409,#92410,#92411,#92412,#92413,#92414,#92415,#92416,#92417,#92418,
#92419,#92420,#92421,#92422,#92423,#92424,#92425,#92426,#92427,#92428,#92429,
#92430,#92431,#92432,#92433,#92434,#92435,#92436,#92437,#92438,#92439,#92440,
#92441,#92442,#92443,#92444,#92445,#92446,#92447,#92448,#92449,#92450,#92451,
#92452,#92453,#92454,#92455,#92456,#92457,#92458,#92459,#92460,#92461,#92462,
#92463,#92464,#92465,#92466,#92467,#92468,#92469,#92470,#92471,#92472,#92473,
#92474,#92475,#92476,#92477,#92478,#92479,#92480,#92481,#92482,#92483,#92484,
#92485,#92486,#92487,#92488,#92489,#92490,#92491,#92492,#92493,#92494,#92495,
#92496,#92497,#92498,#92499,#92500,#92501,#92502,#92503,#92504,#92505,#92506,
#92507,#92508,#92509,#92510,#92511,#92512,#92513,#92514,#92515,#92516,#92517,
#92518,#92519,#92520,#92521,#92522,#92523,#92524,#92525,#92526,#92527,#92528,
#92529,#92530,#92531,#92532,#92533,#92534,#92535,#92536,#92537,#92538,#92539,
#92540,#92541,#92542,#92543,#92544,#92545,#92546,#92547,#92548,#92549,#92550,
#92551,#92552,#92553,#92554,#92555,#92556,#92557,#92558,#92559,#92560,#92561,
#92562,#92563,#92564,#92565,#92566,#92567,#92568,#92569,#92570,#92571,#92572,
#92573,#92574,#92575,#92576,#92577,#92578,#92579,#92580,#92581,#92582,#92583,
#92584,#92585,#92586,#92587,#92588,#92589,#92590,#92591,#92592,#92593,#92594,
#92595,#92596,#92597,#92598,#92599,#92600,#92601,#92602,#92603,#92604,#92605,
#92606,#92607,#92608,#92609,#92610,#92611,#92612,#92613,#92614,#92615,#92616,
#92617,#92618,#92619,#92620,#92621,#92622,#92623,#92624,#92625,#92626,#92627,
#92628,#92629,#92630,#92631,#92632,#92633,#92634,#92635,#92636,#92637,#92638,
#92639,#92640,#92641,#92642,#92643,#92644,#92645,#92646,#92647,#92648,#92649,
#92650,#92651,#92652,#92653,#92654,#92655,#92656,#92657,#92658,#92659,#92660,
#92661,#92662,#92663,#92664,#92665,#92666,#92667,#92668,#92669,#92670,#92671,
#92672,#92673,#92674,#92675,#92676,#92677,#92678,#92679,#92680,#92681,#92682,
#92683,#92684,#92685,#92686,#92687,#92688,#92689,#92690,#92691,#92692,#92693,
#92694,#92695,#92696,#92697,#92698,#92699,#92700,#92701,#92702,#92703,#92704,
#92705,#92706,#92707,#92708,#92709,#92710,#92711,#92712,#92713,#92714,#92715,
#92716,#92717,#92718,#92719,#92720,#92721,#92722,#92723,#92724,#92725,#92726,
#92727,#92728,#92729,#92730,#92731,#92732,#92733,#92734,#92735,#92736,#92737,
#92738,#92739,#92740,#92741,#92742,#92743,#92744,#92745,#92746,#92747,#92748,
#92749,#92750,#92751,#92752,#92753,#92754,#92755,#92756,#92757,#92758,#92759,
#92760,#92761,#92762,#92763,#92764,#92765,#92766,#92767,#92768,#92769,#92770,
#92771,#92772,#92773,#92774,#92775,#92776,#92777,#92778,#92779,#92780,#92781,
#92782,#92783,#92784,#92785,#92786,#92787,#92788,#92789,#92790,#92791,#92792,
#92793,#92794,#92795,#92796,#92797,#92798,#92799,#92800,#92801,#92802,#92803,
#92804,#92805,#92806,#92807,#92808,#92809,#92810,#92811,#92812,#92813,#92814,
#92815,#92816,#92817,#92818,#92819,#92820,#92821,#92822,#92823,#92824,#92825,
#92826,#92827,#92828,#92829,#92830,#92831,#92832,#92833,#92834,#92835,#92836,
#92837,#92838,#92839,#92840,#92841,#92842,#92843,#92844,#92845,#92846,#92847,
#92848,#92849,#92850,#92851,#92852,#92853,#92854,#92855,#92856,#92857,#92858,
#92859,#92860,#92861,#92862,#92863,#92864,#92865,#92866,#92867,#92868,#92869,
#92870,#92871,#92872));
#94666=CLOSED_SHELL('',(#92873,#92874,#92875,#92876,#92877,#92878,#92879,
#92880,#92881,#92882,#92883,#92884,#92885,#92886,#92887,#92888,#92889,#92890,
#92891,#92892,#92893,#92894,#92895,#92896,#92897,#92898,#92899,#92900,#92901,
#92902,#92903,#92904,#92905,#92906,#92907,#92908,#92909,#92910,#92911,#92912,
#92913,#92914,#92915,#92916,#92917,#92918,#92919,#92920,#92921,#92922,#92923,
#92924,#92925,#92926,#92927,#92928,#92929,#92930,#92931,#92932,#92933,#92934,
#92935,#92936,#92937,#92938,#92939,#92940,#92941,#92942,#92943,#92944,#92945,
#92946,#92947,#92948,#92949,#92950,#92951,#92952,#92953,#92954,#92955,#92956,
#92957,#92958,#92959,#92960,#92961,#92962,#92963,#92964,#92965,#92966,#92967,
#92968,#92969,#92970,#92971,#92972,#92973,#92974,#92975,#92976,#92977,#92978,
#92979,#92980,#92981,#92982,#92983,#92984,#92985,#92986,#92987,#92988,#92989,
#92990,#92991,#92992,#92993,#92994,#92995,#92996,#92997,#92998,#92999,#93000,
#93001,#93002,#93003,#93004,#93005,#93006,#93007,#93008,#93009,#93010,#93011,
#93012,#93013,#93014,#93015,#93016,#93017,#93018,#93019,#93020,#93021,#93022,
#93023,#93024,#93025,#93026,#93027,#93028,#93029,#93030,#93031,#93032,#93033,
#93034,#93035,#93036,#93037,#93038,#93039,#93040,#93041,#93042,#93043,#93044,
#93045,#93046,#93047,#93048,#93049,#93050,#93051,#93052,#93053,#93054,#93055,
#93056,#93057,#93058,#93059,#93060,#93061,#93062,#93063,#93064,#93065,#93066,
#93067,#93068,#93069,#93070,#93071,#93072,#93073,#93074,#93075,#93076,#93077,
#93078,#93079,#93080,#93081,#93082,#93083,#93084,#93085,#93086,#93087,#93088,
#93089,#93090,#93091,#93092,#93093,#93094,#93095,#93096,#93097,#93098,#93099,
#93100,#93101,#93102,#93103,#93104,#93105,#93106,#93107,#93108,#93109,#93110,
#93111,#93112,#93113,#93114,#93115,#93116,#93117,#93118,#93119,#93120,#93121,
#93122,#93123,#93124,#93125,#93126,#93127,#93128,#93129,#93130,#93131,#93132,
#93133,#93134,#93135,#93136,#93137,#93138,#93139,#93140,#93141,#93142,#93143,
#93144,#93145,#93146,#93147,#93148,#93149,#93150,#93151,#93152,#93153,#93154,
#93155,#93156,#93157,#93158,#93159,#93160,#93161,#93162,#93163,#93164,#93165,
#93166,#93167,#93168,#93169,#93170,#93171,#93172,#93173,#93174,#93175,#93176,
#93177,#93178,#93179,#93180,#93181,#93182,#93183,#93184,#93185,#93186,#93187,
#93188,#93189,#93190,#93191,#93192,#93193,#93194,#93195,#93196,#93197,#93198,
#93199,#93200,#93201,#93202,#93203,#93204,#93205,#93206,#93207,#93208,#93209,
#93210,#93211,#93212,#93213,#93214,#93215,#93216,#93217,#93218,#93219,#93220,
#93221,#93222,#93223,#93224,#93225,#93226,#93227,#93228,#93229,#93230,#93231,
#93232,#93233,#93234,#93235,#93236,#93237,#93238,#93239,#93240,#93241,#93242,
#93243,#93244,#93245,#93246,#93247,#93248,#93249,#93250,#93251,#93252,#93253,
#93254,#93255,#93256,#93257,#93258,#93259,#93260,#93261,#93262,#93263,#93264,
#93265,#93266,#93267,#93268,#93269,#93270,#93271,#93272,#93273,#93274,#93275,
#93276,#93277,#93278,#93279,#93280,#93281,#93282,#93283,#93284,#93285,#93286,
#93287,#93288,#93289,#93290,#93291,#93292,#93293,#93294,#93295,#93296,#93297,
#93298,#93299,#93300,#93301,#93302,#93303,#93304,#93305,#93306,#93307,#93308,
#93309,#93310,#93311,#93312,#93313,#93314,#93315,#93316,#93317,#93318,#93319,
#93320,#93321,#93322,#93323,#93324,#93325,#93326,#93327,#93328,#93329,#93330,
#93331,#93332,#93333,#93334,#93335,#93336,#93337,#93338,#93339,#93340,#93341,
#93342,#93343,#93344,#93345,#93346,#93347,#93348,#93349,#93350,#93351,#93352,
#93353,#93354,#93355,#93356,#93357,#93358,#93359,#93360,#93361,#93362,#93363,
#93364,#93365,#93366,#93367,#93368,#93369,#93370,#93371,#93372,#93373,#93374,
#93375,#93376,#93377,#93378,#93379,#93380,#93381,#93382,#93383,#93384,#93385,
#93386,#93387,#93388,#93389,#93390,#93391,#93392,#93393,#93394,#93395,#93396,
#93397,#93398,#93399,#93400,#93401,#93402,#93403,#93404,#93405,#93406,#93407,
#93408,#93409,#93410,#93411,#93412,#93413,#93414,#93415,#93416,#93417,#93418,
#93419,#93420,#93421,#93422,#93423,#93424,#93425,#93426,#93427,#93428,#93429,
#93430,#93431,#93432,#93433,#93434,#93435,#93436,#93437,#93438,#93439,#93440,
#93441,#93442,#93443,#93444,#93445,#93446,#93447,#93448,#93449,#93450,#93451,
#93452,#93453,#93454,#93455,#93456,#93457,#93458,#93459,#93460,#93461,#93462,
#93463,#93464,#93465,#93466,#93467,#93468,#93469,#93470,#93471,#93472,#93473,
#93474,#93475,#93476,#93477,#93478,#93479,#93480,#93481,#93482,#93483,#93484,
#93485,#93486,#93487,#93488,#93489,#93490,#93491,#93492,#93493,#93494,#93495,
#93496,#93497,#93498,#93499,#93500,#93501,#93502,#93503,#93504,#93505,#93506,
#93507,#93508,#93509,#93510,#93511,#93512,#93513,#93514,#93515,#93516,#93517,
#93518,#93519,#93520,#93521,#93522,#93523,#93524,#93525,#93526,#93527,#93528,
#93529,#93530,#93531,#93532,#93533,#93534,#93535,#93536,#93537,#93538,#93539,
#93540,#93541,#93542,#93543,#93544,#93545,#93546,#93547,#93548,#93549,#93550,
#93551,#93552,#93553,#93554,#93555,#93556,#93557,#93558,#93559,#93560,#93561,
#93562,#93563,#93564,#93565,#93566,#93567,#93568,#93569,#93570,#93571,#93572,
#93573,#93574,#93575,#93576,#93577,#93578,#93579,#93580,#93581,#93582,#93583,
#93584,#93585,#93586,#93587,#93588,#93589,#93590,#93591,#93592,#93593,#93594,
#93595,#93596,#93597,#93598,#93599,#93600,#93601,#93602,#93603,#93604,#93605,
#93606,#93607,#93608,#93609,#93610,#93611,#93612,#93613,#93614,#93615,#93616,
#93617,#93618,#93619,#93620,#93621,#93622,#93623,#93624,#93625,#93626,#93627,
#93628,#93629,#93630,#93631,#93632,#93633,#93634,#93635,#93636,#93637,#93638,
#93639,#93640,#93641,#93642,#93643,#93644,#93645,#93646,#93647,#93648,#93649,
#93650,#93651,#93652,#93653,#93654,#93655,#93656,#93657,#93658,#93659,#93660,
#93661,#93662,#93663,#93664,#93665,#93666,#93667,#93668,#93669,#93670,#93671,
#93672,#93673,#93674,#93675,#93676,#93677,#93678,#93679,#93680,#93681,#93682,
#93683,#93684,#93685,#93686,#93687,#93688,#93689,#93690,#93691,#93692,#93693,
#93694,#93695,#93696,#93697,#93698,#93699,#93700,#93701,#93702,#93703,#93704,
#93705,#93706,#93707,#93708,#93709,#93710,#93711,#93712,#93713,#93714,#93715,
#93716,#93717,#93718,#93719,#93720,#93721,#93722,#93723,#93724,#93725,#93726,
#93727,#93728,#93729,#93730,#93731,#93732,#93733,#93734,#93735,#93736,#93737,
#93738,#93739,#93740,#93741,#93742,#93743,#93744,#93745,#93746,#93747,#93748,
#93749,#93750,#93751,#93752,#93753,#93754,#93755,#93756,#93757,#93758,#93759,
#93760,#93761,#93762,#93763,#93764,#93765,#93766,#93767,#93768,#93769,#93770,
#93771,#93772,#93773,#93774,#93775,#93776,#93777,#93778,#93779,#93780,#93781,
#93782,#93783,#93784,#93785,#93786,#93787,#93788,#93789,#93790,#93791,#93792,
#93793,#93794,#93795,#93796,#93797,#93798,#93799,#93800,#93801,#93802,#93803,
#93804,#93805,#93806,#93807,#93808,#93809,#93810,#93811,#93812,#93813,#93814,
#93815,#93816,#93817,#93818,#93819,#93820,#93821,#93822,#93823,#93824,#93825,
#93826,#93827,#93828,#93829,#93830,#93831,#93832,#93833,#93834,#93835,#93836,
#93837,#93838,#93839,#93840,#93841,#93842,#93843,#93844,#93845,#93846,#93847,
#93848,#93849,#93850,#93851,#93852,#93853,#93854,#93855,#93856,#93857,#93858,
#93859,#93860,#93861,#93862,#93863,#93864,#93865,#93866,#93867,#93868,#93869,
#93870,#93871,#93872,#93873,#93874,#93875,#93876,#93877,#93878,#93879,#93880,
#93881,#93882,#93883,#93884,#93885,#93886,#93887,#93888,#93889,#93890,#93891,
#93892,#93893,#93894,#93895,#93896,#93897,#93898,#93899,#93900,#93901,#93902,
#93903,#93904,#93905,#93906,#93907,#93908,#93909,#93910,#93911,#93912,#93913,
#93914,#93915,#93916,#93917,#93918,#93919,#93920,#93921,#93922,#93923,#93924,
#93925,#93926,#93927,#93928,#93929,#93930,#93931,#93932,#93933,#93934,#93935,
#93936,#93937,#93938,#93939,#93940,#93941,#93942,#93943,#93944,#93945,#93946,
#93947,#93948,#93949,#93950,#93951,#93952,#93953,#93954,#93955,#93956,#93957,
#93958,#93959,#93960,#93961,#93962,#93963,#93964,#93965,#93966,#93967,#93968,
#93969,#93970,#93971,#93972,#93973,#93974,#93975,#93976,#93977,#93978,#93979,
#93980,#93981,#93982,#93983,#93984,#93985,#93986,#93987,#93988,#93989,#93990,
#93991,#93992,#93993,#93994,#93995,#93996,#93997,#93998,#93999,#94000,#94001,
#94002,#94003,#94004,#94005,#94006,#94007,#94008,#94009,#94010,#94011,#94012,
#94013,#94014,#94015,#94016,#94017,#94018,#94019,#94020,#94021,#94022,#94023,
#94024,#94025,#94026,#94027,#94028,#94029,#94030,#94031,#94032,#94033,#94034,
#94035,#94036,#94037,#94038,#94039,#94040,#94041,#94042,#94043,#94044,#94045,
#94046,#94047,#94048,#94049,#94050,#94051,#94052,#94053,#94054,#94055,#94056,
#94057,#94058,#94059,#94060,#94061,#94062,#94063,#94064,#94065,#94066,#94067,
#94068,#94069,#94070,#94071,#94072,#94073,#94074,#94075,#94076,#94077,#94078,
#94079,#94080,#94081,#94082,#94083,#94084,#94085,#94086,#94087,#94088,#94089,
#94090,#94091,#94092,#94093,#94094,#94095,#94096,#94097,#94098,#94099,#94100,
#94101,#94102,#94103,#94104,#94105,#94106,#94107,#94108,#94109,#94110,#94111,
#94112,#94113,#94114,#94115,#94116,#94117,#94118,#94119,#94120,#94121,#94122,
#94123,#94124,#94125,#94126,#94127,#94128,#94129,#94130,#94131,#94132,#94133,
#94134,#94135,#94136,#94137,#94138,#94139,#94140,#94141,#94142,#94143,#94144,
#94145,#94146,#94147,#94148,#94149,#94150,#94151,#94152,#94153,#94154,#94155,
#94156,#94157,#94158,#94159,#94160,#94161,#94162,#94163,#94164,#94165,#94166,
#94167,#94168,#94169,#94170,#94171,#94172,#94173,#94174,#94175,#94176,#94177,
#94178,#94179,#94180,#94181,#94182,#94183,#94184,#94185,#94186,#94187,#94188,
#94189,#94190,#94191,#94192,#94193,#94194,#94195,#94196,#94197,#94198,#94199,
#94200,#94201,#94202,#94203,#94204,#94205,#94206,#94207,#94208,#94209,#94210,
#94211,#94212,#94213,#94214,#94215,#94216,#94217,#94218,#94219,#94220,#94221,
#94222,#94223,#94224,#94225,#94226,#94227,#94228,#94229,#94230,#94231,#94232,
#94233,#94234,#94235,#94236,#94237,#94238,#94239,#94240,#94241,#94242,#94243,
#94244,#94245,#94246,#94247,#94248,#94249,#94250,#94251,#94252,#94253,#94254,
#94255,#94256,#94257,#94258,#94259,#94260,#94261,#94262,#94263,#94264,#94265,
#94266,#94267,#94268,#94269,#94270,#94271,#94272,#94273,#94274,#94275,#94276,
#94277,#94278,#94279,#94280,#94281,#94282,#94283,#94284,#94285,#94286,#94287,
#94288,#94289,#94290,#94291,#94292,#94293,#94294,#94295,#94296,#94297,#94298,
#94299,#94300,#94301,#94302,#94303,#94304,#94305,#94306,#94307,#94308,#94309,
#94310,#94311,#94312,#94313,#94314,#94315,#94316,#94317,#94318,#94319,#94320,
#94321,#94322,#94323,#94324,#94325,#94326,#94327,#94328,#94329,#94330,#94331,
#94332,#94333,#94334,#94335,#94336,#94337,#94338,#94339,#94340,#94341,#94342,
#94343,#94344,#94345,#94346,#94347,#94348,#94349,#94350,#94351,#94352,#94353,
#94354,#94355,#94356,#94357,#94358,#94359,#94360,#94361,#94362,#94363,#94364,
#94365,#94366));
#94667=CLOSED_SHELL('',(#94367,#94368,#94369,#94370,#94371,#94372,#94373,
#94374,#94375,#94376,#94377,#94378,#94379,#94380,#94381,#94382,#94383,#94384,
#94385,#94386,#94387,#94388,#94389,#94390,#94391,#94392,#94393,#94394,#94395,
#94396,#94397,#94398,#94399,#94400,#94401,#94402,#94403,#94404,#94405,#94406,
#94407,#94408,#94409,#94410,#94411,#94412,#94413,#94414,#94415,#94416,#94417,
#94418,#94419,#94420,#94421,#94422,#94423,#94424,#94425,#94426,#94427,#94428,
#94429,#94430,#94431,#94432,#94433,#94434,#94435,#94436,#94437,#94438,#94439,
#94440,#94441,#94442,#94443,#94444,#94445,#94446,#94447,#94448,#94449,#94450,
#94451,#94452,#94453,#94454,#94455,#94456,#94457,#94458,#94459,#94460,#94461,
#94462,#94463,#94464,#94465,#94466,#94467,#94468,#94469,#94470,#94471,#94472,
#94473,#94474,#94475,#94476,#94477,#94478,#94479,#94480,#94481,#94482,#94483,
#94484,#94485,#94486,#94487,#94488,#94489,#94490,#94491,#94492,#94493));
#94668=CLOSED_SHELL('',(#94494,#94495,#94496,#94497,#94498,#94499,#94500,
#94501,#94502,#94503,#94504,#94505,#94506,#94507,#94508,#94509,#94510,#94511,
#94512,#94513,#94514,#94515,#94516,#94517,#94518,#94519,#94520,#94521,#94522,
#94523,#94524,#94525,#94526,#94527,#94528,#94529,#94530,#94531,#94532,#94533,
#94534,#94535,#94536,#94537,#94538,#94539,#94540,#94541,#94542,#94543));
#94669=CLOSED_SHELL('',(#94544,#94545,#94546,#94547));
#94670=CLOSED_SHELL('',(#94548,#94549,#94550,#94551,#94552,#94553,#94554,
#94555,#94556,#94557,#94558,#94559,#94560,#94561,#94562,#94563,#94564,#94565,
#94566,#94567,#94568,#94569,#94570,#94571,#94572,#94573,#94574,#94575,#94576,
#94577,#94578,#94579,#94580,#94581,#94582,#94583));
#94671=CLOSED_SHELL('',(#94584,#94585,#94586,#94587,#94588,#94589,#94590,
#94591,#94592,#94593,#94594,#94595,#94596,#94597,#94598,#94599,#94600,#94601,
#94602,#94603,#94604,#94605,#94606,#94607,#94608,#94609,#94610,#94611,#94612,
#94613,#94614,#94615,#94616,#94617,#94618,#94619,#94620,#94621,#94622));
#94672=DERIVED_UNIT_ELEMENT(#94714,1.);
#94673=DERIVED_UNIT_ELEMENT(#459244,-3.);
#94674=DERIVED_UNIT_ELEMENT(#94714,1.);
#94675=DERIVED_UNIT_ELEMENT(#459244,-3.);
#94676=DERIVED_UNIT_ELEMENT(#94714,1.);
#94677=DERIVED_UNIT_ELEMENT(#459244,-3.);
#94678=DERIVED_UNIT_ELEMENT(#94714,1.);
#94679=DERIVED_UNIT_ELEMENT(#459244,-3.);
#94680=DERIVED_UNIT_ELEMENT(#94714,1.);
#94681=DERIVED_UNIT_ELEMENT(#459244,-3.);
#94682=DERIVED_UNIT_ELEMENT(#94714,1.);
#94683=DERIVED_UNIT_ELEMENT(#459244,-3.);
#94684=DERIVED_UNIT_ELEMENT(#94714,1.);
#94685=DERIVED_UNIT_ELEMENT(#459244,-3.);
#94686=DERIVED_UNIT_ELEMENT(#94714,1.);
#94687=DERIVED_UNIT_ELEMENT(#459244,-3.);
#94688=DERIVED_UNIT_ELEMENT(#94714,1.);
#94689=DERIVED_UNIT_ELEMENT(#459244,-3.);
#94690=DERIVED_UNIT_ELEMENT(#94714,1.);
#94691=DERIVED_UNIT_ELEMENT(#459244,-3.);
#94692=DERIVED_UNIT_ELEMENT(#94714,1.);
#94693=DERIVED_UNIT_ELEMENT(#459244,-3.);
#94694=DERIVED_UNIT_ELEMENT(#94714,1.);
#94695=DERIVED_UNIT_ELEMENT(#459244,-3.);
#94696=DERIVED_UNIT_ELEMENT(#94714,1.);
#94697=DERIVED_UNIT_ELEMENT(#459244,-3.);
#94698=DERIVED_UNIT_ELEMENT(#94714,1.);
#94699=DERIVED_UNIT_ELEMENT(#459244,-3.);
#94700=DERIVED_UNIT_ELEMENT(#94714,1.);
#94701=DERIVED_UNIT_ELEMENT(#459244,-3.);
#94702=DERIVED_UNIT_ELEMENT(#94714,1.);
#94703=DERIVED_UNIT_ELEMENT(#459244,-3.);
#94704=DERIVED_UNIT_ELEMENT(#94714,1.);
#94705=DERIVED_UNIT_ELEMENT(#459244,-3.);
#94706=DERIVED_UNIT_ELEMENT(#94714,1.);
#94707=DERIVED_UNIT_ELEMENT(#459244,-3.);
#94708=DERIVED_UNIT_ELEMENT(#94714,1.);
#94709=DERIVED_UNIT_ELEMENT(#459244,-3.);
#94710=DERIVED_UNIT_ELEMENT(#94714,1.);
#94711=DERIVED_UNIT_ELEMENT(#459244,-3.);
#94712=DERIVED_UNIT_ELEMENT(#94714,1.);
#94713=DERIVED_UNIT_ELEMENT(#459244,-3.);
#94714=(
MASS_UNIT()
NAMED_UNIT(*)
SI_UNIT(.KILO.,.GRAM.)
);
#94715=DERIVED_UNIT((#94672,#94673));
#94716=DERIVED_UNIT((#94674,#94675));
#94717=DERIVED_UNIT((#94676,#94677));
#94718=DERIVED_UNIT((#94678,#94679));
#94719=DERIVED_UNIT((#94680,#94681));
#94720=DERIVED_UNIT((#94682,#94683));
#94721=DERIVED_UNIT((#94684,#94685));
#94722=DERIVED_UNIT((#94686,#94687));
#94723=DERIVED_UNIT((#94688,#94689));
#94724=DERIVED_UNIT((#94690,#94691));
#94725=DERIVED_UNIT((#94692,#94693));
#94726=DERIVED_UNIT((#94694,#94695));
#94727=DERIVED_UNIT((#94696,#94697));
#94728=DERIVED_UNIT((#94698,#94699));
#94729=DERIVED_UNIT((#94700,#94701));
#94730=DERIVED_UNIT((#94702,#94703));
#94731=DERIVED_UNIT((#94704,#94705));
#94732=DERIVED_UNIT((#94706,#94707));
#94733=DERIVED_UNIT((#94708,#94709));
#94734=DERIVED_UNIT((#94710,#94711));
#94735=DERIVED_UNIT((#94712,#94713));
#94736=MEASURE_REPRESENTATION_ITEM('density measure',
POSITIVE_RATIO_MEASURE(7850.),#94715);
#94737=MEASURE_REPRESENTATION_ITEM('density measure',
POSITIVE_RATIO_MEASURE(7850.),#94716);
#94738=MEASURE_REPRESENTATION_ITEM('density measure',
POSITIVE_RATIO_MEASURE(7850.),#94717);
#94739=MEASURE_REPRESENTATION_ITEM('density measure',
POSITIVE_RATIO_MEASURE(7850.),#94718);
#94740=MEASURE_REPRESENTATION_ITEM('density measure',
POSITIVE_RATIO_MEASURE(7850.),#94719);
#94741=MEASURE_REPRESENTATION_ITEM('density measure',
POSITIVE_RATIO_MEASURE(7850.),#94720);
#94742=MEASURE_REPRESENTATION_ITEM('density measure',
POSITIVE_RATIO_MEASURE(7850.),#94721);
#94743=MEASURE_REPRESENTATION_ITEM('density measure',
POSITIVE_RATIO_MEASURE(7850.),#94722);
#94744=MEASURE_REPRESENTATION_ITEM('density measure',
POSITIVE_RATIO_MEASURE(2700.),#94723);
#94745=MEASURE_REPRESENTATION_ITEM('density measure',
POSITIVE_RATIO_MEASURE(7850.),#94724);
#94746=MEASURE_REPRESENTATION_ITEM('density measure',
POSITIVE_RATIO_MEASURE(7850.),#94725);
#94747=MEASURE_REPRESENTATION_ITEM('density measure',
POSITIVE_RATIO_MEASURE(7850.),#94726);
#94748=MEASURE_REPRESENTATION_ITEM('density measure',
POSITIVE_RATIO_MEASURE(7850.),#94727);
#94749=MEASURE_REPRESENTATION_ITEM('density measure',
POSITIVE_RATIO_MEASURE(7850.),#94728);
#94750=MEASURE_REPRESENTATION_ITEM('density measure',
POSITIVE_RATIO_MEASURE(7850.),#94729);
#94751=MEASURE_REPRESENTATION_ITEM('density measure',
POSITIVE_RATIO_MEASURE(7850.),#94730);
#94752=MEASURE_REPRESENTATION_ITEM('density measure',
POSITIVE_RATIO_MEASURE(7850.),#94731);
#94753=MEASURE_REPRESENTATION_ITEM('density measure',
POSITIVE_RATIO_MEASURE(7850.),#94732);
#94754=MEASURE_REPRESENTATION_ITEM('density measure',
POSITIVE_RATIO_MEASURE(7850.),#94733);
#94755=MEASURE_REPRESENTATION_ITEM('density measure',
POSITIVE_RATIO_MEASURE(7850.),#94734);
#94756=MEASURE_REPRESENTATION_ITEM('density measure',
POSITIVE_RATIO_MEASURE(7850.),#94735);
#94757=PROPERTY_DEFINITION_REPRESENTATION(#94862,#94799);
#94758=PROPERTY_DEFINITION_REPRESENTATION(#94863,#94800);
#94759=PROPERTY_DEFINITION_REPRESENTATION(#94864,#94801);
#94760=PROPERTY_DEFINITION_REPRESENTATION(#94865,#94802);
#94761=PROPERTY_DEFINITION_REPRESENTATION(#94866,#94803);
#94762=PROPERTY_DEFINITION_REPRESENTATION(#94867,#94804);
#94763=PROPERTY_DEFINITION_REPRESENTATION(#94868,#94805);
#94764=PROPERTY_DEFINITION_REPRESENTATION(#94869,#94806);
#94765=PROPERTY_DEFINITION_REPRESENTATION(#94870,#94807);
#94766=PROPERTY_DEFINITION_REPRESENTATION(#94871,#94808);
#94767=PROPERTY_DEFINITION_REPRESENTATION(#94872,#94809);
#94768=PROPERTY_DEFINITION_REPRESENTATION(#94873,#94810);
#94769=PROPERTY_DEFINITION_REPRESENTATION(#94874,#94811);
#94770=PROPERTY_DEFINITION_REPRESENTATION(#94875,#94812);
#94771=PROPERTY_DEFINITION_REPRESENTATION(#94876,#94813);
#94772=PROPERTY_DEFINITION_REPRESENTATION(#94877,#94814);
#94773=PROPERTY_DEFINITION_REPRESENTATION(#94878,#94815);
#94774=PROPERTY_DEFINITION_REPRESENTATION(#94879,#94816);
#94775=PROPERTY_DEFINITION_REPRESENTATION(#94880,#94817);
#94776=PROPERTY_DEFINITION_REPRESENTATION(#94881,#94818);
#94777=PROPERTY_DEFINITION_REPRESENTATION(#94882,#94819);
#94778=PROPERTY_DEFINITION_REPRESENTATION(#94883,#94820);
#94779=PROPERTY_DEFINITION_REPRESENTATION(#94884,#94821);
#94780=PROPERTY_DEFINITION_REPRESENTATION(#94885,#94822);
#94781=PROPERTY_DEFINITION_REPRESENTATION(#94886,#94823);
#94782=PROPERTY_DEFINITION_REPRESENTATION(#94887,#94824);
#94783=PROPERTY_DEFINITION_REPRESENTATION(#94888,#94825);
#94784=PROPERTY_DEFINITION_REPRESENTATION(#94889,#94826);
#94785=PROPERTY_DEFINITION_REPRESENTATION(#94890,#94827);
#94786=PROPERTY_DEFINITION_REPRESENTATION(#94891,#94828);
#94787=PROPERTY_DEFINITION_REPRESENTATION(#94892,#94829);
#94788=PROPERTY_DEFINITION_REPRESENTATION(#94893,#94830);
#94789=PROPERTY_DEFINITION_REPRESENTATION(#94894,#94831);
#94790=PROPERTY_DEFINITION_REPRESENTATION(#94895,#94832);
#94791=PROPERTY_DEFINITION_REPRESENTATION(#94896,#94833);
#94792=PROPERTY_DEFINITION_REPRESENTATION(#94897,#94834);
#94793=PROPERTY_DEFINITION_REPRESENTATION(#94898,#94835);
#94794=PROPERTY_DEFINITION_REPRESENTATION(#94899,#94836);
#94795=PROPERTY_DEFINITION_REPRESENTATION(#94900,#94837);
#94796=PROPERTY_DEFINITION_REPRESENTATION(#94901,#94838);
#94797=PROPERTY_DEFINITION_REPRESENTATION(#94902,#94839);
#94798=PROPERTY_DEFINITION_REPRESENTATION(#94903,#94840);
#94799=REPRESENTATION('material name',(#94841),#459219);
#94800=REPRESENTATION('density',(#94736),#459219);
#94801=REPRESENTATION('material name',(#94842),#459220);
#94802=REPRESENTATION('density',(#94737),#459220);
#94803=REPRESENTATION('material name',(#94843),#459221);
#94804=REPRESENTATION('density',(#94738),#459221);
#94805=REPRESENTATION('material name',(#94844),#459222);
#94806=REPRESENTATION('density',(#94739),#459222);
#94807=REPRESENTATION('material name',(#94845),#459223);
#94808=REPRESENTATION('density',(#94740),#459223);
#94809=REPRESENTATION('material name',(#94846),#459224);
#94810=REPRESENTATION('density',(#94741),#459224);
#94811=REPRESENTATION('material name',(#94847),#459225);
#94812=REPRESENTATION('density',(#94742),#459225);
#94813=REPRESENTATION('material name',(#94848),#459226);
#94814=REPRESENTATION('density',(#94743),#459226);
#94815=REPRESENTATION('material name',(#94849),#459227);
#94816=REPRESENTATION('density',(#94744),#459227);
#94817=REPRESENTATION('material name',(#94850),#459229);
#94818=REPRESENTATION('density',(#94745),#459229);
#94819=REPRESENTATION('material name',(#94851),#459230);
#94820=REPRESENTATION('density',(#94746),#459230);
#94821=REPRESENTATION('material name',(#94852),#459231);
#94822=REPRESENTATION('density',(#94747),#459231);
#94823=REPRESENTATION('material name',(#94853),#459232);
#94824=REPRESENTATION('density',(#94748),#459232);
#94825=REPRESENTATION('material name',(#94854),#459233);
#94826=REPRESENTATION('density',(#94749),#459233);
#94827=REPRESENTATION('material name',(#94855),#459234);
#94828=REPRESENTATION('density',(#94750),#459234);
#94829=REPRESENTATION('material name',(#94856),#459235);
#94830=REPRESENTATION('density',(#94751),#459235);
#94831=REPRESENTATION('material name',(#94857),#459237);
#94832=REPRESENTATION('density',(#94752),#459237);
#94833=REPRESENTATION('material name',(#94858),#459238);
#94834=REPRESENTATION('density',(#94753),#459238);
#94835=REPRESENTATION('material name',(#94859),#459239);
#94836=REPRESENTATION('density',(#94754),#459239);
#94837=REPRESENTATION('material name',(#94860),#459240);
#94838=REPRESENTATION('density',(#94755),#459240);
#94839=REPRESENTATION('material name',(#94861),#459241);
#94840=REPRESENTATION('density',(#94756),#459241);
#94841=DESCRIPTIVE_REPRESENTATION_ITEM('Steel','Steel');
#94842=DESCRIPTIVE_REPRESENTATION_ITEM('Steel','Steel');
#94843=DESCRIPTIVE_REPRESENTATION_ITEM('Steel','Steel');
#94844=DESCRIPTIVE_REPRESENTATION_ITEM('Steel','Steel');
#94845=DESCRIPTIVE_REPRESENTATION_ITEM('Steel','Steel');
#94846=DESCRIPTIVE_REPRESENTATION_ITEM('Steel','Steel');
#94847=DESCRIPTIVE_REPRESENTATION_ITEM('Steel','Steel');
#94848=DESCRIPTIVE_REPRESENTATION_ITEM('Steel','Steel');
#94849=DESCRIPTIVE_REPRESENTATION_ITEM('Aluminum 6061 T6 0 Cold Formed',
'Aluminum 6061 T6 0 Cold Formed');
#94850=DESCRIPTIVE_REPRESENTATION_ITEM('Steel','Steel');
#94851=DESCRIPTIVE_REPRESENTATION_ITEM('Steel','Steel');
#94852=DESCRIPTIVE_REPRESENTATION_ITEM('Steel','Steel');
#94853=DESCRIPTIVE_REPRESENTATION_ITEM('Steel','Steel');
#94854=DESCRIPTIVE_REPRESENTATION_ITEM('Steel','Steel');
#94855=DESCRIPTIVE_REPRESENTATION_ITEM('Steel','Steel');
#94856=DESCRIPTIVE_REPRESENTATION_ITEM('Steel','Steel');
#94857=DESCRIPTIVE_REPRESENTATION_ITEM('Steel','Steel');
#94858=DESCRIPTIVE_REPRESENTATION_ITEM('Steel','Steel');
#94859=DESCRIPTIVE_REPRESENTATION_ITEM('Steel','Steel');
#94860=DESCRIPTIVE_REPRESENTATION_ITEM('Steel','Steel');
#94861=DESCRIPTIVE_REPRESENTATION_ITEM('Steel','Steel');
#94862=PROPERTY_DEFINITION('material property','material name',#459356);
#94863=PROPERTY_DEFINITION('material property','density of part',#459356);
#94864=PROPERTY_DEFINITION('material property','material name',#459357);
#94865=PROPERTY_DEFINITION('material property','density of part',#459357);
#94866=PROPERTY_DEFINITION('material property','material name',#459358);
#94867=PROPERTY_DEFINITION('material property','density of part',#459358);
#94868=PROPERTY_DEFINITION('material property','material name',#459359);
#94869=PROPERTY_DEFINITION('material property','density of part',#459359);
#94870=PROPERTY_DEFINITION('material property','material name',#459360);
#94871=PROPERTY_DEFINITION('material property','density of part',#459360);
#94872=PROPERTY_DEFINITION('material property','material name',#459361);
#94873=PROPERTY_DEFINITION('material property','density of part',#459361);
#94874=PROPERTY_DEFINITION('material property','material name',#459362);
#94875=PROPERTY_DEFINITION('material property','density of part',#459362);
#94876=PROPERTY_DEFINITION('material property','material name',#459363);
#94877=PROPERTY_DEFINITION('material property','density of part',#459363);
#94878=PROPERTY_DEFINITION('material property','material name',#459364);
#94879=PROPERTY_DEFINITION('material property','density of part',#459364);
#94880=PROPERTY_DEFINITION('material property','material name',#459366);
#94881=PROPERTY_DEFINITION('material property','density of part',#459366);
#94882=PROPERTY_DEFINITION('material property','material name',#459367);
#94883=PROPERTY_DEFINITION('material property','density of part',#459367);
#94884=PROPERTY_DEFINITION('material property','material name',#459368);
#94885=PROPERTY_DEFINITION('material property','density of part',#459368);
#94886=PROPERTY_DEFINITION('material property','material name',#459369);
#94887=PROPERTY_DEFINITION('material property','density of part',#459369);
#94888=PROPERTY_DEFINITION('material property','material name',#459370);
#94889=PROPERTY_DEFINITION('material property','density of part',#459370);
#94890=PROPERTY_DEFINITION('material property','material name',#459371);
#94891=PROPERTY_DEFINITION('material property','density of part',#459371);
#94892=PROPERTY_DEFINITION('material property','material name',#459372);
#94893=PROPERTY_DEFINITION('material property','density of part',#459372);
#94894=PROPERTY_DEFINITION('material property','material name',#459374);
#94895=PROPERTY_DEFINITION('material property','density of part',#459374);
#94896=PROPERTY_DEFINITION('material property','material name',#459375);
#94897=PROPERTY_DEFINITION('material property','density of part',#459375);
#94898=PROPERTY_DEFINITION('material property','material name',#459376);
#94899=PROPERTY_DEFINITION('material property','density of part',#459376);
#94900=PROPERTY_DEFINITION('material property','material name',#459377);
#94901=PROPERTY_DEFINITION('material property','density of part',#459377);
#94902=PROPERTY_DEFINITION('material property','material name',#459378);
#94903=PROPERTY_DEFINITION('material property','density of part',#459378);
#94904=AXIS2_PLACEMENT_3D('',#130719,#105575,#105576);
#94905=AXIS2_PLACEMENT_3D('',#130720,#105577,#105578);
#94906=AXIS2_PLACEMENT_3D('',#130721,#105579,#105580);
#94907=AXIS2_PLACEMENT_3D('',#130722,#105581,#105582);
#94908=AXIS2_PLACEMENT_3D('',#130818,#105584,#105585);
#94909=AXIS2_PLACEMENT_3D('',#130903,#105586,#105587);
#94910=AXIS2_PLACEMENT_3D('',#131279,#105589,#105590);
#94911=AXIS2_PLACEMENT_3D('',#131637,#105592,#105593);
#94912=AXIS2_PLACEMENT_3D('',#131685,#105595,#105596);
#94913=AXIS2_PLACEMENT_3D('',#131810,#105597,#105598);
#94914=AXIS2_PLACEMENT_3D('',#131906,#105600,#105601);
#94915=AXIS2_PLACEMENT_3D('',#131993,#105602,#105603);
#94916=AXIS2_PLACEMENT_3D('',#132365,#105605,#105606);
#94917=AXIS2_PLACEMENT_3D('',#132723,#105608,#105609);
#94918=AXIS2_PLACEMENT_3D('',#132769,#105611,#105612);
#94919=AXIS2_PLACEMENT_3D('',#132894,#105613,#105614);
#94920=AXIS2_PLACEMENT_3D('',#132952,#105616,#105617);
#94921=AXIS2_PLACEMENT_3D('',#133011,#105618,#105619);
#94922=AXIS2_PLACEMENT_3D('',#133305,#105621,#105622);
#94923=AXIS2_PLACEMENT_3D('',#133658,#105624,#105625);
#94924=AXIS2_PLACEMENT_3D('',#133756,#105627,#105628);
#94925=AXIS2_PLACEMENT_3D('',#133849,#105629,#105630);
#94926=AXIS2_PLACEMENT_3D('',#133907,#105632,#105633);
#94927=AXIS2_PLACEMENT_3D('',#133968,#105634,#105635);
#94928=AXIS2_PLACEMENT_3D('',#134264,#105637,#105638);
#94929=AXIS2_PLACEMENT_3D('',#134617,#105640,#105641);
#94930=AXIS2_PLACEMENT_3D('',#134715,#105643,#105644);
#94931=AXIS2_PLACEMENT_3D('',#134808,#105645,#105646);
#94932=AXIS2_PLACEMENT_3D('',#135097,#105647,#105648);
#94933=AXIS2_PLACEMENT_3D('',#135386,#105649,#105650);
#94934=AXIS2_PLACEMENT_3D('',#135751,#105651,#105652);
#94935=AXIS2_PLACEMENT_3D('',#136626,#105653,#105654);
#94936=AXIS2_PLACEMENT_3D('',#136629,#105655,#105656);
#94937=AXIS2_PLACEMENT_3D('',#136633,#105658,#105659);
#94938=AXIS2_PLACEMENT_3D('',#136637,#105661,#105662);
#94939=AXIS2_PLACEMENT_3D('',#136638,#105663,#105664);
#94940=AXIS2_PLACEMENT_3D('',#137146,#105665,#105666);
#94941=AXIS2_PLACEMENT_3D('',#137149,#105667,#105668);
#94942=AXIS2_PLACEMENT_3D('',#137153,#105670,#105671);
#94943=AXIS2_PLACEMENT_3D('',#137157,#105673,#105674);
#94944=AXIS2_PLACEMENT_3D('',#137159,#105675,#105676);
#94945=AXIS2_PLACEMENT_3D('',#137160,#105677,#105678);
#94946=AXIS2_PLACEMENT_3D('',#137161,#105679,#105680);
#94947=AXIS2_PLACEMENT_3D('',#137163,#105681,#105682);
#94948=AXIS2_PLACEMENT_3D('',#137166,#105684,#105685);
#94949=AXIS2_PLACEMENT_3D('',#137167,#105686,#105687);
#94950=AXIS2_PLACEMENT_3D('',#137170,#105689,#105690);
#94951=AXIS2_PLACEMENT_3D('',#137171,#105691,#105692);
#94952=AXIS2_PLACEMENT_3D('',#137173,#105693,#105694);
#94953=AXIS2_PLACEMENT_3D('',#137174,#105695,#105696);
#94954=AXIS2_PLACEMENT_3D('',#137177,#105697,#105698);
#94955=AXIS2_PLACEMENT_3D('',#137180,#105700,#105701);
#94956=AXIS2_PLACEMENT_3D('',#137181,#105702,#105703);
#94957=AXIS2_PLACEMENT_3D('',#137182,#105704,#105705);
#94958=AXIS2_PLACEMENT_3D('',#137192,#105708,#105709);
#94959=AXIS2_PLACEMENT_3D('',#137207,#105712,#105713);
#94960=AXIS2_PLACEMENT_3D('',#137214,#105715,#105716);
#94961=AXIS2_PLACEMENT_3D('',#137216,#105717,#105718);
#94962=AXIS2_PLACEMENT_3D('',#137217,#105719,#105720);
#94963=AXIS2_PLACEMENT_3D('',#137220,#105721,#105722);
#94964=AXIS2_PLACEMENT_3D('',#137223,#105724,#105725);
#94965=AXIS2_PLACEMENT_3D('',#137224,#105726,#105727);
#94966=AXIS2_PLACEMENT_3D('',#137225,#105728,#105729);
#94967=AXIS2_PLACEMENT_3D('',#137227,#105730,#105731);
#94968=AXIS2_PLACEMENT_3D('',#137229,#105733,#105734);
#94969=AXIS2_PLACEMENT_3D('',#137231,#105735,#105736);
#94970=AXIS2_PLACEMENT_3D('',#137232,#105737,#105738);
#94971=AXIS2_PLACEMENT_3D('',#137234,#105739,#105740);
#94972=AXIS2_PLACEMENT_3D('',#137237,#105742,#105743);
#94973=AXIS2_PLACEMENT_3D('',#137238,#105744,#105745);
#94974=AXIS2_PLACEMENT_3D('',#137240,#105746,#105747);
#94975=AXIS2_PLACEMENT_3D('',#137241,#105748,#105749);
#94976=AXIS2_PLACEMENT_3D('',#137244,#105751,#105752);
#94977=AXIS2_PLACEMENT_3D('',#137245,#105753,#105754);
#94978=AXIS2_PLACEMENT_3D('',#137247,#105756,#105757);
#94979=AXIS2_PLACEMENT_3D('',#137250,#105759,#105760);
#94980=AXIS2_PLACEMENT_3D('',#137251,#105761,#105762);
#94981=AXIS2_PLACEMENT_3D('',#137255,#105765,#105766);
#94982=AXIS2_PLACEMENT_3D('',#137258,#105768,#105769);
#94983=AXIS2_PLACEMENT_3D('',#137259,#105770,#105771);
#94984=AXIS2_PLACEMENT_3D('',#137263,#105774,#105775);
#94985=AXIS2_PLACEMENT_3D('',#137264,#105776,#105777);
#94986=AXIS2_PLACEMENT_3D('',#137265,#105778,#105779);
#94987=AXIS2_PLACEMENT_3D('',#137268,#105781,#105782);
#94988=AXIS2_PLACEMENT_3D('',#137269,#105783,#105784);
#94989=AXIS2_PLACEMENT_3D('',#137273,#105787,#105788);
#94990=AXIS2_PLACEMENT_3D('',#137276,#105790,#105791);
#94991=AXIS2_PLACEMENT_3D('',#137277,#105792,#105793);
#94992=AXIS2_PLACEMENT_3D('',#137281,#105796,#105797);
#94993=AXIS2_PLACEMENT_3D('',#137282,#105798,#105799);
#94994=AXIS2_PLACEMENT_3D('',#137283,#105800,#105801);
#94995=AXIS2_PLACEMENT_3D('',#137292,#105806,#105807);
#94996=AXIS2_PLACEMENT_3D('',#137296,#105809,#105810);
#94997=AXIS2_PLACEMENT_3D('',#137297,#105811,#105812);
#94998=AXIS2_PLACEMENT_3D('',#137298,#105813,#105814);
#94999=AXIS2_PLACEMENT_3D('',#137304,#105818,#105819);
#95000=AXIS2_PLACEMENT_3D('',#137307,#105821,#105822);
#95001=AXIS2_PLACEMENT_3D('',#137308,#105823,#105824);
#95002=AXIS2_PLACEMENT_3D('',#137309,#105825,#105826);
#95003=AXIS2_PLACEMENT_3D('',#137312,#105828,#105829);
#95004=AXIS2_PLACEMENT_3D('',#137313,#105830,#105831);
#95005=AXIS2_PLACEMENT_3D('',#137317,#105833,#105834);
#95006=AXIS2_PLACEMENT_3D('',#137318,#105835,#105836);
#95007=AXIS2_PLACEMENT_3D('',#137319,#105837,#105838);
#95008=AXIS2_PLACEMENT_3D('',#137325,#105842,#105843);
#95009=AXIS2_PLACEMENT_3D('',#137329,#105845,#105846);
#95010=AXIS2_PLACEMENT_3D('',#137330,#105847,#105848);
#95011=AXIS2_PLACEMENT_3D('',#137331,#105849,#105850);
#95012=AXIS2_PLACEMENT_3D('',#137337,#105854,#105855);
#95013=AXIS2_PLACEMENT_3D('',#137340,#105857,#105858);
#95014=AXIS2_PLACEMENT_3D('',#137341,#105859,#105860);
#95015=AXIS2_PLACEMENT_3D('',#137342,#105861,#105862);
#95016=AXIS2_PLACEMENT_3D('',#137345,#105864,#105865);
#95017=AXIS2_PLACEMENT_3D('',#137346,#105866,#105867);
#95018=AXIS2_PLACEMENT_3D('',#137347,#105868,#105869);
#95019=AXIS2_PLACEMENT_3D('',#137348,#105870,#105871);
#95020=AXIS2_PLACEMENT_3D('',#137349,#105872,#105873);
#95021=AXIS2_PLACEMENT_3D('',#137352,#105876,#105877);
#95022=AXIS2_PLACEMENT_3D('',#137354,#105879,#105880);
#95023=AXIS2_PLACEMENT_3D('',#137355,#105881,#105882);
#95024=AXIS2_PLACEMENT_3D('',#137357,#105884,#105885);
#95025=AXIS2_PLACEMENT_3D('',#137359,#105887,#105888);
#95026=AXIS2_PLACEMENT_3D('',#137360,#105889,#105890);
#95027=AXIS2_PLACEMENT_3D('',#137362,#105892,#105893);
#95028=AXIS2_PLACEMENT_3D('',#137364,#105895,#105896);
#95029=AXIS2_PLACEMENT_3D('',#137366,#105898,#105899);
#95030=AXIS2_PLACEMENT_3D('',#137368,#105900,#105901);
#95031=AXIS2_PLACEMENT_3D('',#137371,#105903,#105904);
#95032=AXIS2_PLACEMENT_3D('',#137372,#105905,#105906);
#95033=AXIS2_PLACEMENT_3D('',#137375,#105908,#105909);
#95034=AXIS2_PLACEMENT_3D('',#137376,#105910,#105911);
#95035=AXIS2_PLACEMENT_3D('',#137379,#105912,#105913);
#95036=AXIS2_PLACEMENT_3D('',#137390,#105915,#105916);
#95037=AXIS2_PLACEMENT_3D('',#137401,#105918,#105919);
#95038=AXIS2_PLACEMENT_3D('',#137412,#105921,#105922);
#95039=AXIS2_PLACEMENT_3D('',#137423,#105924,#105925);
#95040=AXIS2_PLACEMENT_3D('',#137434,#105927,#105928);
#95041=AXIS2_PLACEMENT_3D('',#137445,#105930,#105931);
#95042=AXIS2_PLACEMENT_3D('',#137456,#105933,#105934);
#95043=AXIS2_PLACEMENT_3D('',#137467,#105936,#105937);
#95044=AXIS2_PLACEMENT_3D('',#137478,#105939,#105940);
#95045=AXIS2_PLACEMENT_3D('',#137489,#105942,#105943);
#95046=AXIS2_PLACEMENT_3D('',#137500,#105945,#105946);
#95047=AXIS2_PLACEMENT_3D('',#137511,#105948,#105949);
#95048=AXIS2_PLACEMENT_3D('',#137522,#105951,#105952);
#95049=AXIS2_PLACEMENT_3D('',#137533,#105954,#105955);
#95050=AXIS2_PLACEMENT_3D('',#137544,#105957,#105958);
#95051=AXIS2_PLACEMENT_3D('',#137555,#105960,#105961);
#95052=AXIS2_PLACEMENT_3D('',#137566,#105963,#105964);
#95053=AXIS2_PLACEMENT_3D('',#137577,#105966,#105967);
#95054=AXIS2_PLACEMENT_3D('',#137588,#105969,#105970);
#95055=AXIS2_PLACEMENT_3D('',#137597,#105972,#105973);
#95056=AXIS2_PLACEMENT_3D('',#137598,#105974,#105975);
#95057=AXIS2_PLACEMENT_3D('',#137601,#105976,#105977);
#95058=AXIS2_PLACEMENT_3D('',#137612,#105979,#105980);
#95059=AXIS2_PLACEMENT_3D('',#137623,#105982,#105983);
#95060=AXIS2_PLACEMENT_3D('',#137634,#105985,#105986);
#95061=AXIS2_PLACEMENT_3D('',#137645,#105988,#105989);
#95062=AXIS2_PLACEMENT_3D('',#137656,#105991,#105992);
#95063=AXIS2_PLACEMENT_3D('',#137667,#105994,#105995);
#95064=AXIS2_PLACEMENT_3D('',#137678,#105997,#105998);
#95065=AXIS2_PLACEMENT_3D('',#137689,#106000,#106001);
#95066=AXIS2_PLACEMENT_3D('',#137700,#106003,#106004);
#95067=AXIS2_PLACEMENT_3D('',#137711,#106006,#106007);
#95068=AXIS2_PLACEMENT_3D('',#137722,#106009,#106010);
#95069=AXIS2_PLACEMENT_3D('',#137733,#106012,#106013);
#95070=AXIS2_PLACEMENT_3D('',#137744,#106015,#106016);
#95071=AXIS2_PLACEMENT_3D('',#137755,#106018,#106019);
#95072=AXIS2_PLACEMENT_3D('',#137766,#106021,#106022);
#95073=AXIS2_PLACEMENT_3D('',#137777,#106024,#106025);
#95074=AXIS2_PLACEMENT_3D('',#137788,#106027,#106028);
#95075=AXIS2_PLACEMENT_3D('',#137799,#106030,#106031);
#95076=AXIS2_PLACEMENT_3D('',#137810,#106033,#106034);
#95077=AXIS2_PLACEMENT_3D('',#137820,#106036,#106037);
#95078=AXIS2_PLACEMENT_3D('',#137821,#106038,#106039);
#95079=AXIS2_PLACEMENT_3D('',#137837,#106043,#106044);
#95080=AXIS2_PLACEMENT_3D('',#137852,#106047,#106048);
#95081=AXIS2_PLACEMENT_3D('',#137854,#106050,#106051);
#95082=AXIS2_PLACEMENT_3D('',#137856,#106053,#106054);
#95083=AXIS2_PLACEMENT_3D('',#137858,#106056,#106057);
#95084=AXIS2_PLACEMENT_3D('',#137874,#106061,#106062);
#95085=AXIS2_PLACEMENT_3D('',#137889,#106065,#106066);
#95086=AXIS2_PLACEMENT_3D('',#137890,#106067,#106068);
#95087=AXIS2_PLACEMENT_3D('',#137892,#106070,#106071);
#95088=AXIS2_PLACEMENT_3D('',#137908,#106075,#106076);
#95089=AXIS2_PLACEMENT_3D('',#137923,#106079,#106080);
#95090=AXIS2_PLACEMENT_3D('',#137924,#106081,#106082);
#95091=AXIS2_PLACEMENT_3D('',#137926,#106084,#106085);
#95092=AXIS2_PLACEMENT_3D('',#137942,#106089,#106090);
#95093=AXIS2_PLACEMENT_3D('',#137957,#106093,#106094);
#95094=AXIS2_PLACEMENT_3D('',#137958,#106095,#106096);
#95095=AXIS2_PLACEMENT_3D('',#137960,#106098,#106099);
#95096=AXIS2_PLACEMENT_3D('',#137976,#106103,#106104);
#95097=AXIS2_PLACEMENT_3D('',#137991,#106107,#106108);
#95098=AXIS2_PLACEMENT_3D('',#137992,#106109,#106110);
#95099=AXIS2_PLACEMENT_3D('',#137994,#106112,#106113);
#95100=AXIS2_PLACEMENT_3D('',#138010,#106117,#106118);
#95101=AXIS2_PLACEMENT_3D('',#138025,#106121,#106122);
#95102=AXIS2_PLACEMENT_3D('',#138026,#106123,#106124);
#95103=AXIS2_PLACEMENT_3D('',#138028,#106126,#106127);
#95104=AXIS2_PLACEMENT_3D('',#138044,#106131,#106132);
#95105=AXIS2_PLACEMENT_3D('',#138059,#106135,#106136);
#95106=AXIS2_PLACEMENT_3D('',#138060,#106137,#106138);
#95107=AXIS2_PLACEMENT_3D('',#138062,#106140,#106141);
#95108=AXIS2_PLACEMENT_3D('',#138078,#106145,#106146);
#95109=AXIS2_PLACEMENT_3D('',#138093,#106149,#106150);
#95110=AXIS2_PLACEMENT_3D('',#138094,#106151,#106152);
#95111=AXIS2_PLACEMENT_3D('',#138096,#106154,#106155);
#95112=AXIS2_PLACEMENT_3D('',#138112,#106159,#106160);
#95113=AXIS2_PLACEMENT_3D('',#138127,#106163,#106164);
#95114=AXIS2_PLACEMENT_3D('',#138128,#106165,#106166);
#95115=AXIS2_PLACEMENT_3D('',#138130,#106168,#106169);
#95116=AXIS2_PLACEMENT_3D('',#138145,#106172,#106173);
#95117=AXIS2_PLACEMENT_3D('',#138160,#106176,#106177);
#95118=AXIS2_PLACEMENT_3D('',#138161,#106178,#106179);
#95119=AXIS2_PLACEMENT_3D('',#138164,#106180,#106181);
#95120=AXIS2_PLACEMENT_3D('',#138167,#106183,#106184);
#95121=AXIS2_PLACEMENT_3D('',#138168,#106185,#106186);
#95122=AXIS2_PLACEMENT_3D('',#138169,#106187,#106188);
#95123=AXIS2_PLACEMENT_3D('',#138172,#106189,#106190);
#95124=AXIS2_PLACEMENT_3D('',#138174,#106192,#106193);
#95125=AXIS2_PLACEMENT_3D('',#138175,#106194,#106195);
#95126=AXIS2_PLACEMENT_3D('',#138179,#106197,#106198);
#95127=AXIS2_PLACEMENT_3D('',#138180,#106199,#106200);
#95128=AXIS2_PLACEMENT_3D('',#138181,#106201,#106202);
#95129=AXIS2_PLACEMENT_3D('',#138183,#106204,#106205);
#95130=AXIS2_PLACEMENT_3D('',#138186,#106206,#106207);
#95131=AXIS2_PLACEMENT_3D('',#138189,#106209,#106210);
#95132=AXIS2_PLACEMENT_3D('',#138190,#106211,#106212);
#95133=AXIS2_PLACEMENT_3D('',#138191,#106213,#106214);
#95134=AXIS2_PLACEMENT_3D('',#138193,#106216,#106217);
#95135=AXIS2_PLACEMENT_3D('',#138197,#106219,#106220);
#95136=AXIS2_PLACEMENT_3D('',#138198,#106221,#106222);
#95137=AXIS2_PLACEMENT_3D('',#138199,#106223,#106224);
#95138=AXIS2_PLACEMENT_3D('',#138202,#106225,#106226);
#95139=AXIS2_PLACEMENT_3D('',#138205,#106228,#106229);
#95140=AXIS2_PLACEMENT_3D('',#138206,#106230,#106231);
#95141=AXIS2_PLACEMENT_3D('',#138207,#106232,#106233);
#95142=AXIS2_PLACEMENT_3D('',#138209,#106235,#106236);
#95143=AXIS2_PLACEMENT_3D('',#138213,#106238,#106239);
#95144=AXIS2_PLACEMENT_3D('',#138214,#106240,#106241);
#95145=AXIS2_PLACEMENT_3D('',#138215,#106242,#106243);
#95146=AXIS2_PLACEMENT_3D('',#138218,#106244,#106245);
#95147=AXIS2_PLACEMENT_3D('',#138221,#106247,#106248);
#95148=AXIS2_PLACEMENT_3D('',#138222,#106249,#106250);
#95149=AXIS2_PLACEMENT_3D('',#138223,#106251,#106252);
#95150=AXIS2_PLACEMENT_3D('',#138225,#106254,#106255);
#95151=AXIS2_PLACEMENT_3D('',#138229,#106257,#106258);
#95152=AXIS2_PLACEMENT_3D('',#138230,#106259,#106260);
#95153=AXIS2_PLACEMENT_3D('',#138231,#106261,#106262);
#95154=AXIS2_PLACEMENT_3D('',#138234,#106263,#106264);
#95155=AXIS2_PLACEMENT_3D('',#138237,#106266,#106267);
#95156=AXIS2_PLACEMENT_3D('',#138238,#106268,#106269);
#95157=AXIS2_PLACEMENT_3D('',#138239,#106270,#106271);
#95158=AXIS2_PLACEMENT_3D('',#138241,#106273,#106274);
#95159=AXIS2_PLACEMENT_3D('',#138245,#106276,#106277);
#95160=AXIS2_PLACEMENT_3D('',#138246,#106278,#106279);
#95161=AXIS2_PLACEMENT_3D('',#138247,#106280,#106281);
#95162=AXIS2_PLACEMENT_3D('',#138250,#106282,#106283);
#95163=AXIS2_PLACEMENT_3D('',#138253,#106285,#106286);
#95164=AXIS2_PLACEMENT_3D('',#138254,#106287,#106288);
#95165=AXIS2_PLACEMENT_3D('',#138255,#106289,#106290);
#95166=AXIS2_PLACEMENT_3D('',#138257,#106292,#106293);
#95167=AXIS2_PLACEMENT_3D('',#138261,#106295,#106296);
#95168=AXIS2_PLACEMENT_3D('',#138262,#106297,#106298);
#95169=AXIS2_PLACEMENT_3D('',#138263,#106299,#106300);
#95170=AXIS2_PLACEMENT_3D('',#138266,#106301,#106302);
#95171=AXIS2_PLACEMENT_3D('',#138269,#106304,#106305);
#95172=AXIS2_PLACEMENT_3D('',#138270,#106306,#106307);
#95173=AXIS2_PLACEMENT_3D('',#138271,#106308,#106309);
#95174=AXIS2_PLACEMENT_3D('',#138273,#106311,#106312);
#95175=AXIS2_PLACEMENT_3D('',#138277,#106314,#106315);
#95176=AXIS2_PLACEMENT_3D('',#138278,#106316,#106317);
#95177=AXIS2_PLACEMENT_3D('',#138279,#106318,#106319);
#95178=AXIS2_PLACEMENT_3D('',#138282,#106320,#106321);
#95179=AXIS2_PLACEMENT_3D('',#138285,#106323,#106324);
#95180=AXIS2_PLACEMENT_3D('',#138286,#106325,#106326);
#95181=AXIS2_PLACEMENT_3D('',#138287,#106327,#106328);
#95182=AXIS2_PLACEMENT_3D('',#138289,#106330,#106331);
#95183=AXIS2_PLACEMENT_3D('',#138293,#106333,#106334);
#95184=AXIS2_PLACEMENT_3D('',#138294,#106335,#106336);
#95185=AXIS2_PLACEMENT_3D('',#138295,#106337,#106338);
#95186=AXIS2_PLACEMENT_3D('',#138298,#106339,#106340);
#95187=AXIS2_PLACEMENT_3D('',#138301,#106342,#106343);
#95188=AXIS2_PLACEMENT_3D('',#138302,#106344,#106345);
#95189=AXIS2_PLACEMENT_3D('',#138303,#106346,#106347);
#95190=AXIS2_PLACEMENT_3D('',#138305,#106349,#106350);
#95191=AXIS2_PLACEMENT_3D('',#138309,#106352,#106353);
#95192=AXIS2_PLACEMENT_3D('',#138310,#106354,#106355);
#95193=AXIS2_PLACEMENT_3D('',#138311,#106356,#106357);
#95194=AXIS2_PLACEMENT_3D('',#138314,#106358,#106359);
#95195=AXIS2_PLACEMENT_3D('',#138317,#106361,#106362);
#95196=AXIS2_PLACEMENT_3D('',#138318,#106363,#106364);
#95197=AXIS2_PLACEMENT_3D('',#138319,#106365,#106366);
#95198=AXIS2_PLACEMENT_3D('',#138321,#106368,#106369);
#95199=AXIS2_PLACEMENT_3D('',#138325,#106371,#106372);
#95200=AXIS2_PLACEMENT_3D('',#138326,#106373,#106374);
#95201=AXIS2_PLACEMENT_3D('',#138327,#106375,#106376);
#95202=AXIS2_PLACEMENT_3D('',#138330,#106377,#106378);
#95203=AXIS2_PLACEMENT_3D('',#138333,#106380,#106381);
#95204=AXIS2_PLACEMENT_3D('',#138334,#106382,#106383);
#95205=AXIS2_PLACEMENT_3D('',#138335,#106384,#106385);
#95206=AXIS2_PLACEMENT_3D('',#138337,#106387,#106388);
#95207=AXIS2_PLACEMENT_3D('',#138341,#106390,#106391);
#95208=AXIS2_PLACEMENT_3D('',#138342,#106392,#106393);
#95209=AXIS2_PLACEMENT_3D('',#138343,#106394,#106395);
#95210=AXIS2_PLACEMENT_3D('',#138346,#106396,#106397);
#95211=AXIS2_PLACEMENT_3D('',#138349,#106399,#106400);
#95212=AXIS2_PLACEMENT_3D('',#138350,#106401,#106402);
#95213=AXIS2_PLACEMENT_3D('',#138351,#106403,#106404);
#95214=AXIS2_PLACEMENT_3D('',#138353,#106406,#106407);
#95215=AXIS2_PLACEMENT_3D('',#138357,#106409,#106410);
#95216=AXIS2_PLACEMENT_3D('',#138358,#106411,#106412);
#95217=AXIS2_PLACEMENT_3D('',#138359,#106413,#106414);
#95218=AXIS2_PLACEMENT_3D('',#138362,#106415,#106416);
#95219=AXIS2_PLACEMENT_3D('',#138365,#106418,#106419);
#95220=AXIS2_PLACEMENT_3D('',#138366,#106420,#106421);
#95221=AXIS2_PLACEMENT_3D('',#138367,#106422,#106423);
#95222=AXIS2_PLACEMENT_3D('',#138369,#106425,#106426);
#95223=AXIS2_PLACEMENT_3D('',#138373,#106428,#106429);
#95224=AXIS2_PLACEMENT_3D('',#138374,#106430,#106431);
#95225=AXIS2_PLACEMENT_3D('',#138375,#106432,#106433);
#95226=AXIS2_PLACEMENT_3D('',#138378,#106434,#106435);
#95227=AXIS2_PLACEMENT_3D('',#138381,#106437,#106438);
#95228=AXIS2_PLACEMENT_3D('',#138382,#106439,#106440);
#95229=AXIS2_PLACEMENT_3D('',#138383,#106441,#106442);
#95230=AXIS2_PLACEMENT_3D('',#138385,#106444,#106445);
#95231=AXIS2_PLACEMENT_3D('',#138386,#106446,#106447);
#95232=AXIS2_PLACEMENT_3D('',#138390,#106449,#106450);
#95233=AXIS2_PLACEMENT_3D('',#138391,#106451,#106452);
#95234=AXIS2_PLACEMENT_3D('',#138392,#106453,#106454);
#95235=AXIS2_PLACEMENT_3D('',#138395,#106455,#106456);
#95236=AXIS2_PLACEMENT_3D('',#138396,#106457,#106458);
#95237=AXIS2_PLACEMENT_3D('',#138399,#106460,#106461);
#95238=AXIS2_PLACEMENT_3D('',#138400,#106462,#106463);
#95239=AXIS2_PLACEMENT_3D('',#138402,#106465,#106466);
#95240=AXIS2_PLACEMENT_3D('',#138404,#106468,#106469);
#95241=AXIS2_PLACEMENT_3D('',#138406,#106471,#106472);
#95242=AXIS2_PLACEMENT_3D('',#138407,#106473,#106474);
#95243=AXIS2_PLACEMENT_3D('',#138408,#106475,#106476);
#95244=AXIS2_PLACEMENT_3D('',#138409,#106477,#106478);
#95245=AXIS2_PLACEMENT_3D('',#138414,#106480,#106481);
#95246=AXIS2_PLACEMENT_3D('',#138417,#106483,#106484);
#95247=AXIS2_PLACEMENT_3D('',#138418,#106485,#106486);
#95248=AXIS2_PLACEMENT_3D('',#138423,#106488,#106489);
#95249=AXIS2_PLACEMENT_3D('',#138426,#106491,#106492);
#95250=AXIS2_PLACEMENT_3D('',#138427,#106493,#106494);
#95251=AXIS2_PLACEMENT_3D('',#138432,#106496,#106497);
#95252=AXIS2_PLACEMENT_3D('',#138435,#106499,#106500);
#95253=AXIS2_PLACEMENT_3D('',#138436,#106501,#106502);
#95254=AXIS2_PLACEMENT_3D('',#138442,#106503,#106504);
#95255=AXIS2_PLACEMENT_3D('',#138446,#106505,#106506);
#95256=AXIS2_PLACEMENT_3D('',#138455,#106507,#106508);
#95257=AXIS2_PLACEMENT_3D('',#138456,#106509,#106510);
#95258=AXIS2_PLACEMENT_3D('',#138465,#106511,#106512);
#95259=AXIS2_PLACEMENT_3D('',#138466,#106513,#106514);
#95260=AXIS2_PLACEMENT_3D('',#138472,#106515,#106516);
#95261=AXIS2_PLACEMENT_3D('',#138476,#106517,#106518);
#95262=AXIS2_PLACEMENT_3D('',#138485,#106519,#106520);
#95263=AXIS2_PLACEMENT_3D('',#138486,#106521,#106522);
#95264=AXIS2_PLACEMENT_3D('',#138495,#106523,#106524);
#95265=AXIS2_PLACEMENT_3D('',#138496,#106525,#106526);
#95266=AXIS2_PLACEMENT_3D('',#138500,#106528,#106529);
#95267=AXIS2_PLACEMENT_3D('',#138502,#106531,#106532);
#95268=AXIS2_PLACEMENT_3D('',#138507,#106535,#106536);
#95269=AXIS2_PLACEMENT_3D('',#138508,#106537,#106538);
#95270=AXIS2_PLACEMENT_3D('',#138513,#106541,#106542);
#95271=AXIS2_PLACEMENT_3D('',#138514,#106543,#106544);
#95272=AXIS2_PLACEMENT_3D('',#138516,#106545,#106546);
#95273=AXIS2_PLACEMENT_3D('',#138520,#106548,#106549);
#95274=AXIS2_PLACEMENT_3D('',#138525,#106552,#106553);
#95275=AXIS2_PLACEMENT_3D('',#138530,#106556,#106557);
#95276=AXIS2_PLACEMENT_3D('',#138535,#106560,#106561);
#95277=AXIS2_PLACEMENT_3D('',#138539,#106563,#106564);
#95278=AXIS2_PLACEMENT_3D('',#138542,#106566,#106567);
#95279=AXIS2_PLACEMENT_3D('',#138543,#106568,#106569);
#95280=AXIS2_PLACEMENT_3D('',#138547,#106571,#106572);
#95281=AXIS2_PLACEMENT_3D('',#138549,#106574,#106575);
#95282=AXIS2_PLACEMENT_3D('',#138555,#106576,#106577);
#95283=AXIS2_PLACEMENT_3D('',#138559,#106578,#106579);
#95284=AXIS2_PLACEMENT_3D('',#138565,#106580,#106581);
#95285=AXIS2_PLACEMENT_3D('',#138569,#106582,#106583);
#95286=AXIS2_PLACEMENT_3D('',#138573,#106585,#106586);
#95287=AXIS2_PLACEMENT_3D('',#138575,#106588,#106589);
#95288=AXIS2_PLACEMENT_3D('',#138578,#106590,#106591);
#95289=AXIS2_PLACEMENT_3D('',#138581,#106593,#106594);
#95290=AXIS2_PLACEMENT_3D('',#138583,#106595,#106596);
#95291=AXIS2_PLACEMENT_3D('',#138588,#106599,#106600);
#95292=AXIS2_PLACEMENT_3D('',#138593,#106603,#106604);
#95293=AXIS2_PLACEMENT_3D('',#138598,#106607,#106608);
#95294=AXIS2_PLACEMENT_3D('',#138601,#106611,#106612);
#95295=AXIS2_PLACEMENT_3D('',#138603,#106613,#106614);
#95296=AXIS2_PLACEMENT_3D('',#138604,#106615,#106616);
#95297=AXIS2_PLACEMENT_3D('',#138607,#106618,#106619);
#95298=AXIS2_PLACEMENT_3D('',#138608,#106620,#106621);
#95299=AXIS2_PLACEMENT_3D('',#138609,#106622,#106623);
#95300=AXIS2_PLACEMENT_3D('',#138611,#106625,#106626);
#95301=AXIS2_PLACEMENT_3D('',#138613,#106628,#106629);
#95302=AXIS2_PLACEMENT_3D('',#138614,#106630,#106631);
#95303=AXIS2_PLACEMENT_3D('',#138616,#106633,#106634);
#95304=AXIS2_PLACEMENT_3D('',#138618,#106636,#106637);
#95305=AXIS2_PLACEMENT_3D('',#138619,#106638,#106639);
#95306=AXIS2_PLACEMENT_3D('',#138621,#106641,#106642);
#95307=AXIS2_PLACEMENT_3D('',#138623,#106644,#106645);
#95308=AXIS2_PLACEMENT_3D('',#138624,#106646,#106647);
#95309=AXIS2_PLACEMENT_3D('',#138626,#106649,#106650);
#95310=AXIS2_PLACEMENT_3D('',#138628,#106652,#106653);
#95311=AXIS2_PLACEMENT_3D('',#138629,#106654,#106655);
#95312=AXIS2_PLACEMENT_3D('',#138632,#106656,#106657);
#95313=AXIS2_PLACEMENT_3D('',#138636,#106659,#106660);
#95314=AXIS2_PLACEMENT_3D('',#138638,#106662,#106663);
#95315=AXIS2_PLACEMENT_3D('',#138644,#106667,#106668);
#95316=AXIS2_PLACEMENT_3D('',#138646,#106669,#106670);
#95317=AXIS2_PLACEMENT_3D('',#138648,#106671,#106672);
#95318=AXIS2_PLACEMENT_3D('',#138652,#106674,#106675);
#95319=AXIS2_PLACEMENT_3D('',#138654,#106676,#106677);
#95320=AXIS2_PLACEMENT_3D('',#138662,#106681,#106682);
#95321=AXIS2_PLACEMENT_3D('',#138663,#106683,#106684);
#95322=AXIS2_PLACEMENT_3D('',#138664,#106685,#106686);
#95323=AXIS2_PLACEMENT_3D('',#138666,#106687,#106688);
#95324=AXIS2_PLACEMENT_3D('',#138668,#106690,#106691);
#95325=AXIS2_PLACEMENT_3D('',#138671,#106693,#106694);
#95326=AXIS2_PLACEMENT_3D('',#138672,#106695,#106696);
#95327=AXIS2_PLACEMENT_3D('',#138675,#106697,#106698);
#95328=AXIS2_PLACEMENT_3D('',#138678,#106701,#106702);
#95329=AXIS2_PLACEMENT_3D('',#138679,#106703,#106704);
#95330=AXIS2_PLACEMENT_3D('',#138680,#106705,#106706);
#95331=AXIS2_PLACEMENT_3D('',#138683,#106707,#106708);
#95332=AXIS2_PLACEMENT_3D('',#138686,#106711,#106712);
#95333=AXIS2_PLACEMENT_3D('',#138688,#106713,#106714);
#95334=AXIS2_PLACEMENT_3D('',#138690,#106716,#106717);
#95335=AXIS2_PLACEMENT_3D('',#138696,#106721,#106722);
#95336=AXIS2_PLACEMENT_3D('',#138702,#106726,#106727);
#95337=AXIS2_PLACEMENT_3D('',#138708,#106731,#106732);
#95338=AXIS2_PLACEMENT_3D('',#138710,#106734,#106735);
#95339=AXIS2_PLACEMENT_3D('',#138712,#106737,#106738);
#95340=AXIS2_PLACEMENT_3D('',#138714,#106740,#106741);
#95341=AXIS2_PLACEMENT_3D('',#138715,#106742,#106743);
#95342=AXIS2_PLACEMENT_3D('',#138716,#106744,#106745);
#95343=AXIS2_PLACEMENT_3D('',#138719,#106746,#106747);
#95344=AXIS2_PLACEMENT_3D('',#138723,#106749,#106750);
#95345=AXIS2_PLACEMENT_3D('',#138742,#106752,#106753);
#95346=AXIS2_PLACEMENT_3D('',#138743,#106754,#106755);
#95347=AXIS2_PLACEMENT_3D('',#138744,#106756,#106757);
#95348=AXIS2_PLACEMENT_3D('',#138745,#106758,#106759);
#95349=AXIS2_PLACEMENT_3D('',#138748,#106760,#106761);
#95350=AXIS2_PLACEMENT_3D('',#138749,#106762,#106763);
#95351=AXIS2_PLACEMENT_3D('',#138750,#106764,#106765);
#95352=AXIS2_PLACEMENT_3D('',#138768,#106766,#106767);
#95353=AXIS2_PLACEMENT_3D('',#138769,#106768,#106769);
#95354=AXIS2_PLACEMENT_3D('',#138770,#106770,#106771);
#95355=AXIS2_PLACEMENT_3D('',#138771,#106772,#106773);
#95356=AXIS2_PLACEMENT_3D('',#138774,#106774,#106775);
#95357=AXIS2_PLACEMENT_3D('',#138775,#106776,#106777);
#95358=AXIS2_PLACEMENT_3D('',#138776,#106778,#106779);
#95359=AXIS2_PLACEMENT_3D('',#138794,#106780,#106781);
#95360=AXIS2_PLACEMENT_3D('',#138795,#106782,#106783);
#95361=AXIS2_PLACEMENT_3D('',#138796,#106784,#106785);
#95362=AXIS2_PLACEMENT_3D('',#138797,#106786,#106787);
#95363=AXIS2_PLACEMENT_3D('',#138800,#106788,#106789);
#95364=AXIS2_PLACEMENT_3D('',#138801,#106790,#106791);
#95365=AXIS2_PLACEMENT_3D('',#138802,#106792,#106793);
#95366=AXIS2_PLACEMENT_3D('',#138814,#106794,#106795);
#95367=AXIS2_PLACEMENT_3D('',#138815,#106796,#106797);
#95368=AXIS2_PLACEMENT_3D('',#138816,#106798,#106799);
#95369=AXIS2_PLACEMENT_3D('',#138817,#106800,#106801);
#95370=AXIS2_PLACEMENT_3D('',#138820,#106802,#106803);
#95371=AXIS2_PLACEMENT_3D('',#138832,#106806,#106807);
#95372=AXIS2_PLACEMENT_3D('',#138833,#106808,#106809);
#95373=AXIS2_PLACEMENT_3D('',#138834,#106810,#106811);
#95374=AXIS2_PLACEMENT_3D('',#138838,#106813,#106814);
#95375=AXIS2_PLACEMENT_3D('',#138842,#106816,#106817);
#95376=AXIS2_PLACEMENT_3D('',#138856,#106820,#106821);
#95377=AXIS2_PLACEMENT_3D('',#138858,#106823,#106824);
#95378=AXIS2_PLACEMENT_3D('',#138861,#106826,#106827);
#95379=AXIS2_PLACEMENT_3D('',#138862,#106828,#106829);
#95380=AXIS2_PLACEMENT_3D('',#138866,#106832,#106833);
#95381=AXIS2_PLACEMENT_3D('',#138869,#106835,#106836);
#95382=AXIS2_PLACEMENT_3D('',#138870,#106837,#106838);
#95383=AXIS2_PLACEMENT_3D('',#138874,#106841,#106842);
#95384=AXIS2_PLACEMENT_3D('',#138875,#106843,#106844);
#95385=AXIS2_PLACEMENT_3D('',#138878,#106845,#106846);
#95386=AXIS2_PLACEMENT_3D('',#138882,#106848,#106849);
#95387=AXIS2_PLACEMENT_3D('',#138895,#106851,#106852);
#95388=AXIS2_PLACEMENT_3D('',#138896,#106853,#106854);
#95389=AXIS2_PLACEMENT_3D('',#138897,#106855,#106856);
#95390=AXIS2_PLACEMENT_3D('',#138898,#106857,#106858);
#95391=AXIS2_PLACEMENT_3D('',#138901,#106859,#106860);
#95392=AXIS2_PLACEMENT_3D('',#138902,#106861,#106862);
#95393=AXIS2_PLACEMENT_3D('',#138903,#106863,#106864);
#95394=AXIS2_PLACEMENT_3D('',#138921,#106865,#106866);
#95395=AXIS2_PLACEMENT_3D('',#138922,#106867,#106868);
#95396=AXIS2_PLACEMENT_3D('',#138923,#106869,#106870);
#95397=AXIS2_PLACEMENT_3D('',#138924,#106871,#106872);
#95398=AXIS2_PLACEMENT_3D('',#138927,#106873,#106874);
#95399=AXIS2_PLACEMENT_3D('',#138941,#106877,#106878);
#95400=AXIS2_PLACEMENT_3D('',#138942,#106879,#106880);
#95401=AXIS2_PLACEMENT_3D('',#138943,#106881,#106882);
#95402=AXIS2_PLACEMENT_3D('',#138944,#106883,#106884);
#95403=AXIS2_PLACEMENT_3D('',#138947,#106885,#106886);
#95404=AXIS2_PLACEMENT_3D('',#138950,#106889,#106890);
#95405=AXIS2_PLACEMENT_3D('',#138953,#106891,#106892);
#95406=AXIS2_PLACEMENT_3D('',#138954,#106893,#106894);
#95407=AXIS2_PLACEMENT_3D('',#138955,#106895,#106896);
#95408=AXIS2_PLACEMENT_3D('',#138956,#106897,#106898);
#95409=AXIS2_PLACEMENT_3D('',#138959,#106899,#106900);
#95410=AXIS2_PLACEMENT_3D('',#138979,#106903,#106904);
#95411=AXIS2_PLACEMENT_3D('',#138980,#106905,#106906);
#95412=AXIS2_PLACEMENT_3D('',#138981,#106907,#106908);
#95413=AXIS2_PLACEMENT_3D('',#138982,#106909,#106910);
#95414=AXIS2_PLACEMENT_3D('',#138985,#106911,#106912);
#95415=AXIS2_PLACEMENT_3D('',#138986,#106913,#106914);
#95416=AXIS2_PLACEMENT_3D('',#138987,#106915,#106916);
#95417=AXIS2_PLACEMENT_3D('',#138999,#106917,#106918);
#95418=AXIS2_PLACEMENT_3D('',#139000,#106919,#106920);
#95419=AXIS2_PLACEMENT_3D('',#139001,#106921,#106922);
#95420=AXIS2_PLACEMENT_3D('',#139002,#106923,#106924);
#95421=AXIS2_PLACEMENT_3D('',#139005,#106925,#106926);
#95422=AXIS2_PLACEMENT_3D('',#139007,#106927,#106928);
#95423=AXIS2_PLACEMENT_3D('',#139008,#106929,#106930);
#95424=AXIS2_PLACEMENT_3D('',#139009,#106931,#106932);
#95425=AXIS2_PLACEMENT_3D('',#139019,#106933,#106934);
#95426=AXIS2_PLACEMENT_3D('',#139020,#106935,#106936);
#95427=AXIS2_PLACEMENT_3D('',#139021,#106937,#106938);
#95428=AXIS2_PLACEMENT_3D('',#139027,#106942,#106943);
#95429=AXIS2_PLACEMENT_3D('',#139030,#106945,#106946);
#95430=AXIS2_PLACEMENT_3D('',#139031,#106947,#106948);
#95431=AXIS2_PLACEMENT_3D('',#139034,#106950,#106951);
#95432=AXIS2_PLACEMENT_3D('',#139035,#106952,#106953);
#95433=AXIS2_PLACEMENT_3D('',#139038,#106955,#106956);
#95434=AXIS2_PLACEMENT_3D('',#139039,#106957,#106958);
#95435=AXIS2_PLACEMENT_3D('',#139041,#106959,#106960);
#95436=AXIS2_PLACEMENT_3D('',#139046,#106963,#106964);
#95437=AXIS2_PLACEMENT_3D('',#139050,#106966,#106967);
#95438=AXIS2_PLACEMENT_3D('',#139054,#106969,#106970);
#95439=AXIS2_PLACEMENT_3D('',#139058,#106972,#106973);
#95440=AXIS2_PLACEMENT_3D('',#139061,#106975,#106976);
#95441=AXIS2_PLACEMENT_3D('',#139062,#106977,#106978);
#95442=AXIS2_PLACEMENT_3D('',#139065,#106980,#106981);
#95443=AXIS2_PLACEMENT_3D('',#139066,#106982,#106983);
#95444=AXIS2_PLACEMENT_3D('',#139070,#106986,#106987);
#95445=AXIS2_PLACEMENT_3D('',#139071,#106988,#106989);
#95446=AXIS2_PLACEMENT_3D('',#139074,#106990,#106991);
#95447=AXIS2_PLACEMENT_3D('',#139076,#106992,#106993);
#95448=AXIS2_PLACEMENT_3D('',#139078,#106994,#106995);
#95449=AXIS2_PLACEMENT_3D('',#139079,#106996,#106997);
#95450=AXIS2_PLACEMENT_3D('',#139091,#106998,#106999);
#95451=AXIS2_PLACEMENT_3D('',#139092,#107000,#107001);
#95452=AXIS2_PLACEMENT_3D('',#139093,#107002,#107003);
#95453=AXIS2_PLACEMENT_3D('',#139094,#107004,#107005);
#95454=AXIS2_PLACEMENT_3D('',#139097,#107006,#107007);
#95455=AXIS2_PLACEMENT_3D('',#139117,#107010,#107011);
#95456=AXIS2_PLACEMENT_3D('',#139118,#107012,#107013);
#95457=AXIS2_PLACEMENT_3D('',#139119,#107014,#107015);
#95458=AXIS2_PLACEMENT_3D('',#139120,#107016,#107017);
#95459=AXIS2_PLACEMENT_3D('',#139123,#107018,#107019);
#95460=AXIS2_PLACEMENT_3D('',#139143,#107022,#107023);
#95461=AXIS2_PLACEMENT_3D('',#139144,#107024,#107025);
#95462=AXIS2_PLACEMENT_3D('',#139145,#107026,#107027);
#95463=AXIS2_PLACEMENT_3D('',#139146,#107028,#107029);
#95464=AXIS2_PLACEMENT_3D('',#139149,#107030,#107031);
#95465=AXIS2_PLACEMENT_3D('',#139150,#107032,#107033);
#95466=AXIS2_PLACEMENT_3D('',#139151,#107034,#107035);
#95467=AXIS2_PLACEMENT_3D('',#139163,#107036,#107037);
#95468=AXIS2_PLACEMENT_3D('',#139164,#107038,#107039);
#95469=AXIS2_PLACEMENT_3D('',#139165,#107040,#107041);
#95470=AXIS2_PLACEMENT_3D('',#139166,#107042,#107043);
#95471=AXIS2_PLACEMENT_3D('',#139169,#107044,#107045);
#95472=AXIS2_PLACEMENT_3D('',#139182,#107048,#107049);
#95473=AXIS2_PLACEMENT_3D('',#139183,#107050,#107051);
#95474=AXIS2_PLACEMENT_3D('',#139184,#107052,#107053);
#95475=AXIS2_PLACEMENT_3D('',#139185,#107054,#107055);
#95476=AXIS2_PLACEMENT_3D('',#139187,#107056,#107057);
#95477=AXIS2_PLACEMENT_3D('',#139188,#107058,#107059);
#95478=AXIS2_PLACEMENT_3D('',#139198,#107060,#107061);
#95479=AXIS2_PLACEMENT_3D('',#139199,#107062,#107063);
#95480=AXIS2_PLACEMENT_3D('',#139200,#107064,#107065);
#95481=AXIS2_PLACEMENT_3D('',#139204,#107067,#107068);
#95482=AXIS2_PLACEMENT_3D('',#139208,#107070,#107071);
#95483=AXIS2_PLACEMENT_3D('',#139210,#107073,#107074);
#95484=AXIS2_PLACEMENT_3D('',#139214,#107077,#107078);
#95485=AXIS2_PLACEMENT_3D('',#139215,#107079,#107080);
#95486=AXIS2_PLACEMENT_3D('',#139216,#107081,#107082);
#95487=AXIS2_PLACEMENT_3D('',#139219,#107084,#107085);
#95488=AXIS2_PLACEMENT_3D('',#139220,#107086,#107087);
#95489=AXIS2_PLACEMENT_3D('',#139223,#107089,#107090);
#95490=AXIS2_PLACEMENT_3D('',#139224,#107091,#107092);
#95491=AXIS2_PLACEMENT_3D('',#139225,#107093,#107094);
#95492=AXIS2_PLACEMENT_3D('',#139228,#107095,#107096);
#95493=AXIS2_PLACEMENT_3D('',#139232,#107098,#107099);
#95494=AXIS2_PLACEMENT_3D('',#139245,#107101,#107102);
#95495=AXIS2_PLACEMENT_3D('',#139246,#107103,#107104);
#95496=AXIS2_PLACEMENT_3D('',#139247,#107105,#107106);
#95497=AXIS2_PLACEMENT_3D('',#139248,#107107,#107108);
#95498=AXIS2_PLACEMENT_3D('',#139251,#107109,#107110);
#95499=AXIS2_PLACEMENT_3D('',#139252,#107111,#107112);
#95500=AXIS2_PLACEMENT_3D('',#139253,#107113,#107114);
#95501=AXIS2_PLACEMENT_3D('',#139265,#107115,#107116);
#95502=AXIS2_PLACEMENT_3D('',#139266,#107117,#107118);
#95503=AXIS2_PLACEMENT_3D('',#139267,#107119,#107120);
#95504=AXIS2_PLACEMENT_3D('',#139268,#107121,#107122);
#95505=AXIS2_PLACEMENT_3D('',#139271,#107123,#107124);
#95506=AXIS2_PLACEMENT_3D('',#139272,#107125,#107126);
#95507=AXIS2_PLACEMENT_3D('',#139273,#107127,#107128);
#95508=AXIS2_PLACEMENT_3D('',#139274,#107129,#107130);
#95509=AXIS2_PLACEMENT_3D('',#139277,#107131,#107132);
#95510=AXIS2_PLACEMENT_3D('',#139278,#107133,#107134);
#95511=AXIS2_PLACEMENT_3D('',#139279,#107135,#107136);
#95512=AXIS2_PLACEMENT_3D('',#139280,#107137,#107138);
#95513=AXIS2_PLACEMENT_3D('',#139283,#107139,#107140);
#95514=AXIS2_PLACEMENT_3D('',#139286,#107143,#107144);
#95515=AXIS2_PLACEMENT_3D('',#139289,#107145,#107146);
#95516=AXIS2_PLACEMENT_3D('',#139290,#107147,#107148);
#95517=AXIS2_PLACEMENT_3D('',#139291,#107149,#107150);
#95518=AXIS2_PLACEMENT_3D('',#139309,#107151,#107152);
#95519=AXIS2_PLACEMENT_3D('',#139310,#107153,#107154);
#95520=AXIS2_PLACEMENT_3D('',#139311,#107155,#107156);
#95521=AXIS2_PLACEMENT_3D('',#139312,#107157,#107158);
#95522=AXIS2_PLACEMENT_3D('',#139315,#107159,#107160);
#95523=AXIS2_PLACEMENT_3D('',#139327,#107163,#107164);
#95524=AXIS2_PLACEMENT_3D('',#139328,#107165,#107166);
#95525=AXIS2_PLACEMENT_3D('',#139329,#107167,#107168);
#95526=AXIS2_PLACEMENT_3D('',#139339,#107174,#107175);
#95527=AXIS2_PLACEMENT_3D('',#139342,#107177,#107178);
#95528=AXIS2_PLACEMENT_3D('',#139343,#107179,#107180);
#95529=AXIS2_PLACEMENT_3D('',#139346,#107182,#107183);
#95530=AXIS2_PLACEMENT_3D('',#139347,#107184,#107185);
#95531=AXIS2_PLACEMENT_3D('',#139351,#107188,#107189);
#95532=AXIS2_PLACEMENT_3D('',#139354,#107191,#107192);
#95533=AXIS2_PLACEMENT_3D('',#139355,#107193,#107194);
#95534=AXIS2_PLACEMENT_3D('',#139363,#107199,#107200);
#95535=AXIS2_PLACEMENT_3D('',#139364,#107201,#107202);
#95536=AXIS2_PLACEMENT_3D('',#139367,#107203,#107204);
#95537=AXIS2_PLACEMENT_3D('',#139369,#107205,#107206);
#95538=AXIS2_PLACEMENT_3D('',#139371,#107207,#107208);
#95539=AXIS2_PLACEMENT_3D('',#139372,#107209,#107210);
#95540=AXIS2_PLACEMENT_3D('',#139390,#107211,#107212);
#95541=AXIS2_PLACEMENT_3D('',#139391,#107213,#107214);
#95542=AXIS2_PLACEMENT_3D('',#139392,#107215,#107216);
#95543=AXIS2_PLACEMENT_3D('',#139393,#107217,#107218);
#95544=AXIS2_PLACEMENT_3D('',#139396,#107219,#107220);
#95545=AXIS2_PLACEMENT_3D('',#139397,#107221,#107222);
#95546=AXIS2_PLACEMENT_3D('',#139398,#107223,#107224);
#95547=AXIS2_PLACEMENT_3D('',#139399,#107225,#107226);
#95548=AXIS2_PLACEMENT_3D('',#139402,#107227,#107228);
#95549=AXIS2_PLACEMENT_3D('',#139403,#107229,#107230);
#95550=AXIS2_PLACEMENT_3D('',#139404,#107231,#107232);
#95551=AXIS2_PLACEMENT_3D('',#139422,#107233,#107234);
#95552=AXIS2_PLACEMENT_3D('',#139423,#107235,#107236);
#95553=AXIS2_PLACEMENT_3D('',#139424,#107237,#107238);
#95554=AXIS2_PLACEMENT_3D('',#139425,#107239,#107240);
#95555=AXIS2_PLACEMENT_3D('',#139428,#107241,#107242);
#95556=AXIS2_PLACEMENT_3D('',#139431,#107245,#107246);
#95557=AXIS2_PLACEMENT_3D('',#139434,#107247,#107248);
#95558=AXIS2_PLACEMENT_3D('',#139435,#107249,#107250);
#95559=AXIS2_PLACEMENT_3D('',#139436,#107251,#107252);
#95560=AXIS2_PLACEMENT_3D('',#139437,#107253,#107254);
#95561=AXIS2_PLACEMENT_3D('',#139440,#107255,#107256);
#95562=AXIS2_PLACEMENT_3D('',#139454,#107259,#107260);
#95563=AXIS2_PLACEMENT_3D('',#139455,#107261,#107262);
#95564=AXIS2_PLACEMENT_3D('',#139456,#107263,#107264);
#95565=AXIS2_PLACEMENT_3D('',#139457,#107265,#107266);
#95566=AXIS2_PLACEMENT_3D('',#139460,#107267,#107268);
#95567=AXIS2_PLACEMENT_3D('',#139480,#107271,#107272);
#95568=AXIS2_PLACEMENT_3D('',#139481,#107273,#107274);
#95569=AXIS2_PLACEMENT_3D('',#139482,#107275,#107276);
#95570=AXIS2_PLACEMENT_3D('',#139483,#107277,#107278);
#95571=AXIS2_PLACEMENT_3D('',#139486,#107279,#107280);
#95572=AXIS2_PLACEMENT_3D('',#139487,#107281,#107282);
#95573=AXIS2_PLACEMENT_3D('',#139488,#107283,#107284);
#95574=AXIS2_PLACEMENT_3D('',#139506,#107285,#107286);
#95575=AXIS2_PLACEMENT_3D('',#139507,#107287,#107288);
#95576=AXIS2_PLACEMENT_3D('',#139508,#107289,#107290);
#95577=AXIS2_PLACEMENT_3D('',#139509,#107291,#107292);
#95578=AXIS2_PLACEMENT_3D('',#139512,#107295,#107296);
#95579=AXIS2_PLACEMENT_3D('',#139516,#107298,#107299);
#95580=AXIS2_PLACEMENT_3D('',#139518,#107301,#107302);
#95581=AXIS2_PLACEMENT_3D('',#139522,#107305,#107306);
#95582=AXIS2_PLACEMENT_3D('',#139525,#107308,#107309);
#95583=AXIS2_PLACEMENT_3D('',#139526,#107310,#107311);
#95584=AXIS2_PLACEMENT_3D('',#139529,#107313,#107314);
#95585=AXIS2_PLACEMENT_3D('',#139530,#107315,#107316);
#95586=AXIS2_PLACEMENT_3D('',#139533,#107318,#107319);
#95587=AXIS2_PLACEMENT_3D('',#139534,#107320,#107321);
#95588=AXIS2_PLACEMENT_3D('',#139538,#107324,#107325);
#95589=AXIS2_PLACEMENT_3D('',#139541,#107327,#107328);
#95590=AXIS2_PLACEMENT_3D('',#139542,#107329,#107330);
#95591=AXIS2_PLACEMENT_3D('',#139543,#107331,#107332);
#95592=AXIS2_PLACEMENT_3D('',#139546,#107333,#107334);
#95593=AXIS2_PLACEMENT_3D('',#139548,#107335,#107336);
#95594=AXIS2_PLACEMENT_3D('',#139550,#107337,#107338);
#95595=AXIS2_PLACEMENT_3D('',#139551,#107339,#107340);
#95596=AXIS2_PLACEMENT_3D('',#139552,#107341,#107342);
#95597=AXIS2_PLACEMENT_3D('',#139555,#107343,#107344);
#95598=AXIS2_PLACEMENT_3D('',#139556,#107345,#107346);
#95599=AXIS2_PLACEMENT_3D('',#139557,#107347,#107348);
#95600=AXIS2_PLACEMENT_3D('',#139575,#107349,#107350);
#95601=AXIS2_PLACEMENT_3D('',#139576,#107351,#107352);
#95602=AXIS2_PLACEMENT_3D('',#139577,#107353,#107354);
#95603=AXIS2_PLACEMENT_3D('',#139578,#107355,#107356);
#95604=AXIS2_PLACEMENT_3D('',#139581,#107357,#107358);
#95605=AXIS2_PLACEMENT_3D('',#139582,#107359,#107360);
#95606=AXIS2_PLACEMENT_3D('',#139583,#107361,#107362);
#95607=AXIS2_PLACEMENT_3D('',#139595,#107363,#107364);
#95608=AXIS2_PLACEMENT_3D('',#139596,#107365,#107366);
#95609=AXIS2_PLACEMENT_3D('',#139597,#107367,#107368);
#95610=AXIS2_PLACEMENT_3D('',#139598,#107369,#107370);
#95611=AXIS2_PLACEMENT_3D('',#139601,#107371,#107372);
#95612=AXIS2_PLACEMENT_3D('',#139602,#107373,#107374);
#95613=AXIS2_PLACEMENT_3D('',#139603,#107375,#107376);
#95614=AXIS2_PLACEMENT_3D('',#139621,#107377,#107378);
#95615=AXIS2_PLACEMENT_3D('',#139622,#107379,#107380);
#95616=AXIS2_PLACEMENT_3D('',#139623,#107381,#107382);
#95617=AXIS2_PLACEMENT_3D('',#139624,#107383,#107384);
#95618=AXIS2_PLACEMENT_3D('',#139627,#107385,#107386);
#95619=AXIS2_PLACEMENT_3D('',#139639,#107389,#107390);
#95620=AXIS2_PLACEMENT_3D('',#139640,#107391,#107392);
#95621=AXIS2_PLACEMENT_3D('',#139641,#107393,#107394);
#95622=AXIS2_PLACEMENT_3D('',#139645,#107396,#107397);
#95623=AXIS2_PLACEMENT_3D('',#139647,#107399,#107400);
#95624=AXIS2_PLACEMENT_3D('',#139650,#107402,#107403);
#95625=AXIS2_PLACEMENT_3D('',#139651,#107404,#107405);
#95626=AXIS2_PLACEMENT_3D('',#139655,#107408,#107409);
#95627=AXIS2_PLACEMENT_3D('',#139658,#107411,#107412);
#95628=AXIS2_PLACEMENT_3D('',#139659,#107413,#107414);
#95629=AXIS2_PLACEMENT_3D('',#139662,#107416,#107417);
#95630=AXIS2_PLACEMENT_3D('',#139663,#107418,#107419);
#95631=AXIS2_PLACEMENT_3D('',#139664,#107420,#107421);
#95632=AXIS2_PLACEMENT_3D('',#139667,#107422,#107423);
#95633=AXIS2_PLACEMENT_3D('',#139669,#107424,#107425);
#95634=AXIS2_PLACEMENT_3D('',#139671,#107426,#107427);
#95635=AXIS2_PLACEMENT_3D('',#139672,#107428,#107429);
#95636=AXIS2_PLACEMENT_3D('',#139684,#107430,#107431);
#95637=AXIS2_PLACEMENT_3D('',#139685,#107432,#107433);
#95638=AXIS2_PLACEMENT_3D('',#139686,#107434,#107435);
#95639=AXIS2_PLACEMENT_3D('',#139687,#107436,#107437);
#95640=AXIS2_PLACEMENT_3D('',#139690,#107438,#107439);
#95641=AXIS2_PLACEMENT_3D('',#139691,#107440,#107441);
#95642=AXIS2_PLACEMENT_3D('',#139692,#107442,#107443);
#95643=AXIS2_PLACEMENT_3D('',#139693,#107444,#107445);
#95644=AXIS2_PLACEMENT_3D('',#139696,#107446,#107447);
#95645=AXIS2_PLACEMENT_3D('',#139697,#107448,#107449);
#95646=AXIS2_PLACEMENT_3D('',#139698,#107450,#107451);
#95647=AXIS2_PLACEMENT_3D('',#139699,#107452,#107453);
#95648=AXIS2_PLACEMENT_3D('',#139702,#107454,#107455);
#95649=AXIS2_PLACEMENT_3D('',#139703,#107456,#107457);
#95650=AXIS2_PLACEMENT_3D('',#139704,#107458,#107459);
#95651=AXIS2_PLACEMENT_3D('',#139716,#107460,#107461);
#95652=AXIS2_PLACEMENT_3D('',#139717,#107462,#107463);
#95653=AXIS2_PLACEMENT_3D('',#139718,#107464,#107465);
#95654=AXIS2_PLACEMENT_3D('',#139719,#107466,#107467);
#95655=AXIS2_PLACEMENT_3D('',#139722,#107468,#107469);
#95656=AXIS2_PLACEMENT_3D('',#139742,#107472,#107473);
#95657=AXIS2_PLACEMENT_3D('',#139743,#107474,#107475);
#95658=AXIS2_PLACEMENT_3D('',#139744,#107476,#107477);
#95659=AXIS2_PLACEMENT_3D('',#139745,#107478,#107479);
#95660=AXIS2_PLACEMENT_3D('',#139748,#107480,#107481);
#95661=AXIS2_PLACEMENT_3D('',#139762,#107484,#107485);
#95662=AXIS2_PLACEMENT_3D('',#139763,#107486,#107487);
#95663=AXIS2_PLACEMENT_3D('',#139764,#107488,#107489);
#95664=AXIS2_PLACEMENT_3D('',#139765,#107490,#107491);
#95665=AXIS2_PLACEMENT_3D('',#139768,#107492,#107493);
#95666=AXIS2_PLACEMENT_3D('',#139782,#107496,#107497);
#95667=AXIS2_PLACEMENT_3D('',#139783,#107498,#107499);
#95668=AXIS2_PLACEMENT_3D('',#139784,#107500,#107501);
#95669=AXIS2_PLACEMENT_3D('',#139785,#107502,#107503);
#95670=AXIS2_PLACEMENT_3D('',#139788,#107504,#107505);
#95671=AXIS2_PLACEMENT_3D('',#139789,#107506,#107507);
#95672=AXIS2_PLACEMENT_3D('',#139790,#107508,#107509);
#95673=AXIS2_PLACEMENT_3D('',#139802,#107510,#107511);
#95674=AXIS2_PLACEMENT_3D('',#139803,#107512,#107513);
#95675=AXIS2_PLACEMENT_3D('',#139804,#107514,#107515);
#95676=AXIS2_PLACEMENT_3D('',#139805,#107516,#107517);
#95677=AXIS2_PLACEMENT_3D('',#139808,#107518,#107519);
#95678=AXIS2_PLACEMENT_3D('',#139809,#107520,#107521);
#95679=AXIS2_PLACEMENT_3D('',#139810,#107522,#107523);
#95680=AXIS2_PLACEMENT_3D('',#139826,#107524,#107525);
#95681=AXIS2_PLACEMENT_3D('',#139827,#107526,#107527);
#95682=AXIS2_PLACEMENT_3D('',#139828,#107528,#107529);
#95683=AXIS2_PLACEMENT_3D('',#139832,#107531,#107532);
#95684=AXIS2_PLACEMENT_3D('',#139834,#107534,#107535);
#95685=AXIS2_PLACEMENT_3D('',#139838,#107538,#107539);
#95686=AXIS2_PLACEMENT_3D('',#139841,#107541,#107542);
#95687=AXIS2_PLACEMENT_3D('',#139842,#107543,#107544);
#95688=AXIS2_PLACEMENT_3D('',#139845,#107546,#107547);
#95689=AXIS2_PLACEMENT_3D('',#139846,#107548,#107549);
#95690=AXIS2_PLACEMENT_3D('',#139849,#107551,#107552);
#95691=AXIS2_PLACEMENT_3D('',#139850,#107553,#107554);
#95692=AXIS2_PLACEMENT_3D('',#139853,#107556,#107557);
#95693=AXIS2_PLACEMENT_3D('',#139854,#107558,#107559);
#95694=AXIS2_PLACEMENT_3D('',#139857,#107561,#107562);
#95695=AXIS2_PLACEMENT_3D('',#139858,#107563,#107564);
#95696=AXIS2_PLACEMENT_3D('',#139862,#107566,#107567);
#95697=AXIS2_PLACEMENT_3D('',#139865,#107569,#107570);
#95698=AXIS2_PLACEMENT_3D('',#139866,#107571,#107572);
#95699=AXIS2_PLACEMENT_3D('',#139867,#107573,#107574);
#95700=AXIS2_PLACEMENT_3D('',#139870,#107575,#107576);
#95701=AXIS2_PLACEMENT_3D('',#139872,#107577,#107578);
#95702=AXIS2_PLACEMENT_3D('',#139874,#107579,#107580);
#95703=AXIS2_PLACEMENT_3D('',#139875,#107581,#107582);
#95704=AXIS2_PLACEMENT_3D('',#139893,#107583,#107584);
#95705=AXIS2_PLACEMENT_3D('',#139894,#107585,#107586);
#95706=AXIS2_PLACEMENT_3D('',#139895,#107587,#107588);
#95707=AXIS2_PLACEMENT_3D('',#139896,#107589,#107590);
#95708=AXIS2_PLACEMENT_3D('',#139899,#107591,#107592);
#95709=AXIS2_PLACEMENT_3D('',#139900,#107593,#107594);
#95710=AXIS2_PLACEMENT_3D('',#139901,#107595,#107596);
#95711=AXIS2_PLACEMENT_3D('',#139902,#107597,#107598);
#95712=AXIS2_PLACEMENT_3D('',#139905,#107599,#107600);
#95713=AXIS2_PLACEMENT_3D('',#139919,#107603,#107604);
#95714=AXIS2_PLACEMENT_3D('',#139920,#107605,#107606);
#95715=AXIS2_PLACEMENT_3D('',#139921,#107607,#107608);
#95716=AXIS2_PLACEMENT_3D('',#139922,#107609,#107610);
#95717=AXIS2_PLACEMENT_3D('',#139925,#107611,#107612);
#95718=AXIS2_PLACEMENT_3D('',#139926,#107613,#107614);
#95719=AXIS2_PLACEMENT_3D('',#139927,#107615,#107616);
#95720=AXIS2_PLACEMENT_3D('',#139945,#107617,#107618);
#95721=AXIS2_PLACEMENT_3D('',#139946,#107619,#107620);
#95722=AXIS2_PLACEMENT_3D('',#139947,#107621,#107622);
#95723=AXIS2_PLACEMENT_3D('',#139948,#107623,#107624);
#95724=AXIS2_PLACEMENT_3D('',#139951,#107625,#107626);
#95725=AXIS2_PLACEMENT_3D('',#139952,#107627,#107628);
#95726=AXIS2_PLACEMENT_3D('',#139953,#107629,#107630);
#95727=AXIS2_PLACEMENT_3D('',#139969,#107631,#107632);
#95728=AXIS2_PLACEMENT_3D('',#139970,#107633,#107634);
#95729=AXIS2_PLACEMENT_3D('',#139971,#107635,#107636);
#95730=AXIS2_PLACEMENT_3D('',#139975,#107638,#107639);
#95731=AXIS2_PLACEMENT_3D('',#139979,#107641,#107642);
#95732=AXIS2_PLACEMENT_3D('',#139983,#107644,#107645);
#95733=AXIS2_PLACEMENT_3D('',#139985,#107647,#107648);
#95734=AXIS2_PLACEMENT_3D('',#139988,#107650,#107651);
#95735=AXIS2_PLACEMENT_3D('',#139989,#107652,#107653);
#95736=AXIS2_PLACEMENT_3D('',#139992,#107655,#107656);
#95737=AXIS2_PLACEMENT_3D('',#139993,#107657,#107658);
#95738=AXIS2_PLACEMENT_3D('',#139996,#107660,#107661);
#95739=AXIS2_PLACEMENT_3D('',#139997,#107662,#107663);
#95740=AXIS2_PLACEMENT_3D('',#140000,#107665,#107666);
#95741=AXIS2_PLACEMENT_3D('',#140001,#107667,#107668);
#95742=AXIS2_PLACEMENT_3D('',#140002,#107669,#107670);
#95743=AXIS2_PLACEMENT_3D('',#140005,#107671,#107672);
#95744=AXIS2_PLACEMENT_3D('',#140009,#107674,#107675);
#95745=AXIS2_PLACEMENT_3D('',#140022,#107677,#107678);
#95746=AXIS2_PLACEMENT_3D('',#140023,#107679,#107680);
#95747=AXIS2_PLACEMENT_3D('',#140024,#107681,#107682);
#95748=AXIS2_PLACEMENT_3D('',#140025,#107683,#107684);
#95749=AXIS2_PLACEMENT_3D('',#140028,#107685,#107686);
#95750=AXIS2_PLACEMENT_3D('',#140048,#107689,#107690);
#95751=AXIS2_PLACEMENT_3D('',#140049,#107691,#107692);
#95752=AXIS2_PLACEMENT_3D('',#140050,#107693,#107694);
#95753=AXIS2_PLACEMENT_3D('',#140051,#107695,#107696);
#95754=AXIS2_PLACEMENT_3D('',#140054,#107697,#107698);
#95755=AXIS2_PLACEMENT_3D('',#140055,#107699,#107700);
#95756=AXIS2_PLACEMENT_3D('',#140056,#107701,#107702);
#95757=AXIS2_PLACEMENT_3D('',#140074,#107703,#107704);
#95758=AXIS2_PLACEMENT_3D('',#140075,#107705,#107706);
#95759=AXIS2_PLACEMENT_3D('',#140076,#107707,#107708);
#95760=AXIS2_PLACEMENT_3D('',#140077,#107709,#107710);
#95761=AXIS2_PLACEMENT_3D('',#140080,#107711,#107712);
#95762=AXIS2_PLACEMENT_3D('',#140081,#107713,#107714);
#95763=AXIS2_PLACEMENT_3D('',#140082,#107715,#107716);
#95764=AXIS2_PLACEMENT_3D('',#140098,#107717,#107718);
#95765=AXIS2_PLACEMENT_3D('',#140099,#107719,#107720);
#95766=AXIS2_PLACEMENT_3D('',#140100,#107721,#107722);
#95767=AXIS2_PLACEMENT_3D('',#140104,#107724,#107725);
#95768=AXIS2_PLACEMENT_3D('',#140106,#107727,#107728);
#95769=AXIS2_PLACEMENT_3D('',#140109,#107730,#107731);
#95770=AXIS2_PLACEMENT_3D('',#140110,#107732,#107733);
#95771=AXIS2_PLACEMENT_3D('',#140113,#107735,#107736);
#95772=AXIS2_PLACEMENT_3D('',#140114,#107737,#107738);
#95773=AXIS2_PLACEMENT_3D('',#140118,#107741,#107742);
#95774=AXIS2_PLACEMENT_3D('',#140208,#107743,#107744);
#95775=AXIS2_PLACEMENT_3D('',#140243,#107745,#107746);
#95776=AXIS2_PLACEMENT_3D('',#140327,#107747,#107748);
#95777=AXIS2_PLACEMENT_3D('',#140330,#107750,#107751);
#95778=AXIS2_PLACEMENT_3D('',#140331,#107752,#107753);
#95779=AXIS2_PLACEMENT_3D('',#140335,#107755,#107756);
#95780=AXIS2_PLACEMENT_3D('',#140339,#107758,#107759);
#95781=AXIS2_PLACEMENT_3D('',#140348,#107760,#107761);
#95782=AXIS2_PLACEMENT_3D('',#140358,#107762,#107763);
#95783=AXIS2_PLACEMENT_3D('',#140362,#107765,#107766);
#95784=AXIS2_PLACEMENT_3D('',#140366,#107768,#107769);
#95785=AXIS2_PLACEMENT_3D('',#140369,#107771,#107772);
#95786=AXIS2_PLACEMENT_3D('',#140370,#107773,#107774);
#95787=AXIS2_PLACEMENT_3D('',#140371,#107775,#107776);
#95788=AXIS2_PLACEMENT_3D('',#140384,#107777,#107778);
#95789=AXIS2_PLACEMENT_3D('',#140386,#107779,#107780);
#95790=AXIS2_PLACEMENT_3D('',#140388,#107781,#107782);
#95791=AXIS2_PLACEMENT_3D('',#140390,#107784,#107785);
#95792=AXIS2_PLACEMENT_3D('',#140394,#107787,#107788);
#95793=AXIS2_PLACEMENT_3D('',#140401,#107792,#107793);
#95794=AXIS2_PLACEMENT_3D('',#140402,#107794,#107795);
#95795=AXIS2_PLACEMENT_3D('',#140403,#107796,#107797);
#95796=AXIS2_PLACEMENT_3D('',#140411,#107802,#107803);
#95797=AXIS2_PLACEMENT_3D('',#140414,#107804,#107805);
#95798=AXIS2_PLACEMENT_3D('',#140418,#107807,#107808);
#95799=AXIS2_PLACEMENT_3D('',#140420,#107810,#107811);
#95800=AXIS2_PLACEMENT_3D('',#140422,#107812,#107813);
#95801=AXIS2_PLACEMENT_3D('',#140426,#107815,#107816);
#95802=AXIS2_PLACEMENT_3D('',#140429,#107818,#107819);
#95803=AXIS2_PLACEMENT_3D('',#140433,#107821,#107822);
#95804=AXIS2_PLACEMENT_3D('',#140437,#107824,#107825);
#95805=AXIS2_PLACEMENT_3D('',#140438,#107826,#107827);
#95806=AXIS2_PLACEMENT_3D('',#140440,#107828,#107829);
#95807=AXIS2_PLACEMENT_3D('',#140442,#107830,#107831);
#95808=AXIS2_PLACEMENT_3D('',#140444,#107832,#107833);
#95809=AXIS2_PLACEMENT_3D('',#140446,#107834,#107835);
#95810=AXIS2_PLACEMENT_3D('',#140448,#107836,#107837);
#95811=AXIS2_PLACEMENT_3D('',#140452,#107839,#107840);
#95812=AXIS2_PLACEMENT_3D('',#140460,#107844,#107845);
#95813=AXIS2_PLACEMENT_3D('',#140464,#107847,#107848);
#95814=AXIS2_PLACEMENT_3D('',#140467,#107850,#107851);
#95815=AXIS2_PLACEMENT_3D('',#140468,#107852,#107853);
#95816=AXIS2_PLACEMENT_3D('',#140470,#107854,#107855);
#95817=AXIS2_PLACEMENT_3D('',#140472,#107857,#107858);
#95818=AXIS2_PLACEMENT_3D('',#140476,#107860,#107861);
#95819=AXIS2_PLACEMENT_3D('',#140480,#107863,#107864);
#95820=AXIS2_PLACEMENT_3D('',#140484,#107866,#107867);
#95821=AXIS2_PLACEMENT_3D('',#140488,#107869,#107870);
#95822=AXIS2_PLACEMENT_3D('',#140489,#107871,#107872);
#95823=AXIS2_PLACEMENT_3D('',#140490,#107873,#107874);
#95824=AXIS2_PLACEMENT_3D('',#140492,#107875,#107876);
#95825=AXIS2_PLACEMENT_3D('',#140494,#107877,#107878);
#95826=AXIS2_PLACEMENT_3D('',#140496,#107879,#107880);
#95827=AXIS2_PLACEMENT_3D('',#140498,#107881,#107882);
#95828=AXIS2_PLACEMENT_3D('',#140499,#107883,#107884);
#95829=AXIS2_PLACEMENT_3D('',#140503,#107886,#107887);
#95830=AXIS2_PLACEMENT_3D('',#140507,#107889,#107890);
#95831=AXIS2_PLACEMENT_3D('',#140510,#107892,#107893);
#95832=AXIS2_PLACEMENT_3D('',#140512,#107894,#107895);
#95833=AXIS2_PLACEMENT_3D('',#140514,#107896,#107897);
#95834=AXIS2_PLACEMENT_3D('',#140516,#107898,#107899);
#95835=AXIS2_PLACEMENT_3D('',#140519,#107901,#107902);
#95836=AXIS2_PLACEMENT_3D('',#140520,#107903,#107904);
#95837=AXIS2_PLACEMENT_3D('',#140526,#107908,#107909);
#95838=AXIS2_PLACEMENT_3D('',#140530,#107911,#107912);
#95839=AXIS2_PLACEMENT_3D('',#140532,#107914,#107915);
#95840=AXIS2_PLACEMENT_3D('',#140536,#107918,#107919);
#95841=AXIS2_PLACEMENT_3D('',#140539,#107921,#107922);
#95842=AXIS2_PLACEMENT_3D('',#140541,#107923,#107924);
#95843=AXIS2_PLACEMENT_3D('',#140545,#107926,#107927);
#95844=AXIS2_PLACEMENT_3D('',#140548,#107929,#107930);
#95845=AXIS2_PLACEMENT_3D('',#140550,#107931,#107932);
#95846=AXIS2_PLACEMENT_3D('',#140554,#107934,#107935);
#95847=AXIS2_PLACEMENT_3D('',#140558,#107937,#107938);
#95848=AXIS2_PLACEMENT_3D('',#140560,#107939,#107940);
#95849=AXIS2_PLACEMENT_3D('',#140564,#107942,#107943);
#95850=AXIS2_PLACEMENT_3D('',#140566,#107944,#107945);
#95851=AXIS2_PLACEMENT_3D('',#140570,#107947,#107948);
#95852=AXIS2_PLACEMENT_3D('',#140574,#107950,#107951);
#95853=AXIS2_PLACEMENT_3D('',#140577,#107953,#107954);
#95854=AXIS2_PLACEMENT_3D('',#140582,#107956,#107957);
#95855=AXIS2_PLACEMENT_3D('',#140585,#107959,#107960);
#95856=AXIS2_PLACEMENT_3D('',#140587,#107961,#107962);
#95857=AXIS2_PLACEMENT_3D('',#140589,#107963,#107964);
#95858=AXIS2_PLACEMENT_3D('',#140591,#107965,#107966);
#95859=AXIS2_PLACEMENT_3D('',#140592,#107967,#107968);
#95860=AXIS2_PLACEMENT_3D('',#140594,#107970,#107971);
#95861=AXIS2_PLACEMENT_3D('',#140602,#107974,#107975);
#95862=AXIS2_PLACEMENT_3D('',#140604,#107976,#107977);
#95863=AXIS2_PLACEMENT_3D('',#140606,#107979,#107980);
#95864=AXIS2_PLACEMENT_3D('',#140610,#107982,#107983);
#95865=AXIS2_PLACEMENT_3D('',#140612,#107985,#107986);
#95866=AXIS2_PLACEMENT_3D('',#140620,#107989,#107990);
#95867=AXIS2_PLACEMENT_3D('',#140624,#107992,#107993);
#95868=AXIS2_PLACEMENT_3D('',#140628,#107995,#107996);
#95869=AXIS2_PLACEMENT_3D('',#140634,#107999,#108000);
#95870=AXIS2_PLACEMENT_3D('',#140636,#108001,#108002);
#95871=AXIS2_PLACEMENT_3D('',#140640,#108004,#108005);
#95872=AXIS2_PLACEMENT_3D('',#140643,#108007,#108008);
#95873=AXIS2_PLACEMENT_3D('',#140644,#108009,#108010);
#95874=AXIS2_PLACEMENT_3D('',#140645,#108011,#108012);
#95875=AXIS2_PLACEMENT_3D('',#140646,#108013,#108014);
#95876=AXIS2_PLACEMENT_3D('',#140650,#108016,#108017);
#95877=AXIS2_PLACEMENT_3D('',#140652,#108019,#108020);
#95878=AXIS2_PLACEMENT_3D('',#140656,#108023,#108024);
#95879=AXIS2_PLACEMENT_3D('',#140657,#108025,#108026);
#95880=AXIS2_PLACEMENT_3D('',#140658,#108027,#108028);
#95881=AXIS2_PLACEMENT_3D('',#140660,#108029,#108030);
#95882=AXIS2_PLACEMENT_3D('',#140662,#108031,#108032);
#95883=AXIS2_PLACEMENT_3D('',#140664,#108033,#108034);
#95884=AXIS2_PLACEMENT_3D('',#140666,#108035,#108036);
#95885=AXIS2_PLACEMENT_3D('',#140667,#108037,#108038);
#95886=AXIS2_PLACEMENT_3D('',#140668,#108039,#108040);
#95887=AXIS2_PLACEMENT_3D('',#140670,#108041,#108042);
#95888=AXIS2_PLACEMENT_3D('',#140672,#108043,#108044);
#95889=AXIS2_PLACEMENT_3D('',#140675,#108046,#108047);
#95890=AXIS2_PLACEMENT_3D('',#140677,#108048,#108049);
#95891=AXIS2_PLACEMENT_3D('',#140680,#108051,#108052);
#95892=AXIS2_PLACEMENT_3D('',#140681,#108053,#108054);
#95893=AXIS2_PLACEMENT_3D('',#140683,#108056,#108057);
#95894=AXIS2_PLACEMENT_3D('',#140686,#108060,#108061);
#95895=AXIS2_PLACEMENT_3D('',#140688,#108063,#108064);
#95896=AXIS2_PLACEMENT_3D('',#140690,#108066,#108067);
#95897=AXIS2_PLACEMENT_3D('',#140693,#108070,#108071);
#95898=AXIS2_PLACEMENT_3D('',#140695,#108073,#108074);
#95899=AXIS2_PLACEMENT_3D('',#140697,#108076,#108077);
#95900=AXIS2_PLACEMENT_3D('',#140699,#108079,#108080);
#95901=AXIS2_PLACEMENT_3D('',#140701,#108082,#108083);
#95902=AXIS2_PLACEMENT_3D('',#140702,#108084,#108085);
#95903=AXIS2_PLACEMENT_3D('',#140706,#108087,#108088);
#95904=AXIS2_PLACEMENT_3D('',#140708,#108090,#108091);
#95905=AXIS2_PLACEMENT_3D('',#140711,#108093,#108094);
#95906=AXIS2_PLACEMENT_3D('',#140712,#108095,#108096);
#95907=AXIS2_PLACEMENT_3D('',#140713,#108097,#108098);
#95908=AXIS2_PLACEMENT_3D('',#140714,#108099,#108100);
#95909=AXIS2_PLACEMENT_3D('',#140718,#108102,#108103);
#95910=AXIS2_PLACEMENT_3D('',#140720,#108105,#108106);
#95911=AXIS2_PLACEMENT_3D('',#140723,#108108,#108109);
#95912=AXIS2_PLACEMENT_3D('',#140724,#108110,#108111);
#95913=AXIS2_PLACEMENT_3D('',#140728,#108114,#108115);
#95914=AXIS2_PLACEMENT_3D('',#140729,#108116,#108117);
#95915=AXIS2_PLACEMENT_3D('',#140731,#108119,#108120);
#95916=AXIS2_PLACEMENT_3D('',#140733,#108122,#108123);
#95917=AXIS2_PLACEMENT_3D('',#140735,#108125,#108126);
#95918=AXIS2_PLACEMENT_3D('',#140736,#108127,#108128);
#95919=AXIS2_PLACEMENT_3D('',#140737,#108129,#108130);
#95920=AXIS2_PLACEMENT_3D('',#140738,#108131,#108132);
#95921=AXIS2_PLACEMENT_3D('',#140739,#108133,#108134);
#95922=AXIS2_PLACEMENT_3D('',#140742,#108137,#108138);
#95923=AXIS2_PLACEMENT_3D('',#140744,#108140,#108141);
#95924=AXIS2_PLACEMENT_3D('',#140746,#108143,#108144);
#95925=AXIS2_PLACEMENT_3D('',#140748,#108146,#108147);
#95926=AXIS2_PLACEMENT_3D('',#140750,#108149,#108150);
#95927=AXIS2_PLACEMENT_3D('',#140751,#108151,#108152);
#95928=AXIS2_PLACEMENT_3D('',#140754,#108155,#108156);
#95929=AXIS2_PLACEMENT_3D('',#140756,#108158,#108159);
#95930=AXIS2_PLACEMENT_3D('',#140757,#108160,#108161);
#95931=AXIS2_PLACEMENT_3D('',#140759,#108163,#108164);
#95932=AXIS2_PLACEMENT_3D('',#140760,#108165,#108166);
#95933=AXIS2_PLACEMENT_3D('',#140762,#108168,#108169);
#95934=AXIS2_PLACEMENT_3D('',#140763,#108170,#108171);
#95935=AXIS2_PLACEMENT_3D('',#140764,#108172,#108173);
#95936=AXIS2_PLACEMENT_3D('',#140766,#108175,#108176);
#95937=AXIS2_PLACEMENT_3D('',#140772,#108180,#108181);
#95938=AXIS2_PLACEMENT_3D('',#140773,#108182,#108183);
#95939=AXIS2_PLACEMENT_3D('',#140775,#108184,#108185);
#95940=AXIS2_PLACEMENT_3D('',#140776,#108186,#108187);
#95941=AXIS2_PLACEMENT_3D('',#140778,#108188,#108189);
#95942=AXIS2_PLACEMENT_3D('',#140780,#108191,#108192);
#95943=AXIS2_PLACEMENT_3D('',#140782,#108194,#108195);
#95944=AXIS2_PLACEMENT_3D('',#140783,#108196,#108197);
#95945=AXIS2_PLACEMENT_3D('',#140784,#108198,#108199);
#95946=AXIS2_PLACEMENT_3D('',#140786,#108200,#108201);
#95947=AXIS2_PLACEMENT_3D('',#140787,#108202,#108203);
#95948=AXIS2_PLACEMENT_3D('',#140791,#108205,#108206);
#95949=AXIS2_PLACEMENT_3D('',#140793,#108208,#108209);
#95950=AXIS2_PLACEMENT_3D('',#140794,#108210,#108211);
#95951=AXIS2_PLACEMENT_3D('',#140795,#108212,#108213);
#95952=AXIS2_PLACEMENT_3D('',#140796,#108214,#108215);
#95953=AXIS2_PLACEMENT_3D('',#140797,#108216,#108217);
#95954=AXIS2_PLACEMENT_3D('',#140798,#108218,#108219);
#95955=AXIS2_PLACEMENT_3D('',#140800,#108220,#108221);
#95956=AXIS2_PLACEMENT_3D('',#140802,#108223,#108224);
#95957=AXIS2_PLACEMENT_3D('',#140803,#108225,#108226);
#95958=AXIS2_PLACEMENT_3D('',#140804,#108227,#108228);
#95959=AXIS2_PLACEMENT_3D('',#140810,#108232,#108233);
#95960=AXIS2_PLACEMENT_3D('',#140813,#108235,#108236);
#95961=AXIS2_PLACEMENT_3D('',#140814,#108237,#108238);
#95962=AXIS2_PLACEMENT_3D('',#140815,#108239,#108240);
#95963=AXIS2_PLACEMENT_3D('',#140816,#108241,#108242);
#95964=AXIS2_PLACEMENT_3D('',#140819,#108245,#108246);
#95965=AXIS2_PLACEMENT_3D('',#140821,#108248,#108249);
#95966=AXIS2_PLACEMENT_3D('',#140822,#108250,#108251);
#95967=AXIS2_PLACEMENT_3D('',#140825,#108254,#108255);
#95968=AXIS2_PLACEMENT_3D('',#140827,#108257,#108258);
#95969=AXIS2_PLACEMENT_3D('',#140829,#108260,#108261);
#95970=AXIS2_PLACEMENT_3D('',#140831,#108263,#108264);
#95971=AXIS2_PLACEMENT_3D('',#140832,#108265,#108266);
#95972=AXIS2_PLACEMENT_3D('',#140834,#108268,#108269);
#95973=AXIS2_PLACEMENT_3D('',#140836,#108271,#108272);
#95974=AXIS2_PLACEMENT_3D('',#140838,#108274,#108275);
#95975=AXIS2_PLACEMENT_3D('',#140839,#108276,#108277);
#95976=AXIS2_PLACEMENT_3D('',#140840,#108278,#108279);
#95977=AXIS2_PLACEMENT_3D('',#140841,#108280,#108281);
#95978=AXIS2_PLACEMENT_3D('',#140842,#108282,#108283);
#95979=AXIS2_PLACEMENT_3D('',#140844,#108285,#108286);
#95980=AXIS2_PLACEMENT_3D('',#140845,#108287,#108288);
#95981=AXIS2_PLACEMENT_3D('',#140846,#108289,#108290);
#95982=AXIS2_PLACEMENT_3D('',#140847,#108291,#108292);
#95983=AXIS2_PLACEMENT_3D('',#140853,#108295,#108296);
#95984=AXIS2_PLACEMENT_3D('',#140857,#108298,#108299);
#95985=AXIS2_PLACEMENT_3D('',#140860,#108301,#108302);
#95986=AXIS2_PLACEMENT_3D('',#140861,#108303,#108304);
#95987=AXIS2_PLACEMENT_3D('',#140863,#108305,#108306);
#95988=AXIS2_PLACEMENT_3D('',#140864,#108307,#108308);
#95989=AXIS2_PLACEMENT_3D('',#140865,#108309,#108310);
#95990=AXIS2_PLACEMENT_3D('',#140866,#108311,#108312);
#95991=AXIS2_PLACEMENT_3D('',#140868,#108314,#108315);
#95992=AXIS2_PLACEMENT_3D('',#140869,#108316,#108317);
#95993=AXIS2_PLACEMENT_3D('',#140870,#108318,#108319);
#95994=AXIS2_PLACEMENT_3D('',#140872,#108321,#108322);
#95995=AXIS2_PLACEMENT_3D('',#140874,#108324,#108325);
#95996=AXIS2_PLACEMENT_3D('',#140875,#108326,#108327);
#95997=AXIS2_PLACEMENT_3D('',#140876,#108328,#108329);
#95998=AXIS2_PLACEMENT_3D('',#140877,#108330,#108331);
#95999=AXIS2_PLACEMENT_3D('',#140879,#108332,#108333);
#96000=AXIS2_PLACEMENT_3D('',#140880,#108334,#108335);
#96001=AXIS2_PLACEMENT_3D('',#140882,#108336,#108337);
#96002=AXIS2_PLACEMENT_3D('',#140884,#108339,#108340);
#96003=AXIS2_PLACEMENT_3D('',#140886,#108341,#108342);
#96004=AXIS2_PLACEMENT_3D('',#140887,#108343,#108344);
#96005=AXIS2_PLACEMENT_3D('',#140889,#108346,#108347);
#96006=AXIS2_PLACEMENT_3D('',#140893,#108349,#108350);
#96007=AXIS2_PLACEMENT_3D('',#140895,#108352,#108353);
#96008=AXIS2_PLACEMENT_3D('',#140899,#108356,#108357);
#96009=AXIS2_PLACEMENT_3D('',#140902,#108359,#108360);
#96010=AXIS2_PLACEMENT_3D('',#140903,#108361,#108362);
#96011=AXIS2_PLACEMENT_3D('',#140906,#108363,#108364);
#96012=AXIS2_PLACEMENT_3D('',#140909,#108367,#108368);
#96013=AXIS2_PLACEMENT_3D('',#140913,#108371,#108372);
#96014=AXIS2_PLACEMENT_3D('',#140915,#108373,#108374);
#96015=AXIS2_PLACEMENT_3D('',#140917,#108376,#108377);
#96016=AXIS2_PLACEMENT_3D('',#140919,#108379,#108380);
#96017=AXIS2_PLACEMENT_3D('',#140921,#108381,#108382);
#96018=AXIS2_PLACEMENT_3D('',#140922,#108383,#108384);
#96019=AXIS2_PLACEMENT_3D('',#140924,#108386,#108387);
#96020=AXIS2_PLACEMENT_3D('',#140926,#108388,#108389);
#96021=AXIS2_PLACEMENT_3D('',#140928,#108391,#108392);
#96022=AXIS2_PLACEMENT_3D('',#140930,#108393,#108394);
#96023=AXIS2_PLACEMENT_3D('',#140932,#108396,#108397);
#96024=AXIS2_PLACEMENT_3D('',#140935,#108398,#108399);
#96025=AXIS2_PLACEMENT_3D('',#140938,#108402,#108403);
#96026=AXIS2_PLACEMENT_3D('',#140942,#108406,#108407);
#96027=AXIS2_PLACEMENT_3D('',#140943,#108408,#108409);
#96028=AXIS2_PLACEMENT_3D('',#140944,#108410,#108411);
#96029=AXIS2_PLACEMENT_3D('',#140945,#108412,#108413);
#96030=AXIS2_PLACEMENT_3D('',#140946,#108414,#108415);
#96031=AXIS2_PLACEMENT_3D('',#140947,#108416,#108417);
#96032=AXIS2_PLACEMENT_3D('',#140950,#108418,#108419);
#96033=AXIS2_PLACEMENT_3D('',#140955,#108422,#108423);
#96034=AXIS2_PLACEMENT_3D('',#140957,#108425,#108426);
#96035=AXIS2_PLACEMENT_3D('',#140958,#108427,#108428);
#96036=AXIS2_PLACEMENT_3D('',#140960,#108430,#108431);
#96037=AXIS2_PLACEMENT_3D('',#140962,#108433,#108434);
#96038=AXIS2_PLACEMENT_3D('',#140964,#108436,#108437);
#96039=AXIS2_PLACEMENT_3D('',#140966,#108439,#108440);
#96040=AXIS2_PLACEMENT_3D('',#140968,#108442,#108443);
#96041=AXIS2_PLACEMENT_3D('',#140970,#108445,#108446);
#96042=AXIS2_PLACEMENT_3D('',#140972,#108448,#108449);
#96043=AXIS2_PLACEMENT_3D('',#140974,#108451,#108452);
#96044=AXIS2_PLACEMENT_3D('',#140976,#108454,#108455);
#96045=AXIS2_PLACEMENT_3D('',#140977,#108456,#108457);
#96046=AXIS2_PLACEMENT_3D('',#141000,#108459,#108460);
#96047=AXIS2_PLACEMENT_3D('',#141006,#108464,#108465);
#96048=AXIS2_PLACEMENT_3D('',#141008,#108466,#108467);
#96049=AXIS2_PLACEMENT_3D('',#141009,#108468,#108469);
#96050=AXIS2_PLACEMENT_3D('',#141010,#108470,#108471);
#96051=AXIS2_PLACEMENT_3D('',#141012,#108473,#108474);
#96052=AXIS2_PLACEMENT_3D('',#141013,#108475,#108476);
#96053=AXIS2_PLACEMENT_3D('',#141016,#108477,#108478);
#96054=AXIS2_PLACEMENT_3D('',#141020,#108480,#108481);
#96055=AXIS2_PLACEMENT_3D('',#141022,#108483,#108484);
#96056=AXIS2_PLACEMENT_3D('',#141024,#108485,#108486);
#96057=AXIS2_PLACEMENT_3D('',#141026,#108487,#108488);
#96058=AXIS2_PLACEMENT_3D('',#141030,#108490,#108491);
#96059=AXIS2_PLACEMENT_3D('',#141034,#108493,#108494);
#96060=AXIS2_PLACEMENT_3D('',#141036,#108495,#108496);
#96061=AXIS2_PLACEMENT_3D('',#141038,#108497,#108498);
#96062=AXIS2_PLACEMENT_3D('',#141042,#108500,#108501);
#96063=AXIS2_PLACEMENT_3D('',#141046,#108503,#108504);
#96064=AXIS2_PLACEMENT_3D('',#141050,#108506,#108507);
#96065=AXIS2_PLACEMENT_3D('',#141054,#108509,#108510);
#96066=AXIS2_PLACEMENT_3D('',#141058,#108512,#108513);
#96067=AXIS2_PLACEMENT_3D('',#141060,#108515,#108516);
#96068=AXIS2_PLACEMENT_3D('',#141062,#108517,#108518);
#96069=AXIS2_PLACEMENT_3D('',#141064,#108520,#108521);
#96070=AXIS2_PLACEMENT_3D('',#141066,#108522,#108523);
#96071=AXIS2_PLACEMENT_3D('',#141068,#108525,#108526);
#96072=AXIS2_PLACEMENT_3D('',#141076,#108531,#108532);
#96073=AXIS2_PLACEMENT_3D('',#141079,#108533,#108534);
#96074=AXIS2_PLACEMENT_3D('',#141081,#108535,#108536);
#96075=AXIS2_PLACEMENT_3D('',#141083,#108537,#108538);
#96076=AXIS2_PLACEMENT_3D('',#141084,#108539,#108540);
#96077=AXIS2_PLACEMENT_3D('',#141101,#108541,#108542);
#96078=AXIS2_PLACEMENT_3D('',#141102,#108543,#108544);
#96079=AXIS2_PLACEMENT_3D('',#141103,#108545,#108546);
#96080=AXIS2_PLACEMENT_3D('',#141104,#108547,#108548);
#96081=AXIS2_PLACEMENT_3D('',#141106,#108549,#108550);
#96082=AXIS2_PLACEMENT_3D('',#141119,#108552,#108553);
#96083=AXIS2_PLACEMENT_3D('',#141120,#108554,#108555);
#96084=AXIS2_PLACEMENT_3D('',#141121,#108556,#108557);
#96085=AXIS2_PLACEMENT_3D('',#141122,#108558,#108559);
#96086=AXIS2_PLACEMENT_3D('',#141125,#108560,#108561);
#96087=AXIS2_PLACEMENT_3D('',#141145,#108564,#108565);
#96088=AXIS2_PLACEMENT_3D('',#141146,#108566,#108567);
#96089=AXIS2_PLACEMENT_3D('',#141147,#108568,#108569);
#96090=AXIS2_PLACEMENT_3D('',#141148,#108570,#108571);
#96091=AXIS2_PLACEMENT_3D('',#141151,#108572,#108573);
#96092=AXIS2_PLACEMENT_3D('',#141152,#108574,#108575);
#96093=AXIS2_PLACEMENT_3D('',#141153,#108576,#108577);
#96094=AXIS2_PLACEMENT_3D('',#141169,#108578,#108579);
#96095=AXIS2_PLACEMENT_3D('',#141170,#108580,#108581);
#96096=AXIS2_PLACEMENT_3D('',#141171,#108582,#108583);
#96097=AXIS2_PLACEMENT_3D('',#141175,#108585,#108586);
#96098=AXIS2_PLACEMENT_3D('',#141177,#108588,#108589);
#96099=AXIS2_PLACEMENT_3D('',#141180,#108591,#108592);
#96100=AXIS2_PLACEMENT_3D('',#141181,#108593,#108594);
#96101=AXIS2_PLACEMENT_3D('',#141184,#108596,#108597);
#96102=AXIS2_PLACEMENT_3D('',#141185,#108598,#108599);
#96103=AXIS2_PLACEMENT_3D('',#141189,#108601,#108602);
#96104=AXIS2_PLACEMENT_3D('',#141192,#108604,#108605);
#96105=AXIS2_PLACEMENT_3D('',#141193,#108606,#108607);
#96106=AXIS2_PLACEMENT_3D('',#141194,#108608,#108609);
#96107=AXIS2_PLACEMENT_3D('',#141197,#108610,#108611);
#96108=AXIS2_PLACEMENT_3D('',#141199,#108612,#108613);
#96109=AXIS2_PLACEMENT_3D('',#141201,#108614,#108615);
#96110=AXIS2_PLACEMENT_3D('',#141216,#108616,#108617);
#96111=AXIS2_PLACEMENT_3D('',#141219,#108618,#108619);
#96112=AXIS2_PLACEMENT_3D('',#141221,#108620,#108621);
#96113=AXIS2_PLACEMENT_3D('',#141223,#108622,#108623);
#96114=AXIS2_PLACEMENT_3D('',#141238,#108624,#108625);
#96115=AXIS2_PLACEMENT_3D('',#141241,#108626,#108627);
#96116=AXIS2_PLACEMENT_3D('',#141244,#108630,#108631);
#96117=AXIS2_PLACEMENT_3D('',#141245,#108632,#108633);
#96118=AXIS2_PLACEMENT_3D('',#141246,#108634,#108635);
#96119=AXIS2_PLACEMENT_3D('',#141247,#108636,#108637);
#96120=AXIS2_PLACEMENT_3D('',#141250,#108638,#108639);
#96121=AXIS2_PLACEMENT_3D('',#141252,#108640,#108641);
#96122=AXIS2_PLACEMENT_3D('',#141254,#108642,#108643);
#96123=AXIS2_PLACEMENT_3D('',#141269,#108644,#108645);
#96124=AXIS2_PLACEMENT_3D('',#141270,#108646,#108647);
#96125=AXIS2_PLACEMENT_3D('',#141271,#108648,#108649);
#96126=AXIS2_PLACEMENT_3D('',#141272,#108650,#108651);
#96127=AXIS2_PLACEMENT_3D('',#141274,#108652,#108653);
#96128=AXIS2_PLACEMENT_3D('',#141276,#108654,#108655);
#96129=AXIS2_PLACEMENT_3D('',#141293,#108656,#108657);
#96130=AXIS2_PLACEMENT_3D('',#141296,#108660,#108661);
#96131=AXIS2_PLACEMENT_3D('',#141300,#108663,#108664);
#96132=AXIS2_PLACEMENT_3D('',#141302,#108666,#108667);
#96133=AXIS2_PLACEMENT_3D('',#141305,#108669,#108670);
#96134=AXIS2_PLACEMENT_3D('',#141306,#108671,#108672);
#96135=AXIS2_PLACEMENT_3D('',#141310,#108675,#108676);
#96136=AXIS2_PLACEMENT_3D('',#141313,#108678,#108679);
#96137=AXIS2_PLACEMENT_3D('',#141314,#108680,#108681);
#96138=AXIS2_PLACEMENT_3D('',#141315,#108682,#108683);
#96139=AXIS2_PLACEMENT_3D('',#141331,#108684,#108685);
#96140=AXIS2_PLACEMENT_3D('',#141333,#108686,#108687);
#96141=AXIS2_PLACEMENT_3D('',#141335,#108688,#108689);
#96142=AXIS2_PLACEMENT_3D('',#141361,#108690,#108691);
#96143=AXIS2_PLACEMENT_3D('',#141362,#108692,#108693);
#96144=AXIS2_PLACEMENT_3D('',#141363,#108694,#108695);
#96145=AXIS2_PLACEMENT_3D('',#141364,#108696,#108697);
#96146=AXIS2_PLACEMENT_3D('',#141374,#108698,#108699);
#96147=AXIS2_PLACEMENT_3D('',#141390,#108700,#108701);
#96148=AXIS2_PLACEMENT_3D('',#141392,#108702,#108703);
#96149=AXIS2_PLACEMENT_3D('',#141399,#108704,#108705);
#96150=AXIS2_PLACEMENT_3D('',#141417,#108709,#108710);
#96151=AXIS2_PLACEMENT_3D('',#141455,#108713,#108714);
#96152=AXIS2_PLACEMENT_3D('',#141470,#108716,#108717);
#96153=AXIS2_PLACEMENT_3D('',#141474,#108719,#108720);
#96154=AXIS2_PLACEMENT_3D('',#141507,#108721,#108722);
#96155=AXIS2_PLACEMENT_3D('',#141508,#108723,#108724);
#96156=AXIS2_PLACEMENT_3D('',#141512,#108726,#108727);
#96157=AXIS2_PLACEMENT_3D('',#141514,#108729,#108730);
#96158=AXIS2_PLACEMENT_3D('',#141519,#108733,#108734);
#96159=AXIS2_PLACEMENT_3D('',#141520,#108735,#108736);
#96160=AXIS2_PLACEMENT_3D('',#141522,#108737,#108738);
#96161=AXIS2_PLACEMENT_3D('',#141546,#108742,#108743);
#96162=AXIS2_PLACEMENT_3D('',#141557,#108744,#108745);
#96163=AXIS2_PLACEMENT_3D('',#141558,#108746,#108747);
#96164=AXIS2_PLACEMENT_3D('',#141559,#108748,#108749);
#96165=AXIS2_PLACEMENT_3D('',#141561,#108751,#108752);
#96166=AXIS2_PLACEMENT_3D('',#141565,#108754,#108755);
#96167=AXIS2_PLACEMENT_3D('',#141567,#108756,#108757);
#96168=AXIS2_PLACEMENT_3D('',#141574,#108759,#108760);
#96169=AXIS2_PLACEMENT_3D('',#141575,#108761,#108762);
#96170=AXIS2_PLACEMENT_3D('',#141592,#108764,#108765);
#96171=AXIS2_PLACEMENT_3D('',#141594,#108766,#108767);
#96172=AXIS2_PLACEMENT_3D('',#141617,#108778,#108779);
#96173=AXIS2_PLACEMENT_3D('',#141621,#108781,#108782);
#96174=AXIS2_PLACEMENT_3D('',#141623,#108784,#108785);
#96175=AXIS2_PLACEMENT_3D('',#141625,#108786,#108787);
#96176=AXIS2_PLACEMENT_3D('',#141628,#108790,#108791);
#96177=AXIS2_PLACEMENT_3D('',#141634,#108793,#108794);
#96178=AXIS2_PLACEMENT_3D('',#141638,#108797,#108798);
#96179=AXIS2_PLACEMENT_3D('',#141641,#108799,#108800);
#96180=AXIS2_PLACEMENT_3D('',#141643,#108801,#108802);
#96181=AXIS2_PLACEMENT_3D('',#141645,#108803,#108804);
#96182=AXIS2_PLACEMENT_3D('',#141679,#108805,#108806);
#96183=AXIS2_PLACEMENT_3D('',#141680,#108807,#108808);
#96184=AXIS2_PLACEMENT_3D('',#141681,#108809,#108810);
#96185=AXIS2_PLACEMENT_3D('',#141682,#108811,#108812);
#96186=AXIS2_PLACEMENT_3D('',#141685,#108813,#108814);
#96187=AXIS2_PLACEMENT_3D('',#141686,#108815,#108816);
#96188=AXIS2_PLACEMENT_3D('',#141687,#108817,#108818);
#96189=AXIS2_PLACEMENT_3D('',#141699,#108819,#108820);
#96190=AXIS2_PLACEMENT_3D('',#141700,#108821,#108822);
#96191=AXIS2_PLACEMENT_3D('',#141701,#108823,#108824);
#96192=AXIS2_PLACEMENT_3D('',#141702,#108825,#108826);
#96193=AXIS2_PLACEMENT_3D('',#141707,#108829,#108830);
#96194=AXIS2_PLACEMENT_3D('',#141708,#108831,#108832);
#96195=AXIS2_PLACEMENT_3D('',#141711,#108835,#108836);
#96196=AXIS2_PLACEMENT_3D('',#141715,#108838,#108839);
#96197=AXIS2_PLACEMENT_3D('',#141721,#108843,#108844);
#96198=AXIS2_PLACEMENT_3D('',#141743,#108848,#108849);
#96199=AXIS2_PLACEMENT_3D('',#141746,#108851,#108852);
#96200=AXIS2_PLACEMENT_3D('',#141747,#108853,#108854);
#96201=AXIS2_PLACEMENT_3D('',#141748,#108855,#108856);
#96202=AXIS2_PLACEMENT_3D('',#141756,#108857,#108858);
#96203=AXIS2_PLACEMENT_3D('',#141778,#108859,#108860);
#96204=AXIS2_PLACEMENT_3D('',#141821,#108861,#108862);
#96205=AXIS2_PLACEMENT_3D('',#141822,#108863,#108864);
#96206=AXIS2_PLACEMENT_3D('',#141823,#108865,#108866);
#96207=AXIS2_PLACEMENT_3D('',#141825,#108867,#108868);
#96208=AXIS2_PLACEMENT_3D('',#141826,#108869,#108870);
#96209=AXIS2_PLACEMENT_3D('',#141827,#108871,#108872);
#96210=AXIS2_PLACEMENT_3D('',#141829,#108873,#108874);
#96211=AXIS2_PLACEMENT_3D('',#141831,#108875,#108876);
#96212=AXIS2_PLACEMENT_3D('',#141832,#108877,#108878);
#96213=AXIS2_PLACEMENT_3D('',#141833,#108879,#108880);
#96214=AXIS2_PLACEMENT_3D('',#141835,#108881,#108882);
#96215=AXIS2_PLACEMENT_3D('',#141837,#108883,#108884);
#96216=AXIS2_PLACEMENT_3D('',#141841,#108886,#108887);
#96217=AXIS2_PLACEMENT_3D('',#141845,#108889,#108890);
#96218=AXIS2_PLACEMENT_3D('',#141847,#108892,#108893);
#96219=AXIS2_PLACEMENT_3D('',#141849,#108894,#108895);
#96220=AXIS2_PLACEMENT_3D('',#141861,#108897,#108898);
#96221=AXIS2_PLACEMENT_3D('',#141862,#108899,#108900);
#96222=AXIS2_PLACEMENT_3D('',#141863,#108901,#108902);
#96223=AXIS2_PLACEMENT_3D('',#141865,#108903,#108904);
#96224=AXIS2_PLACEMENT_3D('',#141877,#108906,#108907);
#96225=AXIS2_PLACEMENT_3D('',#141878,#108908,#108909);
#96226=AXIS2_PLACEMENT_3D('',#141879,#108910,#108911);
#96227=AXIS2_PLACEMENT_3D('',#141881,#108912,#108913);
#96228=AXIS2_PLACEMENT_3D('',#141893,#108915,#108916);
#96229=AXIS2_PLACEMENT_3D('',#141894,#108917,#108918);
#96230=AXIS2_PLACEMENT_3D('',#141895,#108919,#108920);
#96231=AXIS2_PLACEMENT_3D('',#141896,#108921,#108922);
#96232=AXIS2_PLACEMENT_3D('',#141897,#108923,#108924);
#96233=AXIS2_PLACEMENT_3D('',#141901,#108926,#108927);
#96234=AXIS2_PLACEMENT_3D('',#141913,#108929,#108930);
#96235=AXIS2_PLACEMENT_3D('',#141916,#108932,#108933);
#96236=AXIS2_PLACEMENT_3D('',#141917,#108934,#108935);
#96237=AXIS2_PLACEMENT_3D('',#141920,#108937,#108938);
#96238=AXIS2_PLACEMENT_3D('',#141921,#108939,#108940);
#96239=AXIS2_PLACEMENT_3D('',#141925,#108943,#108944);
#96240=AXIS2_PLACEMENT_3D('',#141928,#108946,#108947);
#96241=AXIS2_PLACEMENT_3D('',#141929,#108948,#108949);
#96242=AXIS2_PLACEMENT_3D('',#141933,#108952,#108953);
#96243=AXIS2_PLACEMENT_3D('',#141936,#108955,#108956);
#96244=AXIS2_PLACEMENT_3D('',#141937,#108957,#108958);
#96245=AXIS2_PLACEMENT_3D('',#141941,#108961,#108962);
#96246=AXIS2_PLACEMENT_3D('',#141944,#108964,#108965);
#96247=AXIS2_PLACEMENT_3D('',#141945,#108966,#108967);
#96248=AXIS2_PLACEMENT_3D('',#141972,#108968,#108969);
#96249=AXIS2_PLACEMENT_3D('',#141976,#108971,#108972);
#96250=AXIS2_PLACEMENT_3D('',#141980,#108974,#108975);
#96251=AXIS2_PLACEMENT_3D('',#142029,#108977,#108978);
#96252=AXIS2_PLACEMENT_3D('',#142030,#108979,#108980);
#96253=AXIS2_PLACEMENT_3D('',#142031,#108981,#108982);
#96254=AXIS2_PLACEMENT_3D('',#142034,#108983,#108984);
#96255=AXIS2_PLACEMENT_3D('',#142036,#108985,#108986);
#96256=AXIS2_PLACEMENT_3D('',#142038,#108987,#108988);
#96257=AXIS2_PLACEMENT_3D('',#142039,#108989,#108990);
#96258=AXIS2_PLACEMENT_3D('',#142057,#108991,#108992);
#96259=AXIS2_PLACEMENT_3D('',#142058,#108993,#108994);
#96260=AXIS2_PLACEMENT_3D('',#142059,#108995,#108996);
#96261=AXIS2_PLACEMENT_3D('',#142060,#108997,#108998);
#96262=AXIS2_PLACEMENT_3D('',#142063,#108999,#109000);
#96263=AXIS2_PLACEMENT_3D('',#142066,#109003,#109004);
#96264=AXIS2_PLACEMENT_3D('',#142069,#109005,#109006);
#96265=AXIS2_PLACEMENT_3D('',#142070,#109007,#109008);
#96266=AXIS2_PLACEMENT_3D('',#142071,#109009,#109010);
#96267=AXIS2_PLACEMENT_3D('',#142072,#109011,#109012);
#96268=AXIS2_PLACEMENT_3D('',#142075,#109013,#109014);
#96269=AXIS2_PLACEMENT_3D('',#142095,#109017,#109018);
#96270=AXIS2_PLACEMENT_3D('',#142096,#109019,#109020);
#96271=AXIS2_PLACEMENT_3D('',#142097,#109021,#109022);
#96272=AXIS2_PLACEMENT_3D('',#142098,#109023,#109024);
#96273=AXIS2_PLACEMENT_3D('',#142101,#109025,#109026);
#96274=AXIS2_PLACEMENT_3D('',#142103,#109027,#109028);
#96275=AXIS2_PLACEMENT_3D('',#142105,#109029,#109030);
#96276=AXIS2_PLACEMENT_3D('',#142106,#109031,#109032);
#96277=AXIS2_PLACEMENT_3D('',#142124,#109033,#109034);
#96278=AXIS2_PLACEMENT_3D('',#142125,#109035,#109036);
#96279=AXIS2_PLACEMENT_3D('',#142126,#109037,#109038);
#96280=AXIS2_PLACEMENT_3D('',#142127,#109039,#109040);
#96281=AXIS2_PLACEMENT_3D('',#142130,#109041,#109042);
#96282=AXIS2_PLACEMENT_3D('',#142131,#109043,#109044);
#96283=AXIS2_PLACEMENT_3D('',#142132,#109045,#109046);
#96284=AXIS2_PLACEMENT_3D('',#142133,#109047,#109048);
#96285=AXIS2_PLACEMENT_3D('',#142135,#109049,#109050);
#96286=AXIS2_PLACEMENT_3D('',#142138,#109053,#109054);
#96287=AXIS2_PLACEMENT_3D('',#142139,#109055,#109056);
#96288=AXIS2_PLACEMENT_3D('',#142140,#109057,#109058);
#96289=AXIS2_PLACEMENT_3D('',#142141,#109059,#109060);
#96290=AXIS2_PLACEMENT_3D('',#142142,#109061,#109062);
#96291=AXIS2_PLACEMENT_3D('',#142143,#109063,#109064);
#96292=AXIS2_PLACEMENT_3D('',#142149,#109068,#109069);
#96293=AXIS2_PLACEMENT_3D('',#142152,#109071,#109072);
#96294=AXIS2_PLACEMENT_3D('',#142153,#109073,#109074);
#96295=AXIS2_PLACEMENT_3D('',#142157,#109077,#109078);
#96296=AXIS2_PLACEMENT_3D('',#142160,#109080,#109081);
#96297=AXIS2_PLACEMENT_3D('',#142161,#109082,#109083);
#96298=AXIS2_PLACEMENT_3D('',#142164,#109085,#109086);
#96299=AXIS2_PLACEMENT_3D('',#142165,#109087,#109088);
#96300=AXIS2_PLACEMENT_3D('',#142168,#109090,#109091);
#96301=AXIS2_PLACEMENT_3D('',#142169,#109092,#109093);
#96302=AXIS2_PLACEMENT_3D('',#142170,#109094,#109095);
#96303=AXIS2_PLACEMENT_3D('',#142173,#109096,#109097);
#96304=AXIS2_PLACEMENT_3D('',#142177,#109099,#109100);
#96305=AXIS2_PLACEMENT_3D('',#142190,#109102,#109103);
#96306=AXIS2_PLACEMENT_3D('',#142191,#109104,#109105);
#96307=AXIS2_PLACEMENT_3D('',#142192,#109106,#109107);
#96308=AXIS2_PLACEMENT_3D('',#142193,#109108,#109109);
#96309=AXIS2_PLACEMENT_3D('',#142196,#109110,#109111);
#96310=AXIS2_PLACEMENT_3D('',#142199,#109114,#109115);
#96311=AXIS2_PLACEMENT_3D('',#142202,#109116,#109117);
#96312=AXIS2_PLACEMENT_3D('',#142203,#109118,#109119);
#96313=AXIS2_PLACEMENT_3D('',#142204,#109120,#109121);
#96314=AXIS2_PLACEMENT_3D('',#142222,#109122,#109123);
#96315=AXIS2_PLACEMENT_3D('',#142223,#109124,#109125);
#96316=AXIS2_PLACEMENT_3D('',#142224,#109126,#109127);
#96317=AXIS2_PLACEMENT_3D('',#142225,#109128,#109129);
#96318=AXIS2_PLACEMENT_3D('',#142228,#109130,#109131);
#96319=AXIS2_PLACEMENT_3D('',#142231,#109134,#109135);
#96320=AXIS2_PLACEMENT_3D('',#142234,#109136,#109137);
#96321=AXIS2_PLACEMENT_3D('',#142235,#109138,#109139);
#96322=AXIS2_PLACEMENT_3D('',#142236,#109140,#109141);
#96323=AXIS2_PLACEMENT_3D('',#142254,#109142,#109143);
#96324=AXIS2_PLACEMENT_3D('',#142255,#109144,#109145);
#96325=AXIS2_PLACEMENT_3D('',#142256,#109146,#109147);
#96326=AXIS2_PLACEMENT_3D('',#142257,#109148,#109149);
#96327=AXIS2_PLACEMENT_3D('',#142260,#109150,#109151);
#96328=AXIS2_PLACEMENT_3D('',#142261,#109152,#109153);
#96329=AXIS2_PLACEMENT_3D('',#142262,#109154,#109155);
#96330=AXIS2_PLACEMENT_3D('',#142274,#109156,#109157);
#96331=AXIS2_PLACEMENT_3D('',#142275,#109158,#109159);
#96332=AXIS2_PLACEMENT_3D('',#142276,#109160,#109161);
#96333=AXIS2_PLACEMENT_3D('',#142277,#109162,#109163);
#96334=AXIS2_PLACEMENT_3D('',#142280,#109164,#109165);
#96335=AXIS2_PLACEMENT_3D('',#142292,#109168,#109169);
#96336=AXIS2_PLACEMENT_3D('',#142293,#109170,#109171);
#96337=AXIS2_PLACEMENT_3D('',#142294,#109172,#109173);
#96338=AXIS2_PLACEMENT_3D('',#142298,#109175,#109176);
#96339=AXIS2_PLACEMENT_3D('',#142300,#109178,#109179);
#96340=AXIS2_PLACEMENT_3D('',#142303,#109181,#109182);
#96341=AXIS2_PLACEMENT_3D('',#142304,#109183,#109184);
#96342=AXIS2_PLACEMENT_3D('',#142307,#109186,#109187);
#96343=AXIS2_PLACEMENT_3D('',#142308,#109188,#109189);
#96344=AXIS2_PLACEMENT_3D('',#142312,#109192,#109193);
#96345=AXIS2_PLACEMENT_3D('',#142315,#109195,#109196);
#96346=AXIS2_PLACEMENT_3D('',#142316,#109197,#109198);
#96347=AXIS2_PLACEMENT_3D('',#142320,#109201,#109202);
#96348=AXIS2_PLACEMENT_3D('',#142321,#109203,#109204);
#96349=AXIS2_PLACEMENT_3D('',#142324,#109205,#109206);
#96350=AXIS2_PLACEMENT_3D('',#142328,#109208,#109209);
#96351=AXIS2_PLACEMENT_3D('',#142341,#109211,#109212);
#96352=AXIS2_PLACEMENT_3D('',#142342,#109213,#109214);
#96353=AXIS2_PLACEMENT_3D('',#142343,#109215,#109216);
#96354=AXIS2_PLACEMENT_3D('',#142344,#109217,#109218);
#96355=AXIS2_PLACEMENT_3D('',#142347,#109219,#109220);
#96356=AXIS2_PLACEMENT_3D('',#142361,#109223,#109224);
#96357=AXIS2_PLACEMENT_3D('',#142362,#109225,#109226);
#96358=AXIS2_PLACEMENT_3D('',#142363,#109227,#109228);
#96359=AXIS2_PLACEMENT_3D('',#142364,#109229,#109230);
#96360=AXIS2_PLACEMENT_3D('',#142367,#109231,#109232);
#96361=AXIS2_PLACEMENT_3D('',#142370,#109235,#109236);
#96362=AXIS2_PLACEMENT_3D('',#142373,#109237,#109238);
#96363=AXIS2_PLACEMENT_3D('',#142374,#109239,#109240);
#96364=AXIS2_PLACEMENT_3D('',#142375,#109241,#109242);
#96365=AXIS2_PLACEMENT_3D('',#142376,#109243,#109244);
#96366=AXIS2_PLACEMENT_3D('',#142379,#109245,#109246);
#96367=AXIS2_PLACEMENT_3D('',#142380,#109247,#109248);
#96368=AXIS2_PLACEMENT_3D('',#142381,#109249,#109250);
#96369=AXIS2_PLACEMENT_3D('',#142399,#109251,#109252);
#96370=AXIS2_PLACEMENT_3D('',#142400,#109253,#109254);
#96371=AXIS2_PLACEMENT_3D('',#142401,#109255,#109256);
#96372=AXIS2_PLACEMENT_3D('',#142402,#109257,#109258);
#96373=AXIS2_PLACEMENT_3D('',#142405,#109259,#109260);
#96374=AXIS2_PLACEMENT_3D('',#142406,#109261,#109262);
#96375=AXIS2_PLACEMENT_3D('',#142407,#109263,#109264);
#96376=AXIS2_PLACEMENT_3D('',#142408,#109265,#109266);
#96377=AXIS2_PLACEMENT_3D('',#142411,#109267,#109268);
#96378=AXIS2_PLACEMENT_3D('',#142412,#109269,#109270);
#96379=AXIS2_PLACEMENT_3D('',#142413,#109271,#109272);
#96380=AXIS2_PLACEMENT_3D('',#142423,#109273,#109274);
#96381=AXIS2_PLACEMENT_3D('',#142424,#109275,#109276);
#96382=AXIS2_PLACEMENT_3D('',#142425,#109277,#109278);
#96383=AXIS2_PLACEMENT_3D('',#142429,#109280,#109281);
#96384=AXIS2_PLACEMENT_3D('',#142431,#109283,#109284);
#96385=AXIS2_PLACEMENT_3D('',#142434,#109286,#109287);
#96386=AXIS2_PLACEMENT_3D('',#142435,#109288,#109289);
#96387=AXIS2_PLACEMENT_3D('',#142439,#109291,#109292);
#96388=AXIS2_PLACEMENT_3D('',#142442,#109294,#109295);
#96389=AXIS2_PLACEMENT_3D('',#142443,#109296,#109297);
#96390=AXIS2_PLACEMENT_3D('',#142447,#109299,#109300);
#96391=AXIS2_PLACEMENT_3D('',#142520,#109302,#109303);
#96392=AXIS2_PLACEMENT_3D('',#142523,#109305,#109306);
#96393=AXIS2_PLACEMENT_3D('',#142524,#109307,#109308);
#96394=AXIS2_PLACEMENT_3D('',#142527,#109310,#109311);
#96395=AXIS2_PLACEMENT_3D('',#142528,#109312,#109313);
#96396=AXIS2_PLACEMENT_3D('',#142532,#109316,#109317);
#96397=AXIS2_PLACEMENT_3D('',#142533,#109318,#109319);
#96398=AXIS2_PLACEMENT_3D('',#142536,#109320,#109321);
#96399=AXIS2_PLACEMENT_3D('',#142538,#109322,#109323);
#96400=AXIS2_PLACEMENT_3D('',#142540,#109324,#109325);
#96401=AXIS2_PLACEMENT_3D('',#142572,#109326,#109327);
#96402=AXIS2_PLACEMENT_3D('',#142573,#109328,#109329);
#96403=AXIS2_PLACEMENT_3D('',#142574,#109330,#109331);
#96404=AXIS2_PLACEMENT_3D('',#142575,#109332,#109333);
#96405=AXIS2_PLACEMENT_3D('',#142578,#109334,#109335);
#96406=AXIS2_PLACEMENT_3D('',#142579,#109336,#109337);
#96407=AXIS2_PLACEMENT_3D('',#142580,#109338,#109339);
#96408=AXIS2_PLACEMENT_3D('',#142598,#109340,#109341);
#96409=AXIS2_PLACEMENT_3D('',#142599,#109342,#109343);
#96410=AXIS2_PLACEMENT_3D('',#142600,#109344,#109345);
#96411=AXIS2_PLACEMENT_3D('',#142601,#109346,#109347);
#96412=AXIS2_PLACEMENT_3D('',#142606,#109350,#109351);
#96413=AXIS2_PLACEMENT_3D('',#142607,#109352,#109353);
#96414=AXIS2_PLACEMENT_3D('',#142616,#109356,#109357);
#96415=AXIS2_PLACEMENT_3D('',#142617,#109358,#109359);
#96416=AXIS2_PLACEMENT_3D('',#142621,#109361,#109362);
#96417=AXIS2_PLACEMENT_3D('',#142623,#109364,#109365);
#96418=AXIS2_PLACEMENT_3D('',#142625,#109366,#109367);
#96419=AXIS2_PLACEMENT_3D('',#142629,#109369,#109370);
#96420=AXIS2_PLACEMENT_3D('',#142635,#109373,#109374);
#96421=AXIS2_PLACEMENT_3D('',#142637,#109376,#109377);
#96422=AXIS2_PLACEMENT_3D('',#142657,#109379,#109380);
#96423=AXIS2_PLACEMENT_3D('',#142658,#109381,#109382);
#96424=AXIS2_PLACEMENT_3D('',#142662,#109384,#109385);
#96425=AXIS2_PLACEMENT_3D('',#142709,#109388,#109389);
#96426=AXIS2_PLACEMENT_3D('',#142726,#109392,#109393);
#96427=AXIS2_PLACEMENT_3D('',#142729,#109394,#109395);
#96428=AXIS2_PLACEMENT_3D('',#142733,#109397,#109398);
#96429=AXIS2_PLACEMENT_3D('',#142735,#109400,#109401);
#96430=AXIS2_PLACEMENT_3D('',#142738,#109402,#109403);
#96431=AXIS2_PLACEMENT_3D('',#142739,#109404,#109405);
#96432=AXIS2_PLACEMENT_3D('',#142740,#109406,#109407);
#96433=AXIS2_PLACEMENT_3D('',#142741,#109408,#109409);
#96434=AXIS2_PLACEMENT_3D('',#142744,#109410,#109411);
#96435=AXIS2_PLACEMENT_3D('',#142764,#109414,#109415);
#96436=AXIS2_PLACEMENT_3D('',#142765,#109416,#109417);
#96437=AXIS2_PLACEMENT_3D('',#142766,#109418,#109419);
#96438=AXIS2_PLACEMENT_3D('',#142767,#109420,#109421);
#96439=AXIS2_PLACEMENT_3D('',#142770,#109422,#109423);
#96440=AXIS2_PLACEMENT_3D('',#142771,#109424,#109425);
#96441=AXIS2_PLACEMENT_3D('',#142772,#109426,#109427);
#96442=AXIS2_PLACEMENT_3D('',#142790,#109428,#109429);
#96443=AXIS2_PLACEMENT_3D('',#142791,#109430,#109431);
#96444=AXIS2_PLACEMENT_3D('',#142792,#109432,#109433);
#96445=AXIS2_PLACEMENT_3D('',#142793,#109434,#109435);
#96446=AXIS2_PLACEMENT_3D('',#142796,#109436,#109437);
#96447=AXIS2_PLACEMENT_3D('',#142810,#109440,#109441);
#96448=AXIS2_PLACEMENT_3D('',#142811,#109442,#109443);
#96449=AXIS2_PLACEMENT_3D('',#142812,#109444,#109445);
#96450=AXIS2_PLACEMENT_3D('',#142813,#109446,#109447);
#96451=AXIS2_PLACEMENT_3D('',#142816,#109448,#109449);
#96452=AXIS2_PLACEMENT_3D('',#142818,#109450,#109451);
#96453=AXIS2_PLACEMENT_3D('',#142819,#109452,#109453);
#96454=AXIS2_PLACEMENT_3D('',#142820,#109454,#109455);
#96455=AXIS2_PLACEMENT_3D('',#142832,#109456,#109457);
#96456=AXIS2_PLACEMENT_3D('',#142833,#109458,#109459);
#96457=AXIS2_PLACEMENT_3D('',#142834,#109460,#109461);
#96458=AXIS2_PLACEMENT_3D('',#142835,#109462,#109463);
#96459=AXIS2_PLACEMENT_3D('',#142838,#109464,#109465);
#96460=AXIS2_PLACEMENT_3D('',#142856,#109468,#109469);
#96461=AXIS2_PLACEMENT_3D('',#142857,#109470,#109471);
#96462=AXIS2_PLACEMENT_3D('',#142858,#109472,#109473);
#96463=AXIS2_PLACEMENT_3D('',#142862,#109475,#109476);
#96464=AXIS2_PLACEMENT_3D('',#142864,#109478,#109479);
#96465=AXIS2_PLACEMENT_3D('',#142866,#109480,#109481);
#96466=AXIS2_PLACEMENT_3D('',#142871,#109484,#109485);
#96467=AXIS2_PLACEMENT_3D('',#142875,#109487,#109488);
#96468=AXIS2_PLACEMENT_3D('',#142879,#109490,#109491);
#96469=AXIS2_PLACEMENT_3D('',#142883,#109493,#109494);
#96470=AXIS2_PLACEMENT_3D('',#142886,#109496,#109497);
#96471=AXIS2_PLACEMENT_3D('',#142887,#109498,#109499);
#96472=AXIS2_PLACEMENT_3D('',#142890,#109501,#109502);
#96473=AXIS2_PLACEMENT_3D('',#142891,#109503,#109504);
#96474=AXIS2_PLACEMENT_3D('',#142895,#109507,#109508);
#96475=AXIS2_PLACEMENT_3D('',#142898,#109510,#109511);
#96476=AXIS2_PLACEMENT_3D('',#142899,#109512,#109513);
#96477=AXIS2_PLACEMENT_3D('',#142903,#109516,#109517);
#96478=AXIS2_PLACEMENT_3D('',#142904,#109518,#109519);
#96479=AXIS2_PLACEMENT_3D('',#142907,#109520,#109521);
#96480=AXIS2_PLACEMENT_3D('',#142909,#109522,#109523);
#96481=AXIS2_PLACEMENT_3D('',#142911,#109524,#109525);
#96482=AXIS2_PLACEMENT_3D('',#142937,#109526,#109527);
#96483=AXIS2_PLACEMENT_3D('',#142938,#109528,#109529);
#96484=AXIS2_PLACEMENT_3D('',#142939,#109530,#109531);
#96485=AXIS2_PLACEMENT_3D('',#142940,#109532,#109533);
#96486=AXIS2_PLACEMENT_3D('',#142943,#109534,#109535);
#96487=AXIS2_PLACEMENT_3D('',#142957,#109538,#109539);
#96488=AXIS2_PLACEMENT_3D('',#142958,#109540,#109541);
#96489=AXIS2_PLACEMENT_3D('',#142959,#109542,#109543);
#96490=AXIS2_PLACEMENT_3D('',#142960,#109544,#109545);
#96491=AXIS2_PLACEMENT_3D('',#142963,#109546,#109547);
#96492=AXIS2_PLACEMENT_3D('',#142976,#109550,#109551);
#96493=AXIS2_PLACEMENT_3D('',#142977,#109552,#109553);
#96494=AXIS2_PLACEMENT_3D('',#142978,#109554,#109555);
#96495=AXIS2_PLACEMENT_3D('',#142979,#109556,#109557);
#96496=AXIS2_PLACEMENT_3D('',#142981,#109558,#109559);
#96497=AXIS2_PLACEMENT_3D('',#142982,#109560,#109561);
#96498=AXIS2_PLACEMENT_3D('',#142994,#109562,#109563);
#96499=AXIS2_PLACEMENT_3D('',#142995,#109564,#109565);
#96500=AXIS2_PLACEMENT_3D('',#142996,#109566,#109567);
#96501=AXIS2_PLACEMENT_3D('',#142997,#109568,#109569);
#96502=AXIS2_PLACEMENT_3D('',#143000,#109570,#109571);
#96503=AXIS2_PLACEMENT_3D('',#143020,#109574,#109575);
#96504=AXIS2_PLACEMENT_3D('',#143021,#109576,#109577);
#96505=AXIS2_PLACEMENT_3D('',#143022,#109578,#109579);
#96506=AXIS2_PLACEMENT_3D('',#143023,#109580,#109581);
#96507=AXIS2_PLACEMENT_3D('',#143025,#109582,#109583);
#96508=AXIS2_PLACEMENT_3D('',#143027,#109584,#109585);
#96509=AXIS2_PLACEMENT_3D('',#143042,#109586,#109587);
#96510=AXIS2_PLACEMENT_3D('',#143045,#109588,#109589);
#96511=AXIS2_PLACEMENT_3D('',#143050,#109590,#109591);
#96512=AXIS2_PLACEMENT_3D('',#143057,#109592,#109593);
#96513=AXIS2_PLACEMENT_3D('',#143063,#109597,#109598);
#96514=AXIS2_PLACEMENT_3D('',#143066,#109600,#109601);
#96515=AXIS2_PLACEMENT_3D('',#143067,#109602,#109603);
#96516=AXIS2_PLACEMENT_3D('',#143096,#109604,#109605);
#96517=AXIS2_PLACEMENT_3D('',#143099,#109607,#109608);
#96518=AXIS2_PLACEMENT_3D('',#143103,#109610,#109611);
#96519=AXIS2_PLACEMENT_3D('',#143107,#109613,#109614);
#96520=AXIS2_PLACEMENT_3D('',#143165,#109615,#109616);
#96521=AXIS2_PLACEMENT_3D('',#143167,#109617,#109618);
#96522=AXIS2_PLACEMENT_3D('',#143171,#109620,#109621);
#96523=AXIS2_PLACEMENT_3D('',#143175,#109623,#109624);
#96524=AXIS2_PLACEMENT_3D('',#143177,#109626,#109627);
#96525=AXIS2_PLACEMENT_3D('',#143178,#109628,#109629);
#96526=AXIS2_PLACEMENT_3D('',#143181,#109630,#109631);
#96527=AXIS2_PLACEMENT_3D('',#143183,#109632,#109633);
#96528=AXIS2_PLACEMENT_3D('',#143185,#109634,#109635);
#96529=AXIS2_PLACEMENT_3D('',#143186,#109636,#109637);
#96530=AXIS2_PLACEMENT_3D('',#143204,#109638,#109639);
#96531=AXIS2_PLACEMENT_3D('',#143205,#109640,#109641);
#96532=AXIS2_PLACEMENT_3D('',#143206,#109642,#109643);
#96533=AXIS2_PLACEMENT_3D('',#143207,#109644,#109645);
#96534=AXIS2_PLACEMENT_3D('',#143210,#109646,#109647);
#96535=AXIS2_PLACEMENT_3D('',#143223,#109650,#109651);
#96536=AXIS2_PLACEMENT_3D('',#143224,#109652,#109653);
#96537=AXIS2_PLACEMENT_3D('',#143225,#109654,#109655);
#96538=AXIS2_PLACEMENT_3D('',#143226,#109656,#109657);
#96539=AXIS2_PLACEMENT_3D('',#143228,#109658,#109659);
#96540=AXIS2_PLACEMENT_3D('',#143229,#109660,#109661);
#96541=AXIS2_PLACEMENT_3D('',#143241,#109662,#109663);
#96542=AXIS2_PLACEMENT_3D('',#143242,#109664,#109665);
#96543=AXIS2_PLACEMENT_3D('',#143243,#109666,#109667);
#96544=AXIS2_PLACEMENT_3D('',#143244,#109668,#109669);
#96545=AXIS2_PLACEMENT_3D('',#143247,#109670,#109671);
#96546=AXIS2_PLACEMENT_3D('',#143261,#109674,#109675);
#96547=AXIS2_PLACEMENT_3D('',#143262,#109676,#109677);
#96548=AXIS2_PLACEMENT_3D('',#143263,#109678,#109679);
#96549=AXIS2_PLACEMENT_3D('',#143264,#109680,#109681);
#96550=AXIS2_PLACEMENT_3D('',#143267,#109682,#109683);
#96551=AXIS2_PLACEMENT_3D('',#143279,#109686,#109687);
#96552=AXIS2_PLACEMENT_3D('',#143280,#109688,#109689);
#96553=AXIS2_PLACEMENT_3D('',#143281,#109690,#109691);
#96554=AXIS2_PLACEMENT_3D('',#143287,#109695,#109696);
#96555=AXIS2_PLACEMENT_3D('',#143290,#109698,#109699);
#96556=AXIS2_PLACEMENT_3D('',#143291,#109700,#109701);
#96557=AXIS2_PLACEMENT_3D('',#143295,#109704,#109705);
#96558=AXIS2_PLACEMENT_3D('',#143298,#109707,#109708);
#96559=AXIS2_PLACEMENT_3D('',#143299,#109709,#109710);
#96560=AXIS2_PLACEMENT_3D('',#143303,#109712,#109713);
#96561=AXIS2_PLACEMENT_3D('',#143307,#109715,#109716);
#96562=AXIS2_PLACEMENT_3D('',#143311,#109718,#109719);
#96563=AXIS2_PLACEMENT_3D('',#143355,#109720,#109721);
#96564=AXIS2_PLACEMENT_3D('',#143358,#109723,#109724);
#96565=AXIS2_PLACEMENT_3D('',#143359,#109725,#109726);
#96566=AXIS2_PLACEMENT_3D('',#143360,#109727,#109728);
#96567=AXIS2_PLACEMENT_3D('',#143363,#109730,#109731);
#96568=AXIS2_PLACEMENT_3D('',#143364,#109732,#109733);
#96569=AXIS2_PLACEMENT_3D('',#143368,#109736,#109737);
#96570=AXIS2_PLACEMENT_3D('',#143369,#109738,#109739);
#96571=AXIS2_PLACEMENT_3D('',#143370,#109740,#109741);
#96572=AXIS2_PLACEMENT_3D('',#143373,#109743,#109744);
#96573=AXIS2_PLACEMENT_3D('',#143374,#109745,#109746);
#96574=AXIS2_PLACEMENT_3D('',#143375,#109747,#109748);
#96575=AXIS2_PLACEMENT_3D('',#143376,#109749,#109750);
#96576=AXIS2_PLACEMENT_3D('',#143379,#109751,#109752);
#96577=AXIS2_PLACEMENT_3D('',#143383,#109754,#109755);
#96578=AXIS2_PLACEMENT_3D('',#143385,#109757,#109758);
#96579=AXIS2_PLACEMENT_3D('',#143399,#109766,#109767);
#96580=AXIS2_PLACEMENT_3D('',#143405,#109771,#109772);
#96581=AXIS2_PLACEMENT_3D('',#143406,#109773,#109774);
#96582=AXIS2_PLACEMENT_3D('',#143407,#109775,#109776);
#96583=AXIS2_PLACEMENT_3D('',#143408,#109777,#109778);
#96584=AXIS2_PLACEMENT_3D('',#143411,#109780,#109781);
#96585=AXIS2_PLACEMENT_3D('',#143412,#109782,#109783);
#96586=AXIS2_PLACEMENT_3D('',#143414,#109784,#109785);
#96587=AXIS2_PLACEMENT_3D('',#143417,#109787,#109788);
#96588=AXIS2_PLACEMENT_3D('',#143418,#109789,#109790);
#96589=AXIS2_PLACEMENT_3D('',#143420,#109791,#109792);
#96590=AXIS2_PLACEMENT_3D('',#143423,#109794,#109795);
#96591=AXIS2_PLACEMENT_3D('',#143424,#109796,#109797);
#96592=AXIS2_PLACEMENT_3D('',#143426,#109798,#109799);
#96593=AXIS2_PLACEMENT_3D('',#143429,#109801,#109802);
#96594=AXIS2_PLACEMENT_3D('',#143430,#109803,#109804);
#96595=AXIS2_PLACEMENT_3D('',#143436,#109808,#109809);
#96596=AXIS2_PLACEMENT_3D('',#143438,#109810,#109811);
#96597=AXIS2_PLACEMENT_3D('',#143440,#109812,#109813);
#96598=AXIS2_PLACEMENT_3D('',#143442,#109815,#109816);
#96599=AXIS2_PLACEMENT_3D('',#143444,#109817,#109818);
#96600=AXIS2_PLACEMENT_3D('',#143446,#109819,#109820);
#96601=AXIS2_PLACEMENT_3D('',#143447,#109821,#109822);
#96602=AXIS2_PLACEMENT_3D('',#143449,#109823,#109824);
#96603=AXIS2_PLACEMENT_3D('',#143451,#109826,#109827);
#96604=AXIS2_PLACEMENT_3D('',#143453,#109828,#109829);
#96605=AXIS2_PLACEMENT_3D('',#143455,#109831,#109832);
#96606=AXIS2_PLACEMENT_3D('',#143473,#109842,#109843);
#96607=AXIS2_PLACEMENT_3D('',#143476,#109845,#109846);
#96608=AXIS2_PLACEMENT_3D('',#143477,#109847,#109848);
#96609=AXIS2_PLACEMENT_3D('',#143480,#109850,#109851);
#96610=AXIS2_PLACEMENT_3D('',#143481,#109852,#109853);
#96611=AXIS2_PLACEMENT_3D('',#143482,#109854,#109855);
#96612=AXIS2_PLACEMENT_3D('',#143483,#109856,#109857);
#96613=AXIS2_PLACEMENT_3D('',#143485,#109858,#109859);
#96614=AXIS2_PLACEMENT_3D('',#143488,#109861,#109862);
#96615=AXIS2_PLACEMENT_3D('',#143489,#109863,#109864);
#96616=AXIS2_PLACEMENT_3D('',#143492,#109865,#109866);
#96617=AXIS2_PLACEMENT_3D('',#143496,#109868,#109869);
#96618=AXIS2_PLACEMENT_3D('',#143498,#109871,#109872);
#96619=AXIS2_PLACEMENT_3D('',#143504,#109876,#109877);
#96620=AXIS2_PLACEMENT_3D('',#143507,#109879,#109880);
#96621=AXIS2_PLACEMENT_3D('',#143508,#109881,#109882);
#96622=AXIS2_PLACEMENT_3D('',#143514,#109886,#109887);
#96623=AXIS2_PLACEMENT_3D('',#143516,#109888,#109889);
#96624=AXIS2_PLACEMENT_3D('',#143519,#109891,#109892);
#96625=AXIS2_PLACEMENT_3D('',#143520,#109893,#109894);
#96626=AXIS2_PLACEMENT_3D('',#143523,#109895,#109896);
#96627=AXIS2_PLACEMENT_3D('',#143527,#109898,#109899);
#96628=AXIS2_PLACEMENT_3D('',#143529,#109901,#109902);
#96629=AXIS2_PLACEMENT_3D('',#143530,#109903,#109904);
#96630=AXIS2_PLACEMENT_3D('',#143531,#109905,#109906);
#96631=AXIS2_PLACEMENT_3D('',#143532,#109907,#109908);
#96632=AXIS2_PLACEMENT_3D('',#143534,#109909,#109910);
#96633=AXIS2_PLACEMENT_3D('',#143537,#109912,#109913);
#96634=AXIS2_PLACEMENT_3D('',#143538,#109914,#109915);
#96635=AXIS2_PLACEMENT_3D('',#143540,#109916,#109917);
#96636=AXIS2_PLACEMENT_3D('',#143543,#109919,#109920);
#96637=AXIS2_PLACEMENT_3D('',#143544,#109921,#109922);
#96638=AXIS2_PLACEMENT_3D('',#143549,#109924,#109925);
#96639=AXIS2_PLACEMENT_3D('',#143552,#109927,#109928);
#96640=AXIS2_PLACEMENT_3D('',#143553,#109929,#109930);
#96641=AXIS2_PLACEMENT_3D('',#143596,#109933,#109934);
#96642=AXIS2_PLACEMENT_3D('',#143619,#109937,#109938);
#96643=AXIS2_PLACEMENT_3D('',#143621,#109939,#109940);
#96644=AXIS2_PLACEMENT_3D('',#143624,#109942,#109943);
#96645=AXIS2_PLACEMENT_3D('',#143625,#109944,#109945);
#96646=AXIS2_PLACEMENT_3D('',#143629,#109947,#109948);
#96647=AXIS2_PLACEMENT_3D('',#143631,#109949,#109950);
#96648=AXIS2_PLACEMENT_3D('',#143632,#109951,#109952);
#96649=AXIS2_PLACEMENT_3D('',#143634,#109954,#109955);
#96650=AXIS2_PLACEMENT_3D('',#143636,#109956,#109957);
#96651=AXIS2_PLACEMENT_3D('',#143639,#109959,#109960);
#96652=AXIS2_PLACEMENT_3D('',#143640,#109961,#109962);
#96653=AXIS2_PLACEMENT_3D('',#143644,#109964,#109965);
#96654=AXIS2_PLACEMENT_3D('',#143646,#109966,#109967);
#96655=AXIS2_PLACEMENT_3D('',#143647,#109968,#109969);
#96656=AXIS2_PLACEMENT_3D('',#143649,#109971,#109972);
#96657=AXIS2_PLACEMENT_3D('',#143656,#109973,#109974);
#96658=AXIS2_PLACEMENT_3D('',#143659,#109975,#109976);
#96659=AXIS2_PLACEMENT_3D('',#143665,#109979,#109980);
#96660=AXIS2_PLACEMENT_3D('',#143669,#109983,#109984);
#96661=AXIS2_PLACEMENT_3D('',#143672,#109985,#109986);
#96662=AXIS2_PLACEMENT_3D('',#143678,#109989,#109990);
#96663=AXIS2_PLACEMENT_3D('',#143682,#109993,#109994);
#96664=AXIS2_PLACEMENT_3D('',#143688,#109998,#109999);
#96665=AXIS2_PLACEMENT_3D('',#143690,#110000,#110001);
#96666=AXIS2_PLACEMENT_3D('',#143692,#110002,#110003);
#96667=AXIS2_PLACEMENT_3D('',#143694,#110005,#110006);
#96668=AXIS2_PLACEMENT_3D('',#143698,#110009,#110010);
#96669=AXIS2_PLACEMENT_3D('',#143704,#110014,#110015);
#96670=AXIS2_PLACEMENT_3D('',#143706,#110016,#110017);
#96671=AXIS2_PLACEMENT_3D('',#143708,#110018,#110019);
#96672=AXIS2_PLACEMENT_3D('',#143710,#110021,#110022);
#96673=AXIS2_PLACEMENT_3D('',#143714,#110025,#110026);
#96674=AXIS2_PLACEMENT_3D('',#143715,#110027,#110028);
#96675=AXIS2_PLACEMENT_3D('',#143717,#110029,#110030);
#96676=AXIS2_PLACEMENT_3D('',#143718,#110031,#110032);
#96677=AXIS2_PLACEMENT_3D('',#143719,#110033,#110034);
#96678=AXIS2_PLACEMENT_3D('',#143720,#110035,#110036);
#96679=AXIS2_PLACEMENT_3D('',#143721,#110037,#110038);
#96680=AXIS2_PLACEMENT_3D('',#143723,#110039,#110040);
#96681=AXIS2_PLACEMENT_3D('',#143724,#110041,#110042);
#96682=AXIS2_PLACEMENT_3D('',#143725,#110043,#110044);
#96683=AXIS2_PLACEMENT_3D('',#143726,#110045,#110046);
#96684=AXIS2_PLACEMENT_3D('',#143737,#110050,#110051);
#96685=AXIS2_PLACEMENT_3D('',#143739,#110052,#110053);
#96686=AXIS2_PLACEMENT_3D('',#143741,#110054,#110055);
#96687=AXIS2_PLACEMENT_3D('',#143743,#110057,#110058);
#96688=AXIS2_PLACEMENT_3D('',#143751,#110061,#110062);
#96689=AXIS2_PLACEMENT_3D('',#143758,#110063,#110064);
#96690=AXIS2_PLACEMENT_3D('',#143769,#110068,#110069);
#96691=AXIS2_PLACEMENT_3D('',#143771,#110070,#110071);
#96692=AXIS2_PLACEMENT_3D('',#143773,#110072,#110073);
#96693=AXIS2_PLACEMENT_3D('',#143775,#110075,#110076);
#96694=AXIS2_PLACEMENT_3D('',#143783,#110079,#110080);
#96695=AXIS2_PLACEMENT_3D('',#143790,#110081,#110082);
#96696=AXIS2_PLACEMENT_3D('',#143796,#110086,#110087);
#96697=AXIS2_PLACEMENT_3D('',#143799,#110090,#110091);
#96698=AXIS2_PLACEMENT_3D('',#143828,#110094,#110095);
#96699=AXIS2_PLACEMENT_3D('',#143829,#110096,#110097);
#96700=AXIS2_PLACEMENT_3D('',#143835,#110101,#110102);
#96701=AXIS2_PLACEMENT_3D('',#143838,#110103,#110104);
#96702=AXIS2_PLACEMENT_3D('',#143857,#110107,#110108);
#96703=AXIS2_PLACEMENT_3D('',#143864,#110111,#110112);
#96704=AXIS2_PLACEMENT_3D('',#143866,#110114,#110115);
#96705=AXIS2_PLACEMENT_3D('',#143872,#110119,#110120);
#96706=AXIS2_PLACEMENT_3D('',#143896,#110122,#110123);
#96707=AXIS2_PLACEMENT_3D('',#143897,#110124,#110125);
#96708=AXIS2_PLACEMENT_3D('',#143899,#110126,#110127);
#96709=AXIS2_PLACEMENT_3D('',#143901,#110128,#110129);
#96710=AXIS2_PLACEMENT_3D('',#143902,#110130,#110131);
#96711=AXIS2_PLACEMENT_3D('',#143904,#110132,#110133);
#96712=AXIS2_PLACEMENT_3D('',#143906,#110135,#110136);
#96713=AXIS2_PLACEMENT_3D('',#143933,#110137,#110138);
#96714=AXIS2_PLACEMENT_3D('',#143934,#110139,#110140);
#96715=AXIS2_PLACEMENT_3D('',#143938,#110143,#110144);
#96716=AXIS2_PLACEMENT_3D('',#143941,#110146,#110147);
#96717=AXIS2_PLACEMENT_3D('',#143942,#110148,#110149);
#96718=AXIS2_PLACEMENT_3D('',#143946,#110152,#110153);
#96719=AXIS2_PLACEMENT_3D('',#143947,#110154,#110155);
#96720=AXIS2_PLACEMENT_3D('',#143976,#110157,#110158);
#96721=AXIS2_PLACEMENT_3D('',#143978,#110159,#110160);
#96722=AXIS2_PLACEMENT_3D('',#143981,#110162,#110163);
#96723=AXIS2_PLACEMENT_3D('',#143982,#110164,#110165);
#96724=AXIS2_PLACEMENT_3D('',#143984,#110166,#110167);
#96725=AXIS2_PLACEMENT_3D('',#143985,#110168,#110169);
#96726=AXIS2_PLACEMENT_3D('',#143986,#110170,#110171);
#96727=AXIS2_PLACEMENT_3D('',#143987,#110172,#110173);
#96728=AXIS2_PLACEMENT_3D('',#143988,#110174,#110175);
#96729=AXIS2_PLACEMENT_3D('',#143990,#110176,#110177);
#96730=AXIS2_PLACEMENT_3D('',#143992,#110179,#110180);
#96731=AXIS2_PLACEMENT_3D('',#144003,#110181,#110182);
#96732=AXIS2_PLACEMENT_3D('',#144005,#110184,#110185);
#96733=AXIS2_PLACEMENT_3D('',#144011,#110189,#110190);
#96734=AXIS2_PLACEMENT_3D('',#144032,#110192,#110193);
#96735=AXIS2_PLACEMENT_3D('',#144038,#110197,#110198);
#96736=AXIS2_PLACEMENT_3D('',#144050,#110199,#110200);
#96737=AXIS2_PLACEMENT_3D('',#144051,#110201,#110202);
#96738=AXIS2_PLACEMENT_3D('',#144052,#110203,#110204);
#96739=AXIS2_PLACEMENT_3D('',#144053,#110205,#110206);
#96740=AXIS2_PLACEMENT_3D('',#144057,#110209,#110210);
#96741=AXIS2_PLACEMENT_3D('',#144058,#110211,#110212);
#96742=AXIS2_PLACEMENT_3D('',#144060,#110213,#110214);
#96743=AXIS2_PLACEMENT_3D('',#144084,#110216,#110217);
#96744=AXIS2_PLACEMENT_3D('',#144085,#110218,#110219);
#96745=AXIS2_PLACEMENT_3D('',#144087,#110221,#110222);
#96746=AXIS2_PLACEMENT_3D('',#144099,#110223,#110224);
#96747=AXIS2_PLACEMENT_3D('',#144100,#110225,#110226);
#96748=AXIS2_PLACEMENT_3D('',#144101,#110227,#110228);
#96749=AXIS2_PLACEMENT_3D('',#144102,#110229,#110230);
#96750=AXIS2_PLACEMENT_3D('',#144104,#110232,#110233);
#96751=AXIS2_PLACEMENT_3D('',#144106,#110235,#110236);
#96752=AXIS2_PLACEMENT_3D('',#144108,#110238,#110239);
#96753=AXIS2_PLACEMENT_3D('',#144110,#110241,#110242);
#96754=AXIS2_PLACEMENT_3D('',#144115,#110247,#110248);
#96755=AXIS2_PLACEMENT_3D('',#144134,#110250,#110251);
#96756=AXIS2_PLACEMENT_3D('',#144136,#110253,#110254);
#96757=AXIS2_PLACEMENT_3D('',#144152,#110256,#110257);
#96758=AXIS2_PLACEMENT_3D('',#144153,#110258,#110259);
#96759=AXIS2_PLACEMENT_3D('',#144168,#110260,#110261);
#96760=AXIS2_PLACEMENT_3D('',#144200,#110262,#110263);
#96761=AXIS2_PLACEMENT_3D('',#144201,#110264,#110265);
#96762=AXIS2_PLACEMENT_3D('',#144206,#110267,#110268);
#96763=AXIS2_PLACEMENT_3D('',#144223,#110269,#110270);
#96764=AXIS2_PLACEMENT_3D('',#144224,#110271,#110272);
#96765=AXIS2_PLACEMENT_3D('',#144225,#110273,#110274);
#96766=AXIS2_PLACEMENT_3D('',#144226,#110275,#110276);
#96767=AXIS2_PLACEMENT_3D('',#144227,#110277,#110278);
#96768=AXIS2_PLACEMENT_3D('',#144229,#110280,#110281);
#96769=AXIS2_PLACEMENT_3D('',#144246,#110283,#110284);
#96770=AXIS2_PLACEMENT_3D('',#144268,#110286,#110287);
#96771=AXIS2_PLACEMENT_3D('',#144270,#110289,#110290);
#96772=AXIS2_PLACEMENT_3D('',#144272,#110291,#110292);
#96773=AXIS2_PLACEMENT_3D('',#144306,#110294,#110295);
#96774=AXIS2_PLACEMENT_3D('',#144323,#110296,#110297);
#96775=AXIS2_PLACEMENT_3D('',#144325,#110299,#110300);
#96776=AXIS2_PLACEMENT_3D('',#144344,#110301,#110302);
#96777=AXIS2_PLACEMENT_3D('',#144345,#110303,#110304);
#96778=AXIS2_PLACEMENT_3D('',#144347,#110305,#110306);
#96779=AXIS2_PLACEMENT_3D('',#144350,#110308,#110309);
#96780=AXIS2_PLACEMENT_3D('',#144351,#110310,#110311);
#96781=AXIS2_PLACEMENT_3D('',#144353,#110312,#110313);
#96782=AXIS2_PLACEMENT_3D('',#144354,#110314,#110315);
#96783=AXIS2_PLACEMENT_3D('',#144357,#110317,#110318);
#96784=AXIS2_PLACEMENT_3D('',#144358,#110319,#110320);
#96785=AXIS2_PLACEMENT_3D('',#144361,#110322,#110323);
#96786=AXIS2_PLACEMENT_3D('',#144362,#110324,#110325);
#96787=AXIS2_PLACEMENT_3D('',#144364,#110326,#110327);
#96788=AXIS2_PLACEMENT_3D('',#144367,#110329,#110330);
#96789=AXIS2_PLACEMENT_3D('',#144368,#110331,#110332);
#96790=AXIS2_PLACEMENT_3D('',#144379,#110333,#110334);
#96791=AXIS2_PLACEMENT_3D('',#144381,#110335,#110336);
#96792=AXIS2_PLACEMENT_3D('',#144384,#110338,#110339);
#96793=AXIS2_PLACEMENT_3D('',#144385,#110340,#110341);
#96794=AXIS2_PLACEMENT_3D('',#144401,#110343,#110344);
#96795=AXIS2_PLACEMENT_3D('',#144403,#110345,#110346);
#96796=AXIS2_PLACEMENT_3D('',#144406,#110348,#110349);
#96797=AXIS2_PLACEMENT_3D('',#144407,#110350,#110351);
#96798=AXIS2_PLACEMENT_3D('',#144410,#110353,#110354);
#96799=AXIS2_PLACEMENT_3D('',#144411,#110355,#110356);
#96800=AXIS2_PLACEMENT_3D('',#144414,#110357,#110358);
#96801=AXIS2_PLACEMENT_3D('',#144418,#110360,#110361);
#96802=AXIS2_PLACEMENT_3D('',#144420,#110363,#110364);
#96803=AXIS2_PLACEMENT_3D('',#144425,#110366,#110367);
#96804=AXIS2_PLACEMENT_3D('',#144428,#110369,#110370);
#96805=AXIS2_PLACEMENT_3D('',#144429,#110371,#110372);
#96806=AXIS2_PLACEMENT_3D('',#144433,#110374,#110375);
#96807=AXIS2_PLACEMENT_3D('',#144434,#110376,#110377);
#96808=AXIS2_PLACEMENT_3D('',#144435,#110378,#110379);
#96809=AXIS2_PLACEMENT_3D('',#144438,#110381,#110382);
#96810=AXIS2_PLACEMENT_3D('',#144439,#110383,#110384);
#96811=AXIS2_PLACEMENT_3D('',#144443,#110387,#110388);
#96812=AXIS2_PLACEMENT_3D('',#144445,#110389,#110390);
#96813=AXIS2_PLACEMENT_3D('',#144447,#110392,#110393);
#96814=AXIS2_PLACEMENT_3D('',#144451,#110395,#110396);
#96815=AXIS2_PLACEMENT_3D('',#144471,#110399,#110400);
#96816=AXIS2_PLACEMENT_3D('',#144473,#110401,#110402);
#96817=AXIS2_PLACEMENT_3D('',#144476,#110404,#110405);
#96818=AXIS2_PLACEMENT_3D('',#144477,#110406,#110407);
#96819=AXIS2_PLACEMENT_3D('',#144481,#110410,#110411);
#96820=AXIS2_PLACEMENT_3D('',#144496,#110413,#110414);
#96821=AXIS2_PLACEMENT_3D('',#144497,#110415,#110416);
#96822=AXIS2_PLACEMENT_3D('',#144499,#110417,#110418);
#96823=AXIS2_PLACEMENT_3D('',#144501,#110420,#110421);
#96824=AXIS2_PLACEMENT_3D('',#144503,#110423,#110424);
#96825=AXIS2_PLACEMENT_3D('',#144504,#110425,#110426);
#96826=AXIS2_PLACEMENT_3D('',#144508,#110428,#110429);
#96827=AXIS2_PLACEMENT_3D('',#144513,#110430,#110431);
#96828=AXIS2_PLACEMENT_3D('',#144514,#110432,#110433);
#96829=AXIS2_PLACEMENT_3D('',#144515,#110434,#110435);
#96830=AXIS2_PLACEMENT_3D('',#144517,#110436,#110437);
#96831=AXIS2_PLACEMENT_3D('',#144518,#110438,#110439);
#96832=AXIS2_PLACEMENT_3D('',#144520,#110440,#110441);
#96833=AXIS2_PLACEMENT_3D('',#144522,#110442,#110443);
#96834=AXIS2_PLACEMENT_3D('',#144523,#110444,#110445);
#96835=AXIS2_PLACEMENT_3D('',#144526,#110447,#110448);
#96836=AXIS2_PLACEMENT_3D('',#144527,#110449,#110450);
#96837=AXIS2_PLACEMENT_3D('',#144530,#110452,#110453);
#96838=AXIS2_PLACEMENT_3D('',#144531,#110454,#110455);
#96839=AXIS2_PLACEMENT_3D('',#144532,#110456,#110457);
#96840=AXIS2_PLACEMENT_3D('',#144533,#110458,#110459);
#96841=AXIS2_PLACEMENT_3D('',#144539,#110460,#110461);
#96842=AXIS2_PLACEMENT_3D('',#144540,#110462,#110463);
#96843=AXIS2_PLACEMENT_3D('',#144541,#110464,#110465);
#96844=AXIS2_PLACEMENT_3D('',#144542,#110466,#110467);
#96845=AXIS2_PLACEMENT_3D('',#144543,#110468,#110469);
#96846=AXIS2_PLACEMENT_3D('',#144544,#110470,#110471);
#96847=AXIS2_PLACEMENT_3D('',#144546,#110472,#110473);
#96848=AXIS2_PLACEMENT_3D('',#144548,#110475,#110476);
#96849=AXIS2_PLACEMENT_3D('',#144549,#110477,#110478);
#96850=AXIS2_PLACEMENT_3D('',#144551,#110480,#110481);
#96851=AXIS2_PLACEMENT_3D('',#144553,#110482,#110483);
#96852=AXIS2_PLACEMENT_3D('',#144555,#110484,#110485);
#96853=AXIS2_PLACEMENT_3D('',#144556,#110486,#110487);
#96854=AXIS2_PLACEMENT_3D('',#144559,#110488,#110489);
#96855=AXIS2_PLACEMENT_3D('',#144561,#110491,#110492);
#96856=AXIS2_PLACEMENT_3D('',#144562,#110493,#110494);
#96857=AXIS2_PLACEMENT_3D('',#144564,#110495,#110496);
#96858=AXIS2_PLACEMENT_3D('',#144571,#110497,#110498);
#96859=AXIS2_PLACEMENT_3D('',#144593,#110499,#110500);
#96860=AXIS2_PLACEMENT_3D('',#144594,#110501,#110502);
#96861=AXIS2_PLACEMENT_3D('',#144613,#110503,#110504);
#96862=AXIS2_PLACEMENT_3D('',#144614,#110505,#110506);
#96863=AXIS2_PLACEMENT_3D('',#144616,#110508,#110509);
#96864=AXIS2_PLACEMENT_3D('',#144628,#110510,#110511);
#96865=AXIS2_PLACEMENT_3D('',#144629,#110512,#110513);
#96866=AXIS2_PLACEMENT_3D('',#144630,#110514,#110515);
#96867=AXIS2_PLACEMENT_3D('',#144631,#110516,#110517);
#96868=AXIS2_PLACEMENT_3D('',#144632,#110518,#110519);
#96869=AXIS2_PLACEMENT_3D('',#144633,#110520,#110521);
#96870=AXIS2_PLACEMENT_3D('',#144634,#110522,#110523);
#96871=AXIS2_PLACEMENT_3D('',#144635,#110524,#110525);
#96872=AXIS2_PLACEMENT_3D('',#144639,#110526,#110527);
#96873=AXIS2_PLACEMENT_3D('',#144640,#110528,#110529);
#96874=AXIS2_PLACEMENT_3D('',#144641,#110530,#110531);
#96875=AXIS2_PLACEMENT_3D('',#144642,#110532,#110533);
#96876=AXIS2_PLACEMENT_3D('',#144646,#110535,#110536);
#96877=AXIS2_PLACEMENT_3D('',#144648,#110538,#110539);
#96878=AXIS2_PLACEMENT_3D('',#144684,#110540,#110541);
#96879=AXIS2_PLACEMENT_3D('',#144685,#110542,#110543);
#96880=AXIS2_PLACEMENT_3D('',#144694,#110548,#110549);
#96881=AXIS2_PLACEMENT_3D('',#144702,#110553,#110554);
#96882=AXIS2_PLACEMENT_3D('',#144703,#110555,#110556);
#96883=AXIS2_PLACEMENT_3D('',#144709,#110557,#110558);
#96884=AXIS2_PLACEMENT_3D('',#144710,#110559,#110560);
#96885=AXIS2_PLACEMENT_3D('',#144712,#110561,#110562);
#96886=AXIS2_PLACEMENT_3D('',#144713,#110563,#110564);
#96887=AXIS2_PLACEMENT_3D('',#144714,#110565,#110566);
#96888=AXIS2_PLACEMENT_3D('',#144717,#110567,#110568);
#96889=AXIS2_PLACEMENT_3D('',#144738,#110571,#110572);
#96890=AXIS2_PLACEMENT_3D('',#144739,#110573,#110574);
#96891=AXIS2_PLACEMENT_3D('',#144740,#110575,#110576);
#96892=AXIS2_PLACEMENT_3D('',#144741,#110577,#110578);
#96893=AXIS2_PLACEMENT_3D('',#144742,#110579,#110580);
#96894=AXIS2_PLACEMENT_3D('',#144743,#110581,#110582);
#96895=AXIS2_PLACEMENT_3D('',#144744,#110583,#110584);
#96896=AXIS2_PLACEMENT_3D('',#144745,#110585,#110586);
#96897=AXIS2_PLACEMENT_3D('',#144746,#110587,#110588);
#96898=AXIS2_PLACEMENT_3D('',#144747,#110589,#110590);
#96899=AXIS2_PLACEMENT_3D('',#144748,#110591,#110592);
#96900=AXIS2_PLACEMENT_3D('',#144749,#110593,#110594);
#96901=AXIS2_PLACEMENT_3D('',#144775,#110595,#110596);
#96902=AXIS2_PLACEMENT_3D('',#144776,#110597,#110598);
#96903=AXIS2_PLACEMENT_3D('',#144777,#110599,#110600);
#96904=AXIS2_PLACEMENT_3D('',#144778,#110601,#110602);
#96905=AXIS2_PLACEMENT_3D('',#144779,#110603,#110604);
#96906=AXIS2_PLACEMENT_3D('',#144794,#110606,#110607);
#96907=AXIS2_PLACEMENT_3D('',#144795,#110608,#110609);
#96908=AXIS2_PLACEMENT_3D('',#144809,#110610,#110611);
#96909=AXIS2_PLACEMENT_3D('',#144812,#110613,#110614);
#96910=AXIS2_PLACEMENT_3D('',#144822,#110616,#110617);
#96911=AXIS2_PLACEMENT_3D('',#144836,#110618,#110619);
#96912=AXIS2_PLACEMENT_3D('',#144911,#110620,#110621);
#96913=AXIS2_PLACEMENT_3D('',#144912,#110622,#110623);
#96914=AXIS2_PLACEMENT_3D('',#144913,#110624,#110625);
#96915=AXIS2_PLACEMENT_3D('',#144914,#110626,#110627);
#96916=AXIS2_PLACEMENT_3D('',#144915,#110628,#110629);
#96917=AXIS2_PLACEMENT_3D('',#144921,#110633,#110634);
#96918=AXIS2_PLACEMENT_3D('',#144922,#110635,#110636);
#96919=AXIS2_PLACEMENT_3D('',#144923,#110637,#110638);
#96920=AXIS2_PLACEMENT_3D('',#144926,#110640,#110641);
#96921=AXIS2_PLACEMENT_3D('',#144927,#110642,#110643);
#96922=AXIS2_PLACEMENT_3D('',#144928,#110644,#110645);
#96923=AXIS2_PLACEMENT_3D('',#144929,#110646,#110647);
#96924=AXIS2_PLACEMENT_3D('',#144937,#110652,#110653);
#96925=AXIS2_PLACEMENT_3D('',#144939,#110654,#110655);
#96926=AXIS2_PLACEMENT_3D('',#144942,#110657,#110658);
#96927=AXIS2_PLACEMENT_3D('',#144943,#110659,#110660);
#96928=AXIS2_PLACEMENT_3D('',#144946,#110661,#110662);
#96929=AXIS2_PLACEMENT_3D('',#144950,#110664,#110665);
#96930=AXIS2_PLACEMENT_3D('',#144952,#110667,#110668);
#96931=AXIS2_PLACEMENT_3D('',#144958,#110672,#110673);
#96932=AXIS2_PLACEMENT_3D('',#144960,#110674,#110675);
#96933=AXIS2_PLACEMENT_3D('',#144963,#110677,#110678);
#96934=AXIS2_PLACEMENT_3D('',#144964,#110679,#110680);
#96935=AXIS2_PLACEMENT_3D('',#144970,#110681,#110682);
#96936=AXIS2_PLACEMENT_3D('',#144978,#110683,#110684);
#96937=AXIS2_PLACEMENT_3D('',#144979,#110685,#110686);
#96938=AXIS2_PLACEMENT_3D('',#144980,#110687,#110688);
#96939=AXIS2_PLACEMENT_3D('',#144983,#110690,#110691);
#96940=AXIS2_PLACEMENT_3D('',#144984,#110692,#110693);
#96941=AXIS2_PLACEMENT_3D('',#144987,#110695,#110696);
#96942=AXIS2_PLACEMENT_3D('',#144988,#110697,#110698);
#96943=AXIS2_PLACEMENT_3D('',#144989,#110699,#110700);
#96944=AXIS2_PLACEMENT_3D('',#144990,#110701,#110702);
#96945=AXIS2_PLACEMENT_3D('',#144994,#110705,#110706);
#96946=AXIS2_PLACEMENT_3D('',#144995,#110707,#110708);
#96947=AXIS2_PLACEMENT_3D('',#144996,#110709,#110710);
#96948=AXIS2_PLACEMENT_3D('',#145005,#110715,#110716);
#96949=AXIS2_PLACEMENT_3D('',#145006,#110717,#110718);
#96950=AXIS2_PLACEMENT_3D('',#145007,#110719,#110720);
#96951=AXIS2_PLACEMENT_3D('',#145008,#110721,#110722);
#96952=AXIS2_PLACEMENT_3D('',#145022,#110730,#110731);
#96953=AXIS2_PLACEMENT_3D('',#145024,#110732,#110733);
#96954=AXIS2_PLACEMENT_3D('',#145026,#110735,#110736);
#96955=AXIS2_PLACEMENT_3D('',#145030,#110739,#110740);
#96956=AXIS2_PLACEMENT_3D('',#145031,#110741,#110742);
#96957=AXIS2_PLACEMENT_3D('',#145032,#110743,#110744);
#96958=AXIS2_PLACEMENT_3D('',#145035,#110745,#110746);
#96959=AXIS2_PLACEMENT_3D('',#145037,#110748,#110749);
#96960=AXIS2_PLACEMENT_3D('',#145040,#110752,#110753);
#96961=AXIS2_PLACEMENT_3D('',#145044,#110756,#110757);
#96962=AXIS2_PLACEMENT_3D('',#145046,#110758,#110759);
#96963=AXIS2_PLACEMENT_3D('',#145048,#110761,#110762);
#96964=AXIS2_PLACEMENT_3D('',#145051,#110764,#110765);
#96965=AXIS2_PLACEMENT_3D('',#145052,#110766,#110767);
#96966=AXIS2_PLACEMENT_3D('',#145056,#110769,#110770);
#96967=AXIS2_PLACEMENT_3D('',#145057,#110771,#110772);
#96968=AXIS2_PLACEMENT_3D('',#145058,#110773,#110774);
#96969=AXIS2_PLACEMENT_3D('',#145060,#110775,#110776);
#96970=AXIS2_PLACEMENT_3D('',#145063,#110778,#110779);
#96971=AXIS2_PLACEMENT_3D('',#145064,#110780,#110781);
#96972=AXIS2_PLACEMENT_3D('',#145065,#110782,#110783);
#96973=AXIS2_PLACEMENT_3D('',#145068,#110785,#110786);
#96974=AXIS2_PLACEMENT_3D('',#145069,#110787,#110788);
#96975=AXIS2_PLACEMENT_3D('',#145078,#110789,#110790);
#96976=AXIS2_PLACEMENT_3D('',#145080,#110791,#110792);
#96977=AXIS2_PLACEMENT_3D('',#145083,#110794,#110795);
#96978=AXIS2_PLACEMENT_3D('',#145084,#110796,#110797);
#96979=AXIS2_PLACEMENT_3D('',#145085,#110798,#110799);
#96980=AXIS2_PLACEMENT_3D('',#145086,#110800,#110801);
#96981=AXIS2_PLACEMENT_3D('',#145087,#110802,#110803);
#96982=AXIS2_PLACEMENT_3D('',#145090,#110804,#110805);
#96983=AXIS2_PLACEMENT_3D('',#145091,#110806,#110807);
#96984=AXIS2_PLACEMENT_3D('',#145093,#110809,#110810);
#96985=AXIS2_PLACEMENT_3D('',#145095,#110811,#110812);
#96986=AXIS2_PLACEMENT_3D('',#145096,#110813,#110814);
#96987=AXIS2_PLACEMENT_3D('',#145097,#110815,#110816);
#96988=AXIS2_PLACEMENT_3D('',#145099,#110818,#110819);
#96989=AXIS2_PLACEMENT_3D('',#145105,#110823,#110824);
#96990=AXIS2_PLACEMENT_3D('',#145107,#110825,#110826);
#96991=AXIS2_PLACEMENT_3D('',#145110,#110828,#110829);
#96992=AXIS2_PLACEMENT_3D('',#145112,#110830,#110831);
#96993=AXIS2_PLACEMENT_3D('',#145116,#110833,#110834);
#96994=AXIS2_PLACEMENT_3D('',#145118,#110836,#110837);
#96995=AXIS2_PLACEMENT_3D('',#145120,#110838,#110839);
#96996=AXIS2_PLACEMENT_3D('',#145123,#110841,#110842);
#96997=AXIS2_PLACEMENT_3D('',#145125,#110843,#110844);
#96998=AXIS2_PLACEMENT_3D('',#145129,#110846,#110847);
#96999=AXIS2_PLACEMENT_3D('',#145132,#110849,#110850);
#97000=AXIS2_PLACEMENT_3D('',#145134,#110851,#110852);
#97001=AXIS2_PLACEMENT_3D('',#145135,#110853,#110854);
#97002=AXIS2_PLACEMENT_3D('',#145136,#110855,#110856);
#97003=AXIS2_PLACEMENT_3D('',#145137,#110857,#110858);
#97004=AXIS2_PLACEMENT_3D('',#145138,#110859,#110860);
#97005=AXIS2_PLACEMENT_3D('',#145139,#110861,#110862);
#97006=AXIS2_PLACEMENT_3D('',#145140,#110863,#110864);
#97007=AXIS2_PLACEMENT_3D('',#145141,#110865,#110866);
#97008=AXIS2_PLACEMENT_3D('',#145143,#110868,#110869);
#97009=AXIS2_PLACEMENT_3D('',#145145,#110870,#110871);
#97010=AXIS2_PLACEMENT_3D('',#145147,#110872,#110873);
#97011=AXIS2_PLACEMENT_3D('',#145150,#110875,#110876);
#97012=AXIS2_PLACEMENT_3D('',#145151,#110877,#110878);
#97013=AXIS2_PLACEMENT_3D('',#145160,#110883,#110884);
#97014=AXIS2_PLACEMENT_3D('',#145169,#110889,#110890);
#97015=AXIS2_PLACEMENT_3D('',#145170,#110891,#110892);
#97016=AXIS2_PLACEMENT_3D('',#145171,#110893,#110894);
#97017=AXIS2_PLACEMENT_3D('',#145172,#110895,#110896);
#97018=AXIS2_PLACEMENT_3D('',#145173,#110897,#110898);
#97019=AXIS2_PLACEMENT_3D('',#145176,#110901,#110902);
#97020=AXIS2_PLACEMENT_3D('',#145177,#110903,#110904);
#97021=AXIS2_PLACEMENT_3D('',#145182,#110905,#110906);
#97022=AXIS2_PLACEMENT_3D('',#145183,#110907,#110908);
#97023=AXIS2_PLACEMENT_3D('',#145184,#110909,#110910);
#97024=AXIS2_PLACEMENT_3D('',#145185,#110911,#110912);
#97025=AXIS2_PLACEMENT_3D('',#145186,#110913,#110914);
#97026=AXIS2_PLACEMENT_3D('',#145187,#110915,#110916);
#97027=AXIS2_PLACEMENT_3D('',#145188,#110917,#110918);
#97028=AXIS2_PLACEMENT_3D('',#145189,#110919,#110920);
#97029=AXIS2_PLACEMENT_3D('',#145190,#110921,#110922);
#97030=AXIS2_PLACEMENT_3D('',#145191,#110923,#110924);
#97031=AXIS2_PLACEMENT_3D('',#145192,#110925,#110926);
#97032=AXIS2_PLACEMENT_3D('',#145198,#110930,#110931);
#97033=AXIS2_PLACEMENT_3D('',#145199,#110932,#110933);
#97034=AXIS2_PLACEMENT_3D('',#145200,#110934,#110935);
#97035=AXIS2_PLACEMENT_3D('',#145206,#110936,#110937);
#97036=AXIS2_PLACEMENT_3D('',#145207,#110938,#110939);
#97037=AXIS2_PLACEMENT_3D('',#145208,#110940,#110941);
#97038=AXIS2_PLACEMENT_3D('',#145241,#110942,#110943);
#97039=AXIS2_PLACEMENT_3D('',#145273,#110944,#110945);
#97040=AXIS2_PLACEMENT_3D('',#145294,#110946,#110947);
#97041=AXIS2_PLACEMENT_3D('',#145295,#110948,#110949);
#97042=AXIS2_PLACEMENT_3D('',#145296,#110950,#110951);
#97043=AXIS2_PLACEMENT_3D('',#145317,#110952,#110953);
#97044=AXIS2_PLACEMENT_3D('',#145319,#110954,#110955);
#97045=AXIS2_PLACEMENT_3D('',#145321,#110957,#110958);
#97046=AXIS2_PLACEMENT_3D('',#145323,#110960,#110961);
#97047=AXIS2_PLACEMENT_3D('',#145326,#110964,#110965);
#97048=AXIS2_PLACEMENT_3D('',#145327,#110966,#110967);
#97049=AXIS2_PLACEMENT_3D('',#145328,#110968,#110969);
#97050=AXIS2_PLACEMENT_3D('',#145329,#110970,#110971);
#97051=AXIS2_PLACEMENT_3D('',#145333,#110973,#110974);
#97052=AXIS2_PLACEMENT_3D('',#145335,#110976,#110977);
#97053=AXIS2_PLACEMENT_3D('',#145338,#110979,#110980);
#97054=AXIS2_PLACEMENT_3D('',#145339,#110981,#110982);
#97055=AXIS2_PLACEMENT_3D('',#145340,#110983,#110984);
#97056=AXIS2_PLACEMENT_3D('',#145341,#110985,#110986);
#97057=AXIS2_PLACEMENT_3D('',#145342,#110987,#110988);
#97058=AXIS2_PLACEMENT_3D('',#145344,#110990,#110991);
#97059=AXIS2_PLACEMENT_3D('',#145345,#110992,#110993);
#97060=AXIS2_PLACEMENT_3D('',#145346,#110994,#110995);
#97061=AXIS2_PLACEMENT_3D('',#145347,#110996,#110997);
#97062=AXIS2_PLACEMENT_3D('',#145348,#110998,#110999);
#97063=AXIS2_PLACEMENT_3D('',#145350,#111001,#111002);
#97064=AXIS2_PLACEMENT_3D('',#145352,#111004,#111005);
#97065=AXIS2_PLACEMENT_3D('',#145354,#111007,#111008);
#97066=AXIS2_PLACEMENT_3D('',#145355,#111009,#111010);
#97067=AXIS2_PLACEMENT_3D('',#145356,#111011,#111012);
#97068=AXIS2_PLACEMENT_3D('',#145358,#111014,#111015);
#97069=AXIS2_PLACEMENT_3D('',#145359,#111016,#111017);
#97070=AXIS2_PLACEMENT_3D('',#145361,#111019,#111020);
#97071=AXIS2_PLACEMENT_3D('',#145363,#111022,#111023);
#97072=AXIS2_PLACEMENT_3D('',#145365,#111025,#111026);
#97073=AXIS2_PLACEMENT_3D('',#145366,#111027,#111028);
#97074=AXIS2_PLACEMENT_3D('',#145367,#111029,#111030);
#97075=AXIS2_PLACEMENT_3D('',#145368,#111031,#111032);
#97076=AXIS2_PLACEMENT_3D('',#145369,#111033,#111034);
#97077=AXIS2_PLACEMENT_3D('',#145370,#111035,#111036);
#97078=AXIS2_PLACEMENT_3D('',#145376,#111040,#111041);
#97079=AXIS2_PLACEMENT_3D('',#145378,#111042,#111043);
#97080=AXIS2_PLACEMENT_3D('',#145381,#111045,#111046);
#97081=AXIS2_PLACEMENT_3D('',#145382,#111047,#111048);
#97082=AXIS2_PLACEMENT_3D('',#145385,#111051,#111052);
#97083=AXIS2_PLACEMENT_3D('',#145386,#111053,#111054);
#97084=AXIS2_PLACEMENT_3D('',#145387,#111055,#111056);
#97085=AXIS2_PLACEMENT_3D('',#145389,#111058,#111059);
#97086=AXIS2_PLACEMENT_3D('',#145390,#111060,#111061);
#97087=AXIS2_PLACEMENT_3D('',#145391,#111062,#111063);
#97088=AXIS2_PLACEMENT_3D('',#145392,#111064,#111065);
#97089=AXIS2_PLACEMENT_3D('',#145393,#111066,#111067);
#97090=AXIS2_PLACEMENT_3D('',#145394,#111068,#111069);
#97091=AXIS2_PLACEMENT_3D('',#145396,#111071,#111072);
#97092=AXIS2_PLACEMENT_3D('',#145397,#111073,#111074);
#97093=AXIS2_PLACEMENT_3D('',#145398,#111075,#111076);
#97094=AXIS2_PLACEMENT_3D('',#145399,#111077,#111078);
#97095=AXIS2_PLACEMENT_3D('',#145408,#111083,#111084);
#97096=AXIS2_PLACEMENT_3D('',#145417,#111089,#111090);
#97097=AXIS2_PLACEMENT_3D('',#145423,#111093,#111094);
#97098=AXIS2_PLACEMENT_3D('',#145427,#111096,#111097);
#97099=AXIS2_PLACEMENT_3D('',#145429,#111098,#111099);
#97100=AXIS2_PLACEMENT_3D('',#145431,#111100,#111101);
#97101=AXIS2_PLACEMENT_3D('',#145439,#111105,#111106);
#97102=AXIS2_PLACEMENT_3D('',#145443,#111108,#111109);
#97103=AXIS2_PLACEMENT_3D('',#145449,#111113,#111114);
#97104=AXIS2_PLACEMENT_3D('',#145455,#111117,#111118);
#97105=AXIS2_PLACEMENT_3D('',#145457,#111119,#111120);
#97106=AXIS2_PLACEMENT_3D('',#145459,#111121,#111122);
#97107=AXIS2_PLACEMENT_3D('',#145463,#111124,#111125);
#97108=AXIS2_PLACEMENT_3D('',#145465,#111126,#111127);
#97109=AXIS2_PLACEMENT_3D('',#145467,#111128,#111129);
#97110=AXIS2_PLACEMENT_3D('',#145469,#111130,#111131);
#97111=AXIS2_PLACEMENT_3D('',#145471,#111132,#111133);
#97112=AXIS2_PLACEMENT_3D('',#145481,#111139,#111140);
#97113=AXIS2_PLACEMENT_3D('',#145486,#111144,#111145);
#97114=AXIS2_PLACEMENT_3D('',#145500,#111152,#111153);
#97115=AXIS2_PLACEMENT_3D('',#145502,#111154,#111155);
#97116=AXIS2_PLACEMENT_3D('',#145504,#111156,#111157);
#97117=AXIS2_PLACEMENT_3D('',#145506,#111158,#111159);
#97118=AXIS2_PLACEMENT_3D('',#145508,#111160,#111161);
#97119=AXIS2_PLACEMENT_3D('',#145512,#111163,#111164);
#97120=AXIS2_PLACEMENT_3D('',#145514,#111165,#111166);
#97121=AXIS2_PLACEMENT_3D('',#145515,#111167,#111168);
#97122=AXIS2_PLACEMENT_3D('',#145516,#111169,#111170);
#97123=AXIS2_PLACEMENT_3D('',#145519,#111173,#111174);
#97124=AXIS2_PLACEMENT_3D('',#145527,#111178,#111179);
#97125=AXIS2_PLACEMENT_3D('',#145531,#111181,#111182);
#97126=AXIS2_PLACEMENT_3D('',#145535,#111184,#111185);
#97127=AXIS2_PLACEMENT_3D('',#145538,#111188,#111189);
#97128=AXIS2_PLACEMENT_3D('',#145548,#111195,#111196);
#97129=AXIS2_PLACEMENT_3D('',#145552,#111198,#111199);
#97130=AXIS2_PLACEMENT_3D('',#145554,#111201,#111202);
#97131=AXIS2_PLACEMENT_3D('',#145556,#111204,#111205);
#97132=AXIS2_PLACEMENT_3D('',#145557,#111206,#111207);
#97133=AXIS2_PLACEMENT_3D('',#145566,#111209,#111210);
#97134=AXIS2_PLACEMENT_3D('',#145568,#111212,#111213);
#97135=AXIS2_PLACEMENT_3D('',#145571,#111216,#111217);
#97136=AXIS2_PLACEMENT_3D('',#145573,#111219,#111220);
#97137=AXIS2_PLACEMENT_3D('',#145577,#111223,#111224);
#97138=AXIS2_PLACEMENT_3D('',#145579,#111226,#111227);
#97139=AXIS2_PLACEMENT_3D('',#145580,#111228,#111229);
#97140=AXIS2_PLACEMENT_3D('',#145591,#111235,#111236);
#97141=AXIS2_PLACEMENT_3D('',#145592,#111237,#111238);
#97142=AXIS2_PLACEMENT_3D('',#145595,#111239,#111240);
#97143=AXIS2_PLACEMENT_3D('',#145598,#111243,#111244);
#97144=AXIS2_PLACEMENT_3D('',#145602,#111247,#111248);
#97145=AXIS2_PLACEMENT_3D('',#145605,#111250,#111251);
#97146=AXIS2_PLACEMENT_3D('',#145610,#111254,#111255);
#97147=AXIS2_PLACEMENT_3D('',#145612,#111256,#111257);
#97148=AXIS2_PLACEMENT_3D('',#145614,#111258,#111259);
#97149=AXIS2_PLACEMENT_3D('',#145617,#111261,#111262);
#97150=AXIS2_PLACEMENT_3D('',#145618,#111263,#111264);
#97151=AXIS2_PLACEMENT_3D('',#145620,#111266,#111267);
#97152=AXIS2_PLACEMENT_3D('',#145622,#111269,#111270);
#97153=AXIS2_PLACEMENT_3D('',#145623,#111271,#111272);
#97154=AXIS2_PLACEMENT_3D('',#145624,#111273,#111274);
#97155=AXIS2_PLACEMENT_3D('',#145628,#111276,#111277);
#97156=AXIS2_PLACEMENT_3D('',#145630,#111279,#111280);
#97157=AXIS2_PLACEMENT_3D('',#145635,#111283,#111284);
#97158=AXIS2_PLACEMENT_3D('',#145636,#111285,#111286);
#97159=AXIS2_PLACEMENT_3D('',#145640,#111289,#111290);
#97160=AXIS2_PLACEMENT_3D('',#145643,#111292,#111293);
#97161=AXIS2_PLACEMENT_3D('',#145644,#111294,#111295);
#97162=AXIS2_PLACEMENT_3D('',#145646,#111297,#111298);
#97163=AXIS2_PLACEMENT_3D('',#145652,#111302,#111303);
#97164=AXIS2_PLACEMENT_3D('',#145655,#111305,#111306);
#97165=AXIS2_PLACEMENT_3D('',#145656,#111307,#111308);
#97166=AXIS2_PLACEMENT_3D('',#145660,#111311,#111312);
#97167=AXIS2_PLACEMENT_3D('',#145661,#111313,#111314);
#97168=AXIS2_PLACEMENT_3D('',#145662,#111315,#111316);
#97169=AXIS2_PLACEMENT_3D('',#145666,#111318,#111319);
#97170=AXIS2_PLACEMENT_3D('',#145668,#111321,#111322);
#97171=AXIS2_PLACEMENT_3D('',#145670,#111324,#111325);
#97172=AXIS2_PLACEMENT_3D('',#145672,#111327,#111328);
#97173=AXIS2_PLACEMENT_3D('',#145673,#111329,#111330);
#97174=AXIS2_PLACEMENT_3D('',#145689,#111331,#111332);
#97175=AXIS2_PLACEMENT_3D('',#145698,#111333,#111334);
#97176=AXIS2_PLACEMENT_3D('',#145723,#111335,#111336);
#97177=AXIS2_PLACEMENT_3D('',#145730,#111337,#111338);
#97178=AXIS2_PLACEMENT_3D('',#145734,#111340,#111341);
#97179=AXIS2_PLACEMENT_3D('',#145735,#111342,#111343);
#97180=AXIS2_PLACEMENT_3D('',#145737,#111344,#111345);
#97181=AXIS2_PLACEMENT_3D('',#145738,#111346,#111347);
#97182=AXIS2_PLACEMENT_3D('',#145740,#111348,#111349);
#97183=AXIS2_PLACEMENT_3D('',#145743,#111351,#111352);
#97184=AXIS2_PLACEMENT_3D('',#145745,#111353,#111354);
#97185=AXIS2_PLACEMENT_3D('',#145746,#111355,#111356);
#97186=AXIS2_PLACEMENT_3D('',#145753,#111357,#111358);
#97187=AXIS2_PLACEMENT_3D('',#145760,#111359,#111360);
#97188=AXIS2_PLACEMENT_3D('',#145769,#111361,#111362);
#97189=AXIS2_PLACEMENT_3D('',#145774,#111363,#111364);
#97190=AXIS2_PLACEMENT_3D('',#145778,#111366,#111367);
#97191=AXIS2_PLACEMENT_3D('',#145779,#111368,#111369);
#97192=AXIS2_PLACEMENT_3D('',#145781,#111370,#111371);
#97193=AXIS2_PLACEMENT_3D('',#145782,#111372,#111373);
#97194=AXIS2_PLACEMENT_3D('',#145784,#111374,#111375);
#97195=AXIS2_PLACEMENT_3D('',#145786,#111376,#111377);
#97196=AXIS2_PLACEMENT_3D('',#145789,#111379,#111380);
#97197=AXIS2_PLACEMENT_3D('',#145790,#111381,#111382);
#97198=AXIS2_PLACEMENT_3D('',#145792,#111384,#111385);
#97199=AXIS2_PLACEMENT_3D('',#145795,#111388,#111389);
#97200=AXIS2_PLACEMENT_3D('',#145797,#111391,#111392);
#97201=AXIS2_PLACEMENT_3D('',#145798,#111393,#111394);
#97202=AXIS2_PLACEMENT_3D('',#145800,#111395,#111396);
#97203=AXIS2_PLACEMENT_3D('',#145802,#111397,#111398);
#97204=AXIS2_PLACEMENT_3D('',#145803,#111399,#111400);
#97205=AXIS2_PLACEMENT_3D('',#145805,#111401,#111402);
#97206=AXIS2_PLACEMENT_3D('',#145807,#111404,#111405);
#97207=AXIS2_PLACEMENT_3D('',#145809,#111406,#111407);
#97208=AXIS2_PLACEMENT_3D('',#145811,#111408,#111409);
#97209=AXIS2_PLACEMENT_3D('',#145812,#111410,#111411);
#97210=AXIS2_PLACEMENT_3D('',#145814,#111412,#111413);
#97211=AXIS2_PLACEMENT_3D('',#145816,#111415,#111416);
#97212=AXIS2_PLACEMENT_3D('',#145819,#111419,#111420);
#97213=AXIS2_PLACEMENT_3D('',#145822,#111423,#111424);
#97214=AXIS2_PLACEMENT_3D('',#145823,#111425,#111426);
#97215=AXIS2_PLACEMENT_3D('',#145825,#111428,#111429);
#97216=AXIS2_PLACEMENT_3D('',#145826,#111430,#111431);
#97217=AXIS2_PLACEMENT_3D('',#145828,#111433,#111434);
#97218=AXIS2_PLACEMENT_3D('',#145829,#111435,#111436);
#97219=AXIS2_PLACEMENT_3D('',#145830,#111437,#111438);
#97220=AXIS2_PLACEMENT_3D('',#145832,#111440,#111441);
#97221=AXIS2_PLACEMENT_3D('',#145834,#111443,#111444);
#97222=AXIS2_PLACEMENT_3D('',#145836,#111446,#111447);
#97223=AXIS2_PLACEMENT_3D('',#145839,#111450,#111451);
#97224=AXIS2_PLACEMENT_3D('',#145840,#111452,#111453);
#97225=AXIS2_PLACEMENT_3D('',#145842,#111454,#111455);
#97226=AXIS2_PLACEMENT_3D('',#145845,#111457,#111458);
#97227=AXIS2_PLACEMENT_3D('',#145846,#111459,#111460);
#97228=AXIS2_PLACEMENT_3D('',#145849,#111462,#111463);
#97229=AXIS2_PLACEMENT_3D('',#145850,#111464,#111465);
#97230=AXIS2_PLACEMENT_3D('',#145851,#111466,#111467);
#97231=AXIS2_PLACEMENT_3D('',#145853,#111468,#111469);
#97232=AXIS2_PLACEMENT_3D('',#145855,#111471,#111472);
#97233=AXIS2_PLACEMENT_3D('',#145856,#111473,#111474);
#97234=AXIS2_PLACEMENT_3D('',#145857,#111475,#111476);
#97235=AXIS2_PLACEMENT_3D('',#145859,#111477,#111478);
#97236=AXIS2_PLACEMENT_3D('',#145862,#111480,#111481);
#97237=AXIS2_PLACEMENT_3D('',#145863,#111482,#111483);
#97238=AXIS2_PLACEMENT_3D('',#145865,#111484,#111485);
#97239=AXIS2_PLACEMENT_3D('',#145867,#111487,#111488);
#97240=AXIS2_PLACEMENT_3D('',#145868,#111489,#111490);
#97241=AXIS2_PLACEMENT_3D('',#145870,#111491,#111492);
#97242=AXIS2_PLACEMENT_3D('',#145872,#111494,#111495);
#97243=AXIS2_PLACEMENT_3D('',#145873,#111496,#111497);
#97244=AXIS2_PLACEMENT_3D('',#145874,#111498,#111499);
#97245=AXIS2_PLACEMENT_3D('',#145888,#111500,#111501);
#97246=AXIS2_PLACEMENT_3D('',#145900,#111502,#111503);
#97247=AXIS2_PLACEMENT_3D('',#145901,#111504,#111505);
#97248=AXIS2_PLACEMENT_3D('',#145915,#111506,#111507);
#97249=AXIS2_PLACEMENT_3D('',#145927,#111508,#111509);
#97250=AXIS2_PLACEMENT_3D('',#145928,#111510,#111511);
#97251=AXIS2_PLACEMENT_3D('',#145942,#111512,#111513);
#97252=AXIS2_PLACEMENT_3D('',#145954,#111514,#111515);
#97253=AXIS2_PLACEMENT_3D('',#145955,#111516,#111517);
#97254=AXIS2_PLACEMENT_3D('',#145969,#111518,#111519);
#97255=AXIS2_PLACEMENT_3D('',#145981,#111520,#111521);
#97256=AXIS2_PLACEMENT_3D('',#145982,#111522,#111523);
#97257=AXIS2_PLACEMENT_3D('',#145996,#111524,#111525);
#97258=AXIS2_PLACEMENT_3D('',#146008,#111526,#111527);
#97259=AXIS2_PLACEMENT_3D('',#146009,#111528,#111529);
#97260=AXIS2_PLACEMENT_3D('',#146023,#111530,#111531);
#97261=AXIS2_PLACEMENT_3D('',#146035,#111532,#111533);
#97262=AXIS2_PLACEMENT_3D('',#146036,#111534,#111535);
#97263=AXIS2_PLACEMENT_3D('',#146050,#111536,#111537);
#97264=AXIS2_PLACEMENT_3D('',#146062,#111538,#111539);
#97265=AXIS2_PLACEMENT_3D('',#146063,#111540,#111541);
#97266=AXIS2_PLACEMENT_3D('',#146077,#111542,#111543);
#97267=AXIS2_PLACEMENT_3D('',#146089,#111544,#111545);
#97268=AXIS2_PLACEMENT_3D('',#146090,#111546,#111547);
#97269=AXIS2_PLACEMENT_3D('',#146104,#111548,#111549);
#97270=AXIS2_PLACEMENT_3D('',#146116,#111550,#111551);
#97271=AXIS2_PLACEMENT_3D('',#146117,#111552,#111553);
#97272=AXIS2_PLACEMENT_3D('',#146131,#111554,#111555);
#97273=AXIS2_PLACEMENT_3D('',#146143,#111556,#111557);
#97274=AXIS2_PLACEMENT_3D('',#146144,#111558,#111559);
#97275=AXIS2_PLACEMENT_3D('',#146158,#111560,#111561);
#97276=AXIS2_PLACEMENT_3D('',#146170,#111562,#111563);
#97277=AXIS2_PLACEMENT_3D('',#146171,#111564,#111565);
#97278=AXIS2_PLACEMENT_3D('',#146185,#111566,#111567);
#97279=AXIS2_PLACEMENT_3D('',#146197,#111568,#111569);
#97280=AXIS2_PLACEMENT_3D('',#146198,#111570,#111571);
#97281=AXIS2_PLACEMENT_3D('',#146212,#111572,#111573);
#97282=AXIS2_PLACEMENT_3D('',#146224,#111574,#111575);
#97283=AXIS2_PLACEMENT_3D('',#146225,#111576,#111577);
#97284=AXIS2_PLACEMENT_3D('',#146239,#111578,#111579);
#97285=AXIS2_PLACEMENT_3D('',#146251,#111580,#111581);
#97286=AXIS2_PLACEMENT_3D('',#146252,#111582,#111583);
#97287=AXIS2_PLACEMENT_3D('',#146266,#111584,#111585);
#97288=AXIS2_PLACEMENT_3D('',#146278,#111586,#111587);
#97289=AXIS2_PLACEMENT_3D('',#146279,#111588,#111589);
#97290=AXIS2_PLACEMENT_3D('',#146293,#111590,#111591);
#97291=AXIS2_PLACEMENT_3D('',#146305,#111592,#111593);
#97292=AXIS2_PLACEMENT_3D('',#146306,#111594,#111595);
#97293=AXIS2_PLACEMENT_3D('',#146320,#111596,#111597);
#97294=AXIS2_PLACEMENT_3D('',#146332,#111598,#111599);
#97295=AXIS2_PLACEMENT_3D('',#146333,#111600,#111601);
#97296=AXIS2_PLACEMENT_3D('',#146347,#111602,#111603);
#97297=AXIS2_PLACEMENT_3D('',#146359,#111604,#111605);
#97298=AXIS2_PLACEMENT_3D('',#146360,#111606,#111607);
#97299=AXIS2_PLACEMENT_3D('',#146374,#111608,#111609);
#97300=AXIS2_PLACEMENT_3D('',#146386,#111610,#111611);
#97301=AXIS2_PLACEMENT_3D('',#146387,#111612,#111613);
#97302=AXIS2_PLACEMENT_3D('',#146401,#111614,#111615);
#97303=AXIS2_PLACEMENT_3D('',#146413,#111616,#111617);
#97304=AXIS2_PLACEMENT_3D('',#146414,#111618,#111619);
#97305=AXIS2_PLACEMENT_3D('',#146428,#111620,#111621);
#97306=AXIS2_PLACEMENT_3D('',#146440,#111622,#111623);
#97307=AXIS2_PLACEMENT_3D('',#146441,#111624,#111625);
#97308=AXIS2_PLACEMENT_3D('',#146455,#111626,#111627);
#97309=AXIS2_PLACEMENT_3D('',#146467,#111628,#111629);
#97310=AXIS2_PLACEMENT_3D('',#146468,#111630,#111631);
#97311=AXIS2_PLACEMENT_3D('',#146482,#111632,#111633);
#97312=AXIS2_PLACEMENT_3D('',#146494,#111634,#111635);
#97313=AXIS2_PLACEMENT_3D('',#146495,#111636,#111637);
#97314=AXIS2_PLACEMENT_3D('',#146509,#111638,#111639);
#97315=AXIS2_PLACEMENT_3D('',#146521,#111640,#111641);
#97316=AXIS2_PLACEMENT_3D('',#146522,#111642,#111643);
#97317=AXIS2_PLACEMENT_3D('',#146536,#111644,#111645);
#97318=AXIS2_PLACEMENT_3D('',#146548,#111646,#111647);
#97319=AXIS2_PLACEMENT_3D('',#146549,#111648,#111649);
#97320=AXIS2_PLACEMENT_3D('',#146563,#111650,#111651);
#97321=AXIS2_PLACEMENT_3D('',#146575,#111652,#111653);
#97322=AXIS2_PLACEMENT_3D('',#146576,#111654,#111655);
#97323=AXIS2_PLACEMENT_3D('',#146590,#111656,#111657);
#97324=AXIS2_PLACEMENT_3D('',#146602,#111658,#111659);
#97325=AXIS2_PLACEMENT_3D('',#146603,#111660,#111661);
#97326=AXIS2_PLACEMENT_3D('',#146617,#111662,#111663);
#97327=AXIS2_PLACEMENT_3D('',#146629,#111664,#111665);
#97328=AXIS2_PLACEMENT_3D('',#146630,#111666,#111667);
#97329=AXIS2_PLACEMENT_3D('',#146644,#111668,#111669);
#97330=AXIS2_PLACEMENT_3D('',#146656,#111670,#111671);
#97331=AXIS2_PLACEMENT_3D('',#146657,#111672,#111673);
#97332=AXIS2_PLACEMENT_3D('',#146671,#111674,#111675);
#97333=AXIS2_PLACEMENT_3D('',#146683,#111676,#111677);
#97334=AXIS2_PLACEMENT_3D('',#146684,#111678,#111679);
#97335=AXIS2_PLACEMENT_3D('',#146698,#111680,#111681);
#97336=AXIS2_PLACEMENT_3D('',#146710,#111682,#111683);
#97337=AXIS2_PLACEMENT_3D('',#146711,#111684,#111685);
#97338=AXIS2_PLACEMENT_3D('',#146725,#111686,#111687);
#97339=AXIS2_PLACEMENT_3D('',#146737,#111688,#111689);
#97340=AXIS2_PLACEMENT_3D('',#146738,#111690,#111691);
#97341=AXIS2_PLACEMENT_3D('',#146752,#111692,#111693);
#97342=AXIS2_PLACEMENT_3D('',#146764,#111694,#111695);
#97343=AXIS2_PLACEMENT_3D('',#146765,#111696,#111697);
#97344=AXIS2_PLACEMENT_3D('',#146779,#111698,#111699);
#97345=AXIS2_PLACEMENT_3D('',#146791,#111700,#111701);
#97346=AXIS2_PLACEMENT_3D('',#146792,#111702,#111703);
#97347=AXIS2_PLACEMENT_3D('',#146806,#111704,#111705);
#97348=AXIS2_PLACEMENT_3D('',#146818,#111706,#111707);
#97349=AXIS2_PLACEMENT_3D('',#146819,#111708,#111709);
#97350=AXIS2_PLACEMENT_3D('',#146833,#111710,#111711);
#97351=AXIS2_PLACEMENT_3D('',#146845,#111712,#111713);
#97352=AXIS2_PLACEMENT_3D('',#146846,#111714,#111715);
#97353=AXIS2_PLACEMENT_3D('',#146860,#111716,#111717);
#97354=AXIS2_PLACEMENT_3D('',#146872,#111718,#111719);
#97355=AXIS2_PLACEMENT_3D('',#146873,#111720,#111721);
#97356=AXIS2_PLACEMENT_3D('',#146887,#111722,#111723);
#97357=AXIS2_PLACEMENT_3D('',#146899,#111724,#111725);
#97358=AXIS2_PLACEMENT_3D('',#146900,#111726,#111727);
#97359=AXIS2_PLACEMENT_3D('',#146914,#111728,#111729);
#97360=AXIS2_PLACEMENT_3D('',#146926,#111730,#111731);
#97361=AXIS2_PLACEMENT_3D('',#146927,#111732,#111733);
#97362=AXIS2_PLACEMENT_3D('',#146941,#111734,#111735);
#97363=AXIS2_PLACEMENT_3D('',#146953,#111736,#111737);
#97364=AXIS2_PLACEMENT_3D('',#146954,#111738,#111739);
#97365=AXIS2_PLACEMENT_3D('',#146968,#111740,#111741);
#97366=AXIS2_PLACEMENT_3D('',#146980,#111742,#111743);
#97367=AXIS2_PLACEMENT_3D('',#146981,#111744,#111745);
#97368=AXIS2_PLACEMENT_3D('',#146995,#111746,#111747);
#97369=AXIS2_PLACEMENT_3D('',#147007,#111748,#111749);
#97370=AXIS2_PLACEMENT_3D('',#147008,#111750,#111751);
#97371=AXIS2_PLACEMENT_3D('',#147022,#111752,#111753);
#97372=AXIS2_PLACEMENT_3D('',#147034,#111754,#111755);
#97373=AXIS2_PLACEMENT_3D('',#147035,#111756,#111757);
#97374=AXIS2_PLACEMENT_3D('',#147049,#111758,#111759);
#97375=AXIS2_PLACEMENT_3D('',#147061,#111760,#111761);
#97376=AXIS2_PLACEMENT_3D('',#147062,#111762,#111763);
#97377=AXIS2_PLACEMENT_3D('',#147076,#111764,#111765);
#97378=AXIS2_PLACEMENT_3D('',#147088,#111766,#111767);
#97379=AXIS2_PLACEMENT_3D('',#147089,#111768,#111769);
#97380=AXIS2_PLACEMENT_3D('',#147103,#111770,#111771);
#97381=AXIS2_PLACEMENT_3D('',#147115,#111772,#111773);
#97382=AXIS2_PLACEMENT_3D('',#147116,#111774,#111775);
#97383=AXIS2_PLACEMENT_3D('',#147130,#111776,#111777);
#97384=AXIS2_PLACEMENT_3D('',#147142,#111778,#111779);
#97385=AXIS2_PLACEMENT_3D('',#147143,#111780,#111781);
#97386=AXIS2_PLACEMENT_3D('',#147157,#111782,#111783);
#97387=AXIS2_PLACEMENT_3D('',#147169,#111784,#111785);
#97388=AXIS2_PLACEMENT_3D('',#147170,#111786,#111787);
#97389=AXIS2_PLACEMENT_3D('',#147184,#111788,#111789);
#97390=AXIS2_PLACEMENT_3D('',#147196,#111790,#111791);
#97391=AXIS2_PLACEMENT_3D('',#147197,#111792,#111793);
#97392=AXIS2_PLACEMENT_3D('',#147211,#111794,#111795);
#97393=AXIS2_PLACEMENT_3D('',#147223,#111796,#111797);
#97394=AXIS2_PLACEMENT_3D('',#147224,#111798,#111799);
#97395=AXIS2_PLACEMENT_3D('',#147238,#111800,#111801);
#97396=AXIS2_PLACEMENT_3D('',#147250,#111802,#111803);
#97397=AXIS2_PLACEMENT_3D('',#147251,#111804,#111805);
#97398=AXIS2_PLACEMENT_3D('',#147265,#111806,#111807);
#97399=AXIS2_PLACEMENT_3D('',#147277,#111808,#111809);
#97400=AXIS2_PLACEMENT_3D('',#147278,#111810,#111811);
#97401=AXIS2_PLACEMENT_3D('',#147292,#111812,#111813);
#97402=AXIS2_PLACEMENT_3D('',#147304,#111814,#111815);
#97403=AXIS2_PLACEMENT_3D('',#147305,#111816,#111817);
#97404=AXIS2_PLACEMENT_3D('',#147319,#111818,#111819);
#97405=AXIS2_PLACEMENT_3D('',#147331,#111820,#111821);
#97406=AXIS2_PLACEMENT_3D('',#147332,#111822,#111823);
#97407=AXIS2_PLACEMENT_3D('',#147346,#111824,#111825);
#97408=AXIS2_PLACEMENT_3D('',#147358,#111826,#111827);
#97409=AXIS2_PLACEMENT_3D('',#147359,#111828,#111829);
#97410=AXIS2_PLACEMENT_3D('',#147373,#111830,#111831);
#97411=AXIS2_PLACEMENT_3D('',#147385,#111832,#111833);
#97412=AXIS2_PLACEMENT_3D('',#147386,#111834,#111835);
#97413=AXIS2_PLACEMENT_3D('',#147400,#111836,#111837);
#97414=AXIS2_PLACEMENT_3D('',#147412,#111838,#111839);
#97415=AXIS2_PLACEMENT_3D('',#147413,#111840,#111841);
#97416=AXIS2_PLACEMENT_3D('',#147427,#111842,#111843);
#97417=AXIS2_PLACEMENT_3D('',#147439,#111844,#111845);
#97418=AXIS2_PLACEMENT_3D('',#147440,#111846,#111847);
#97419=AXIS2_PLACEMENT_3D('',#147454,#111848,#111849);
#97420=AXIS2_PLACEMENT_3D('',#147466,#111850,#111851);
#97421=AXIS2_PLACEMENT_3D('',#147467,#111852,#111853);
#97422=AXIS2_PLACEMENT_3D('',#147481,#111854,#111855);
#97423=AXIS2_PLACEMENT_3D('',#147493,#111856,#111857);
#97424=AXIS2_PLACEMENT_3D('',#147494,#111858,#111859);
#97425=AXIS2_PLACEMENT_3D('',#147508,#111860,#111861);
#97426=AXIS2_PLACEMENT_3D('',#147520,#111862,#111863);
#97427=AXIS2_PLACEMENT_3D('',#147521,#111864,#111865);
#97428=AXIS2_PLACEMENT_3D('',#147535,#111866,#111867);
#97429=AXIS2_PLACEMENT_3D('',#147547,#111868,#111869);
#97430=AXIS2_PLACEMENT_3D('',#147548,#111870,#111871);
#97431=AXIS2_PLACEMENT_3D('',#147562,#111872,#111873);
#97432=AXIS2_PLACEMENT_3D('',#147574,#111874,#111875);
#97433=AXIS2_PLACEMENT_3D('',#147575,#111876,#111877);
#97434=AXIS2_PLACEMENT_3D('',#147589,#111878,#111879);
#97435=AXIS2_PLACEMENT_3D('',#147601,#111880,#111881);
#97436=AXIS2_PLACEMENT_3D('',#147602,#111882,#111883);
#97437=AXIS2_PLACEMENT_3D('',#147616,#111884,#111885);
#97438=AXIS2_PLACEMENT_3D('',#147628,#111886,#111887);
#97439=AXIS2_PLACEMENT_3D('',#147629,#111888,#111889);
#97440=AXIS2_PLACEMENT_3D('',#147643,#111890,#111891);
#97441=AXIS2_PLACEMENT_3D('',#147655,#111892,#111893);
#97442=AXIS2_PLACEMENT_3D('',#147656,#111894,#111895);
#97443=AXIS2_PLACEMENT_3D('',#147670,#111896,#111897);
#97444=AXIS2_PLACEMENT_3D('',#147682,#111898,#111899);
#97445=AXIS2_PLACEMENT_3D('',#147683,#111900,#111901);
#97446=AXIS2_PLACEMENT_3D('',#147697,#111902,#111903);
#97447=AXIS2_PLACEMENT_3D('',#147709,#111904,#111905);
#97448=AXIS2_PLACEMENT_3D('',#147710,#111906,#111907);
#97449=AXIS2_PLACEMENT_3D('',#147724,#111908,#111909);
#97450=AXIS2_PLACEMENT_3D('',#147736,#111910,#111911);
#97451=AXIS2_PLACEMENT_3D('',#147737,#111912,#111913);
#97452=AXIS2_PLACEMENT_3D('',#147751,#111914,#111915);
#97453=AXIS2_PLACEMENT_3D('',#147763,#111916,#111917);
#97454=AXIS2_PLACEMENT_3D('',#147764,#111918,#111919);
#97455=AXIS2_PLACEMENT_3D('',#147767,#111920,#111921);
#97456=AXIS2_PLACEMENT_3D('',#147770,#111923,#111924);
#97457=AXIS2_PLACEMENT_3D('',#147771,#111925,#111926);
#97458=AXIS2_PLACEMENT_3D('',#147772,#111927,#111928);
#97459=AXIS2_PLACEMENT_3D('',#147775,#111929,#111930);
#97460=AXIS2_PLACEMENT_3D('',#147778,#111932,#111933);
#97461=AXIS2_PLACEMENT_3D('',#147779,#111934,#111935);
#97462=AXIS2_PLACEMENT_3D('',#147780,#111936,#111937);
#97463=AXIS2_PLACEMENT_3D('',#147783,#111938,#111939);
#97464=AXIS2_PLACEMENT_3D('',#147786,#111941,#111942);
#97465=AXIS2_PLACEMENT_3D('',#147787,#111943,#111944);
#97466=AXIS2_PLACEMENT_3D('',#147788,#111945,#111946);
#97467=AXIS2_PLACEMENT_3D('',#147791,#111947,#111948);
#97468=AXIS2_PLACEMENT_3D('',#147794,#111950,#111951);
#97469=AXIS2_PLACEMENT_3D('',#147795,#111952,#111953);
#97470=AXIS2_PLACEMENT_3D('',#147796,#111954,#111955);
#97471=AXIS2_PLACEMENT_3D('',#147798,#111956,#111957);
#97472=AXIS2_PLACEMENT_3D('',#147801,#111959,#111960);
#97473=AXIS2_PLACEMENT_3D('',#147802,#111961,#111962);
#97474=AXIS2_PLACEMENT_3D('',#147804,#111963,#111964);
#97475=AXIS2_PLACEMENT_3D('',#147807,#111966,#111967);
#97476=AXIS2_PLACEMENT_3D('',#147808,#111968,#111969);
#97477=AXIS2_PLACEMENT_3D('',#147811,#111970,#111971);
#97478=AXIS2_PLACEMENT_3D('',#147814,#111973,#111974);
#97479=AXIS2_PLACEMENT_3D('',#147815,#111975,#111976);
#97480=AXIS2_PLACEMENT_3D('',#147816,#111977,#111978);
#97481=AXIS2_PLACEMENT_3D('',#147818,#111979,#111980);
#97482=AXIS2_PLACEMENT_3D('',#147821,#111982,#111983);
#97483=AXIS2_PLACEMENT_3D('',#147822,#111984,#111985);
#97484=AXIS2_PLACEMENT_3D('',#147824,#111987,#111988);
#97485=AXIS2_PLACEMENT_3D('',#147826,#111990,#111991);
#97486=AXIS2_PLACEMENT_3D('',#148786,#111993,#111994);
#97487=AXIS2_PLACEMENT_3D('',#149722,#111995,#111996);
#97488=AXIS2_PLACEMENT_3D('',#152036,#111998,#111999);
#97489=AXIS2_PLACEMENT_3D('',#152039,#112001,#112002);
#97490=AXIS2_PLACEMENT_3D('',#152040,#112003,#112004);
#97491=AXIS2_PLACEMENT_3D('',#152042,#112006,#112007);
#97492=AXIS2_PLACEMENT_3D('',#152043,#112008,#112009);
#97493=AXIS2_PLACEMENT_3D('',#152044,#112010,#112011);
#97494=AXIS2_PLACEMENT_3D('',#152045,#112012,#112013);
#97495=AXIS2_PLACEMENT_3D('',#152046,#112014,#112015);
#97496=AXIS2_PLACEMENT_3D('',#152047,#112016,#112017);
#97497=AXIS2_PLACEMENT_3D('',#152048,#112018,#112019);
#97498=AXIS2_PLACEMENT_3D('',#152049,#112020,#112021);
#97499=AXIS2_PLACEMENT_3D('',#152050,#112022,#112023);
#97500=AXIS2_PLACEMENT_3D('',#152051,#112024,#112025);
#97501=AXIS2_PLACEMENT_3D('',#152052,#112026,#112027);
#97502=AXIS2_PLACEMENT_3D('',#152053,#112028,#112029);
#97503=AXIS2_PLACEMENT_3D('',#152054,#112030,#112031);
#97504=AXIS2_PLACEMENT_3D('',#152055,#112032,#112033);
#97505=AXIS2_PLACEMENT_3D('',#152056,#112034,#112035);
#97506=AXIS2_PLACEMENT_3D('',#152057,#112036,#112037);
#97507=AXIS2_PLACEMENT_3D('',#152058,#112038,#112039);
#97508=AXIS2_PLACEMENT_3D('',#152059,#112040,#112041);
#97509=AXIS2_PLACEMENT_3D('',#152060,#112042,#112043);
#97510=AXIS2_PLACEMENT_3D('',#152061,#112044,#112045);
#97511=AXIS2_PLACEMENT_3D('',#152062,#112046,#112047);
#97512=AXIS2_PLACEMENT_3D('',#152063,#112048,#112049);
#97513=AXIS2_PLACEMENT_3D('',#152064,#112050,#112051);
#97514=AXIS2_PLACEMENT_3D('',#152065,#112052,#112053);
#97515=AXIS2_PLACEMENT_3D('',#152066,#112054,#112055);
#97516=AXIS2_PLACEMENT_3D('',#152067,#112056,#112057);
#97517=AXIS2_PLACEMENT_3D('',#152068,#112058,#112059);
#97518=AXIS2_PLACEMENT_3D('',#152069,#112060,#112061);
#97519=AXIS2_PLACEMENT_3D('',#152070,#112062,#112063);
#97520=AXIS2_PLACEMENT_3D('',#152071,#112064,#112065);
#97521=AXIS2_PLACEMENT_3D('',#152072,#112066,#112067);
#97522=AXIS2_PLACEMENT_3D('',#152073,#112068,#112069);
#97523=AXIS2_PLACEMENT_3D('',#152074,#112070,#112071);
#97524=AXIS2_PLACEMENT_3D('',#152075,#112072,#112073);
#97525=AXIS2_PLACEMENT_3D('',#152076,#112074,#112075);
#97526=AXIS2_PLACEMENT_3D('',#152077,#112076,#112077);
#97527=AXIS2_PLACEMENT_3D('',#152078,#112078,#112079);
#97528=AXIS2_PLACEMENT_3D('',#152079,#112080,#112081);
#97529=AXIS2_PLACEMENT_3D('',#152080,#112082,#112083);
#97530=AXIS2_PLACEMENT_3D('',#152081,#112084,#112085);
#97531=AXIS2_PLACEMENT_3D('',#152082,#112086,#112087);
#97532=AXIS2_PLACEMENT_3D('',#152083,#112088,#112089);
#97533=AXIS2_PLACEMENT_3D('',#152084,#112090,#112091);
#97534=AXIS2_PLACEMENT_3D('',#152085,#112092,#112093);
#97535=AXIS2_PLACEMENT_3D('',#152086,#112094,#112095);
#97536=AXIS2_PLACEMENT_3D('',#152087,#112096,#112097);
#97537=AXIS2_PLACEMENT_3D('',#152088,#112098,#112099);
#97538=AXIS2_PLACEMENT_3D('',#152089,#112100,#112101);
#97539=AXIS2_PLACEMENT_3D('',#152090,#112102,#112103);
#97540=AXIS2_PLACEMENT_3D('',#152091,#112104,#112105);
#97541=AXIS2_PLACEMENT_3D('',#152092,#112106,#112107);
#97542=AXIS2_PLACEMENT_3D('',#152093,#112108,#112109);
#97543=AXIS2_PLACEMENT_3D('',#152094,#112110,#112111);
#97544=AXIS2_PLACEMENT_3D('',#152095,#112112,#112113);
#97545=AXIS2_PLACEMENT_3D('',#152096,#112114,#112115);
#97546=AXIS2_PLACEMENT_3D('',#152097,#112116,#112117);
#97547=AXIS2_PLACEMENT_3D('',#152098,#112118,#112119);
#97548=AXIS2_PLACEMENT_3D('',#152099,#112120,#112121);
#97549=AXIS2_PLACEMENT_3D('',#152100,#112122,#112123);
#97550=AXIS2_PLACEMENT_3D('',#152101,#112124,#112125);
#97551=AXIS2_PLACEMENT_3D('',#152102,#112126,#112127);
#97552=AXIS2_PLACEMENT_3D('',#152103,#112128,#112129);
#97553=AXIS2_PLACEMENT_3D('',#152104,#112130,#112131);
#97554=AXIS2_PLACEMENT_3D('',#152105,#112132,#112133);
#97555=AXIS2_PLACEMENT_3D('',#152106,#112134,#112135);
#97556=AXIS2_PLACEMENT_3D('',#152107,#112136,#112137);
#97557=AXIS2_PLACEMENT_3D('',#152108,#112138,#112139);
#97558=AXIS2_PLACEMENT_3D('',#152109,#112140,#112141);
#97559=AXIS2_PLACEMENT_3D('',#152110,#112142,#112143);
#97560=AXIS2_PLACEMENT_3D('',#152111,#112144,#112145);
#97561=AXIS2_PLACEMENT_3D('',#152112,#112146,#112147);
#97562=AXIS2_PLACEMENT_3D('',#152113,#112148,#112149);
#97563=AXIS2_PLACEMENT_3D('',#152114,#112150,#112151);
#97564=AXIS2_PLACEMENT_3D('',#152115,#112152,#112153);
#97565=AXIS2_PLACEMENT_3D('',#152116,#112154,#112155);
#97566=AXIS2_PLACEMENT_3D('',#152117,#112156,#112157);
#97567=AXIS2_PLACEMENT_3D('',#152118,#112158,#112159);
#97568=AXIS2_PLACEMENT_3D('',#152119,#112160,#112161);
#97569=AXIS2_PLACEMENT_3D('',#152120,#112162,#112163);
#97570=AXIS2_PLACEMENT_3D('',#152121,#112164,#112165);
#97571=AXIS2_PLACEMENT_3D('',#152122,#112166,#112167);
#97572=AXIS2_PLACEMENT_3D('',#152123,#112168,#112169);
#97573=AXIS2_PLACEMENT_3D('',#152124,#112170,#112171);
#97574=AXIS2_PLACEMENT_3D('',#152125,#112172,#112173);
#97575=AXIS2_PLACEMENT_3D('',#152126,#112174,#112175);
#97576=AXIS2_PLACEMENT_3D('',#152127,#112176,#112177);
#97577=AXIS2_PLACEMENT_3D('',#152128,#112178,#112179);
#97578=AXIS2_PLACEMENT_3D('',#152129,#112180,#112181);
#97579=AXIS2_PLACEMENT_3D('',#152130,#112182,#112183);
#97580=AXIS2_PLACEMENT_3D('',#152131,#112184,#112185);
#97581=AXIS2_PLACEMENT_3D('',#152132,#112186,#112187);
#97582=AXIS2_PLACEMENT_3D('',#152133,#112188,#112189);
#97583=AXIS2_PLACEMENT_3D('',#152134,#112190,#112191);
#97584=AXIS2_PLACEMENT_3D('',#152135,#112192,#112193);
#97585=AXIS2_PLACEMENT_3D('',#152136,#112194,#112195);
#97586=AXIS2_PLACEMENT_3D('',#152137,#112196,#112197);
#97587=AXIS2_PLACEMENT_3D('',#152138,#112198,#112199);
#97588=AXIS2_PLACEMENT_3D('',#152139,#112200,#112201);
#97589=AXIS2_PLACEMENT_3D('',#152140,#112202,#112203);
#97590=AXIS2_PLACEMENT_3D('',#152141,#112204,#112205);
#97591=AXIS2_PLACEMENT_3D('',#152142,#112206,#112207);
#97592=AXIS2_PLACEMENT_3D('',#152143,#112208,#112209);
#97593=AXIS2_PLACEMENT_3D('',#152144,#112210,#112211);
#97594=AXIS2_PLACEMENT_3D('',#152145,#112212,#112213);
#97595=AXIS2_PLACEMENT_3D('',#152146,#112214,#112215);
#97596=AXIS2_PLACEMENT_3D('',#152147,#112216,#112217);
#97597=AXIS2_PLACEMENT_3D('',#152148,#112218,#112219);
#97598=AXIS2_PLACEMENT_3D('',#152149,#112220,#112221);
#97599=AXIS2_PLACEMENT_3D('',#152150,#112222,#112223);
#97600=AXIS2_PLACEMENT_3D('',#152151,#112224,#112225);
#97601=AXIS2_PLACEMENT_3D('',#152152,#112226,#112227);
#97602=AXIS2_PLACEMENT_3D('',#152153,#112228,#112229);
#97603=AXIS2_PLACEMENT_3D('',#152154,#112230,#112231);
#97604=AXIS2_PLACEMENT_3D('',#152155,#112232,#112233);
#97605=AXIS2_PLACEMENT_3D('',#152156,#112234,#112235);
#97606=AXIS2_PLACEMENT_3D('',#152157,#112236,#112237);
#97607=AXIS2_PLACEMENT_3D('',#152158,#112238,#112239);
#97608=AXIS2_PLACEMENT_3D('',#152159,#112240,#112241);
#97609=AXIS2_PLACEMENT_3D('',#152160,#112242,#112243);
#97610=AXIS2_PLACEMENT_3D('',#152161,#112244,#112245);
#97611=AXIS2_PLACEMENT_3D('',#152162,#112246,#112247);
#97612=AXIS2_PLACEMENT_3D('',#152163,#112248,#112249);
#97613=AXIS2_PLACEMENT_3D('',#152164,#112250,#112251);
#97614=AXIS2_PLACEMENT_3D('',#152165,#112252,#112253);
#97615=AXIS2_PLACEMENT_3D('',#152166,#112254,#112255);
#97616=AXIS2_PLACEMENT_3D('',#152167,#112256,#112257);
#97617=AXIS2_PLACEMENT_3D('',#152168,#112258,#112259);
#97618=AXIS2_PLACEMENT_3D('',#152169,#112260,#112261);
#97619=AXIS2_PLACEMENT_3D('',#152170,#112262,#112263);
#97620=AXIS2_PLACEMENT_3D('',#152171,#112264,#112265);
#97621=AXIS2_PLACEMENT_3D('',#152172,#112266,#112267);
#97622=AXIS2_PLACEMENT_3D('',#152173,#112268,#112269);
#97623=AXIS2_PLACEMENT_3D('',#152174,#112270,#112271);
#97624=AXIS2_PLACEMENT_3D('',#152175,#112272,#112273);
#97625=AXIS2_PLACEMENT_3D('',#152176,#112274,#112275);
#97626=AXIS2_PLACEMENT_3D('',#152177,#112276,#112277);
#97627=AXIS2_PLACEMENT_3D('',#152178,#112278,#112279);
#97628=AXIS2_PLACEMENT_3D('',#152179,#112280,#112281);
#97629=AXIS2_PLACEMENT_3D('',#152180,#112282,#112283);
#97630=AXIS2_PLACEMENT_3D('',#152181,#112284,#112285);
#97631=AXIS2_PLACEMENT_3D('',#152182,#112286,#112287);
#97632=AXIS2_PLACEMENT_3D('',#152183,#112288,#112289);
#97633=AXIS2_PLACEMENT_3D('',#152184,#112290,#112291);
#97634=AXIS2_PLACEMENT_3D('',#152185,#112292,#112293);
#97635=AXIS2_PLACEMENT_3D('',#152186,#112294,#112295);
#97636=AXIS2_PLACEMENT_3D('',#152187,#112296,#112297);
#97637=AXIS2_PLACEMENT_3D('',#152188,#112298,#112299);
#97638=AXIS2_PLACEMENT_3D('',#152189,#112300,#112301);
#97639=AXIS2_PLACEMENT_3D('',#152190,#112302,#112303);
#97640=AXIS2_PLACEMENT_3D('',#152191,#112304,#112305);
#97641=AXIS2_PLACEMENT_3D('',#152192,#112306,#112307);
#97642=AXIS2_PLACEMENT_3D('',#152193,#112308,#112309);
#97643=AXIS2_PLACEMENT_3D('',#152194,#112310,#112311);
#97644=AXIS2_PLACEMENT_3D('',#152195,#112312,#112313);
#97645=AXIS2_PLACEMENT_3D('',#152196,#112314,#112315);
#97646=AXIS2_PLACEMENT_3D('',#152197,#112316,#112317);
#97647=AXIS2_PLACEMENT_3D('',#152198,#112318,#112319);
#97648=AXIS2_PLACEMENT_3D('',#152199,#112320,#112321);
#97649=AXIS2_PLACEMENT_3D('',#152200,#112322,#112323);
#97650=AXIS2_PLACEMENT_3D('',#152201,#112324,#112325);
#97651=AXIS2_PLACEMENT_3D('',#152202,#112326,#112327);
#97652=AXIS2_PLACEMENT_3D('',#152203,#112328,#112329);
#97653=AXIS2_PLACEMENT_3D('',#152204,#112330,#112331);
#97654=AXIS2_PLACEMENT_3D('',#152205,#112332,#112333);
#97655=AXIS2_PLACEMENT_3D('',#152206,#112334,#112335);
#97656=AXIS2_PLACEMENT_3D('',#152207,#112336,#112337);
#97657=AXIS2_PLACEMENT_3D('',#152208,#112338,#112339);
#97658=AXIS2_PLACEMENT_3D('',#152209,#112340,#112341);
#97659=AXIS2_PLACEMENT_3D('',#152210,#112342,#112343);
#97660=AXIS2_PLACEMENT_3D('',#152211,#112344,#112345);
#97661=AXIS2_PLACEMENT_3D('',#152212,#112346,#112347);
#97662=AXIS2_PLACEMENT_3D('',#152213,#112348,#112349);
#97663=AXIS2_PLACEMENT_3D('',#152214,#112350,#112351);
#97664=AXIS2_PLACEMENT_3D('',#152215,#112352,#112353);
#97665=AXIS2_PLACEMENT_3D('',#152216,#112354,#112355);
#97666=AXIS2_PLACEMENT_3D('',#152217,#112356,#112357);
#97667=AXIS2_PLACEMENT_3D('',#152218,#112358,#112359);
#97668=AXIS2_PLACEMENT_3D('',#152219,#112360,#112361);
#97669=AXIS2_PLACEMENT_3D('',#152220,#112362,#112363);
#97670=AXIS2_PLACEMENT_3D('',#152221,#112364,#112365);
#97671=AXIS2_PLACEMENT_3D('',#152222,#112366,#112367);
#97672=AXIS2_PLACEMENT_3D('',#152223,#112368,#112369);
#97673=AXIS2_PLACEMENT_3D('',#152224,#112370,#112371);
#97674=AXIS2_PLACEMENT_3D('',#152225,#112372,#112373);
#97675=AXIS2_PLACEMENT_3D('',#152226,#112374,#112375);
#97676=AXIS2_PLACEMENT_3D('',#152227,#112376,#112377);
#97677=AXIS2_PLACEMENT_3D('',#152228,#112378,#112379);
#97678=AXIS2_PLACEMENT_3D('',#152229,#112380,#112381);
#97679=AXIS2_PLACEMENT_3D('',#152230,#112382,#112383);
#97680=AXIS2_PLACEMENT_3D('',#152231,#112384,#112385);
#97681=AXIS2_PLACEMENT_3D('',#152232,#112386,#112387);
#97682=AXIS2_PLACEMENT_3D('',#152233,#112388,#112389);
#97683=AXIS2_PLACEMENT_3D('',#152234,#112390,#112391);
#97684=AXIS2_PLACEMENT_3D('',#152235,#112392,#112393);
#97685=AXIS2_PLACEMENT_3D('',#152236,#112394,#112395);
#97686=AXIS2_PLACEMENT_3D('',#152237,#112396,#112397);
#97687=AXIS2_PLACEMENT_3D('',#152238,#112398,#112399);
#97688=AXIS2_PLACEMENT_3D('',#152239,#112400,#112401);
#97689=AXIS2_PLACEMENT_3D('',#152240,#112402,#112403);
#97690=AXIS2_PLACEMENT_3D('',#152241,#112404,#112405);
#97691=AXIS2_PLACEMENT_3D('',#152242,#112406,#112407);
#97692=AXIS2_PLACEMENT_3D('',#152243,#112408,#112409);
#97693=AXIS2_PLACEMENT_3D('',#152244,#112410,#112411);
#97694=AXIS2_PLACEMENT_3D('',#152245,#112412,#112413);
#97695=AXIS2_PLACEMENT_3D('',#152246,#112414,#112415);
#97696=AXIS2_PLACEMENT_3D('',#152247,#112416,#112417);
#97697=AXIS2_PLACEMENT_3D('',#152248,#112418,#112419);
#97698=AXIS2_PLACEMENT_3D('',#152249,#112420,#112421);
#97699=AXIS2_PLACEMENT_3D('',#152250,#112422,#112423);
#97700=AXIS2_PLACEMENT_3D('',#152251,#112424,#112425);
#97701=AXIS2_PLACEMENT_3D('',#152252,#112426,#112427);
#97702=AXIS2_PLACEMENT_3D('',#152253,#112428,#112429);
#97703=AXIS2_PLACEMENT_3D('',#152254,#112430,#112431);
#97704=AXIS2_PLACEMENT_3D('',#152255,#112432,#112433);
#97705=AXIS2_PLACEMENT_3D('',#152256,#112434,#112435);
#97706=AXIS2_PLACEMENT_3D('',#152257,#112436,#112437);
#97707=AXIS2_PLACEMENT_3D('',#152258,#112438,#112439);
#97708=AXIS2_PLACEMENT_3D('',#152259,#112440,#112441);
#97709=AXIS2_PLACEMENT_3D('',#152260,#112442,#112443);
#97710=AXIS2_PLACEMENT_3D('',#152261,#112444,#112445);
#97711=AXIS2_PLACEMENT_3D('',#152262,#112446,#112447);
#97712=AXIS2_PLACEMENT_3D('',#152263,#112448,#112449);
#97713=AXIS2_PLACEMENT_3D('',#152264,#112450,#112451);
#97714=AXIS2_PLACEMENT_3D('',#152265,#112452,#112453);
#97715=AXIS2_PLACEMENT_3D('',#152266,#112454,#112455);
#97716=AXIS2_PLACEMENT_3D('',#152267,#112456,#112457);
#97717=AXIS2_PLACEMENT_3D('',#152268,#112458,#112459);
#97718=AXIS2_PLACEMENT_3D('',#152269,#112460,#112461);
#97719=AXIS2_PLACEMENT_3D('',#152270,#112462,#112463);
#97720=AXIS2_PLACEMENT_3D('',#152271,#112464,#112465);
#97721=AXIS2_PLACEMENT_3D('',#152272,#112466,#112467);
#97722=AXIS2_PLACEMENT_3D('',#152273,#112468,#112469);
#97723=AXIS2_PLACEMENT_3D('',#152274,#112470,#112471);
#97724=AXIS2_PLACEMENT_3D('',#152275,#112472,#112473);
#97725=AXIS2_PLACEMENT_3D('',#152276,#112474,#112475);
#97726=AXIS2_PLACEMENT_3D('',#152277,#112476,#112477);
#97727=AXIS2_PLACEMENT_3D('',#152278,#112478,#112479);
#97728=AXIS2_PLACEMENT_3D('',#152279,#112480,#112481);
#97729=AXIS2_PLACEMENT_3D('',#152280,#112482,#112483);
#97730=AXIS2_PLACEMENT_3D('',#152281,#112484,#112485);
#97731=AXIS2_PLACEMENT_3D('',#152282,#112486,#112487);
#97732=AXIS2_PLACEMENT_3D('',#152283,#112488,#112489);
#97733=AXIS2_PLACEMENT_3D('',#152284,#112490,#112491);
#97734=AXIS2_PLACEMENT_3D('',#152285,#112492,#112493);
#97735=AXIS2_PLACEMENT_3D('',#152286,#112494,#112495);
#97736=AXIS2_PLACEMENT_3D('',#152287,#112496,#112497);
#97737=AXIS2_PLACEMENT_3D('',#152288,#112498,#112499);
#97738=AXIS2_PLACEMENT_3D('',#152289,#112500,#112501);
#97739=AXIS2_PLACEMENT_3D('',#152290,#112502,#112503);
#97740=AXIS2_PLACEMENT_3D('',#152291,#112504,#112505);
#97741=AXIS2_PLACEMENT_3D('',#152292,#112506,#112507);
#97742=AXIS2_PLACEMENT_3D('',#152293,#112508,#112509);
#97743=AXIS2_PLACEMENT_3D('',#152294,#112510,#112511);
#97744=AXIS2_PLACEMENT_3D('',#152295,#112512,#112513);
#97745=AXIS2_PLACEMENT_3D('',#152296,#112514,#112515);
#97746=AXIS2_PLACEMENT_3D('',#152297,#112516,#112517);
#97747=AXIS2_PLACEMENT_3D('',#152298,#112518,#112519);
#97748=AXIS2_PLACEMENT_3D('',#152299,#112520,#112521);
#97749=AXIS2_PLACEMENT_3D('',#152300,#112522,#112523);
#97750=AXIS2_PLACEMENT_3D('',#152301,#112524,#112525);
#97751=AXIS2_PLACEMENT_3D('',#152302,#112526,#112527);
#97752=AXIS2_PLACEMENT_3D('',#152303,#112528,#112529);
#97753=AXIS2_PLACEMENT_3D('',#152304,#112530,#112531);
#97754=AXIS2_PLACEMENT_3D('',#152305,#112532,#112533);
#97755=AXIS2_PLACEMENT_3D('',#152306,#112534,#112535);
#97756=AXIS2_PLACEMENT_3D('',#152307,#112536,#112537);
#97757=AXIS2_PLACEMENT_3D('',#152308,#112538,#112539);
#97758=AXIS2_PLACEMENT_3D('',#152309,#112540,#112541);
#97759=AXIS2_PLACEMENT_3D('',#152310,#112542,#112543);
#97760=AXIS2_PLACEMENT_3D('',#152311,#112544,#112545);
#97761=AXIS2_PLACEMENT_3D('',#152312,#112546,#112547);
#97762=AXIS2_PLACEMENT_3D('',#152313,#112548,#112549);
#97763=AXIS2_PLACEMENT_3D('',#152314,#112550,#112551);
#97764=AXIS2_PLACEMENT_3D('',#152315,#112552,#112553);
#97765=AXIS2_PLACEMENT_3D('',#152316,#112554,#112555);
#97766=AXIS2_PLACEMENT_3D('',#152317,#112556,#112557);
#97767=AXIS2_PLACEMENT_3D('',#152318,#112558,#112559);
#97768=AXIS2_PLACEMENT_3D('',#152319,#112560,#112561);
#97769=AXIS2_PLACEMENT_3D('',#152320,#112562,#112563);
#97770=AXIS2_PLACEMENT_3D('',#152321,#112564,#112565);
#97771=AXIS2_PLACEMENT_3D('',#152322,#112566,#112567);
#97772=AXIS2_PLACEMENT_3D('',#152323,#112568,#112569);
#97773=AXIS2_PLACEMENT_3D('',#152324,#112570,#112571);
#97774=AXIS2_PLACEMENT_3D('',#152325,#112572,#112573);
#97775=AXIS2_PLACEMENT_3D('',#152326,#112574,#112575);
#97776=AXIS2_PLACEMENT_3D('',#152327,#112576,#112577);
#97777=AXIS2_PLACEMENT_3D('',#152328,#112578,#112579);
#97778=AXIS2_PLACEMENT_3D('',#152329,#112580,#112581);
#97779=AXIS2_PLACEMENT_3D('',#152330,#112582,#112583);
#97780=AXIS2_PLACEMENT_3D('',#152331,#112584,#112585);
#97781=AXIS2_PLACEMENT_3D('',#152332,#112586,#112587);
#97782=AXIS2_PLACEMENT_3D('',#152333,#112588,#112589);
#97783=AXIS2_PLACEMENT_3D('',#152334,#112590,#112591);
#97784=AXIS2_PLACEMENT_3D('',#152335,#112592,#112593);
#97785=AXIS2_PLACEMENT_3D('',#152336,#112594,#112595);
#97786=AXIS2_PLACEMENT_3D('',#152337,#112596,#112597);
#97787=AXIS2_PLACEMENT_3D('',#152338,#112598,#112599);
#97788=AXIS2_PLACEMENT_3D('',#152339,#112600,#112601);
#97789=AXIS2_PLACEMENT_3D('',#152340,#112602,#112603);
#97790=AXIS2_PLACEMENT_3D('',#152341,#112604,#112605);
#97791=AXIS2_PLACEMENT_3D('',#152342,#112606,#112607);
#97792=AXIS2_PLACEMENT_3D('',#152343,#112608,#112609);
#97793=AXIS2_PLACEMENT_3D('',#152344,#112610,#112611);
#97794=AXIS2_PLACEMENT_3D('',#152345,#112612,#112613);
#97795=AXIS2_PLACEMENT_3D('',#152346,#112614,#112615);
#97796=AXIS2_PLACEMENT_3D('',#152347,#112616,#112617);
#97797=AXIS2_PLACEMENT_3D('',#152348,#112618,#112619);
#97798=AXIS2_PLACEMENT_3D('',#152349,#112620,#112621);
#97799=AXIS2_PLACEMENT_3D('',#152350,#112622,#112623);
#97800=AXIS2_PLACEMENT_3D('',#152351,#112624,#112625);
#97801=AXIS2_PLACEMENT_3D('',#152352,#112626,#112627);
#97802=AXIS2_PLACEMENT_3D('',#152353,#112628,#112629);
#97803=AXIS2_PLACEMENT_3D('',#152354,#112630,#112631);
#97804=AXIS2_PLACEMENT_3D('',#152355,#112632,#112633);
#97805=AXIS2_PLACEMENT_3D('',#152356,#112634,#112635);
#97806=AXIS2_PLACEMENT_3D('',#152357,#112636,#112637);
#97807=AXIS2_PLACEMENT_3D('',#152358,#112638,#112639);
#97808=AXIS2_PLACEMENT_3D('',#152359,#112640,#112641);
#97809=AXIS2_PLACEMENT_3D('',#152360,#112642,#112643);
#97810=AXIS2_PLACEMENT_3D('',#152361,#112644,#112645);
#97811=AXIS2_PLACEMENT_3D('',#152362,#112646,#112647);
#97812=AXIS2_PLACEMENT_3D('',#152363,#112648,#112649);
#97813=AXIS2_PLACEMENT_3D('',#152364,#112650,#112651);
#97814=AXIS2_PLACEMENT_3D('',#152365,#112652,#112653);
#97815=AXIS2_PLACEMENT_3D('',#152366,#112654,#112655);
#97816=AXIS2_PLACEMENT_3D('',#152367,#112656,#112657);
#97817=AXIS2_PLACEMENT_3D('',#152368,#112658,#112659);
#97818=AXIS2_PLACEMENT_3D('',#152369,#112660,#112661);
#97819=AXIS2_PLACEMENT_3D('',#152370,#112662,#112663);
#97820=AXIS2_PLACEMENT_3D('',#152371,#112664,#112665);
#97821=AXIS2_PLACEMENT_3D('',#152372,#112666,#112667);
#97822=AXIS2_PLACEMENT_3D('',#152373,#112668,#112669);
#97823=AXIS2_PLACEMENT_3D('',#152374,#112670,#112671);
#97824=AXIS2_PLACEMENT_3D('',#152375,#112672,#112673);
#97825=AXIS2_PLACEMENT_3D('',#152376,#112674,#112675);
#97826=AXIS2_PLACEMENT_3D('',#152377,#112676,#112677);
#97827=AXIS2_PLACEMENT_3D('',#152378,#112678,#112679);
#97828=AXIS2_PLACEMENT_3D('',#152379,#112680,#112681);
#97829=AXIS2_PLACEMENT_3D('',#152380,#112682,#112683);
#97830=AXIS2_PLACEMENT_3D('',#152381,#112684,#112685);
#97831=AXIS2_PLACEMENT_3D('',#152382,#112686,#112687);
#97832=AXIS2_PLACEMENT_3D('',#152383,#112688,#112689);
#97833=AXIS2_PLACEMENT_3D('',#152384,#112690,#112691);
#97834=AXIS2_PLACEMENT_3D('',#152385,#112692,#112693);
#97835=AXIS2_PLACEMENT_3D('',#152386,#112694,#112695);
#97836=AXIS2_PLACEMENT_3D('',#152387,#112696,#112697);
#97837=AXIS2_PLACEMENT_3D('',#152388,#112698,#112699);
#97838=AXIS2_PLACEMENT_3D('',#152389,#112700,#112701);
#97839=AXIS2_PLACEMENT_3D('',#152390,#112702,#112703);
#97840=AXIS2_PLACEMENT_3D('',#152391,#112704,#112705);
#97841=AXIS2_PLACEMENT_3D('',#152392,#112706,#112707);
#97842=AXIS2_PLACEMENT_3D('',#152393,#112708,#112709);
#97843=AXIS2_PLACEMENT_3D('',#152394,#112710,#112711);
#97844=AXIS2_PLACEMENT_3D('',#152395,#112712,#112713);
#97845=AXIS2_PLACEMENT_3D('',#152397,#112714,#112715);
#97846=AXIS2_PLACEMENT_3D('',#152400,#112717,#112718);
#97847=AXIS2_PLACEMENT_3D('',#152401,#112719,#112720);
#97848=AXIS2_PLACEMENT_3D('',#152403,#112721,#112722);
#97849=AXIS2_PLACEMENT_3D('',#152406,#112724,#112725);
#97850=AXIS2_PLACEMENT_3D('',#152407,#112726,#112727);
#97851=AXIS2_PLACEMENT_3D('',#152409,#112728,#112729);
#97852=AXIS2_PLACEMENT_3D('',#152411,#112730,#112731);
#97853=AXIS2_PLACEMENT_3D('',#152412,#112732,#112733);
#97854=AXIS2_PLACEMENT_3D('',#152413,#112734,#112735);
#97855=AXIS2_PLACEMENT_3D('',#152415,#112736,#112737);
#97856=AXIS2_PLACEMENT_3D('',#152417,#112738,#112739);
#97857=AXIS2_PLACEMENT_3D('',#152418,#112740,#112741);
#97858=AXIS2_PLACEMENT_3D('',#152419,#112742,#112743);
#97859=AXIS2_PLACEMENT_3D('',#152422,#112744,#112745);
#97860=AXIS2_PLACEMENT_3D('',#152424,#112746,#112747);
#97861=AXIS2_PLACEMENT_3D('',#152425,#112748,#112749);
#97862=AXIS2_PLACEMENT_3D('',#152426,#112750,#112751);
#97863=AXIS2_PLACEMENT_3D('',#152427,#112752,#112753);
#97864=AXIS2_PLACEMENT_3D('',#152429,#112754,#112755);
#97865=AXIS2_PLACEMENT_3D('',#152431,#112756,#112757);
#97866=AXIS2_PLACEMENT_3D('',#152432,#112758,#112759);
#97867=AXIS2_PLACEMENT_3D('',#152433,#112760,#112761);
#97868=AXIS2_PLACEMENT_3D('',#152435,#112762,#112763);
#97869=AXIS2_PLACEMENT_3D('',#152437,#112764,#112765);
#97870=AXIS2_PLACEMENT_3D('',#152439,#112766,#112767);
#97871=AXIS2_PLACEMENT_3D('',#152440,#112768,#112769);
#97872=AXIS2_PLACEMENT_3D('',#152441,#112770,#112771);
#97873=AXIS2_PLACEMENT_3D('',#152444,#112772,#112773);
#97874=AXIS2_PLACEMENT_3D('',#152446,#112774,#112775);
#97875=AXIS2_PLACEMENT_3D('',#152448,#112776,#112777);
#97876=AXIS2_PLACEMENT_3D('',#152449,#112778,#112779);
#97877=AXIS2_PLACEMENT_3D('',#152450,#112780,#112781);
#97878=AXIS2_PLACEMENT_3D('',#152453,#112782,#112783);
#97879=AXIS2_PLACEMENT_3D('',#152455,#112784,#112785);
#97880=AXIS2_PLACEMENT_3D('',#152457,#112786,#112787);
#97881=AXIS2_PLACEMENT_3D('',#152458,#112788,#112789);
#97882=AXIS2_PLACEMENT_3D('',#152459,#112790,#112791);
#97883=AXIS2_PLACEMENT_3D('',#152461,#112792,#112793);
#97884=AXIS2_PLACEMENT_3D('',#152463,#112794,#112795);
#97885=AXIS2_PLACEMENT_3D('',#152465,#112796,#112797);
#97886=AXIS2_PLACEMENT_3D('',#152466,#112798,#112799);
#97887=AXIS2_PLACEMENT_3D('',#152467,#112800,#112801);
#97888=AXIS2_PLACEMENT_3D('',#152469,#112802,#112803);
#97889=AXIS2_PLACEMENT_3D('',#152471,#112804,#112805);
#97890=AXIS2_PLACEMENT_3D('',#152473,#112806,#112807);
#97891=AXIS2_PLACEMENT_3D('',#152474,#112808,#112809);
#97892=AXIS2_PLACEMENT_3D('',#152475,#112810,#112811);
#97893=AXIS2_PLACEMENT_3D('',#152477,#112812,#112813);
#97894=AXIS2_PLACEMENT_3D('',#152479,#112814,#112815);
#97895=AXIS2_PLACEMENT_3D('',#152481,#112816,#112817);
#97896=AXIS2_PLACEMENT_3D('',#152482,#112818,#112819);
#97897=AXIS2_PLACEMENT_3D('',#152483,#112820,#112821);
#97898=AXIS2_PLACEMENT_3D('',#152486,#112822,#112823);
#97899=AXIS2_PLACEMENT_3D('',#152490,#112825,#112826);
#97900=AXIS2_PLACEMENT_3D('',#152492,#112828,#112829);
#97901=AXIS2_PLACEMENT_3D('',#152495,#112830,#112831);
#97902=AXIS2_PLACEMENT_3D('',#152499,#112833,#112834);
#97903=AXIS2_PLACEMENT_3D('',#152501,#112836,#112837);
#97904=AXIS2_PLACEMENT_3D('',#152503,#112838,#112839);
#97905=AXIS2_PLACEMENT_3D('',#152505,#112841,#112842);
#97906=AXIS2_PLACEMENT_3D('',#152507,#112844,#112845);
#97907=AXIS2_PLACEMENT_3D('',#152509,#112847,#112848);
#97908=AXIS2_PLACEMENT_3D('',#152511,#112849,#112850);
#97909=AXIS2_PLACEMENT_3D('',#152513,#112852,#112853);
#97910=AXIS2_PLACEMENT_3D('',#152516,#112854,#112855);
#97911=AXIS2_PLACEMENT_3D('',#152520,#112857,#112858);
#97912=AXIS2_PLACEMENT_3D('',#152522,#112860,#112861);
#97913=AXIS2_PLACEMENT_3D('',#152525,#112862,#112863);
#97914=AXIS2_PLACEMENT_3D('',#152529,#112865,#112866);
#97915=AXIS2_PLACEMENT_3D('',#152531,#112868,#112869);
#97916=AXIS2_PLACEMENT_3D('',#152534,#112870,#112871);
#97917=AXIS2_PLACEMENT_3D('',#152538,#112873,#112874);
#97918=AXIS2_PLACEMENT_3D('',#152540,#112876,#112877);
#97919=AXIS2_PLACEMENT_3D('',#152543,#112878,#112879);
#97920=AXIS2_PLACEMENT_3D('',#152547,#112881,#112882);
#97921=AXIS2_PLACEMENT_3D('',#152549,#112884,#112885);
#97922=AXIS2_PLACEMENT_3D('',#152551,#112887,#112888);
#97923=AXIS2_PLACEMENT_3D('',#152554,#112889,#112890);
#97924=AXIS2_PLACEMENT_3D('',#152556,#112891,#112892);
#97925=AXIS2_PLACEMENT_3D('',#152558,#112893,#112894);
#97926=AXIS2_PLACEMENT_3D('',#152560,#112895,#112896);
#97927=AXIS2_PLACEMENT_3D('',#152562,#112897,#112898);
#97928=AXIS2_PLACEMENT_3D('',#152564,#112899,#112900);
#97929=AXIS2_PLACEMENT_3D('',#152566,#112901,#112902);
#97930=AXIS2_PLACEMENT_3D('',#152568,#112903,#112904);
#97931=AXIS2_PLACEMENT_3D('',#152570,#112905,#112906);
#97932=AXIS2_PLACEMENT_3D('',#152572,#112907,#112908);
#97933=AXIS2_PLACEMENT_3D('',#152574,#112909,#112910);
#97934=AXIS2_PLACEMENT_3D('',#152576,#112911,#112912);
#97935=AXIS2_PLACEMENT_3D('',#152578,#112913,#112914);
#97936=AXIS2_PLACEMENT_3D('',#152580,#112915,#112916);
#97937=AXIS2_PLACEMENT_3D('',#152582,#112917,#112918);
#97938=AXIS2_PLACEMENT_3D('',#152584,#112919,#112920);
#97939=AXIS2_PLACEMENT_3D('',#152586,#112921,#112922);
#97940=AXIS2_PLACEMENT_3D('',#152588,#112923,#112924);
#97941=AXIS2_PLACEMENT_3D('',#152590,#112925,#112926);
#97942=AXIS2_PLACEMENT_3D('',#152592,#112927,#112928);
#97943=AXIS2_PLACEMENT_3D('',#152594,#112929,#112930);
#97944=AXIS2_PLACEMENT_3D('',#152596,#112931,#112932);
#97945=AXIS2_PLACEMENT_3D('',#152598,#112933,#112934);
#97946=AXIS2_PLACEMENT_3D('',#152600,#112935,#112936);
#97947=AXIS2_PLACEMENT_3D('',#152602,#112937,#112938);
#97948=AXIS2_PLACEMENT_3D('',#152604,#112939,#112940);
#97949=AXIS2_PLACEMENT_3D('',#152606,#112941,#112942);
#97950=AXIS2_PLACEMENT_3D('',#152608,#112943,#112944);
#97951=AXIS2_PLACEMENT_3D('',#152610,#112945,#112946);
#97952=AXIS2_PLACEMENT_3D('',#152611,#112947,#112948);
#97953=AXIS2_PLACEMENT_3D('',#152613,#112949,#112950);
#97954=AXIS2_PLACEMENT_3D('',#152615,#112951,#112952);
#97955=AXIS2_PLACEMENT_3D('',#152616,#112953,#112954);
#97956=AXIS2_PLACEMENT_3D('',#152618,#112955,#112956);
#97957=AXIS2_PLACEMENT_3D('',#152620,#112957,#112958);
#97958=AXIS2_PLACEMENT_3D('',#152622,#112959,#112960);
#97959=AXIS2_PLACEMENT_3D('',#152624,#112961,#112962);
#97960=AXIS2_PLACEMENT_3D('',#152626,#112963,#112964);
#97961=AXIS2_PLACEMENT_3D('',#152628,#112965,#112966);
#97962=AXIS2_PLACEMENT_3D('',#152630,#112967,#112968);
#97963=AXIS2_PLACEMENT_3D('',#152632,#112969,#112970);
#97964=AXIS2_PLACEMENT_3D('',#152634,#112971,#112972);
#97965=AXIS2_PLACEMENT_3D('',#152636,#112973,#112974);
#97966=AXIS2_PLACEMENT_3D('',#152638,#112975,#112976);
#97967=AXIS2_PLACEMENT_3D('',#152640,#112977,#112978);
#97968=AXIS2_PLACEMENT_3D('',#152642,#112979,#112980);
#97969=AXIS2_PLACEMENT_3D('',#152644,#112981,#112982);
#97970=AXIS2_PLACEMENT_3D('',#152646,#112983,#112984);
#97971=AXIS2_PLACEMENT_3D('',#152648,#112985,#112986);
#97972=AXIS2_PLACEMENT_3D('',#152650,#112987,#112988);
#97973=AXIS2_PLACEMENT_3D('',#152652,#112989,#112990);
#97974=AXIS2_PLACEMENT_3D('',#152654,#112991,#112992);
#97975=AXIS2_PLACEMENT_3D('',#152656,#112993,#112994);
#97976=AXIS2_PLACEMENT_3D('',#152658,#112995,#112996);
#97977=AXIS2_PLACEMENT_3D('',#152660,#112997,#112998);
#97978=AXIS2_PLACEMENT_3D('',#152662,#112999,#113000);
#97979=AXIS2_PLACEMENT_3D('',#152664,#113001,#113002);
#97980=AXIS2_PLACEMENT_3D('',#152666,#113003,#113004);
#97981=AXIS2_PLACEMENT_3D('',#152668,#113005,#113006);
#97982=AXIS2_PLACEMENT_3D('',#152670,#113007,#113008);
#97983=AXIS2_PLACEMENT_3D('',#152672,#113009,#113010);
#97984=AXIS2_PLACEMENT_3D('',#152674,#113011,#113012);
#97985=AXIS2_PLACEMENT_3D('',#152676,#113013,#113014);
#97986=AXIS2_PLACEMENT_3D('',#152678,#113015,#113016);
#97987=AXIS2_PLACEMENT_3D('',#152680,#113017,#113018);
#97988=AXIS2_PLACEMENT_3D('',#152682,#113019,#113020);
#97989=AXIS2_PLACEMENT_3D('',#152684,#113021,#113022);
#97990=AXIS2_PLACEMENT_3D('',#152686,#113023,#113024);
#97991=AXIS2_PLACEMENT_3D('',#152688,#113025,#113026);
#97992=AXIS2_PLACEMENT_3D('',#152690,#113027,#113028);
#97993=AXIS2_PLACEMENT_3D('',#152692,#113029,#113030);
#97994=AXIS2_PLACEMENT_3D('',#152694,#113031,#113032);
#97995=AXIS2_PLACEMENT_3D('',#152696,#113033,#113034);
#97996=AXIS2_PLACEMENT_3D('',#152698,#113035,#113036);
#97997=AXIS2_PLACEMENT_3D('',#152700,#113037,#113038);
#97998=AXIS2_PLACEMENT_3D('',#152702,#113039,#113040);
#97999=AXIS2_PLACEMENT_3D('',#152704,#113041,#113042);
#98000=AXIS2_PLACEMENT_3D('',#152706,#113043,#113044);
#98001=AXIS2_PLACEMENT_3D('',#152708,#113045,#113046);
#98002=AXIS2_PLACEMENT_3D('',#152710,#113047,#113048);
#98003=AXIS2_PLACEMENT_3D('',#152712,#113049,#113050);
#98004=AXIS2_PLACEMENT_3D('',#152714,#113051,#113052);
#98005=AXIS2_PLACEMENT_3D('',#152716,#113053,#113054);
#98006=AXIS2_PLACEMENT_3D('',#152718,#113055,#113056);
#98007=AXIS2_PLACEMENT_3D('',#152720,#113057,#113058);
#98008=AXIS2_PLACEMENT_3D('',#152722,#113059,#113060);
#98009=AXIS2_PLACEMENT_3D('',#152724,#113061,#113062);
#98010=AXIS2_PLACEMENT_3D('',#152726,#113063,#113064);
#98011=AXIS2_PLACEMENT_3D('',#152728,#113065,#113066);
#98012=AXIS2_PLACEMENT_3D('',#152730,#113067,#113068);
#98013=AXIS2_PLACEMENT_3D('',#152732,#113069,#113070);
#98014=AXIS2_PLACEMENT_3D('',#152734,#113071,#113072);
#98015=AXIS2_PLACEMENT_3D('',#152736,#113073,#113074);
#98016=AXIS2_PLACEMENT_3D('',#152738,#113075,#113076);
#98017=AXIS2_PLACEMENT_3D('',#152740,#113077,#113078);
#98018=AXIS2_PLACEMENT_3D('',#152742,#113079,#113080);
#98019=AXIS2_PLACEMENT_3D('',#152744,#113081,#113082);
#98020=AXIS2_PLACEMENT_3D('',#152746,#113083,#113084);
#98021=AXIS2_PLACEMENT_3D('',#152748,#113085,#113086);
#98022=AXIS2_PLACEMENT_3D('',#152750,#113087,#113088);
#98023=AXIS2_PLACEMENT_3D('',#152752,#113089,#113090);
#98024=AXIS2_PLACEMENT_3D('',#152754,#113091,#113092);
#98025=AXIS2_PLACEMENT_3D('',#152756,#113093,#113094);
#98026=AXIS2_PLACEMENT_3D('',#152758,#113095,#113096);
#98027=AXIS2_PLACEMENT_3D('',#152760,#113097,#113098);
#98028=AXIS2_PLACEMENT_3D('',#152762,#113099,#113100);
#98029=AXIS2_PLACEMENT_3D('',#152764,#113101,#113102);
#98030=AXIS2_PLACEMENT_3D('',#152766,#113103,#113104);
#98031=AXIS2_PLACEMENT_3D('',#152768,#113105,#113106);
#98032=AXIS2_PLACEMENT_3D('',#152770,#113107,#113108);
#98033=AXIS2_PLACEMENT_3D('',#152772,#113109,#113110);
#98034=AXIS2_PLACEMENT_3D('',#152774,#113111,#113112);
#98035=AXIS2_PLACEMENT_3D('',#152776,#113113,#113114);
#98036=AXIS2_PLACEMENT_3D('',#152778,#113115,#113116);
#98037=AXIS2_PLACEMENT_3D('',#152780,#113117,#113118);
#98038=AXIS2_PLACEMENT_3D('',#152782,#113119,#113120);
#98039=AXIS2_PLACEMENT_3D('',#152784,#113121,#113122);
#98040=AXIS2_PLACEMENT_3D('',#152785,#113123,#113124);
#98041=AXIS2_PLACEMENT_3D('',#152787,#113125,#113126);
#98042=AXIS2_PLACEMENT_3D('',#152789,#113127,#113128);
#98043=AXIS2_PLACEMENT_3D('',#152790,#113129,#113130);
#98044=AXIS2_PLACEMENT_3D('',#152792,#113131,#113132);
#98045=AXIS2_PLACEMENT_3D('',#152794,#113133,#113134);
#98046=AXIS2_PLACEMENT_3D('',#152796,#113135,#113136);
#98047=AXIS2_PLACEMENT_3D('',#152798,#113137,#113138);
#98048=AXIS2_PLACEMENT_3D('',#152800,#113139,#113140);
#98049=AXIS2_PLACEMENT_3D('',#152802,#113141,#113142);
#98050=AXIS2_PLACEMENT_3D('',#152804,#113143,#113144);
#98051=AXIS2_PLACEMENT_3D('',#152806,#113145,#113146);
#98052=AXIS2_PLACEMENT_3D('',#152808,#113147,#113148);
#98053=AXIS2_PLACEMENT_3D('',#152810,#113149,#113150);
#98054=AXIS2_PLACEMENT_3D('',#152812,#113151,#113152);
#98055=AXIS2_PLACEMENT_3D('',#152814,#113153,#113154);
#98056=AXIS2_PLACEMENT_3D('',#152816,#113155,#113156);
#98057=AXIS2_PLACEMENT_3D('',#152818,#113157,#113158);
#98058=AXIS2_PLACEMENT_3D('',#152820,#113159,#113160);
#98059=AXIS2_PLACEMENT_3D('',#152822,#113161,#113162);
#98060=AXIS2_PLACEMENT_3D('',#152824,#113163,#113164);
#98061=AXIS2_PLACEMENT_3D('',#152826,#113165,#113166);
#98062=AXIS2_PLACEMENT_3D('',#152828,#113167,#113168);
#98063=AXIS2_PLACEMENT_3D('',#152830,#113169,#113170);
#98064=AXIS2_PLACEMENT_3D('',#152832,#113171,#113172);
#98065=AXIS2_PLACEMENT_3D('',#152834,#113173,#113174);
#98066=AXIS2_PLACEMENT_3D('',#152835,#113175,#113176);
#98067=AXIS2_PLACEMENT_3D('',#152838,#113177,#113178);
#98068=AXIS2_PLACEMENT_3D('',#152840,#113179,#113180);
#98069=AXIS2_PLACEMENT_3D('',#152843,#113182,#113183);
#98070=AXIS2_PLACEMENT_3D('',#152845,#113184,#113185);
#98071=AXIS2_PLACEMENT_3D('',#152848,#113187,#113188);
#98072=AXIS2_PLACEMENT_3D('',#152853,#113190,#113191);
#98073=AXIS2_PLACEMENT_3D('',#152854,#113192,#113193);
#98074=AXIS2_PLACEMENT_3D('',#152858,#113195,#113196);
#98075=AXIS2_PLACEMENT_3D('',#152860,#113197,#113198);
#98076=AXIS2_PLACEMENT_3D('',#152861,#113199,#113200);
#98077=AXIS2_PLACEMENT_3D('',#152862,#113201,#113202);
#98078=AXIS2_PLACEMENT_3D('',#152867,#113205,#113206);
#98079=AXIS2_PLACEMENT_3D('',#152868,#113207,#113208);
#98080=AXIS2_PLACEMENT_3D('',#152872,#113210,#113211);
#98081=AXIS2_PLACEMENT_3D('',#152874,#113213,#113214);
#98082=AXIS2_PLACEMENT_3D('',#152879,#113217,#113218);
#98083=AXIS2_PLACEMENT_3D('',#152880,#113219,#113220);
#98084=AXIS2_PLACEMENT_3D('',#152885,#113223,#113224);
#98085=AXIS2_PLACEMENT_3D('',#152886,#113225,#113226);
#98086=AXIS2_PLACEMENT_3D('',#152891,#113229,#113230);
#98087=AXIS2_PLACEMENT_3D('',#152892,#113231,#113232);
#98088=AXIS2_PLACEMENT_3D('',#152895,#113234,#113235);
#98089=AXIS2_PLACEMENT_3D('',#152896,#113236,#113237);
#98090=AXIS2_PLACEMENT_3D('',#152899,#113239,#113240);
#98091=AXIS2_PLACEMENT_3D('',#152900,#113241,#113242);
#98092=AXIS2_PLACEMENT_3D('',#152904,#113244,#113245);
#98093=AXIS2_PLACEMENT_3D('',#152906,#113247,#113248);
#98094=AXIS2_PLACEMENT_3D('',#152911,#113251,#113252);
#98095=AXIS2_PLACEMENT_3D('',#152912,#113253,#113254);
#98096=AXIS2_PLACEMENT_3D('',#152917,#113257,#113258);
#98097=AXIS2_PLACEMENT_3D('',#152918,#113259,#113260);
#98098=AXIS2_PLACEMENT_3D('',#152922,#113262,#113263);
#98099=AXIS2_PLACEMENT_3D('',#152924,#113265,#113266);
#98100=AXIS2_PLACEMENT_3D('',#152929,#113269,#113270);
#98101=AXIS2_PLACEMENT_3D('',#152930,#113271,#113272);
#98102=AXIS2_PLACEMENT_3D('',#152932,#113273,#113274);
#98103=AXIS2_PLACEMENT_3D('',#152934,#113276,#113277);
#98104=AXIS2_PLACEMENT_3D('',#152936,#113278,#113279);
#98105=AXIS2_PLACEMENT_3D('',#152938,#113281,#113282);
#98106=AXIS2_PLACEMENT_3D('',#152942,#113284,#113285);
#98107=AXIS2_PLACEMENT_3D('',#152944,#113287,#113288);
#98108=AXIS2_PLACEMENT_3D('',#152949,#113291,#113292);
#98109=AXIS2_PLACEMENT_3D('',#152950,#113293,#113294);
#98110=AXIS2_PLACEMENT_3D('',#152954,#113296,#113297);
#98111=AXIS2_PLACEMENT_3D('',#152956,#113299,#113300);
#98112=AXIS2_PLACEMENT_3D('',#152961,#113303,#113304);
#98113=AXIS2_PLACEMENT_3D('',#152962,#113305,#113306);
#98114=AXIS2_PLACEMENT_3D('',#152967,#113309,#113310);
#98115=AXIS2_PLACEMENT_3D('',#152968,#113311,#113312);
#98116=AXIS2_PLACEMENT_3D('',#152972,#113314,#113315);
#98117=AXIS2_PLACEMENT_3D('',#152974,#113317,#113318);
#98118=AXIS2_PLACEMENT_3D('',#152979,#113321,#113322);
#98119=AXIS2_PLACEMENT_3D('',#152980,#113323,#113324);
#98120=AXIS2_PLACEMENT_3D('',#152984,#113326,#113327);
#98121=AXIS2_PLACEMENT_3D('',#152986,#113329,#113330);
#98122=AXIS2_PLACEMENT_3D('',#152990,#113332,#113333);
#98123=AXIS2_PLACEMENT_3D('',#152992,#113335,#113336);
#98124=AXIS2_PLACEMENT_3D('',#152996,#113338,#113339);
#98125=AXIS2_PLACEMENT_3D('',#152998,#113341,#113342);
#98126=AXIS2_PLACEMENT_3D('',#153003,#113345,#113346);
#98127=AXIS2_PLACEMENT_3D('',#153004,#113347,#113348);
#98128=AXIS2_PLACEMENT_3D('',#153008,#113350,#113351);
#98129=AXIS2_PLACEMENT_3D('',#153010,#113353,#113354);
#98130=AXIS2_PLACEMENT_3D('',#153015,#113357,#113358);
#98131=AXIS2_PLACEMENT_3D('',#153016,#113359,#113360);
#98132=AXIS2_PLACEMENT_3D('',#153021,#113363,#113364);
#98133=AXIS2_PLACEMENT_3D('',#153022,#113365,#113366);
#98134=AXIS2_PLACEMENT_3D('',#153026,#113368,#113369);
#98135=AXIS2_PLACEMENT_3D('',#153028,#113371,#113372);
#98136=AXIS2_PLACEMENT_3D('',#153033,#113375,#113376);
#98137=AXIS2_PLACEMENT_3D('',#153034,#113377,#113378);
#98138=AXIS2_PLACEMENT_3D('',#153038,#113380,#113381);
#98139=AXIS2_PLACEMENT_3D('',#153040,#113383,#113384);
#98140=AXIS2_PLACEMENT_3D('',#153044,#113386,#113387);
#98141=AXIS2_PLACEMENT_3D('',#153046,#113389,#113390);
#98142=AXIS2_PLACEMENT_3D('',#153050,#113392,#113393);
#98143=AXIS2_PLACEMENT_3D('',#153052,#113395,#113396);
#98144=AXIS2_PLACEMENT_3D('',#153057,#113399,#113400);
#98145=AXIS2_PLACEMENT_3D('',#153058,#113401,#113402);
#98146=AXIS2_PLACEMENT_3D('',#153063,#113405,#113406);
#98147=AXIS2_PLACEMENT_3D('',#153064,#113407,#113408);
#98148=AXIS2_PLACEMENT_3D('',#153069,#113411,#113412);
#98149=AXIS2_PLACEMENT_3D('',#153070,#113413,#113414);
#98150=AXIS2_PLACEMENT_3D('',#153072,#113415,#113416);
#98151=AXIS2_PLACEMENT_3D('',#153074,#113417,#113418);
#98152=AXIS2_PLACEMENT_3D('',#153076,#113419,#113420);
#98153=AXIS2_PLACEMENT_3D('',#153077,#113421,#113422);
#98154=AXIS2_PLACEMENT_3D('',#153079,#113423,#113424);
#98155=AXIS2_PLACEMENT_3D('',#153081,#113425,#113426);
#98156=AXIS2_PLACEMENT_3D('',#153082,#113427,#113428);
#98157=AXIS2_PLACEMENT_3D('',#153084,#113429,#113430);
#98158=AXIS2_PLACEMENT_3D('',#153086,#113431,#113432);
#98159=AXIS2_PLACEMENT_3D('',#153087,#113433,#113434);
#98160=AXIS2_PLACEMENT_3D('',#153089,#113435,#113436);
#98161=AXIS2_PLACEMENT_3D('',#153091,#113437,#113438);
#98162=AXIS2_PLACEMENT_3D('',#153092,#113439,#113440);
#98163=AXIS2_PLACEMENT_3D('',#153094,#113441,#113442);
#98164=AXIS2_PLACEMENT_3D('',#153096,#113443,#113444);
#98165=AXIS2_PLACEMENT_3D('',#153097,#113445,#113446);
#98166=AXIS2_PLACEMENT_3D('',#153099,#113447,#113448);
#98167=AXIS2_PLACEMENT_3D('',#153100,#113449,#113450);
#98168=AXIS2_PLACEMENT_3D('',#153102,#113451,#113452);
#98169=AXIS2_PLACEMENT_3D('',#153103,#113453,#113454);
#98170=AXIS2_PLACEMENT_3D('',#153105,#113455,#113456);
#98171=AXIS2_PLACEMENT_3D('',#153107,#113457,#113458);
#98172=AXIS2_PLACEMENT_3D('',#153109,#113459,#113460);
#98173=AXIS2_PLACEMENT_3D('',#153111,#113461,#113462);
#98174=AXIS2_PLACEMENT_3D('',#153113,#113463,#113464);
#98175=AXIS2_PLACEMENT_3D('',#153115,#113465,#113466);
#98176=AXIS2_PLACEMENT_3D('',#153116,#113467,#113468);
#98177=AXIS2_PLACEMENT_3D('',#153118,#113469,#113470);
#98178=AXIS2_PLACEMENT_3D('',#153120,#113471,#113472);
#98179=AXIS2_PLACEMENT_3D('',#153121,#113473,#113474);
#98180=AXIS2_PLACEMENT_3D('',#153123,#113475,#113476);
#98181=AXIS2_PLACEMENT_3D('',#153125,#113477,#113478);
#98182=AXIS2_PLACEMENT_3D('',#153126,#113479,#113480);
#98183=AXIS2_PLACEMENT_3D('',#153128,#113481,#113482);
#98184=AXIS2_PLACEMENT_3D('',#153130,#113483,#113484);
#98185=AXIS2_PLACEMENT_3D('',#153131,#113485,#113486);
#98186=AXIS2_PLACEMENT_3D('',#153133,#113487,#113488);
#98187=AXIS2_PLACEMENT_3D('',#153135,#113489,#113490);
#98188=AXIS2_PLACEMENT_3D('',#153136,#113491,#113492);
#98189=AXIS2_PLACEMENT_3D('',#153138,#113493,#113494);
#98190=AXIS2_PLACEMENT_3D('',#153140,#113495,#113496);
#98191=AXIS2_PLACEMENT_3D('',#153141,#113497,#113498);
#98192=AXIS2_PLACEMENT_3D('',#153143,#113499,#113500);
#98193=AXIS2_PLACEMENT_3D('',#153145,#113501,#113502);
#98194=AXIS2_PLACEMENT_3D('',#153146,#113503,#113504);
#98195=AXIS2_PLACEMENT_3D('',#153148,#113505,#113506);
#98196=AXIS2_PLACEMENT_3D('',#153150,#113507,#113508);
#98197=AXIS2_PLACEMENT_3D('',#153151,#113509,#113510);
#98198=AXIS2_PLACEMENT_3D('',#153153,#113511,#113512);
#98199=AXIS2_PLACEMENT_3D('',#153155,#113513,#113514);
#98200=AXIS2_PLACEMENT_3D('',#153156,#113515,#113516);
#98201=AXIS2_PLACEMENT_3D('',#153158,#113517,#113518);
#98202=AXIS2_PLACEMENT_3D('',#153160,#113519,#113520);
#98203=AXIS2_PLACEMENT_3D('',#153161,#113521,#113522);
#98204=AXIS2_PLACEMENT_3D('',#153163,#113523,#113524);
#98205=AXIS2_PLACEMENT_3D('',#153165,#113525,#113526);
#98206=AXIS2_PLACEMENT_3D('',#153166,#113527,#113528);
#98207=AXIS2_PLACEMENT_3D('',#153168,#113529,#113530);
#98208=AXIS2_PLACEMENT_3D('',#153170,#113531,#113532);
#98209=AXIS2_PLACEMENT_3D('',#153171,#113533,#113534);
#98210=AXIS2_PLACEMENT_3D('',#153173,#113535,#113536);
#98211=AXIS2_PLACEMENT_3D('',#153175,#113537,#113538);
#98212=AXIS2_PLACEMENT_3D('',#153176,#113539,#113540);
#98213=AXIS2_PLACEMENT_3D('',#153178,#113541,#113542);
#98214=AXIS2_PLACEMENT_3D('',#153180,#113543,#113544);
#98215=AXIS2_PLACEMENT_3D('',#153181,#113545,#113546);
#98216=AXIS2_PLACEMENT_3D('',#153183,#113547,#113548);
#98217=AXIS2_PLACEMENT_3D('',#153185,#113549,#113550);
#98218=AXIS2_PLACEMENT_3D('',#153186,#113551,#113552);
#98219=AXIS2_PLACEMENT_3D('',#153188,#113553,#113554);
#98220=AXIS2_PLACEMENT_3D('',#153190,#113555,#113556);
#98221=AXIS2_PLACEMENT_3D('',#153191,#113557,#113558);
#98222=AXIS2_PLACEMENT_3D('',#153193,#113559,#113560);
#98223=AXIS2_PLACEMENT_3D('',#153195,#113561,#113562);
#98224=AXIS2_PLACEMENT_3D('',#153196,#113563,#113564);
#98225=AXIS2_PLACEMENT_3D('',#153198,#113565,#113566);
#98226=AXIS2_PLACEMENT_3D('',#153200,#113567,#113568);
#98227=AXIS2_PLACEMENT_3D('',#153201,#113569,#113570);
#98228=AXIS2_PLACEMENT_3D('',#153203,#113571,#113572);
#98229=AXIS2_PLACEMENT_3D('',#153205,#113573,#113574);
#98230=AXIS2_PLACEMENT_3D('',#153206,#113575,#113576);
#98231=AXIS2_PLACEMENT_3D('',#153208,#113577,#113578);
#98232=AXIS2_PLACEMENT_3D('',#153210,#113579,#113580);
#98233=AXIS2_PLACEMENT_3D('',#153211,#113581,#113582);
#98234=AXIS2_PLACEMENT_3D('',#153213,#113583,#113584);
#98235=AXIS2_PLACEMENT_3D('',#153214,#113585,#113586);
#98236=AXIS2_PLACEMENT_3D('',#153216,#113587,#113588);
#98237=AXIS2_PLACEMENT_3D('',#153217,#113589,#113590);
#98238=AXIS2_PLACEMENT_3D('',#153219,#113591,#113592);
#98239=AXIS2_PLACEMENT_3D('',#153221,#113593,#113594);
#98240=AXIS2_PLACEMENT_3D('',#153222,#113595,#113596);
#98241=AXIS2_PLACEMENT_3D('',#153224,#113597,#113598);
#98242=AXIS2_PLACEMENT_3D('',#153226,#113599,#113600);
#98243=AXIS2_PLACEMENT_3D('',#153227,#113601,#113602);
#98244=AXIS2_PLACEMENT_3D('',#153229,#113603,#113604);
#98245=AXIS2_PLACEMENT_3D('',#153231,#113605,#113606);
#98246=AXIS2_PLACEMENT_3D('',#153232,#113607,#113608);
#98247=AXIS2_PLACEMENT_3D('',#153234,#113609,#113610);
#98248=AXIS2_PLACEMENT_3D('',#153236,#113611,#113612);
#98249=AXIS2_PLACEMENT_3D('',#153237,#113613,#113614);
#98250=AXIS2_PLACEMENT_3D('',#153239,#113615,#113616);
#98251=AXIS2_PLACEMENT_3D('',#153241,#113617,#113618);
#98252=AXIS2_PLACEMENT_3D('',#153242,#113619,#113620);
#98253=AXIS2_PLACEMENT_3D('',#153244,#113621,#113622);
#98254=AXIS2_PLACEMENT_3D('',#153246,#113623,#113624);
#98255=AXIS2_PLACEMENT_3D('',#153247,#113625,#113626);
#98256=AXIS2_PLACEMENT_3D('',#153249,#113627,#113628);
#98257=AXIS2_PLACEMENT_3D('',#153250,#113629,#113630);
#98258=AXIS2_PLACEMENT_3D('',#153251,#113631,#113632);
#98259=AXIS2_PLACEMENT_3D('',#153254,#113635,#113636);
#98260=AXIS2_PLACEMENT_3D('',#153256,#113638,#113639);
#98261=AXIS2_PLACEMENT_3D('',#153258,#113641,#113642);
#98262=AXIS2_PLACEMENT_3D('',#153259,#113643,#113644);
#98263=AXIS2_PLACEMENT_3D('',#153261,#113646,#113647);
#98264=AXIS2_PLACEMENT_3D('',#153263,#113649,#113650);
#98265=AXIS2_PLACEMENT_3D('',#153264,#113651,#113652);
#98266=AXIS2_PLACEMENT_3D('',#153266,#113654,#113655);
#98267=AXIS2_PLACEMENT_3D('',#153268,#113657,#113658);
#98268=AXIS2_PLACEMENT_3D('',#153269,#113659,#113660);
#98269=AXIS2_PLACEMENT_3D('',#153271,#113662,#113663);
#98270=AXIS2_PLACEMENT_3D('',#153273,#113665,#113666);
#98271=AXIS2_PLACEMENT_3D('',#153274,#113667,#113668);
#98272=AXIS2_PLACEMENT_3D('',#153276,#113670,#113671);
#98273=AXIS2_PLACEMENT_3D('',#153278,#113673,#113674);
#98274=AXIS2_PLACEMENT_3D('',#153279,#113675,#113676);
#98275=AXIS2_PLACEMENT_3D('',#153281,#113678,#113679);
#98276=AXIS2_PLACEMENT_3D('',#153283,#113681,#113682);
#98277=AXIS2_PLACEMENT_3D('',#153284,#113683,#113684);
#98278=AXIS2_PLACEMENT_3D('',#153286,#113686,#113687);
#98279=AXIS2_PLACEMENT_3D('',#153288,#113689,#113690);
#98280=AXIS2_PLACEMENT_3D('',#153289,#113691,#113692);
#98281=AXIS2_PLACEMENT_3D('',#153291,#113694,#113695);
#98282=AXIS2_PLACEMENT_3D('',#153293,#113697,#113698);
#98283=AXIS2_PLACEMENT_3D('',#153294,#113699,#113700);
#98284=AXIS2_PLACEMENT_3D('',#153296,#113702,#113703);
#98285=AXIS2_PLACEMENT_3D('',#153298,#113705,#113706);
#98286=AXIS2_PLACEMENT_3D('',#153299,#113707,#113708);
#98287=AXIS2_PLACEMENT_3D('',#153301,#113710,#113711);
#98288=AXIS2_PLACEMENT_3D('',#153303,#113713,#113714);
#98289=AXIS2_PLACEMENT_3D('',#153304,#113715,#113716);
#98290=AXIS2_PLACEMENT_3D('',#153306,#113718,#113719);
#98291=AXIS2_PLACEMENT_3D('',#153308,#113721,#113722);
#98292=AXIS2_PLACEMENT_3D('',#153309,#113723,#113724);
#98293=AXIS2_PLACEMENT_3D('',#153311,#113726,#113727);
#98294=AXIS2_PLACEMENT_3D('',#153313,#113729,#113730);
#98295=AXIS2_PLACEMENT_3D('',#153314,#113731,#113732);
#98296=AXIS2_PLACEMENT_3D('',#153316,#113734,#113735);
#98297=AXIS2_PLACEMENT_3D('',#153318,#113737,#113738);
#98298=AXIS2_PLACEMENT_3D('',#153319,#113739,#113740);
#98299=AXIS2_PLACEMENT_3D('',#153321,#113742,#113743);
#98300=AXIS2_PLACEMENT_3D('',#153323,#113745,#113746);
#98301=AXIS2_PLACEMENT_3D('',#153324,#113747,#113748);
#98302=AXIS2_PLACEMENT_3D('',#153326,#113750,#113751);
#98303=AXIS2_PLACEMENT_3D('',#153328,#113753,#113754);
#98304=AXIS2_PLACEMENT_3D('',#153329,#113755,#113756);
#98305=AXIS2_PLACEMENT_3D('',#153331,#113758,#113759);
#98306=AXIS2_PLACEMENT_3D('',#153333,#113761,#113762);
#98307=AXIS2_PLACEMENT_3D('',#153334,#113763,#113764);
#98308=AXIS2_PLACEMENT_3D('',#153336,#113766,#113767);
#98309=AXIS2_PLACEMENT_3D('',#153338,#113769,#113770);
#98310=AXIS2_PLACEMENT_3D('',#153339,#113771,#113772);
#98311=AXIS2_PLACEMENT_3D('',#153341,#113774,#113775);
#98312=AXIS2_PLACEMENT_3D('',#153343,#113777,#113778);
#98313=AXIS2_PLACEMENT_3D('',#153344,#113779,#113780);
#98314=AXIS2_PLACEMENT_3D('',#153346,#113782,#113783);
#98315=AXIS2_PLACEMENT_3D('',#153348,#113785,#113786);
#98316=AXIS2_PLACEMENT_3D('',#153349,#113787,#113788);
#98317=AXIS2_PLACEMENT_3D('',#153351,#113790,#113791);
#98318=AXIS2_PLACEMENT_3D('',#153353,#113793,#113794);
#98319=AXIS2_PLACEMENT_3D('',#153354,#113795,#113796);
#98320=AXIS2_PLACEMENT_3D('',#153356,#113798,#113799);
#98321=AXIS2_PLACEMENT_3D('',#153358,#113801,#113802);
#98322=AXIS2_PLACEMENT_3D('',#153359,#113803,#113804);
#98323=AXIS2_PLACEMENT_3D('',#153361,#113806,#113807);
#98324=AXIS2_PLACEMENT_3D('',#153363,#113809,#113810);
#98325=AXIS2_PLACEMENT_3D('',#153364,#113811,#113812);
#98326=AXIS2_PLACEMENT_3D('',#153366,#113814,#113815);
#98327=AXIS2_PLACEMENT_3D('',#153368,#113817,#113818);
#98328=AXIS2_PLACEMENT_3D('',#153369,#113819,#113820);
#98329=AXIS2_PLACEMENT_3D('',#153371,#113822,#113823);
#98330=AXIS2_PLACEMENT_3D('',#153373,#113825,#113826);
#98331=AXIS2_PLACEMENT_3D('',#153374,#113827,#113828);
#98332=AXIS2_PLACEMENT_3D('',#153376,#113830,#113831);
#98333=AXIS2_PLACEMENT_3D('',#153378,#113833,#113834);
#98334=AXIS2_PLACEMENT_3D('',#153379,#113835,#113836);
#98335=AXIS2_PLACEMENT_3D('',#153381,#113838,#113839);
#98336=AXIS2_PLACEMENT_3D('',#153382,#113840,#113841);
#98337=AXIS2_PLACEMENT_3D('',#153384,#113843,#113844);
#98338=AXIS2_PLACEMENT_3D('',#153385,#113845,#113846);
#98339=AXIS2_PLACEMENT_3D('',#153387,#113848,#113849);
#98340=AXIS2_PLACEMENT_3D('',#153389,#113851,#113852);
#98341=AXIS2_PLACEMENT_3D('',#153390,#113853,#113854);
#98342=AXIS2_PLACEMENT_3D('',#153392,#113856,#113857);
#98343=AXIS2_PLACEMENT_3D('',#153394,#113859,#113860);
#98344=AXIS2_PLACEMENT_3D('',#153395,#113861,#113862);
#98345=AXIS2_PLACEMENT_3D('',#153397,#113864,#113865);
#98346=AXIS2_PLACEMENT_3D('',#153399,#113867,#113868);
#98347=AXIS2_PLACEMENT_3D('',#153400,#113869,#113870);
#98348=AXIS2_PLACEMENT_3D('',#153402,#113872,#113873);
#98349=AXIS2_PLACEMENT_3D('',#153404,#113875,#113876);
#98350=AXIS2_PLACEMENT_3D('',#153405,#113877,#113878);
#98351=AXIS2_PLACEMENT_3D('',#153407,#113880,#113881);
#98352=AXIS2_PLACEMENT_3D('',#153408,#113882,#113883);
#98353=AXIS2_PLACEMENT_3D('',#153410,#113885,#113886);
#98354=AXIS2_PLACEMENT_3D('',#153411,#113887,#113888);
#98355=AXIS2_PLACEMENT_3D('',#153413,#113890,#113891);
#98356=AXIS2_PLACEMENT_3D('',#153415,#113893,#113894);
#98357=AXIS2_PLACEMENT_3D('',#153416,#113895,#113896);
#98358=AXIS2_PLACEMENT_3D('',#153418,#113898,#113899);
#98359=AXIS2_PLACEMENT_3D('',#153420,#113901,#113902);
#98360=AXIS2_PLACEMENT_3D('',#153421,#113903,#113904);
#98361=AXIS2_PLACEMENT_3D('',#153423,#113906,#113907);
#98362=AXIS2_PLACEMENT_3D('',#153425,#113909,#113910);
#98363=AXIS2_PLACEMENT_3D('',#153426,#113911,#113912);
#98364=AXIS2_PLACEMENT_3D('',#153428,#113914,#113915);
#98365=AXIS2_PLACEMENT_3D('',#153430,#113917,#113918);
#98366=AXIS2_PLACEMENT_3D('',#153431,#113919,#113920);
#98367=AXIS2_PLACEMENT_3D('',#153432,#113921,#113922);
#98368=AXIS2_PLACEMENT_3D('',#153433,#113923,#113924);
#98369=AXIS2_PLACEMENT_3D('',#153434,#113925,#113926);
#98370=AXIS2_PLACEMENT_3D('',#153435,#113927,#113928);
#98371=AXIS2_PLACEMENT_3D('',#153441,#113932,#113933);
#98372=AXIS2_PLACEMENT_3D('',#153445,#113935,#113936);
#98373=AXIS2_PLACEMENT_3D('',#153446,#113937,#113938);
#98374=AXIS2_PLACEMENT_3D('',#153447,#113939,#113940);
#98375=AXIS2_PLACEMENT_3D('',#153451,#113942,#113943);
#98376=AXIS2_PLACEMENT_3D('',#153452,#113944,#113945);
#98377=AXIS2_PLACEMENT_3D('',#153453,#113946,#113947);
#98378=AXIS2_PLACEMENT_3D('',#153457,#113949,#113950);
#98379=AXIS2_PLACEMENT_3D('',#153458,#113951,#113952);
#98380=AXIS2_PLACEMENT_3D('',#153459,#113953,#113954);
#98381=AXIS2_PLACEMENT_3D('',#153464,#113958,#113959);
#98382=AXIS2_PLACEMENT_3D('',#153467,#113961,#113962);
#98383=AXIS2_PLACEMENT_3D('',#153468,#113963,#113964);
#98384=AXIS2_PLACEMENT_3D('',#153469,#113965,#113966);
#98385=AXIS2_PLACEMENT_3D('',#153470,#113967,#113968);
#98386=AXIS2_PLACEMENT_3D('',#153471,#113969,#113970);
#98387=AXIS2_PLACEMENT_3D('',#153472,#113971,#113972);
#98388=AXIS2_PLACEMENT_3D('',#153477,#113974,#113975);
#98389=AXIS2_PLACEMENT_3D('',#153480,#113977,#113978);
#98390=AXIS2_PLACEMENT_3D('',#153481,#113979,#113980);
#98391=AXIS2_PLACEMENT_3D('',#153484,#113983,#113984);
#98392=AXIS2_PLACEMENT_3D('',#153487,#113986,#113987);
#98393=AXIS2_PLACEMENT_3D('',#153488,#113988,#113989);
#98394=AXIS2_PLACEMENT_3D('',#153489,#113990,#113991);
#98395=AXIS2_PLACEMENT_3D('',#153492,#113993,#113994);
#98396=AXIS2_PLACEMENT_3D('',#153493,#113995,#113996);
#98397=AXIS2_PLACEMENT_3D('',#153499,#114000,#114001);
#98398=AXIS2_PLACEMENT_3D('',#153503,#114003,#114004);
#98399=AXIS2_PLACEMENT_3D('',#153504,#114005,#114006);
#98400=AXIS2_PLACEMENT_3D('',#153505,#114007,#114008);
#98401=AXIS2_PLACEMENT_3D('',#153506,#114009,#114010);
#98402=AXIS2_PLACEMENT_3D('',#153507,#114011,#114012);
#98403=AXIS2_PLACEMENT_3D('',#153508,#114013,#114014);
#98404=AXIS2_PLACEMENT_3D('',#153509,#114015,#114016);
#98405=AXIS2_PLACEMENT_3D('',#153510,#114017,#114018);
#98406=AXIS2_PLACEMENT_3D('',#153511,#114019,#114020);
#98407=AXIS2_PLACEMENT_3D('',#153512,#114021,#114022);
#98408=AXIS2_PLACEMENT_3D('',#153513,#114023,#114024);
#98409=AXIS2_PLACEMENT_3D('',#153514,#114025,#114026);
#98410=AXIS2_PLACEMENT_3D('',#153515,#114027,#114028);
#98411=AXIS2_PLACEMENT_3D('',#153516,#114029,#114030);
#98412=AXIS2_PLACEMENT_3D('',#153517,#114031,#114032);
#98413=AXIS2_PLACEMENT_3D('',#153518,#114033,#114034);
#98414=AXIS2_PLACEMENT_3D('',#153519,#114035,#114036);
#98415=AXIS2_PLACEMENT_3D('',#153520,#114037,#114038);
#98416=AXIS2_PLACEMENT_3D('',#153521,#114039,#114040);
#98417=AXIS2_PLACEMENT_3D('',#153522,#114041,#114042);
#98418=AXIS2_PLACEMENT_3D('',#153523,#114043,#114044);
#98419=AXIS2_PLACEMENT_3D('',#153524,#114045,#114046);
#98420=AXIS2_PLACEMENT_3D('',#153525,#114047,#114048);
#98421=AXIS2_PLACEMENT_3D('',#153526,#114049,#114050);
#98422=AXIS2_PLACEMENT_3D('',#153527,#114051,#114052);
#98423=AXIS2_PLACEMENT_3D('',#153528,#114053,#114054);
#98424=AXIS2_PLACEMENT_3D('',#153529,#114055,#114056);
#98425=AXIS2_PLACEMENT_3D('',#153530,#114057,#114058);
#98426=AXIS2_PLACEMENT_3D('',#153531,#114059,#114060);
#98427=AXIS2_PLACEMENT_3D('',#153532,#114061,#114062);
#98428=AXIS2_PLACEMENT_3D('',#153533,#114063,#114064);
#98429=AXIS2_PLACEMENT_3D('',#153534,#114065,#114066);
#98430=AXIS2_PLACEMENT_3D('',#153535,#114067,#114068);
#98431=AXIS2_PLACEMENT_3D('',#153536,#114069,#114070);
#98432=AXIS2_PLACEMENT_3D('',#153537,#114071,#114072);
#98433=AXIS2_PLACEMENT_3D('',#153538,#114073,#114074);
#98434=AXIS2_PLACEMENT_3D('',#153541,#114075,#114076);
#98435=AXIS2_PLACEMENT_3D('',#153545,#114078,#114079);
#98436=AXIS2_PLACEMENT_3D('',#157327,#114083,#114084);
#98437=AXIS2_PLACEMENT_3D('',#157331,#114086,#114087);
#98438=AXIS2_PLACEMENT_3D('',#157332,#114088,#114089);
#98439=AXIS2_PLACEMENT_3D('',#157333,#114090,#114091);
#98440=AXIS2_PLACEMENT_3D('',#157336,#114092,#114093);
#98441=AXIS2_PLACEMENT_3D('',#157340,#114095,#114096);
#98442=AXIS2_PLACEMENT_3D('',#160815,#114099,#114100);
#98443=AXIS2_PLACEMENT_3D('',#160819,#114102,#114103);
#98444=AXIS2_PLACEMENT_3D('',#160820,#114104,#114105);
#98445=AXIS2_PLACEMENT_3D('',#160821,#114106,#114107);
#98446=AXIS2_PLACEMENT_3D('',#160824,#114108,#114109);
#98447=AXIS2_PLACEMENT_3D('',#160828,#114111,#114112);
#98448=AXIS2_PLACEMENT_3D('',#164015,#114115,#114116);
#98449=AXIS2_PLACEMENT_3D('',#164019,#114118,#114119);
#98450=AXIS2_PLACEMENT_3D('',#164020,#114120,#114121);
#98451=AXIS2_PLACEMENT_3D('',#164021,#114122,#114123);
#98452=AXIS2_PLACEMENT_3D('',#164024,#114124,#114125);
#98453=AXIS2_PLACEMENT_3D('',#164028,#114127,#114128);
#98454=AXIS2_PLACEMENT_3D('',#167215,#114131,#114132);
#98455=AXIS2_PLACEMENT_3D('',#167219,#114134,#114135);
#98456=AXIS2_PLACEMENT_3D('',#167220,#114136,#114137);
#98457=AXIS2_PLACEMENT_3D('',#167221,#114138,#114139);
#98458=AXIS2_PLACEMENT_3D('',#167224,#114140,#114141);
#98459=AXIS2_PLACEMENT_3D('',#167228,#114143,#114144);
#98460=AXIS2_PLACEMENT_3D('',#171009,#114147,#114148);
#98461=AXIS2_PLACEMENT_3D('',#171013,#114150,#114151);
#98462=AXIS2_PLACEMENT_3D('',#171014,#114152,#114153);
#98463=AXIS2_PLACEMENT_3D('',#171015,#114154,#114155);
#98464=AXIS2_PLACEMENT_3D('',#171018,#114156,#114157);
#98465=AXIS2_PLACEMENT_3D('',#171022,#114159,#114160);
#98466=AXIS2_PLACEMENT_3D('',#174497,#114163,#114164);
#98467=AXIS2_PLACEMENT_3D('',#174501,#114166,#114167);
#98468=AXIS2_PLACEMENT_3D('',#174502,#114168,#114169);
#98469=AXIS2_PLACEMENT_3D('',#174503,#114170,#114171);
#98470=AXIS2_PLACEMENT_3D('',#174506,#114172,#114173);
#98471=AXIS2_PLACEMENT_3D('',#174510,#114175,#114176);
#98472=AXIS2_PLACEMENT_3D('',#177706,#114179,#114180);
#98473=AXIS2_PLACEMENT_3D('',#177710,#114182,#114183);
#98474=AXIS2_PLACEMENT_3D('',#177711,#114184,#114185);
#98475=AXIS2_PLACEMENT_3D('',#177712,#114186,#114187);
#98476=AXIS2_PLACEMENT_3D('',#177715,#114188,#114189);
#98477=AXIS2_PLACEMENT_3D('',#177719,#114191,#114192);
#98478=AXIS2_PLACEMENT_3D('',#181197,#114195,#114196);
#98479=AXIS2_PLACEMENT_3D('',#181201,#114198,#114199);
#98480=AXIS2_PLACEMENT_3D('',#181202,#114200,#114201);
#98481=AXIS2_PLACEMENT_3D('',#181203,#114202,#114203);
#98482=AXIS2_PLACEMENT_3D('',#181206,#114204,#114205);
#98483=AXIS2_PLACEMENT_3D('',#181210,#114207,#114208);
#98484=AXIS2_PLACEMENT_3D('',#184679,#114211,#114212);
#98485=AXIS2_PLACEMENT_3D('',#184683,#114214,#114215);
#98486=AXIS2_PLACEMENT_3D('',#184684,#114216,#114217);
#98487=AXIS2_PLACEMENT_3D('',#184685,#114218,#114219);
#98488=AXIS2_PLACEMENT_3D('',#184688,#114220,#114221);
#98489=AXIS2_PLACEMENT_3D('',#184692,#114223,#114224);
#98490=AXIS2_PLACEMENT_3D('',#187867,#114227,#114228);
#98491=AXIS2_PLACEMENT_3D('',#187871,#114230,#114231);
#98492=AXIS2_PLACEMENT_3D('',#187872,#114232,#114233);
#98493=AXIS2_PLACEMENT_3D('',#187873,#114234,#114235);
#98494=AXIS2_PLACEMENT_3D('',#187876,#114236,#114237);
#98495=AXIS2_PLACEMENT_3D('',#187880,#114239,#114240);
#98496=AXIS2_PLACEMENT_3D('',#191001,#114243,#114244);
#98497=AXIS2_PLACEMENT_3D('',#191005,#114246,#114247);
#98498=AXIS2_PLACEMENT_3D('',#191006,#114248,#114249);
#98499=AXIS2_PLACEMENT_3D('',#191007,#114250,#114251);
#98500=AXIS2_PLACEMENT_3D('',#191010,#114252,#114253);
#98501=AXIS2_PLACEMENT_3D('',#191014,#114255,#114256);
#98502=AXIS2_PLACEMENT_3D('',#194469,#114259,#114260);
#98503=AXIS2_PLACEMENT_3D('',#194473,#114262,#114263);
#98504=AXIS2_PLACEMENT_3D('',#194474,#114264,#114265);
#98505=AXIS2_PLACEMENT_3D('',#194475,#114266,#114267);
#98506=AXIS2_PLACEMENT_3D('',#194478,#114268,#114269);
#98507=AXIS2_PLACEMENT_3D('',#194482,#114271,#114272);
#98508=AXIS2_PLACEMENT_3D('',#197945,#114275,#114276);
#98509=AXIS2_PLACEMENT_3D('',#197949,#114278,#114279);
#98510=AXIS2_PLACEMENT_3D('',#197950,#114280,#114281);
#98511=AXIS2_PLACEMENT_3D('',#197951,#114282,#114283);
#98512=AXIS2_PLACEMENT_3D('',#197954,#114284,#114285);
#98513=AXIS2_PLACEMENT_3D('',#197958,#114287,#114288);
#98514=AXIS2_PLACEMENT_3D('',#201103,#114291,#114292);
#98515=AXIS2_PLACEMENT_3D('',#201107,#114294,#114295);
#98516=AXIS2_PLACEMENT_3D('',#201108,#114296,#114297);
#98517=AXIS2_PLACEMENT_3D('',#201109,#114298,#114299);
#98518=AXIS2_PLACEMENT_3D('',#201112,#114300,#114301);
#98519=AXIS2_PLACEMENT_3D('',#201116,#114303,#114304);
#98520=AXIS2_PLACEMENT_3D('',#204279,#114307,#114308);
#98521=AXIS2_PLACEMENT_3D('',#204283,#114310,#114311);
#98522=AXIS2_PLACEMENT_3D('',#204284,#114312,#114313);
#98523=AXIS2_PLACEMENT_3D('',#204285,#114314,#114315);
#98524=AXIS2_PLACEMENT_3D('',#204288,#114316,#114317);
#98525=AXIS2_PLACEMENT_3D('',#204292,#114319,#114320);
#98526=AXIS2_PLACEMENT_3D('',#207431,#114323,#114324);
#98527=AXIS2_PLACEMENT_3D('',#207435,#114326,#114327);
#98528=AXIS2_PLACEMENT_3D('',#207436,#114328,#114329);
#98529=AXIS2_PLACEMENT_3D('',#207437,#114330,#114331);
#98530=AXIS2_PLACEMENT_3D('',#207440,#114332,#114333);
#98531=AXIS2_PLACEMENT_3D('',#207444,#114335,#114336);
#98532=AXIS2_PLACEMENT_3D('',#210610,#114339,#114340);
#98533=AXIS2_PLACEMENT_3D('',#210614,#114342,#114343);
#98534=AXIS2_PLACEMENT_3D('',#210615,#114344,#114345);
#98535=AXIS2_PLACEMENT_3D('',#210616,#114346,#114347);
#98536=AXIS2_PLACEMENT_3D('',#210619,#114348,#114349);
#98537=AXIS2_PLACEMENT_3D('',#210623,#114351,#114352);
#98538=AXIS2_PLACEMENT_3D('',#213774,#114355,#114356);
#98539=AXIS2_PLACEMENT_3D('',#213778,#114358,#114359);
#98540=AXIS2_PLACEMENT_3D('',#213779,#114360,#114361);
#98541=AXIS2_PLACEMENT_3D('',#213780,#114362,#114363);
#98542=AXIS2_PLACEMENT_3D('',#213783,#114364,#114365);
#98543=AXIS2_PLACEMENT_3D('',#213787,#114367,#114368);
#98544=AXIS2_PLACEMENT_3D('',#216941,#114371,#114372);
#98545=AXIS2_PLACEMENT_3D('',#216945,#114374,#114375);
#98546=AXIS2_PLACEMENT_3D('',#216946,#114376,#114377);
#98547=AXIS2_PLACEMENT_3D('',#216947,#114378,#114379);
#98548=AXIS2_PLACEMENT_3D('',#216950,#114380,#114381);
#98549=AXIS2_PLACEMENT_3D('',#216954,#114383,#114384);
#98550=AXIS2_PLACEMENT_3D('',#220406,#114387,#114388);
#98551=AXIS2_PLACEMENT_3D('',#220410,#114390,#114391);
#98552=AXIS2_PLACEMENT_3D('',#220411,#114392,#114393);
#98553=AXIS2_PLACEMENT_3D('',#220412,#114394,#114395);
#98554=AXIS2_PLACEMENT_3D('',#220415,#114396,#114397);
#98555=AXIS2_PLACEMENT_3D('',#220419,#114399,#114400);
#98556=AXIS2_PLACEMENT_3D('',#223549,#114403,#114404);
#98557=AXIS2_PLACEMENT_3D('',#223553,#114406,#114407);
#98558=AXIS2_PLACEMENT_3D('',#223554,#114408,#114409);
#98559=AXIS2_PLACEMENT_3D('',#223555,#114410,#114411);
#98560=AXIS2_PLACEMENT_3D('',#223558,#114412,#114413);
#98561=AXIS2_PLACEMENT_3D('',#223562,#114415,#114416);
#98562=AXIS2_PLACEMENT_3D('',#226993,#114419,#114420);
#98563=AXIS2_PLACEMENT_3D('',#226997,#114422,#114423);
#98564=AXIS2_PLACEMENT_3D('',#226998,#114424,#114425);
#98565=AXIS2_PLACEMENT_3D('',#226999,#114426,#114427);
#98566=AXIS2_PLACEMENT_3D('',#227002,#114428,#114429);
#98567=AXIS2_PLACEMENT_3D('',#227006,#114431,#114432);
#98568=AXIS2_PLACEMENT_3D('',#230133,#114435,#114436);
#98569=AXIS2_PLACEMENT_3D('',#230137,#114438,#114439);
#98570=AXIS2_PLACEMENT_3D('',#230138,#114440,#114441);
#98571=AXIS2_PLACEMENT_3D('',#230139,#114442,#114443);
#98572=AXIS2_PLACEMENT_3D('',#230142,#114444,#114445);
#98573=AXIS2_PLACEMENT_3D('',#230146,#114447,#114448);
#98574=AXIS2_PLACEMENT_3D('',#233273,#114451,#114452);
#98575=AXIS2_PLACEMENT_3D('',#233277,#114454,#114455);
#98576=AXIS2_PLACEMENT_3D('',#233278,#114456,#114457);
#98577=AXIS2_PLACEMENT_3D('',#233279,#114458,#114459);
#98578=AXIS2_PLACEMENT_3D('',#233282,#114460,#114461);
#98579=AXIS2_PLACEMENT_3D('',#233286,#114463,#114464);
#98580=AXIS2_PLACEMENT_3D('',#236431,#114467,#114468);
#98581=AXIS2_PLACEMENT_3D('',#236435,#114470,#114471);
#98582=AXIS2_PLACEMENT_3D('',#236436,#114472,#114473);
#98583=AXIS2_PLACEMENT_3D('',#236437,#114474,#114475);
#98584=AXIS2_PLACEMENT_3D('',#236440,#114476,#114477);
#98585=AXIS2_PLACEMENT_3D('',#236444,#114479,#114480);
#98586=AXIS2_PLACEMENT_3D('',#239601,#114483,#114484);
#98587=AXIS2_PLACEMENT_3D('',#239605,#114486,#114487);
#98588=AXIS2_PLACEMENT_3D('',#239606,#114488,#114489);
#98589=AXIS2_PLACEMENT_3D('',#239607,#114490,#114491);
#98590=AXIS2_PLACEMENT_3D('',#239610,#114492,#114493);
#98591=AXIS2_PLACEMENT_3D('',#239614,#114495,#114496);
#98592=AXIS2_PLACEMENT_3D('',#242768,#114499,#114500);
#98593=AXIS2_PLACEMENT_3D('',#242772,#114502,#114503);
#98594=AXIS2_PLACEMENT_3D('',#242773,#114504,#114505);
#98595=AXIS2_PLACEMENT_3D('',#242774,#114506,#114507);
#98596=AXIS2_PLACEMENT_3D('',#242777,#114508,#114509);
#98597=AXIS2_PLACEMENT_3D('',#242781,#114511,#114512);
#98598=AXIS2_PLACEMENT_3D('',#246250,#114515,#114516);
#98599=AXIS2_PLACEMENT_3D('',#246254,#114518,#114519);
#98600=AXIS2_PLACEMENT_3D('',#246255,#114520,#114521);
#98601=AXIS2_PLACEMENT_3D('',#246256,#114522,#114523);
#98602=AXIS2_PLACEMENT_3D('',#246259,#114524,#114525);
#98603=AXIS2_PLACEMENT_3D('',#246263,#114527,#114528);
#98604=AXIS2_PLACEMENT_3D('',#249423,#114531,#114532);
#98605=AXIS2_PLACEMENT_3D('',#249427,#114534,#114535);
#98606=AXIS2_PLACEMENT_3D('',#249428,#114536,#114537);
#98607=AXIS2_PLACEMENT_3D('',#249429,#114538,#114539);
#98608=AXIS2_PLACEMENT_3D('',#249432,#114540,#114541);
#98609=AXIS2_PLACEMENT_3D('',#249436,#114543,#114544);
#98610=AXIS2_PLACEMENT_3D('',#252596,#114547,#114548);
#98611=AXIS2_PLACEMENT_3D('',#252600,#114550,#114551);
#98612=AXIS2_PLACEMENT_3D('',#252601,#114552,#114553);
#98613=AXIS2_PLACEMENT_3D('',#252602,#114554,#114555);
#98614=AXIS2_PLACEMENT_3D('',#252605,#114556,#114557);
#98615=AXIS2_PLACEMENT_3D('',#252609,#114559,#114560);
#98616=AXIS2_PLACEMENT_3D('',#255748,#114563,#114564);
#98617=AXIS2_PLACEMENT_3D('',#255752,#114566,#114567);
#98618=AXIS2_PLACEMENT_3D('',#255753,#114568,#114569);
#98619=AXIS2_PLACEMENT_3D('',#255754,#114570,#114571);
#98620=AXIS2_PLACEMENT_3D('',#255757,#114572,#114573);
#98621=AXIS2_PLACEMENT_3D('',#255761,#114575,#114576);
#98622=AXIS2_PLACEMENT_3D('',#258897,#114579,#114580);
#98623=AXIS2_PLACEMENT_3D('',#258901,#114582,#114583);
#98624=AXIS2_PLACEMENT_3D('',#258902,#114584,#114585);
#98625=AXIS2_PLACEMENT_3D('',#258903,#114586,#114587);
#98626=AXIS2_PLACEMENT_3D('',#258906,#114588,#114589);
#98627=AXIS2_PLACEMENT_3D('',#258910,#114591,#114592);
#98628=AXIS2_PLACEMENT_3D('',#262689,#114595,#114596);
#98629=AXIS2_PLACEMENT_3D('',#262693,#114598,#114599);
#98630=AXIS2_PLACEMENT_3D('',#262694,#114600,#114601);
#98631=AXIS2_PLACEMENT_3D('',#262695,#114602,#114603);
#98632=AXIS2_PLACEMENT_3D('',#262698,#114604,#114605);
#98633=AXIS2_PLACEMENT_3D('',#262702,#114607,#114608);
#98634=AXIS2_PLACEMENT_3D('',#266143,#114611,#114612);
#98635=AXIS2_PLACEMENT_3D('',#266147,#114614,#114615);
#98636=AXIS2_PLACEMENT_3D('',#266148,#114616,#114617);
#98637=AXIS2_PLACEMENT_3D('',#266149,#114618,#114619);
#98638=AXIS2_PLACEMENT_3D('',#266152,#114620,#114621);
#98639=AXIS2_PLACEMENT_3D('',#266156,#114623,#114624);
#98640=AXIS2_PLACEMENT_3D('',#269632,#114627,#114628);
#98641=AXIS2_PLACEMENT_3D('',#269636,#114630,#114631);
#98642=AXIS2_PLACEMENT_3D('',#269637,#114632,#114633);
#98643=AXIS2_PLACEMENT_3D('',#269638,#114634,#114635);
#98644=AXIS2_PLACEMENT_3D('',#269641,#114636,#114637);
#98645=AXIS2_PLACEMENT_3D('',#269645,#114639,#114640);
#98646=AXIS2_PLACEMENT_3D('',#272829,#114643,#114644);
#98647=AXIS2_PLACEMENT_3D('',#272833,#114646,#114647);
#98648=AXIS2_PLACEMENT_3D('',#272834,#114648,#114649);
#98649=AXIS2_PLACEMENT_3D('',#272835,#114650,#114651);
#98650=AXIS2_PLACEMENT_3D('',#272838,#114652,#114653);
#98651=AXIS2_PLACEMENT_3D('',#272842,#114655,#114656);
#98652=AXIS2_PLACEMENT_3D('',#276032,#114659,#114660);
#98653=AXIS2_PLACEMENT_3D('',#276036,#114662,#114663);
#98654=AXIS2_PLACEMENT_3D('',#276037,#114664,#114665);
#98655=AXIS2_PLACEMENT_3D('',#276038,#114666,#114667);
#98656=AXIS2_PLACEMENT_3D('',#276041,#114668,#114669);
#98657=AXIS2_PLACEMENT_3D('',#276045,#114671,#114672);
#98658=AXIS2_PLACEMENT_3D('',#279527,#114675,#114676);
#98659=AXIS2_PLACEMENT_3D('',#279531,#114678,#114679);
#98660=AXIS2_PLACEMENT_3D('',#279532,#114680,#114681);
#98661=AXIS2_PLACEMENT_3D('',#279533,#114682,#114683);
#98662=AXIS2_PLACEMENT_3D('',#279536,#114684,#114685);
#98663=AXIS2_PLACEMENT_3D('',#279540,#114687,#114688);
#98664=AXIS2_PLACEMENT_3D('',#282736,#114691,#114692);
#98665=AXIS2_PLACEMENT_3D('',#282740,#114694,#114695);
#98666=AXIS2_PLACEMENT_3D('',#282741,#114696,#114697);
#98667=AXIS2_PLACEMENT_3D('',#282742,#114698,#114699);
#98668=AXIS2_PLACEMENT_3D('',#282745,#114700,#114701);
#98669=AXIS2_PLACEMENT_3D('',#282749,#114703,#114704);
#98670=AXIS2_PLACEMENT_3D('',#286530,#114707,#114708);
#98671=AXIS2_PLACEMENT_3D('',#286534,#114710,#114711);
#98672=AXIS2_PLACEMENT_3D('',#286535,#114712,#114713);
#98673=AXIS2_PLACEMENT_3D('',#286536,#114714,#114715);
#98674=AXIS2_PLACEMENT_3D('',#286539,#114716,#114717);
#98675=AXIS2_PLACEMENT_3D('',#286543,#114719,#114720);
#98676=AXIS2_PLACEMENT_3D('',#290025,#114723,#114724);
#98677=AXIS2_PLACEMENT_3D('',#290029,#114726,#114727);
#98678=AXIS2_PLACEMENT_3D('',#290030,#114728,#114729);
#98679=AXIS2_PLACEMENT_3D('',#290031,#114730,#114731);
#98680=AXIS2_PLACEMENT_3D('',#290034,#114732,#114733);
#98681=AXIS2_PLACEMENT_3D('',#290038,#114735,#114736);
#98682=AXIS2_PLACEMENT_3D('',#293213,#114739,#114740);
#98683=AXIS2_PLACEMENT_3D('',#293217,#114742,#114743);
#98684=AXIS2_PLACEMENT_3D('',#293218,#114744,#114745);
#98685=AXIS2_PLACEMENT_3D('',#293219,#114746,#114747);
#98686=AXIS2_PLACEMENT_3D('',#293222,#114748,#114749);
#98687=AXIS2_PLACEMENT_3D('',#293226,#114751,#114752);
#98688=AXIS2_PLACEMENT_3D('',#296698,#114755,#114756);
#98689=AXIS2_PLACEMENT_3D('',#296700,#114757,#114758);
#98690=AXIS2_PLACEMENT_3D('',#296702,#114759,#114760);
#98691=AXIS2_PLACEMENT_3D('',#297176,#114761,#114762);
#98692=AXIS2_PLACEMENT_3D('',#297500,#114763,#114764);
#98693=AXIS2_PLACEMENT_3D('',#297501,#114765,#114766);
#98694=AXIS2_PLACEMENT_3D('',#297504,#114768,#114769);
#98695=AXIS2_PLACEMENT_3D('',#297505,#114770,#114771);
#98696=AXIS2_PLACEMENT_3D('',#297508,#114773,#114774);
#98697=AXIS2_PLACEMENT_3D('',#297509,#114775,#114776);
#98698=AXIS2_PLACEMENT_3D('',#297513,#114778,#114779);
#98699=AXIS2_PLACEMENT_3D('',#300196,#114781,#114782);
#98700=AXIS2_PLACEMENT_3D('',#300199,#114784,#114785);
#98701=AXIS2_PLACEMENT_3D('',#300200,#114786,#114787);
#98702=AXIS2_PLACEMENT_3D('',#300201,#114788,#114789);
#98703=AXIS2_PLACEMENT_3D('',#300203,#114790,#114791);
#98704=AXIS2_PLACEMENT_3D('',#300206,#114793,#114794);
#98705=AXIS2_PLACEMENT_3D('',#300207,#114795,#114796);
#98706=AXIS2_PLACEMENT_3D('',#300209,#114797,#114798);
#98707=AXIS2_PLACEMENT_3D('',#300212,#114800,#114801);
#98708=AXIS2_PLACEMENT_3D('',#300213,#114802,#114803);
#98709=AXIS2_PLACEMENT_3D('',#300214,#114804,#114805);
#98710=AXIS2_PLACEMENT_3D('',#300215,#114806,#114807);
#98711=AXIS2_PLACEMENT_3D('',#300220,#114809,#114810);
#98712=AXIS2_PLACEMENT_3D('',#300239,#114812,#114813);
#98713=AXIS2_PLACEMENT_3D('',#300287,#114815,#114816);
#98714=AXIS2_PLACEMENT_3D('',#300308,#114818,#114819);
#98715=AXIS2_PLACEMENT_3D('',#300359,#114821,#114822);
#98716=AXIS2_PLACEMENT_3D('',#300380,#114824,#114825);
#98717=AXIS2_PLACEMENT_3D('',#300431,#114827,#114828);
#98718=AXIS2_PLACEMENT_3D('',#300452,#114830,#114831);
#98719=AXIS2_PLACEMENT_3D('',#300503,#114833,#114834);
#98720=AXIS2_PLACEMENT_3D('',#300522,#114836,#114837);
#98721=AXIS2_PLACEMENT_3D('',#300570,#114839,#114840);
#98722=AXIS2_PLACEMENT_3D('',#300591,#114842,#114843);
#98723=AXIS2_PLACEMENT_3D('',#300612,#114845,#114846);
#98724=AXIS2_PLACEMENT_3D('',#300633,#114848,#114849);
#98725=AXIS2_PLACEMENT_3D('',#300684,#114851,#114852);
#98726=AXIS2_PLACEMENT_3D('',#300705,#114854,#114855);
#98727=AXIS2_PLACEMENT_3D('',#300720,#114857,#114858);
#98728=AXIS2_PLACEMENT_3D('',#300741,#114860,#114861);
#98729=AXIS2_PLACEMENT_3D('',#300789,#114863,#114864);
#98730=AXIS2_PLACEMENT_3D('',#300810,#114866,#114867);
#98731=AXIS2_PLACEMENT_3D('',#300858,#114869,#114870);
#98732=AXIS2_PLACEMENT_3D('',#300879,#114872,#114873);
#98733=AXIS2_PLACEMENT_3D('',#300900,#114875,#114876);
#98734=AXIS2_PLACEMENT_3D('',#300921,#114878,#114879);
#98735=AXIS2_PLACEMENT_3D('',#300969,#114881,#114882);
#98736=AXIS2_PLACEMENT_3D('',#300990,#114884,#114885);
#98737=AXIS2_PLACEMENT_3D('',#301011,#114887,#114888);
#98738=AXIS2_PLACEMENT_3D('',#301032,#114890,#114891);
#98739=AXIS2_PLACEMENT_3D('',#301080,#114893,#114894);
#98740=AXIS2_PLACEMENT_3D('',#301101,#114896,#114897);
#98741=AXIS2_PLACEMENT_3D('',#301149,#114899,#114900);
#98742=AXIS2_PLACEMENT_3D('',#301168,#114902,#114903);
#98743=AXIS2_PLACEMENT_3D('',#301216,#114905,#114906);
#98744=AXIS2_PLACEMENT_3D('',#301237,#114908,#114909);
#98745=AXIS2_PLACEMENT_3D('',#301282,#114910,#114911);
#98746=AXIS2_PLACEMENT_3D('',#301283,#114912,#114913);
#98747=AXIS2_PLACEMENT_3D('',#301285,#114914,#114915);
#98748=AXIS2_PLACEMENT_3D('',#301288,#114917,#114918);
#98749=AXIS2_PLACEMENT_3D('',#301289,#114919,#114920);
#98750=AXIS2_PLACEMENT_3D('',#301290,#114921,#114922);
#98751=AXIS2_PLACEMENT_3D('',#301294,#114924,#114925);
#98752=AXIS2_PLACEMENT_3D('',#302956,#114928,#114929);
#98753=AXIS2_PLACEMENT_3D('',#302960,#114932,#114933);
#98754=AXIS2_PLACEMENT_3D('',#302963,#114935,#114936);
#98755=AXIS2_PLACEMENT_3D('',#302964,#114937,#114938);
#98756=AXIS2_PLACEMENT_3D('',#304631,#114942,#114943);
#98757=AXIS2_PLACEMENT_3D('',#304634,#114945,#114946);
#98758=AXIS2_PLACEMENT_3D('',#306295,#114948,#114949);
#98759=AXIS2_PLACEMENT_3D('',#306299,#114952,#114953);
#98760=AXIS2_PLACEMENT_3D('',#306302,#114955,#114956);
#98761=AXIS2_PLACEMENT_3D('',#306303,#114957,#114958);
#98762=AXIS2_PLACEMENT_3D('',#307974,#114962,#114963);
#98763=AXIS2_PLACEMENT_3D('',#307977,#114965,#114966);
#98764=AXIS2_PLACEMENT_3D('',#309638,#114968,#114969);
#98765=AXIS2_PLACEMENT_3D('',#309642,#114972,#114973);
#98766=AXIS2_PLACEMENT_3D('',#309645,#114975,#114976);
#98767=AXIS2_PLACEMENT_3D('',#309646,#114977,#114978);
#98768=AXIS2_PLACEMENT_3D('',#311314,#114982,#114983);
#98769=AXIS2_PLACEMENT_3D('',#311317,#114985,#114986);
#98770=AXIS2_PLACEMENT_3D('',#312978,#114988,#114989);
#98771=AXIS2_PLACEMENT_3D('',#312982,#114992,#114993);
#98772=AXIS2_PLACEMENT_3D('',#312985,#114995,#114996);
#98773=AXIS2_PLACEMENT_3D('',#312986,#114997,#114998);
#98774=AXIS2_PLACEMENT_3D('',#314661,#115002,#115003);
#98775=AXIS2_PLACEMENT_3D('',#314664,#115005,#115006);
#98776=AXIS2_PLACEMENT_3D('',#316325,#115008,#115009);
#98777=AXIS2_PLACEMENT_3D('',#316329,#115012,#115013);
#98778=AXIS2_PLACEMENT_3D('',#316332,#115015,#115016);
#98779=AXIS2_PLACEMENT_3D('',#316333,#115017,#115018);
#98780=AXIS2_PLACEMENT_3D('',#318008,#115022,#115023);
#98781=AXIS2_PLACEMENT_3D('',#318011,#115025,#115026);
#98782=AXIS2_PLACEMENT_3D('',#319672,#115028,#115029);
#98783=AXIS2_PLACEMENT_3D('',#319676,#115032,#115033);
#98784=AXIS2_PLACEMENT_3D('',#319679,#115035,#115036);
#98785=AXIS2_PLACEMENT_3D('',#319680,#115037,#115038);
#98786=AXIS2_PLACEMENT_3D('',#321355,#115042,#115043);
#98787=AXIS2_PLACEMENT_3D('',#321358,#115045,#115046);
#98788=AXIS2_PLACEMENT_3D('',#323019,#115048,#115049);
#98789=AXIS2_PLACEMENT_3D('',#323023,#115052,#115053);
#98790=AXIS2_PLACEMENT_3D('',#323026,#115055,#115056);
#98791=AXIS2_PLACEMENT_3D('',#323027,#115057,#115058);
#98792=AXIS2_PLACEMENT_3D('',#324702,#115062,#115063);
#98793=AXIS2_PLACEMENT_3D('',#324705,#115065,#115066);
#98794=AXIS2_PLACEMENT_3D('',#326366,#115068,#115069);
#98795=AXIS2_PLACEMENT_3D('',#326370,#115072,#115073);
#98796=AXIS2_PLACEMENT_3D('',#326373,#115075,#115076);
#98797=AXIS2_PLACEMENT_3D('',#326374,#115077,#115078);
#98798=AXIS2_PLACEMENT_3D('',#328045,#115082,#115083);
#98799=AXIS2_PLACEMENT_3D('',#328048,#115085,#115086);
#98800=AXIS2_PLACEMENT_3D('',#329709,#115088,#115089);
#98801=AXIS2_PLACEMENT_3D('',#329713,#115092,#115093);
#98802=AXIS2_PLACEMENT_3D('',#329715,#115094,#115095);
#98803=AXIS2_PLACEMENT_3D('',#329736,#115097,#115098);
#98804=AXIS2_PLACEMENT_3D('',#329749,#115100,#115101);
#98805=AXIS2_PLACEMENT_3D('',#329770,#115103,#115104);
#98806=AXIS2_PLACEMENT_3D('',#329783,#115106,#115107);
#98807=AXIS2_PLACEMENT_3D('',#329804,#115109,#115110);
#98808=AXIS2_PLACEMENT_3D('',#329817,#115112,#115113);
#98809=AXIS2_PLACEMENT_3D('',#329834,#115115,#115116);
#98810=AXIS2_PLACEMENT_3D('',#329847,#115118,#115119);
#98811=AXIS2_PLACEMENT_3D('',#329868,#115121,#115122);
#98812=AXIS2_PLACEMENT_3D('',#329881,#115124,#115125);
#98813=AXIS2_PLACEMENT_3D('',#329902,#115127,#115128);
#98814=AXIS2_PLACEMENT_3D('',#329915,#115130,#115131);
#98815=AXIS2_PLACEMENT_3D('',#329936,#115133,#115134);
#98816=AXIS2_PLACEMENT_3D('',#329949,#115136,#115137);
#98817=AXIS2_PLACEMENT_3D('',#329968,#115139,#115140);
#98818=AXIS2_PLACEMENT_3D('',#329981,#115142,#115143);
#98819=AXIS2_PLACEMENT_3D('',#329994,#115145,#115146);
#98820=AXIS2_PLACEMENT_3D('',#331650,#115149,#115150);
#98821=AXIS2_PLACEMENT_3D('',#331652,#115152,#115153);
#98822=AXIS2_PLACEMENT_3D('',#333305,#115156,#115157);
#98823=AXIS2_PLACEMENT_3D('',#334961,#115160,#115161);
#98824=AXIS2_PLACEMENT_3D('',#334963,#115163,#115164);
#98825=AXIS2_PLACEMENT_3D('',#334965,#115166,#115167);
#98826=AXIS2_PLACEMENT_3D('',#334968,#115170,#115171);
#98827=AXIS2_PLACEMENT_3D('',#336621,#115174,#115175);
#98828=AXIS2_PLACEMENT_3D('',#338276,#115177,#115178);
#98829=AXIS2_PLACEMENT_3D('',#338279,#115181,#115182);
#98830=AXIS2_PLACEMENT_3D('',#339933,#115186,#115187);
#98831=AXIS2_PLACEMENT_3D('',#341588,#115189,#115190);
#98832=AXIS2_PLACEMENT_3D('',#341590,#115192,#115193);
#98833=AXIS2_PLACEMENT_3D('',#343243,#115196,#115197);
#98834=AXIS2_PLACEMENT_3D('',#344899,#115200,#115201);
#98835=AXIS2_PLACEMENT_3D('',#344901,#115203,#115204);
#98836=AXIS2_PLACEMENT_3D('',#344902,#115205,#115206);
#98837=AXIS2_PLACEMENT_3D('',#344904,#115208,#115209);
#98838=AXIS2_PLACEMENT_3D('',#344907,#115212,#115213);
#98839=AXIS2_PLACEMENT_3D('',#346560,#115216,#115217);
#98840=AXIS2_PLACEMENT_3D('',#348215,#115219,#115220);
#98841=AXIS2_PLACEMENT_3D('',#348218,#115223,#115224);
#98842=AXIS2_PLACEMENT_3D('',#349872,#115228,#115229);
#98843=AXIS2_PLACEMENT_3D('',#351527,#115231,#115232);
#98844=AXIS2_PLACEMENT_3D('',#351529,#115234,#115235);
#98845=AXIS2_PLACEMENT_3D('',#353182,#115238,#115239);
#98846=AXIS2_PLACEMENT_3D('',#354838,#115242,#115243);
#98847=AXIS2_PLACEMENT_3D('',#354840,#115245,#115246);
#98848=AXIS2_PLACEMENT_3D('',#354841,#115247,#115248);
#98849=AXIS2_PLACEMENT_3D('',#354843,#115250,#115251);
#98850=AXIS2_PLACEMENT_3D('',#354846,#115254,#115255);
#98851=AXIS2_PLACEMENT_3D('',#356499,#115258,#115259);
#98852=AXIS2_PLACEMENT_3D('',#358154,#115261,#115262);
#98853=AXIS2_PLACEMENT_3D('',#358155,#115263,#115264);
#98854=AXIS2_PLACEMENT_3D('',#358158,#115266,#115267);
#98855=AXIS2_PLACEMENT_3D('',#358159,#115268,#115269);
#98856=AXIS2_PLACEMENT_3D('',#358160,#115270,#115271);
#98857=AXIS2_PLACEMENT_3D('',#358161,#115272,#115273);
#98858=AXIS2_PLACEMENT_3D('',#358163,#115274,#115275);
#98859=AXIS2_PLACEMENT_3D('',#358165,#115276,#115277);
#98860=AXIS2_PLACEMENT_3D('',#358166,#115278,#115279);
#98861=AXIS2_PLACEMENT_3D('',#358167,#115280,#115281);
#98862=AXIS2_PLACEMENT_3D('',#358169,#115282,#115283);
#98863=AXIS2_PLACEMENT_3D('',#358170,#115284,#115285);
#98864=AXIS2_PLACEMENT_3D('',#358174,#115287,#115288);
#98865=AXIS2_PLACEMENT_3D('',#358178,#115290,#115291);
#98866=AXIS2_PLACEMENT_3D('',#358182,#115293,#115294);
#98867=AXIS2_PLACEMENT_3D('',#358183,#115295,#115296);
#98868=AXIS2_PLACEMENT_3D('',#358185,#115297,#115298);
#98869=AXIS2_PLACEMENT_3D('',#358188,#115300,#115301);
#98870=AXIS2_PLACEMENT_3D('',#358191,#115302,#115303);
#98871=AXIS2_PLACEMENT_3D('',#358195,#115305,#115306);
#98872=AXIS2_PLACEMENT_3D('',#358199,#115308,#115309);
#98873=AXIS2_PLACEMENT_3D('',#358203,#115311,#115312);
#98874=AXIS2_PLACEMENT_3D('',#358207,#115314,#115315);
#98875=AXIS2_PLACEMENT_3D('',#358211,#115317,#115318);
#98876=AXIS2_PLACEMENT_3D('',#358215,#115320,#115321);
#98877=AXIS2_PLACEMENT_3D('',#358219,#115323,#115324);
#98878=AXIS2_PLACEMENT_3D('',#358223,#115326,#115327);
#98879=AXIS2_PLACEMENT_3D('',#358227,#115329,#115330);
#98880=AXIS2_PLACEMENT_3D('',#358231,#115332,#115333);
#98881=AXIS2_PLACEMENT_3D('',#358235,#115335,#115336);
#98882=AXIS2_PLACEMENT_3D('',#358239,#115338,#115339);
#98883=AXIS2_PLACEMENT_3D('',#358243,#115341,#115342);
#98884=AXIS2_PLACEMENT_3D('',#358245,#115344,#115345);
#98885=AXIS2_PLACEMENT_3D('',#358247,#115346,#115347);
#98886=AXIS2_PLACEMENT_3D('',#358249,#115348,#115349);
#98887=AXIS2_PLACEMENT_3D('',#358250,#115350,#115351);
#98888=AXIS2_PLACEMENT_3D('',#358251,#115352,#115353);
#98889=AXIS2_PLACEMENT_3D('',#358253,#115354,#115355);
#98890=AXIS2_PLACEMENT_3D('',#358257,#115357,#115358);
#98891=AXIS2_PLACEMENT_3D('',#358261,#115360,#115361);
#98892=AXIS2_PLACEMENT_3D('',#358264,#115363,#115364);
#98893=AXIS2_PLACEMENT_3D('',#358267,#115366,#115367);
#98894=AXIS2_PLACEMENT_3D('',#358270,#115368,#115369);
#98895=AXIS2_PLACEMENT_3D('',#358274,#115371,#115372);
#98896=AXIS2_PLACEMENT_3D('',#358278,#115374,#115375);
#98897=AXIS2_PLACEMENT_3D('',#358282,#115377,#115378);
#98898=AXIS2_PLACEMENT_3D('',#358286,#115380,#115381);
#98899=AXIS2_PLACEMENT_3D('',#358290,#115383,#115384);
#98900=AXIS2_PLACEMENT_3D('',#358294,#115386,#115387);
#98901=AXIS2_PLACEMENT_3D('',#358298,#115389,#115390);
#98902=AXIS2_PLACEMENT_3D('',#358302,#115392,#115393);
#98903=AXIS2_PLACEMENT_3D('',#358306,#115395,#115396);
#98904=AXIS2_PLACEMENT_3D('',#358310,#115398,#115399);
#98905=AXIS2_PLACEMENT_3D('',#358314,#115401,#115402);
#98906=AXIS2_PLACEMENT_3D('',#358318,#115404,#115405);
#98907=AXIS2_PLACEMENT_3D('',#358322,#115407,#115408);
#98908=AXIS2_PLACEMENT_3D('',#358324,#115410,#115411);
#98909=AXIS2_PLACEMENT_3D('',#358326,#115412,#115413);
#98910=AXIS2_PLACEMENT_3D('',#358327,#115414,#115415);
#98911=AXIS2_PLACEMENT_3D('',#358328,#115416,#115417);
#98912=AXIS2_PLACEMENT_3D('',#358330,#115418,#115419);
#98913=AXIS2_PLACEMENT_3D('',#358331,#115420,#115421);
#98914=AXIS2_PLACEMENT_3D('',#358332,#115422,#115423);
#98915=AXIS2_PLACEMENT_3D('',#358333,#115424,#115425);
#98916=AXIS2_PLACEMENT_3D('',#358334,#115426,#115427);
#98917=AXIS2_PLACEMENT_3D('',#358335,#115428,#115429);
#98918=AXIS2_PLACEMENT_3D('',#358336,#115430,#115431);
#98919=AXIS2_PLACEMENT_3D('',#358337,#115432,#115433);
#98920=AXIS2_PLACEMENT_3D('',#358338,#115434,#115435);
#98921=AXIS2_PLACEMENT_3D('',#358339,#115436,#115437);
#98922=AXIS2_PLACEMENT_3D('',#358340,#115438,#115439);
#98923=AXIS2_PLACEMENT_3D('',#358341,#115440,#115441);
#98924=AXIS2_PLACEMENT_3D('',#358342,#115442,#115443);
#98925=AXIS2_PLACEMENT_3D('',#358343,#115444,#115445);
#98926=AXIS2_PLACEMENT_3D('',#358344,#115446,#115447);
#98927=AXIS2_PLACEMENT_3D('',#358345,#115448,#115449);
#98928=AXIS2_PLACEMENT_3D('',#358346,#115450,#115451);
#98929=AXIS2_PLACEMENT_3D('',#358347,#115452,#115453);
#98930=AXIS2_PLACEMENT_3D('',#358348,#115454,#115455);
#98931=AXIS2_PLACEMENT_3D('',#358349,#115456,#115457);
#98932=AXIS2_PLACEMENT_3D('',#358350,#115458,#115459);
#98933=AXIS2_PLACEMENT_3D('',#358351,#115460,#115461);
#98934=AXIS2_PLACEMENT_3D('',#358352,#115462,#115463);
#98935=AXIS2_PLACEMENT_3D('',#358353,#115464,#115465);
#98936=AXIS2_PLACEMENT_3D('',#358354,#115466,#115467);
#98937=AXIS2_PLACEMENT_3D('',#358355,#115468,#115469);
#98938=AXIS2_PLACEMENT_3D('',#358356,#115470,#115471);
#98939=AXIS2_PLACEMENT_3D('',#358357,#115472,#115473);
#98940=AXIS2_PLACEMENT_3D('',#358358,#115474,#115475);
#98941=AXIS2_PLACEMENT_3D('',#358359,#115476,#115477);
#98942=AXIS2_PLACEMENT_3D('',#358360,#115478,#115479);
#98943=AXIS2_PLACEMENT_3D('',#358361,#115480,#115481);
#98944=AXIS2_PLACEMENT_3D('',#358362,#115482,#115483);
#98945=AXIS2_PLACEMENT_3D('',#358363,#115484,#115485);
#98946=AXIS2_PLACEMENT_3D('',#358364,#115486,#115487);
#98947=AXIS2_PLACEMENT_3D('',#358365,#115488,#115489);
#98948=AXIS2_PLACEMENT_3D('',#358366,#115490,#115491);
#98949=AXIS2_PLACEMENT_3D('',#358367,#115492,#115493);
#98950=AXIS2_PLACEMENT_3D('',#358368,#115494,#115495);
#98951=AXIS2_PLACEMENT_3D('',#358369,#115496,#115497);
#98952=AXIS2_PLACEMENT_3D('',#358370,#115498,#115499);
#98953=AXIS2_PLACEMENT_3D('',#358371,#115500,#115501);
#98954=AXIS2_PLACEMENT_3D('',#358372,#115502,#115503);
#98955=AXIS2_PLACEMENT_3D('',#358373,#115504,#115505);
#98956=AXIS2_PLACEMENT_3D('',#358374,#115506,#115507);
#98957=AXIS2_PLACEMENT_3D('',#358375,#115508,#115509);
#98958=AXIS2_PLACEMENT_3D('',#358376,#115510,#115511);
#98959=AXIS2_PLACEMENT_3D('',#358377,#115512,#115513);
#98960=AXIS2_PLACEMENT_3D('',#358378,#115514,#115515);
#98961=AXIS2_PLACEMENT_3D('',#358379,#115516,#115517);
#98962=AXIS2_PLACEMENT_3D('',#358380,#115518,#115519);
#98963=AXIS2_PLACEMENT_3D('',#358381,#115520,#115521);
#98964=AXIS2_PLACEMENT_3D('',#358382,#115522,#115523);
#98965=AXIS2_PLACEMENT_3D('',#358383,#115524,#115525);
#98966=AXIS2_PLACEMENT_3D('',#358384,#115526,#115527);
#98967=AXIS2_PLACEMENT_3D('',#358385,#115528,#115529);
#98968=AXIS2_PLACEMENT_3D('',#358386,#115530,#115531);
#98969=AXIS2_PLACEMENT_3D('',#358387,#115532,#115533);
#98970=AXIS2_PLACEMENT_3D('',#358388,#115534,#115535);
#98971=AXIS2_PLACEMENT_3D('',#358389,#115536,#115537);
#98972=AXIS2_PLACEMENT_3D('',#358390,#115538,#115539);
#98973=AXIS2_PLACEMENT_3D('',#358391,#115540,#115541);
#98974=AXIS2_PLACEMENT_3D('',#358392,#115542,#115543);
#98975=AXIS2_PLACEMENT_3D('',#358393,#115544,#115545);
#98976=AXIS2_PLACEMENT_3D('',#358394,#115546,#115547);
#98977=AXIS2_PLACEMENT_3D('',#358395,#115548,#115549);
#98978=AXIS2_PLACEMENT_3D('',#358396,#115550,#115551);
#98979=AXIS2_PLACEMENT_3D('',#358397,#115552,#115553);
#98980=AXIS2_PLACEMENT_3D('',#358399,#115554,#115555);
#98981=AXIS2_PLACEMENT_3D('',#358402,#115557,#115558);
#98982=AXIS2_PLACEMENT_3D('',#358403,#115559,#115560);
#98983=AXIS2_PLACEMENT_3D('',#358405,#115561,#115562);
#98984=AXIS2_PLACEMENT_3D('',#358407,#115564,#115565);
#98985=AXIS2_PLACEMENT_3D('',#358408,#115566,#115567);
#98986=AXIS2_PLACEMENT_3D('',#358411,#115569,#115570);
#98987=AXIS2_PLACEMENT_3D('',#358412,#115571,#115572);
#98988=AXIS2_PLACEMENT_3D('',#358413,#115573,#115574);
#98989=AXIS2_PLACEMENT_3D('',#358415,#115575,#115576);
#98990=AXIS2_PLACEMENT_3D('',#358418,#115578,#115579);
#98991=AXIS2_PLACEMENT_3D('',#358419,#115580,#115581);
#98992=AXIS2_PLACEMENT_3D('',#358421,#115582,#115583);
#98993=AXIS2_PLACEMENT_3D('',#358423,#115585,#115586);
#98994=AXIS2_PLACEMENT_3D('',#358424,#115587,#115588);
#98995=AXIS2_PLACEMENT_3D('',#358427,#115590,#115591);
#98996=AXIS2_PLACEMENT_3D('',#358428,#115592,#115593);
#98997=AXIS2_PLACEMENT_3D('',#358429,#115594,#115595);
#98998=AXIS2_PLACEMENT_3D('',#358431,#115596,#115597);
#98999=AXIS2_PLACEMENT_3D('',#358434,#115599,#115600);
#99000=AXIS2_PLACEMENT_3D('',#358435,#115601,#115602);
#99001=AXIS2_PLACEMENT_3D('',#358437,#115603,#115604);
#99002=AXIS2_PLACEMENT_3D('',#358439,#115606,#115607);
#99003=AXIS2_PLACEMENT_3D('',#358440,#115608,#115609);
#99004=AXIS2_PLACEMENT_3D('',#358443,#115611,#115612);
#99005=AXIS2_PLACEMENT_3D('',#358444,#115613,#115614);
#99006=AXIS2_PLACEMENT_3D('',#358445,#115615,#115616);
#99007=AXIS2_PLACEMENT_3D('',#358447,#115617,#115618);
#99008=AXIS2_PLACEMENT_3D('',#358450,#115620,#115621);
#99009=AXIS2_PLACEMENT_3D('',#358451,#115622,#115623);
#99010=AXIS2_PLACEMENT_3D('',#358453,#115624,#115625);
#99011=AXIS2_PLACEMENT_3D('',#358455,#115627,#115628);
#99012=AXIS2_PLACEMENT_3D('',#358456,#115629,#115630);
#99013=AXIS2_PLACEMENT_3D('',#358459,#115632,#115633);
#99014=AXIS2_PLACEMENT_3D('',#358460,#115634,#115635);
#99015=AXIS2_PLACEMENT_3D('',#358461,#115636,#115637);
#99016=AXIS2_PLACEMENT_3D('',#358463,#115638,#115639);
#99017=AXIS2_PLACEMENT_3D('',#358466,#115641,#115642);
#99018=AXIS2_PLACEMENT_3D('',#358467,#115643,#115644);
#99019=AXIS2_PLACEMENT_3D('',#358469,#115645,#115646);
#99020=AXIS2_PLACEMENT_3D('',#358471,#115648,#115649);
#99021=AXIS2_PLACEMENT_3D('',#358472,#115650,#115651);
#99022=AXIS2_PLACEMENT_3D('',#358475,#115653,#115654);
#99023=AXIS2_PLACEMENT_3D('',#358476,#115655,#115656);
#99024=AXIS2_PLACEMENT_3D('',#358477,#115657,#115658);
#99025=AXIS2_PLACEMENT_3D('',#358479,#115659,#115660);
#99026=AXIS2_PLACEMENT_3D('',#358482,#115662,#115663);
#99027=AXIS2_PLACEMENT_3D('',#358483,#115664,#115665);
#99028=AXIS2_PLACEMENT_3D('',#358485,#115666,#115667);
#99029=AXIS2_PLACEMENT_3D('',#358487,#115669,#115670);
#99030=AXIS2_PLACEMENT_3D('',#358488,#115671,#115672);
#99031=AXIS2_PLACEMENT_3D('',#358491,#115674,#115675);
#99032=AXIS2_PLACEMENT_3D('',#358492,#115676,#115677);
#99033=AXIS2_PLACEMENT_3D('',#358493,#115678,#115679);
#99034=AXIS2_PLACEMENT_3D('',#358495,#115680,#115681);
#99035=AXIS2_PLACEMENT_3D('',#358498,#115683,#115684);
#99036=AXIS2_PLACEMENT_3D('',#358499,#115685,#115686);
#99037=AXIS2_PLACEMENT_3D('',#358501,#115687,#115688);
#99038=AXIS2_PLACEMENT_3D('',#358503,#115690,#115691);
#99039=AXIS2_PLACEMENT_3D('',#358504,#115692,#115693);
#99040=AXIS2_PLACEMENT_3D('',#358507,#115695,#115696);
#99041=AXIS2_PLACEMENT_3D('',#358508,#115697,#115698);
#99042=AXIS2_PLACEMENT_3D('',#358509,#115699,#115700);
#99043=AXIS2_PLACEMENT_3D('',#358511,#115701,#115702);
#99044=AXIS2_PLACEMENT_3D('',#358514,#115704,#115705);
#99045=AXIS2_PLACEMENT_3D('',#358515,#115706,#115707);
#99046=AXIS2_PLACEMENT_3D('',#358517,#115708,#115709);
#99047=AXIS2_PLACEMENT_3D('',#358519,#115711,#115712);
#99048=AXIS2_PLACEMENT_3D('',#358520,#115713,#115714);
#99049=AXIS2_PLACEMENT_3D('',#358523,#115716,#115717);
#99050=AXIS2_PLACEMENT_3D('',#358524,#115718,#115719);
#99051=AXIS2_PLACEMENT_3D('',#358525,#115720,#115721);
#99052=AXIS2_PLACEMENT_3D('',#358526,#115722,#115723);
#99053=AXIS2_PLACEMENT_3D('',#358527,#115724,#115725);
#99054=AXIS2_PLACEMENT_3D('',#358546,#115727,#115728);
#99055=AXIS2_PLACEMENT_3D('',#358560,#115729,#115730);
#99056=AXIS2_PLACEMENT_3D('',#358590,#115732,#115733);
#99057=AXIS2_PLACEMENT_3D('',#358620,#115735,#115736);
#99058=AXIS2_PLACEMENT_3D('',#358650,#115738,#115739);
#99059=AXIS2_PLACEMENT_3D('',#358680,#115741,#115742);
#99060=AXIS2_PLACEMENT_3D('',#358710,#115744,#115745);
#99061=AXIS2_PLACEMENT_3D('',#358740,#115747,#115748);
#99062=AXIS2_PLACEMENT_3D('',#358770,#115750,#115751);
#99063=AXIS2_PLACEMENT_3D('',#358800,#115753,#115754);
#99064=AXIS2_PLACEMENT_3D('',#358830,#115756,#115757);
#99065=AXIS2_PLACEMENT_3D('',#358860,#115759,#115760);
#99066=AXIS2_PLACEMENT_3D('',#358890,#115762,#115763);
#99067=AXIS2_PLACEMENT_3D('',#358920,#115765,#115766);
#99068=AXIS2_PLACEMENT_3D('',#358950,#115768,#115769);
#99069=AXIS2_PLACEMENT_3D('',#358980,#115771,#115772);
#99070=AXIS2_PLACEMENT_3D('',#359010,#115774,#115775);
#99071=AXIS2_PLACEMENT_3D('',#359040,#115777,#115778);
#99072=AXIS2_PLACEMENT_3D('',#359070,#115780,#115781);
#99073=AXIS2_PLACEMENT_3D('',#359100,#115783,#115784);
#99074=AXIS2_PLACEMENT_3D('',#359130,#115786,#115787);
#99075=AXIS2_PLACEMENT_3D('',#359160,#115789,#115790);
#99076=AXIS2_PLACEMENT_3D('',#359190,#115792,#115793);
#99077=AXIS2_PLACEMENT_3D('',#359220,#115795,#115796);
#99078=AXIS2_PLACEMENT_3D('',#359250,#115798,#115799);
#99079=AXIS2_PLACEMENT_3D('',#359280,#115801,#115802);
#99080=AXIS2_PLACEMENT_3D('',#359310,#115804,#115805);
#99081=AXIS2_PLACEMENT_3D('',#359340,#115807,#115808);
#99082=AXIS2_PLACEMENT_3D('',#359370,#115810,#115811);
#99083=AXIS2_PLACEMENT_3D('',#359400,#115813,#115814);
#99084=AXIS2_PLACEMENT_3D('',#359430,#115816,#115817);
#99085=AXIS2_PLACEMENT_3D('',#359460,#115819,#115820);
#99086=AXIS2_PLACEMENT_3D('',#359465,#115822,#115823);
#99087=AXIS2_PLACEMENT_3D('',#359492,#115824,#115825);
#99088=AXIS2_PLACEMENT_3D('',#359505,#115827,#115828);
#99089=AXIS2_PLACEMENT_3D('',#359522,#115829,#115830);
#99090=AXIS2_PLACEMENT_3D('',#359598,#115832,#115833);
#99091=AXIS2_PLACEMENT_3D('',#359674,#115835,#115836);
#99092=AXIS2_PLACEMENT_3D('',#359752,#115838,#115839);
#99093=AXIS2_PLACEMENT_3D('',#359830,#115841,#115842);
#99094=AXIS2_PLACEMENT_3D('',#359906,#115844,#115845);
#99095=AXIS2_PLACEMENT_3D('',#359982,#115847,#115848);
#99096=AXIS2_PLACEMENT_3D('',#360058,#115850,#115851);
#99097=AXIS2_PLACEMENT_3D('',#360134,#115853,#115854);
#99098=AXIS2_PLACEMENT_3D('',#360212,#115856,#115857);
#99099=AXIS2_PLACEMENT_3D('',#360290,#115859,#115860);
#99100=AXIS2_PLACEMENT_3D('',#360366,#115862,#115863);
#99101=AXIS2_PLACEMENT_3D('',#360442,#115865,#115866);
#99102=AXIS2_PLACEMENT_3D('',#360518,#115868,#115869);
#99103=AXIS2_PLACEMENT_3D('',#360594,#115871,#115872);
#99104=AXIS2_PLACEMENT_3D('',#360670,#115874,#115875);
#99105=AXIS2_PLACEMENT_3D('',#360748,#115877,#115878);
#99106=AXIS2_PLACEMENT_3D('',#360826,#115880,#115881);
#99107=AXIS2_PLACEMENT_3D('',#360902,#115883,#115884);
#99108=AXIS2_PLACEMENT_3D('',#360978,#115886,#115887);
#99109=AXIS2_PLACEMENT_3D('',#361054,#115889,#115890);
#99110=AXIS2_PLACEMENT_3D('',#361130,#115892,#115893);
#99111=AXIS2_PLACEMENT_3D('',#361206,#115895,#115896);
#99112=AXIS2_PLACEMENT_3D('',#361284,#115898,#115899);
#99113=AXIS2_PLACEMENT_3D('',#361362,#115901,#115902);
#99114=AXIS2_PLACEMENT_3D('',#361438,#115904,#115905);
#99115=AXIS2_PLACEMENT_3D('',#361514,#115907,#115908);
#99116=AXIS2_PLACEMENT_3D('',#361590,#115910,#115911);
#99117=AXIS2_PLACEMENT_3D('',#361666,#115913,#115914);
#99118=AXIS2_PLACEMENT_3D('',#361744,#115916,#115917);
#99119=AXIS2_PLACEMENT_3D('',#361822,#115919,#115920);
#99120=AXIS2_PLACEMENT_3D('',#361828,#115921,#115922);
#99121=AXIS2_PLACEMENT_3D('',#361829,#115923,#115924);
#99122=AXIS2_PLACEMENT_3D('',#361831,#115925,#115926);
#99123=AXIS2_PLACEMENT_3D('',#361833,#115927,#115928);
#99124=AXIS2_PLACEMENT_3D('',#361834,#115929,#115930);
#99125=AXIS2_PLACEMENT_3D('',#361836,#115931,#115932);
#99126=AXIS2_PLACEMENT_3D('',#361839,#115934,#115935);
#99127=AXIS2_PLACEMENT_3D('',#361840,#115936,#115937);
#99128=AXIS2_PLACEMENT_3D('',#361842,#115938,#115939);
#99129=AXIS2_PLACEMENT_3D('',#361857,#115940,#115941);
#99130=AXIS2_PLACEMENT_3D('',#361885,#115943,#115944);
#99131=AXIS2_PLACEMENT_3D('',#361902,#115945,#115946);
#99132=AXIS2_PLACEMENT_3D('',#361959,#115947,#115948);
#99133=AXIS2_PLACEMENT_3D('',#361960,#115949,#115950);
#99134=AXIS2_PLACEMENT_3D('',#361995,#115951,#115952);
#99135=AXIS2_PLACEMENT_3D('',#361996,#115953,#115954);
#99136=AXIS2_PLACEMENT_3D('',#361999,#115955,#115956);
#99137=AXIS2_PLACEMENT_3D('',#362001,#115957,#115958);
#99138=AXIS2_PLACEMENT_3D('',#362002,#115959,#115960);
#99139=AXIS2_PLACEMENT_3D('',#362004,#115961,#115962);
#99140=AXIS2_PLACEMENT_3D('',#362005,#115963,#115964);
#99141=AXIS2_PLACEMENT_3D('',#362006,#115965,#115966);
#99142=AXIS2_PLACEMENT_3D('',#362010,#115967,#115968);
#99143=AXIS2_PLACEMENT_3D('',#362014,#115969,#115970);
#99144=AXIS2_PLACEMENT_3D('',#362018,#115971,#115972);
#99145=AXIS2_PLACEMENT_3D('',#362022,#115973,#115974);
#99146=AXIS2_PLACEMENT_3D('',#362026,#115975,#115976);
#99147=AXIS2_PLACEMENT_3D('',#362039,#115983,#115984);
#99148=AXIS2_PLACEMENT_3D('',#362042,#115987,#115988);
#99149=AXIS2_PLACEMENT_3D('',#362044,#115990,#115991);
#99150=AXIS2_PLACEMENT_3D('',#362046,#115993,#115994);
#99151=AXIS2_PLACEMENT_3D('',#362048,#115996,#115997);
#99152=AXIS2_PLACEMENT_3D('',#362050,#115999,#116000);
#99153=AXIS2_PLACEMENT_3D('',#362845,#116001,#116002);
#99154=AXIS2_PLACEMENT_3D('',#363643,#116003,#116004);
#99155=AXIS2_PLACEMENT_3D('',#363849,#116005,#116006);
#99156=AXIS2_PLACEMENT_3D('',#363881,#116007,#116008);
#99157=AXIS2_PLACEMENT_3D('',#363912,#116009,#116010);
#99158=AXIS2_PLACEMENT_3D('',#364608,#116011,#116012);
#99159=AXIS2_PLACEMENT_3D('',#364610,#116013,#116014);
#99160=AXIS2_PLACEMENT_3D('',#365014,#116015,#116016);
#99161=AXIS2_PLACEMENT_3D('',#365276,#116017,#116018);
#99162=AXIS2_PLACEMENT_3D('',#365278,#116019,#116020);
#99163=AXIS2_PLACEMENT_3D('',#365279,#116021,#116022);
#99164=AXIS2_PLACEMENT_3D('',#365280,#116023,#116024);
#99165=AXIS2_PLACEMENT_3D('',#365975,#116025,#116026);
#99166=AXIS2_PLACEMENT_3D('',#365976,#116027,#116028);
#99167=AXIS2_PLACEMENT_3D('',#365977,#116029,#116030);
#99168=AXIS2_PLACEMENT_3D('',#365978,#116031,#116032);
#99169=AXIS2_PLACEMENT_3D('',#366182,#116033,#116034);
#99170=AXIS2_PLACEMENT_3D('',#366183,#116035,#116036);
#99171=AXIS2_PLACEMENT_3D('',#366184,#116037,#116038);
#99172=AXIS2_PLACEMENT_3D('',#366185,#116039,#116040);
#99173=AXIS2_PLACEMENT_3D('',#366187,#116041,#116042);
#99174=AXIS2_PLACEMENT_3D('',#366190,#116044,#116045);
#99175=AXIS2_PLACEMENT_3D('',#366191,#116046,#116047);
#99176=AXIS2_PLACEMENT_3D('',#366193,#116048,#116049);
#99177=AXIS2_PLACEMENT_3D('',#366194,#116050,#116051);
#99178=AXIS2_PLACEMENT_3D('',#366195,#116052,#116053);
#99179=AXIS2_PLACEMENT_3D('',#366197,#116054,#116055);
#99180=AXIS2_PLACEMENT_3D('',#366199,#116057,#116058);
#99181=AXIS2_PLACEMENT_3D('',#366201,#116059,#116060);
#99182=AXIS2_PLACEMENT_3D('',#366204,#116062,#116063);
#99183=AXIS2_PLACEMENT_3D('',#366205,#116064,#116065);
#99184=AXIS2_PLACEMENT_3D('',#366208,#116066,#116067);
#99185=AXIS2_PLACEMENT_3D('',#366209,#116068,#116069);
#99186=AXIS2_PLACEMENT_3D('',#366211,#116071,#116072);
#99187=AXIS2_PLACEMENT_3D('',#366214,#116074,#116075);
#99188=AXIS2_PLACEMENT_3D('',#366215,#116076,#116077);
#99189=AXIS2_PLACEMENT_3D('',#366216,#116078,#116079);
#99190=AXIS2_PLACEMENT_3D('',#366217,#116080,#116081);
#99191=AXIS2_PLACEMENT_3D('',#366219,#116082,#116083);
#99192=AXIS2_PLACEMENT_3D('',#366221,#116084,#116085);
#99193=AXIS2_PLACEMENT_3D('',#366222,#116086,#116087);
#99194=AXIS2_PLACEMENT_3D('',#366223,#116088,#116089);
#99195=AXIS2_PLACEMENT_3D('',#366225,#116090,#116091);
#99196=AXIS2_PLACEMENT_3D('',#366228,#116093,#116094);
#99197=AXIS2_PLACEMENT_3D('',#366229,#116095,#116096);
#99198=AXIS2_PLACEMENT_3D('',#366232,#116097,#116098);
#99199=AXIS2_PLACEMENT_3D('',#366233,#116099,#116100);
#99200=AXIS2_PLACEMENT_3D('',#366235,#116102,#116103);
#99201=AXIS2_PLACEMENT_3D('',#366238,#116105,#116106);
#99202=AXIS2_PLACEMENT_3D('',#366239,#116107,#116108);
#99203=AXIS2_PLACEMENT_3D('',#366242,#116110,#116111);
#99204=AXIS2_PLACEMENT_3D('',#366243,#116112,#116113);
#99205=AXIS2_PLACEMENT_3D('',#366245,#116114,#116115);
#99206=AXIS2_PLACEMENT_3D('',#366247,#116117,#116118);
#99207=AXIS2_PLACEMENT_3D('',#366248,#116119,#116120);
#99208=AXIS2_PLACEMENT_3D('',#366249,#116121,#116122);
#99209=AXIS2_PLACEMENT_3D('',#366252,#116123,#116124);
#99210=AXIS2_PLACEMENT_3D('',#366253,#116125,#116126);
#99211=AXIS2_PLACEMENT_3D('',#366256,#116127,#116128);
#99212=AXIS2_PLACEMENT_3D('',#366257,#116129,#116130);
#99213=AXIS2_PLACEMENT_3D('',#366260,#116131,#116132);
#99214=AXIS2_PLACEMENT_3D('',#366261,#116133,#116134);
#99215=AXIS2_PLACEMENT_3D('',#366264,#116135,#116136);
#99216=AXIS2_PLACEMENT_3D('',#366265,#116137,#116138);
#99217=AXIS2_PLACEMENT_3D('',#366268,#116139,#116140);
#99218=AXIS2_PLACEMENT_3D('',#366269,#116141,#116142);
#99219=AXIS2_PLACEMENT_3D('',#366272,#116143,#116144);
#99220=AXIS2_PLACEMENT_3D('',#366273,#116145,#116146);
#99221=AXIS2_PLACEMENT_3D('',#366276,#116147,#116148);
#99222=AXIS2_PLACEMENT_3D('',#366277,#116149,#116150);
#99223=AXIS2_PLACEMENT_3D('',#366280,#116151,#116152);
#99224=AXIS2_PLACEMENT_3D('',#366281,#116153,#116154);
#99225=AXIS2_PLACEMENT_3D('',#366284,#116155,#116156);
#99226=AXIS2_PLACEMENT_3D('',#366285,#116157,#116158);
#99227=AXIS2_PLACEMENT_3D('',#366288,#116159,#116160);
#99228=AXIS2_PLACEMENT_3D('',#366289,#116161,#116162);
#99229=AXIS2_PLACEMENT_3D('',#366292,#116163,#116164);
#99230=AXIS2_PLACEMENT_3D('',#366293,#116165,#116166);
#99231=AXIS2_PLACEMENT_3D('',#366296,#116167,#116168);
#99232=AXIS2_PLACEMENT_3D('',#366297,#116169,#116170);
#99233=AXIS2_PLACEMENT_3D('',#366299,#116171,#116172);
#99234=AXIS2_PLACEMENT_3D('',#366302,#116174,#116175);
#99235=AXIS2_PLACEMENT_3D('',#366303,#116176,#116177);
#99236=AXIS2_PLACEMENT_3D('',#366305,#116178,#116179);
#99237=AXIS2_PLACEMENT_3D('',#366308,#116181,#116182);
#99238=AXIS2_PLACEMENT_3D('',#366309,#116183,#116184);
#99239=AXIS2_PLACEMENT_3D('',#366310,#116185,#116186);
#99240=AXIS2_PLACEMENT_3D('',#366311,#116187,#116188);
#99241=AXIS2_PLACEMENT_3D('',#366313,#116189,#116190);
#99242=AXIS2_PLACEMENT_3D('',#366316,#116192,#116193);
#99243=AXIS2_PLACEMENT_3D('',#366317,#116194,#116195);
#99244=AXIS2_PLACEMENT_3D('',#366319,#116196,#116197);
#99245=AXIS2_PLACEMENT_3D('',#366322,#116199,#116200);
#99246=AXIS2_PLACEMENT_3D('',#366323,#116201,#116202);
#99247=AXIS2_PLACEMENT_3D('',#366324,#116203,#116204);
#99248=AXIS2_PLACEMENT_3D('',#366325,#116205,#116206);
#99249=AXIS2_PLACEMENT_3D('',#366326,#116207,#116208);
#99250=AXIS2_PLACEMENT_3D('',#366334,#116210,#116211);
#99251=AXIS2_PLACEMENT_3D('',#366335,#116212,#116213);
#99252=AXIS2_PLACEMENT_3D('',#366353,#116215,#116216);
#99253=AXIS2_PLACEMENT_3D('',#366367,#116217,#116218);
#99254=AXIS2_PLACEMENT_3D('',#366397,#116220,#116221);
#99255=AXIS2_PLACEMENT_3D('',#366427,#116223,#116224);
#99256=AXIS2_PLACEMENT_3D('',#366457,#116226,#116227);
#99257=AXIS2_PLACEMENT_3D('',#366487,#116229,#116230);
#99258=AXIS2_PLACEMENT_3D('',#366517,#116232,#116233);
#99259=AXIS2_PLACEMENT_3D('',#366547,#116235,#116236);
#99260=AXIS2_PLACEMENT_3D('',#366577,#116238,#116239);
#99261=AXIS2_PLACEMENT_3D('',#366607,#116241,#116242);
#99262=AXIS2_PLACEMENT_3D('',#366637,#116244,#116245);
#99263=AXIS2_PLACEMENT_3D('',#366667,#116247,#116248);
#99264=AXIS2_PLACEMENT_3D('',#366697,#116250,#116251);
#99265=AXIS2_PLACEMENT_3D('',#366727,#116253,#116254);
#99266=AXIS2_PLACEMENT_3D('',#366757,#116256,#116257);
#99267=AXIS2_PLACEMENT_3D('',#366787,#116259,#116260);
#99268=AXIS2_PLACEMENT_3D('',#366813,#116262,#116263);
#99269=AXIS2_PLACEMENT_3D('',#366830,#116264,#116265);
#99270=AXIS2_PLACEMENT_3D('',#366906,#116267,#116268);
#99271=AXIS2_PLACEMENT_3D('',#366984,#116270,#116271);
#99272=AXIS2_PLACEMENT_3D('',#367060,#116273,#116274);
#99273=AXIS2_PLACEMENT_3D('',#367136,#116276,#116277);
#99274=AXIS2_PLACEMENT_3D('',#367212,#116279,#116280);
#99275=AXIS2_PLACEMENT_3D('',#367288,#116282,#116283);
#99276=AXIS2_PLACEMENT_3D('',#367366,#116285,#116286);
#99277=AXIS2_PLACEMENT_3D('',#367444,#116288,#116289);
#99278=AXIS2_PLACEMENT_3D('',#367520,#116291,#116292);
#99279=AXIS2_PLACEMENT_3D('',#367596,#116294,#116295);
#99280=AXIS2_PLACEMENT_3D('',#367672,#116297,#116298);
#99281=AXIS2_PLACEMENT_3D('',#367748,#116300,#116301);
#99282=AXIS2_PLACEMENT_3D('',#367826,#116303,#116304);
#99283=AXIS2_PLACEMENT_3D('',#367902,#116306,#116307);
#99284=AXIS2_PLACEMENT_3D('',#367908,#116308,#116309);
#99285=AXIS2_PLACEMENT_3D('',#367909,#116310,#116311);
#99286=AXIS2_PLACEMENT_3D('',#367911,#116312,#116313);
#99287=AXIS2_PLACEMENT_3D('',#367913,#116314,#116315);
#99288=AXIS2_PLACEMENT_3D('',#367914,#116316,#116317);
#99289=AXIS2_PLACEMENT_3D('',#367916,#116318,#116319);
#99290=AXIS2_PLACEMENT_3D('',#367919,#116321,#116322);
#99291=AXIS2_PLACEMENT_3D('',#367920,#116323,#116324);
#99292=AXIS2_PLACEMENT_3D('',#367935,#116325,#116326);
#99293=AXIS2_PLACEMENT_3D('',#367965,#116328,#116329);
#99294=AXIS2_PLACEMENT_3D('',#367982,#116330,#116331);
#99295=AXIS2_PLACEMENT_3D('',#368045,#116332,#116333);
#99296=AXIS2_PLACEMENT_3D('',#368046,#116334,#116335);
#99297=AXIS2_PLACEMENT_3D('',#368067,#116336,#116337);
#99298=AXIS2_PLACEMENT_3D('',#368084,#116338,#116339);
#99299=AXIS2_PLACEMENT_3D('',#368085,#116340,#116341);
#99300=AXIS2_PLACEMENT_3D('',#368088,#116342,#116343);
#99301=AXIS2_PLACEMENT_3D('',#368090,#116344,#116345);
#99302=AXIS2_PLACEMENT_3D('',#368091,#116346,#116347);
#99303=AXIS2_PLACEMENT_3D('',#368093,#116348,#116349);
#99304=AXIS2_PLACEMENT_3D('',#368094,#116350,#116351);
#99305=AXIS2_PLACEMENT_3D('',#368095,#116352,#116353);
#99306=AXIS2_PLACEMENT_3D('',#368099,#116354,#116355);
#99307=AXIS2_PLACEMENT_3D('',#368103,#116356,#116357);
#99308=AXIS2_PLACEMENT_3D('',#368107,#116358,#116359);
#99309=AXIS2_PLACEMENT_3D('',#368111,#116360,#116361);
#99310=AXIS2_PLACEMENT_3D('',#368115,#116362,#116363);
#99311=AXIS2_PLACEMENT_3D('',#368128,#116370,#116371);
#99312=AXIS2_PLACEMENT_3D('',#368131,#116374,#116375);
#99313=AXIS2_PLACEMENT_3D('',#368133,#116377,#116378);
#99314=AXIS2_PLACEMENT_3D('',#368135,#116380,#116381);
#99315=AXIS2_PLACEMENT_3D('',#368137,#116383,#116384);
#99316=AXIS2_PLACEMENT_3D('',#368139,#116386,#116387);
#99317=AXIS2_PLACEMENT_3D('',#368563,#116388,#116389);
#99318=AXIS2_PLACEMENT_3D('',#368987,#116390,#116391);
#99319=AXIS2_PLACEMENT_3D('',#368988,#116392,#116393);
#99320=AXIS2_PLACEMENT_3D('',#369001,#116395,#116396);
#99321=AXIS2_PLACEMENT_3D('',#369007,#116397,#116398);
#99322=AXIS2_PLACEMENT_3D('',#369037,#116400,#116401);
#99323=AXIS2_PLACEMENT_3D('',#369067,#116403,#116404);
#99324=AXIS2_PLACEMENT_3D('',#369097,#116406,#116407);
#99325=AXIS2_PLACEMENT_3D('',#369127,#116409,#116410);
#99326=AXIS2_PLACEMENT_3D('',#369157,#116412,#116413);
#99327=AXIS2_PLACEMENT_3D('',#369187,#116415,#116416);
#99328=AXIS2_PLACEMENT_3D('',#369217,#116418,#116419);
#99329=AXIS2_PLACEMENT_3D('',#369247,#116421,#116422);
#99330=AXIS2_PLACEMENT_3D('',#369277,#116424,#116425);
#99331=AXIS2_PLACEMENT_3D('',#369307,#116427,#116428);
#99332=AXIS2_PLACEMENT_3D('',#369337,#116430,#116431);
#99333=AXIS2_PLACEMENT_3D('',#369367,#116433,#116434);
#99334=AXIS2_PLACEMENT_3D('',#369397,#116436,#116437);
#99335=AXIS2_PLACEMENT_3D('',#369402,#116439,#116440);
#99336=AXIS2_PLACEMENT_3D('',#369429,#116441,#116442);
#99337=AXIS2_PLACEMENT_3D('',#369451,#116444,#116445);
#99338=AXIS2_PLACEMENT_3D('',#369464,#116446,#116447);
#99339=AXIS2_PLACEMENT_3D('',#369540,#116449,#116450);
#99340=AXIS2_PLACEMENT_3D('',#369616,#116452,#116453);
#99341=AXIS2_PLACEMENT_3D('',#369692,#116455,#116456);
#99342=AXIS2_PLACEMENT_3D('',#369768,#116458,#116459);
#99343=AXIS2_PLACEMENT_3D('',#369846,#116461,#116462);
#99344=AXIS2_PLACEMENT_3D('',#369924,#116464,#116465);
#99345=AXIS2_PLACEMENT_3D('',#370000,#116467,#116468);
#99346=AXIS2_PLACEMENT_3D('',#370076,#116470,#116471);
#99347=AXIS2_PLACEMENT_3D('',#370152,#116473,#116474);
#99348=AXIS2_PLACEMENT_3D('',#370228,#116476,#116477);
#99349=AXIS2_PLACEMENT_3D('',#370304,#116479,#116480);
#99350=AXIS2_PLACEMENT_3D('',#370382,#116482,#116483);
#99351=AXIS2_PLACEMENT_3D('',#370460,#116485,#116486);
#99352=AXIS2_PLACEMENT_3D('',#370462,#116487,#116488);
#99353=AXIS2_PLACEMENT_3D('',#370502,#116490,#116491);
#99354=AXIS2_PLACEMENT_3D('',#370521,#116492,#116493);
#99355=AXIS2_PLACEMENT_3D('',#370554,#116494,#116495);
#99356=AXIS2_PLACEMENT_3D('',#370581,#116496,#116497);
#99357=AXIS2_PLACEMENT_3D('',#370587,#116498,#116499);
#99358=AXIS2_PLACEMENT_3D('',#370588,#116500,#116501);
#99359=AXIS2_PLACEMENT_3D('',#370590,#116502,#116503);
#99360=AXIS2_PLACEMENT_3D('',#370593,#116505,#116506);
#99361=AXIS2_PLACEMENT_3D('',#370594,#116507,#116508);
#99362=AXIS2_PLACEMENT_3D('',#370598,#116510,#116511);
#99363=AXIS2_PLACEMENT_3D('',#370661,#116512,#116513);
#99364=AXIS2_PLACEMENT_3D('',#370662,#116514,#116515);
#99365=AXIS2_PLACEMENT_3D('',#370664,#116516,#116517);
#99366=AXIS2_PLACEMENT_3D('',#370666,#116518,#116519);
#99367=AXIS2_PLACEMENT_3D('',#370668,#116520,#116521);
#99368=AXIS2_PLACEMENT_3D('',#370670,#116522,#116523);
#99369=AXIS2_PLACEMENT_3D('',#370671,#116524,#116525);
#99370=AXIS2_PLACEMENT_3D('',#370672,#116526,#116527);
#99371=AXIS2_PLACEMENT_3D('',#370693,#116528,#116529);
#99372=AXIS2_PLACEMENT_3D('',#370697,#116530,#116531);
#99373=AXIS2_PLACEMENT_3D('',#370701,#116532,#116533);
#99374=AXIS2_PLACEMENT_3D('',#370705,#116534,#116535);
#99375=AXIS2_PLACEMENT_3D('',#370709,#116536,#116537);
#99376=AXIS2_PLACEMENT_3D('',#370713,#116538,#116539);
#99377=AXIS2_PLACEMENT_3D('',#370726,#116546,#116547);
#99378=AXIS2_PLACEMENT_3D('',#370729,#116550,#116551);
#99379=AXIS2_PLACEMENT_3D('',#370731,#116553,#116554);
#99380=AXIS2_PLACEMENT_3D('',#370733,#116556,#116557);
#99381=AXIS2_PLACEMENT_3D('',#370735,#116559,#116560);
#99382=AXIS2_PLACEMENT_3D('',#370737,#116562,#116563);
#99383=AXIS2_PLACEMENT_3D('',#370738,#116564,#116565);
#99384=AXIS2_PLACEMENT_3D('',#371173,#116566,#116567);
#99385=AXIS2_PLACEMENT_3D('',#371607,#116568,#116569);
#99386=AXIS2_PLACEMENT_3D('',#371608,#116570,#116571);
#99387=AXIS2_PLACEMENT_3D('',#371616,#116573,#116574);
#99388=AXIS2_PLACEMENT_3D('',#371617,#116575,#116576);
#99389=AXIS2_PLACEMENT_3D('',#371647,#116578,#116579);
#99390=AXIS2_PLACEMENT_3D('',#371677,#116581,#116582);
#99391=AXIS2_PLACEMENT_3D('',#371707,#116584,#116585);
#99392=AXIS2_PLACEMENT_3D('',#371737,#116587,#116588);
#99393=AXIS2_PLACEMENT_3D('',#371767,#116590,#116591);
#99394=AXIS2_PLACEMENT_3D('',#371797,#116593,#116594);
#99395=AXIS2_PLACEMENT_3D('',#371827,#116596,#116597);
#99396=AXIS2_PLACEMENT_3D('',#371857,#116599,#116600);
#99397=AXIS2_PLACEMENT_3D('',#371887,#116602,#116603);
#99398=AXIS2_PLACEMENT_3D('',#371917,#116605,#116606);
#99399=AXIS2_PLACEMENT_3D('',#371947,#116608,#116609);
#99400=AXIS2_PLACEMENT_3D('',#371977,#116611,#116612);
#99401=AXIS2_PLACEMENT_3D('',#372007,#116614,#116615);
#99402=AXIS2_PLACEMENT_3D('',#372037,#116617,#116618);
#99403=AXIS2_PLACEMENT_3D('',#372067,#116620,#116621);
#99404=AXIS2_PLACEMENT_3D('',#372097,#116623,#116624);
#99405=AXIS2_PLACEMENT_3D('',#372127,#116626,#116627);
#99406=AXIS2_PLACEMENT_3D('',#372157,#116629,#116630);
#99407=AXIS2_PLACEMENT_3D('',#372187,#116632,#116633);
#99408=AXIS2_PLACEMENT_3D('',#372217,#116635,#116636);
#99409=AXIS2_PLACEMENT_3D('',#372247,#116638,#116639);
#99410=AXIS2_PLACEMENT_3D('',#372277,#116641,#116642);
#99411=AXIS2_PLACEMENT_3D('',#372307,#116644,#116645);
#99412=AXIS2_PLACEMENT_3D('',#372337,#116647,#116648);
#99413=AXIS2_PLACEMENT_3D('',#372367,#116650,#116651);
#99414=AXIS2_PLACEMENT_3D('',#372397,#116653,#116654);
#99415=AXIS2_PLACEMENT_3D('',#372427,#116656,#116657);
#99416=AXIS2_PLACEMENT_3D('',#372457,#116659,#116660);
#99417=AXIS2_PLACEMENT_3D('',#372483,#116662,#116663);
#99418=AXIS2_PLACEMENT_3D('',#372486,#116665,#116666);
#99419=AXIS2_PLACEMENT_3D('',#372488,#116667,#116668);
#99420=AXIS2_PLACEMENT_3D('',#372505,#116669,#116670);
#99421=AXIS2_PLACEMENT_3D('',#372581,#116672,#116673);
#99422=AXIS2_PLACEMENT_3D('',#372657,#116675,#116676);
#99423=AXIS2_PLACEMENT_3D('',#372735,#116678,#116679);
#99424=AXIS2_PLACEMENT_3D('',#372813,#116681,#116682);
#99425=AXIS2_PLACEMENT_3D('',#372889,#116684,#116685);
#99426=AXIS2_PLACEMENT_3D('',#372965,#116687,#116688);
#99427=AXIS2_PLACEMENT_3D('',#373041,#116690,#116691);
#99428=AXIS2_PLACEMENT_3D('',#373117,#116693,#116694);
#99429=AXIS2_PLACEMENT_3D('',#373193,#116696,#116697);
#99430=AXIS2_PLACEMENT_3D('',#373273,#116699,#116700);
#99431=AXIS2_PLACEMENT_3D('',#373349,#116702,#116703);
#99432=AXIS2_PLACEMENT_3D('',#373425,#116705,#116706);
#99433=AXIS2_PLACEMENT_3D('',#373501,#116708,#116709);
#99434=AXIS2_PLACEMENT_3D('',#373577,#116711,#116712);
#99435=AXIS2_PLACEMENT_3D('',#373653,#116714,#116715);
#99436=AXIS2_PLACEMENT_3D('',#373729,#116717,#116718);
#99437=AXIS2_PLACEMENT_3D('',#373809,#116720,#116721);
#99438=AXIS2_PLACEMENT_3D('',#373885,#116723,#116724);
#99439=AXIS2_PLACEMENT_3D('',#373961,#116726,#116727);
#99440=AXIS2_PLACEMENT_3D('',#374037,#116729,#116730);
#99441=AXIS2_PLACEMENT_3D('',#374113,#116732,#116733);
#99442=AXIS2_PLACEMENT_3D('',#374189,#116735,#116736);
#99443=AXIS2_PLACEMENT_3D('',#374267,#116738,#116739);
#99444=AXIS2_PLACEMENT_3D('',#374345,#116741,#116742);
#99445=AXIS2_PLACEMENT_3D('',#374421,#116744,#116745);
#99446=AXIS2_PLACEMENT_3D('',#374497,#116747,#116748);
#99447=AXIS2_PLACEMENT_3D('',#374573,#116750,#116751);
#99448=AXIS2_PLACEMENT_3D('',#374592,#116753,#116754);
#99449=AXIS2_PLACEMENT_3D('',#374603,#116755,#116756);
#99450=AXIS2_PLACEMENT_3D('',#374635,#116758,#116759);
#99451=AXIS2_PLACEMENT_3D('',#374636,#116760,#116761);
#99452=AXIS2_PLACEMENT_3D('',#374637,#116762,#116763);
#99453=AXIS2_PLACEMENT_3D('',#374654,#116764,#116765);
#99454=AXIS2_PLACEMENT_3D('',#374669,#116766,#116767);
#99455=AXIS2_PLACEMENT_3D('',#374702,#116768,#116769);
#99456=AXIS2_PLACEMENT_3D('',#374771,#116770,#116771);
#99457=AXIS2_PLACEMENT_3D('',#374773,#116772,#116773);
#99458=AXIS2_PLACEMENT_3D('',#374774,#116774,#116775);
#99459=AXIS2_PLACEMENT_3D('',#374775,#116776,#116777);
#99460=AXIS2_PLACEMENT_3D('',#374780,#116779,#116780);
#99461=AXIS2_PLACEMENT_3D('',#374782,#116781,#116782);
#99462=AXIS2_PLACEMENT_3D('',#374784,#116783,#116784);
#99463=AXIS2_PLACEMENT_3D('',#374786,#116785,#116786);
#99464=AXIS2_PLACEMENT_3D('',#374788,#116787,#116788);
#99465=AXIS2_PLACEMENT_3D('',#374789,#116789,#116790);
#99466=AXIS2_PLACEMENT_3D('',#374790,#116791,#116792);
#99467=AXIS2_PLACEMENT_3D('',#374796,#116793,#116794);
#99468=AXIS2_PLACEMENT_3D('',#374797,#116795,#116796);
#99469=AXIS2_PLACEMENT_3D('',#374799,#116797,#116798);
#99470=AXIS2_PLACEMENT_3D('',#374801,#116799,#116800);
#99471=AXIS2_PLACEMENT_3D('',#374802,#116801,#116802);
#99472=AXIS2_PLACEMENT_3D('',#374803,#116803,#116804);
#99473=AXIS2_PLACEMENT_3D('',#374805,#116805,#116806);
#99474=AXIS2_PLACEMENT_3D('',#374807,#116808,#116809);
#99475=AXIS2_PLACEMENT_3D('',#374809,#116810,#116811);
#99476=AXIS2_PLACEMENT_3D('',#374810,#116812,#116813);
#99477=AXIS2_PLACEMENT_3D('',#374811,#116814,#116815);
#99478=AXIS2_PLACEMENT_3D('',#374814,#116816,#116817);
#99479=AXIS2_PLACEMENT_3D('',#374824,#116818,#116819);
#99480=AXIS2_PLACEMENT_3D('',#374834,#116820,#116821);
#99481=AXIS2_PLACEMENT_3D('',#374844,#116822,#116823);
#99482=AXIS2_PLACEMENT_3D('',#374854,#116824,#116825);
#99483=AXIS2_PLACEMENT_3D('',#374864,#116826,#116827);
#99484=AXIS2_PLACEMENT_3D('',#374874,#116828,#116829);
#99485=AXIS2_PLACEMENT_3D('',#374884,#116830,#116831);
#99486=AXIS2_PLACEMENT_3D('',#374894,#116832,#116833);
#99487=AXIS2_PLACEMENT_3D('',#374904,#116834,#116835);
#99488=AXIS2_PLACEMENT_3D('',#374914,#116836,#116837);
#99489=AXIS2_PLACEMENT_3D('',#374924,#116838,#116839);
#99490=AXIS2_PLACEMENT_3D('',#374934,#116840,#116841);
#99491=AXIS2_PLACEMENT_3D('',#374944,#116842,#116843);
#99492=AXIS2_PLACEMENT_3D('',#374954,#116844,#116845);
#99493=AXIS2_PLACEMENT_3D('',#374964,#116846,#116847);
#99494=AXIS2_PLACEMENT_3D('',#374974,#116848,#116849);
#99495=AXIS2_PLACEMENT_3D('',#374984,#116850,#116851);
#99496=AXIS2_PLACEMENT_3D('',#374994,#116852,#116853);
#99497=AXIS2_PLACEMENT_3D('',#375004,#116854,#116855);
#99498=AXIS2_PLACEMENT_3D('',#375014,#116856,#116857);
#99499=AXIS2_PLACEMENT_3D('',#375024,#116858,#116859);
#99500=AXIS2_PLACEMENT_3D('',#375034,#116860,#116861);
#99501=AXIS2_PLACEMENT_3D('',#375044,#116862,#116863);
#99502=AXIS2_PLACEMENT_3D('',#375054,#116864,#116865);
#99503=AXIS2_PLACEMENT_3D('',#375064,#116866,#116867);
#99504=AXIS2_PLACEMENT_3D('',#375074,#116868,#116869);
#99505=AXIS2_PLACEMENT_3D('',#375084,#116870,#116871);
#99506=AXIS2_PLACEMENT_3D('',#375094,#116872,#116873);
#99507=AXIS2_PLACEMENT_3D('',#375104,#116874,#116875);
#99508=AXIS2_PLACEMENT_3D('',#375114,#116876,#116877);
#99509=AXIS2_PLACEMENT_3D('',#375124,#116878,#116879);
#99510=AXIS2_PLACEMENT_3D('',#375134,#116880,#116881);
#99511=AXIS2_PLACEMENT_3D('',#375144,#116882,#116883);
#99512=AXIS2_PLACEMENT_3D('',#375154,#116884,#116885);
#99513=AXIS2_PLACEMENT_3D('',#375164,#116886,#116887);
#99514=AXIS2_PLACEMENT_3D('',#375174,#116888,#116889);
#99515=AXIS2_PLACEMENT_3D('',#375184,#116890,#116891);
#99516=AXIS2_PLACEMENT_3D('',#375194,#116892,#116893);
#99517=AXIS2_PLACEMENT_3D('',#375204,#116894,#116895);
#99518=AXIS2_PLACEMENT_3D('',#375214,#116896,#116897);
#99519=AXIS2_PLACEMENT_3D('',#375224,#116898,#116899);
#99520=AXIS2_PLACEMENT_3D('',#375234,#116900,#116901);
#99521=AXIS2_PLACEMENT_3D('',#375244,#116902,#116903);
#99522=AXIS2_PLACEMENT_3D('',#375254,#116904,#116905);
#99523=AXIS2_PLACEMENT_3D('',#375264,#116906,#116907);
#99524=AXIS2_PLACEMENT_3D('',#375274,#116908,#116909);
#99525=AXIS2_PLACEMENT_3D('',#375284,#116910,#116911);
#99526=AXIS2_PLACEMENT_3D('',#375294,#116912,#116913);
#99527=AXIS2_PLACEMENT_3D('',#375304,#116914,#116915);
#99528=AXIS2_PLACEMENT_3D('',#375314,#116916,#116917);
#99529=AXIS2_PLACEMENT_3D('',#375324,#116918,#116919);
#99530=AXIS2_PLACEMENT_3D('',#375334,#116920,#116921);
#99531=AXIS2_PLACEMENT_3D('',#375344,#116922,#116923);
#99532=AXIS2_PLACEMENT_3D('',#375354,#116924,#116925);
#99533=AXIS2_PLACEMENT_3D('',#375364,#116926,#116927);
#99534=AXIS2_PLACEMENT_3D('',#375374,#116928,#116929);
#99535=AXIS2_PLACEMENT_3D('',#375384,#116930,#116931);
#99536=AXIS2_PLACEMENT_3D('',#375394,#116932,#116933);
#99537=AXIS2_PLACEMENT_3D('',#375404,#116934,#116935);
#99538=AXIS2_PLACEMENT_3D('',#375414,#116936,#116937);
#99539=AXIS2_PLACEMENT_3D('',#375424,#116938,#116939);
#99540=AXIS2_PLACEMENT_3D('',#375434,#116940,#116941);
#99541=AXIS2_PLACEMENT_3D('',#375444,#116942,#116943);
#99542=AXIS2_PLACEMENT_3D('',#375454,#116944,#116945);
#99543=AXIS2_PLACEMENT_3D('',#375464,#116946,#116947);
#99544=AXIS2_PLACEMENT_3D('',#375474,#116948,#116949);
#99545=AXIS2_PLACEMENT_3D('',#375484,#116950,#116951);
#99546=AXIS2_PLACEMENT_3D('',#375494,#116952,#116953);
#99547=AXIS2_PLACEMENT_3D('',#375504,#116954,#116955);
#99548=AXIS2_PLACEMENT_3D('',#375514,#116956,#116957);
#99549=AXIS2_PLACEMENT_3D('',#375524,#116958,#116959);
#99550=AXIS2_PLACEMENT_3D('',#375534,#116960,#116961);
#99551=AXIS2_PLACEMENT_3D('',#375544,#116962,#116963);
#99552=AXIS2_PLACEMENT_3D('',#375554,#116964,#116965);
#99553=AXIS2_PLACEMENT_3D('',#375564,#116966,#116967);
#99554=AXIS2_PLACEMENT_3D('',#375574,#116968,#116969);
#99555=AXIS2_PLACEMENT_3D('',#375584,#116970,#116971);
#99556=AXIS2_PLACEMENT_3D('',#375594,#116972,#116973);
#99557=AXIS2_PLACEMENT_3D('',#375604,#116974,#116975);
#99558=AXIS2_PLACEMENT_3D('',#375614,#116976,#116977);
#99559=AXIS2_PLACEMENT_3D('',#375624,#116978,#116979);
#99560=AXIS2_PLACEMENT_3D('',#375634,#116980,#116981);
#99561=AXIS2_PLACEMENT_3D('',#375644,#116982,#116983);
#99562=AXIS2_PLACEMENT_3D('',#375654,#116984,#116985);
#99563=AXIS2_PLACEMENT_3D('',#375664,#116986,#116987);
#99564=AXIS2_PLACEMENT_3D('',#375674,#116988,#116989);
#99565=AXIS2_PLACEMENT_3D('',#375684,#116990,#116991);
#99566=AXIS2_PLACEMENT_3D('',#375694,#116992,#116993);
#99567=AXIS2_PLACEMENT_3D('',#375704,#116994,#116995);
#99568=AXIS2_PLACEMENT_3D('',#375714,#116996,#116997);
#99569=AXIS2_PLACEMENT_3D('',#375724,#116998,#116999);
#99570=AXIS2_PLACEMENT_3D('',#375734,#117000,#117001);
#99571=AXIS2_PLACEMENT_3D('',#375744,#117002,#117003);
#99572=AXIS2_PLACEMENT_3D('',#375754,#117004,#117005);
#99573=AXIS2_PLACEMENT_3D('',#375764,#117006,#117007);
#99574=AXIS2_PLACEMENT_3D('',#375774,#117008,#117009);
#99575=AXIS2_PLACEMENT_3D('',#375784,#117010,#117011);
#99576=AXIS2_PLACEMENT_3D('',#375794,#117012,#117013);
#99577=AXIS2_PLACEMENT_3D('',#375798,#117015,#117016);
#99578=AXIS2_PLACEMENT_3D('',#375799,#117017,#117018);
#99579=AXIS2_PLACEMENT_3D('',#375801,#117019,#117020);
#99580=AXIS2_PLACEMENT_3D('',#375811,#117021,#117022);
#99581=AXIS2_PLACEMENT_3D('',#375821,#117023,#117024);
#99582=AXIS2_PLACEMENT_3D('',#375831,#117025,#117026);
#99583=AXIS2_PLACEMENT_3D('',#375841,#117027,#117028);
#99584=AXIS2_PLACEMENT_3D('',#375851,#117029,#117030);
#99585=AXIS2_PLACEMENT_3D('',#375861,#117031,#117032);
#99586=AXIS2_PLACEMENT_3D('',#375871,#117033,#117034);
#99587=AXIS2_PLACEMENT_3D('',#375881,#117035,#117036);
#99588=AXIS2_PLACEMENT_3D('',#375891,#117037,#117038);
#99589=AXIS2_PLACEMENT_3D('',#375901,#117039,#117040);
#99590=AXIS2_PLACEMENT_3D('',#375911,#117041,#117042);
#99591=AXIS2_PLACEMENT_3D('',#375921,#117043,#117044);
#99592=AXIS2_PLACEMENT_3D('',#375931,#117045,#117046);
#99593=AXIS2_PLACEMENT_3D('',#375941,#117047,#117048);
#99594=AXIS2_PLACEMENT_3D('',#375951,#117049,#117050);
#99595=AXIS2_PLACEMENT_3D('',#375961,#117051,#117052);
#99596=AXIS2_PLACEMENT_3D('',#375971,#117053,#117054);
#99597=AXIS2_PLACEMENT_3D('',#375981,#117055,#117056);
#99598=AXIS2_PLACEMENT_3D('',#375991,#117057,#117058);
#99599=AXIS2_PLACEMENT_3D('',#376001,#117059,#117060);
#99600=AXIS2_PLACEMENT_3D('',#376011,#117061,#117062);
#99601=AXIS2_PLACEMENT_3D('',#376021,#117063,#117064);
#99602=AXIS2_PLACEMENT_3D('',#376031,#117065,#117066);
#99603=AXIS2_PLACEMENT_3D('',#376041,#117067,#117068);
#99604=AXIS2_PLACEMENT_3D('',#376051,#117069,#117070);
#99605=AXIS2_PLACEMENT_3D('',#376061,#117071,#117072);
#99606=AXIS2_PLACEMENT_3D('',#376071,#117073,#117074);
#99607=AXIS2_PLACEMENT_3D('',#376081,#117075,#117076);
#99608=AXIS2_PLACEMENT_3D('',#376091,#117077,#117078);
#99609=AXIS2_PLACEMENT_3D('',#376101,#117079,#117080);
#99610=AXIS2_PLACEMENT_3D('',#376111,#117081,#117082);
#99611=AXIS2_PLACEMENT_3D('',#376121,#117083,#117084);
#99612=AXIS2_PLACEMENT_3D('',#376131,#117085,#117086);
#99613=AXIS2_PLACEMENT_3D('',#376141,#117087,#117088);
#99614=AXIS2_PLACEMENT_3D('',#376151,#117089,#117090);
#99615=AXIS2_PLACEMENT_3D('',#376161,#117091,#117092);
#99616=AXIS2_PLACEMENT_3D('',#376171,#117093,#117094);
#99617=AXIS2_PLACEMENT_3D('',#376181,#117095,#117096);
#99618=AXIS2_PLACEMENT_3D('',#376191,#117097,#117098);
#99619=AXIS2_PLACEMENT_3D('',#376201,#117099,#117100);
#99620=AXIS2_PLACEMENT_3D('',#376211,#117101,#117102);
#99621=AXIS2_PLACEMENT_3D('',#376221,#117103,#117104);
#99622=AXIS2_PLACEMENT_3D('',#376231,#117105,#117106);
#99623=AXIS2_PLACEMENT_3D('',#376241,#117107,#117108);
#99624=AXIS2_PLACEMENT_3D('',#376251,#117109,#117110);
#99625=AXIS2_PLACEMENT_3D('',#376261,#117111,#117112);
#99626=AXIS2_PLACEMENT_3D('',#376271,#117113,#117114);
#99627=AXIS2_PLACEMENT_3D('',#376281,#117115,#117116);
#99628=AXIS2_PLACEMENT_3D('',#376291,#117117,#117118);
#99629=AXIS2_PLACEMENT_3D('',#376301,#117119,#117120);
#99630=AXIS2_PLACEMENT_3D('',#376311,#117121,#117122);
#99631=AXIS2_PLACEMENT_3D('',#376321,#117123,#117124);
#99632=AXIS2_PLACEMENT_3D('',#376331,#117125,#117126);
#99633=AXIS2_PLACEMENT_3D('',#376341,#117127,#117128);
#99634=AXIS2_PLACEMENT_3D('',#376351,#117129,#117130);
#99635=AXIS2_PLACEMENT_3D('',#376361,#117131,#117132);
#99636=AXIS2_PLACEMENT_3D('',#376371,#117133,#117134);
#99637=AXIS2_PLACEMENT_3D('',#376381,#117135,#117136);
#99638=AXIS2_PLACEMENT_3D('',#376391,#117137,#117138);
#99639=AXIS2_PLACEMENT_3D('',#376401,#117139,#117140);
#99640=AXIS2_PLACEMENT_3D('',#376411,#117141,#117142);
#99641=AXIS2_PLACEMENT_3D('',#376421,#117143,#117144);
#99642=AXIS2_PLACEMENT_3D('',#376431,#117145,#117146);
#99643=AXIS2_PLACEMENT_3D('',#376441,#117147,#117148);
#99644=AXIS2_PLACEMENT_3D('',#376451,#117149,#117150);
#99645=AXIS2_PLACEMENT_3D('',#376461,#117151,#117152);
#99646=AXIS2_PLACEMENT_3D('',#376471,#117153,#117154);
#99647=AXIS2_PLACEMENT_3D('',#376481,#117155,#117156);
#99648=AXIS2_PLACEMENT_3D('',#376491,#117157,#117158);
#99649=AXIS2_PLACEMENT_3D('',#376501,#117159,#117160);
#99650=AXIS2_PLACEMENT_3D('',#376511,#117161,#117162);
#99651=AXIS2_PLACEMENT_3D('',#376521,#117163,#117164);
#99652=AXIS2_PLACEMENT_3D('',#376531,#117165,#117166);
#99653=AXIS2_PLACEMENT_3D('',#376541,#117167,#117168);
#99654=AXIS2_PLACEMENT_3D('',#376551,#117169,#117170);
#99655=AXIS2_PLACEMENT_3D('',#376561,#117171,#117172);
#99656=AXIS2_PLACEMENT_3D('',#376571,#117173,#117174);
#99657=AXIS2_PLACEMENT_3D('',#376581,#117175,#117176);
#99658=AXIS2_PLACEMENT_3D('',#376591,#117177,#117178);
#99659=AXIS2_PLACEMENT_3D('',#376601,#117179,#117180);
#99660=AXIS2_PLACEMENT_3D('',#376611,#117181,#117182);
#99661=AXIS2_PLACEMENT_3D('',#376621,#117183,#117184);
#99662=AXIS2_PLACEMENT_3D('',#376631,#117185,#117186);
#99663=AXIS2_PLACEMENT_3D('',#376641,#117187,#117188);
#99664=AXIS2_PLACEMENT_3D('',#376651,#117189,#117190);
#99665=AXIS2_PLACEMENT_3D('',#376661,#117191,#117192);
#99666=AXIS2_PLACEMENT_3D('',#376671,#117193,#117194);
#99667=AXIS2_PLACEMENT_3D('',#376681,#117195,#117196);
#99668=AXIS2_PLACEMENT_3D('',#376691,#117197,#117198);
#99669=AXIS2_PLACEMENT_3D('',#376701,#117199,#117200);
#99670=AXIS2_PLACEMENT_3D('',#376711,#117201,#117202);
#99671=AXIS2_PLACEMENT_3D('',#376721,#117203,#117204);
#99672=AXIS2_PLACEMENT_3D('',#376731,#117205,#117206);
#99673=AXIS2_PLACEMENT_3D('',#376741,#117207,#117208);
#99674=AXIS2_PLACEMENT_3D('',#376751,#117209,#117210);
#99675=AXIS2_PLACEMENT_3D('',#376761,#117211,#117212);
#99676=AXIS2_PLACEMENT_3D('',#376771,#117213,#117214);
#99677=AXIS2_PLACEMENT_3D('',#376779,#117215,#117216);
#99678=AXIS2_PLACEMENT_3D('',#376781,#117217,#117218);
#99679=AXIS2_PLACEMENT_3D('',#376782,#117219,#117220);
#99680=AXIS2_PLACEMENT_3D('',#376783,#117221,#117222);
#99681=AXIS2_PLACEMENT_3D('',#376786,#117223,#117224);
#99682=AXIS2_PLACEMENT_3D('',#376790,#117226,#117227);
#99683=AXIS2_PLACEMENT_3D('',#376792,#117228,#117229);
#99684=AXIS2_PLACEMENT_3D('',#376794,#117230,#117231);
#99685=AXIS2_PLACEMENT_3D('',#376798,#117233,#117234);
#99686=AXIS2_PLACEMENT_3D('',#376802,#117236,#117237);
#99687=AXIS2_PLACEMENT_3D('',#376804,#117238,#117239);
#99688=AXIS2_PLACEMENT_3D('',#376806,#117240,#117241);
#99689=AXIS2_PLACEMENT_3D('',#376810,#117243,#117244);
#99690=AXIS2_PLACEMENT_3D('',#376814,#117246,#117247);
#99691=AXIS2_PLACEMENT_3D('',#376816,#117248,#117249);
#99692=AXIS2_PLACEMENT_3D('',#376818,#117250,#117251);
#99693=AXIS2_PLACEMENT_3D('',#376822,#117253,#117254);
#99694=AXIS2_PLACEMENT_3D('',#376826,#117256,#117257);
#99695=AXIS2_PLACEMENT_3D('',#376828,#117258,#117259);
#99696=AXIS2_PLACEMENT_3D('',#376830,#117260,#117261);
#99697=AXIS2_PLACEMENT_3D('',#376834,#117263,#117264);
#99698=AXIS2_PLACEMENT_3D('',#376838,#117266,#117267);
#99699=AXIS2_PLACEMENT_3D('',#376840,#117268,#117269);
#99700=AXIS2_PLACEMENT_3D('',#376842,#117270,#117271);
#99701=AXIS2_PLACEMENT_3D('',#376846,#117273,#117274);
#99702=AXIS2_PLACEMENT_3D('',#376850,#117276,#117277);
#99703=AXIS2_PLACEMENT_3D('',#376852,#117278,#117279);
#99704=AXIS2_PLACEMENT_3D('',#376854,#117280,#117281);
#99705=AXIS2_PLACEMENT_3D('',#376858,#117283,#117284);
#99706=AXIS2_PLACEMENT_3D('',#376862,#117286,#117287);
#99707=AXIS2_PLACEMENT_3D('',#376864,#117288,#117289);
#99708=AXIS2_PLACEMENT_3D('',#376866,#117290,#117291);
#99709=AXIS2_PLACEMENT_3D('',#376870,#117293,#117294);
#99710=AXIS2_PLACEMENT_3D('',#376874,#117296,#117297);
#99711=AXIS2_PLACEMENT_3D('',#376876,#117298,#117299);
#99712=AXIS2_PLACEMENT_3D('',#376878,#117300,#117301);
#99713=AXIS2_PLACEMENT_3D('',#376882,#117303,#117304);
#99714=AXIS2_PLACEMENT_3D('',#376886,#117306,#117307);
#99715=AXIS2_PLACEMENT_3D('',#376888,#117308,#117309);
#99716=AXIS2_PLACEMENT_3D('',#376890,#117310,#117311);
#99717=AXIS2_PLACEMENT_3D('',#376894,#117313,#117314);
#99718=AXIS2_PLACEMENT_3D('',#376898,#117316,#117317);
#99719=AXIS2_PLACEMENT_3D('',#376900,#117318,#117319);
#99720=AXIS2_PLACEMENT_3D('',#376902,#117320,#117321);
#99721=AXIS2_PLACEMENT_3D('',#376906,#117323,#117324);
#99722=AXIS2_PLACEMENT_3D('',#376910,#117326,#117327);
#99723=AXIS2_PLACEMENT_3D('',#376912,#117328,#117329);
#99724=AXIS2_PLACEMENT_3D('',#376914,#117330,#117331);
#99725=AXIS2_PLACEMENT_3D('',#376918,#117333,#117334);
#99726=AXIS2_PLACEMENT_3D('',#376922,#117336,#117337);
#99727=AXIS2_PLACEMENT_3D('',#376924,#117338,#117339);
#99728=AXIS2_PLACEMENT_3D('',#376926,#117340,#117341);
#99729=AXIS2_PLACEMENT_3D('',#376930,#117343,#117344);
#99730=AXIS2_PLACEMENT_3D('',#376934,#117346,#117347);
#99731=AXIS2_PLACEMENT_3D('',#376936,#117348,#117349);
#99732=AXIS2_PLACEMENT_3D('',#376938,#117350,#117351);
#99733=AXIS2_PLACEMENT_3D('',#376942,#117353,#117354);
#99734=AXIS2_PLACEMENT_3D('',#376946,#117356,#117357);
#99735=AXIS2_PLACEMENT_3D('',#376948,#117358,#117359);
#99736=AXIS2_PLACEMENT_3D('',#376950,#117360,#117361);
#99737=AXIS2_PLACEMENT_3D('',#376954,#117363,#117364);
#99738=AXIS2_PLACEMENT_3D('',#376958,#117366,#117367);
#99739=AXIS2_PLACEMENT_3D('',#376960,#117368,#117369);
#99740=AXIS2_PLACEMENT_3D('',#376962,#117370,#117371);
#99741=AXIS2_PLACEMENT_3D('',#376966,#117373,#117374);
#99742=AXIS2_PLACEMENT_3D('',#376970,#117376,#117377);
#99743=AXIS2_PLACEMENT_3D('',#376972,#117378,#117379);
#99744=AXIS2_PLACEMENT_3D('',#376974,#117380,#117381);
#99745=AXIS2_PLACEMENT_3D('',#376978,#117383,#117384);
#99746=AXIS2_PLACEMENT_3D('',#376982,#117386,#117387);
#99747=AXIS2_PLACEMENT_3D('',#376984,#117388,#117389);
#99748=AXIS2_PLACEMENT_3D('',#376986,#117390,#117391);
#99749=AXIS2_PLACEMENT_3D('',#376990,#117393,#117394);
#99750=AXIS2_PLACEMENT_3D('',#376994,#117396,#117397);
#99751=AXIS2_PLACEMENT_3D('',#376996,#117398,#117399);
#99752=AXIS2_PLACEMENT_3D('',#376998,#117400,#117401);
#99753=AXIS2_PLACEMENT_3D('',#377002,#117403,#117404);
#99754=AXIS2_PLACEMENT_3D('',#377006,#117406,#117407);
#99755=AXIS2_PLACEMENT_3D('',#377008,#117408,#117409);
#99756=AXIS2_PLACEMENT_3D('',#377010,#117410,#117411);
#99757=AXIS2_PLACEMENT_3D('',#377014,#117413,#117414);
#99758=AXIS2_PLACEMENT_3D('',#377018,#117416,#117417);
#99759=AXIS2_PLACEMENT_3D('',#377020,#117418,#117419);
#99760=AXIS2_PLACEMENT_3D('',#377022,#117420,#117421);
#99761=AXIS2_PLACEMENT_3D('',#377026,#117423,#117424);
#99762=AXIS2_PLACEMENT_3D('',#377030,#117426,#117427);
#99763=AXIS2_PLACEMENT_3D('',#377032,#117428,#117429);
#99764=AXIS2_PLACEMENT_3D('',#377034,#117430,#117431);
#99765=AXIS2_PLACEMENT_3D('',#377038,#117433,#117434);
#99766=AXIS2_PLACEMENT_3D('',#377042,#117436,#117437);
#99767=AXIS2_PLACEMENT_3D('',#377044,#117438,#117439);
#99768=AXIS2_PLACEMENT_3D('',#377046,#117440,#117441);
#99769=AXIS2_PLACEMENT_3D('',#377050,#117443,#117444);
#99770=AXIS2_PLACEMENT_3D('',#377054,#117446,#117447);
#99771=AXIS2_PLACEMENT_3D('',#377056,#117448,#117449);
#99772=AXIS2_PLACEMENT_3D('',#377058,#117450,#117451);
#99773=AXIS2_PLACEMENT_3D('',#377062,#117453,#117454);
#99774=AXIS2_PLACEMENT_3D('',#377066,#117456,#117457);
#99775=AXIS2_PLACEMENT_3D('',#377068,#117458,#117459);
#99776=AXIS2_PLACEMENT_3D('',#377070,#117460,#117461);
#99777=AXIS2_PLACEMENT_3D('',#377074,#117463,#117464);
#99778=AXIS2_PLACEMENT_3D('',#377078,#117466,#117467);
#99779=AXIS2_PLACEMENT_3D('',#377080,#117468,#117469);
#99780=AXIS2_PLACEMENT_3D('',#377082,#117470,#117471);
#99781=AXIS2_PLACEMENT_3D('',#377086,#117473,#117474);
#99782=AXIS2_PLACEMENT_3D('',#377090,#117476,#117477);
#99783=AXIS2_PLACEMENT_3D('',#377092,#117478,#117479);
#99784=AXIS2_PLACEMENT_3D('',#377094,#117480,#117481);
#99785=AXIS2_PLACEMENT_3D('',#377098,#117483,#117484);
#99786=AXIS2_PLACEMENT_3D('',#377102,#117486,#117487);
#99787=AXIS2_PLACEMENT_3D('',#377104,#117488,#117489);
#99788=AXIS2_PLACEMENT_3D('',#377106,#117490,#117491);
#99789=AXIS2_PLACEMENT_3D('',#377110,#117493,#117494);
#99790=AXIS2_PLACEMENT_3D('',#377114,#117496,#117497);
#99791=AXIS2_PLACEMENT_3D('',#377116,#117498,#117499);
#99792=AXIS2_PLACEMENT_3D('',#377118,#117500,#117501);
#99793=AXIS2_PLACEMENT_3D('',#377122,#117503,#117504);
#99794=AXIS2_PLACEMENT_3D('',#377126,#117506,#117507);
#99795=AXIS2_PLACEMENT_3D('',#377128,#117508,#117509);
#99796=AXIS2_PLACEMENT_3D('',#377130,#117510,#117511);
#99797=AXIS2_PLACEMENT_3D('',#377134,#117513,#117514);
#99798=AXIS2_PLACEMENT_3D('',#377138,#117516,#117517);
#99799=AXIS2_PLACEMENT_3D('',#377140,#117518,#117519);
#99800=AXIS2_PLACEMENT_3D('',#377142,#117520,#117521);
#99801=AXIS2_PLACEMENT_3D('',#377146,#117523,#117524);
#99802=AXIS2_PLACEMENT_3D('',#377150,#117526,#117527);
#99803=AXIS2_PLACEMENT_3D('',#377152,#117528,#117529);
#99804=AXIS2_PLACEMENT_3D('',#377154,#117530,#117531);
#99805=AXIS2_PLACEMENT_3D('',#377158,#117533,#117534);
#99806=AXIS2_PLACEMENT_3D('',#377162,#117536,#117537);
#99807=AXIS2_PLACEMENT_3D('',#377164,#117538,#117539);
#99808=AXIS2_PLACEMENT_3D('',#377166,#117540,#117541);
#99809=AXIS2_PLACEMENT_3D('',#377170,#117543,#117544);
#99810=AXIS2_PLACEMENT_3D('',#377174,#117546,#117547);
#99811=AXIS2_PLACEMENT_3D('',#377176,#117548,#117549);
#99812=AXIS2_PLACEMENT_3D('',#377178,#117550,#117551);
#99813=AXIS2_PLACEMENT_3D('',#377182,#117553,#117554);
#99814=AXIS2_PLACEMENT_3D('',#377186,#117556,#117557);
#99815=AXIS2_PLACEMENT_3D('',#377188,#117558,#117559);
#99816=AXIS2_PLACEMENT_3D('',#377190,#117560,#117561);
#99817=AXIS2_PLACEMENT_3D('',#377194,#117563,#117564);
#99818=AXIS2_PLACEMENT_3D('',#377198,#117566,#117567);
#99819=AXIS2_PLACEMENT_3D('',#377200,#117568,#117569);
#99820=AXIS2_PLACEMENT_3D('',#377202,#117570,#117571);
#99821=AXIS2_PLACEMENT_3D('',#377206,#117573,#117574);
#99822=AXIS2_PLACEMENT_3D('',#377210,#117576,#117577);
#99823=AXIS2_PLACEMENT_3D('',#377212,#117578,#117579);
#99824=AXIS2_PLACEMENT_3D('',#377214,#117580,#117581);
#99825=AXIS2_PLACEMENT_3D('',#377218,#117583,#117584);
#99826=AXIS2_PLACEMENT_3D('',#377222,#117586,#117587);
#99827=AXIS2_PLACEMENT_3D('',#377224,#117588,#117589);
#99828=AXIS2_PLACEMENT_3D('',#377226,#117590,#117591);
#99829=AXIS2_PLACEMENT_3D('',#377230,#117593,#117594);
#99830=AXIS2_PLACEMENT_3D('',#377234,#117596,#117597);
#99831=AXIS2_PLACEMENT_3D('',#377236,#117598,#117599);
#99832=AXIS2_PLACEMENT_3D('',#377238,#117600,#117601);
#99833=AXIS2_PLACEMENT_3D('',#377242,#117603,#117604);
#99834=AXIS2_PLACEMENT_3D('',#377246,#117606,#117607);
#99835=AXIS2_PLACEMENT_3D('',#377248,#117608,#117609);
#99836=AXIS2_PLACEMENT_3D('',#377250,#117610,#117611);
#99837=AXIS2_PLACEMENT_3D('',#377254,#117613,#117614);
#99838=AXIS2_PLACEMENT_3D('',#377258,#117616,#117617);
#99839=AXIS2_PLACEMENT_3D('',#377260,#117618,#117619);
#99840=AXIS2_PLACEMENT_3D('',#377262,#117620,#117621);
#99841=AXIS2_PLACEMENT_3D('',#377266,#117623,#117624);
#99842=AXIS2_PLACEMENT_3D('',#377270,#117626,#117627);
#99843=AXIS2_PLACEMENT_3D('',#377272,#117628,#117629);
#99844=AXIS2_PLACEMENT_3D('',#377274,#117630,#117631);
#99845=AXIS2_PLACEMENT_3D('',#377278,#117633,#117634);
#99846=AXIS2_PLACEMENT_3D('',#377282,#117636,#117637);
#99847=AXIS2_PLACEMENT_3D('',#377284,#117638,#117639);
#99848=AXIS2_PLACEMENT_3D('',#377286,#117640,#117641);
#99849=AXIS2_PLACEMENT_3D('',#377290,#117643,#117644);
#99850=AXIS2_PLACEMENT_3D('',#377294,#117646,#117647);
#99851=AXIS2_PLACEMENT_3D('',#377296,#117648,#117649);
#99852=AXIS2_PLACEMENT_3D('',#377298,#117650,#117651);
#99853=AXIS2_PLACEMENT_3D('',#377302,#117653,#117654);
#99854=AXIS2_PLACEMENT_3D('',#377306,#117656,#117657);
#99855=AXIS2_PLACEMENT_3D('',#377308,#117658,#117659);
#99856=AXIS2_PLACEMENT_3D('',#377310,#117660,#117661);
#99857=AXIS2_PLACEMENT_3D('',#377314,#117663,#117664);
#99858=AXIS2_PLACEMENT_3D('',#377318,#117666,#117667);
#99859=AXIS2_PLACEMENT_3D('',#377320,#117668,#117669);
#99860=AXIS2_PLACEMENT_3D('',#377322,#117670,#117671);
#99861=AXIS2_PLACEMENT_3D('',#377326,#117673,#117674);
#99862=AXIS2_PLACEMENT_3D('',#377330,#117676,#117677);
#99863=AXIS2_PLACEMENT_3D('',#377332,#117678,#117679);
#99864=AXIS2_PLACEMENT_3D('',#377334,#117680,#117681);
#99865=AXIS2_PLACEMENT_3D('',#377338,#117683,#117684);
#99866=AXIS2_PLACEMENT_3D('',#377342,#117686,#117687);
#99867=AXIS2_PLACEMENT_3D('',#377344,#117688,#117689);
#99868=AXIS2_PLACEMENT_3D('',#377346,#117690,#117691);
#99869=AXIS2_PLACEMENT_3D('',#377350,#117693,#117694);
#99870=AXIS2_PLACEMENT_3D('',#377354,#117696,#117697);
#99871=AXIS2_PLACEMENT_3D('',#377356,#117698,#117699);
#99872=AXIS2_PLACEMENT_3D('',#377358,#117700,#117701);
#99873=AXIS2_PLACEMENT_3D('',#377362,#117703,#117704);
#99874=AXIS2_PLACEMENT_3D('',#377366,#117706,#117707);
#99875=AXIS2_PLACEMENT_3D('',#377368,#117708,#117709);
#99876=AXIS2_PLACEMENT_3D('',#377370,#117710,#117711);
#99877=AXIS2_PLACEMENT_3D('',#377374,#117713,#117714);
#99878=AXIS2_PLACEMENT_3D('',#377377,#117716,#117717);
#99879=AXIS2_PLACEMENT_3D('',#377381,#117719,#117720);
#99880=AXIS2_PLACEMENT_3D('',#377383,#117721,#117722);
#99881=AXIS2_PLACEMENT_3D('',#377385,#117723,#117724);
#99882=AXIS2_PLACEMENT_3D('',#377389,#117726,#117727);
#99883=AXIS2_PLACEMENT_3D('',#377393,#117729,#117730);
#99884=AXIS2_PLACEMENT_3D('',#377395,#117731,#117732);
#99885=AXIS2_PLACEMENT_3D('',#377397,#117733,#117734);
#99886=AXIS2_PLACEMENT_3D('',#377401,#117736,#117737);
#99887=AXIS2_PLACEMENT_3D('',#377405,#117739,#117740);
#99888=AXIS2_PLACEMENT_3D('',#377407,#117741,#117742);
#99889=AXIS2_PLACEMENT_3D('',#377409,#117743,#117744);
#99890=AXIS2_PLACEMENT_3D('',#377413,#117746,#117747);
#99891=AXIS2_PLACEMENT_3D('',#377417,#117749,#117750);
#99892=AXIS2_PLACEMENT_3D('',#377419,#117751,#117752);
#99893=AXIS2_PLACEMENT_3D('',#377421,#117753,#117754);
#99894=AXIS2_PLACEMENT_3D('',#377425,#117756,#117757);
#99895=AXIS2_PLACEMENT_3D('',#377429,#117759,#117760);
#99896=AXIS2_PLACEMENT_3D('',#377431,#117761,#117762);
#99897=AXIS2_PLACEMENT_3D('',#377433,#117763,#117764);
#99898=AXIS2_PLACEMENT_3D('',#377437,#117766,#117767);
#99899=AXIS2_PLACEMENT_3D('',#377441,#117769,#117770);
#99900=AXIS2_PLACEMENT_3D('',#377443,#117771,#117772);
#99901=AXIS2_PLACEMENT_3D('',#377445,#117773,#117774);
#99902=AXIS2_PLACEMENT_3D('',#377449,#117776,#117777);
#99903=AXIS2_PLACEMENT_3D('',#377453,#117779,#117780);
#99904=AXIS2_PLACEMENT_3D('',#377455,#117781,#117782);
#99905=AXIS2_PLACEMENT_3D('',#377457,#117783,#117784);
#99906=AXIS2_PLACEMENT_3D('',#377461,#117786,#117787);
#99907=AXIS2_PLACEMENT_3D('',#377465,#117789,#117790);
#99908=AXIS2_PLACEMENT_3D('',#377467,#117791,#117792);
#99909=AXIS2_PLACEMENT_3D('',#377469,#117793,#117794);
#99910=AXIS2_PLACEMENT_3D('',#377473,#117796,#117797);
#99911=AXIS2_PLACEMENT_3D('',#377477,#117799,#117800);
#99912=AXIS2_PLACEMENT_3D('',#377479,#117801,#117802);
#99913=AXIS2_PLACEMENT_3D('',#377481,#117803,#117804);
#99914=AXIS2_PLACEMENT_3D('',#377485,#117806,#117807);
#99915=AXIS2_PLACEMENT_3D('',#377489,#117809,#117810);
#99916=AXIS2_PLACEMENT_3D('',#377491,#117811,#117812);
#99917=AXIS2_PLACEMENT_3D('',#377493,#117813,#117814);
#99918=AXIS2_PLACEMENT_3D('',#377497,#117816,#117817);
#99919=AXIS2_PLACEMENT_3D('',#377501,#117819,#117820);
#99920=AXIS2_PLACEMENT_3D('',#377503,#117821,#117822);
#99921=AXIS2_PLACEMENT_3D('',#377505,#117823,#117824);
#99922=AXIS2_PLACEMENT_3D('',#377509,#117826,#117827);
#99923=AXIS2_PLACEMENT_3D('',#377513,#117829,#117830);
#99924=AXIS2_PLACEMENT_3D('',#377515,#117831,#117832);
#99925=AXIS2_PLACEMENT_3D('',#377517,#117833,#117834);
#99926=AXIS2_PLACEMENT_3D('',#377521,#117836,#117837);
#99927=AXIS2_PLACEMENT_3D('',#377525,#117839,#117840);
#99928=AXIS2_PLACEMENT_3D('',#377527,#117841,#117842);
#99929=AXIS2_PLACEMENT_3D('',#377529,#117843,#117844);
#99930=AXIS2_PLACEMENT_3D('',#377533,#117846,#117847);
#99931=AXIS2_PLACEMENT_3D('',#377537,#117849,#117850);
#99932=AXIS2_PLACEMENT_3D('',#377539,#117851,#117852);
#99933=AXIS2_PLACEMENT_3D('',#377541,#117853,#117854);
#99934=AXIS2_PLACEMENT_3D('',#377545,#117856,#117857);
#99935=AXIS2_PLACEMENT_3D('',#377549,#117859,#117860);
#99936=AXIS2_PLACEMENT_3D('',#377551,#117861,#117862);
#99937=AXIS2_PLACEMENT_3D('',#377553,#117863,#117864);
#99938=AXIS2_PLACEMENT_3D('',#377557,#117866,#117867);
#99939=AXIS2_PLACEMENT_3D('',#377561,#117869,#117870);
#99940=AXIS2_PLACEMENT_3D('',#377563,#117871,#117872);
#99941=AXIS2_PLACEMENT_3D('',#377565,#117873,#117874);
#99942=AXIS2_PLACEMENT_3D('',#377569,#117876,#117877);
#99943=AXIS2_PLACEMENT_3D('',#377573,#117879,#117880);
#99944=AXIS2_PLACEMENT_3D('',#377575,#117881,#117882);
#99945=AXIS2_PLACEMENT_3D('',#377577,#117883,#117884);
#99946=AXIS2_PLACEMENT_3D('',#377581,#117886,#117887);
#99947=AXIS2_PLACEMENT_3D('',#377585,#117889,#117890);
#99948=AXIS2_PLACEMENT_3D('',#377587,#117891,#117892);
#99949=AXIS2_PLACEMENT_3D('',#377589,#117893,#117894);
#99950=AXIS2_PLACEMENT_3D('',#377593,#117896,#117897);
#99951=AXIS2_PLACEMENT_3D('',#377597,#117899,#117900);
#99952=AXIS2_PLACEMENT_3D('',#377599,#117901,#117902);
#99953=AXIS2_PLACEMENT_3D('',#377601,#117903,#117904);
#99954=AXIS2_PLACEMENT_3D('',#377605,#117906,#117907);
#99955=AXIS2_PLACEMENT_3D('',#377609,#117909,#117910);
#99956=AXIS2_PLACEMENT_3D('',#377611,#117911,#117912);
#99957=AXIS2_PLACEMENT_3D('',#377613,#117913,#117914);
#99958=AXIS2_PLACEMENT_3D('',#377617,#117916,#117917);
#99959=AXIS2_PLACEMENT_3D('',#377621,#117919,#117920);
#99960=AXIS2_PLACEMENT_3D('',#377623,#117921,#117922);
#99961=AXIS2_PLACEMENT_3D('',#377625,#117923,#117924);
#99962=AXIS2_PLACEMENT_3D('',#377629,#117926,#117927);
#99963=AXIS2_PLACEMENT_3D('',#377633,#117929,#117930);
#99964=AXIS2_PLACEMENT_3D('',#377635,#117931,#117932);
#99965=AXIS2_PLACEMENT_3D('',#377637,#117933,#117934);
#99966=AXIS2_PLACEMENT_3D('',#377641,#117936,#117937);
#99967=AXIS2_PLACEMENT_3D('',#377645,#117939,#117940);
#99968=AXIS2_PLACEMENT_3D('',#377647,#117941,#117942);
#99969=AXIS2_PLACEMENT_3D('',#377649,#117943,#117944);
#99970=AXIS2_PLACEMENT_3D('',#377653,#117946,#117947);
#99971=AXIS2_PLACEMENT_3D('',#377657,#117949,#117950);
#99972=AXIS2_PLACEMENT_3D('',#377659,#117951,#117952);
#99973=AXIS2_PLACEMENT_3D('',#377661,#117953,#117954);
#99974=AXIS2_PLACEMENT_3D('',#377665,#117956,#117957);
#99975=AXIS2_PLACEMENT_3D('',#377669,#117959,#117960);
#99976=AXIS2_PLACEMENT_3D('',#377671,#117961,#117962);
#99977=AXIS2_PLACEMENT_3D('',#377673,#117963,#117964);
#99978=AXIS2_PLACEMENT_3D('',#377677,#117966,#117967);
#99979=AXIS2_PLACEMENT_3D('',#377681,#117969,#117970);
#99980=AXIS2_PLACEMENT_3D('',#377683,#117971,#117972);
#99981=AXIS2_PLACEMENT_3D('',#377685,#117973,#117974);
#99982=AXIS2_PLACEMENT_3D('',#377689,#117976,#117977);
#99983=AXIS2_PLACEMENT_3D('',#377693,#117979,#117980);
#99984=AXIS2_PLACEMENT_3D('',#377695,#117981,#117982);
#99985=AXIS2_PLACEMENT_3D('',#377697,#117983,#117984);
#99986=AXIS2_PLACEMENT_3D('',#377701,#117986,#117987);
#99987=AXIS2_PLACEMENT_3D('',#377705,#117989,#117990);
#99988=AXIS2_PLACEMENT_3D('',#377707,#117991,#117992);
#99989=AXIS2_PLACEMENT_3D('',#377709,#117993,#117994);
#99990=AXIS2_PLACEMENT_3D('',#377713,#117996,#117997);
#99991=AXIS2_PLACEMENT_3D('',#377717,#117999,#118000);
#99992=AXIS2_PLACEMENT_3D('',#377719,#118001,#118002);
#99993=AXIS2_PLACEMENT_3D('',#377721,#118003,#118004);
#99994=AXIS2_PLACEMENT_3D('',#377725,#118006,#118007);
#99995=AXIS2_PLACEMENT_3D('',#377729,#118009,#118010);
#99996=AXIS2_PLACEMENT_3D('',#377731,#118011,#118012);
#99997=AXIS2_PLACEMENT_3D('',#377733,#118013,#118014);
#99998=AXIS2_PLACEMENT_3D('',#377737,#118016,#118017);
#99999=AXIS2_PLACEMENT_3D('',#377741,#118019,#118020);
#100000=AXIS2_PLACEMENT_3D('',#377743,#118021,#118022);
#100001=AXIS2_PLACEMENT_3D('',#377745,#118023,#118024);
#100002=AXIS2_PLACEMENT_3D('',#377749,#118026,#118027);
#100003=AXIS2_PLACEMENT_3D('',#377753,#118029,#118030);
#100004=AXIS2_PLACEMENT_3D('',#377755,#118031,#118032);
#100005=AXIS2_PLACEMENT_3D('',#377757,#118033,#118034);
#100006=AXIS2_PLACEMENT_3D('',#377761,#118036,#118037);
#100007=AXIS2_PLACEMENT_3D('',#377765,#118039,#118040);
#100008=AXIS2_PLACEMENT_3D('',#377767,#118041,#118042);
#100009=AXIS2_PLACEMENT_3D('',#377769,#118043,#118044);
#100010=AXIS2_PLACEMENT_3D('',#377773,#118046,#118047);
#100011=AXIS2_PLACEMENT_3D('',#377777,#118049,#118050);
#100012=AXIS2_PLACEMENT_3D('',#377779,#118051,#118052);
#100013=AXIS2_PLACEMENT_3D('',#377781,#118053,#118054);
#100014=AXIS2_PLACEMENT_3D('',#377785,#118056,#118057);
#100015=AXIS2_PLACEMENT_3D('',#377789,#118059,#118060);
#100016=AXIS2_PLACEMENT_3D('',#377791,#118061,#118062);
#100017=AXIS2_PLACEMENT_3D('',#377793,#118063,#118064);
#100018=AXIS2_PLACEMENT_3D('',#377797,#118066,#118067);
#100019=AXIS2_PLACEMENT_3D('',#377801,#118069,#118070);
#100020=AXIS2_PLACEMENT_3D('',#377803,#118071,#118072);
#100021=AXIS2_PLACEMENT_3D('',#377805,#118073,#118074);
#100022=AXIS2_PLACEMENT_3D('',#377809,#118076,#118077);
#100023=AXIS2_PLACEMENT_3D('',#377813,#118079,#118080);
#100024=AXIS2_PLACEMENT_3D('',#377815,#118081,#118082);
#100025=AXIS2_PLACEMENT_3D('',#377817,#118083,#118084);
#100026=AXIS2_PLACEMENT_3D('',#377821,#118086,#118087);
#100027=AXIS2_PLACEMENT_3D('',#377825,#118089,#118090);
#100028=AXIS2_PLACEMENT_3D('',#377827,#118091,#118092);
#100029=AXIS2_PLACEMENT_3D('',#377829,#118093,#118094);
#100030=AXIS2_PLACEMENT_3D('',#377833,#118096,#118097);
#100031=AXIS2_PLACEMENT_3D('',#377837,#118099,#118100);
#100032=AXIS2_PLACEMENT_3D('',#377839,#118101,#118102);
#100033=AXIS2_PLACEMENT_3D('',#377841,#118103,#118104);
#100034=AXIS2_PLACEMENT_3D('',#377845,#118106,#118107);
#100035=AXIS2_PLACEMENT_3D('',#377849,#118109,#118110);
#100036=AXIS2_PLACEMENT_3D('',#377851,#118111,#118112);
#100037=AXIS2_PLACEMENT_3D('',#377853,#118113,#118114);
#100038=AXIS2_PLACEMENT_3D('',#377857,#118116,#118117);
#100039=AXIS2_PLACEMENT_3D('',#377861,#118119,#118120);
#100040=AXIS2_PLACEMENT_3D('',#377863,#118121,#118122);
#100041=AXIS2_PLACEMENT_3D('',#377865,#118123,#118124);
#100042=AXIS2_PLACEMENT_3D('',#377869,#118126,#118127);
#100043=AXIS2_PLACEMENT_3D('',#377873,#118129,#118130);
#100044=AXIS2_PLACEMENT_3D('',#377875,#118131,#118132);
#100045=AXIS2_PLACEMENT_3D('',#377877,#118133,#118134);
#100046=AXIS2_PLACEMENT_3D('',#377881,#118136,#118137);
#100047=AXIS2_PLACEMENT_3D('',#377885,#118139,#118140);
#100048=AXIS2_PLACEMENT_3D('',#377887,#118141,#118142);
#100049=AXIS2_PLACEMENT_3D('',#377889,#118143,#118144);
#100050=AXIS2_PLACEMENT_3D('',#377893,#118146,#118147);
#100051=AXIS2_PLACEMENT_3D('',#377897,#118149,#118150);
#100052=AXIS2_PLACEMENT_3D('',#377899,#118151,#118152);
#100053=AXIS2_PLACEMENT_3D('',#377901,#118153,#118154);
#100054=AXIS2_PLACEMENT_3D('',#377905,#118156,#118157);
#100055=AXIS2_PLACEMENT_3D('',#377909,#118159,#118160);
#100056=AXIS2_PLACEMENT_3D('',#377911,#118161,#118162);
#100057=AXIS2_PLACEMENT_3D('',#377913,#118163,#118164);
#100058=AXIS2_PLACEMENT_3D('',#377917,#118166,#118167);
#100059=AXIS2_PLACEMENT_3D('',#377921,#118169,#118170);
#100060=AXIS2_PLACEMENT_3D('',#377923,#118171,#118172);
#100061=AXIS2_PLACEMENT_3D('',#377925,#118173,#118174);
#100062=AXIS2_PLACEMENT_3D('',#377929,#118176,#118177);
#100063=AXIS2_PLACEMENT_3D('',#377933,#118179,#118180);
#100064=AXIS2_PLACEMENT_3D('',#377935,#118181,#118182);
#100065=AXIS2_PLACEMENT_3D('',#377937,#118183,#118184);
#100066=AXIS2_PLACEMENT_3D('',#377941,#118186,#118187);
#100067=AXIS2_PLACEMENT_3D('',#377945,#118189,#118190);
#100068=AXIS2_PLACEMENT_3D('',#377947,#118191,#118192);
#100069=AXIS2_PLACEMENT_3D('',#377949,#118193,#118194);
#100070=AXIS2_PLACEMENT_3D('',#377953,#118196,#118197);
#100071=AXIS2_PLACEMENT_3D('',#377957,#118199,#118200);
#100072=AXIS2_PLACEMENT_3D('',#377959,#118201,#118202);
#100073=AXIS2_PLACEMENT_3D('',#377961,#118203,#118204);
#100074=AXIS2_PLACEMENT_3D('',#377963,#118206,#118207);
#100075=AXIS2_PLACEMENT_3D('',#377964,#118208,#118209);
#100076=AXIS2_PLACEMENT_3D('',#377965,#118210,#118211);
#100077=AXIS2_PLACEMENT_3D('',#377966,#118212,#118213);
#100078=AXIS2_PLACEMENT_3D('',#377967,#118214,#118215);
#100079=AXIS2_PLACEMENT_3D('',#377968,#118216,#118217);
#100080=AXIS2_PLACEMENT_3D('',#377969,#118218,#118219);
#100081=AXIS2_PLACEMENT_3D('',#377970,#118220,#118221);
#100082=AXIS2_PLACEMENT_3D('',#377971,#118222,#118223);
#100083=AXIS2_PLACEMENT_3D('',#377972,#118224,#118225);
#100084=AXIS2_PLACEMENT_3D('',#377973,#118226,#118227);
#100085=AXIS2_PLACEMENT_3D('',#377974,#118228,#118229);
#100086=AXIS2_PLACEMENT_3D('',#377975,#118230,#118231);
#100087=AXIS2_PLACEMENT_3D('',#377976,#118232,#118233);
#100088=AXIS2_PLACEMENT_3D('',#377977,#118234,#118235);
#100089=AXIS2_PLACEMENT_3D('',#377978,#118236,#118237);
#100090=AXIS2_PLACEMENT_3D('',#377979,#118238,#118239);
#100091=AXIS2_PLACEMENT_3D('',#377980,#118240,#118241);
#100092=AXIS2_PLACEMENT_3D('',#377981,#118242,#118243);
#100093=AXIS2_PLACEMENT_3D('',#377982,#118244,#118245);
#100094=AXIS2_PLACEMENT_3D('',#377983,#118246,#118247);
#100095=AXIS2_PLACEMENT_3D('',#377984,#118248,#118249);
#100096=AXIS2_PLACEMENT_3D('',#377985,#118250,#118251);
#100097=AXIS2_PLACEMENT_3D('',#377986,#118252,#118253);
#100098=AXIS2_PLACEMENT_3D('',#377987,#118254,#118255);
#100099=AXIS2_PLACEMENT_3D('',#377988,#118256,#118257);
#100100=AXIS2_PLACEMENT_3D('',#377989,#118258,#118259);
#100101=AXIS2_PLACEMENT_3D('',#377990,#118260,#118261);
#100102=AXIS2_PLACEMENT_3D('',#377991,#118262,#118263);
#100103=AXIS2_PLACEMENT_3D('',#377992,#118264,#118265);
#100104=AXIS2_PLACEMENT_3D('',#377993,#118266,#118267);
#100105=AXIS2_PLACEMENT_3D('',#377994,#118268,#118269);
#100106=AXIS2_PLACEMENT_3D('',#377995,#118270,#118271);
#100107=AXIS2_PLACEMENT_3D('',#377996,#118272,#118273);
#100108=AXIS2_PLACEMENT_3D('',#377997,#118274,#118275);
#100109=AXIS2_PLACEMENT_3D('',#377998,#118276,#118277);
#100110=AXIS2_PLACEMENT_3D('',#377999,#118278,#118279);
#100111=AXIS2_PLACEMENT_3D('',#378000,#118280,#118281);
#100112=AXIS2_PLACEMENT_3D('',#378001,#118282,#118283);
#100113=AXIS2_PLACEMENT_3D('',#378002,#118284,#118285);
#100114=AXIS2_PLACEMENT_3D('',#378003,#118286,#118287);
#100115=AXIS2_PLACEMENT_3D('',#378004,#118288,#118289);
#100116=AXIS2_PLACEMENT_3D('',#378005,#118290,#118291);
#100117=AXIS2_PLACEMENT_3D('',#378006,#118292,#118293);
#100118=AXIS2_PLACEMENT_3D('',#378007,#118294,#118295);
#100119=AXIS2_PLACEMENT_3D('',#378008,#118296,#118297);
#100120=AXIS2_PLACEMENT_3D('',#378009,#118298,#118299);
#100121=AXIS2_PLACEMENT_3D('',#378010,#118300,#118301);
#100122=AXIS2_PLACEMENT_3D('',#378011,#118302,#118303);
#100123=AXIS2_PLACEMENT_3D('',#378012,#118304,#118305);
#100124=AXIS2_PLACEMENT_3D('',#378013,#118306,#118307);
#100125=AXIS2_PLACEMENT_3D('',#378014,#118308,#118309);
#100126=AXIS2_PLACEMENT_3D('',#378015,#118310,#118311);
#100127=AXIS2_PLACEMENT_3D('',#378016,#118312,#118313);
#100128=AXIS2_PLACEMENT_3D('',#378017,#118314,#118315);
#100129=AXIS2_PLACEMENT_3D('',#378018,#118316,#118317);
#100130=AXIS2_PLACEMENT_3D('',#378019,#118318,#118319);
#100131=AXIS2_PLACEMENT_3D('',#378020,#118320,#118321);
#100132=AXIS2_PLACEMENT_3D('',#378021,#118322,#118323);
#100133=AXIS2_PLACEMENT_3D('',#378022,#118324,#118325);
#100134=AXIS2_PLACEMENT_3D('',#378023,#118326,#118327);
#100135=AXIS2_PLACEMENT_3D('',#378024,#118328,#118329);
#100136=AXIS2_PLACEMENT_3D('',#378025,#118330,#118331);
#100137=AXIS2_PLACEMENT_3D('',#378026,#118332,#118333);
#100138=AXIS2_PLACEMENT_3D('',#378027,#118334,#118335);
#100139=AXIS2_PLACEMENT_3D('',#378028,#118336,#118337);
#100140=AXIS2_PLACEMENT_3D('',#378029,#118338,#118339);
#100141=AXIS2_PLACEMENT_3D('',#378030,#118340,#118341);
#100142=AXIS2_PLACEMENT_3D('',#378031,#118342,#118343);
#100143=AXIS2_PLACEMENT_3D('',#378032,#118344,#118345);
#100144=AXIS2_PLACEMENT_3D('',#378033,#118346,#118347);
#100145=AXIS2_PLACEMENT_3D('',#378034,#118348,#118349);
#100146=AXIS2_PLACEMENT_3D('',#378035,#118350,#118351);
#100147=AXIS2_PLACEMENT_3D('',#378036,#118352,#118353);
#100148=AXIS2_PLACEMENT_3D('',#378037,#118354,#118355);
#100149=AXIS2_PLACEMENT_3D('',#378038,#118356,#118357);
#100150=AXIS2_PLACEMENT_3D('',#378039,#118358,#118359);
#100151=AXIS2_PLACEMENT_3D('',#378040,#118360,#118361);
#100152=AXIS2_PLACEMENT_3D('',#378041,#118362,#118363);
#100153=AXIS2_PLACEMENT_3D('',#378042,#118364,#118365);
#100154=AXIS2_PLACEMENT_3D('',#378043,#118366,#118367);
#100155=AXIS2_PLACEMENT_3D('',#378044,#118368,#118369);
#100156=AXIS2_PLACEMENT_3D('',#378045,#118370,#118371);
#100157=AXIS2_PLACEMENT_3D('',#378046,#118372,#118373);
#100158=AXIS2_PLACEMENT_3D('',#378047,#118374,#118375);
#100159=AXIS2_PLACEMENT_3D('',#378048,#118376,#118377);
#100160=AXIS2_PLACEMENT_3D('',#378049,#118378,#118379);
#100161=AXIS2_PLACEMENT_3D('',#378050,#118380,#118381);
#100162=AXIS2_PLACEMENT_3D('',#378051,#118382,#118383);
#100163=AXIS2_PLACEMENT_3D('',#378052,#118384,#118385);
#100164=AXIS2_PLACEMENT_3D('',#378053,#118386,#118387);
#100165=AXIS2_PLACEMENT_3D('',#378054,#118388,#118389);
#100166=AXIS2_PLACEMENT_3D('',#378055,#118390,#118391);
#100167=AXIS2_PLACEMENT_3D('',#378056,#118392,#118393);
#100168=AXIS2_PLACEMENT_3D('',#378057,#118394,#118395);
#100169=AXIS2_PLACEMENT_3D('',#378058,#118396,#118397);
#100170=AXIS2_PLACEMENT_3D('',#378059,#118398,#118399);
#100171=AXIS2_PLACEMENT_3D('',#378060,#118400,#118401);
#100172=AXIS2_PLACEMENT_3D('',#378061,#118402,#118403);
#100173=AXIS2_PLACEMENT_3D('',#378062,#118404,#118405);
#100174=AXIS2_PLACEMENT_3D('',#378063,#118406,#118407);
#100175=AXIS2_PLACEMENT_3D('',#378064,#118408,#118409);
#100176=AXIS2_PLACEMENT_3D('',#378065,#118410,#118411);
#100177=AXIS2_PLACEMENT_3D('',#378066,#118412,#118413);
#100178=AXIS2_PLACEMENT_3D('',#378067,#118414,#118415);
#100179=AXIS2_PLACEMENT_3D('',#378068,#118416,#118417);
#100180=AXIS2_PLACEMENT_3D('',#378069,#118418,#118419);
#100181=AXIS2_PLACEMENT_3D('',#378070,#118420,#118421);
#100182=AXIS2_PLACEMENT_3D('',#378071,#118422,#118423);
#100183=AXIS2_PLACEMENT_3D('',#378072,#118424,#118425);
#100184=AXIS2_PLACEMENT_3D('',#378073,#118426,#118427);
#100185=AXIS2_PLACEMENT_3D('',#378074,#118428,#118429);
#100186=AXIS2_PLACEMENT_3D('',#378075,#118430,#118431);
#100187=AXIS2_PLACEMENT_3D('',#378076,#118432,#118433);
#100188=AXIS2_PLACEMENT_3D('',#378077,#118434,#118435);
#100189=AXIS2_PLACEMENT_3D('',#378078,#118436,#118437);
#100190=AXIS2_PLACEMENT_3D('',#378079,#118438,#118439);
#100191=AXIS2_PLACEMENT_3D('',#378080,#118440,#118441);
#100192=AXIS2_PLACEMENT_3D('',#378081,#118442,#118443);
#100193=AXIS2_PLACEMENT_3D('',#378082,#118444,#118445);
#100194=AXIS2_PLACEMENT_3D('',#378083,#118446,#118447);
#100195=AXIS2_PLACEMENT_3D('',#378084,#118448,#118449);
#100196=AXIS2_PLACEMENT_3D('',#378085,#118450,#118451);
#100197=AXIS2_PLACEMENT_3D('',#378086,#118452,#118453);
#100198=AXIS2_PLACEMENT_3D('',#378087,#118454,#118455);
#100199=AXIS2_PLACEMENT_3D('',#378088,#118456,#118457);
#100200=AXIS2_PLACEMENT_3D('',#378089,#118458,#118459);
#100201=AXIS2_PLACEMENT_3D('',#378090,#118460,#118461);
#100202=AXIS2_PLACEMENT_3D('',#378091,#118462,#118463);
#100203=AXIS2_PLACEMENT_3D('',#378092,#118464,#118465);
#100204=AXIS2_PLACEMENT_3D('',#378093,#118466,#118467);
#100205=AXIS2_PLACEMENT_3D('',#378094,#118468,#118469);
#100206=AXIS2_PLACEMENT_3D('',#378095,#118470,#118471);
#100207=AXIS2_PLACEMENT_3D('',#378096,#118472,#118473);
#100208=AXIS2_PLACEMENT_3D('',#378097,#118474,#118475);
#100209=AXIS2_PLACEMENT_3D('',#378098,#118476,#118477);
#100210=AXIS2_PLACEMENT_3D('',#378099,#118478,#118479);
#100211=AXIS2_PLACEMENT_3D('',#378100,#118480,#118481);
#100212=AXIS2_PLACEMENT_3D('',#378101,#118482,#118483);
#100213=AXIS2_PLACEMENT_3D('',#378102,#118484,#118485);
#100214=AXIS2_PLACEMENT_3D('',#378103,#118486,#118487);
#100215=AXIS2_PLACEMENT_3D('',#378104,#118488,#118489);
#100216=AXIS2_PLACEMENT_3D('',#378105,#118490,#118491);
#100217=AXIS2_PLACEMENT_3D('',#378106,#118492,#118493);
#100218=AXIS2_PLACEMENT_3D('',#378107,#118494,#118495);
#100219=AXIS2_PLACEMENT_3D('',#378108,#118496,#118497);
#100220=AXIS2_PLACEMENT_3D('',#378109,#118498,#118499);
#100221=AXIS2_PLACEMENT_3D('',#378110,#118500,#118501);
#100222=AXIS2_PLACEMENT_3D('',#378111,#118502,#118503);
#100223=AXIS2_PLACEMENT_3D('',#378112,#118504,#118505);
#100224=AXIS2_PLACEMENT_3D('',#378113,#118506,#118507);
#100225=AXIS2_PLACEMENT_3D('',#378114,#118508,#118509);
#100226=AXIS2_PLACEMENT_3D('',#378115,#118510,#118511);
#100227=AXIS2_PLACEMENT_3D('',#378116,#118512,#118513);
#100228=AXIS2_PLACEMENT_3D('',#378117,#118514,#118515);
#100229=AXIS2_PLACEMENT_3D('',#378118,#118516,#118517);
#100230=AXIS2_PLACEMENT_3D('',#378119,#118518,#118519);
#100231=AXIS2_PLACEMENT_3D('',#378120,#118520,#118521);
#100232=AXIS2_PLACEMENT_3D('',#378121,#118522,#118523);
#100233=AXIS2_PLACEMENT_3D('',#378122,#118524,#118525);
#100234=AXIS2_PLACEMENT_3D('',#378123,#118526,#118527);
#100235=AXIS2_PLACEMENT_3D('',#378124,#118528,#118529);
#100236=AXIS2_PLACEMENT_3D('',#378125,#118530,#118531);
#100237=AXIS2_PLACEMENT_3D('',#378126,#118532,#118533);
#100238=AXIS2_PLACEMENT_3D('',#378127,#118534,#118535);
#100239=AXIS2_PLACEMENT_3D('',#378128,#118536,#118537);
#100240=AXIS2_PLACEMENT_3D('',#378129,#118538,#118539);
#100241=AXIS2_PLACEMENT_3D('',#378130,#118540,#118541);
#100242=AXIS2_PLACEMENT_3D('',#378131,#118542,#118543);
#100243=AXIS2_PLACEMENT_3D('',#378132,#118544,#118545);
#100244=AXIS2_PLACEMENT_3D('',#378133,#118546,#118547);
#100245=AXIS2_PLACEMENT_3D('',#378134,#118548,#118549);
#100246=AXIS2_PLACEMENT_3D('',#378135,#118550,#118551);
#100247=AXIS2_PLACEMENT_3D('',#378136,#118552,#118553);
#100248=AXIS2_PLACEMENT_3D('',#378137,#118554,#118555);
#100249=AXIS2_PLACEMENT_3D('',#378138,#118556,#118557);
#100250=AXIS2_PLACEMENT_3D('',#378139,#118558,#118559);
#100251=AXIS2_PLACEMENT_3D('',#378140,#118560,#118561);
#100252=AXIS2_PLACEMENT_3D('',#378141,#118562,#118563);
#100253=AXIS2_PLACEMENT_3D('',#378142,#118564,#118565);
#100254=AXIS2_PLACEMENT_3D('',#378143,#118566,#118567);
#100255=AXIS2_PLACEMENT_3D('',#378144,#118568,#118569);
#100256=AXIS2_PLACEMENT_3D('',#378145,#118570,#118571);
#100257=AXIS2_PLACEMENT_3D('',#378146,#118572,#118573);
#100258=AXIS2_PLACEMENT_3D('',#378147,#118574,#118575);
#100259=AXIS2_PLACEMENT_3D('',#378148,#118576,#118577);
#100260=AXIS2_PLACEMENT_3D('',#378149,#118578,#118579);
#100261=AXIS2_PLACEMENT_3D('',#378150,#118580,#118581);
#100262=AXIS2_PLACEMENT_3D('',#378151,#118582,#118583);
#100263=AXIS2_PLACEMENT_3D('',#378152,#118584,#118585);
#100264=AXIS2_PLACEMENT_3D('',#378153,#118586,#118587);
#100265=AXIS2_PLACEMENT_3D('',#378154,#118588,#118589);
#100266=AXIS2_PLACEMENT_3D('',#378155,#118590,#118591);
#100267=AXIS2_PLACEMENT_3D('',#378156,#118592,#118593);
#100268=AXIS2_PLACEMENT_3D('',#378157,#118594,#118595);
#100269=AXIS2_PLACEMENT_3D('',#378158,#118596,#118597);
#100270=AXIS2_PLACEMENT_3D('',#378159,#118598,#118599);
#100271=AXIS2_PLACEMENT_3D('',#378160,#118600,#118601);
#100272=AXIS2_PLACEMENT_3D('',#378161,#118602,#118603);
#100273=AXIS2_PLACEMENT_3D('',#378162,#118604,#118605);
#100274=AXIS2_PLACEMENT_3D('',#378163,#118606,#118607);
#100275=AXIS2_PLACEMENT_3D('',#378164,#118608,#118609);
#100276=AXIS2_PLACEMENT_3D('',#378165,#118610,#118611);
#100277=AXIS2_PLACEMENT_3D('',#378166,#118612,#118613);
#100278=AXIS2_PLACEMENT_3D('',#378167,#118614,#118615);
#100279=AXIS2_PLACEMENT_3D('',#378168,#118616,#118617);
#100280=AXIS2_PLACEMENT_3D('',#378169,#118618,#118619);
#100281=AXIS2_PLACEMENT_3D('',#378170,#118620,#118621);
#100282=AXIS2_PLACEMENT_3D('',#378171,#118622,#118623);
#100283=AXIS2_PLACEMENT_3D('',#378172,#118624,#118625);
#100284=AXIS2_PLACEMENT_3D('',#378173,#118626,#118627);
#100285=AXIS2_PLACEMENT_3D('',#378174,#118628,#118629);
#100286=AXIS2_PLACEMENT_3D('',#378175,#118630,#118631);
#100287=AXIS2_PLACEMENT_3D('',#378176,#118632,#118633);
#100288=AXIS2_PLACEMENT_3D('',#378177,#118634,#118635);
#100289=AXIS2_PLACEMENT_3D('',#378178,#118636,#118637);
#100290=AXIS2_PLACEMENT_3D('',#378179,#118638,#118639);
#100291=AXIS2_PLACEMENT_3D('',#378180,#118640,#118641);
#100292=AXIS2_PLACEMENT_3D('',#378181,#118642,#118643);
#100293=AXIS2_PLACEMENT_3D('',#378182,#118644,#118645);
#100294=AXIS2_PLACEMENT_3D('',#378183,#118646,#118647);
#100295=AXIS2_PLACEMENT_3D('',#378184,#118648,#118649);
#100296=AXIS2_PLACEMENT_3D('',#378185,#118650,#118651);
#100297=AXIS2_PLACEMENT_3D('',#378186,#118652,#118653);
#100298=AXIS2_PLACEMENT_3D('',#378187,#118654,#118655);
#100299=AXIS2_PLACEMENT_3D('',#378188,#118656,#118657);
#100300=AXIS2_PLACEMENT_3D('',#378189,#118658,#118659);
#100301=AXIS2_PLACEMENT_3D('',#378190,#118660,#118661);
#100302=AXIS2_PLACEMENT_3D('',#378191,#118662,#118663);
#100303=AXIS2_PLACEMENT_3D('',#378192,#118664,#118665);
#100304=AXIS2_PLACEMENT_3D('',#378193,#118666,#118667);
#100305=AXIS2_PLACEMENT_3D('',#378194,#118668,#118669);
#100306=AXIS2_PLACEMENT_3D('',#378195,#118670,#118671);
#100307=AXIS2_PLACEMENT_3D('',#378196,#118672,#118673);
#100308=AXIS2_PLACEMENT_3D('',#378197,#118674,#118675);
#100309=AXIS2_PLACEMENT_3D('',#378198,#118676,#118677);
#100310=AXIS2_PLACEMENT_3D('',#378199,#118678,#118679);
#100311=AXIS2_PLACEMENT_3D('',#378200,#118680,#118681);
#100312=AXIS2_PLACEMENT_3D('',#378201,#118682,#118683);
#100313=AXIS2_PLACEMENT_3D('',#378202,#118684,#118685);
#100314=AXIS2_PLACEMENT_3D('',#378203,#118686,#118687);
#100315=AXIS2_PLACEMENT_3D('',#378204,#118688,#118689);
#100316=AXIS2_PLACEMENT_3D('',#378205,#118690,#118691);
#100317=AXIS2_PLACEMENT_3D('',#378206,#118692,#118693);
#100318=AXIS2_PLACEMENT_3D('',#378207,#118694,#118695);
#100319=AXIS2_PLACEMENT_3D('',#378208,#118696,#118697);
#100320=AXIS2_PLACEMENT_3D('',#378209,#118698,#118699);
#100321=AXIS2_PLACEMENT_3D('',#378210,#118700,#118701);
#100322=AXIS2_PLACEMENT_3D('',#378211,#118702,#118703);
#100323=AXIS2_PLACEMENT_3D('',#378212,#118704,#118705);
#100324=AXIS2_PLACEMENT_3D('',#378213,#118706,#118707);
#100325=AXIS2_PLACEMENT_3D('',#378214,#118708,#118709);
#100326=AXIS2_PLACEMENT_3D('',#378215,#118710,#118711);
#100327=AXIS2_PLACEMENT_3D('',#378216,#118712,#118713);
#100328=AXIS2_PLACEMENT_3D('',#378217,#118714,#118715);
#100329=AXIS2_PLACEMENT_3D('',#378218,#118716,#118717);
#100330=AXIS2_PLACEMENT_3D('',#378219,#118718,#118719);
#100331=AXIS2_PLACEMENT_3D('',#378220,#118720,#118721);
#100332=AXIS2_PLACEMENT_3D('',#378221,#118722,#118723);
#100333=AXIS2_PLACEMENT_3D('',#378222,#118724,#118725);
#100334=AXIS2_PLACEMENT_3D('',#378223,#118726,#118727);
#100335=AXIS2_PLACEMENT_3D('',#378224,#118728,#118729);
#100336=AXIS2_PLACEMENT_3D('',#378225,#118730,#118731);
#100337=AXIS2_PLACEMENT_3D('',#378226,#118732,#118733);
#100338=AXIS2_PLACEMENT_3D('',#378227,#118734,#118735);
#100339=AXIS2_PLACEMENT_3D('',#378228,#118736,#118737);
#100340=AXIS2_PLACEMENT_3D('',#378229,#118738,#118739);
#100341=AXIS2_PLACEMENT_3D('',#378230,#118740,#118741);
#100342=AXIS2_PLACEMENT_3D('',#378231,#118742,#118743);
#100343=AXIS2_PLACEMENT_3D('',#378232,#118744,#118745);
#100344=AXIS2_PLACEMENT_3D('',#378233,#118746,#118747);
#100345=AXIS2_PLACEMENT_3D('',#378234,#118748,#118749);
#100346=AXIS2_PLACEMENT_3D('',#378235,#118750,#118751);
#100347=AXIS2_PLACEMENT_3D('',#378236,#118752,#118753);
#100348=AXIS2_PLACEMENT_3D('',#378237,#118754,#118755);
#100349=AXIS2_PLACEMENT_3D('',#378238,#118756,#118757);
#100350=AXIS2_PLACEMENT_3D('',#378239,#118758,#118759);
#100351=AXIS2_PLACEMENT_3D('',#378240,#118760,#118761);
#100352=AXIS2_PLACEMENT_3D('',#378241,#118762,#118763);
#100353=AXIS2_PLACEMENT_3D('',#378242,#118764,#118765);
#100354=AXIS2_PLACEMENT_3D('',#378243,#118766,#118767);
#100355=AXIS2_PLACEMENT_3D('',#378244,#118768,#118769);
#100356=AXIS2_PLACEMENT_3D('',#378245,#118770,#118771);
#100357=AXIS2_PLACEMENT_3D('',#378246,#118772,#118773);
#100358=AXIS2_PLACEMENT_3D('',#378247,#118774,#118775);
#100359=AXIS2_PLACEMENT_3D('',#378248,#118776,#118777);
#100360=AXIS2_PLACEMENT_3D('',#378249,#118778,#118779);
#100361=AXIS2_PLACEMENT_3D('',#378250,#118780,#118781);
#100362=AXIS2_PLACEMENT_3D('',#378251,#118782,#118783);
#100363=AXIS2_PLACEMENT_3D('',#378252,#118784,#118785);
#100364=AXIS2_PLACEMENT_3D('',#378253,#118786,#118787);
#100365=AXIS2_PLACEMENT_3D('',#378254,#118788,#118789);
#100366=AXIS2_PLACEMENT_3D('',#378310,#118792,#118793);
#100367=AXIS2_PLACEMENT_3D('',#378311,#118794,#118795);
#100368=AXIS2_PLACEMENT_3D('',#378314,#118796,#118797);
#100369=AXIS2_PLACEMENT_3D('',#378328,#118799,#118800);
#100370=AXIS2_PLACEMENT_3D('',#378335,#118801,#118802);
#100371=AXIS2_PLACEMENT_3D('',#378345,#118804,#118805);
#100372=AXIS2_PLACEMENT_3D('',#378349,#118808,#118809);
#100373=AXIS2_PLACEMENT_3D('',#378353,#118812,#118813);
#100374=AXIS2_PLACEMENT_3D('',#378357,#118816,#118817);
#100375=AXIS2_PLACEMENT_3D('',#378361,#118820,#118821);
#100376=AXIS2_PLACEMENT_3D('',#378365,#118824,#118825);
#100377=AXIS2_PLACEMENT_3D('',#378368,#118826,#118827);
#100378=AXIS2_PLACEMENT_3D('',#378369,#118828,#118829);
#100379=AXIS2_PLACEMENT_3D('',#378371,#118830,#118831);
#100380=AXIS2_PLACEMENT_3D('',#378373,#118832,#118833);
#100381=AXIS2_PLACEMENT_3D('',#378374,#118834,#118835);
#100382=AXIS2_PLACEMENT_3D('',#378375,#118836,#118837);
#100383=AXIS2_PLACEMENT_3D('',#378376,#118838,#118839);
#100384=AXIS2_PLACEMENT_3D('',#378377,#118840,#118841);
#100385=AXIS2_PLACEMENT_3D('',#378378,#118842,#118843);
#100386=AXIS2_PLACEMENT_3D('',#378384,#118846,#118847);
#100387=AXIS2_PLACEMENT_3D('',#378386,#118849,#118850);
#100388=AXIS2_PLACEMENT_3D('',#378391,#118852,#118853);
#100389=AXIS2_PLACEMENT_3D('',#378398,#118856,#118857);
#100390=AXIS2_PLACEMENT_3D('',#378404,#118860,#118861);
#100391=AXIS2_PLACEMENT_3D('',#378408,#118862,#118863);
#100392=AXIS2_PLACEMENT_3D('',#378409,#118864,#118865);
#100393=AXIS2_PLACEMENT_3D('',#378410,#118866,#118867);
#100394=AXIS2_PLACEMENT_3D('',#378411,#118868,#118869);
#100395=AXIS2_PLACEMENT_3D('',#378412,#118870,#118871);
#100396=AXIS2_PLACEMENT_3D('',#378413,#118872,#118873);
#100397=AXIS2_PLACEMENT_3D('',#378414,#118874,#118875);
#100398=AXIS2_PLACEMENT_3D('',#378415,#118876,#118877);
#100399=AXIS2_PLACEMENT_3D('',#378416,#118878,#118879);
#100400=AXIS2_PLACEMENT_3D('',#379921,#118880,#118881);
#100401=AXIS2_PLACEMENT_3D('',#379933,#118882,#118883);
#100402=AXIS2_PLACEMENT_3D('',#379977,#118884,#118885);
#100403=AXIS2_PLACEMENT_3D('',#379978,#118886,#118887);
#100404=AXIS2_PLACEMENT_3D('',#379979,#118888,#118889);
#100405=AXIS2_PLACEMENT_3D('',#379980,#118890,#118891);
#100406=AXIS2_PLACEMENT_3D('',#379993,#118892,#118893);
#100407=AXIS2_PLACEMENT_3D('',#380006,#118894,#118895);
#100408=AXIS2_PLACEMENT_3D('',#380019,#118896,#118897);
#100409=AXIS2_PLACEMENT_3D('',#380066,#118898,#118899);
#100410=AXIS2_PLACEMENT_3D('',#380067,#118900,#118901);
#100411=AXIS2_PLACEMENT_3D('',#380080,#118902,#118903);
#100412=AXIS2_PLACEMENT_3D('',#380093,#118904,#118905);
#100413=AXIS2_PLACEMENT_3D('',#380106,#118906,#118907);
#100414=AXIS2_PLACEMENT_3D('',#380107,#118908,#118909);
#100415=AXIS2_PLACEMENT_3D('',#380108,#118910,#118911);
#100416=AXIS2_PLACEMENT_3D('',#380121,#118912,#118913);
#100417=AXIS2_PLACEMENT_3D('',#380134,#118914,#118915);
#100418=AXIS2_PLACEMENT_3D('',#380144,#118917,#118918);
#100419=AXIS2_PLACEMENT_3D('',#380154,#118920,#118921);
#100420=AXIS2_PLACEMENT_3D('',#380157,#118922,#118923);
#100421=AXIS2_PLACEMENT_3D('',#380174,#118926,#118927);
#100422=AXIS2_PLACEMENT_3D('',#380224,#118928,#118929);
#100423=AXIS2_PLACEMENT_3D('',#380270,#118930,#118931);
#100424=AXIS2_PLACEMENT_3D('',#380287,#118932,#118933);
#100425=AXIS2_PLACEMENT_3D('',#380339,#118934,#118935);
#100426=AXIS2_PLACEMENT_3D('',#380340,#118936,#118937);
#100427=AXIS2_PLACEMENT_3D('',#380341,#118938,#118939);
#100428=AXIS2_PLACEMENT_3D('',#380342,#118940,#118941);
#100429=AXIS2_PLACEMENT_3D('',#380355,#118942,#118943);
#100430=AXIS2_PLACEMENT_3D('',#380356,#118944,#118945);
#100431=AXIS2_PLACEMENT_3D('',#380357,#118946,#118947);
#100432=AXIS2_PLACEMENT_3D('',#380370,#118948,#118949);
#100433=AXIS2_PLACEMENT_3D('',#380383,#118950,#118951);
#100434=AXIS2_PLACEMENT_3D('',#380396,#118952,#118953);
#100435=AXIS2_PLACEMENT_3D('',#380409,#118954,#118955);
#100436=AXIS2_PLACEMENT_3D('',#380422,#118956,#118957);
#100437=AXIS2_PLACEMENT_3D('',#380423,#118958,#118959);
#100438=AXIS2_PLACEMENT_3D('',#380424,#118960,#118961);
#100439=AXIS2_PLACEMENT_3D('',#380437,#118962,#118963);
#100440=AXIS2_PLACEMENT_3D('',#380438,#118964,#118965);
#100441=AXIS2_PLACEMENT_3D('',#380448,#118967,#118968);
#100442=AXIS2_PLACEMENT_3D('',#380458,#118970,#118971);
#100443=AXIS2_PLACEMENT_3D('',#380461,#118972,#118973);
#100444=AXIS2_PLACEMENT_3D('',#380478,#118976,#118977);
#100445=AXIS2_PLACEMENT_3D('',#380528,#118978,#118979);
#100446=AXIS2_PLACEMENT_3D('',#380574,#118980,#118981);
#100447=AXIS2_PLACEMENT_3D('',#380591,#118982,#118983);
#100448=AXIS2_PLACEMENT_3D('',#380643,#118984,#118985);
#100449=AXIS2_PLACEMENT_3D('',#380644,#118986,#118987);
#100450=AXIS2_PLACEMENT_3D('',#380645,#118988,#118989);
#100451=AXIS2_PLACEMENT_3D('',#380646,#118990,#118991);
#100452=AXIS2_PLACEMENT_3D('',#380659,#118992,#118993);
#100453=AXIS2_PLACEMENT_3D('',#380660,#118994,#118995);
#100454=AXIS2_PLACEMENT_3D('',#380661,#118996,#118997);
#100455=AXIS2_PLACEMENT_3D('',#380674,#118998,#118999);
#100456=AXIS2_PLACEMENT_3D('',#380687,#119000,#119001);
#100457=AXIS2_PLACEMENT_3D('',#380700,#119002,#119003);
#100458=AXIS2_PLACEMENT_3D('',#380713,#119004,#119005);
#100459=AXIS2_PLACEMENT_3D('',#380726,#119006,#119007);
#100460=AXIS2_PLACEMENT_3D('',#380727,#119008,#119009);
#100461=AXIS2_PLACEMENT_3D('',#380728,#119010,#119011);
#100462=AXIS2_PLACEMENT_3D('',#380741,#119012,#119013);
#100463=AXIS2_PLACEMENT_3D('',#380742,#119014,#119015);
#100464=AXIS2_PLACEMENT_3D('',#380752,#119017,#119018);
#100465=AXIS2_PLACEMENT_3D('',#380762,#119020,#119021);
#100466=AXIS2_PLACEMENT_3D('',#380765,#119022,#119023);
#100467=AXIS2_PLACEMENT_3D('',#380782,#119026,#119027);
#100468=AXIS2_PLACEMENT_3D('',#380832,#119028,#119029);
#100469=AXIS2_PLACEMENT_3D('',#380878,#119030,#119031);
#100470=AXIS2_PLACEMENT_3D('',#380895,#119032,#119033);
#100471=AXIS2_PLACEMENT_3D('',#380947,#119034,#119035);
#100472=AXIS2_PLACEMENT_3D('',#380948,#119036,#119037);
#100473=AXIS2_PLACEMENT_3D('',#380949,#119038,#119039);
#100474=AXIS2_PLACEMENT_3D('',#380950,#119040,#119041);
#100475=AXIS2_PLACEMENT_3D('',#380963,#119042,#119043);
#100476=AXIS2_PLACEMENT_3D('',#380964,#119044,#119045);
#100477=AXIS2_PLACEMENT_3D('',#380965,#119046,#119047);
#100478=AXIS2_PLACEMENT_3D('',#380978,#119048,#119049);
#100479=AXIS2_PLACEMENT_3D('',#380991,#119050,#119051);
#100480=AXIS2_PLACEMENT_3D('',#381004,#119052,#119053);
#100481=AXIS2_PLACEMENT_3D('',#381017,#119054,#119055);
#100482=AXIS2_PLACEMENT_3D('',#381030,#119056,#119057);
#100483=AXIS2_PLACEMENT_3D('',#381031,#119058,#119059);
#100484=AXIS2_PLACEMENT_3D('',#381032,#119060,#119061);
#100485=AXIS2_PLACEMENT_3D('',#381045,#119062,#119063);
#100486=AXIS2_PLACEMENT_3D('',#381046,#119064,#119065);
#100487=AXIS2_PLACEMENT_3D('',#381056,#119067,#119068);
#100488=AXIS2_PLACEMENT_3D('',#381066,#119070,#119071);
#100489=AXIS2_PLACEMENT_3D('',#381069,#119072,#119073);
#100490=AXIS2_PLACEMENT_3D('',#381086,#119076,#119077);
#100491=AXIS2_PLACEMENT_3D('',#381136,#119078,#119079);
#100492=AXIS2_PLACEMENT_3D('',#381182,#119080,#119081);
#100493=AXIS2_PLACEMENT_3D('',#381199,#119082,#119083);
#100494=AXIS2_PLACEMENT_3D('',#381251,#119084,#119085);
#100495=AXIS2_PLACEMENT_3D('',#381252,#119086,#119087);
#100496=AXIS2_PLACEMENT_3D('',#381253,#119088,#119089);
#100497=AXIS2_PLACEMENT_3D('',#381254,#119090,#119091);
#100498=AXIS2_PLACEMENT_3D('',#381267,#119092,#119093);
#100499=AXIS2_PLACEMENT_3D('',#381268,#119094,#119095);
#100500=AXIS2_PLACEMENT_3D('',#381269,#119096,#119097);
#100501=AXIS2_PLACEMENT_3D('',#381282,#119098,#119099);
#100502=AXIS2_PLACEMENT_3D('',#381295,#119100,#119101);
#100503=AXIS2_PLACEMENT_3D('',#381308,#119102,#119103);
#100504=AXIS2_PLACEMENT_3D('',#381321,#119104,#119105);
#100505=AXIS2_PLACEMENT_3D('',#381334,#119106,#119107);
#100506=AXIS2_PLACEMENT_3D('',#381335,#119108,#119109);
#100507=AXIS2_PLACEMENT_3D('',#381336,#119110,#119111);
#100508=AXIS2_PLACEMENT_3D('',#381349,#119112,#119113);
#100509=AXIS2_PLACEMENT_3D('',#381350,#119114,#119115);
#100510=AXIS2_PLACEMENT_3D('',#381360,#119117,#119118);
#100511=AXIS2_PLACEMENT_3D('',#381370,#119120,#119121);
#100512=AXIS2_PLACEMENT_3D('',#381373,#119122,#119123);
#100513=AXIS2_PLACEMENT_3D('',#381390,#119126,#119127);
#100514=AXIS2_PLACEMENT_3D('',#381440,#119128,#119129);
#100515=AXIS2_PLACEMENT_3D('',#381486,#119130,#119131);
#100516=AXIS2_PLACEMENT_3D('',#381503,#119132,#119133);
#100517=AXIS2_PLACEMENT_3D('',#381555,#119134,#119135);
#100518=AXIS2_PLACEMENT_3D('',#381556,#119136,#119137);
#100519=AXIS2_PLACEMENT_3D('',#381557,#119138,#119139);
#100520=AXIS2_PLACEMENT_3D('',#381558,#119140,#119141);
#100521=AXIS2_PLACEMENT_3D('',#381571,#119142,#119143);
#100522=AXIS2_PLACEMENT_3D('',#381572,#119144,#119145);
#100523=AXIS2_PLACEMENT_3D('',#381573,#119146,#119147);
#100524=AXIS2_PLACEMENT_3D('',#381586,#119148,#119149);
#100525=AXIS2_PLACEMENT_3D('',#381599,#119150,#119151);
#100526=AXIS2_PLACEMENT_3D('',#381612,#119152,#119153);
#100527=AXIS2_PLACEMENT_3D('',#381625,#119154,#119155);
#100528=AXIS2_PLACEMENT_3D('',#381638,#119156,#119157);
#100529=AXIS2_PLACEMENT_3D('',#381639,#119158,#119159);
#100530=AXIS2_PLACEMENT_3D('',#381640,#119160,#119161);
#100531=AXIS2_PLACEMENT_3D('',#381653,#119162,#119163);
#100532=AXIS2_PLACEMENT_3D('',#381654,#119164,#119165);
#100533=AXIS2_PLACEMENT_3D('',#381664,#119167,#119168);
#100534=AXIS2_PLACEMENT_3D('',#381674,#119170,#119171);
#100535=AXIS2_PLACEMENT_3D('',#381677,#119172,#119173);
#100536=AXIS2_PLACEMENT_3D('',#381694,#119176,#119177);
#100537=AXIS2_PLACEMENT_3D('',#381744,#119178,#119179);
#100538=AXIS2_PLACEMENT_3D('',#381790,#119180,#119181);
#100539=AXIS2_PLACEMENT_3D('',#381807,#119182,#119183);
#100540=AXIS2_PLACEMENT_3D('',#381859,#119184,#119185);
#100541=AXIS2_PLACEMENT_3D('',#381860,#119186,#119187);
#100542=AXIS2_PLACEMENT_3D('',#381861,#119188,#119189);
#100543=AXIS2_PLACEMENT_3D('',#381862,#119190,#119191);
#100544=AXIS2_PLACEMENT_3D('',#381875,#119192,#119193);
#100545=AXIS2_PLACEMENT_3D('',#381876,#119194,#119195);
#100546=AXIS2_PLACEMENT_3D('',#381877,#119196,#119197);
#100547=AXIS2_PLACEMENT_3D('',#381890,#119198,#119199);
#100548=AXIS2_PLACEMENT_3D('',#381903,#119200,#119201);
#100549=AXIS2_PLACEMENT_3D('',#381916,#119202,#119203);
#100550=AXIS2_PLACEMENT_3D('',#381929,#119204,#119205);
#100551=AXIS2_PLACEMENT_3D('',#381942,#119206,#119207);
#100552=AXIS2_PLACEMENT_3D('',#381943,#119208,#119209);
#100553=AXIS2_PLACEMENT_3D('',#381944,#119210,#119211);
#100554=AXIS2_PLACEMENT_3D('',#381957,#119212,#119213);
#100555=AXIS2_PLACEMENT_3D('',#381958,#119214,#119215);
#100556=AXIS2_PLACEMENT_3D('',#381968,#119217,#119218);
#100557=AXIS2_PLACEMENT_3D('',#381978,#119220,#119221);
#100558=AXIS2_PLACEMENT_3D('',#381981,#119222,#119223);
#100559=AXIS2_PLACEMENT_3D('',#381998,#119226,#119227);
#100560=AXIS2_PLACEMENT_3D('',#382048,#119228,#119229);
#100561=AXIS2_PLACEMENT_3D('',#382094,#119230,#119231);
#100562=AXIS2_PLACEMENT_3D('',#382111,#119232,#119233);
#100563=AXIS2_PLACEMENT_3D('',#382163,#119234,#119235);
#100564=AXIS2_PLACEMENT_3D('',#382164,#119236,#119237);
#100565=AXIS2_PLACEMENT_3D('',#382165,#119238,#119239);
#100566=AXIS2_PLACEMENT_3D('',#382166,#119240,#119241);
#100567=AXIS2_PLACEMENT_3D('',#382179,#119242,#119243);
#100568=AXIS2_PLACEMENT_3D('',#382180,#119244,#119245);
#100569=AXIS2_PLACEMENT_3D('',#382181,#119246,#119247);
#100570=AXIS2_PLACEMENT_3D('',#382194,#119248,#119249);
#100571=AXIS2_PLACEMENT_3D('',#382207,#119250,#119251);
#100572=AXIS2_PLACEMENT_3D('',#382220,#119252,#119253);
#100573=AXIS2_PLACEMENT_3D('',#382233,#119254,#119255);
#100574=AXIS2_PLACEMENT_3D('',#382246,#119256,#119257);
#100575=AXIS2_PLACEMENT_3D('',#382247,#119258,#119259);
#100576=AXIS2_PLACEMENT_3D('',#382248,#119260,#119261);
#100577=AXIS2_PLACEMENT_3D('',#382261,#119262,#119263);
#100578=AXIS2_PLACEMENT_3D('',#382262,#119264,#119265);
#100579=AXIS2_PLACEMENT_3D('',#382272,#119267,#119268);
#100580=AXIS2_PLACEMENT_3D('',#382282,#119270,#119271);
#100581=AXIS2_PLACEMENT_3D('',#382285,#119272,#119273);
#100582=AXIS2_PLACEMENT_3D('',#382302,#119276,#119277);
#100583=AXIS2_PLACEMENT_3D('',#382352,#119278,#119279);
#100584=AXIS2_PLACEMENT_3D('',#382398,#119280,#119281);
#100585=AXIS2_PLACEMENT_3D('',#382415,#119282,#119283);
#100586=AXIS2_PLACEMENT_3D('',#382467,#119284,#119285);
#100587=AXIS2_PLACEMENT_3D('',#382468,#119286,#119287);
#100588=AXIS2_PLACEMENT_3D('',#382469,#119288,#119289);
#100589=AXIS2_PLACEMENT_3D('',#382470,#119290,#119291);
#100590=AXIS2_PLACEMENT_3D('',#382483,#119292,#119293);
#100591=AXIS2_PLACEMENT_3D('',#382484,#119294,#119295);
#100592=AXIS2_PLACEMENT_3D('',#382485,#119296,#119297);
#100593=AXIS2_PLACEMENT_3D('',#382498,#119298,#119299);
#100594=AXIS2_PLACEMENT_3D('',#382511,#119300,#119301);
#100595=AXIS2_PLACEMENT_3D('',#382524,#119302,#119303);
#100596=AXIS2_PLACEMENT_3D('',#382537,#119304,#119305);
#100597=AXIS2_PLACEMENT_3D('',#382550,#119306,#119307);
#100598=AXIS2_PLACEMENT_3D('',#382551,#119308,#119309);
#100599=AXIS2_PLACEMENT_3D('',#382552,#119310,#119311);
#100600=AXIS2_PLACEMENT_3D('',#382565,#119312,#119313);
#100601=AXIS2_PLACEMENT_3D('',#382566,#119314,#119315);
#100602=AXIS2_PLACEMENT_3D('',#382576,#119317,#119318);
#100603=AXIS2_PLACEMENT_3D('',#382586,#119320,#119321);
#100604=AXIS2_PLACEMENT_3D('',#382589,#119322,#119323);
#100605=AXIS2_PLACEMENT_3D('',#382606,#119326,#119327);
#100606=AXIS2_PLACEMENT_3D('',#382656,#119328,#119329);
#100607=AXIS2_PLACEMENT_3D('',#382702,#119330,#119331);
#100608=AXIS2_PLACEMENT_3D('',#382719,#119332,#119333);
#100609=AXIS2_PLACEMENT_3D('',#382771,#119334,#119335);
#100610=AXIS2_PLACEMENT_3D('',#382772,#119336,#119337);
#100611=AXIS2_PLACEMENT_3D('',#382773,#119338,#119339);
#100612=AXIS2_PLACEMENT_3D('',#382774,#119340,#119341);
#100613=AXIS2_PLACEMENT_3D('',#382787,#119342,#119343);
#100614=AXIS2_PLACEMENT_3D('',#382788,#119344,#119345);
#100615=AXIS2_PLACEMENT_3D('',#382789,#119346,#119347);
#100616=AXIS2_PLACEMENT_3D('',#382802,#119348,#119349);
#100617=AXIS2_PLACEMENT_3D('',#382815,#119350,#119351);
#100618=AXIS2_PLACEMENT_3D('',#382828,#119352,#119353);
#100619=AXIS2_PLACEMENT_3D('',#382841,#119354,#119355);
#100620=AXIS2_PLACEMENT_3D('',#382854,#119356,#119357);
#100621=AXIS2_PLACEMENT_3D('',#382855,#119358,#119359);
#100622=AXIS2_PLACEMENT_3D('',#382856,#119360,#119361);
#100623=AXIS2_PLACEMENT_3D('',#382869,#119362,#119363);
#100624=AXIS2_PLACEMENT_3D('',#382870,#119364,#119365);
#100625=AXIS2_PLACEMENT_3D('',#382880,#119367,#119368);
#100626=AXIS2_PLACEMENT_3D('',#382890,#119370,#119371);
#100627=AXIS2_PLACEMENT_3D('',#382893,#119372,#119373);
#100628=AXIS2_PLACEMENT_3D('',#382910,#119376,#119377);
#100629=AXIS2_PLACEMENT_3D('',#382960,#119378,#119379);
#100630=AXIS2_PLACEMENT_3D('',#383006,#119380,#119381);
#100631=AXIS2_PLACEMENT_3D('',#383023,#119382,#119383);
#100632=AXIS2_PLACEMENT_3D('',#383075,#119384,#119385);
#100633=AXIS2_PLACEMENT_3D('',#383076,#119386,#119387);
#100634=AXIS2_PLACEMENT_3D('',#383077,#119388,#119389);
#100635=AXIS2_PLACEMENT_3D('',#383078,#119390,#119391);
#100636=AXIS2_PLACEMENT_3D('',#383091,#119392,#119393);
#100637=AXIS2_PLACEMENT_3D('',#383092,#119394,#119395);
#100638=AXIS2_PLACEMENT_3D('',#383093,#119396,#119397);
#100639=AXIS2_PLACEMENT_3D('',#383106,#119398,#119399);
#100640=AXIS2_PLACEMENT_3D('',#383119,#119400,#119401);
#100641=AXIS2_PLACEMENT_3D('',#383132,#119402,#119403);
#100642=AXIS2_PLACEMENT_3D('',#383145,#119404,#119405);
#100643=AXIS2_PLACEMENT_3D('',#383158,#119406,#119407);
#100644=AXIS2_PLACEMENT_3D('',#383159,#119408,#119409);
#100645=AXIS2_PLACEMENT_3D('',#383160,#119410,#119411);
#100646=AXIS2_PLACEMENT_3D('',#383173,#119412,#119413);
#100647=AXIS2_PLACEMENT_3D('',#383174,#119414,#119415);
#100648=AXIS2_PLACEMENT_3D('',#383184,#119417,#119418);
#100649=AXIS2_PLACEMENT_3D('',#383194,#119420,#119421);
#100650=AXIS2_PLACEMENT_3D('',#383197,#119422,#119423);
#100651=AXIS2_PLACEMENT_3D('',#383214,#119426,#119427);
#100652=AXIS2_PLACEMENT_3D('',#383264,#119428,#119429);
#100653=AXIS2_PLACEMENT_3D('',#383310,#119430,#119431);
#100654=AXIS2_PLACEMENT_3D('',#383327,#119432,#119433);
#100655=AXIS2_PLACEMENT_3D('',#383379,#119434,#119435);
#100656=AXIS2_PLACEMENT_3D('',#383380,#119436,#119437);
#100657=AXIS2_PLACEMENT_3D('',#383381,#119438,#119439);
#100658=AXIS2_PLACEMENT_3D('',#383382,#119440,#119441);
#100659=AXIS2_PLACEMENT_3D('',#383395,#119442,#119443);
#100660=AXIS2_PLACEMENT_3D('',#383396,#119444,#119445);
#100661=AXIS2_PLACEMENT_3D('',#383397,#119446,#119447);
#100662=AXIS2_PLACEMENT_3D('',#383410,#119448,#119449);
#100663=AXIS2_PLACEMENT_3D('',#383423,#119450,#119451);
#100664=AXIS2_PLACEMENT_3D('',#383436,#119452,#119453);
#100665=AXIS2_PLACEMENT_3D('',#383449,#119454,#119455);
#100666=AXIS2_PLACEMENT_3D('',#383462,#119456,#119457);
#100667=AXIS2_PLACEMENT_3D('',#383463,#119458,#119459);
#100668=AXIS2_PLACEMENT_3D('',#383464,#119460,#119461);
#100669=AXIS2_PLACEMENT_3D('',#383477,#119462,#119463);
#100670=AXIS2_PLACEMENT_3D('',#383478,#119464,#119465);
#100671=AXIS2_PLACEMENT_3D('',#383488,#119467,#119468);
#100672=AXIS2_PLACEMENT_3D('',#383498,#119470,#119471);
#100673=AXIS2_PLACEMENT_3D('',#383501,#119472,#119473);
#100674=AXIS2_PLACEMENT_3D('',#383518,#119476,#119477);
#100675=AXIS2_PLACEMENT_3D('',#383568,#119478,#119479);
#100676=AXIS2_PLACEMENT_3D('',#383614,#119480,#119481);
#100677=AXIS2_PLACEMENT_3D('',#383631,#119482,#119483);
#100678=AXIS2_PLACEMENT_3D('',#383683,#119484,#119485);
#100679=AXIS2_PLACEMENT_3D('',#383684,#119486,#119487);
#100680=AXIS2_PLACEMENT_3D('',#383685,#119488,#119489);
#100681=AXIS2_PLACEMENT_3D('',#383686,#119490,#119491);
#100682=AXIS2_PLACEMENT_3D('',#383699,#119492,#119493);
#100683=AXIS2_PLACEMENT_3D('',#383700,#119494,#119495);
#100684=AXIS2_PLACEMENT_3D('',#383701,#119496,#119497);
#100685=AXIS2_PLACEMENT_3D('',#383714,#119498,#119499);
#100686=AXIS2_PLACEMENT_3D('',#383727,#119500,#119501);
#100687=AXIS2_PLACEMENT_3D('',#383740,#119502,#119503);
#100688=AXIS2_PLACEMENT_3D('',#383753,#119504,#119505);
#100689=AXIS2_PLACEMENT_3D('',#383766,#119506,#119507);
#100690=AXIS2_PLACEMENT_3D('',#383767,#119508,#119509);
#100691=AXIS2_PLACEMENT_3D('',#383768,#119510,#119511);
#100692=AXIS2_PLACEMENT_3D('',#383781,#119512,#119513);
#100693=AXIS2_PLACEMENT_3D('',#383782,#119514,#119515);
#100694=AXIS2_PLACEMENT_3D('',#383792,#119517,#119518);
#100695=AXIS2_PLACEMENT_3D('',#383802,#119520,#119521);
#100696=AXIS2_PLACEMENT_3D('',#383805,#119522,#119523);
#100697=AXIS2_PLACEMENT_3D('',#383822,#119526,#119527);
#100698=AXIS2_PLACEMENT_3D('',#383872,#119528,#119529);
#100699=AXIS2_PLACEMENT_3D('',#383918,#119530,#119531);
#100700=AXIS2_PLACEMENT_3D('',#383935,#119532,#119533);
#100701=AXIS2_PLACEMENT_3D('',#383987,#119534,#119535);
#100702=AXIS2_PLACEMENT_3D('',#383988,#119536,#119537);
#100703=AXIS2_PLACEMENT_3D('',#383989,#119538,#119539);
#100704=AXIS2_PLACEMENT_3D('',#383990,#119540,#119541);
#100705=AXIS2_PLACEMENT_3D('',#384003,#119542,#119543);
#100706=AXIS2_PLACEMENT_3D('',#384004,#119544,#119545);
#100707=AXIS2_PLACEMENT_3D('',#384005,#119546,#119547);
#100708=AXIS2_PLACEMENT_3D('',#384018,#119548,#119549);
#100709=AXIS2_PLACEMENT_3D('',#384031,#119550,#119551);
#100710=AXIS2_PLACEMENT_3D('',#384044,#119552,#119553);
#100711=AXIS2_PLACEMENT_3D('',#384057,#119554,#119555);
#100712=AXIS2_PLACEMENT_3D('',#384070,#119556,#119557);
#100713=AXIS2_PLACEMENT_3D('',#384071,#119558,#119559);
#100714=AXIS2_PLACEMENT_3D('',#384072,#119560,#119561);
#100715=AXIS2_PLACEMENT_3D('',#384085,#119562,#119563);
#100716=AXIS2_PLACEMENT_3D('',#384086,#119564,#119565);
#100717=AXIS2_PLACEMENT_3D('',#384096,#119567,#119568);
#100718=AXIS2_PLACEMENT_3D('',#384106,#119570,#119571);
#100719=AXIS2_PLACEMENT_3D('',#384109,#119572,#119573);
#100720=AXIS2_PLACEMENT_3D('',#384126,#119576,#119577);
#100721=AXIS2_PLACEMENT_3D('',#384176,#119578,#119579);
#100722=AXIS2_PLACEMENT_3D('',#384222,#119580,#119581);
#100723=AXIS2_PLACEMENT_3D('',#384239,#119582,#119583);
#100724=AXIS2_PLACEMENT_3D('',#384291,#119584,#119585);
#100725=AXIS2_PLACEMENT_3D('',#384292,#119586,#119587);
#100726=AXIS2_PLACEMENT_3D('',#384293,#119588,#119589);
#100727=AXIS2_PLACEMENT_3D('',#384294,#119590,#119591);
#100728=AXIS2_PLACEMENT_3D('',#384307,#119592,#119593);
#100729=AXIS2_PLACEMENT_3D('',#384308,#119594,#119595);
#100730=AXIS2_PLACEMENT_3D('',#384309,#119596,#119597);
#100731=AXIS2_PLACEMENT_3D('',#384322,#119598,#119599);
#100732=AXIS2_PLACEMENT_3D('',#384335,#119600,#119601);
#100733=AXIS2_PLACEMENT_3D('',#384348,#119602,#119603);
#100734=AXIS2_PLACEMENT_3D('',#384361,#119604,#119605);
#100735=AXIS2_PLACEMENT_3D('',#384374,#119606,#119607);
#100736=AXIS2_PLACEMENT_3D('',#384375,#119608,#119609);
#100737=AXIS2_PLACEMENT_3D('',#384376,#119610,#119611);
#100738=AXIS2_PLACEMENT_3D('',#384389,#119612,#119613);
#100739=AXIS2_PLACEMENT_3D('',#384390,#119614,#119615);
#100740=AXIS2_PLACEMENT_3D('',#384400,#119617,#119618);
#100741=AXIS2_PLACEMENT_3D('',#384410,#119620,#119621);
#100742=AXIS2_PLACEMENT_3D('',#384413,#119622,#119623);
#100743=AXIS2_PLACEMENT_3D('',#384430,#119626,#119627);
#100744=AXIS2_PLACEMENT_3D('',#384480,#119628,#119629);
#100745=AXIS2_PLACEMENT_3D('',#384526,#119630,#119631);
#100746=AXIS2_PLACEMENT_3D('',#384543,#119632,#119633);
#100747=AXIS2_PLACEMENT_3D('',#384595,#119634,#119635);
#100748=AXIS2_PLACEMENT_3D('',#384596,#119636,#119637);
#100749=AXIS2_PLACEMENT_3D('',#384597,#119638,#119639);
#100750=AXIS2_PLACEMENT_3D('',#384598,#119640,#119641);
#100751=AXIS2_PLACEMENT_3D('',#384611,#119642,#119643);
#100752=AXIS2_PLACEMENT_3D('',#384612,#119644,#119645);
#100753=AXIS2_PLACEMENT_3D('',#384613,#119646,#119647);
#100754=AXIS2_PLACEMENT_3D('',#384626,#119648,#119649);
#100755=AXIS2_PLACEMENT_3D('',#384639,#119650,#119651);
#100756=AXIS2_PLACEMENT_3D('',#384652,#119652,#119653);
#100757=AXIS2_PLACEMENT_3D('',#384665,#119654,#119655);
#100758=AXIS2_PLACEMENT_3D('',#384678,#119656,#119657);
#100759=AXIS2_PLACEMENT_3D('',#384679,#119658,#119659);
#100760=AXIS2_PLACEMENT_3D('',#384680,#119660,#119661);
#100761=AXIS2_PLACEMENT_3D('',#384693,#119662,#119663);
#100762=AXIS2_PLACEMENT_3D('',#384694,#119664,#119665);
#100763=AXIS2_PLACEMENT_3D('',#384704,#119667,#119668);
#100764=AXIS2_PLACEMENT_3D('',#384714,#119670,#119671);
#100765=AXIS2_PLACEMENT_3D('',#384717,#119672,#119673);
#100766=AXIS2_PLACEMENT_3D('',#384734,#119676,#119677);
#100767=AXIS2_PLACEMENT_3D('',#384784,#119678,#119679);
#100768=AXIS2_PLACEMENT_3D('',#384830,#119680,#119681);
#100769=AXIS2_PLACEMENT_3D('',#384847,#119682,#119683);
#100770=AXIS2_PLACEMENT_3D('',#384899,#119684,#119685);
#100771=AXIS2_PLACEMENT_3D('',#384900,#119686,#119687);
#100772=AXIS2_PLACEMENT_3D('',#384901,#119688,#119689);
#100773=AXIS2_PLACEMENT_3D('',#384902,#119690,#119691);
#100774=AXIS2_PLACEMENT_3D('',#384915,#119692,#119693);
#100775=AXIS2_PLACEMENT_3D('',#384916,#119694,#119695);
#100776=AXIS2_PLACEMENT_3D('',#384917,#119696,#119697);
#100777=AXIS2_PLACEMENT_3D('',#384930,#119698,#119699);
#100778=AXIS2_PLACEMENT_3D('',#384943,#119700,#119701);
#100779=AXIS2_PLACEMENT_3D('',#384956,#119702,#119703);
#100780=AXIS2_PLACEMENT_3D('',#384969,#119704,#119705);
#100781=AXIS2_PLACEMENT_3D('',#384982,#119706,#119707);
#100782=AXIS2_PLACEMENT_3D('',#384983,#119708,#119709);
#100783=AXIS2_PLACEMENT_3D('',#384984,#119710,#119711);
#100784=AXIS2_PLACEMENT_3D('',#384997,#119712,#119713);
#100785=AXIS2_PLACEMENT_3D('',#384998,#119714,#119715);
#100786=AXIS2_PLACEMENT_3D('',#385008,#119717,#119718);
#100787=AXIS2_PLACEMENT_3D('',#385018,#119720,#119721);
#100788=AXIS2_PLACEMENT_3D('',#385021,#119722,#119723);
#100789=AXIS2_PLACEMENT_3D('',#385038,#119726,#119727);
#100790=AXIS2_PLACEMENT_3D('',#385088,#119728,#119729);
#100791=AXIS2_PLACEMENT_3D('',#385134,#119730,#119731);
#100792=AXIS2_PLACEMENT_3D('',#385151,#119732,#119733);
#100793=AXIS2_PLACEMENT_3D('',#385203,#119734,#119735);
#100794=AXIS2_PLACEMENT_3D('',#385204,#119736,#119737);
#100795=AXIS2_PLACEMENT_3D('',#385205,#119738,#119739);
#100796=AXIS2_PLACEMENT_3D('',#385206,#119740,#119741);
#100797=AXIS2_PLACEMENT_3D('',#385219,#119742,#119743);
#100798=AXIS2_PLACEMENT_3D('',#385220,#119744,#119745);
#100799=AXIS2_PLACEMENT_3D('',#385221,#119746,#119747);
#100800=AXIS2_PLACEMENT_3D('',#385234,#119748,#119749);
#100801=AXIS2_PLACEMENT_3D('',#385247,#119750,#119751);
#100802=AXIS2_PLACEMENT_3D('',#385260,#119752,#119753);
#100803=AXIS2_PLACEMENT_3D('',#385273,#119754,#119755);
#100804=AXIS2_PLACEMENT_3D('',#385286,#119756,#119757);
#100805=AXIS2_PLACEMENT_3D('',#385287,#119758,#119759);
#100806=AXIS2_PLACEMENT_3D('',#385288,#119760,#119761);
#100807=AXIS2_PLACEMENT_3D('',#385301,#119762,#119763);
#100808=AXIS2_PLACEMENT_3D('',#385302,#119764,#119765);
#100809=AXIS2_PLACEMENT_3D('',#385312,#119767,#119768);
#100810=AXIS2_PLACEMENT_3D('',#385322,#119770,#119771);
#100811=AXIS2_PLACEMENT_3D('',#385325,#119772,#119773);
#100812=AXIS2_PLACEMENT_3D('',#385342,#119776,#119777);
#100813=AXIS2_PLACEMENT_3D('',#385392,#119778,#119779);
#100814=AXIS2_PLACEMENT_3D('',#385438,#119780,#119781);
#100815=AXIS2_PLACEMENT_3D('',#385455,#119782,#119783);
#100816=AXIS2_PLACEMENT_3D('',#385507,#119784,#119785);
#100817=AXIS2_PLACEMENT_3D('',#385508,#119786,#119787);
#100818=AXIS2_PLACEMENT_3D('',#385509,#119788,#119789);
#100819=AXIS2_PLACEMENT_3D('',#385510,#119790,#119791);
#100820=AXIS2_PLACEMENT_3D('',#385523,#119792,#119793);
#100821=AXIS2_PLACEMENT_3D('',#385524,#119794,#119795);
#100822=AXIS2_PLACEMENT_3D('',#385525,#119796,#119797);
#100823=AXIS2_PLACEMENT_3D('',#385538,#119798,#119799);
#100824=AXIS2_PLACEMENT_3D('',#385551,#119800,#119801);
#100825=AXIS2_PLACEMENT_3D('',#385564,#119802,#119803);
#100826=AXIS2_PLACEMENT_3D('',#385577,#119804,#119805);
#100827=AXIS2_PLACEMENT_3D('',#385590,#119806,#119807);
#100828=AXIS2_PLACEMENT_3D('',#385591,#119808,#119809);
#100829=AXIS2_PLACEMENT_3D('',#385592,#119810,#119811);
#100830=AXIS2_PLACEMENT_3D('',#385605,#119812,#119813);
#100831=AXIS2_PLACEMENT_3D('',#385606,#119814,#119815);
#100832=AXIS2_PLACEMENT_3D('',#385616,#119817,#119818);
#100833=AXIS2_PLACEMENT_3D('',#385626,#119820,#119821);
#100834=AXIS2_PLACEMENT_3D('',#385629,#119822,#119823);
#100835=AXIS2_PLACEMENT_3D('',#385646,#119826,#119827);
#100836=AXIS2_PLACEMENT_3D('',#385696,#119828,#119829);
#100837=AXIS2_PLACEMENT_3D('',#385742,#119830,#119831);
#100838=AXIS2_PLACEMENT_3D('',#385759,#119832,#119833);
#100839=AXIS2_PLACEMENT_3D('',#385811,#119834,#119835);
#100840=AXIS2_PLACEMENT_3D('',#385812,#119836,#119837);
#100841=AXIS2_PLACEMENT_3D('',#385813,#119838,#119839);
#100842=AXIS2_PLACEMENT_3D('',#385814,#119840,#119841);
#100843=AXIS2_PLACEMENT_3D('',#385827,#119842,#119843);
#100844=AXIS2_PLACEMENT_3D('',#385828,#119844,#119845);
#100845=AXIS2_PLACEMENT_3D('',#385829,#119846,#119847);
#100846=AXIS2_PLACEMENT_3D('',#385842,#119848,#119849);
#100847=AXIS2_PLACEMENT_3D('',#385855,#119850,#119851);
#100848=AXIS2_PLACEMENT_3D('',#385868,#119852,#119853);
#100849=AXIS2_PLACEMENT_3D('',#385881,#119854,#119855);
#100850=AXIS2_PLACEMENT_3D('',#385894,#119856,#119857);
#100851=AXIS2_PLACEMENT_3D('',#385895,#119858,#119859);
#100852=AXIS2_PLACEMENT_3D('',#385896,#119860,#119861);
#100853=AXIS2_PLACEMENT_3D('',#385909,#119862,#119863);
#100854=AXIS2_PLACEMENT_3D('',#385910,#119864,#119865);
#100855=AXIS2_PLACEMENT_3D('',#385920,#119867,#119868);
#100856=AXIS2_PLACEMENT_3D('',#385930,#119870,#119871);
#100857=AXIS2_PLACEMENT_3D('',#385933,#119872,#119873);
#100858=AXIS2_PLACEMENT_3D('',#385950,#119876,#119877);
#100859=AXIS2_PLACEMENT_3D('',#386000,#119878,#119879);
#100860=AXIS2_PLACEMENT_3D('',#386046,#119880,#119881);
#100861=AXIS2_PLACEMENT_3D('',#386063,#119882,#119883);
#100862=AXIS2_PLACEMENT_3D('',#386115,#119884,#119885);
#100863=AXIS2_PLACEMENT_3D('',#386116,#119886,#119887);
#100864=AXIS2_PLACEMENT_3D('',#386117,#119888,#119889);
#100865=AXIS2_PLACEMENT_3D('',#386118,#119890,#119891);
#100866=AXIS2_PLACEMENT_3D('',#386131,#119892,#119893);
#100867=AXIS2_PLACEMENT_3D('',#386132,#119894,#119895);
#100868=AXIS2_PLACEMENT_3D('',#386133,#119896,#119897);
#100869=AXIS2_PLACEMENT_3D('',#386146,#119898,#119899);
#100870=AXIS2_PLACEMENT_3D('',#386159,#119900,#119901);
#100871=AXIS2_PLACEMENT_3D('',#386172,#119902,#119903);
#100872=AXIS2_PLACEMENT_3D('',#386185,#119904,#119905);
#100873=AXIS2_PLACEMENT_3D('',#386198,#119906,#119907);
#100874=AXIS2_PLACEMENT_3D('',#386199,#119908,#119909);
#100875=AXIS2_PLACEMENT_3D('',#386200,#119910,#119911);
#100876=AXIS2_PLACEMENT_3D('',#386213,#119912,#119913);
#100877=AXIS2_PLACEMENT_3D('',#386214,#119914,#119915);
#100878=AXIS2_PLACEMENT_3D('',#386224,#119917,#119918);
#100879=AXIS2_PLACEMENT_3D('',#386234,#119920,#119921);
#100880=AXIS2_PLACEMENT_3D('',#386237,#119922,#119923);
#100881=AXIS2_PLACEMENT_3D('',#386254,#119926,#119927);
#100882=AXIS2_PLACEMENT_3D('',#386304,#119928,#119929);
#100883=AXIS2_PLACEMENT_3D('',#386350,#119930,#119931);
#100884=AXIS2_PLACEMENT_3D('',#386367,#119932,#119933);
#100885=AXIS2_PLACEMENT_3D('',#386419,#119934,#119935);
#100886=AXIS2_PLACEMENT_3D('',#386420,#119936,#119937);
#100887=AXIS2_PLACEMENT_3D('',#386421,#119938,#119939);
#100888=AXIS2_PLACEMENT_3D('',#386422,#119940,#119941);
#100889=AXIS2_PLACEMENT_3D('',#386435,#119942,#119943);
#100890=AXIS2_PLACEMENT_3D('',#386436,#119944,#119945);
#100891=AXIS2_PLACEMENT_3D('',#386437,#119946,#119947);
#100892=AXIS2_PLACEMENT_3D('',#386450,#119948,#119949);
#100893=AXIS2_PLACEMENT_3D('',#386463,#119950,#119951);
#100894=AXIS2_PLACEMENT_3D('',#386476,#119952,#119953);
#100895=AXIS2_PLACEMENT_3D('',#386489,#119954,#119955);
#100896=AXIS2_PLACEMENT_3D('',#386502,#119956,#119957);
#100897=AXIS2_PLACEMENT_3D('',#386503,#119958,#119959);
#100898=AXIS2_PLACEMENT_3D('',#386504,#119960,#119961);
#100899=AXIS2_PLACEMENT_3D('',#386517,#119962,#119963);
#100900=AXIS2_PLACEMENT_3D('',#386518,#119964,#119965);
#100901=AXIS2_PLACEMENT_3D('',#386528,#119967,#119968);
#100902=AXIS2_PLACEMENT_3D('',#386538,#119970,#119971);
#100903=AXIS2_PLACEMENT_3D('',#386541,#119972,#119973);
#100904=AXIS2_PLACEMENT_3D('',#386558,#119976,#119977);
#100905=AXIS2_PLACEMENT_3D('',#386608,#119978,#119979);
#100906=AXIS2_PLACEMENT_3D('',#386654,#119980,#119981);
#100907=AXIS2_PLACEMENT_3D('',#386671,#119982,#119983);
#100908=AXIS2_PLACEMENT_3D('',#386723,#119984,#119985);
#100909=AXIS2_PLACEMENT_3D('',#386724,#119986,#119987);
#100910=AXIS2_PLACEMENT_3D('',#386725,#119988,#119989);
#100911=AXIS2_PLACEMENT_3D('',#386726,#119990,#119991);
#100912=AXIS2_PLACEMENT_3D('',#386739,#119992,#119993);
#100913=AXIS2_PLACEMENT_3D('',#386740,#119994,#119995);
#100914=AXIS2_PLACEMENT_3D('',#386741,#119996,#119997);
#100915=AXIS2_PLACEMENT_3D('',#386754,#119998,#119999);
#100916=AXIS2_PLACEMENT_3D('',#386767,#120000,#120001);
#100917=AXIS2_PLACEMENT_3D('',#386780,#120002,#120003);
#100918=AXIS2_PLACEMENT_3D('',#386793,#120004,#120005);
#100919=AXIS2_PLACEMENT_3D('',#386806,#120006,#120007);
#100920=AXIS2_PLACEMENT_3D('',#386807,#120008,#120009);
#100921=AXIS2_PLACEMENT_3D('',#386808,#120010,#120011);
#100922=AXIS2_PLACEMENT_3D('',#386821,#120012,#120013);
#100923=AXIS2_PLACEMENT_3D('',#386822,#120014,#120015);
#100924=AXIS2_PLACEMENT_3D('',#386832,#120017,#120018);
#100925=AXIS2_PLACEMENT_3D('',#386842,#120020,#120021);
#100926=AXIS2_PLACEMENT_3D('',#386845,#120022,#120023);
#100927=AXIS2_PLACEMENT_3D('',#386862,#120026,#120027);
#100928=AXIS2_PLACEMENT_3D('',#386912,#120028,#120029);
#100929=AXIS2_PLACEMENT_3D('',#386958,#120030,#120031);
#100930=AXIS2_PLACEMENT_3D('',#386975,#120032,#120033);
#100931=AXIS2_PLACEMENT_3D('',#387027,#120034,#120035);
#100932=AXIS2_PLACEMENT_3D('',#387028,#120036,#120037);
#100933=AXIS2_PLACEMENT_3D('',#387029,#120038,#120039);
#100934=AXIS2_PLACEMENT_3D('',#387030,#120040,#120041);
#100935=AXIS2_PLACEMENT_3D('',#387043,#120042,#120043);
#100936=AXIS2_PLACEMENT_3D('',#387044,#120044,#120045);
#100937=AXIS2_PLACEMENT_3D('',#387045,#120046,#120047);
#100938=AXIS2_PLACEMENT_3D('',#387058,#120048,#120049);
#100939=AXIS2_PLACEMENT_3D('',#387071,#120050,#120051);
#100940=AXIS2_PLACEMENT_3D('',#387084,#120052,#120053);
#100941=AXIS2_PLACEMENT_3D('',#387097,#120054,#120055);
#100942=AXIS2_PLACEMENT_3D('',#387110,#120056,#120057);
#100943=AXIS2_PLACEMENT_3D('',#387111,#120058,#120059);
#100944=AXIS2_PLACEMENT_3D('',#387112,#120060,#120061);
#100945=AXIS2_PLACEMENT_3D('',#387125,#120062,#120063);
#100946=AXIS2_PLACEMENT_3D('',#387126,#120064,#120065);
#100947=AXIS2_PLACEMENT_3D('',#387136,#120067,#120068);
#100948=AXIS2_PLACEMENT_3D('',#387146,#120070,#120071);
#100949=AXIS2_PLACEMENT_3D('',#387149,#120072,#120073);
#100950=AXIS2_PLACEMENT_3D('',#387166,#120076,#120077);
#100951=AXIS2_PLACEMENT_3D('',#387216,#120078,#120079);
#100952=AXIS2_PLACEMENT_3D('',#387262,#120080,#120081);
#100953=AXIS2_PLACEMENT_3D('',#387279,#120082,#120083);
#100954=AXIS2_PLACEMENT_3D('',#387331,#120084,#120085);
#100955=AXIS2_PLACEMENT_3D('',#387332,#120086,#120087);
#100956=AXIS2_PLACEMENT_3D('',#387333,#120088,#120089);
#100957=AXIS2_PLACEMENT_3D('',#387334,#120090,#120091);
#100958=AXIS2_PLACEMENT_3D('',#387347,#120092,#120093);
#100959=AXIS2_PLACEMENT_3D('',#387348,#120094,#120095);
#100960=AXIS2_PLACEMENT_3D('',#387349,#120096,#120097);
#100961=AXIS2_PLACEMENT_3D('',#387362,#120098,#120099);
#100962=AXIS2_PLACEMENT_3D('',#387375,#120100,#120101);
#100963=AXIS2_PLACEMENT_3D('',#387388,#120102,#120103);
#100964=AXIS2_PLACEMENT_3D('',#387401,#120104,#120105);
#100965=AXIS2_PLACEMENT_3D('',#387414,#120106,#120107);
#100966=AXIS2_PLACEMENT_3D('',#387415,#120108,#120109);
#100967=AXIS2_PLACEMENT_3D('',#387416,#120110,#120111);
#100968=AXIS2_PLACEMENT_3D('',#387429,#120112,#120113);
#100969=AXIS2_PLACEMENT_3D('',#387430,#120114,#120115);
#100970=AXIS2_PLACEMENT_3D('',#387440,#120117,#120118);
#100971=AXIS2_PLACEMENT_3D('',#387450,#120120,#120121);
#100972=AXIS2_PLACEMENT_3D('',#387453,#120122,#120123);
#100973=AXIS2_PLACEMENT_3D('',#387470,#120126,#120127);
#100974=AXIS2_PLACEMENT_3D('',#387520,#120128,#120129);
#100975=AXIS2_PLACEMENT_3D('',#387566,#120130,#120131);
#100976=AXIS2_PLACEMENT_3D('',#387583,#120132,#120133);
#100977=AXIS2_PLACEMENT_3D('',#387635,#120134,#120135);
#100978=AXIS2_PLACEMENT_3D('',#387636,#120136,#120137);
#100979=AXIS2_PLACEMENT_3D('',#387637,#120138,#120139);
#100980=AXIS2_PLACEMENT_3D('',#387638,#120140,#120141);
#100981=AXIS2_PLACEMENT_3D('',#387651,#120142,#120143);
#100982=AXIS2_PLACEMENT_3D('',#387652,#120144,#120145);
#100983=AXIS2_PLACEMENT_3D('',#387653,#120146,#120147);
#100984=AXIS2_PLACEMENT_3D('',#387666,#120148,#120149);
#100985=AXIS2_PLACEMENT_3D('',#387679,#120150,#120151);
#100986=AXIS2_PLACEMENT_3D('',#387692,#120152,#120153);
#100987=AXIS2_PLACEMENT_3D('',#387705,#120154,#120155);
#100988=AXIS2_PLACEMENT_3D('',#387718,#120156,#120157);
#100989=AXIS2_PLACEMENT_3D('',#387719,#120158,#120159);
#100990=AXIS2_PLACEMENT_3D('',#387720,#120160,#120161);
#100991=AXIS2_PLACEMENT_3D('',#387733,#120162,#120163);
#100992=AXIS2_PLACEMENT_3D('',#387734,#120164,#120165);
#100993=AXIS2_PLACEMENT_3D('',#387744,#120167,#120168);
#100994=AXIS2_PLACEMENT_3D('',#387754,#120170,#120171);
#100995=AXIS2_PLACEMENT_3D('',#387757,#120172,#120173);
#100996=AXIS2_PLACEMENT_3D('',#387774,#120176,#120177);
#100997=AXIS2_PLACEMENT_3D('',#387824,#120178,#120179);
#100998=AXIS2_PLACEMENT_3D('',#387870,#120180,#120181);
#100999=AXIS2_PLACEMENT_3D('',#387887,#120182,#120183);
#101000=AXIS2_PLACEMENT_3D('',#387939,#120184,#120185);
#101001=AXIS2_PLACEMENT_3D('',#387940,#120186,#120187);
#101002=AXIS2_PLACEMENT_3D('',#387941,#120188,#120189);
#101003=AXIS2_PLACEMENT_3D('',#387942,#120190,#120191);
#101004=AXIS2_PLACEMENT_3D('',#387955,#120192,#120193);
#101005=AXIS2_PLACEMENT_3D('',#387956,#120194,#120195);
#101006=AXIS2_PLACEMENT_3D('',#387957,#120196,#120197);
#101007=AXIS2_PLACEMENT_3D('',#387970,#120198,#120199);
#101008=AXIS2_PLACEMENT_3D('',#387983,#120200,#120201);
#101009=AXIS2_PLACEMENT_3D('',#387996,#120202,#120203);
#101010=AXIS2_PLACEMENT_3D('',#388009,#120204,#120205);
#101011=AXIS2_PLACEMENT_3D('',#388022,#120206,#120207);
#101012=AXIS2_PLACEMENT_3D('',#388023,#120208,#120209);
#101013=AXIS2_PLACEMENT_3D('',#388024,#120210,#120211);
#101014=AXIS2_PLACEMENT_3D('',#388037,#120212,#120213);
#101015=AXIS2_PLACEMENT_3D('',#388038,#120214,#120215);
#101016=AXIS2_PLACEMENT_3D('',#388048,#120217,#120218);
#101017=AXIS2_PLACEMENT_3D('',#388058,#120220,#120221);
#101018=AXIS2_PLACEMENT_3D('',#388061,#120222,#120223);
#101019=AXIS2_PLACEMENT_3D('',#388078,#120226,#120227);
#101020=AXIS2_PLACEMENT_3D('',#388128,#120228,#120229);
#101021=AXIS2_PLACEMENT_3D('',#388174,#120230,#120231);
#101022=AXIS2_PLACEMENT_3D('',#388191,#120232,#120233);
#101023=AXIS2_PLACEMENT_3D('',#388243,#120234,#120235);
#101024=AXIS2_PLACEMENT_3D('',#388244,#120236,#120237);
#101025=AXIS2_PLACEMENT_3D('',#388245,#120238,#120239);
#101026=AXIS2_PLACEMENT_3D('',#388246,#120240,#120241);
#101027=AXIS2_PLACEMENT_3D('',#388259,#120242,#120243);
#101028=AXIS2_PLACEMENT_3D('',#388260,#120244,#120245);
#101029=AXIS2_PLACEMENT_3D('',#388261,#120246,#120247);
#101030=AXIS2_PLACEMENT_3D('',#388274,#120248,#120249);
#101031=AXIS2_PLACEMENT_3D('',#388287,#120250,#120251);
#101032=AXIS2_PLACEMENT_3D('',#388300,#120252,#120253);
#101033=AXIS2_PLACEMENT_3D('',#388313,#120254,#120255);
#101034=AXIS2_PLACEMENT_3D('',#388326,#120256,#120257);
#101035=AXIS2_PLACEMENT_3D('',#388327,#120258,#120259);
#101036=AXIS2_PLACEMENT_3D('',#388328,#120260,#120261);
#101037=AXIS2_PLACEMENT_3D('',#388341,#120262,#120263);
#101038=AXIS2_PLACEMENT_3D('',#388342,#120264,#120265);
#101039=AXIS2_PLACEMENT_3D('',#388352,#120267,#120268);
#101040=AXIS2_PLACEMENT_3D('',#388362,#120270,#120271);
#101041=AXIS2_PLACEMENT_3D('',#388365,#120272,#120273);
#101042=AXIS2_PLACEMENT_3D('',#388382,#120276,#120277);
#101043=AXIS2_PLACEMENT_3D('',#388432,#120278,#120279);
#101044=AXIS2_PLACEMENT_3D('',#388478,#120280,#120281);
#101045=AXIS2_PLACEMENT_3D('',#388495,#120282,#120283);
#101046=AXIS2_PLACEMENT_3D('',#388547,#120284,#120285);
#101047=AXIS2_PLACEMENT_3D('',#388548,#120286,#120287);
#101048=AXIS2_PLACEMENT_3D('',#388549,#120288,#120289);
#101049=AXIS2_PLACEMENT_3D('',#388550,#120290,#120291);
#101050=AXIS2_PLACEMENT_3D('',#388563,#120292,#120293);
#101051=AXIS2_PLACEMENT_3D('',#388564,#120294,#120295);
#101052=AXIS2_PLACEMENT_3D('',#388565,#120296,#120297);
#101053=AXIS2_PLACEMENT_3D('',#388578,#120298,#120299);
#101054=AXIS2_PLACEMENT_3D('',#388591,#120300,#120301);
#101055=AXIS2_PLACEMENT_3D('',#388604,#120302,#120303);
#101056=AXIS2_PLACEMENT_3D('',#388617,#120304,#120305);
#101057=AXIS2_PLACEMENT_3D('',#388630,#120306,#120307);
#101058=AXIS2_PLACEMENT_3D('',#388631,#120308,#120309);
#101059=AXIS2_PLACEMENT_3D('',#388632,#120310,#120311);
#101060=AXIS2_PLACEMENT_3D('',#388645,#120312,#120313);
#101061=AXIS2_PLACEMENT_3D('',#388646,#120314,#120315);
#101062=AXIS2_PLACEMENT_3D('',#388656,#120317,#120318);
#101063=AXIS2_PLACEMENT_3D('',#388666,#120320,#120321);
#101064=AXIS2_PLACEMENT_3D('',#388669,#120322,#120323);
#101065=AXIS2_PLACEMENT_3D('',#388686,#120326,#120327);
#101066=AXIS2_PLACEMENT_3D('',#388736,#120328,#120329);
#101067=AXIS2_PLACEMENT_3D('',#388782,#120330,#120331);
#101068=AXIS2_PLACEMENT_3D('',#388799,#120332,#120333);
#101069=AXIS2_PLACEMENT_3D('',#388851,#120334,#120335);
#101070=AXIS2_PLACEMENT_3D('',#388852,#120336,#120337);
#101071=AXIS2_PLACEMENT_3D('',#388853,#120338,#120339);
#101072=AXIS2_PLACEMENT_3D('',#388854,#120340,#120341);
#101073=AXIS2_PLACEMENT_3D('',#388867,#120342,#120343);
#101074=AXIS2_PLACEMENT_3D('',#388868,#120344,#120345);
#101075=AXIS2_PLACEMENT_3D('',#388869,#120346,#120347);
#101076=AXIS2_PLACEMENT_3D('',#388882,#120348,#120349);
#101077=AXIS2_PLACEMENT_3D('',#388895,#120350,#120351);
#101078=AXIS2_PLACEMENT_3D('',#388908,#120352,#120353);
#101079=AXIS2_PLACEMENT_3D('',#388921,#120354,#120355);
#101080=AXIS2_PLACEMENT_3D('',#388934,#120356,#120357);
#101081=AXIS2_PLACEMENT_3D('',#388935,#120358,#120359);
#101082=AXIS2_PLACEMENT_3D('',#388936,#120360,#120361);
#101083=AXIS2_PLACEMENT_3D('',#388949,#120362,#120363);
#101084=AXIS2_PLACEMENT_3D('',#388950,#120364,#120365);
#101085=AXIS2_PLACEMENT_3D('',#388960,#120367,#120368);
#101086=AXIS2_PLACEMENT_3D('',#388970,#120370,#120371);
#101087=AXIS2_PLACEMENT_3D('',#388973,#120372,#120373);
#101088=AXIS2_PLACEMENT_3D('',#388990,#120376,#120377);
#101089=AXIS2_PLACEMENT_3D('',#389040,#120378,#120379);
#101090=AXIS2_PLACEMENT_3D('',#389086,#120380,#120381);
#101091=AXIS2_PLACEMENT_3D('',#389103,#120382,#120383);
#101092=AXIS2_PLACEMENT_3D('',#389155,#120384,#120385);
#101093=AXIS2_PLACEMENT_3D('',#389156,#120386,#120387);
#101094=AXIS2_PLACEMENT_3D('',#389157,#120388,#120389);
#101095=AXIS2_PLACEMENT_3D('',#389158,#120390,#120391);
#101096=AXIS2_PLACEMENT_3D('',#389171,#120392,#120393);
#101097=AXIS2_PLACEMENT_3D('',#389172,#120394,#120395);
#101098=AXIS2_PLACEMENT_3D('',#389173,#120396,#120397);
#101099=AXIS2_PLACEMENT_3D('',#389186,#120398,#120399);
#101100=AXIS2_PLACEMENT_3D('',#389199,#120400,#120401);
#101101=AXIS2_PLACEMENT_3D('',#389212,#120402,#120403);
#101102=AXIS2_PLACEMENT_3D('',#389225,#120404,#120405);
#101103=AXIS2_PLACEMENT_3D('',#389238,#120406,#120407);
#101104=AXIS2_PLACEMENT_3D('',#389239,#120408,#120409);
#101105=AXIS2_PLACEMENT_3D('',#389240,#120410,#120411);
#101106=AXIS2_PLACEMENT_3D('',#389253,#120412,#120413);
#101107=AXIS2_PLACEMENT_3D('',#389254,#120414,#120415);
#101108=AXIS2_PLACEMENT_3D('',#389264,#120417,#120418);
#101109=AXIS2_PLACEMENT_3D('',#389274,#120420,#120421);
#101110=AXIS2_PLACEMENT_3D('',#389277,#120422,#120423);
#101111=AXIS2_PLACEMENT_3D('',#389294,#120426,#120427);
#101112=AXIS2_PLACEMENT_3D('',#389344,#120428,#120429);
#101113=AXIS2_PLACEMENT_3D('',#389390,#120430,#120431);
#101114=AXIS2_PLACEMENT_3D('',#389407,#120432,#120433);
#101115=AXIS2_PLACEMENT_3D('',#389459,#120434,#120435);
#101116=AXIS2_PLACEMENT_3D('',#389460,#120436,#120437);
#101117=AXIS2_PLACEMENT_3D('',#389461,#120438,#120439);
#101118=AXIS2_PLACEMENT_3D('',#389462,#120440,#120441);
#101119=AXIS2_PLACEMENT_3D('',#389475,#120442,#120443);
#101120=AXIS2_PLACEMENT_3D('',#389476,#120444,#120445);
#101121=AXIS2_PLACEMENT_3D('',#389477,#120446,#120447);
#101122=AXIS2_PLACEMENT_3D('',#389490,#120448,#120449);
#101123=AXIS2_PLACEMENT_3D('',#389503,#120450,#120451);
#101124=AXIS2_PLACEMENT_3D('',#389516,#120452,#120453);
#101125=AXIS2_PLACEMENT_3D('',#389529,#120454,#120455);
#101126=AXIS2_PLACEMENT_3D('',#389542,#120456,#120457);
#101127=AXIS2_PLACEMENT_3D('',#389543,#120458,#120459);
#101128=AXIS2_PLACEMENT_3D('',#389544,#120460,#120461);
#101129=AXIS2_PLACEMENT_3D('',#389557,#120462,#120463);
#101130=AXIS2_PLACEMENT_3D('',#389558,#120464,#120465);
#101131=AXIS2_PLACEMENT_3D('',#389568,#120467,#120468);
#101132=AXIS2_PLACEMENT_3D('',#389578,#120470,#120471);
#101133=AXIS2_PLACEMENT_3D('',#389581,#120472,#120473);
#101134=AXIS2_PLACEMENT_3D('',#389598,#120476,#120477);
#101135=AXIS2_PLACEMENT_3D('',#389648,#120478,#120479);
#101136=AXIS2_PLACEMENT_3D('',#389694,#120480,#120481);
#101137=AXIS2_PLACEMENT_3D('',#389711,#120482,#120483);
#101138=AXIS2_PLACEMENT_3D('',#389763,#120484,#120485);
#101139=AXIS2_PLACEMENT_3D('',#389764,#120486,#120487);
#101140=AXIS2_PLACEMENT_3D('',#389765,#120488,#120489);
#101141=AXIS2_PLACEMENT_3D('',#389766,#120490,#120491);
#101142=AXIS2_PLACEMENT_3D('',#389779,#120492,#120493);
#101143=AXIS2_PLACEMENT_3D('',#389780,#120494,#120495);
#101144=AXIS2_PLACEMENT_3D('',#389781,#120496,#120497);
#101145=AXIS2_PLACEMENT_3D('',#389794,#120498,#120499);
#101146=AXIS2_PLACEMENT_3D('',#389807,#120500,#120501);
#101147=AXIS2_PLACEMENT_3D('',#389820,#120502,#120503);
#101148=AXIS2_PLACEMENT_3D('',#389833,#120504,#120505);
#101149=AXIS2_PLACEMENT_3D('',#389846,#120506,#120507);
#101150=AXIS2_PLACEMENT_3D('',#389847,#120508,#120509);
#101151=AXIS2_PLACEMENT_3D('',#389848,#120510,#120511);
#101152=AXIS2_PLACEMENT_3D('',#389861,#120512,#120513);
#101153=AXIS2_PLACEMENT_3D('',#389862,#120514,#120515);
#101154=AXIS2_PLACEMENT_3D('',#389872,#120517,#120518);
#101155=AXIS2_PLACEMENT_3D('',#389882,#120520,#120521);
#101156=AXIS2_PLACEMENT_3D('',#389885,#120522,#120523);
#101157=AXIS2_PLACEMENT_3D('',#389902,#120526,#120527);
#101158=AXIS2_PLACEMENT_3D('',#389952,#120528,#120529);
#101159=AXIS2_PLACEMENT_3D('',#389998,#120530,#120531);
#101160=AXIS2_PLACEMENT_3D('',#390015,#120532,#120533);
#101161=AXIS2_PLACEMENT_3D('',#390067,#120534,#120535);
#101162=AXIS2_PLACEMENT_3D('',#390068,#120536,#120537);
#101163=AXIS2_PLACEMENT_3D('',#390069,#120538,#120539);
#101164=AXIS2_PLACEMENT_3D('',#390070,#120540,#120541);
#101165=AXIS2_PLACEMENT_3D('',#390083,#120542,#120543);
#101166=AXIS2_PLACEMENT_3D('',#390084,#120544,#120545);
#101167=AXIS2_PLACEMENT_3D('',#390085,#120546,#120547);
#101168=AXIS2_PLACEMENT_3D('',#390098,#120548,#120549);
#101169=AXIS2_PLACEMENT_3D('',#390111,#120550,#120551);
#101170=AXIS2_PLACEMENT_3D('',#390124,#120552,#120553);
#101171=AXIS2_PLACEMENT_3D('',#390137,#120554,#120555);
#101172=AXIS2_PLACEMENT_3D('',#390150,#120556,#120557);
#101173=AXIS2_PLACEMENT_3D('',#390151,#120558,#120559);
#101174=AXIS2_PLACEMENT_3D('',#390152,#120560,#120561);
#101175=AXIS2_PLACEMENT_3D('',#390165,#120562,#120563);
#101176=AXIS2_PLACEMENT_3D('',#390166,#120564,#120565);
#101177=AXIS2_PLACEMENT_3D('',#390176,#120567,#120568);
#101178=AXIS2_PLACEMENT_3D('',#390186,#120570,#120571);
#101179=AXIS2_PLACEMENT_3D('',#390189,#120572,#120573);
#101180=AXIS2_PLACEMENT_3D('',#390206,#120576,#120577);
#101181=AXIS2_PLACEMENT_3D('',#390256,#120578,#120579);
#101182=AXIS2_PLACEMENT_3D('',#390302,#120580,#120581);
#101183=AXIS2_PLACEMENT_3D('',#390319,#120582,#120583);
#101184=AXIS2_PLACEMENT_3D('',#390371,#120584,#120585);
#101185=AXIS2_PLACEMENT_3D('',#390372,#120586,#120587);
#101186=AXIS2_PLACEMENT_3D('',#390373,#120588,#120589);
#101187=AXIS2_PLACEMENT_3D('',#390374,#120590,#120591);
#101188=AXIS2_PLACEMENT_3D('',#390387,#120592,#120593);
#101189=AXIS2_PLACEMENT_3D('',#390388,#120594,#120595);
#101190=AXIS2_PLACEMENT_3D('',#390389,#120596,#120597);
#101191=AXIS2_PLACEMENT_3D('',#390402,#120598,#120599);
#101192=AXIS2_PLACEMENT_3D('',#390415,#120600,#120601);
#101193=AXIS2_PLACEMENT_3D('',#390428,#120602,#120603);
#101194=AXIS2_PLACEMENT_3D('',#390441,#120604,#120605);
#101195=AXIS2_PLACEMENT_3D('',#390454,#120606,#120607);
#101196=AXIS2_PLACEMENT_3D('',#390455,#120608,#120609);
#101197=AXIS2_PLACEMENT_3D('',#390456,#120610,#120611);
#101198=AXIS2_PLACEMENT_3D('',#390469,#120612,#120613);
#101199=AXIS2_PLACEMENT_3D('',#390470,#120614,#120615);
#101200=AXIS2_PLACEMENT_3D('',#390480,#120617,#120618);
#101201=AXIS2_PLACEMENT_3D('',#390490,#120620,#120621);
#101202=AXIS2_PLACEMENT_3D('',#390493,#120622,#120623);
#101203=AXIS2_PLACEMENT_3D('',#390510,#120626,#120627);
#101204=AXIS2_PLACEMENT_3D('',#390560,#120628,#120629);
#101205=AXIS2_PLACEMENT_3D('',#390606,#120630,#120631);
#101206=AXIS2_PLACEMENT_3D('',#390623,#120632,#120633);
#101207=AXIS2_PLACEMENT_3D('',#390675,#120634,#120635);
#101208=AXIS2_PLACEMENT_3D('',#390676,#120636,#120637);
#101209=AXIS2_PLACEMENT_3D('',#390677,#120638,#120639);
#101210=AXIS2_PLACEMENT_3D('',#390678,#120640,#120641);
#101211=AXIS2_PLACEMENT_3D('',#390691,#120642,#120643);
#101212=AXIS2_PLACEMENT_3D('',#390692,#120644,#120645);
#101213=AXIS2_PLACEMENT_3D('',#390693,#120646,#120647);
#101214=AXIS2_PLACEMENT_3D('',#390706,#120648,#120649);
#101215=AXIS2_PLACEMENT_3D('',#390719,#120650,#120651);
#101216=AXIS2_PLACEMENT_3D('',#390732,#120652,#120653);
#101217=AXIS2_PLACEMENT_3D('',#390745,#120654,#120655);
#101218=AXIS2_PLACEMENT_3D('',#390758,#120656,#120657);
#101219=AXIS2_PLACEMENT_3D('',#390759,#120658,#120659);
#101220=AXIS2_PLACEMENT_3D('',#390760,#120660,#120661);
#101221=AXIS2_PLACEMENT_3D('',#390773,#120662,#120663);
#101222=AXIS2_PLACEMENT_3D('',#390774,#120664,#120665);
#101223=AXIS2_PLACEMENT_3D('',#390784,#120667,#120668);
#101224=AXIS2_PLACEMENT_3D('',#390794,#120670,#120671);
#101225=AXIS2_PLACEMENT_3D('',#390797,#120672,#120673);
#101226=AXIS2_PLACEMENT_3D('',#390814,#120676,#120677);
#101227=AXIS2_PLACEMENT_3D('',#390864,#120678,#120679);
#101228=AXIS2_PLACEMENT_3D('',#390910,#120680,#120681);
#101229=AXIS2_PLACEMENT_3D('',#390927,#120682,#120683);
#101230=AXIS2_PLACEMENT_3D('',#390979,#120684,#120685);
#101231=AXIS2_PLACEMENT_3D('',#390980,#120686,#120687);
#101232=AXIS2_PLACEMENT_3D('',#390981,#120688,#120689);
#101233=AXIS2_PLACEMENT_3D('',#390982,#120690,#120691);
#101234=AXIS2_PLACEMENT_3D('',#390995,#120692,#120693);
#101235=AXIS2_PLACEMENT_3D('',#390996,#120694,#120695);
#101236=AXIS2_PLACEMENT_3D('',#390997,#120696,#120697);
#101237=AXIS2_PLACEMENT_3D('',#391010,#120698,#120699);
#101238=AXIS2_PLACEMENT_3D('',#391023,#120700,#120701);
#101239=AXIS2_PLACEMENT_3D('',#391036,#120702,#120703);
#101240=AXIS2_PLACEMENT_3D('',#391049,#120704,#120705);
#101241=AXIS2_PLACEMENT_3D('',#391062,#120706,#120707);
#101242=AXIS2_PLACEMENT_3D('',#391063,#120708,#120709);
#101243=AXIS2_PLACEMENT_3D('',#391064,#120710,#120711);
#101244=AXIS2_PLACEMENT_3D('',#391077,#120712,#120713);
#101245=AXIS2_PLACEMENT_3D('',#391078,#120714,#120715);
#101246=AXIS2_PLACEMENT_3D('',#391088,#120717,#120718);
#101247=AXIS2_PLACEMENT_3D('',#391098,#120720,#120721);
#101248=AXIS2_PLACEMENT_3D('',#391101,#120722,#120723);
#101249=AXIS2_PLACEMENT_3D('',#391118,#120726,#120727);
#101250=AXIS2_PLACEMENT_3D('',#391168,#120728,#120729);
#101251=AXIS2_PLACEMENT_3D('',#391214,#120730,#120731);
#101252=AXIS2_PLACEMENT_3D('',#391231,#120732,#120733);
#101253=AXIS2_PLACEMENT_3D('',#391283,#120734,#120735);
#101254=AXIS2_PLACEMENT_3D('',#391284,#120736,#120737);
#101255=AXIS2_PLACEMENT_3D('',#391285,#120738,#120739);
#101256=AXIS2_PLACEMENT_3D('',#391286,#120740,#120741);
#101257=AXIS2_PLACEMENT_3D('',#391299,#120742,#120743);
#101258=AXIS2_PLACEMENT_3D('',#391300,#120744,#120745);
#101259=AXIS2_PLACEMENT_3D('',#391301,#120746,#120747);
#101260=AXIS2_PLACEMENT_3D('',#391314,#120748,#120749);
#101261=AXIS2_PLACEMENT_3D('',#391327,#120750,#120751);
#101262=AXIS2_PLACEMENT_3D('',#391340,#120752,#120753);
#101263=AXIS2_PLACEMENT_3D('',#391353,#120754,#120755);
#101264=AXIS2_PLACEMENT_3D('',#391366,#120756,#120757);
#101265=AXIS2_PLACEMENT_3D('',#391367,#120758,#120759);
#101266=AXIS2_PLACEMENT_3D('',#391368,#120760,#120761);
#101267=AXIS2_PLACEMENT_3D('',#391381,#120762,#120763);
#101268=AXIS2_PLACEMENT_3D('',#391382,#120764,#120765);
#101269=AXIS2_PLACEMENT_3D('',#391392,#120767,#120768);
#101270=AXIS2_PLACEMENT_3D('',#391402,#120770,#120771);
#101271=AXIS2_PLACEMENT_3D('',#391405,#120772,#120773);
#101272=AXIS2_PLACEMENT_3D('',#391422,#120776,#120777);
#101273=AXIS2_PLACEMENT_3D('',#391472,#120778,#120779);
#101274=AXIS2_PLACEMENT_3D('',#391518,#120780,#120781);
#101275=AXIS2_PLACEMENT_3D('',#391535,#120782,#120783);
#101276=AXIS2_PLACEMENT_3D('',#391587,#120784,#120785);
#101277=AXIS2_PLACEMENT_3D('',#391588,#120786,#120787);
#101278=AXIS2_PLACEMENT_3D('',#391589,#120788,#120789);
#101279=AXIS2_PLACEMENT_3D('',#391590,#120790,#120791);
#101280=AXIS2_PLACEMENT_3D('',#391603,#120792,#120793);
#101281=AXIS2_PLACEMENT_3D('',#391604,#120794,#120795);
#101282=AXIS2_PLACEMENT_3D('',#391605,#120796,#120797);
#101283=AXIS2_PLACEMENT_3D('',#391618,#120798,#120799);
#101284=AXIS2_PLACEMENT_3D('',#391631,#120800,#120801);
#101285=AXIS2_PLACEMENT_3D('',#391644,#120802,#120803);
#101286=AXIS2_PLACEMENT_3D('',#391657,#120804,#120805);
#101287=AXIS2_PLACEMENT_3D('',#391670,#120806,#120807);
#101288=AXIS2_PLACEMENT_3D('',#391671,#120808,#120809);
#101289=AXIS2_PLACEMENT_3D('',#391672,#120810,#120811);
#101290=AXIS2_PLACEMENT_3D('',#391685,#120812,#120813);
#101291=AXIS2_PLACEMENT_3D('',#391686,#120814,#120815);
#101292=AXIS2_PLACEMENT_3D('',#391696,#120817,#120818);
#101293=AXIS2_PLACEMENT_3D('',#391706,#120820,#120821);
#101294=AXIS2_PLACEMENT_3D('',#391709,#120822,#120823);
#101295=AXIS2_PLACEMENT_3D('',#391726,#120826,#120827);
#101296=AXIS2_PLACEMENT_3D('',#391776,#120828,#120829);
#101297=AXIS2_PLACEMENT_3D('',#391822,#120830,#120831);
#101298=AXIS2_PLACEMENT_3D('',#391839,#120832,#120833);
#101299=AXIS2_PLACEMENT_3D('',#391891,#120834,#120835);
#101300=AXIS2_PLACEMENT_3D('',#391892,#120836,#120837);
#101301=AXIS2_PLACEMENT_3D('',#391893,#120838,#120839);
#101302=AXIS2_PLACEMENT_3D('',#391894,#120840,#120841);
#101303=AXIS2_PLACEMENT_3D('',#391907,#120842,#120843);
#101304=AXIS2_PLACEMENT_3D('',#391908,#120844,#120845);
#101305=AXIS2_PLACEMENT_3D('',#391909,#120846,#120847);
#101306=AXIS2_PLACEMENT_3D('',#391922,#120848,#120849);
#101307=AXIS2_PLACEMENT_3D('',#391935,#120850,#120851);
#101308=AXIS2_PLACEMENT_3D('',#391948,#120852,#120853);
#101309=AXIS2_PLACEMENT_3D('',#391961,#120854,#120855);
#101310=AXIS2_PLACEMENT_3D('',#391974,#120856,#120857);
#101311=AXIS2_PLACEMENT_3D('',#391975,#120858,#120859);
#101312=AXIS2_PLACEMENT_3D('',#391976,#120860,#120861);
#101313=AXIS2_PLACEMENT_3D('',#391989,#120862,#120863);
#101314=AXIS2_PLACEMENT_3D('',#391990,#120864,#120865);
#101315=AXIS2_PLACEMENT_3D('',#392000,#120867,#120868);
#101316=AXIS2_PLACEMENT_3D('',#392010,#120870,#120871);
#101317=AXIS2_PLACEMENT_3D('',#392013,#120872,#120873);
#101318=AXIS2_PLACEMENT_3D('',#392030,#120876,#120877);
#101319=AXIS2_PLACEMENT_3D('',#392080,#120878,#120879);
#101320=AXIS2_PLACEMENT_3D('',#392126,#120880,#120881);
#101321=AXIS2_PLACEMENT_3D('',#392143,#120882,#120883);
#101322=AXIS2_PLACEMENT_3D('',#392195,#120884,#120885);
#101323=AXIS2_PLACEMENT_3D('',#392196,#120886,#120887);
#101324=AXIS2_PLACEMENT_3D('',#392197,#120888,#120889);
#101325=AXIS2_PLACEMENT_3D('',#392198,#120890,#120891);
#101326=AXIS2_PLACEMENT_3D('',#392211,#120892,#120893);
#101327=AXIS2_PLACEMENT_3D('',#392212,#120894,#120895);
#101328=AXIS2_PLACEMENT_3D('',#392213,#120896,#120897);
#101329=AXIS2_PLACEMENT_3D('',#392226,#120898,#120899);
#101330=AXIS2_PLACEMENT_3D('',#392239,#120900,#120901);
#101331=AXIS2_PLACEMENT_3D('',#392252,#120902,#120903);
#101332=AXIS2_PLACEMENT_3D('',#392265,#120904,#120905);
#101333=AXIS2_PLACEMENT_3D('',#392278,#120906,#120907);
#101334=AXIS2_PLACEMENT_3D('',#392279,#120908,#120909);
#101335=AXIS2_PLACEMENT_3D('',#392280,#120910,#120911);
#101336=AXIS2_PLACEMENT_3D('',#392293,#120912,#120913);
#101337=AXIS2_PLACEMENT_3D('',#392294,#120914,#120915);
#101338=AXIS2_PLACEMENT_3D('',#392304,#120917,#120918);
#101339=AXIS2_PLACEMENT_3D('',#392314,#120920,#120921);
#101340=AXIS2_PLACEMENT_3D('',#392317,#120922,#120923);
#101341=AXIS2_PLACEMENT_3D('',#392334,#120926,#120927);
#101342=AXIS2_PLACEMENT_3D('',#392384,#120928,#120929);
#101343=AXIS2_PLACEMENT_3D('',#392430,#120930,#120931);
#101344=AXIS2_PLACEMENT_3D('',#392447,#120932,#120933);
#101345=AXIS2_PLACEMENT_3D('',#392499,#120934,#120935);
#101346=AXIS2_PLACEMENT_3D('',#392500,#120936,#120937);
#101347=AXIS2_PLACEMENT_3D('',#392501,#120938,#120939);
#101348=AXIS2_PLACEMENT_3D('',#392502,#120940,#120941);
#101349=AXIS2_PLACEMENT_3D('',#392515,#120942,#120943);
#101350=AXIS2_PLACEMENT_3D('',#392516,#120944,#120945);
#101351=AXIS2_PLACEMENT_3D('',#392517,#120946,#120947);
#101352=AXIS2_PLACEMENT_3D('',#392530,#120948,#120949);
#101353=AXIS2_PLACEMENT_3D('',#392543,#120950,#120951);
#101354=AXIS2_PLACEMENT_3D('',#392556,#120952,#120953);
#101355=AXIS2_PLACEMENT_3D('',#392569,#120954,#120955);
#101356=AXIS2_PLACEMENT_3D('',#392582,#120956,#120957);
#101357=AXIS2_PLACEMENT_3D('',#392583,#120958,#120959);
#101358=AXIS2_PLACEMENT_3D('',#392584,#120960,#120961);
#101359=AXIS2_PLACEMENT_3D('',#392597,#120962,#120963);
#101360=AXIS2_PLACEMENT_3D('',#392598,#120964,#120965);
#101361=AXIS2_PLACEMENT_3D('',#392608,#120967,#120968);
#101362=AXIS2_PLACEMENT_3D('',#392618,#120970,#120971);
#101363=AXIS2_PLACEMENT_3D('',#392621,#120972,#120973);
#101364=AXIS2_PLACEMENT_3D('',#392638,#120976,#120977);
#101365=AXIS2_PLACEMENT_3D('',#392688,#120978,#120979);
#101366=AXIS2_PLACEMENT_3D('',#392734,#120980,#120981);
#101367=AXIS2_PLACEMENT_3D('',#392751,#120982,#120983);
#101368=AXIS2_PLACEMENT_3D('',#392803,#120984,#120985);
#101369=AXIS2_PLACEMENT_3D('',#392804,#120986,#120987);
#101370=AXIS2_PLACEMENT_3D('',#392805,#120988,#120989);
#101371=AXIS2_PLACEMENT_3D('',#392806,#120990,#120991);
#101372=AXIS2_PLACEMENT_3D('',#392819,#120992,#120993);
#101373=AXIS2_PLACEMENT_3D('',#392820,#120994,#120995);
#101374=AXIS2_PLACEMENT_3D('',#392821,#120996,#120997);
#101375=AXIS2_PLACEMENT_3D('',#392834,#120998,#120999);
#101376=AXIS2_PLACEMENT_3D('',#392847,#121000,#121001);
#101377=AXIS2_PLACEMENT_3D('',#392860,#121002,#121003);
#101378=AXIS2_PLACEMENT_3D('',#392873,#121004,#121005);
#101379=AXIS2_PLACEMENT_3D('',#392886,#121006,#121007);
#101380=AXIS2_PLACEMENT_3D('',#392887,#121008,#121009);
#101381=AXIS2_PLACEMENT_3D('',#392888,#121010,#121011);
#101382=AXIS2_PLACEMENT_3D('',#392901,#121012,#121013);
#101383=AXIS2_PLACEMENT_3D('',#392902,#121014,#121015);
#101384=AXIS2_PLACEMENT_3D('',#392912,#121017,#121018);
#101385=AXIS2_PLACEMENT_3D('',#392922,#121020,#121021);
#101386=AXIS2_PLACEMENT_3D('',#392925,#121022,#121023);
#101387=AXIS2_PLACEMENT_3D('',#392942,#121026,#121027);
#101388=AXIS2_PLACEMENT_3D('',#392992,#121028,#121029);
#101389=AXIS2_PLACEMENT_3D('',#393038,#121030,#121031);
#101390=AXIS2_PLACEMENT_3D('',#393055,#121032,#121033);
#101391=AXIS2_PLACEMENT_3D('',#393107,#121034,#121035);
#101392=AXIS2_PLACEMENT_3D('',#393108,#121036,#121037);
#101393=AXIS2_PLACEMENT_3D('',#393109,#121038,#121039);
#101394=AXIS2_PLACEMENT_3D('',#393110,#121040,#121041);
#101395=AXIS2_PLACEMENT_3D('',#393123,#121042,#121043);
#101396=AXIS2_PLACEMENT_3D('',#393124,#121044,#121045);
#101397=AXIS2_PLACEMENT_3D('',#393125,#121046,#121047);
#101398=AXIS2_PLACEMENT_3D('',#393138,#121048,#121049);
#101399=AXIS2_PLACEMENT_3D('',#393151,#121050,#121051);
#101400=AXIS2_PLACEMENT_3D('',#393164,#121052,#121053);
#101401=AXIS2_PLACEMENT_3D('',#393177,#121054,#121055);
#101402=AXIS2_PLACEMENT_3D('',#393190,#121056,#121057);
#101403=AXIS2_PLACEMENT_3D('',#393191,#121058,#121059);
#101404=AXIS2_PLACEMENT_3D('',#393192,#121060,#121061);
#101405=AXIS2_PLACEMENT_3D('',#393205,#121062,#121063);
#101406=AXIS2_PLACEMENT_3D('',#393206,#121064,#121065);
#101407=AXIS2_PLACEMENT_3D('',#393216,#121067,#121068);
#101408=AXIS2_PLACEMENT_3D('',#393226,#121070,#121071);
#101409=AXIS2_PLACEMENT_3D('',#393229,#121072,#121073);
#101410=AXIS2_PLACEMENT_3D('',#393246,#121076,#121077);
#101411=AXIS2_PLACEMENT_3D('',#393296,#121078,#121079);
#101412=AXIS2_PLACEMENT_3D('',#393342,#121080,#121081);
#101413=AXIS2_PLACEMENT_3D('',#393359,#121082,#121083);
#101414=AXIS2_PLACEMENT_3D('',#393411,#121084,#121085);
#101415=AXIS2_PLACEMENT_3D('',#393412,#121086,#121087);
#101416=AXIS2_PLACEMENT_3D('',#393413,#121088,#121089);
#101417=AXIS2_PLACEMENT_3D('',#393414,#121090,#121091);
#101418=AXIS2_PLACEMENT_3D('',#393427,#121092,#121093);
#101419=AXIS2_PLACEMENT_3D('',#393428,#121094,#121095);
#101420=AXIS2_PLACEMENT_3D('',#393429,#121096,#121097);
#101421=AXIS2_PLACEMENT_3D('',#393442,#121098,#121099);
#101422=AXIS2_PLACEMENT_3D('',#393455,#121100,#121101);
#101423=AXIS2_PLACEMENT_3D('',#393468,#121102,#121103);
#101424=AXIS2_PLACEMENT_3D('',#393481,#121104,#121105);
#101425=AXIS2_PLACEMENT_3D('',#393494,#121106,#121107);
#101426=AXIS2_PLACEMENT_3D('',#393495,#121108,#121109);
#101427=AXIS2_PLACEMENT_3D('',#393496,#121110,#121111);
#101428=AXIS2_PLACEMENT_3D('',#393509,#121112,#121113);
#101429=AXIS2_PLACEMENT_3D('',#393510,#121114,#121115);
#101430=AXIS2_PLACEMENT_3D('',#393520,#121117,#121118);
#101431=AXIS2_PLACEMENT_3D('',#393530,#121120,#121121);
#101432=AXIS2_PLACEMENT_3D('',#393533,#121122,#121123);
#101433=AXIS2_PLACEMENT_3D('',#393550,#121126,#121127);
#101434=AXIS2_PLACEMENT_3D('',#393600,#121128,#121129);
#101435=AXIS2_PLACEMENT_3D('',#393646,#121130,#121131);
#101436=AXIS2_PLACEMENT_3D('',#393663,#121132,#121133);
#101437=AXIS2_PLACEMENT_3D('',#393715,#121134,#121135);
#101438=AXIS2_PLACEMENT_3D('',#393716,#121136,#121137);
#101439=AXIS2_PLACEMENT_3D('',#393717,#121138,#121139);
#101440=AXIS2_PLACEMENT_3D('',#393718,#121140,#121141);
#101441=AXIS2_PLACEMENT_3D('',#393731,#121142,#121143);
#101442=AXIS2_PLACEMENT_3D('',#393732,#121144,#121145);
#101443=AXIS2_PLACEMENT_3D('',#393733,#121146,#121147);
#101444=AXIS2_PLACEMENT_3D('',#393746,#121148,#121149);
#101445=AXIS2_PLACEMENT_3D('',#393759,#121150,#121151);
#101446=AXIS2_PLACEMENT_3D('',#393772,#121152,#121153);
#101447=AXIS2_PLACEMENT_3D('',#393785,#121154,#121155);
#101448=AXIS2_PLACEMENT_3D('',#393798,#121156,#121157);
#101449=AXIS2_PLACEMENT_3D('',#393799,#121158,#121159);
#101450=AXIS2_PLACEMENT_3D('',#393800,#121160,#121161);
#101451=AXIS2_PLACEMENT_3D('',#393813,#121162,#121163);
#101452=AXIS2_PLACEMENT_3D('',#393814,#121164,#121165);
#101453=AXIS2_PLACEMENT_3D('',#393824,#121167,#121168);
#101454=AXIS2_PLACEMENT_3D('',#393834,#121170,#121171);
#101455=AXIS2_PLACEMENT_3D('',#393837,#121172,#121173);
#101456=AXIS2_PLACEMENT_3D('',#393854,#121176,#121177);
#101457=AXIS2_PLACEMENT_3D('',#393904,#121178,#121179);
#101458=AXIS2_PLACEMENT_3D('',#393950,#121180,#121181);
#101459=AXIS2_PLACEMENT_3D('',#393967,#121182,#121183);
#101460=AXIS2_PLACEMENT_3D('',#394019,#121184,#121185);
#101461=AXIS2_PLACEMENT_3D('',#394020,#121186,#121187);
#101462=AXIS2_PLACEMENT_3D('',#394021,#121188,#121189);
#101463=AXIS2_PLACEMENT_3D('',#394022,#121190,#121191);
#101464=AXIS2_PLACEMENT_3D('',#394035,#121192,#121193);
#101465=AXIS2_PLACEMENT_3D('',#394036,#121194,#121195);
#101466=AXIS2_PLACEMENT_3D('',#394037,#121196,#121197);
#101467=AXIS2_PLACEMENT_3D('',#394050,#121198,#121199);
#101468=AXIS2_PLACEMENT_3D('',#394063,#121200,#121201);
#101469=AXIS2_PLACEMENT_3D('',#394076,#121202,#121203);
#101470=AXIS2_PLACEMENT_3D('',#394089,#121204,#121205);
#101471=AXIS2_PLACEMENT_3D('',#394102,#121206,#121207);
#101472=AXIS2_PLACEMENT_3D('',#394103,#121208,#121209);
#101473=AXIS2_PLACEMENT_3D('',#394104,#121210,#121211);
#101474=AXIS2_PLACEMENT_3D('',#394117,#121212,#121213);
#101475=AXIS2_PLACEMENT_3D('',#394118,#121214,#121215);
#101476=AXIS2_PLACEMENT_3D('',#394128,#121217,#121218);
#101477=AXIS2_PLACEMENT_3D('',#394138,#121220,#121221);
#101478=AXIS2_PLACEMENT_3D('',#394141,#121222,#121223);
#101479=AXIS2_PLACEMENT_3D('',#394158,#121226,#121227);
#101480=AXIS2_PLACEMENT_3D('',#394208,#121228,#121229);
#101481=AXIS2_PLACEMENT_3D('',#394254,#121230,#121231);
#101482=AXIS2_PLACEMENT_3D('',#394271,#121232,#121233);
#101483=AXIS2_PLACEMENT_3D('',#394323,#121234,#121235);
#101484=AXIS2_PLACEMENT_3D('',#394324,#121236,#121237);
#101485=AXIS2_PLACEMENT_3D('',#394325,#121238,#121239);
#101486=AXIS2_PLACEMENT_3D('',#394326,#121240,#121241);
#101487=AXIS2_PLACEMENT_3D('',#394339,#121242,#121243);
#101488=AXIS2_PLACEMENT_3D('',#394340,#121244,#121245);
#101489=AXIS2_PLACEMENT_3D('',#394341,#121246,#121247);
#101490=AXIS2_PLACEMENT_3D('',#394354,#121248,#121249);
#101491=AXIS2_PLACEMENT_3D('',#394367,#121250,#121251);
#101492=AXIS2_PLACEMENT_3D('',#394380,#121252,#121253);
#101493=AXIS2_PLACEMENT_3D('',#394393,#121254,#121255);
#101494=AXIS2_PLACEMENT_3D('',#394406,#121256,#121257);
#101495=AXIS2_PLACEMENT_3D('',#394407,#121258,#121259);
#101496=AXIS2_PLACEMENT_3D('',#394408,#121260,#121261);
#101497=AXIS2_PLACEMENT_3D('',#394421,#121262,#121263);
#101498=AXIS2_PLACEMENT_3D('',#394422,#121264,#121265);
#101499=AXIS2_PLACEMENT_3D('',#394432,#121267,#121268);
#101500=AXIS2_PLACEMENT_3D('',#394442,#121270,#121271);
#101501=AXIS2_PLACEMENT_3D('',#394445,#121272,#121273);
#101502=AXIS2_PLACEMENT_3D('',#394462,#121276,#121277);
#101503=AXIS2_PLACEMENT_3D('',#394512,#121278,#121279);
#101504=AXIS2_PLACEMENT_3D('',#394558,#121280,#121281);
#101505=AXIS2_PLACEMENT_3D('',#394575,#121282,#121283);
#101506=AXIS2_PLACEMENT_3D('',#394627,#121284,#121285);
#101507=AXIS2_PLACEMENT_3D('',#394628,#121286,#121287);
#101508=AXIS2_PLACEMENT_3D('',#394629,#121288,#121289);
#101509=AXIS2_PLACEMENT_3D('',#394630,#121290,#121291);
#101510=AXIS2_PLACEMENT_3D('',#394643,#121292,#121293);
#101511=AXIS2_PLACEMENT_3D('',#394644,#121294,#121295);
#101512=AXIS2_PLACEMENT_3D('',#394645,#121296,#121297);
#101513=AXIS2_PLACEMENT_3D('',#394658,#121298,#121299);
#101514=AXIS2_PLACEMENT_3D('',#394671,#121300,#121301);
#101515=AXIS2_PLACEMENT_3D('',#394684,#121302,#121303);
#101516=AXIS2_PLACEMENT_3D('',#394697,#121304,#121305);
#101517=AXIS2_PLACEMENT_3D('',#394710,#121306,#121307);
#101518=AXIS2_PLACEMENT_3D('',#394711,#121308,#121309);
#101519=AXIS2_PLACEMENT_3D('',#394712,#121310,#121311);
#101520=AXIS2_PLACEMENT_3D('',#394725,#121312,#121313);
#101521=AXIS2_PLACEMENT_3D('',#394726,#121314,#121315);
#101522=AXIS2_PLACEMENT_3D('',#394736,#121317,#121318);
#101523=AXIS2_PLACEMENT_3D('',#394746,#121320,#121321);
#101524=AXIS2_PLACEMENT_3D('',#394749,#121322,#121323);
#101525=AXIS2_PLACEMENT_3D('',#394766,#121326,#121327);
#101526=AXIS2_PLACEMENT_3D('',#394816,#121328,#121329);
#101527=AXIS2_PLACEMENT_3D('',#394862,#121330,#121331);
#101528=AXIS2_PLACEMENT_3D('',#394879,#121332,#121333);
#101529=AXIS2_PLACEMENT_3D('',#394931,#121334,#121335);
#101530=AXIS2_PLACEMENT_3D('',#394932,#121336,#121337);
#101531=AXIS2_PLACEMENT_3D('',#394933,#121338,#121339);
#101532=AXIS2_PLACEMENT_3D('',#394934,#121340,#121341);
#101533=AXIS2_PLACEMENT_3D('',#394947,#121342,#121343);
#101534=AXIS2_PLACEMENT_3D('',#394948,#121344,#121345);
#101535=AXIS2_PLACEMENT_3D('',#394949,#121346,#121347);
#101536=AXIS2_PLACEMENT_3D('',#394962,#121348,#121349);
#101537=AXIS2_PLACEMENT_3D('',#394975,#121350,#121351);
#101538=AXIS2_PLACEMENT_3D('',#394988,#121352,#121353);
#101539=AXIS2_PLACEMENT_3D('',#395001,#121354,#121355);
#101540=AXIS2_PLACEMENT_3D('',#395014,#121356,#121357);
#101541=AXIS2_PLACEMENT_3D('',#395015,#121358,#121359);
#101542=AXIS2_PLACEMENT_3D('',#395016,#121360,#121361);
#101543=AXIS2_PLACEMENT_3D('',#395029,#121362,#121363);
#101544=AXIS2_PLACEMENT_3D('',#395030,#121364,#121365);
#101545=AXIS2_PLACEMENT_3D('',#395040,#121367,#121368);
#101546=AXIS2_PLACEMENT_3D('',#395050,#121370,#121371);
#101547=AXIS2_PLACEMENT_3D('',#395053,#121372,#121373);
#101548=AXIS2_PLACEMENT_3D('',#395070,#121376,#121377);
#101549=AXIS2_PLACEMENT_3D('',#395120,#121378,#121379);
#101550=AXIS2_PLACEMENT_3D('',#395166,#121380,#121381);
#101551=AXIS2_PLACEMENT_3D('',#395183,#121382,#121383);
#101552=AXIS2_PLACEMENT_3D('',#395235,#121384,#121385);
#101553=AXIS2_PLACEMENT_3D('',#395236,#121386,#121387);
#101554=AXIS2_PLACEMENT_3D('',#395237,#121388,#121389);
#101555=AXIS2_PLACEMENT_3D('',#395238,#121390,#121391);
#101556=AXIS2_PLACEMENT_3D('',#395251,#121392,#121393);
#101557=AXIS2_PLACEMENT_3D('',#395252,#121394,#121395);
#101558=AXIS2_PLACEMENT_3D('',#395253,#121396,#121397);
#101559=AXIS2_PLACEMENT_3D('',#395266,#121398,#121399);
#101560=AXIS2_PLACEMENT_3D('',#395279,#121400,#121401);
#101561=AXIS2_PLACEMENT_3D('',#395292,#121402,#121403);
#101562=AXIS2_PLACEMENT_3D('',#395305,#121404,#121405);
#101563=AXIS2_PLACEMENT_3D('',#395318,#121406,#121407);
#101564=AXIS2_PLACEMENT_3D('',#395319,#121408,#121409);
#101565=AXIS2_PLACEMENT_3D('',#395320,#121410,#121411);
#101566=AXIS2_PLACEMENT_3D('',#395333,#121412,#121413);
#101567=AXIS2_PLACEMENT_3D('',#395334,#121414,#121415);
#101568=AXIS2_PLACEMENT_3D('',#395344,#121417,#121418);
#101569=AXIS2_PLACEMENT_3D('',#395354,#121420,#121421);
#101570=AXIS2_PLACEMENT_3D('',#395357,#121422,#121423);
#101571=AXIS2_PLACEMENT_3D('',#395374,#121426,#121427);
#101572=AXIS2_PLACEMENT_3D('',#395424,#121428,#121429);
#101573=AXIS2_PLACEMENT_3D('',#395470,#121430,#121431);
#101574=AXIS2_PLACEMENT_3D('',#395487,#121432,#121433);
#101575=AXIS2_PLACEMENT_3D('',#395539,#121434,#121435);
#101576=AXIS2_PLACEMENT_3D('',#395540,#121436,#121437);
#101577=AXIS2_PLACEMENT_3D('',#395541,#121438,#121439);
#101578=AXIS2_PLACEMENT_3D('',#395542,#121440,#121441);
#101579=AXIS2_PLACEMENT_3D('',#395555,#121442,#121443);
#101580=AXIS2_PLACEMENT_3D('',#395556,#121444,#121445);
#101581=AXIS2_PLACEMENT_3D('',#395557,#121446,#121447);
#101582=AXIS2_PLACEMENT_3D('',#395570,#121448,#121449);
#101583=AXIS2_PLACEMENT_3D('',#395583,#121450,#121451);
#101584=AXIS2_PLACEMENT_3D('',#395596,#121452,#121453);
#101585=AXIS2_PLACEMENT_3D('',#395609,#121454,#121455);
#101586=AXIS2_PLACEMENT_3D('',#395622,#121456,#121457);
#101587=AXIS2_PLACEMENT_3D('',#395623,#121458,#121459);
#101588=AXIS2_PLACEMENT_3D('',#395624,#121460,#121461);
#101589=AXIS2_PLACEMENT_3D('',#395637,#121462,#121463);
#101590=AXIS2_PLACEMENT_3D('',#395638,#121464,#121465);
#101591=AXIS2_PLACEMENT_3D('',#395648,#121467,#121468);
#101592=AXIS2_PLACEMENT_3D('',#395658,#121470,#121471);
#101593=AXIS2_PLACEMENT_3D('',#395661,#121472,#121473);
#101594=AXIS2_PLACEMENT_3D('',#395678,#121476,#121477);
#101595=AXIS2_PLACEMENT_3D('',#395728,#121478,#121479);
#101596=AXIS2_PLACEMENT_3D('',#395774,#121480,#121481);
#101597=AXIS2_PLACEMENT_3D('',#395791,#121482,#121483);
#101598=AXIS2_PLACEMENT_3D('',#395843,#121484,#121485);
#101599=AXIS2_PLACEMENT_3D('',#395844,#121486,#121487);
#101600=AXIS2_PLACEMENT_3D('',#395845,#121488,#121489);
#101601=AXIS2_PLACEMENT_3D('',#395846,#121490,#121491);
#101602=AXIS2_PLACEMENT_3D('',#395859,#121492,#121493);
#101603=AXIS2_PLACEMENT_3D('',#395860,#121494,#121495);
#101604=AXIS2_PLACEMENT_3D('',#395861,#121496,#121497);
#101605=AXIS2_PLACEMENT_3D('',#395874,#121498,#121499);
#101606=AXIS2_PLACEMENT_3D('',#395887,#121500,#121501);
#101607=AXIS2_PLACEMENT_3D('',#395900,#121502,#121503);
#101608=AXIS2_PLACEMENT_3D('',#395913,#121504,#121505);
#101609=AXIS2_PLACEMENT_3D('',#395926,#121506,#121507);
#101610=AXIS2_PLACEMENT_3D('',#395927,#121508,#121509);
#101611=AXIS2_PLACEMENT_3D('',#395928,#121510,#121511);
#101612=AXIS2_PLACEMENT_3D('',#395941,#121512,#121513);
#101613=AXIS2_PLACEMENT_3D('',#395942,#121514,#121515);
#101614=AXIS2_PLACEMENT_3D('',#395952,#121517,#121518);
#101615=AXIS2_PLACEMENT_3D('',#395962,#121520,#121521);
#101616=AXIS2_PLACEMENT_3D('',#395965,#121522,#121523);
#101617=AXIS2_PLACEMENT_3D('',#395982,#121526,#121527);
#101618=AXIS2_PLACEMENT_3D('',#396032,#121528,#121529);
#101619=AXIS2_PLACEMENT_3D('',#396078,#121530,#121531);
#101620=AXIS2_PLACEMENT_3D('',#396095,#121532,#121533);
#101621=AXIS2_PLACEMENT_3D('',#396147,#121534,#121535);
#101622=AXIS2_PLACEMENT_3D('',#396148,#121536,#121537);
#101623=AXIS2_PLACEMENT_3D('',#396149,#121538,#121539);
#101624=AXIS2_PLACEMENT_3D('',#396150,#121540,#121541);
#101625=AXIS2_PLACEMENT_3D('',#396163,#121542,#121543);
#101626=AXIS2_PLACEMENT_3D('',#396164,#121544,#121545);
#101627=AXIS2_PLACEMENT_3D('',#396165,#121546,#121547);
#101628=AXIS2_PLACEMENT_3D('',#396178,#121548,#121549);
#101629=AXIS2_PLACEMENT_3D('',#396191,#121550,#121551);
#101630=AXIS2_PLACEMENT_3D('',#396204,#121552,#121553);
#101631=AXIS2_PLACEMENT_3D('',#396217,#121554,#121555);
#101632=AXIS2_PLACEMENT_3D('',#396230,#121556,#121557);
#101633=AXIS2_PLACEMENT_3D('',#396231,#121558,#121559);
#101634=AXIS2_PLACEMENT_3D('',#396232,#121560,#121561);
#101635=AXIS2_PLACEMENT_3D('',#396245,#121562,#121563);
#101636=AXIS2_PLACEMENT_3D('',#396246,#121564,#121565);
#101637=AXIS2_PLACEMENT_3D('',#396256,#121567,#121568);
#101638=AXIS2_PLACEMENT_3D('',#396266,#121570,#121571);
#101639=AXIS2_PLACEMENT_3D('',#396269,#121572,#121573);
#101640=AXIS2_PLACEMENT_3D('',#396286,#121576,#121577);
#101641=AXIS2_PLACEMENT_3D('',#396336,#121578,#121579);
#101642=AXIS2_PLACEMENT_3D('',#396382,#121580,#121581);
#101643=AXIS2_PLACEMENT_3D('',#396399,#121582,#121583);
#101644=AXIS2_PLACEMENT_3D('',#396451,#121584,#121585);
#101645=AXIS2_PLACEMENT_3D('',#396452,#121586,#121587);
#101646=AXIS2_PLACEMENT_3D('',#396453,#121588,#121589);
#101647=AXIS2_PLACEMENT_3D('',#396454,#121590,#121591);
#101648=AXIS2_PLACEMENT_3D('',#396467,#121592,#121593);
#101649=AXIS2_PLACEMENT_3D('',#396468,#121594,#121595);
#101650=AXIS2_PLACEMENT_3D('',#396469,#121596,#121597);
#101651=AXIS2_PLACEMENT_3D('',#396482,#121598,#121599);
#101652=AXIS2_PLACEMENT_3D('',#396495,#121600,#121601);
#101653=AXIS2_PLACEMENT_3D('',#396508,#121602,#121603);
#101654=AXIS2_PLACEMENT_3D('',#396521,#121604,#121605);
#101655=AXIS2_PLACEMENT_3D('',#396534,#121606,#121607);
#101656=AXIS2_PLACEMENT_3D('',#396535,#121608,#121609);
#101657=AXIS2_PLACEMENT_3D('',#396536,#121610,#121611);
#101658=AXIS2_PLACEMENT_3D('',#396549,#121612,#121613);
#101659=AXIS2_PLACEMENT_3D('',#396550,#121614,#121615);
#101660=AXIS2_PLACEMENT_3D('',#396560,#121617,#121618);
#101661=AXIS2_PLACEMENT_3D('',#396570,#121620,#121621);
#101662=AXIS2_PLACEMENT_3D('',#396573,#121622,#121623);
#101663=AXIS2_PLACEMENT_3D('',#396590,#121626,#121627);
#101664=AXIS2_PLACEMENT_3D('',#396640,#121628,#121629);
#101665=AXIS2_PLACEMENT_3D('',#396686,#121630,#121631);
#101666=AXIS2_PLACEMENT_3D('',#396703,#121632,#121633);
#101667=AXIS2_PLACEMENT_3D('',#396755,#121634,#121635);
#101668=AXIS2_PLACEMENT_3D('',#396756,#121636,#121637);
#101669=AXIS2_PLACEMENT_3D('',#396757,#121638,#121639);
#101670=AXIS2_PLACEMENT_3D('',#396758,#121640,#121641);
#101671=AXIS2_PLACEMENT_3D('',#396771,#121642,#121643);
#101672=AXIS2_PLACEMENT_3D('',#396772,#121644,#121645);
#101673=AXIS2_PLACEMENT_3D('',#396773,#121646,#121647);
#101674=AXIS2_PLACEMENT_3D('',#396786,#121648,#121649);
#101675=AXIS2_PLACEMENT_3D('',#396799,#121650,#121651);
#101676=AXIS2_PLACEMENT_3D('',#396812,#121652,#121653);
#101677=AXIS2_PLACEMENT_3D('',#396825,#121654,#121655);
#101678=AXIS2_PLACEMENT_3D('',#396838,#121656,#121657);
#101679=AXIS2_PLACEMENT_3D('',#396839,#121658,#121659);
#101680=AXIS2_PLACEMENT_3D('',#396840,#121660,#121661);
#101681=AXIS2_PLACEMENT_3D('',#396853,#121662,#121663);
#101682=AXIS2_PLACEMENT_3D('',#396854,#121664,#121665);
#101683=AXIS2_PLACEMENT_3D('',#396864,#121667,#121668);
#101684=AXIS2_PLACEMENT_3D('',#396874,#121670,#121671);
#101685=AXIS2_PLACEMENT_3D('',#396877,#121672,#121673);
#101686=AXIS2_PLACEMENT_3D('',#396894,#121676,#121677);
#101687=AXIS2_PLACEMENT_3D('',#396944,#121678,#121679);
#101688=AXIS2_PLACEMENT_3D('',#396990,#121680,#121681);
#101689=AXIS2_PLACEMENT_3D('',#397007,#121682,#121683);
#101690=AXIS2_PLACEMENT_3D('',#397059,#121684,#121685);
#101691=AXIS2_PLACEMENT_3D('',#397060,#121686,#121687);
#101692=AXIS2_PLACEMENT_3D('',#397061,#121688,#121689);
#101693=AXIS2_PLACEMENT_3D('',#397062,#121690,#121691);
#101694=AXIS2_PLACEMENT_3D('',#397075,#121692,#121693);
#101695=AXIS2_PLACEMENT_3D('',#397076,#121694,#121695);
#101696=AXIS2_PLACEMENT_3D('',#397077,#121696,#121697);
#101697=AXIS2_PLACEMENT_3D('',#397090,#121698,#121699);
#101698=AXIS2_PLACEMENT_3D('',#397103,#121700,#121701);
#101699=AXIS2_PLACEMENT_3D('',#397116,#121702,#121703);
#101700=AXIS2_PLACEMENT_3D('',#397129,#121704,#121705);
#101701=AXIS2_PLACEMENT_3D('',#397142,#121706,#121707);
#101702=AXIS2_PLACEMENT_3D('',#397143,#121708,#121709);
#101703=AXIS2_PLACEMENT_3D('',#397144,#121710,#121711);
#101704=AXIS2_PLACEMENT_3D('',#397157,#121712,#121713);
#101705=AXIS2_PLACEMENT_3D('',#397158,#121714,#121715);
#101706=AXIS2_PLACEMENT_3D('',#397168,#121717,#121718);
#101707=AXIS2_PLACEMENT_3D('',#397178,#121720,#121721);
#101708=AXIS2_PLACEMENT_3D('',#397181,#121722,#121723);
#101709=AXIS2_PLACEMENT_3D('',#397198,#121726,#121727);
#101710=AXIS2_PLACEMENT_3D('',#397248,#121728,#121729);
#101711=AXIS2_PLACEMENT_3D('',#397294,#121730,#121731);
#101712=AXIS2_PLACEMENT_3D('',#397311,#121732,#121733);
#101713=AXIS2_PLACEMENT_3D('',#397363,#121734,#121735);
#101714=AXIS2_PLACEMENT_3D('',#397364,#121736,#121737);
#101715=AXIS2_PLACEMENT_3D('',#397365,#121738,#121739);
#101716=AXIS2_PLACEMENT_3D('',#397366,#121740,#121741);
#101717=AXIS2_PLACEMENT_3D('',#397379,#121742,#121743);
#101718=AXIS2_PLACEMENT_3D('',#397380,#121744,#121745);
#101719=AXIS2_PLACEMENT_3D('',#397381,#121746,#121747);
#101720=AXIS2_PLACEMENT_3D('',#397394,#121748,#121749);
#101721=AXIS2_PLACEMENT_3D('',#397407,#121750,#121751);
#101722=AXIS2_PLACEMENT_3D('',#397420,#121752,#121753);
#101723=AXIS2_PLACEMENT_3D('',#397433,#121754,#121755);
#101724=AXIS2_PLACEMENT_3D('',#397446,#121756,#121757);
#101725=AXIS2_PLACEMENT_3D('',#397447,#121758,#121759);
#101726=AXIS2_PLACEMENT_3D('',#397448,#121760,#121761);
#101727=AXIS2_PLACEMENT_3D('',#397461,#121762,#121763);
#101728=AXIS2_PLACEMENT_3D('',#397462,#121764,#121765);
#101729=AXIS2_PLACEMENT_3D('',#397472,#121767,#121768);
#101730=AXIS2_PLACEMENT_3D('',#397482,#121770,#121771);
#101731=AXIS2_PLACEMENT_3D('',#397485,#121772,#121773);
#101732=AXIS2_PLACEMENT_3D('',#397502,#121776,#121777);
#101733=AXIS2_PLACEMENT_3D('',#397552,#121778,#121779);
#101734=AXIS2_PLACEMENT_3D('',#397598,#121780,#121781);
#101735=AXIS2_PLACEMENT_3D('',#397615,#121782,#121783);
#101736=AXIS2_PLACEMENT_3D('',#397667,#121784,#121785);
#101737=AXIS2_PLACEMENT_3D('',#397668,#121786,#121787);
#101738=AXIS2_PLACEMENT_3D('',#397669,#121788,#121789);
#101739=AXIS2_PLACEMENT_3D('',#397670,#121790,#121791);
#101740=AXIS2_PLACEMENT_3D('',#397683,#121792,#121793);
#101741=AXIS2_PLACEMENT_3D('',#397684,#121794,#121795);
#101742=AXIS2_PLACEMENT_3D('',#397685,#121796,#121797);
#101743=AXIS2_PLACEMENT_3D('',#397698,#121798,#121799);
#101744=AXIS2_PLACEMENT_3D('',#397711,#121800,#121801);
#101745=AXIS2_PLACEMENT_3D('',#397724,#121802,#121803);
#101746=AXIS2_PLACEMENT_3D('',#397737,#121804,#121805);
#101747=AXIS2_PLACEMENT_3D('',#397750,#121806,#121807);
#101748=AXIS2_PLACEMENT_3D('',#397751,#121808,#121809);
#101749=AXIS2_PLACEMENT_3D('',#397752,#121810,#121811);
#101750=AXIS2_PLACEMENT_3D('',#397765,#121812,#121813);
#101751=AXIS2_PLACEMENT_3D('',#397766,#121814,#121815);
#101752=AXIS2_PLACEMENT_3D('',#397776,#121817,#121818);
#101753=AXIS2_PLACEMENT_3D('',#397786,#121820,#121821);
#101754=AXIS2_PLACEMENT_3D('',#397789,#121822,#121823);
#101755=AXIS2_PLACEMENT_3D('',#397806,#121826,#121827);
#101756=AXIS2_PLACEMENT_3D('',#397856,#121828,#121829);
#101757=AXIS2_PLACEMENT_3D('',#397902,#121830,#121831);
#101758=AXIS2_PLACEMENT_3D('',#397919,#121832,#121833);
#101759=AXIS2_PLACEMENT_3D('',#397971,#121834,#121835);
#101760=AXIS2_PLACEMENT_3D('',#397972,#121836,#121837);
#101761=AXIS2_PLACEMENT_3D('',#397973,#121838,#121839);
#101762=AXIS2_PLACEMENT_3D('',#397974,#121840,#121841);
#101763=AXIS2_PLACEMENT_3D('',#397987,#121842,#121843);
#101764=AXIS2_PLACEMENT_3D('',#397988,#121844,#121845);
#101765=AXIS2_PLACEMENT_3D('',#397989,#121846,#121847);
#101766=AXIS2_PLACEMENT_3D('',#398002,#121848,#121849);
#101767=AXIS2_PLACEMENT_3D('',#398015,#121850,#121851);
#101768=AXIS2_PLACEMENT_3D('',#398028,#121852,#121853);
#101769=AXIS2_PLACEMENT_3D('',#398041,#121854,#121855);
#101770=AXIS2_PLACEMENT_3D('',#398054,#121856,#121857);
#101771=AXIS2_PLACEMENT_3D('',#398055,#121858,#121859);
#101772=AXIS2_PLACEMENT_3D('',#398056,#121860,#121861);
#101773=AXIS2_PLACEMENT_3D('',#398069,#121862,#121863);
#101774=AXIS2_PLACEMENT_3D('',#398070,#121864,#121865);
#101775=AXIS2_PLACEMENT_3D('',#398080,#121867,#121868);
#101776=AXIS2_PLACEMENT_3D('',#398090,#121870,#121871);
#101777=AXIS2_PLACEMENT_3D('',#398093,#121872,#121873);
#101778=AXIS2_PLACEMENT_3D('',#398110,#121876,#121877);
#101779=AXIS2_PLACEMENT_3D('',#398160,#121878,#121879);
#101780=AXIS2_PLACEMENT_3D('',#398206,#121880,#121881);
#101781=AXIS2_PLACEMENT_3D('',#398223,#121882,#121883);
#101782=AXIS2_PLACEMENT_3D('',#398275,#121884,#121885);
#101783=AXIS2_PLACEMENT_3D('',#398276,#121886,#121887);
#101784=AXIS2_PLACEMENT_3D('',#398277,#121888,#121889);
#101785=AXIS2_PLACEMENT_3D('',#398278,#121890,#121891);
#101786=AXIS2_PLACEMENT_3D('',#398291,#121892,#121893);
#101787=AXIS2_PLACEMENT_3D('',#398292,#121894,#121895);
#101788=AXIS2_PLACEMENT_3D('',#398293,#121896,#121897);
#101789=AXIS2_PLACEMENT_3D('',#398306,#121898,#121899);
#101790=AXIS2_PLACEMENT_3D('',#398319,#121900,#121901);
#101791=AXIS2_PLACEMENT_3D('',#398332,#121902,#121903);
#101792=AXIS2_PLACEMENT_3D('',#398345,#121904,#121905);
#101793=AXIS2_PLACEMENT_3D('',#398358,#121906,#121907);
#101794=AXIS2_PLACEMENT_3D('',#398359,#121908,#121909);
#101795=AXIS2_PLACEMENT_3D('',#398360,#121910,#121911);
#101796=AXIS2_PLACEMENT_3D('',#398373,#121912,#121913);
#101797=AXIS2_PLACEMENT_3D('',#398374,#121914,#121915);
#101798=AXIS2_PLACEMENT_3D('',#398384,#121917,#121918);
#101799=AXIS2_PLACEMENT_3D('',#398394,#121920,#121921);
#101800=AXIS2_PLACEMENT_3D('',#398397,#121922,#121923);
#101801=AXIS2_PLACEMENT_3D('',#398414,#121926,#121927);
#101802=AXIS2_PLACEMENT_3D('',#398464,#121928,#121929);
#101803=AXIS2_PLACEMENT_3D('',#398510,#121930,#121931);
#101804=AXIS2_PLACEMENT_3D('',#398527,#121932,#121933);
#101805=AXIS2_PLACEMENT_3D('',#398579,#121934,#121935);
#101806=AXIS2_PLACEMENT_3D('',#398580,#121936,#121937);
#101807=AXIS2_PLACEMENT_3D('',#398581,#121938,#121939);
#101808=AXIS2_PLACEMENT_3D('',#398582,#121940,#121941);
#101809=AXIS2_PLACEMENT_3D('',#398595,#121942,#121943);
#101810=AXIS2_PLACEMENT_3D('',#398596,#121944,#121945);
#101811=AXIS2_PLACEMENT_3D('',#398597,#121946,#121947);
#101812=AXIS2_PLACEMENT_3D('',#398610,#121948,#121949);
#101813=AXIS2_PLACEMENT_3D('',#398623,#121950,#121951);
#101814=AXIS2_PLACEMENT_3D('',#398636,#121952,#121953);
#101815=AXIS2_PLACEMENT_3D('',#398649,#121954,#121955);
#101816=AXIS2_PLACEMENT_3D('',#398662,#121956,#121957);
#101817=AXIS2_PLACEMENT_3D('',#398663,#121958,#121959);
#101818=AXIS2_PLACEMENT_3D('',#398664,#121960,#121961);
#101819=AXIS2_PLACEMENT_3D('',#398677,#121962,#121963);
#101820=AXIS2_PLACEMENT_3D('',#398678,#121964,#121965);
#101821=AXIS2_PLACEMENT_3D('',#398688,#121967,#121968);
#101822=AXIS2_PLACEMENT_3D('',#398698,#121970,#121971);
#101823=AXIS2_PLACEMENT_3D('',#398701,#121972,#121973);
#101824=AXIS2_PLACEMENT_3D('',#398718,#121976,#121977);
#101825=AXIS2_PLACEMENT_3D('',#398768,#121978,#121979);
#101826=AXIS2_PLACEMENT_3D('',#398814,#121980,#121981);
#101827=AXIS2_PLACEMENT_3D('',#398831,#121982,#121983);
#101828=AXIS2_PLACEMENT_3D('',#398883,#121984,#121985);
#101829=AXIS2_PLACEMENT_3D('',#398884,#121986,#121987);
#101830=AXIS2_PLACEMENT_3D('',#398885,#121988,#121989);
#101831=AXIS2_PLACEMENT_3D('',#398886,#121990,#121991);
#101832=AXIS2_PLACEMENT_3D('',#398899,#121992,#121993);
#101833=AXIS2_PLACEMENT_3D('',#398900,#121994,#121995);
#101834=AXIS2_PLACEMENT_3D('',#398901,#121996,#121997);
#101835=AXIS2_PLACEMENT_3D('',#398914,#121998,#121999);
#101836=AXIS2_PLACEMENT_3D('',#398927,#122000,#122001);
#101837=AXIS2_PLACEMENT_3D('',#398940,#122002,#122003);
#101838=AXIS2_PLACEMENT_3D('',#398953,#122004,#122005);
#101839=AXIS2_PLACEMENT_3D('',#398966,#122006,#122007);
#101840=AXIS2_PLACEMENT_3D('',#398967,#122008,#122009);
#101841=AXIS2_PLACEMENT_3D('',#398968,#122010,#122011);
#101842=AXIS2_PLACEMENT_3D('',#398981,#122012,#122013);
#101843=AXIS2_PLACEMENT_3D('',#398982,#122014,#122015);
#101844=AXIS2_PLACEMENT_3D('',#398992,#122017,#122018);
#101845=AXIS2_PLACEMENT_3D('',#399002,#122020,#122021);
#101846=AXIS2_PLACEMENT_3D('',#399005,#122022,#122023);
#101847=AXIS2_PLACEMENT_3D('',#399022,#122026,#122027);
#101848=AXIS2_PLACEMENT_3D('',#399072,#122028,#122029);
#101849=AXIS2_PLACEMENT_3D('',#399118,#122030,#122031);
#101850=AXIS2_PLACEMENT_3D('',#399135,#122032,#122033);
#101851=AXIS2_PLACEMENT_3D('',#399187,#122034,#122035);
#101852=AXIS2_PLACEMENT_3D('',#399188,#122036,#122037);
#101853=AXIS2_PLACEMENT_3D('',#399189,#122038,#122039);
#101854=AXIS2_PLACEMENT_3D('',#399190,#122040,#122041);
#101855=AXIS2_PLACEMENT_3D('',#399203,#122042,#122043);
#101856=AXIS2_PLACEMENT_3D('',#399204,#122044,#122045);
#101857=AXIS2_PLACEMENT_3D('',#399205,#122046,#122047);
#101858=AXIS2_PLACEMENT_3D('',#399218,#122048,#122049);
#101859=AXIS2_PLACEMENT_3D('',#399231,#122050,#122051);
#101860=AXIS2_PLACEMENT_3D('',#399244,#122052,#122053);
#101861=AXIS2_PLACEMENT_3D('',#399257,#122054,#122055);
#101862=AXIS2_PLACEMENT_3D('',#399270,#122056,#122057);
#101863=AXIS2_PLACEMENT_3D('',#399271,#122058,#122059);
#101864=AXIS2_PLACEMENT_3D('',#399272,#122060,#122061);
#101865=AXIS2_PLACEMENT_3D('',#399285,#122062,#122063);
#101866=AXIS2_PLACEMENT_3D('',#399286,#122064,#122065);
#101867=AXIS2_PLACEMENT_3D('',#399296,#122067,#122068);
#101868=AXIS2_PLACEMENT_3D('',#399306,#122070,#122071);
#101869=AXIS2_PLACEMENT_3D('',#399309,#122072,#122073);
#101870=AXIS2_PLACEMENT_3D('',#399326,#122076,#122077);
#101871=AXIS2_PLACEMENT_3D('',#399376,#122078,#122079);
#101872=AXIS2_PLACEMENT_3D('',#399422,#122080,#122081);
#101873=AXIS2_PLACEMENT_3D('',#399439,#122082,#122083);
#101874=AXIS2_PLACEMENT_3D('',#399491,#122084,#122085);
#101875=AXIS2_PLACEMENT_3D('',#399492,#122086,#122087);
#101876=AXIS2_PLACEMENT_3D('',#399493,#122088,#122089);
#101877=AXIS2_PLACEMENT_3D('',#399494,#122090,#122091);
#101878=AXIS2_PLACEMENT_3D('',#399507,#122092,#122093);
#101879=AXIS2_PLACEMENT_3D('',#399508,#122094,#122095);
#101880=AXIS2_PLACEMENT_3D('',#399509,#122096,#122097);
#101881=AXIS2_PLACEMENT_3D('',#399522,#122098,#122099);
#101882=AXIS2_PLACEMENT_3D('',#399535,#122100,#122101);
#101883=AXIS2_PLACEMENT_3D('',#399548,#122102,#122103);
#101884=AXIS2_PLACEMENT_3D('',#399561,#122104,#122105);
#101885=AXIS2_PLACEMENT_3D('',#399574,#122106,#122107);
#101886=AXIS2_PLACEMENT_3D('',#399575,#122108,#122109);
#101887=AXIS2_PLACEMENT_3D('',#399576,#122110,#122111);
#101888=AXIS2_PLACEMENT_3D('',#399589,#122112,#122113);
#101889=AXIS2_PLACEMENT_3D('',#399590,#122114,#122115);
#101890=AXIS2_PLACEMENT_3D('',#399600,#122117,#122118);
#101891=AXIS2_PLACEMENT_3D('',#399610,#122120,#122121);
#101892=AXIS2_PLACEMENT_3D('',#399613,#122122,#122123);
#101893=AXIS2_PLACEMENT_3D('',#399630,#122126,#122127);
#101894=AXIS2_PLACEMENT_3D('',#399680,#122128,#122129);
#101895=AXIS2_PLACEMENT_3D('',#399726,#122130,#122131);
#101896=AXIS2_PLACEMENT_3D('',#399743,#122132,#122133);
#101897=AXIS2_PLACEMENT_3D('',#399795,#122134,#122135);
#101898=AXIS2_PLACEMENT_3D('',#399796,#122136,#122137);
#101899=AXIS2_PLACEMENT_3D('',#399797,#122138,#122139);
#101900=AXIS2_PLACEMENT_3D('',#399798,#122140,#122141);
#101901=AXIS2_PLACEMENT_3D('',#399811,#122142,#122143);
#101902=AXIS2_PLACEMENT_3D('',#399812,#122144,#122145);
#101903=AXIS2_PLACEMENT_3D('',#399813,#122146,#122147);
#101904=AXIS2_PLACEMENT_3D('',#399826,#122148,#122149);
#101905=AXIS2_PLACEMENT_3D('',#399839,#122150,#122151);
#101906=AXIS2_PLACEMENT_3D('',#399852,#122152,#122153);
#101907=AXIS2_PLACEMENT_3D('',#399865,#122154,#122155);
#101908=AXIS2_PLACEMENT_3D('',#399878,#122156,#122157);
#101909=AXIS2_PLACEMENT_3D('',#399879,#122158,#122159);
#101910=AXIS2_PLACEMENT_3D('',#399880,#122160,#122161);
#101911=AXIS2_PLACEMENT_3D('',#399893,#122162,#122163);
#101912=AXIS2_PLACEMENT_3D('',#399894,#122164,#122165);
#101913=AXIS2_PLACEMENT_3D('',#399904,#122167,#122168);
#101914=AXIS2_PLACEMENT_3D('',#399914,#122170,#122171);
#101915=AXIS2_PLACEMENT_3D('',#399917,#122172,#122173);
#101916=AXIS2_PLACEMENT_3D('',#399934,#122176,#122177);
#101917=AXIS2_PLACEMENT_3D('',#399984,#122178,#122179);
#101918=AXIS2_PLACEMENT_3D('',#400030,#122180,#122181);
#101919=AXIS2_PLACEMENT_3D('',#400047,#122182,#122183);
#101920=AXIS2_PLACEMENT_3D('',#400099,#122184,#122185);
#101921=AXIS2_PLACEMENT_3D('',#400100,#122186,#122187);
#101922=AXIS2_PLACEMENT_3D('',#400101,#122188,#122189);
#101923=AXIS2_PLACEMENT_3D('',#400102,#122190,#122191);
#101924=AXIS2_PLACEMENT_3D('',#400115,#122192,#122193);
#101925=AXIS2_PLACEMENT_3D('',#400116,#122194,#122195);
#101926=AXIS2_PLACEMENT_3D('',#400117,#122196,#122197);
#101927=AXIS2_PLACEMENT_3D('',#400130,#122198,#122199);
#101928=AXIS2_PLACEMENT_3D('',#400143,#122200,#122201);
#101929=AXIS2_PLACEMENT_3D('',#400156,#122202,#122203);
#101930=AXIS2_PLACEMENT_3D('',#400169,#122204,#122205);
#101931=AXIS2_PLACEMENT_3D('',#400182,#122206,#122207);
#101932=AXIS2_PLACEMENT_3D('',#400183,#122208,#122209);
#101933=AXIS2_PLACEMENT_3D('',#400184,#122210,#122211);
#101934=AXIS2_PLACEMENT_3D('',#400197,#122212,#122213);
#101935=AXIS2_PLACEMENT_3D('',#400198,#122214,#122215);
#101936=AXIS2_PLACEMENT_3D('',#400208,#122217,#122218);
#101937=AXIS2_PLACEMENT_3D('',#400218,#122220,#122221);
#101938=AXIS2_PLACEMENT_3D('',#400221,#122222,#122223);
#101939=AXIS2_PLACEMENT_3D('',#400238,#122226,#122227);
#101940=AXIS2_PLACEMENT_3D('',#400288,#122228,#122229);
#101941=AXIS2_PLACEMENT_3D('',#400334,#122230,#122231);
#101942=AXIS2_PLACEMENT_3D('',#400351,#122232,#122233);
#101943=AXIS2_PLACEMENT_3D('',#400403,#122234,#122235);
#101944=AXIS2_PLACEMENT_3D('',#400404,#122236,#122237);
#101945=AXIS2_PLACEMENT_3D('',#400405,#122238,#122239);
#101946=AXIS2_PLACEMENT_3D('',#400406,#122240,#122241);
#101947=AXIS2_PLACEMENT_3D('',#400419,#122242,#122243);
#101948=AXIS2_PLACEMENT_3D('',#400420,#122244,#122245);
#101949=AXIS2_PLACEMENT_3D('',#400421,#122246,#122247);
#101950=AXIS2_PLACEMENT_3D('',#400434,#122248,#122249);
#101951=AXIS2_PLACEMENT_3D('',#400447,#122250,#122251);
#101952=AXIS2_PLACEMENT_3D('',#400460,#122252,#122253);
#101953=AXIS2_PLACEMENT_3D('',#400473,#122254,#122255);
#101954=AXIS2_PLACEMENT_3D('',#400486,#122256,#122257);
#101955=AXIS2_PLACEMENT_3D('',#400487,#122258,#122259);
#101956=AXIS2_PLACEMENT_3D('',#400488,#122260,#122261);
#101957=AXIS2_PLACEMENT_3D('',#400501,#122262,#122263);
#101958=AXIS2_PLACEMENT_3D('',#400502,#122264,#122265);
#101959=AXIS2_PLACEMENT_3D('',#400512,#122267,#122268);
#101960=AXIS2_PLACEMENT_3D('',#400522,#122270,#122271);
#101961=AXIS2_PLACEMENT_3D('',#400525,#122272,#122273);
#101962=AXIS2_PLACEMENT_3D('',#400542,#122276,#122277);
#101963=AXIS2_PLACEMENT_3D('',#400592,#122278,#122279);
#101964=AXIS2_PLACEMENT_3D('',#400638,#122280,#122281);
#101965=AXIS2_PLACEMENT_3D('',#400655,#122282,#122283);
#101966=AXIS2_PLACEMENT_3D('',#400707,#122284,#122285);
#101967=AXIS2_PLACEMENT_3D('',#400708,#122286,#122287);
#101968=AXIS2_PLACEMENT_3D('',#400709,#122288,#122289);
#101969=AXIS2_PLACEMENT_3D('',#400710,#122290,#122291);
#101970=AXIS2_PLACEMENT_3D('',#400723,#122292,#122293);
#101971=AXIS2_PLACEMENT_3D('',#400724,#122294,#122295);
#101972=AXIS2_PLACEMENT_3D('',#400725,#122296,#122297);
#101973=AXIS2_PLACEMENT_3D('',#400738,#122298,#122299);
#101974=AXIS2_PLACEMENT_3D('',#400751,#122300,#122301);
#101975=AXIS2_PLACEMENT_3D('',#400764,#122302,#122303);
#101976=AXIS2_PLACEMENT_3D('',#400777,#122304,#122305);
#101977=AXIS2_PLACEMENT_3D('',#400790,#122306,#122307);
#101978=AXIS2_PLACEMENT_3D('',#400791,#122308,#122309);
#101979=AXIS2_PLACEMENT_3D('',#400792,#122310,#122311);
#101980=AXIS2_PLACEMENT_3D('',#400805,#122312,#122313);
#101981=AXIS2_PLACEMENT_3D('',#400806,#122314,#122315);
#101982=AXIS2_PLACEMENT_3D('',#400816,#122317,#122318);
#101983=AXIS2_PLACEMENT_3D('',#400826,#122320,#122321);
#101984=AXIS2_PLACEMENT_3D('',#400829,#122322,#122323);
#101985=AXIS2_PLACEMENT_3D('',#400846,#122326,#122327);
#101986=AXIS2_PLACEMENT_3D('',#400896,#122328,#122329);
#101987=AXIS2_PLACEMENT_3D('',#400942,#122330,#122331);
#101988=AXIS2_PLACEMENT_3D('',#400959,#122332,#122333);
#101989=AXIS2_PLACEMENT_3D('',#401011,#122334,#122335);
#101990=AXIS2_PLACEMENT_3D('',#401012,#122336,#122337);
#101991=AXIS2_PLACEMENT_3D('',#401013,#122338,#122339);
#101992=AXIS2_PLACEMENT_3D('',#401014,#122340,#122341);
#101993=AXIS2_PLACEMENT_3D('',#401027,#122342,#122343);
#101994=AXIS2_PLACEMENT_3D('',#401028,#122344,#122345);
#101995=AXIS2_PLACEMENT_3D('',#401029,#122346,#122347);
#101996=AXIS2_PLACEMENT_3D('',#401042,#122348,#122349);
#101997=AXIS2_PLACEMENT_3D('',#401055,#122350,#122351);
#101998=AXIS2_PLACEMENT_3D('',#401068,#122352,#122353);
#101999=AXIS2_PLACEMENT_3D('',#401081,#122354,#122355);
#102000=AXIS2_PLACEMENT_3D('',#401094,#122356,#122357);
#102001=AXIS2_PLACEMENT_3D('',#401095,#122358,#122359);
#102002=AXIS2_PLACEMENT_3D('',#401096,#122360,#122361);
#102003=AXIS2_PLACEMENT_3D('',#401109,#122362,#122363);
#102004=AXIS2_PLACEMENT_3D('',#401110,#122364,#122365);
#102005=AXIS2_PLACEMENT_3D('',#401120,#122367,#122368);
#102006=AXIS2_PLACEMENT_3D('',#401130,#122370,#122371);
#102007=AXIS2_PLACEMENT_3D('',#401133,#122372,#122373);
#102008=AXIS2_PLACEMENT_3D('',#401150,#122376,#122377);
#102009=AXIS2_PLACEMENT_3D('',#401200,#122378,#122379);
#102010=AXIS2_PLACEMENT_3D('',#401246,#122380,#122381);
#102011=AXIS2_PLACEMENT_3D('',#401263,#122382,#122383);
#102012=AXIS2_PLACEMENT_3D('',#401315,#122384,#122385);
#102013=AXIS2_PLACEMENT_3D('',#401316,#122386,#122387);
#102014=AXIS2_PLACEMENT_3D('',#401317,#122388,#122389);
#102015=AXIS2_PLACEMENT_3D('',#401318,#122390,#122391);
#102016=AXIS2_PLACEMENT_3D('',#401331,#122392,#122393);
#102017=AXIS2_PLACEMENT_3D('',#401332,#122394,#122395);
#102018=AXIS2_PLACEMENT_3D('',#401333,#122396,#122397);
#102019=AXIS2_PLACEMENT_3D('',#401346,#122398,#122399);
#102020=AXIS2_PLACEMENT_3D('',#401359,#122400,#122401);
#102021=AXIS2_PLACEMENT_3D('',#401372,#122402,#122403);
#102022=AXIS2_PLACEMENT_3D('',#401385,#122404,#122405);
#102023=AXIS2_PLACEMENT_3D('',#401398,#122406,#122407);
#102024=AXIS2_PLACEMENT_3D('',#401399,#122408,#122409);
#102025=AXIS2_PLACEMENT_3D('',#401400,#122410,#122411);
#102026=AXIS2_PLACEMENT_3D('',#401413,#122412,#122413);
#102027=AXIS2_PLACEMENT_3D('',#401414,#122414,#122415);
#102028=AXIS2_PLACEMENT_3D('',#401424,#122417,#122418);
#102029=AXIS2_PLACEMENT_3D('',#401434,#122420,#122421);
#102030=AXIS2_PLACEMENT_3D('',#401437,#122422,#122423);
#102031=AXIS2_PLACEMENT_3D('',#401454,#122426,#122427);
#102032=AXIS2_PLACEMENT_3D('',#401504,#122428,#122429);
#102033=AXIS2_PLACEMENT_3D('',#401550,#122430,#122431);
#102034=AXIS2_PLACEMENT_3D('',#401567,#122432,#122433);
#102035=AXIS2_PLACEMENT_3D('',#401619,#122434,#122435);
#102036=AXIS2_PLACEMENT_3D('',#401620,#122436,#122437);
#102037=AXIS2_PLACEMENT_3D('',#401621,#122438,#122439);
#102038=AXIS2_PLACEMENT_3D('',#401622,#122440,#122441);
#102039=AXIS2_PLACEMENT_3D('',#401635,#122442,#122443);
#102040=AXIS2_PLACEMENT_3D('',#401636,#122444,#122445);
#102041=AXIS2_PLACEMENT_3D('',#401637,#122446,#122447);
#102042=AXIS2_PLACEMENT_3D('',#401650,#122448,#122449);
#102043=AXIS2_PLACEMENT_3D('',#401663,#122450,#122451);
#102044=AXIS2_PLACEMENT_3D('',#401676,#122452,#122453);
#102045=AXIS2_PLACEMENT_3D('',#401689,#122454,#122455);
#102046=AXIS2_PLACEMENT_3D('',#401702,#122456,#122457);
#102047=AXIS2_PLACEMENT_3D('',#401703,#122458,#122459);
#102048=AXIS2_PLACEMENT_3D('',#401704,#122460,#122461);
#102049=AXIS2_PLACEMENT_3D('',#401717,#122462,#122463);
#102050=AXIS2_PLACEMENT_3D('',#401718,#122464,#122465);
#102051=AXIS2_PLACEMENT_3D('',#401728,#122467,#122468);
#102052=AXIS2_PLACEMENT_3D('',#401738,#122470,#122471);
#102053=AXIS2_PLACEMENT_3D('',#401741,#122472,#122473);
#102054=AXIS2_PLACEMENT_3D('',#401758,#122476,#122477);
#102055=AXIS2_PLACEMENT_3D('',#401808,#122478,#122479);
#102056=AXIS2_PLACEMENT_3D('',#401854,#122480,#122481);
#102057=AXIS2_PLACEMENT_3D('',#401871,#122482,#122483);
#102058=AXIS2_PLACEMENT_3D('',#401923,#122484,#122485);
#102059=AXIS2_PLACEMENT_3D('',#401924,#122486,#122487);
#102060=AXIS2_PLACEMENT_3D('',#401925,#122488,#122489);
#102061=AXIS2_PLACEMENT_3D('',#401926,#122490,#122491);
#102062=AXIS2_PLACEMENT_3D('',#401939,#122492,#122493);
#102063=AXIS2_PLACEMENT_3D('',#401940,#122494,#122495);
#102064=AXIS2_PLACEMENT_3D('',#401941,#122496,#122497);
#102065=AXIS2_PLACEMENT_3D('',#401954,#122498,#122499);
#102066=AXIS2_PLACEMENT_3D('',#401967,#122500,#122501);
#102067=AXIS2_PLACEMENT_3D('',#401980,#122502,#122503);
#102068=AXIS2_PLACEMENT_3D('',#401993,#122504,#122505);
#102069=AXIS2_PLACEMENT_3D('',#402006,#122506,#122507);
#102070=AXIS2_PLACEMENT_3D('',#402007,#122508,#122509);
#102071=AXIS2_PLACEMENT_3D('',#402008,#122510,#122511);
#102072=AXIS2_PLACEMENT_3D('',#402021,#122512,#122513);
#102073=AXIS2_PLACEMENT_3D('',#402022,#122514,#122515);
#102074=AXIS2_PLACEMENT_3D('',#402032,#122517,#122518);
#102075=AXIS2_PLACEMENT_3D('',#402042,#122520,#122521);
#102076=AXIS2_PLACEMENT_3D('',#402045,#122522,#122523);
#102077=AXIS2_PLACEMENT_3D('',#402062,#122526,#122527);
#102078=AXIS2_PLACEMENT_3D('',#402112,#122528,#122529);
#102079=AXIS2_PLACEMENT_3D('',#402158,#122530,#122531);
#102080=AXIS2_PLACEMENT_3D('',#402175,#122532,#122533);
#102081=AXIS2_PLACEMENT_3D('',#402227,#122534,#122535);
#102082=AXIS2_PLACEMENT_3D('',#402228,#122536,#122537);
#102083=AXIS2_PLACEMENT_3D('',#402229,#122538,#122539);
#102084=AXIS2_PLACEMENT_3D('',#402230,#122540,#122541);
#102085=AXIS2_PLACEMENT_3D('',#402243,#122542,#122543);
#102086=AXIS2_PLACEMENT_3D('',#402244,#122544,#122545);
#102087=AXIS2_PLACEMENT_3D('',#402245,#122546,#122547);
#102088=AXIS2_PLACEMENT_3D('',#402258,#122548,#122549);
#102089=AXIS2_PLACEMENT_3D('',#402271,#122550,#122551);
#102090=AXIS2_PLACEMENT_3D('',#402284,#122552,#122553);
#102091=AXIS2_PLACEMENT_3D('',#402297,#122554,#122555);
#102092=AXIS2_PLACEMENT_3D('',#402310,#122556,#122557);
#102093=AXIS2_PLACEMENT_3D('',#402311,#122558,#122559);
#102094=AXIS2_PLACEMENT_3D('',#402312,#122560,#122561);
#102095=AXIS2_PLACEMENT_3D('',#402325,#122562,#122563);
#102096=AXIS2_PLACEMENT_3D('',#402326,#122564,#122565);
#102097=AXIS2_PLACEMENT_3D('',#402336,#122567,#122568);
#102098=AXIS2_PLACEMENT_3D('',#402346,#122570,#122571);
#102099=AXIS2_PLACEMENT_3D('',#402349,#122572,#122573);
#102100=AXIS2_PLACEMENT_3D('',#402366,#122576,#122577);
#102101=AXIS2_PLACEMENT_3D('',#402416,#122578,#122579);
#102102=AXIS2_PLACEMENT_3D('',#402462,#122580,#122581);
#102103=AXIS2_PLACEMENT_3D('',#402479,#122582,#122583);
#102104=AXIS2_PLACEMENT_3D('',#402531,#122584,#122585);
#102105=AXIS2_PLACEMENT_3D('',#402532,#122586,#122587);
#102106=AXIS2_PLACEMENT_3D('',#402533,#122588,#122589);
#102107=AXIS2_PLACEMENT_3D('',#402534,#122590,#122591);
#102108=AXIS2_PLACEMENT_3D('',#402547,#122592,#122593);
#102109=AXIS2_PLACEMENT_3D('',#402548,#122594,#122595);
#102110=AXIS2_PLACEMENT_3D('',#402549,#122596,#122597);
#102111=AXIS2_PLACEMENT_3D('',#402562,#122598,#122599);
#102112=AXIS2_PLACEMENT_3D('',#402575,#122600,#122601);
#102113=AXIS2_PLACEMENT_3D('',#402588,#122602,#122603);
#102114=AXIS2_PLACEMENT_3D('',#402601,#122604,#122605);
#102115=AXIS2_PLACEMENT_3D('',#402614,#122606,#122607);
#102116=AXIS2_PLACEMENT_3D('',#402615,#122608,#122609);
#102117=AXIS2_PLACEMENT_3D('',#402616,#122610,#122611);
#102118=AXIS2_PLACEMENT_3D('',#402629,#122612,#122613);
#102119=AXIS2_PLACEMENT_3D('',#402630,#122614,#122615);
#102120=AXIS2_PLACEMENT_3D('',#402640,#122617,#122618);
#102121=AXIS2_PLACEMENT_3D('',#402650,#122620,#122621);
#102122=AXIS2_PLACEMENT_3D('',#402653,#122622,#122623);
#102123=AXIS2_PLACEMENT_3D('',#402670,#122626,#122627);
#102124=AXIS2_PLACEMENT_3D('',#402720,#122628,#122629);
#102125=AXIS2_PLACEMENT_3D('',#402766,#122630,#122631);
#102126=AXIS2_PLACEMENT_3D('',#402783,#122632,#122633);
#102127=AXIS2_PLACEMENT_3D('',#402835,#122634,#122635);
#102128=AXIS2_PLACEMENT_3D('',#402836,#122636,#122637);
#102129=AXIS2_PLACEMENT_3D('',#402837,#122638,#122639);
#102130=AXIS2_PLACEMENT_3D('',#402838,#122640,#122641);
#102131=AXIS2_PLACEMENT_3D('',#402851,#122642,#122643);
#102132=AXIS2_PLACEMENT_3D('',#402852,#122644,#122645);
#102133=AXIS2_PLACEMENT_3D('',#402853,#122646,#122647);
#102134=AXIS2_PLACEMENT_3D('',#402866,#122648,#122649);
#102135=AXIS2_PLACEMENT_3D('',#402879,#122650,#122651);
#102136=AXIS2_PLACEMENT_3D('',#402892,#122652,#122653);
#102137=AXIS2_PLACEMENT_3D('',#402905,#122654,#122655);
#102138=AXIS2_PLACEMENT_3D('',#402918,#122656,#122657);
#102139=AXIS2_PLACEMENT_3D('',#402919,#122658,#122659);
#102140=AXIS2_PLACEMENT_3D('',#402920,#122660,#122661);
#102141=AXIS2_PLACEMENT_3D('',#402933,#122662,#122663);
#102142=AXIS2_PLACEMENT_3D('',#402934,#122664,#122665);
#102143=AXIS2_PLACEMENT_3D('',#402944,#122667,#122668);
#102144=AXIS2_PLACEMENT_3D('',#402954,#122670,#122671);
#102145=AXIS2_PLACEMENT_3D('',#402957,#122672,#122673);
#102146=AXIS2_PLACEMENT_3D('',#402974,#122676,#122677);
#102147=AXIS2_PLACEMENT_3D('',#403024,#122678,#122679);
#102148=AXIS2_PLACEMENT_3D('',#403070,#122680,#122681);
#102149=AXIS2_PLACEMENT_3D('',#403087,#122682,#122683);
#102150=AXIS2_PLACEMENT_3D('',#403139,#122684,#122685);
#102151=AXIS2_PLACEMENT_3D('',#403140,#122686,#122687);
#102152=AXIS2_PLACEMENT_3D('',#403141,#122688,#122689);
#102153=AXIS2_PLACEMENT_3D('',#403142,#122690,#122691);
#102154=AXIS2_PLACEMENT_3D('',#403155,#122692,#122693);
#102155=AXIS2_PLACEMENT_3D('',#403156,#122694,#122695);
#102156=AXIS2_PLACEMENT_3D('',#403157,#122696,#122697);
#102157=AXIS2_PLACEMENT_3D('',#403170,#122698,#122699);
#102158=AXIS2_PLACEMENT_3D('',#403183,#122700,#122701);
#102159=AXIS2_PLACEMENT_3D('',#403196,#122702,#122703);
#102160=AXIS2_PLACEMENT_3D('',#403209,#122704,#122705);
#102161=AXIS2_PLACEMENT_3D('',#403222,#122706,#122707);
#102162=AXIS2_PLACEMENT_3D('',#403223,#122708,#122709);
#102163=AXIS2_PLACEMENT_3D('',#403224,#122710,#122711);
#102164=AXIS2_PLACEMENT_3D('',#403237,#122712,#122713);
#102165=AXIS2_PLACEMENT_3D('',#403238,#122714,#122715);
#102166=AXIS2_PLACEMENT_3D('',#403248,#122717,#122718);
#102167=AXIS2_PLACEMENT_3D('',#403258,#122720,#122721);
#102168=AXIS2_PLACEMENT_3D('',#403261,#122722,#122723);
#102169=AXIS2_PLACEMENT_3D('',#403278,#122726,#122727);
#102170=AXIS2_PLACEMENT_3D('',#403328,#122728,#122729);
#102171=AXIS2_PLACEMENT_3D('',#403374,#122730,#122731);
#102172=AXIS2_PLACEMENT_3D('',#403391,#122732,#122733);
#102173=AXIS2_PLACEMENT_3D('',#403443,#122734,#122735);
#102174=AXIS2_PLACEMENT_3D('',#403444,#122736,#122737);
#102175=AXIS2_PLACEMENT_3D('',#403445,#122738,#122739);
#102176=AXIS2_PLACEMENT_3D('',#403446,#122740,#122741);
#102177=AXIS2_PLACEMENT_3D('',#403459,#122742,#122743);
#102178=AXIS2_PLACEMENT_3D('',#403460,#122744,#122745);
#102179=AXIS2_PLACEMENT_3D('',#403461,#122746,#122747);
#102180=AXIS2_PLACEMENT_3D('',#403474,#122748,#122749);
#102181=AXIS2_PLACEMENT_3D('',#403487,#122750,#122751);
#102182=AXIS2_PLACEMENT_3D('',#403500,#122752,#122753);
#102183=AXIS2_PLACEMENT_3D('',#403513,#122754,#122755);
#102184=AXIS2_PLACEMENT_3D('',#403526,#122756,#122757);
#102185=AXIS2_PLACEMENT_3D('',#403527,#122758,#122759);
#102186=AXIS2_PLACEMENT_3D('',#403528,#122760,#122761);
#102187=AXIS2_PLACEMENT_3D('',#403541,#122762,#122763);
#102188=AXIS2_PLACEMENT_3D('',#403542,#122764,#122765);
#102189=AXIS2_PLACEMENT_3D('',#403552,#122767,#122768);
#102190=AXIS2_PLACEMENT_3D('',#403562,#122770,#122771);
#102191=AXIS2_PLACEMENT_3D('',#403565,#122772,#122773);
#102192=AXIS2_PLACEMENT_3D('',#403582,#122776,#122777);
#102193=AXIS2_PLACEMENT_3D('',#403632,#122778,#122779);
#102194=AXIS2_PLACEMENT_3D('',#403678,#122780,#122781);
#102195=AXIS2_PLACEMENT_3D('',#403695,#122782,#122783);
#102196=AXIS2_PLACEMENT_3D('',#403747,#122784,#122785);
#102197=AXIS2_PLACEMENT_3D('',#403748,#122786,#122787);
#102198=AXIS2_PLACEMENT_3D('',#403749,#122788,#122789);
#102199=AXIS2_PLACEMENT_3D('',#403750,#122790,#122791);
#102200=AXIS2_PLACEMENT_3D('',#403763,#122792,#122793);
#102201=AXIS2_PLACEMENT_3D('',#403764,#122794,#122795);
#102202=AXIS2_PLACEMENT_3D('',#403765,#122796,#122797);
#102203=AXIS2_PLACEMENT_3D('',#403778,#122798,#122799);
#102204=AXIS2_PLACEMENT_3D('',#403791,#122800,#122801);
#102205=AXIS2_PLACEMENT_3D('',#403804,#122802,#122803);
#102206=AXIS2_PLACEMENT_3D('',#403817,#122804,#122805);
#102207=AXIS2_PLACEMENT_3D('',#403830,#122806,#122807);
#102208=AXIS2_PLACEMENT_3D('',#403831,#122808,#122809);
#102209=AXIS2_PLACEMENT_3D('',#403832,#122810,#122811);
#102210=AXIS2_PLACEMENT_3D('',#403845,#122812,#122813);
#102211=AXIS2_PLACEMENT_3D('',#403846,#122814,#122815);
#102212=AXIS2_PLACEMENT_3D('',#403856,#122817,#122818);
#102213=AXIS2_PLACEMENT_3D('',#403866,#122820,#122821);
#102214=AXIS2_PLACEMENT_3D('',#403869,#122822,#122823);
#102215=AXIS2_PLACEMENT_3D('',#403886,#122826,#122827);
#102216=AXIS2_PLACEMENT_3D('',#403936,#122828,#122829);
#102217=AXIS2_PLACEMENT_3D('',#403982,#122830,#122831);
#102218=AXIS2_PLACEMENT_3D('',#403999,#122832,#122833);
#102219=AXIS2_PLACEMENT_3D('',#404051,#122834,#122835);
#102220=AXIS2_PLACEMENT_3D('',#404052,#122836,#122837);
#102221=AXIS2_PLACEMENT_3D('',#404053,#122838,#122839);
#102222=AXIS2_PLACEMENT_3D('',#404054,#122840,#122841);
#102223=AXIS2_PLACEMENT_3D('',#404067,#122842,#122843);
#102224=AXIS2_PLACEMENT_3D('',#404068,#122844,#122845);
#102225=AXIS2_PLACEMENT_3D('',#404069,#122846,#122847);
#102226=AXIS2_PLACEMENT_3D('',#404082,#122848,#122849);
#102227=AXIS2_PLACEMENT_3D('',#404095,#122850,#122851);
#102228=AXIS2_PLACEMENT_3D('',#404108,#122852,#122853);
#102229=AXIS2_PLACEMENT_3D('',#404121,#122854,#122855);
#102230=AXIS2_PLACEMENT_3D('',#404134,#122856,#122857);
#102231=AXIS2_PLACEMENT_3D('',#404135,#122858,#122859);
#102232=AXIS2_PLACEMENT_3D('',#404136,#122860,#122861);
#102233=AXIS2_PLACEMENT_3D('',#404149,#122862,#122863);
#102234=AXIS2_PLACEMENT_3D('',#404150,#122864,#122865);
#102235=AXIS2_PLACEMENT_3D('',#404160,#122867,#122868);
#102236=AXIS2_PLACEMENT_3D('',#404170,#122870,#122871);
#102237=AXIS2_PLACEMENT_3D('',#404173,#122872,#122873);
#102238=AXIS2_PLACEMENT_3D('',#404190,#122876,#122877);
#102239=AXIS2_PLACEMENT_3D('',#404240,#122878,#122879);
#102240=AXIS2_PLACEMENT_3D('',#404286,#122880,#122881);
#102241=AXIS2_PLACEMENT_3D('',#404303,#122882,#122883);
#102242=AXIS2_PLACEMENT_3D('',#404355,#122884,#122885);
#102243=AXIS2_PLACEMENT_3D('',#404356,#122886,#122887);
#102244=AXIS2_PLACEMENT_3D('',#404357,#122888,#122889);
#102245=AXIS2_PLACEMENT_3D('',#404358,#122890,#122891);
#102246=AXIS2_PLACEMENT_3D('',#404371,#122892,#122893);
#102247=AXIS2_PLACEMENT_3D('',#404372,#122894,#122895);
#102248=AXIS2_PLACEMENT_3D('',#404373,#122896,#122897);
#102249=AXIS2_PLACEMENT_3D('',#404386,#122898,#122899);
#102250=AXIS2_PLACEMENT_3D('',#404399,#122900,#122901);
#102251=AXIS2_PLACEMENT_3D('',#404412,#122902,#122903);
#102252=AXIS2_PLACEMENT_3D('',#404425,#122904,#122905);
#102253=AXIS2_PLACEMENT_3D('',#404438,#122906,#122907);
#102254=AXIS2_PLACEMENT_3D('',#404439,#122908,#122909);
#102255=AXIS2_PLACEMENT_3D('',#404440,#122910,#122911);
#102256=AXIS2_PLACEMENT_3D('',#404453,#122912,#122913);
#102257=AXIS2_PLACEMENT_3D('',#404454,#122914,#122915);
#102258=AXIS2_PLACEMENT_3D('',#404464,#122917,#122918);
#102259=AXIS2_PLACEMENT_3D('',#404474,#122920,#122921);
#102260=AXIS2_PLACEMENT_3D('',#404477,#122922,#122923);
#102261=AXIS2_PLACEMENT_3D('',#404494,#122926,#122927);
#102262=AXIS2_PLACEMENT_3D('',#404544,#122928,#122929);
#102263=AXIS2_PLACEMENT_3D('',#404590,#122930,#122931);
#102264=AXIS2_PLACEMENT_3D('',#404607,#122932,#122933);
#102265=AXIS2_PLACEMENT_3D('',#404659,#122934,#122935);
#102266=AXIS2_PLACEMENT_3D('',#404660,#122936,#122937);
#102267=AXIS2_PLACEMENT_3D('',#404661,#122938,#122939);
#102268=AXIS2_PLACEMENT_3D('',#404662,#122940,#122941);
#102269=AXIS2_PLACEMENT_3D('',#404675,#122942,#122943);
#102270=AXIS2_PLACEMENT_3D('',#404676,#122944,#122945);
#102271=AXIS2_PLACEMENT_3D('',#404677,#122946,#122947);
#102272=AXIS2_PLACEMENT_3D('',#404690,#122948,#122949);
#102273=AXIS2_PLACEMENT_3D('',#404703,#122950,#122951);
#102274=AXIS2_PLACEMENT_3D('',#404716,#122952,#122953);
#102275=AXIS2_PLACEMENT_3D('',#404729,#122954,#122955);
#102276=AXIS2_PLACEMENT_3D('',#404742,#122956,#122957);
#102277=AXIS2_PLACEMENT_3D('',#404743,#122958,#122959);
#102278=AXIS2_PLACEMENT_3D('',#404744,#122960,#122961);
#102279=AXIS2_PLACEMENT_3D('',#404757,#122962,#122963);
#102280=AXIS2_PLACEMENT_3D('',#404758,#122964,#122965);
#102281=AXIS2_PLACEMENT_3D('',#404768,#122967,#122968);
#102282=AXIS2_PLACEMENT_3D('',#404778,#122970,#122971);
#102283=AXIS2_PLACEMENT_3D('',#404781,#122972,#122973);
#102284=AXIS2_PLACEMENT_3D('',#404798,#122976,#122977);
#102285=AXIS2_PLACEMENT_3D('',#404848,#122978,#122979);
#102286=AXIS2_PLACEMENT_3D('',#404894,#122980,#122981);
#102287=AXIS2_PLACEMENT_3D('',#404911,#122982,#122983);
#102288=AXIS2_PLACEMENT_3D('',#404963,#122984,#122985);
#102289=AXIS2_PLACEMENT_3D('',#404964,#122986,#122987);
#102290=AXIS2_PLACEMENT_3D('',#404965,#122988,#122989);
#102291=AXIS2_PLACEMENT_3D('',#404966,#122990,#122991);
#102292=AXIS2_PLACEMENT_3D('',#404979,#122992,#122993);
#102293=AXIS2_PLACEMENT_3D('',#404980,#122994,#122995);
#102294=AXIS2_PLACEMENT_3D('',#404981,#122996,#122997);
#102295=AXIS2_PLACEMENT_3D('',#404994,#122998,#122999);
#102296=AXIS2_PLACEMENT_3D('',#405007,#123000,#123001);
#102297=AXIS2_PLACEMENT_3D('',#405020,#123002,#123003);
#102298=AXIS2_PLACEMENT_3D('',#405033,#123004,#123005);
#102299=AXIS2_PLACEMENT_3D('',#405046,#123006,#123007);
#102300=AXIS2_PLACEMENT_3D('',#405047,#123008,#123009);
#102301=AXIS2_PLACEMENT_3D('',#405048,#123010,#123011);
#102302=AXIS2_PLACEMENT_3D('',#405061,#123012,#123013);
#102303=AXIS2_PLACEMENT_3D('',#405062,#123014,#123015);
#102304=AXIS2_PLACEMENT_3D('',#405072,#123017,#123018);
#102305=AXIS2_PLACEMENT_3D('',#405082,#123020,#123021);
#102306=AXIS2_PLACEMENT_3D('',#405085,#123022,#123023);
#102307=AXIS2_PLACEMENT_3D('',#405102,#123026,#123027);
#102308=AXIS2_PLACEMENT_3D('',#405152,#123028,#123029);
#102309=AXIS2_PLACEMENT_3D('',#405198,#123030,#123031);
#102310=AXIS2_PLACEMENT_3D('',#405215,#123032,#123033);
#102311=AXIS2_PLACEMENT_3D('',#405267,#123034,#123035);
#102312=AXIS2_PLACEMENT_3D('',#405268,#123036,#123037);
#102313=AXIS2_PLACEMENT_3D('',#405269,#123038,#123039);
#102314=AXIS2_PLACEMENT_3D('',#405270,#123040,#123041);
#102315=AXIS2_PLACEMENT_3D('',#405283,#123042,#123043);
#102316=AXIS2_PLACEMENT_3D('',#405284,#123044,#123045);
#102317=AXIS2_PLACEMENT_3D('',#405285,#123046,#123047);
#102318=AXIS2_PLACEMENT_3D('',#405298,#123048,#123049);
#102319=AXIS2_PLACEMENT_3D('',#405311,#123050,#123051);
#102320=AXIS2_PLACEMENT_3D('',#405324,#123052,#123053);
#102321=AXIS2_PLACEMENT_3D('',#405337,#123054,#123055);
#102322=AXIS2_PLACEMENT_3D('',#405350,#123056,#123057);
#102323=AXIS2_PLACEMENT_3D('',#405351,#123058,#123059);
#102324=AXIS2_PLACEMENT_3D('',#405352,#123060,#123061);
#102325=AXIS2_PLACEMENT_3D('',#405365,#123062,#123063);
#102326=AXIS2_PLACEMENT_3D('',#405366,#123064,#123065);
#102327=AXIS2_PLACEMENT_3D('',#405376,#123067,#123068);
#102328=AXIS2_PLACEMENT_3D('',#405386,#123070,#123071);
#102329=AXIS2_PLACEMENT_3D('',#405389,#123072,#123073);
#102330=AXIS2_PLACEMENT_3D('',#405406,#123076,#123077);
#102331=AXIS2_PLACEMENT_3D('',#405456,#123078,#123079);
#102332=AXIS2_PLACEMENT_3D('',#405502,#123080,#123081);
#102333=AXIS2_PLACEMENT_3D('',#405519,#123082,#123083);
#102334=AXIS2_PLACEMENT_3D('',#405571,#123084,#123085);
#102335=AXIS2_PLACEMENT_3D('',#405572,#123086,#123087);
#102336=AXIS2_PLACEMENT_3D('',#405573,#123088,#123089);
#102337=AXIS2_PLACEMENT_3D('',#405574,#123090,#123091);
#102338=AXIS2_PLACEMENT_3D('',#405587,#123092,#123093);
#102339=AXIS2_PLACEMENT_3D('',#405588,#123094,#123095);
#102340=AXIS2_PLACEMENT_3D('',#405589,#123096,#123097);
#102341=AXIS2_PLACEMENT_3D('',#405602,#123098,#123099);
#102342=AXIS2_PLACEMENT_3D('',#405615,#123100,#123101);
#102343=AXIS2_PLACEMENT_3D('',#405628,#123102,#123103);
#102344=AXIS2_PLACEMENT_3D('',#405641,#123104,#123105);
#102345=AXIS2_PLACEMENT_3D('',#405654,#123106,#123107);
#102346=AXIS2_PLACEMENT_3D('',#405655,#123108,#123109);
#102347=AXIS2_PLACEMENT_3D('',#405656,#123110,#123111);
#102348=AXIS2_PLACEMENT_3D('',#405669,#123112,#123113);
#102349=AXIS2_PLACEMENT_3D('',#405670,#123114,#123115);
#102350=AXIS2_PLACEMENT_3D('',#405680,#123117,#123118);
#102351=AXIS2_PLACEMENT_3D('',#405690,#123120,#123121);
#102352=AXIS2_PLACEMENT_3D('',#405693,#123122,#123123);
#102353=AXIS2_PLACEMENT_3D('',#405710,#123126,#123127);
#102354=AXIS2_PLACEMENT_3D('',#405760,#123128,#123129);
#102355=AXIS2_PLACEMENT_3D('',#405806,#123130,#123131);
#102356=AXIS2_PLACEMENT_3D('',#405823,#123132,#123133);
#102357=AXIS2_PLACEMENT_3D('',#405875,#123134,#123135);
#102358=AXIS2_PLACEMENT_3D('',#405876,#123136,#123137);
#102359=AXIS2_PLACEMENT_3D('',#405877,#123138,#123139);
#102360=AXIS2_PLACEMENT_3D('',#405878,#123140,#123141);
#102361=AXIS2_PLACEMENT_3D('',#405891,#123142,#123143);
#102362=AXIS2_PLACEMENT_3D('',#405892,#123144,#123145);
#102363=AXIS2_PLACEMENT_3D('',#405893,#123146,#123147);
#102364=AXIS2_PLACEMENT_3D('',#405906,#123148,#123149);
#102365=AXIS2_PLACEMENT_3D('',#405919,#123150,#123151);
#102366=AXIS2_PLACEMENT_3D('',#405932,#123152,#123153);
#102367=AXIS2_PLACEMENT_3D('',#405945,#123154,#123155);
#102368=AXIS2_PLACEMENT_3D('',#405958,#123156,#123157);
#102369=AXIS2_PLACEMENT_3D('',#405959,#123158,#123159);
#102370=AXIS2_PLACEMENT_3D('',#405960,#123160,#123161);
#102371=AXIS2_PLACEMENT_3D('',#405973,#123162,#123163);
#102372=AXIS2_PLACEMENT_3D('',#405974,#123164,#123165);
#102373=AXIS2_PLACEMENT_3D('',#405984,#123167,#123168);
#102374=AXIS2_PLACEMENT_3D('',#405994,#123170,#123171);
#102375=AXIS2_PLACEMENT_3D('',#405997,#123172,#123173);
#102376=AXIS2_PLACEMENT_3D('',#406014,#123176,#123177);
#102377=AXIS2_PLACEMENT_3D('',#406064,#123178,#123179);
#102378=AXIS2_PLACEMENT_3D('',#406110,#123180,#123181);
#102379=AXIS2_PLACEMENT_3D('',#406127,#123182,#123183);
#102380=AXIS2_PLACEMENT_3D('',#406179,#123184,#123185);
#102381=AXIS2_PLACEMENT_3D('',#406180,#123186,#123187);
#102382=AXIS2_PLACEMENT_3D('',#406181,#123188,#123189);
#102383=AXIS2_PLACEMENT_3D('',#406182,#123190,#123191);
#102384=AXIS2_PLACEMENT_3D('',#406195,#123192,#123193);
#102385=AXIS2_PLACEMENT_3D('',#406196,#123194,#123195);
#102386=AXIS2_PLACEMENT_3D('',#406197,#123196,#123197);
#102387=AXIS2_PLACEMENT_3D('',#406210,#123198,#123199);
#102388=AXIS2_PLACEMENT_3D('',#406223,#123200,#123201);
#102389=AXIS2_PLACEMENT_3D('',#406236,#123202,#123203);
#102390=AXIS2_PLACEMENT_3D('',#406249,#123204,#123205);
#102391=AXIS2_PLACEMENT_3D('',#406262,#123206,#123207);
#102392=AXIS2_PLACEMENT_3D('',#406263,#123208,#123209);
#102393=AXIS2_PLACEMENT_3D('',#406264,#123210,#123211);
#102394=AXIS2_PLACEMENT_3D('',#406277,#123212,#123213);
#102395=AXIS2_PLACEMENT_3D('',#406278,#123214,#123215);
#102396=AXIS2_PLACEMENT_3D('',#406288,#123217,#123218);
#102397=AXIS2_PLACEMENT_3D('',#406298,#123220,#123221);
#102398=AXIS2_PLACEMENT_3D('',#406301,#123222,#123223);
#102399=AXIS2_PLACEMENT_3D('',#406318,#123226,#123227);
#102400=AXIS2_PLACEMENT_3D('',#406368,#123228,#123229);
#102401=AXIS2_PLACEMENT_3D('',#406414,#123230,#123231);
#102402=AXIS2_PLACEMENT_3D('',#406431,#123232,#123233);
#102403=AXIS2_PLACEMENT_3D('',#406483,#123234,#123235);
#102404=AXIS2_PLACEMENT_3D('',#406484,#123236,#123237);
#102405=AXIS2_PLACEMENT_3D('',#406485,#123238,#123239);
#102406=AXIS2_PLACEMENT_3D('',#406486,#123240,#123241);
#102407=AXIS2_PLACEMENT_3D('',#406499,#123242,#123243);
#102408=AXIS2_PLACEMENT_3D('',#406500,#123244,#123245);
#102409=AXIS2_PLACEMENT_3D('',#406501,#123246,#123247);
#102410=AXIS2_PLACEMENT_3D('',#406514,#123248,#123249);
#102411=AXIS2_PLACEMENT_3D('',#406527,#123250,#123251);
#102412=AXIS2_PLACEMENT_3D('',#406540,#123252,#123253);
#102413=AXIS2_PLACEMENT_3D('',#406553,#123254,#123255);
#102414=AXIS2_PLACEMENT_3D('',#406566,#123256,#123257);
#102415=AXIS2_PLACEMENT_3D('',#406567,#123258,#123259);
#102416=AXIS2_PLACEMENT_3D('',#406568,#123260,#123261);
#102417=AXIS2_PLACEMENT_3D('',#406581,#123262,#123263);
#102418=AXIS2_PLACEMENT_3D('',#406582,#123264,#123265);
#102419=AXIS2_PLACEMENT_3D('',#406592,#123267,#123268);
#102420=AXIS2_PLACEMENT_3D('',#406602,#123270,#123271);
#102421=AXIS2_PLACEMENT_3D('',#406605,#123272,#123273);
#102422=AXIS2_PLACEMENT_3D('',#406622,#123276,#123277);
#102423=AXIS2_PLACEMENT_3D('',#406672,#123278,#123279);
#102424=AXIS2_PLACEMENT_3D('',#406718,#123280,#123281);
#102425=AXIS2_PLACEMENT_3D('',#406735,#123282,#123283);
#102426=AXIS2_PLACEMENT_3D('',#406787,#123284,#123285);
#102427=AXIS2_PLACEMENT_3D('',#406788,#123286,#123287);
#102428=AXIS2_PLACEMENT_3D('',#406789,#123288,#123289);
#102429=AXIS2_PLACEMENT_3D('',#406790,#123290,#123291);
#102430=AXIS2_PLACEMENT_3D('',#406803,#123292,#123293);
#102431=AXIS2_PLACEMENT_3D('',#406804,#123294,#123295);
#102432=AXIS2_PLACEMENT_3D('',#406805,#123296,#123297);
#102433=AXIS2_PLACEMENT_3D('',#406818,#123298,#123299);
#102434=AXIS2_PLACEMENT_3D('',#406831,#123300,#123301);
#102435=AXIS2_PLACEMENT_3D('',#406844,#123302,#123303);
#102436=AXIS2_PLACEMENT_3D('',#406857,#123304,#123305);
#102437=AXIS2_PLACEMENT_3D('',#406870,#123306,#123307);
#102438=AXIS2_PLACEMENT_3D('',#406871,#123308,#123309);
#102439=AXIS2_PLACEMENT_3D('',#406872,#123310,#123311);
#102440=AXIS2_PLACEMENT_3D('',#406885,#123312,#123313);
#102441=AXIS2_PLACEMENT_3D('',#406886,#123314,#123315);
#102442=AXIS2_PLACEMENT_3D('',#406896,#123317,#123318);
#102443=AXIS2_PLACEMENT_3D('',#406906,#123320,#123321);
#102444=AXIS2_PLACEMENT_3D('',#406909,#123322,#123323);
#102445=AXIS2_PLACEMENT_3D('',#406926,#123326,#123327);
#102446=AXIS2_PLACEMENT_3D('',#406976,#123328,#123329);
#102447=AXIS2_PLACEMENT_3D('',#407022,#123330,#123331);
#102448=AXIS2_PLACEMENT_3D('',#407039,#123332,#123333);
#102449=AXIS2_PLACEMENT_3D('',#407091,#123334,#123335);
#102450=AXIS2_PLACEMENT_3D('',#407092,#123336,#123337);
#102451=AXIS2_PLACEMENT_3D('',#407093,#123338,#123339);
#102452=AXIS2_PLACEMENT_3D('',#407094,#123340,#123341);
#102453=AXIS2_PLACEMENT_3D('',#407107,#123342,#123343);
#102454=AXIS2_PLACEMENT_3D('',#407108,#123344,#123345);
#102455=AXIS2_PLACEMENT_3D('',#407109,#123346,#123347);
#102456=AXIS2_PLACEMENT_3D('',#407122,#123348,#123349);
#102457=AXIS2_PLACEMENT_3D('',#407135,#123350,#123351);
#102458=AXIS2_PLACEMENT_3D('',#407148,#123352,#123353);
#102459=AXIS2_PLACEMENT_3D('',#407161,#123354,#123355);
#102460=AXIS2_PLACEMENT_3D('',#407174,#123356,#123357);
#102461=AXIS2_PLACEMENT_3D('',#407175,#123358,#123359);
#102462=AXIS2_PLACEMENT_3D('',#407176,#123360,#123361);
#102463=AXIS2_PLACEMENT_3D('',#407189,#123362,#123363);
#102464=AXIS2_PLACEMENT_3D('',#407190,#123364,#123365);
#102465=AXIS2_PLACEMENT_3D('',#407200,#123367,#123368);
#102466=AXIS2_PLACEMENT_3D('',#407210,#123370,#123371);
#102467=AXIS2_PLACEMENT_3D('',#407213,#123372,#123373);
#102468=AXIS2_PLACEMENT_3D('',#407230,#123376,#123377);
#102469=AXIS2_PLACEMENT_3D('',#407280,#123378,#123379);
#102470=AXIS2_PLACEMENT_3D('',#407326,#123380,#123381);
#102471=AXIS2_PLACEMENT_3D('',#407343,#123382,#123383);
#102472=AXIS2_PLACEMENT_3D('',#407395,#123384,#123385);
#102473=AXIS2_PLACEMENT_3D('',#407396,#123386,#123387);
#102474=AXIS2_PLACEMENT_3D('',#407397,#123388,#123389);
#102475=AXIS2_PLACEMENT_3D('',#407398,#123390,#123391);
#102476=AXIS2_PLACEMENT_3D('',#407411,#123392,#123393);
#102477=AXIS2_PLACEMENT_3D('',#407412,#123394,#123395);
#102478=AXIS2_PLACEMENT_3D('',#407413,#123396,#123397);
#102479=AXIS2_PLACEMENT_3D('',#407426,#123398,#123399);
#102480=AXIS2_PLACEMENT_3D('',#407439,#123400,#123401);
#102481=AXIS2_PLACEMENT_3D('',#407452,#123402,#123403);
#102482=AXIS2_PLACEMENT_3D('',#407465,#123404,#123405);
#102483=AXIS2_PLACEMENT_3D('',#407478,#123406,#123407);
#102484=AXIS2_PLACEMENT_3D('',#407479,#123408,#123409);
#102485=AXIS2_PLACEMENT_3D('',#407480,#123410,#123411);
#102486=AXIS2_PLACEMENT_3D('',#407493,#123412,#123413);
#102487=AXIS2_PLACEMENT_3D('',#407494,#123414,#123415);
#102488=AXIS2_PLACEMENT_3D('',#407504,#123417,#123418);
#102489=AXIS2_PLACEMENT_3D('',#407514,#123420,#123421);
#102490=AXIS2_PLACEMENT_3D('',#407517,#123422,#123423);
#102491=AXIS2_PLACEMENT_3D('',#407534,#123426,#123427);
#102492=AXIS2_PLACEMENT_3D('',#407584,#123428,#123429);
#102493=AXIS2_PLACEMENT_3D('',#407630,#123430,#123431);
#102494=AXIS2_PLACEMENT_3D('',#407647,#123432,#123433);
#102495=AXIS2_PLACEMENT_3D('',#407699,#123434,#123435);
#102496=AXIS2_PLACEMENT_3D('',#407700,#123436,#123437);
#102497=AXIS2_PLACEMENT_3D('',#407701,#123438,#123439);
#102498=AXIS2_PLACEMENT_3D('',#407702,#123440,#123441);
#102499=AXIS2_PLACEMENT_3D('',#407715,#123442,#123443);
#102500=AXIS2_PLACEMENT_3D('',#407716,#123444,#123445);
#102501=AXIS2_PLACEMENT_3D('',#407717,#123446,#123447);
#102502=AXIS2_PLACEMENT_3D('',#407730,#123448,#123449);
#102503=AXIS2_PLACEMENT_3D('',#407743,#123450,#123451);
#102504=AXIS2_PLACEMENT_3D('',#407756,#123452,#123453);
#102505=AXIS2_PLACEMENT_3D('',#407769,#123454,#123455);
#102506=AXIS2_PLACEMENT_3D('',#407782,#123456,#123457);
#102507=AXIS2_PLACEMENT_3D('',#407783,#123458,#123459);
#102508=AXIS2_PLACEMENT_3D('',#407784,#123460,#123461);
#102509=AXIS2_PLACEMENT_3D('',#407797,#123462,#123463);
#102510=AXIS2_PLACEMENT_3D('',#407798,#123464,#123465);
#102511=AXIS2_PLACEMENT_3D('',#407808,#123467,#123468);
#102512=AXIS2_PLACEMENT_3D('',#407818,#123470,#123471);
#102513=AXIS2_PLACEMENT_3D('',#407821,#123472,#123473);
#102514=AXIS2_PLACEMENT_3D('',#407838,#123476,#123477);
#102515=AXIS2_PLACEMENT_3D('',#407888,#123478,#123479);
#102516=AXIS2_PLACEMENT_3D('',#407934,#123480,#123481);
#102517=AXIS2_PLACEMENT_3D('',#407951,#123482,#123483);
#102518=AXIS2_PLACEMENT_3D('',#408003,#123484,#123485);
#102519=AXIS2_PLACEMENT_3D('',#408004,#123486,#123487);
#102520=AXIS2_PLACEMENT_3D('',#408005,#123488,#123489);
#102521=AXIS2_PLACEMENT_3D('',#408006,#123490,#123491);
#102522=AXIS2_PLACEMENT_3D('',#408019,#123492,#123493);
#102523=AXIS2_PLACEMENT_3D('',#408020,#123494,#123495);
#102524=AXIS2_PLACEMENT_3D('',#408021,#123496,#123497);
#102525=AXIS2_PLACEMENT_3D('',#408034,#123498,#123499);
#102526=AXIS2_PLACEMENT_3D('',#408047,#123500,#123501);
#102527=AXIS2_PLACEMENT_3D('',#408060,#123502,#123503);
#102528=AXIS2_PLACEMENT_3D('',#408073,#123504,#123505);
#102529=AXIS2_PLACEMENT_3D('',#408086,#123506,#123507);
#102530=AXIS2_PLACEMENT_3D('',#408087,#123508,#123509);
#102531=AXIS2_PLACEMENT_3D('',#408088,#123510,#123511);
#102532=AXIS2_PLACEMENT_3D('',#408101,#123512,#123513);
#102533=AXIS2_PLACEMENT_3D('',#408102,#123514,#123515);
#102534=AXIS2_PLACEMENT_3D('',#408112,#123517,#123518);
#102535=AXIS2_PLACEMENT_3D('',#408122,#123520,#123521);
#102536=AXIS2_PLACEMENT_3D('',#408125,#123522,#123523);
#102537=AXIS2_PLACEMENT_3D('',#408142,#123526,#123527);
#102538=AXIS2_PLACEMENT_3D('',#408192,#123528,#123529);
#102539=AXIS2_PLACEMENT_3D('',#408238,#123530,#123531);
#102540=AXIS2_PLACEMENT_3D('',#408255,#123532,#123533);
#102541=AXIS2_PLACEMENT_3D('',#408307,#123534,#123535);
#102542=AXIS2_PLACEMENT_3D('',#408308,#123536,#123537);
#102543=AXIS2_PLACEMENT_3D('',#408309,#123538,#123539);
#102544=AXIS2_PLACEMENT_3D('',#408310,#123540,#123541);
#102545=AXIS2_PLACEMENT_3D('',#408323,#123542,#123543);
#102546=AXIS2_PLACEMENT_3D('',#408324,#123544,#123545);
#102547=AXIS2_PLACEMENT_3D('',#408325,#123546,#123547);
#102548=AXIS2_PLACEMENT_3D('',#408338,#123548,#123549);
#102549=AXIS2_PLACEMENT_3D('',#408351,#123550,#123551);
#102550=AXIS2_PLACEMENT_3D('',#408364,#123552,#123553);
#102551=AXIS2_PLACEMENT_3D('',#408377,#123554,#123555);
#102552=AXIS2_PLACEMENT_3D('',#408390,#123556,#123557);
#102553=AXIS2_PLACEMENT_3D('',#408391,#123558,#123559);
#102554=AXIS2_PLACEMENT_3D('',#408392,#123560,#123561);
#102555=AXIS2_PLACEMENT_3D('',#408405,#123562,#123563);
#102556=AXIS2_PLACEMENT_3D('',#408406,#123564,#123565);
#102557=AXIS2_PLACEMENT_3D('',#408416,#123567,#123568);
#102558=AXIS2_PLACEMENT_3D('',#408426,#123570,#123571);
#102559=AXIS2_PLACEMENT_3D('',#408429,#123572,#123573);
#102560=AXIS2_PLACEMENT_3D('',#408446,#123576,#123577);
#102561=AXIS2_PLACEMENT_3D('',#408496,#123578,#123579);
#102562=AXIS2_PLACEMENT_3D('',#408542,#123580,#123581);
#102563=AXIS2_PLACEMENT_3D('',#408559,#123582,#123583);
#102564=AXIS2_PLACEMENT_3D('',#408611,#123584,#123585);
#102565=AXIS2_PLACEMENT_3D('',#408612,#123586,#123587);
#102566=AXIS2_PLACEMENT_3D('',#408613,#123588,#123589);
#102567=AXIS2_PLACEMENT_3D('',#408614,#123590,#123591);
#102568=AXIS2_PLACEMENT_3D('',#408627,#123592,#123593);
#102569=AXIS2_PLACEMENT_3D('',#408628,#123594,#123595);
#102570=AXIS2_PLACEMENT_3D('',#408629,#123596,#123597);
#102571=AXIS2_PLACEMENT_3D('',#408642,#123598,#123599);
#102572=AXIS2_PLACEMENT_3D('',#408655,#123600,#123601);
#102573=AXIS2_PLACEMENT_3D('',#408668,#123602,#123603);
#102574=AXIS2_PLACEMENT_3D('',#408681,#123604,#123605);
#102575=AXIS2_PLACEMENT_3D('',#408694,#123606,#123607);
#102576=AXIS2_PLACEMENT_3D('',#408695,#123608,#123609);
#102577=AXIS2_PLACEMENT_3D('',#408696,#123610,#123611);
#102578=AXIS2_PLACEMENT_3D('',#408709,#123612,#123613);
#102579=AXIS2_PLACEMENT_3D('',#408710,#123614,#123615);
#102580=AXIS2_PLACEMENT_3D('',#408720,#123617,#123618);
#102581=AXIS2_PLACEMENT_3D('',#408730,#123620,#123621);
#102582=AXIS2_PLACEMENT_3D('',#408733,#123622,#123623);
#102583=AXIS2_PLACEMENT_3D('',#408750,#123626,#123627);
#102584=AXIS2_PLACEMENT_3D('',#408800,#123628,#123629);
#102585=AXIS2_PLACEMENT_3D('',#408846,#123630,#123631);
#102586=AXIS2_PLACEMENT_3D('',#408863,#123632,#123633);
#102587=AXIS2_PLACEMENT_3D('',#408915,#123634,#123635);
#102588=AXIS2_PLACEMENT_3D('',#408916,#123636,#123637);
#102589=AXIS2_PLACEMENT_3D('',#408917,#123638,#123639);
#102590=AXIS2_PLACEMENT_3D('',#408918,#123640,#123641);
#102591=AXIS2_PLACEMENT_3D('',#408931,#123642,#123643);
#102592=AXIS2_PLACEMENT_3D('',#408932,#123644,#123645);
#102593=AXIS2_PLACEMENT_3D('',#408933,#123646,#123647);
#102594=AXIS2_PLACEMENT_3D('',#408946,#123648,#123649);
#102595=AXIS2_PLACEMENT_3D('',#408959,#123650,#123651);
#102596=AXIS2_PLACEMENT_3D('',#408972,#123652,#123653);
#102597=AXIS2_PLACEMENT_3D('',#408985,#123654,#123655);
#102598=AXIS2_PLACEMENT_3D('',#408998,#123656,#123657);
#102599=AXIS2_PLACEMENT_3D('',#408999,#123658,#123659);
#102600=AXIS2_PLACEMENT_3D('',#409000,#123660,#123661);
#102601=AXIS2_PLACEMENT_3D('',#409013,#123662,#123663);
#102602=AXIS2_PLACEMENT_3D('',#409014,#123664,#123665);
#102603=AXIS2_PLACEMENT_3D('',#409024,#123667,#123668);
#102604=AXIS2_PLACEMENT_3D('',#409034,#123670,#123671);
#102605=AXIS2_PLACEMENT_3D('',#409037,#123672,#123673);
#102606=AXIS2_PLACEMENT_3D('',#409054,#123676,#123677);
#102607=AXIS2_PLACEMENT_3D('',#409104,#123678,#123679);
#102608=AXIS2_PLACEMENT_3D('',#409150,#123680,#123681);
#102609=AXIS2_PLACEMENT_3D('',#409167,#123682,#123683);
#102610=AXIS2_PLACEMENT_3D('',#409219,#123684,#123685);
#102611=AXIS2_PLACEMENT_3D('',#409220,#123686,#123687);
#102612=AXIS2_PLACEMENT_3D('',#409221,#123688,#123689);
#102613=AXIS2_PLACEMENT_3D('',#409222,#123690,#123691);
#102614=AXIS2_PLACEMENT_3D('',#409235,#123692,#123693);
#102615=AXIS2_PLACEMENT_3D('',#409236,#123694,#123695);
#102616=AXIS2_PLACEMENT_3D('',#409237,#123696,#123697);
#102617=AXIS2_PLACEMENT_3D('',#409250,#123698,#123699);
#102618=AXIS2_PLACEMENT_3D('',#409263,#123700,#123701);
#102619=AXIS2_PLACEMENT_3D('',#409276,#123702,#123703);
#102620=AXIS2_PLACEMENT_3D('',#409289,#123704,#123705);
#102621=AXIS2_PLACEMENT_3D('',#409302,#123706,#123707);
#102622=AXIS2_PLACEMENT_3D('',#409303,#123708,#123709);
#102623=AXIS2_PLACEMENT_3D('',#409304,#123710,#123711);
#102624=AXIS2_PLACEMENT_3D('',#409317,#123712,#123713);
#102625=AXIS2_PLACEMENT_3D('',#409318,#123714,#123715);
#102626=AXIS2_PLACEMENT_3D('',#409328,#123717,#123718);
#102627=AXIS2_PLACEMENT_3D('',#409338,#123720,#123721);
#102628=AXIS2_PLACEMENT_3D('',#409341,#123722,#123723);
#102629=AXIS2_PLACEMENT_3D('',#409358,#123726,#123727);
#102630=AXIS2_PLACEMENT_3D('',#409408,#123728,#123729);
#102631=AXIS2_PLACEMENT_3D('',#409454,#123730,#123731);
#102632=AXIS2_PLACEMENT_3D('',#409471,#123732,#123733);
#102633=AXIS2_PLACEMENT_3D('',#409523,#123734,#123735);
#102634=AXIS2_PLACEMENT_3D('',#409524,#123736,#123737);
#102635=AXIS2_PLACEMENT_3D('',#409525,#123738,#123739);
#102636=AXIS2_PLACEMENT_3D('',#409526,#123740,#123741);
#102637=AXIS2_PLACEMENT_3D('',#409539,#123742,#123743);
#102638=AXIS2_PLACEMENT_3D('',#409540,#123744,#123745);
#102639=AXIS2_PLACEMENT_3D('',#409541,#123746,#123747);
#102640=AXIS2_PLACEMENT_3D('',#409554,#123748,#123749);
#102641=AXIS2_PLACEMENT_3D('',#409567,#123750,#123751);
#102642=AXIS2_PLACEMENT_3D('',#409580,#123752,#123753);
#102643=AXIS2_PLACEMENT_3D('',#409593,#123754,#123755);
#102644=AXIS2_PLACEMENT_3D('',#409606,#123756,#123757);
#102645=AXIS2_PLACEMENT_3D('',#409607,#123758,#123759);
#102646=AXIS2_PLACEMENT_3D('',#409608,#123760,#123761);
#102647=AXIS2_PLACEMENT_3D('',#409621,#123762,#123763);
#102648=AXIS2_PLACEMENT_3D('',#409622,#123764,#123765);
#102649=AXIS2_PLACEMENT_3D('',#409623,#123766,#123767);
#102650=AXIS2_PLACEMENT_3D('',#409631,#123769,#123770);
#102651=AXIS2_PLACEMENT_3D('',#409632,#123771,#123772);
#102652=AXIS2_PLACEMENT_3D('',#409662,#123774,#123775);
#102653=AXIS2_PLACEMENT_3D('',#409692,#123777,#123778);
#102654=AXIS2_PLACEMENT_3D('',#409722,#123780,#123781);
#102655=AXIS2_PLACEMENT_3D('',#409752,#123783,#123784);
#102656=AXIS2_PLACEMENT_3D('',#409782,#123786,#123787);
#102657=AXIS2_PLACEMENT_3D('',#409812,#123789,#123790);
#102658=AXIS2_PLACEMENT_3D('',#409842,#123792,#123793);
#102659=AXIS2_PLACEMENT_3D('',#409872,#123795,#123796);
#102660=AXIS2_PLACEMENT_3D('',#409902,#123798,#123799);
#102661=AXIS2_PLACEMENT_3D('',#409932,#123801,#123802);
#102662=AXIS2_PLACEMENT_3D('',#409962,#123804,#123805);
#102663=AXIS2_PLACEMENT_3D('',#409992,#123807,#123808);
#102664=AXIS2_PLACEMENT_3D('',#410022,#123810,#123811);
#102665=AXIS2_PLACEMENT_3D('',#410052,#123813,#123814);
#102666=AXIS2_PLACEMENT_3D('',#410082,#123816,#123817);
#102667=AXIS2_PLACEMENT_3D('',#410112,#123819,#123820);
#102668=AXIS2_PLACEMENT_3D('',#410142,#123822,#123823);
#102669=AXIS2_PLACEMENT_3D('',#410172,#123825,#123826);
#102670=AXIS2_PLACEMENT_3D('',#410202,#123828,#123829);
#102671=AXIS2_PLACEMENT_3D('',#410232,#123831,#123832);
#102672=AXIS2_PLACEMENT_3D('',#410262,#123834,#123835);
#102673=AXIS2_PLACEMENT_3D('',#410292,#123837,#123838);
#102674=AXIS2_PLACEMENT_3D('',#410322,#123840,#123841);
#102675=AXIS2_PLACEMENT_3D('',#410352,#123843,#123844);
#102676=AXIS2_PLACEMENT_3D('',#410382,#123846,#123847);
#102677=AXIS2_PLACEMENT_3D('',#410412,#123849,#123850);
#102678=AXIS2_PLACEMENT_3D('',#410442,#123852,#123853);
#102679=AXIS2_PLACEMENT_3D('',#410472,#123855,#123856);
#102680=AXIS2_PLACEMENT_3D('',#410502,#123858,#123859);
#102681=AXIS2_PLACEMENT_3D('',#410532,#123861,#123862);
#102682=AXIS2_PLACEMENT_3D('',#410562,#123864,#123865);
#102683=AXIS2_PLACEMENT_3D('',#410592,#123867,#123868);
#102684=AXIS2_PLACEMENT_3D('',#410622,#123870,#123871);
#102685=AXIS2_PLACEMENT_3D('',#410652,#123873,#123874);
#102686=AXIS2_PLACEMENT_3D('',#410682,#123876,#123877);
#102687=AXIS2_PLACEMENT_3D('',#410702,#123879,#123880);
#102688=AXIS2_PLACEMENT_3D('',#410713,#123881,#123882);
#102689=AXIS2_PLACEMENT_3D('',#410737,#123884,#123885);
#102690=AXIS2_PLACEMENT_3D('',#410738,#123886,#123887);
#102691=AXIS2_PLACEMENT_3D('',#410762,#123889,#123890);
#102692=AXIS2_PLACEMENT_3D('',#410779,#123891,#123892);
#102693=AXIS2_PLACEMENT_3D('',#410855,#123894,#123895);
#102694=AXIS2_PLACEMENT_3D('',#410933,#123897,#123898);
#102695=AXIS2_PLACEMENT_3D('',#411011,#123900,#123901);
#102696=AXIS2_PLACEMENT_3D('',#411087,#123903,#123904);
#102697=AXIS2_PLACEMENT_3D('',#411163,#123906,#123907);
#102698=AXIS2_PLACEMENT_3D('',#411239,#123909,#123910);
#102699=AXIS2_PLACEMENT_3D('',#411317,#123912,#123913);
#102700=AXIS2_PLACEMENT_3D('',#411393,#123915,#123916);
#102701=AXIS2_PLACEMENT_3D('',#411469,#123918,#123919);
#102702=AXIS2_PLACEMENT_3D('',#411547,#123921,#123922);
#102703=AXIS2_PLACEMENT_3D('',#411623,#123924,#123925);
#102704=AXIS2_PLACEMENT_3D('',#411699,#123927,#123928);
#102705=AXIS2_PLACEMENT_3D('',#411775,#123930,#123931);
#102706=AXIS2_PLACEMENT_3D('',#411853,#123933,#123934);
#102707=AXIS2_PLACEMENT_3D('',#411929,#123936,#123937);
#102708=AXIS2_PLACEMENT_3D('',#412005,#123939,#123940);
#102709=AXIS2_PLACEMENT_3D('',#412083,#123942,#123943);
#102710=AXIS2_PLACEMENT_3D('',#412159,#123945,#123946);
#102711=AXIS2_PLACEMENT_3D('',#412235,#123948,#123949);
#102712=AXIS2_PLACEMENT_3D('',#412313,#123951,#123952);
#102713=AXIS2_PLACEMENT_3D('',#412389,#123954,#123955);
#102714=AXIS2_PLACEMENT_3D('',#412465,#123957,#123958);
#102715=AXIS2_PLACEMENT_3D('',#412543,#123960,#123961);
#102716=AXIS2_PLACEMENT_3D('',#412619,#123963,#123964);
#102717=AXIS2_PLACEMENT_3D('',#412695,#123966,#123967);
#102718=AXIS2_PLACEMENT_3D('',#412771,#123969,#123970);
#102719=AXIS2_PLACEMENT_3D('',#412849,#123972,#123973);
#102720=AXIS2_PLACEMENT_3D('',#412925,#123975,#123976);
#102721=AXIS2_PLACEMENT_3D('',#413001,#123978,#123979);
#102722=AXIS2_PLACEMENT_3D('',#413079,#123981,#123982);
#102723=AXIS2_PLACEMENT_3D('',#413160,#123984,#123985);
#102724=AXIS2_PLACEMENT_3D('',#413236,#123987,#123988);
#102725=AXIS2_PLACEMENT_3D('',#413314,#123990,#123991);
#102726=AXIS2_PLACEMENT_3D('',#413316,#123992,#123993);
#102727=AXIS2_PLACEMENT_3D('',#413319,#123995,#123996);
#102728=AXIS2_PLACEMENT_3D('',#413391,#123998,#123999);
#102729=AXIS2_PLACEMENT_3D('',#413394,#124000,#124001);
#102730=AXIS2_PLACEMENT_3D('',#413396,#124002,#124003);
#102731=AXIS2_PLACEMENT_3D('',#413398,#124004,#124005);
#102732=AXIS2_PLACEMENT_3D('',#413399,#124006,#124007);
#102733=AXIS2_PLACEMENT_3D('',#413400,#124008,#124009);
#102734=AXIS2_PLACEMENT_3D('',#413403,#124010,#124011);
#102735=AXIS2_PLACEMENT_3D('',#413405,#124012,#124013);
#102736=AXIS2_PLACEMENT_3D('',#413407,#124014,#124015);
#102737=AXIS2_PLACEMENT_3D('',#413408,#124016,#124017);
#102738=AXIS2_PLACEMENT_3D('',#413409,#124018,#124019);
#102739=AXIS2_PLACEMENT_3D('',#413412,#124020,#124021);
#102740=AXIS2_PLACEMENT_3D('',#413414,#124022,#124023);
#102741=AXIS2_PLACEMENT_3D('',#413416,#124024,#124025);
#102742=AXIS2_PLACEMENT_3D('',#413417,#124026,#124027);
#102743=AXIS2_PLACEMENT_3D('',#413418,#124028,#124029);
#102744=AXIS2_PLACEMENT_3D('',#413421,#124030,#124031);
#102745=AXIS2_PLACEMENT_3D('',#413423,#124032,#124033);
#102746=AXIS2_PLACEMENT_3D('',#413425,#124034,#124035);
#102747=AXIS2_PLACEMENT_3D('',#413426,#124036,#124037);
#102748=AXIS2_PLACEMENT_3D('',#413427,#124038,#124039);
#102749=AXIS2_PLACEMENT_3D('',#413430,#124040,#124041);
#102750=AXIS2_PLACEMENT_3D('',#413432,#124042,#124043);
#102751=AXIS2_PLACEMENT_3D('',#413434,#124044,#124045);
#102752=AXIS2_PLACEMENT_3D('',#413435,#124046,#124047);
#102753=AXIS2_PLACEMENT_3D('',#413436,#124048,#124049);
#102754=AXIS2_PLACEMENT_3D('',#413439,#124050,#124051);
#102755=AXIS2_PLACEMENT_3D('',#413441,#124052,#124053);
#102756=AXIS2_PLACEMENT_3D('',#413443,#124054,#124055);
#102757=AXIS2_PLACEMENT_3D('',#413444,#124056,#124057);
#102758=AXIS2_PLACEMENT_3D('',#413445,#124058,#124059);
#102759=AXIS2_PLACEMENT_3D('',#413448,#124060,#124061);
#102760=AXIS2_PLACEMENT_3D('',#413450,#124062,#124063);
#102761=AXIS2_PLACEMENT_3D('',#413452,#124064,#124065);
#102762=AXIS2_PLACEMENT_3D('',#413453,#124066,#124067);
#102763=AXIS2_PLACEMENT_3D('',#413454,#124068,#124069);
#102764=AXIS2_PLACEMENT_3D('',#413457,#124070,#124071);
#102765=AXIS2_PLACEMENT_3D('',#413459,#124072,#124073);
#102766=AXIS2_PLACEMENT_3D('',#413461,#124074,#124075);
#102767=AXIS2_PLACEMENT_3D('',#413462,#124076,#124077);
#102768=AXIS2_PLACEMENT_3D('',#413463,#124078,#124079);
#102769=AXIS2_PLACEMENT_3D('',#413466,#124080,#124081);
#102770=AXIS2_PLACEMENT_3D('',#413468,#124082,#124083);
#102771=AXIS2_PLACEMENT_3D('',#413470,#124084,#124085);
#102772=AXIS2_PLACEMENT_3D('',#413471,#124086,#124087);
#102773=AXIS2_PLACEMENT_3D('',#413472,#124088,#124089);
#102774=AXIS2_PLACEMENT_3D('',#413475,#124090,#124091);
#102775=AXIS2_PLACEMENT_3D('',#413477,#124092,#124093);
#102776=AXIS2_PLACEMENT_3D('',#413479,#124094,#124095);
#102777=AXIS2_PLACEMENT_3D('',#413480,#124096,#124097);
#102778=AXIS2_PLACEMENT_3D('',#413481,#124098,#124099);
#102779=AXIS2_PLACEMENT_3D('',#413484,#124100,#124101);
#102780=AXIS2_PLACEMENT_3D('',#413486,#124102,#124103);
#102781=AXIS2_PLACEMENT_3D('',#413488,#124104,#124105);
#102782=AXIS2_PLACEMENT_3D('',#413489,#124106,#124107);
#102783=AXIS2_PLACEMENT_3D('',#413490,#124108,#124109);
#102784=AXIS2_PLACEMENT_3D('',#413493,#124110,#124111);
#102785=AXIS2_PLACEMENT_3D('',#413495,#124112,#124113);
#102786=AXIS2_PLACEMENT_3D('',#413497,#124114,#124115);
#102787=AXIS2_PLACEMENT_3D('',#413498,#124116,#124117);
#102788=AXIS2_PLACEMENT_3D('',#413499,#124118,#124119);
#102789=AXIS2_PLACEMENT_3D('',#413502,#124120,#124121);
#102790=AXIS2_PLACEMENT_3D('',#413504,#124122,#124123);
#102791=AXIS2_PLACEMENT_3D('',#413506,#124124,#124125);
#102792=AXIS2_PLACEMENT_3D('',#413507,#124126,#124127);
#102793=AXIS2_PLACEMENT_3D('',#413508,#124128,#124129);
#102794=AXIS2_PLACEMENT_3D('',#413511,#124130,#124131);
#102795=AXIS2_PLACEMENT_3D('',#413513,#124132,#124133);
#102796=AXIS2_PLACEMENT_3D('',#413515,#124134,#124135);
#102797=AXIS2_PLACEMENT_3D('',#413516,#124136,#124137);
#102798=AXIS2_PLACEMENT_3D('',#413517,#124138,#124139);
#102799=AXIS2_PLACEMENT_3D('',#413520,#124140,#124141);
#102800=AXIS2_PLACEMENT_3D('',#413522,#124142,#124143);
#102801=AXIS2_PLACEMENT_3D('',#413524,#124144,#124145);
#102802=AXIS2_PLACEMENT_3D('',#413525,#124146,#124147);
#102803=AXIS2_PLACEMENT_3D('',#413526,#124148,#124149);
#102804=AXIS2_PLACEMENT_3D('',#413529,#124150,#124151);
#102805=AXIS2_PLACEMENT_3D('',#413531,#124152,#124153);
#102806=AXIS2_PLACEMENT_3D('',#413533,#124154,#124155);
#102807=AXIS2_PLACEMENT_3D('',#413534,#124156,#124157);
#102808=AXIS2_PLACEMENT_3D('',#413535,#124158,#124159);
#102809=AXIS2_PLACEMENT_3D('',#413538,#124160,#124161);
#102810=AXIS2_PLACEMENT_3D('',#413540,#124162,#124163);
#102811=AXIS2_PLACEMENT_3D('',#413542,#124164,#124165);
#102812=AXIS2_PLACEMENT_3D('',#413543,#124166,#124167);
#102813=AXIS2_PLACEMENT_3D('',#413544,#124168,#124169);
#102814=AXIS2_PLACEMENT_3D('',#413547,#124170,#124171);
#102815=AXIS2_PLACEMENT_3D('',#413549,#124172,#124173);
#102816=AXIS2_PLACEMENT_3D('',#413551,#124174,#124175);
#102817=AXIS2_PLACEMENT_3D('',#413552,#124176,#124177);
#102818=AXIS2_PLACEMENT_3D('',#413553,#124178,#124179);
#102819=AXIS2_PLACEMENT_3D('',#413556,#124180,#124181);
#102820=AXIS2_PLACEMENT_3D('',#413558,#124182,#124183);
#102821=AXIS2_PLACEMENT_3D('',#413560,#124184,#124185);
#102822=AXIS2_PLACEMENT_3D('',#413561,#124186,#124187);
#102823=AXIS2_PLACEMENT_3D('',#413562,#124188,#124189);
#102824=AXIS2_PLACEMENT_3D('',#413565,#124190,#124191);
#102825=AXIS2_PLACEMENT_3D('',#413567,#124192,#124193);
#102826=AXIS2_PLACEMENT_3D('',#413569,#124194,#124195);
#102827=AXIS2_PLACEMENT_3D('',#413570,#124196,#124197);
#102828=AXIS2_PLACEMENT_3D('',#413571,#124198,#124199);
#102829=AXIS2_PLACEMENT_3D('',#413574,#124200,#124201);
#102830=AXIS2_PLACEMENT_3D('',#413576,#124202,#124203);
#102831=AXIS2_PLACEMENT_3D('',#413578,#124204,#124205);
#102832=AXIS2_PLACEMENT_3D('',#413579,#124206,#124207);
#102833=AXIS2_PLACEMENT_3D('',#413580,#124208,#124209);
#102834=AXIS2_PLACEMENT_3D('',#413583,#124210,#124211);
#102835=AXIS2_PLACEMENT_3D('',#413585,#124212,#124213);
#102836=AXIS2_PLACEMENT_3D('',#413587,#124214,#124215);
#102837=AXIS2_PLACEMENT_3D('',#413588,#124216,#124217);
#102838=AXIS2_PLACEMENT_3D('',#413589,#124218,#124219);
#102839=AXIS2_PLACEMENT_3D('',#413592,#124220,#124221);
#102840=AXIS2_PLACEMENT_3D('',#413594,#124222,#124223);
#102841=AXIS2_PLACEMENT_3D('',#413596,#124224,#124225);
#102842=AXIS2_PLACEMENT_3D('',#413597,#124226,#124227);
#102843=AXIS2_PLACEMENT_3D('',#413598,#124228,#124229);
#102844=AXIS2_PLACEMENT_3D('',#413601,#124230,#124231);
#102845=AXIS2_PLACEMENT_3D('',#413603,#124232,#124233);
#102846=AXIS2_PLACEMENT_3D('',#413605,#124234,#124235);
#102847=AXIS2_PLACEMENT_3D('',#413606,#124236,#124237);
#102848=AXIS2_PLACEMENT_3D('',#413607,#124238,#124239);
#102849=AXIS2_PLACEMENT_3D('',#413610,#124240,#124241);
#102850=AXIS2_PLACEMENT_3D('',#413612,#124242,#124243);
#102851=AXIS2_PLACEMENT_3D('',#413614,#124244,#124245);
#102852=AXIS2_PLACEMENT_3D('',#413615,#124246,#124247);
#102853=AXIS2_PLACEMENT_3D('',#413616,#124248,#124249);
#102854=AXIS2_PLACEMENT_3D('',#413619,#124250,#124251);
#102855=AXIS2_PLACEMENT_3D('',#413621,#124252,#124253);
#102856=AXIS2_PLACEMENT_3D('',#413623,#124254,#124255);
#102857=AXIS2_PLACEMENT_3D('',#413624,#124256,#124257);
#102858=AXIS2_PLACEMENT_3D('',#413625,#124258,#124259);
#102859=AXIS2_PLACEMENT_3D('',#413628,#124260,#124261);
#102860=AXIS2_PLACEMENT_3D('',#413630,#124262,#124263);
#102861=AXIS2_PLACEMENT_3D('',#413632,#124264,#124265);
#102862=AXIS2_PLACEMENT_3D('',#413633,#124266,#124267);
#102863=AXIS2_PLACEMENT_3D('',#413634,#124268,#124269);
#102864=AXIS2_PLACEMENT_3D('',#413637,#124270,#124271);
#102865=AXIS2_PLACEMENT_3D('',#413639,#124272,#124273);
#102866=AXIS2_PLACEMENT_3D('',#413641,#124274,#124275);
#102867=AXIS2_PLACEMENT_3D('',#413642,#124276,#124277);
#102868=AXIS2_PLACEMENT_3D('',#413643,#124278,#124279);
#102869=AXIS2_PLACEMENT_3D('',#413646,#124280,#124281);
#102870=AXIS2_PLACEMENT_3D('',#413648,#124282,#124283);
#102871=AXIS2_PLACEMENT_3D('',#413650,#124284,#124285);
#102872=AXIS2_PLACEMENT_3D('',#413651,#124286,#124287);
#102873=AXIS2_PLACEMENT_3D('',#413652,#124288,#124289);
#102874=AXIS2_PLACEMENT_3D('',#413655,#124290,#124291);
#102875=AXIS2_PLACEMENT_3D('',#413657,#124292,#124293);
#102876=AXIS2_PLACEMENT_3D('',#413659,#124294,#124295);
#102877=AXIS2_PLACEMENT_3D('',#413660,#124296,#124297);
#102878=AXIS2_PLACEMENT_3D('',#413661,#124298,#124299);
#102879=AXIS2_PLACEMENT_3D('',#413664,#124300,#124301);
#102880=AXIS2_PLACEMENT_3D('',#413666,#124302,#124303);
#102881=AXIS2_PLACEMENT_3D('',#413668,#124304,#124305);
#102882=AXIS2_PLACEMENT_3D('',#413669,#124306,#124307);
#102883=AXIS2_PLACEMENT_3D('',#413670,#124308,#124309);
#102884=AXIS2_PLACEMENT_3D('',#413673,#124310,#124311);
#102885=AXIS2_PLACEMENT_3D('',#413675,#124312,#124313);
#102886=AXIS2_PLACEMENT_3D('',#413677,#124314,#124315);
#102887=AXIS2_PLACEMENT_3D('',#413678,#124316,#124317);
#102888=AXIS2_PLACEMENT_3D('',#413679,#124318,#124319);
#102889=AXIS2_PLACEMENT_3D('',#413682,#124320,#124321);
#102890=AXIS2_PLACEMENT_3D('',#413684,#124322,#124323);
#102891=AXIS2_PLACEMENT_3D('',#413686,#124324,#124325);
#102892=AXIS2_PLACEMENT_3D('',#413687,#124326,#124327);
#102893=AXIS2_PLACEMENT_3D('',#413688,#124328,#124329);
#102894=AXIS2_PLACEMENT_3D('',#413691,#124330,#124331);
#102895=AXIS2_PLACEMENT_3D('',#413693,#124332,#124333);
#102896=AXIS2_PLACEMENT_3D('',#413695,#124334,#124335);
#102897=AXIS2_PLACEMENT_3D('',#413696,#124336,#124337);
#102898=AXIS2_PLACEMENT_3D('',#413697,#124338,#124339);
#102899=AXIS2_PLACEMENT_3D('',#413700,#124340,#124341);
#102900=AXIS2_PLACEMENT_3D('',#413702,#124342,#124343);
#102901=AXIS2_PLACEMENT_3D('',#413704,#124344,#124345);
#102902=AXIS2_PLACEMENT_3D('',#413705,#124346,#124347);
#102903=AXIS2_PLACEMENT_3D('',#413706,#124348,#124349);
#102904=AXIS2_PLACEMENT_3D('',#413709,#124350,#124351);
#102905=AXIS2_PLACEMENT_3D('',#413711,#124352,#124353);
#102906=AXIS2_PLACEMENT_3D('',#413713,#124354,#124355);
#102907=AXIS2_PLACEMENT_3D('',#413714,#124356,#124357);
#102908=AXIS2_PLACEMENT_3D('',#413715,#124358,#124359);
#102909=AXIS2_PLACEMENT_3D('',#413718,#124360,#124361);
#102910=AXIS2_PLACEMENT_3D('',#413720,#124362,#124363);
#102911=AXIS2_PLACEMENT_3D('',#413722,#124364,#124365);
#102912=AXIS2_PLACEMENT_3D('',#413723,#124366,#124367);
#102913=AXIS2_PLACEMENT_3D('',#413724,#124368,#124369);
#102914=AXIS2_PLACEMENT_3D('',#413727,#124370,#124371);
#102915=AXIS2_PLACEMENT_3D('',#413729,#124372,#124373);
#102916=AXIS2_PLACEMENT_3D('',#413731,#124374,#124375);
#102917=AXIS2_PLACEMENT_3D('',#413732,#124376,#124377);
#102918=AXIS2_PLACEMENT_3D('',#413733,#124378,#124379);
#102919=AXIS2_PLACEMENT_3D('',#413736,#124380,#124381);
#102920=AXIS2_PLACEMENT_3D('',#413738,#124382,#124383);
#102921=AXIS2_PLACEMENT_3D('',#413740,#124384,#124385);
#102922=AXIS2_PLACEMENT_3D('',#413741,#124386,#124387);
#102923=AXIS2_PLACEMENT_3D('',#413742,#124388,#124389);
#102924=AXIS2_PLACEMENT_3D('',#413745,#124390,#124391);
#102925=AXIS2_PLACEMENT_3D('',#413747,#124392,#124393);
#102926=AXIS2_PLACEMENT_3D('',#413749,#124394,#124395);
#102927=AXIS2_PLACEMENT_3D('',#413750,#124396,#124397);
#102928=AXIS2_PLACEMENT_3D('',#413751,#124398,#124399);
#102929=AXIS2_PLACEMENT_3D('',#413754,#124400,#124401);
#102930=AXIS2_PLACEMENT_3D('',#413756,#124402,#124403);
#102931=AXIS2_PLACEMENT_3D('',#413758,#124404,#124405);
#102932=AXIS2_PLACEMENT_3D('',#413759,#124406,#124407);
#102933=AXIS2_PLACEMENT_3D('',#413760,#124408,#124409);
#102934=AXIS2_PLACEMENT_3D('',#413763,#124410,#124411);
#102935=AXIS2_PLACEMENT_3D('',#413765,#124412,#124413);
#102936=AXIS2_PLACEMENT_3D('',#413767,#124414,#124415);
#102937=AXIS2_PLACEMENT_3D('',#413768,#124416,#124417);
#102938=AXIS2_PLACEMENT_3D('',#413769,#124418,#124419);
#102939=AXIS2_PLACEMENT_3D('',#413772,#124420,#124421);
#102940=AXIS2_PLACEMENT_3D('',#413774,#124422,#124423);
#102941=AXIS2_PLACEMENT_3D('',#413776,#124424,#124425);
#102942=AXIS2_PLACEMENT_3D('',#413777,#124426,#124427);
#102943=AXIS2_PLACEMENT_3D('',#413778,#124428,#124429);
#102944=AXIS2_PLACEMENT_3D('',#413781,#124430,#124431);
#102945=AXIS2_PLACEMENT_3D('',#413783,#124432,#124433);
#102946=AXIS2_PLACEMENT_3D('',#413785,#124434,#124435);
#102947=AXIS2_PLACEMENT_3D('',#413786,#124436,#124437);
#102948=AXIS2_PLACEMENT_3D('',#413787,#124438,#124439);
#102949=AXIS2_PLACEMENT_3D('',#413790,#124440,#124441);
#102950=AXIS2_PLACEMENT_3D('',#413792,#124442,#124443);
#102951=AXIS2_PLACEMENT_3D('',#413794,#124444,#124445);
#102952=AXIS2_PLACEMENT_3D('',#413795,#124446,#124447);
#102953=AXIS2_PLACEMENT_3D('',#413796,#124448,#124449);
#102954=AXIS2_PLACEMENT_3D('',#413799,#124450,#124451);
#102955=AXIS2_PLACEMENT_3D('',#413801,#124452,#124453);
#102956=AXIS2_PLACEMENT_3D('',#413803,#124454,#124455);
#102957=AXIS2_PLACEMENT_3D('',#413804,#124456,#124457);
#102958=AXIS2_PLACEMENT_3D('',#413805,#124458,#124459);
#102959=AXIS2_PLACEMENT_3D('',#413808,#124460,#124461);
#102960=AXIS2_PLACEMENT_3D('',#413810,#124462,#124463);
#102961=AXIS2_PLACEMENT_3D('',#413812,#124464,#124465);
#102962=AXIS2_PLACEMENT_3D('',#413813,#124466,#124467);
#102963=AXIS2_PLACEMENT_3D('',#413814,#124468,#124469);
#102964=AXIS2_PLACEMENT_3D('',#413817,#124470,#124471);
#102965=AXIS2_PLACEMENT_3D('',#413819,#124472,#124473);
#102966=AXIS2_PLACEMENT_3D('',#413821,#124474,#124475);
#102967=AXIS2_PLACEMENT_3D('',#413822,#124476,#124477);
#102968=AXIS2_PLACEMENT_3D('',#413823,#124478,#124479);
#102969=AXIS2_PLACEMENT_3D('',#413826,#124480,#124481);
#102970=AXIS2_PLACEMENT_3D('',#413828,#124482,#124483);
#102971=AXIS2_PLACEMENT_3D('',#413830,#124484,#124485);
#102972=AXIS2_PLACEMENT_3D('',#413831,#124486,#124487);
#102973=AXIS2_PLACEMENT_3D('',#413832,#124488,#124489);
#102974=AXIS2_PLACEMENT_3D('',#413835,#124490,#124491);
#102975=AXIS2_PLACEMENT_3D('',#413837,#124492,#124493);
#102976=AXIS2_PLACEMENT_3D('',#413839,#124494,#124495);
#102977=AXIS2_PLACEMENT_3D('',#413840,#124496,#124497);
#102978=AXIS2_PLACEMENT_3D('',#413841,#124498,#124499);
#102979=AXIS2_PLACEMENT_3D('',#413844,#124500,#124501);
#102980=AXIS2_PLACEMENT_3D('',#413846,#124502,#124503);
#102981=AXIS2_PLACEMENT_3D('',#413848,#124504,#124505);
#102982=AXIS2_PLACEMENT_3D('',#413849,#124506,#124507);
#102983=AXIS2_PLACEMENT_3D('',#413850,#124508,#124509);
#102984=AXIS2_PLACEMENT_3D('',#413853,#124510,#124511);
#102985=AXIS2_PLACEMENT_3D('',#413855,#124512,#124513);
#102986=AXIS2_PLACEMENT_3D('',#413857,#124514,#124515);
#102987=AXIS2_PLACEMENT_3D('',#413858,#124516,#124517);
#102988=AXIS2_PLACEMENT_3D('',#413859,#124518,#124519);
#102989=AXIS2_PLACEMENT_3D('',#413862,#124520,#124521);
#102990=AXIS2_PLACEMENT_3D('',#413864,#124522,#124523);
#102991=AXIS2_PLACEMENT_3D('',#413866,#124524,#124525);
#102992=AXIS2_PLACEMENT_3D('',#413867,#124526,#124527);
#102993=AXIS2_PLACEMENT_3D('',#413868,#124528,#124529);
#102994=AXIS2_PLACEMENT_3D('',#413871,#124530,#124531);
#102995=AXIS2_PLACEMENT_3D('',#413873,#124532,#124533);
#102996=AXIS2_PLACEMENT_3D('',#413875,#124534,#124535);
#102997=AXIS2_PLACEMENT_3D('',#413876,#124536,#124537);
#102998=AXIS2_PLACEMENT_3D('',#413877,#124538,#124539);
#102999=AXIS2_PLACEMENT_3D('',#413880,#124540,#124541);
#103000=AXIS2_PLACEMENT_3D('',#413882,#124542,#124543);
#103001=AXIS2_PLACEMENT_3D('',#413884,#124544,#124545);
#103002=AXIS2_PLACEMENT_3D('',#413885,#124546,#124547);
#103003=AXIS2_PLACEMENT_3D('',#413886,#124548,#124549);
#103004=AXIS2_PLACEMENT_3D('',#413889,#124550,#124551);
#103005=AXIS2_PLACEMENT_3D('',#413891,#124552,#124553);
#103006=AXIS2_PLACEMENT_3D('',#413893,#124554,#124555);
#103007=AXIS2_PLACEMENT_3D('',#413894,#124556,#124557);
#103008=AXIS2_PLACEMENT_3D('',#413895,#124558,#124559);
#103009=AXIS2_PLACEMENT_3D('',#413898,#124560,#124561);
#103010=AXIS2_PLACEMENT_3D('',#413900,#124562,#124563);
#103011=AXIS2_PLACEMENT_3D('',#413902,#124564,#124565);
#103012=AXIS2_PLACEMENT_3D('',#413903,#124566,#124567);
#103013=AXIS2_PLACEMENT_3D('',#413904,#124568,#124569);
#103014=AXIS2_PLACEMENT_3D('',#413907,#124570,#124571);
#103015=AXIS2_PLACEMENT_3D('',#413909,#124572,#124573);
#103016=AXIS2_PLACEMENT_3D('',#413911,#124574,#124575);
#103017=AXIS2_PLACEMENT_3D('',#413912,#124576,#124577);
#103018=AXIS2_PLACEMENT_3D('',#413913,#124578,#124579);
#103019=AXIS2_PLACEMENT_3D('',#413916,#124580,#124581);
#103020=AXIS2_PLACEMENT_3D('',#413918,#124582,#124583);
#103021=AXIS2_PLACEMENT_3D('',#413920,#124584,#124585);
#103022=AXIS2_PLACEMENT_3D('',#413921,#124586,#124587);
#103023=AXIS2_PLACEMENT_3D('',#413922,#124588,#124589);
#103024=AXIS2_PLACEMENT_3D('',#413925,#124590,#124591);
#103025=AXIS2_PLACEMENT_3D('',#413927,#124592,#124593);
#103026=AXIS2_PLACEMENT_3D('',#413929,#124594,#124595);
#103027=AXIS2_PLACEMENT_3D('',#413930,#124596,#124597);
#103028=AXIS2_PLACEMENT_3D('',#413931,#124598,#124599);
#103029=AXIS2_PLACEMENT_3D('',#413934,#124600,#124601);
#103030=AXIS2_PLACEMENT_3D('',#413936,#124602,#124603);
#103031=AXIS2_PLACEMENT_3D('',#413938,#124604,#124605);
#103032=AXIS2_PLACEMENT_3D('',#413939,#124606,#124607);
#103033=AXIS2_PLACEMENT_3D('',#413940,#124608,#124609);
#103034=AXIS2_PLACEMENT_3D('',#413943,#124610,#124611);
#103035=AXIS2_PLACEMENT_3D('',#413945,#124612,#124613);
#103036=AXIS2_PLACEMENT_3D('',#413947,#124614,#124615);
#103037=AXIS2_PLACEMENT_3D('',#413948,#124616,#124617);
#103038=AXIS2_PLACEMENT_3D('',#413949,#124618,#124619);
#103039=AXIS2_PLACEMENT_3D('',#413952,#124620,#124621);
#103040=AXIS2_PLACEMENT_3D('',#413954,#124622,#124623);
#103041=AXIS2_PLACEMENT_3D('',#413956,#124624,#124625);
#103042=AXIS2_PLACEMENT_3D('',#413957,#124626,#124627);
#103043=AXIS2_PLACEMENT_3D('',#413958,#124628,#124629);
#103044=AXIS2_PLACEMENT_3D('',#413961,#124630,#124631);
#103045=AXIS2_PLACEMENT_3D('',#413963,#124632,#124633);
#103046=AXIS2_PLACEMENT_3D('',#413965,#124634,#124635);
#103047=AXIS2_PLACEMENT_3D('',#413966,#124636,#124637);
#103048=AXIS2_PLACEMENT_3D('',#413967,#124638,#124639);
#103049=AXIS2_PLACEMENT_3D('',#413970,#124640,#124641);
#103050=AXIS2_PLACEMENT_3D('',#413972,#124642,#124643);
#103051=AXIS2_PLACEMENT_3D('',#413974,#124644,#124645);
#103052=AXIS2_PLACEMENT_3D('',#413975,#124646,#124647);
#103053=AXIS2_PLACEMENT_3D('',#413976,#124648,#124649);
#103054=AXIS2_PLACEMENT_3D('',#413979,#124650,#124651);
#103055=AXIS2_PLACEMENT_3D('',#413981,#124652,#124653);
#103056=AXIS2_PLACEMENT_3D('',#413983,#124654,#124655);
#103057=AXIS2_PLACEMENT_3D('',#413984,#124656,#124657);
#103058=AXIS2_PLACEMENT_3D('',#413985,#124658,#124659);
#103059=AXIS2_PLACEMENT_3D('',#413988,#124660,#124661);
#103060=AXIS2_PLACEMENT_3D('',#413990,#124662,#124663);
#103061=AXIS2_PLACEMENT_3D('',#413992,#124664,#124665);
#103062=AXIS2_PLACEMENT_3D('',#413993,#124666,#124667);
#103063=AXIS2_PLACEMENT_3D('',#413994,#124668,#124669);
#103064=AXIS2_PLACEMENT_3D('',#413997,#124670,#124671);
#103065=AXIS2_PLACEMENT_3D('',#413999,#124672,#124673);
#103066=AXIS2_PLACEMENT_3D('',#414001,#124674,#124675);
#103067=AXIS2_PLACEMENT_3D('',#414002,#124676,#124677);
#103068=AXIS2_PLACEMENT_3D('',#414003,#124678,#124679);
#103069=AXIS2_PLACEMENT_3D('',#414006,#124680,#124681);
#103070=AXIS2_PLACEMENT_3D('',#414008,#124682,#124683);
#103071=AXIS2_PLACEMENT_3D('',#414010,#124684,#124685);
#103072=AXIS2_PLACEMENT_3D('',#414011,#124686,#124687);
#103073=AXIS2_PLACEMENT_3D('',#414012,#124688,#124689);
#103074=AXIS2_PLACEMENT_3D('',#414015,#124690,#124691);
#103075=AXIS2_PLACEMENT_3D('',#414017,#124692,#124693);
#103076=AXIS2_PLACEMENT_3D('',#414019,#124694,#124695);
#103077=AXIS2_PLACEMENT_3D('',#414020,#124696,#124697);
#103078=AXIS2_PLACEMENT_3D('',#414021,#124698,#124699);
#103079=AXIS2_PLACEMENT_3D('',#414024,#124700,#124701);
#103080=AXIS2_PLACEMENT_3D('',#414026,#124702,#124703);
#103081=AXIS2_PLACEMENT_3D('',#414028,#124704,#124705);
#103082=AXIS2_PLACEMENT_3D('',#414029,#124706,#124707);
#103083=AXIS2_PLACEMENT_3D('',#414030,#124708,#124709);
#103084=AXIS2_PLACEMENT_3D('',#414033,#124710,#124711);
#103085=AXIS2_PLACEMENT_3D('',#414035,#124712,#124713);
#103086=AXIS2_PLACEMENT_3D('',#414037,#124714,#124715);
#103087=AXIS2_PLACEMENT_3D('',#414038,#124716,#124717);
#103088=AXIS2_PLACEMENT_3D('',#414039,#124718,#124719);
#103089=AXIS2_PLACEMENT_3D('',#414042,#124720,#124721);
#103090=AXIS2_PLACEMENT_3D('',#414044,#124722,#124723);
#103091=AXIS2_PLACEMENT_3D('',#414046,#124724,#124725);
#103092=AXIS2_PLACEMENT_3D('',#414047,#124726,#124727);
#103093=AXIS2_PLACEMENT_3D('',#414048,#124728,#124729);
#103094=AXIS2_PLACEMENT_3D('',#414051,#124730,#124731);
#103095=AXIS2_PLACEMENT_3D('',#414053,#124732,#124733);
#103096=AXIS2_PLACEMENT_3D('',#414055,#124734,#124735);
#103097=AXIS2_PLACEMENT_3D('',#414056,#124736,#124737);
#103098=AXIS2_PLACEMENT_3D('',#414057,#124738,#124739);
#103099=AXIS2_PLACEMENT_3D('',#414060,#124740,#124741);
#103100=AXIS2_PLACEMENT_3D('',#414062,#124742,#124743);
#103101=AXIS2_PLACEMENT_3D('',#414064,#124744,#124745);
#103102=AXIS2_PLACEMENT_3D('',#414065,#124746,#124747);
#103103=AXIS2_PLACEMENT_3D('',#414066,#124748,#124749);
#103104=AXIS2_PLACEMENT_3D('',#414069,#124750,#124751);
#103105=AXIS2_PLACEMENT_3D('',#414071,#124752,#124753);
#103106=AXIS2_PLACEMENT_3D('',#414073,#124754,#124755);
#103107=AXIS2_PLACEMENT_3D('',#414074,#124756,#124757);
#103108=AXIS2_PLACEMENT_3D('',#414075,#124758,#124759);
#103109=AXIS2_PLACEMENT_3D('',#414078,#124760,#124761);
#103110=AXIS2_PLACEMENT_3D('',#414080,#124762,#124763);
#103111=AXIS2_PLACEMENT_3D('',#414082,#124764,#124765);
#103112=AXIS2_PLACEMENT_3D('',#414084,#124766,#124767);
#103113=AXIS2_PLACEMENT_3D('',#414085,#124768,#124769);
#103114=AXIS2_PLACEMENT_3D('',#414086,#124770,#124771);
#103115=AXIS2_PLACEMENT_3D('',#414161,#124772,#124773);
#103116=AXIS2_PLACEMENT_3D('',#414162,#124774,#124775);
#103117=AXIS2_PLACEMENT_3D('',#414195,#124776,#124777);
#103118=AXIS2_PLACEMENT_3D('',#414197,#124778,#124779);
#103119=AXIS2_PLACEMENT_3D('',#414199,#124781,#124782);
#103120=AXIS2_PLACEMENT_3D('',#414232,#124783,#124784);
#103121=AXIS2_PLACEMENT_3D('',#414237,#124786,#124787);
#103122=AXIS2_PLACEMENT_3D('',#414239,#124788,#124789);
#103123=AXIS2_PLACEMENT_3D('',#414241,#124790,#124791);
#103124=AXIS2_PLACEMENT_3D('',#414243,#124792,#124793);
#103125=AXIS2_PLACEMENT_3D('',#414245,#124794,#124795);
#103126=AXIS2_PLACEMENT_3D('',#414246,#124796,#124797);
#103127=AXIS2_PLACEMENT_3D('',#414247,#124798,#124799);
#103128=AXIS2_PLACEMENT_3D('',#414253,#124800,#124801);
#103129=AXIS2_PLACEMENT_3D('',#414254,#124802,#124803);
#103130=AXIS2_PLACEMENT_3D('',#414256,#124804,#124805);
#103131=AXIS2_PLACEMENT_3D('',#414258,#124806,#124807);
#103132=AXIS2_PLACEMENT_3D('',#414259,#124808,#124809);
#103133=AXIS2_PLACEMENT_3D('',#414260,#124810,#124811);
#103134=AXIS2_PLACEMENT_3D('',#414262,#124812,#124813);
#103135=AXIS2_PLACEMENT_3D('',#414264,#124815,#124816);
#103136=AXIS2_PLACEMENT_3D('',#414266,#124817,#124818);
#103137=AXIS2_PLACEMENT_3D('',#414267,#124819,#124820);
#103138=AXIS2_PLACEMENT_3D('',#414268,#124821,#124822);
#103139=AXIS2_PLACEMENT_3D('',#414290,#124824,#124825);
#103140=AXIS2_PLACEMENT_3D('',#414322,#124828,#124829);
#103141=AXIS2_PLACEMENT_3D('',#414354,#124832,#124833);
#103142=AXIS2_PLACEMENT_3D('',#414386,#124836,#124837);
#103143=AXIS2_PLACEMENT_3D('',#414418,#124840,#124841);
#103144=AXIS2_PLACEMENT_3D('',#414450,#124844,#124845);
#103145=AXIS2_PLACEMENT_3D('',#414482,#124848,#124849);
#103146=AXIS2_PLACEMENT_3D('',#414514,#124852,#124853);
#103147=AXIS2_PLACEMENT_3D('',#414546,#124856,#124857);
#103148=AXIS2_PLACEMENT_3D('',#414578,#124860,#124861);
#103149=AXIS2_PLACEMENT_3D('',#414610,#124864,#124865);
#103150=AXIS2_PLACEMENT_3D('',#414642,#124868,#124869);
#103151=AXIS2_PLACEMENT_3D('',#414674,#124872,#124873);
#103152=AXIS2_PLACEMENT_3D('',#414706,#124876,#124877);
#103153=AXIS2_PLACEMENT_3D('',#414738,#124880,#124881);
#103154=AXIS2_PLACEMENT_3D('',#414770,#124884,#124885);
#103155=AXIS2_PLACEMENT_3D('',#414802,#124888,#124889);
#103156=AXIS2_PLACEMENT_3D('',#414834,#124892,#124893);
#103157=AXIS2_PLACEMENT_3D('',#414866,#124896,#124897);
#103158=AXIS2_PLACEMENT_3D('',#414898,#124900,#124901);
#103159=AXIS2_PLACEMENT_3D('',#414930,#124904,#124905);
#103160=AXIS2_PLACEMENT_3D('',#414962,#124908,#124909);
#103161=AXIS2_PLACEMENT_3D('',#414994,#124912,#124913);
#103162=AXIS2_PLACEMENT_3D('',#415026,#124916,#124917);
#103163=AXIS2_PLACEMENT_3D('',#415058,#124920,#124921);
#103164=AXIS2_PLACEMENT_3D('',#415090,#124924,#124925);
#103165=AXIS2_PLACEMENT_3D('',#415122,#124928,#124929);
#103166=AXIS2_PLACEMENT_3D('',#415154,#124932,#124933);
#103167=AXIS2_PLACEMENT_3D('',#415186,#124936,#124937);
#103168=AXIS2_PLACEMENT_3D('',#415218,#124940,#124941);
#103169=AXIS2_PLACEMENT_3D('',#415250,#124944,#124945);
#103170=AXIS2_PLACEMENT_3D('',#415282,#124948,#124949);
#103171=AXIS2_PLACEMENT_3D('',#415314,#124952,#124953);
#103172=AXIS2_PLACEMENT_3D('',#415346,#124956,#124957);
#103173=AXIS2_PLACEMENT_3D('',#415378,#124960,#124961);
#103174=AXIS2_PLACEMENT_3D('',#415410,#124964,#124965);
#103175=AXIS2_PLACEMENT_3D('',#415442,#124968,#124969);
#103176=AXIS2_PLACEMENT_3D('',#415474,#124972,#124973);
#103177=AXIS2_PLACEMENT_3D('',#415506,#124976,#124977);
#103178=AXIS2_PLACEMENT_3D('',#415510,#124979,#124980);
#103179=AXIS2_PLACEMENT_3D('',#415511,#124981,#124982);
#103180=AXIS2_PLACEMENT_3D('',#415513,#124983,#124984);
#103181=AXIS2_PLACEMENT_3D('',#415545,#124987,#124988);
#103182=AXIS2_PLACEMENT_3D('',#415577,#124991,#124992);
#103183=AXIS2_PLACEMENT_3D('',#415609,#124995,#124996);
#103184=AXIS2_PLACEMENT_3D('',#415641,#124999,#125000);
#103185=AXIS2_PLACEMENT_3D('',#415673,#125003,#125004);
#103186=AXIS2_PLACEMENT_3D('',#415705,#125007,#125008);
#103187=AXIS2_PLACEMENT_3D('',#415737,#125011,#125012);
#103188=AXIS2_PLACEMENT_3D('',#415769,#125015,#125016);
#103189=AXIS2_PLACEMENT_3D('',#415801,#125019,#125020);
#103190=AXIS2_PLACEMENT_3D('',#415833,#125023,#125024);
#103191=AXIS2_PLACEMENT_3D('',#415865,#125027,#125028);
#103192=AXIS2_PLACEMENT_3D('',#415897,#125031,#125032);
#103193=AXIS2_PLACEMENT_3D('',#415929,#125035,#125036);
#103194=AXIS2_PLACEMENT_3D('',#415961,#125039,#125040);
#103195=AXIS2_PLACEMENT_3D('',#415993,#125043,#125044);
#103196=AXIS2_PLACEMENT_3D('',#416025,#125047,#125048);
#103197=AXIS2_PLACEMENT_3D('',#416057,#125051,#125052);
#103198=AXIS2_PLACEMENT_3D('',#416089,#125055,#125056);
#103199=AXIS2_PLACEMENT_3D('',#416121,#125059,#125060);
#103200=AXIS2_PLACEMENT_3D('',#416153,#125063,#125064);
#103201=AXIS2_PLACEMENT_3D('',#416185,#125067,#125068);
#103202=AXIS2_PLACEMENT_3D('',#416217,#125071,#125072);
#103203=AXIS2_PLACEMENT_3D('',#416249,#125075,#125076);
#103204=AXIS2_PLACEMENT_3D('',#416281,#125079,#125080);
#103205=AXIS2_PLACEMENT_3D('',#416313,#125083,#125084);
#103206=AXIS2_PLACEMENT_3D('',#416345,#125087,#125088);
#103207=AXIS2_PLACEMENT_3D('',#416377,#125091,#125092);
#103208=AXIS2_PLACEMENT_3D('',#416409,#125095,#125096);
#103209=AXIS2_PLACEMENT_3D('',#416441,#125099,#125100);
#103210=AXIS2_PLACEMENT_3D('',#416473,#125103,#125104);
#103211=AXIS2_PLACEMENT_3D('',#416505,#125107,#125108);
#103212=AXIS2_PLACEMENT_3D('',#416537,#125111,#125112);
#103213=AXIS2_PLACEMENT_3D('',#416569,#125115,#125116);
#103214=AXIS2_PLACEMENT_3D('',#416601,#125119,#125120);
#103215=AXIS2_PLACEMENT_3D('',#416633,#125123,#125124);
#103216=AXIS2_PLACEMENT_3D('',#416665,#125127,#125128);
#103217=AXIS2_PLACEMENT_3D('',#416697,#125131,#125132);
#103218=AXIS2_PLACEMENT_3D('',#416729,#125135,#125136);
#103219=AXIS2_PLACEMENT_3D('',#416745,#125138,#125139);
#103220=AXIS2_PLACEMENT_3D('',#416747,#125140,#125141);
#103221=AXIS2_PLACEMENT_3D('',#416748,#125142,#125143);
#103222=AXIS2_PLACEMENT_3D('',#416749,#125144,#125145);
#103223=AXIS2_PLACEMENT_3D('',#416752,#125146,#125147);
#103224=AXIS2_PLACEMENT_3D('',#416791,#125150,#125151);
#103225=AXIS2_PLACEMENT_3D('',#416830,#125154,#125155);
#103226=AXIS2_PLACEMENT_3D('',#416869,#125158,#125159);
#103227=AXIS2_PLACEMENT_3D('',#416908,#125162,#125163);
#103228=AXIS2_PLACEMENT_3D('',#416947,#125166,#125167);
#103229=AXIS2_PLACEMENT_3D('',#416986,#125170,#125171);
#103230=AXIS2_PLACEMENT_3D('',#417025,#125174,#125175);
#103231=AXIS2_PLACEMENT_3D('',#417064,#125178,#125179);
#103232=AXIS2_PLACEMENT_3D('',#417103,#125182,#125183);
#103233=AXIS2_PLACEMENT_3D('',#417142,#125186,#125187);
#103234=AXIS2_PLACEMENT_3D('',#417181,#125190,#125191);
#103235=AXIS2_PLACEMENT_3D('',#417220,#125194,#125195);
#103236=AXIS2_PLACEMENT_3D('',#417259,#125198,#125199);
#103237=AXIS2_PLACEMENT_3D('',#417298,#125202,#125203);
#103238=AXIS2_PLACEMENT_3D('',#417337,#125206,#125207);
#103239=AXIS2_PLACEMENT_3D('',#417376,#125210,#125211);
#103240=AXIS2_PLACEMENT_3D('',#417415,#125214,#125215);
#103241=AXIS2_PLACEMENT_3D('',#417454,#125218,#125219);
#103242=AXIS2_PLACEMENT_3D('',#417493,#125222,#125223);
#103243=AXIS2_PLACEMENT_3D('',#417532,#125226,#125227);
#103244=AXIS2_PLACEMENT_3D('',#417571,#125230,#125231);
#103245=AXIS2_PLACEMENT_3D('',#417610,#125234,#125235);
#103246=AXIS2_PLACEMENT_3D('',#417649,#125238,#125239);
#103247=AXIS2_PLACEMENT_3D('',#417688,#125242,#125243);
#103248=AXIS2_PLACEMENT_3D('',#417727,#125246,#125247);
#103249=AXIS2_PLACEMENT_3D('',#417766,#125250,#125251);
#103250=AXIS2_PLACEMENT_3D('',#417805,#125254,#125255);
#103251=AXIS2_PLACEMENT_3D('',#417844,#125258,#125259);
#103252=AXIS2_PLACEMENT_3D('',#417883,#125262,#125263);
#103253=AXIS2_PLACEMENT_3D('',#417922,#125266,#125267);
#103254=AXIS2_PLACEMENT_3D('',#417961,#125270,#125271);
#103255=AXIS2_PLACEMENT_3D('',#418000,#125274,#125275);
#103256=AXIS2_PLACEMENT_3D('',#418039,#125278,#125279);
#103257=AXIS2_PLACEMENT_3D('',#418078,#125282,#125283);
#103258=AXIS2_PLACEMENT_3D('',#418117,#125286,#125287);
#103259=AXIS2_PLACEMENT_3D('',#418156,#125290,#125291);
#103260=AXIS2_PLACEMENT_3D('',#418195,#125294,#125295);
#103261=AXIS2_PLACEMENT_3D('',#418234,#125298,#125299);
#103262=AXIS2_PLACEMENT_3D('',#418274,#125303,#125304);
#103263=AXIS2_PLACEMENT_3D('',#418313,#125307,#125308);
#103264=AXIS2_PLACEMENT_3D('',#418352,#125311,#125312);
#103265=AXIS2_PLACEMENT_3D('',#418391,#125315,#125316);
#103266=AXIS2_PLACEMENT_3D('',#418430,#125319,#125320);
#103267=AXIS2_PLACEMENT_3D('',#418469,#125323,#125324);
#103268=AXIS2_PLACEMENT_3D('',#418508,#125327,#125328);
#103269=AXIS2_PLACEMENT_3D('',#418547,#125331,#125332);
#103270=AXIS2_PLACEMENT_3D('',#418586,#125335,#125336);
#103271=AXIS2_PLACEMENT_3D('',#418625,#125339,#125340);
#103272=AXIS2_PLACEMENT_3D('',#418664,#125343,#125344);
#103273=AXIS2_PLACEMENT_3D('',#418703,#125347,#125348);
#103274=AXIS2_PLACEMENT_3D('',#418742,#125351,#125352);
#103275=AXIS2_PLACEMENT_3D('',#418781,#125355,#125356);
#103276=AXIS2_PLACEMENT_3D('',#418820,#125359,#125360);
#103277=AXIS2_PLACEMENT_3D('',#418859,#125363,#125364);
#103278=AXIS2_PLACEMENT_3D('',#418898,#125367,#125368);
#103279=AXIS2_PLACEMENT_3D('',#418937,#125371,#125372);
#103280=AXIS2_PLACEMENT_3D('',#418976,#125375,#125376);
#103281=AXIS2_PLACEMENT_3D('',#419015,#125379,#125380);
#103282=AXIS2_PLACEMENT_3D('',#419054,#125383,#125384);
#103283=AXIS2_PLACEMENT_3D('',#419093,#125387,#125388);
#103284=AXIS2_PLACEMENT_3D('',#419132,#125391,#125392);
#103285=AXIS2_PLACEMENT_3D('',#419171,#125395,#125396);
#103286=AXIS2_PLACEMENT_3D('',#419210,#125399,#125400);
#103287=AXIS2_PLACEMENT_3D('',#419249,#125403,#125404);
#103288=AXIS2_PLACEMENT_3D('',#419288,#125407,#125408);
#103289=AXIS2_PLACEMENT_3D('',#419327,#125411,#125412);
#103290=AXIS2_PLACEMENT_3D('',#419366,#125415,#125416);
#103291=AXIS2_PLACEMENT_3D('',#419405,#125419,#125420);
#103292=AXIS2_PLACEMENT_3D('',#419444,#125423,#125424);
#103293=AXIS2_PLACEMENT_3D('',#419483,#125427,#125428);
#103294=AXIS2_PLACEMENT_3D('',#419522,#125431,#125432);
#103295=AXIS2_PLACEMENT_3D('',#419561,#125435,#125436);
#103296=AXIS2_PLACEMENT_3D('',#419600,#125439,#125440);
#103297=AXIS2_PLACEMENT_3D('',#419639,#125443,#125444);
#103298=AXIS2_PLACEMENT_3D('',#419678,#125447,#125448);
#103299=AXIS2_PLACEMENT_3D('',#419717,#125451,#125452);
#103300=AXIS2_PLACEMENT_3D('',#419754,#125455,#125456);
#103301=AXIS2_PLACEMENT_3D('',#419755,#125457,#125458);
#103302=AXIS2_PLACEMENT_3D('',#419756,#125459,#125460);
#103303=AXIS2_PLACEMENT_3D('',#419757,#125461,#125462);
#103304=AXIS2_PLACEMENT_3D('',#419758,#125463,#125464);
#103305=AXIS2_PLACEMENT_3D('',#419759,#125465,#125466);
#103306=AXIS2_PLACEMENT_3D('',#419760,#125467,#125468);
#103307=AXIS2_PLACEMENT_3D('',#419761,#125469,#125470);
#103308=AXIS2_PLACEMENT_3D('',#419762,#125471,#125472);
#103309=AXIS2_PLACEMENT_3D('',#419763,#125473,#125474);
#103310=AXIS2_PLACEMENT_3D('',#419764,#125475,#125476);
#103311=AXIS2_PLACEMENT_3D('',#419765,#125477,#125478);
#103312=AXIS2_PLACEMENT_3D('',#419766,#125479,#125480);
#103313=AXIS2_PLACEMENT_3D('',#419767,#125481,#125482);
#103314=AXIS2_PLACEMENT_3D('',#419768,#125483,#125484);
#103315=AXIS2_PLACEMENT_3D('',#419769,#125485,#125486);
#103316=AXIS2_PLACEMENT_3D('',#419770,#125487,#125488);
#103317=AXIS2_PLACEMENT_3D('',#419771,#125489,#125490);
#103318=AXIS2_PLACEMENT_3D('',#419772,#125491,#125492);
#103319=AXIS2_PLACEMENT_3D('',#419773,#125493,#125494);
#103320=AXIS2_PLACEMENT_3D('',#419774,#125495,#125496);
#103321=AXIS2_PLACEMENT_3D('',#419775,#125497,#125498);
#103322=AXIS2_PLACEMENT_3D('',#419776,#125499,#125500);
#103323=AXIS2_PLACEMENT_3D('',#419777,#125501,#125502);
#103324=AXIS2_PLACEMENT_3D('',#419778,#125503,#125504);
#103325=AXIS2_PLACEMENT_3D('',#419779,#125505,#125506);
#103326=AXIS2_PLACEMENT_3D('',#419780,#125507,#125508);
#103327=AXIS2_PLACEMENT_3D('',#419781,#125509,#125510);
#103328=AXIS2_PLACEMENT_3D('',#419782,#125511,#125512);
#103329=AXIS2_PLACEMENT_3D('',#419783,#125513,#125514);
#103330=AXIS2_PLACEMENT_3D('',#419784,#125515,#125516);
#103331=AXIS2_PLACEMENT_3D('',#419785,#125517,#125518);
#103332=AXIS2_PLACEMENT_3D('',#419786,#125519,#125520);
#103333=AXIS2_PLACEMENT_3D('',#419787,#125521,#125522);
#103334=AXIS2_PLACEMENT_3D('',#419788,#125523,#125524);
#103335=AXIS2_PLACEMENT_3D('',#419789,#125525,#125526);
#103336=AXIS2_PLACEMENT_3D('',#419790,#125527,#125528);
#103337=AXIS2_PLACEMENT_3D('',#419791,#125529,#125530);
#103338=AXIS2_PLACEMENT_3D('',#419792,#125531,#125532);
#103339=AXIS2_PLACEMENT_3D('',#419793,#125533,#125534);
#103340=AXIS2_PLACEMENT_3D('',#419794,#125535,#125536);
#103341=AXIS2_PLACEMENT_3D('',#419795,#125537,#125538);
#103342=AXIS2_PLACEMENT_3D('',#419796,#125539,#125540);
#103343=AXIS2_PLACEMENT_3D('',#419797,#125541,#125542);
#103344=AXIS2_PLACEMENT_3D('',#419798,#125543,#125544);
#103345=AXIS2_PLACEMENT_3D('',#419799,#125545,#125546);
#103346=AXIS2_PLACEMENT_3D('',#419800,#125547,#125548);
#103347=AXIS2_PLACEMENT_3D('',#419801,#125549,#125550);
#103348=AXIS2_PLACEMENT_3D('',#419802,#125551,#125552);
#103349=AXIS2_PLACEMENT_3D('',#419803,#125553,#125554);
#103350=AXIS2_PLACEMENT_3D('',#419804,#125555,#125556);
#103351=AXIS2_PLACEMENT_3D('',#419805,#125557,#125558);
#103352=AXIS2_PLACEMENT_3D('',#419806,#125559,#125560);
#103353=AXIS2_PLACEMENT_3D('',#419807,#125561,#125562);
#103354=AXIS2_PLACEMENT_3D('',#419808,#125563,#125564);
#103355=AXIS2_PLACEMENT_3D('',#419809,#125565,#125566);
#103356=AXIS2_PLACEMENT_3D('',#419810,#125567,#125568);
#103357=AXIS2_PLACEMENT_3D('',#419811,#125569,#125570);
#103358=AXIS2_PLACEMENT_3D('',#419812,#125571,#125572);
#103359=AXIS2_PLACEMENT_3D('',#419813,#125573,#125574);
#103360=AXIS2_PLACEMENT_3D('',#419814,#125575,#125576);
#103361=AXIS2_PLACEMENT_3D('',#419815,#125577,#125578);
#103362=AXIS2_PLACEMENT_3D('',#419816,#125579,#125580);
#103363=AXIS2_PLACEMENT_3D('',#419817,#125581,#125582);
#103364=AXIS2_PLACEMENT_3D('',#419818,#125583,#125584);
#103365=AXIS2_PLACEMENT_3D('',#419819,#125585,#125586);
#103366=AXIS2_PLACEMENT_3D('',#419820,#125587,#125588);
#103367=AXIS2_PLACEMENT_3D('',#419821,#125589,#125590);
#103368=AXIS2_PLACEMENT_3D('',#419822,#125591,#125592);
#103369=AXIS2_PLACEMENT_3D('',#419823,#125593,#125594);
#103370=AXIS2_PLACEMENT_3D('',#419824,#125595,#125596);
#103371=AXIS2_PLACEMENT_3D('',#419825,#125597,#125598);
#103372=AXIS2_PLACEMENT_3D('',#419826,#125599,#125600);
#103373=AXIS2_PLACEMENT_3D('',#419827,#125601,#125602);
#103374=AXIS2_PLACEMENT_3D('',#419828,#125603,#125604);
#103375=AXIS2_PLACEMENT_3D('',#419829,#125605,#125606);
#103376=AXIS2_PLACEMENT_3D('',#419830,#125607,#125608);
#103377=AXIS2_PLACEMENT_3D('',#419831,#125609,#125610);
#103378=AXIS2_PLACEMENT_3D('',#419832,#125611,#125612);
#103379=AXIS2_PLACEMENT_3D('',#419833,#125613,#125614);
#103380=AXIS2_PLACEMENT_3D('',#419834,#125615,#125616);
#103381=AXIS2_PLACEMENT_3D('',#419835,#125617,#125618);
#103382=AXIS2_PLACEMENT_3D('',#419836,#125619,#125620);
#103383=AXIS2_PLACEMENT_3D('',#419837,#125621,#125622);
#103384=AXIS2_PLACEMENT_3D('',#419838,#125623,#125624);
#103385=AXIS2_PLACEMENT_3D('',#419839,#125625,#125626);
#103386=AXIS2_PLACEMENT_3D('',#419840,#125627,#125628);
#103387=AXIS2_PLACEMENT_3D('',#419841,#125629,#125630);
#103388=AXIS2_PLACEMENT_3D('',#419842,#125631,#125632);
#103389=AXIS2_PLACEMENT_3D('',#419843,#125633,#125634);
#103390=AXIS2_PLACEMENT_3D('',#419844,#125635,#125636);
#103391=AXIS2_PLACEMENT_3D('',#419845,#125637,#125638);
#103392=AXIS2_PLACEMENT_3D('',#419846,#125639,#125640);
#103393=AXIS2_PLACEMENT_3D('',#419847,#125641,#125642);
#103394=AXIS2_PLACEMENT_3D('',#419848,#125643,#125644);
#103395=AXIS2_PLACEMENT_3D('',#419849,#125645,#125646);
#103396=AXIS2_PLACEMENT_3D('',#419850,#125647,#125648);
#103397=AXIS2_PLACEMENT_3D('',#419851,#125649,#125650);
#103398=AXIS2_PLACEMENT_3D('',#419852,#125651,#125652);
#103399=AXIS2_PLACEMENT_3D('',#419853,#125653,#125654);
#103400=AXIS2_PLACEMENT_3D('',#419854,#125655,#125656);
#103401=AXIS2_PLACEMENT_3D('',#419855,#125657,#125658);
#103402=AXIS2_PLACEMENT_3D('',#419856,#125659,#125660);
#103403=AXIS2_PLACEMENT_3D('',#419857,#125661,#125662);
#103404=AXIS2_PLACEMENT_3D('',#419858,#125663,#125664);
#103405=AXIS2_PLACEMENT_3D('',#419859,#125665,#125666);
#103406=AXIS2_PLACEMENT_3D('',#419860,#125667,#125668);
#103407=AXIS2_PLACEMENT_3D('',#419861,#125669,#125670);
#103408=AXIS2_PLACEMENT_3D('',#419862,#125671,#125672);
#103409=AXIS2_PLACEMENT_3D('',#419863,#125673,#125674);
#103410=AXIS2_PLACEMENT_3D('',#419864,#125675,#125676);
#103411=AXIS2_PLACEMENT_3D('',#419865,#125677,#125678);
#103412=AXIS2_PLACEMENT_3D('',#419866,#125679,#125680);
#103413=AXIS2_PLACEMENT_3D('',#419867,#125681,#125682);
#103414=AXIS2_PLACEMENT_3D('',#419868,#125683,#125684);
#103415=AXIS2_PLACEMENT_3D('',#419869,#125685,#125686);
#103416=AXIS2_PLACEMENT_3D('',#419870,#125687,#125688);
#103417=AXIS2_PLACEMENT_3D('',#419871,#125689,#125690);
#103418=AXIS2_PLACEMENT_3D('',#419872,#125691,#125692);
#103419=AXIS2_PLACEMENT_3D('',#419873,#125693,#125694);
#103420=AXIS2_PLACEMENT_3D('',#419874,#125695,#125696);
#103421=AXIS2_PLACEMENT_3D('',#419875,#125697,#125698);
#103422=AXIS2_PLACEMENT_3D('',#419876,#125699,#125700);
#103423=AXIS2_PLACEMENT_3D('',#419877,#125701,#125702);
#103424=AXIS2_PLACEMENT_3D('',#419878,#125703,#125704);
#103425=AXIS2_PLACEMENT_3D('',#419879,#125705,#125706);
#103426=AXIS2_PLACEMENT_3D('',#419880,#125707,#125708);
#103427=AXIS2_PLACEMENT_3D('',#419881,#125709,#125710);
#103428=AXIS2_PLACEMENT_3D('',#419882,#125711,#125712);
#103429=AXIS2_PLACEMENT_3D('',#419883,#125713,#125714);
#103430=AXIS2_PLACEMENT_3D('',#419884,#125715,#125716);
#103431=AXIS2_PLACEMENT_3D('',#419885,#125717,#125718);
#103432=AXIS2_PLACEMENT_3D('',#419886,#125719,#125720);
#103433=AXIS2_PLACEMENT_3D('',#419887,#125721,#125722);
#103434=AXIS2_PLACEMENT_3D('',#419888,#125723,#125724);
#103435=AXIS2_PLACEMENT_3D('',#419889,#125725,#125726);
#103436=AXIS2_PLACEMENT_3D('',#419890,#125727,#125728);
#103437=AXIS2_PLACEMENT_3D('',#419891,#125729,#125730);
#103438=AXIS2_PLACEMENT_3D('',#419892,#125731,#125732);
#103439=AXIS2_PLACEMENT_3D('',#419893,#125733,#125734);
#103440=AXIS2_PLACEMENT_3D('',#419894,#125735,#125736);
#103441=AXIS2_PLACEMENT_3D('',#419895,#125737,#125738);
#103442=AXIS2_PLACEMENT_3D('',#419896,#125739,#125740);
#103443=AXIS2_PLACEMENT_3D('',#419897,#125741,#125742);
#103444=AXIS2_PLACEMENT_3D('',#419898,#125743,#125744);
#103445=AXIS2_PLACEMENT_3D('',#419899,#125745,#125746);
#103446=AXIS2_PLACEMENT_3D('',#419900,#125747,#125748);
#103447=AXIS2_PLACEMENT_3D('',#419901,#125749,#125750);
#103448=AXIS2_PLACEMENT_3D('',#419902,#125751,#125752);
#103449=AXIS2_PLACEMENT_3D('',#419903,#125753,#125754);
#103450=AXIS2_PLACEMENT_3D('',#419904,#125755,#125756);
#103451=AXIS2_PLACEMENT_3D('',#419905,#125757,#125758);
#103452=AXIS2_PLACEMENT_3D('',#419906,#125759,#125760);
#103453=AXIS2_PLACEMENT_3D('',#419907,#125761,#125762);
#103454=AXIS2_PLACEMENT_3D('',#419908,#125763,#125764);
#103455=AXIS2_PLACEMENT_3D('',#419909,#125765,#125766);
#103456=AXIS2_PLACEMENT_3D('',#419910,#125767,#125768);
#103457=AXIS2_PLACEMENT_3D('',#419911,#125769,#125770);
#103458=AXIS2_PLACEMENT_3D('',#419912,#125771,#125772);
#103459=AXIS2_PLACEMENT_3D('',#419913,#125773,#125774);
#103460=AXIS2_PLACEMENT_3D('',#419914,#125775,#125776);
#103461=AXIS2_PLACEMENT_3D('',#419915,#125777,#125778);
#103462=AXIS2_PLACEMENT_3D('',#419916,#125779,#125780);
#103463=AXIS2_PLACEMENT_3D('',#419917,#125781,#125782);
#103464=AXIS2_PLACEMENT_3D('',#419918,#125783,#125784);
#103465=AXIS2_PLACEMENT_3D('',#419919,#125785,#125786);
#103466=AXIS2_PLACEMENT_3D('',#419920,#125787,#125788);
#103467=AXIS2_PLACEMENT_3D('',#419921,#125789,#125790);
#103468=AXIS2_PLACEMENT_3D('',#419922,#125791,#125792);
#103469=AXIS2_PLACEMENT_3D('',#419923,#125793,#125794);
#103470=AXIS2_PLACEMENT_3D('',#419924,#125795,#125796);
#103471=AXIS2_PLACEMENT_3D('',#419925,#125797,#125798);
#103472=AXIS2_PLACEMENT_3D('',#419926,#125799,#125800);
#103473=AXIS2_PLACEMENT_3D('',#419927,#125801,#125802);
#103474=AXIS2_PLACEMENT_3D('',#419928,#125803,#125804);
#103475=AXIS2_PLACEMENT_3D('',#419929,#125805,#125806);
#103476=AXIS2_PLACEMENT_3D('',#419930,#125807,#125808);
#103477=AXIS2_PLACEMENT_3D('',#419931,#125809,#125810);
#103478=AXIS2_PLACEMENT_3D('',#419932,#125811,#125812);
#103479=AXIS2_PLACEMENT_3D('',#419933,#125813,#125814);
#103480=AXIS2_PLACEMENT_3D('',#419934,#125815,#125816);
#103481=AXIS2_PLACEMENT_3D('',#419935,#125817,#125818);
#103482=AXIS2_PLACEMENT_3D('',#419936,#125819,#125820);
#103483=AXIS2_PLACEMENT_3D('',#419937,#125821,#125822);
#103484=AXIS2_PLACEMENT_3D('',#419938,#125823,#125824);
#103485=AXIS2_PLACEMENT_3D('',#419939,#125825,#125826);
#103486=AXIS2_PLACEMENT_3D('',#419940,#125827,#125828);
#103487=AXIS2_PLACEMENT_3D('',#419941,#125829,#125830);
#103488=AXIS2_PLACEMENT_3D('',#419942,#125831,#125832);
#103489=AXIS2_PLACEMENT_3D('',#419943,#125833,#125834);
#103490=AXIS2_PLACEMENT_3D('',#419944,#125835,#125836);
#103491=AXIS2_PLACEMENT_3D('',#419945,#125837,#125838);
#103492=AXIS2_PLACEMENT_3D('',#419946,#125839,#125840);
#103493=AXIS2_PLACEMENT_3D('',#419947,#125841,#125842);
#103494=AXIS2_PLACEMENT_3D('',#419948,#125843,#125844);
#103495=AXIS2_PLACEMENT_3D('',#419949,#125845,#125846);
#103496=AXIS2_PLACEMENT_3D('',#419950,#125847,#125848);
#103497=AXIS2_PLACEMENT_3D('',#419951,#125849,#125850);
#103498=AXIS2_PLACEMENT_3D('',#419952,#125851,#125852);
#103499=AXIS2_PLACEMENT_3D('',#419953,#125853,#125854);
#103500=AXIS2_PLACEMENT_3D('',#419954,#125855,#125856);
#103501=AXIS2_PLACEMENT_3D('',#419955,#125857,#125858);
#103502=AXIS2_PLACEMENT_3D('',#419956,#125859,#125860);
#103503=AXIS2_PLACEMENT_3D('',#419957,#125861,#125862);
#103504=AXIS2_PLACEMENT_3D('',#419958,#125863,#125864);
#103505=AXIS2_PLACEMENT_3D('',#419959,#125865,#125866);
#103506=AXIS2_PLACEMENT_3D('',#419960,#125867,#125868);
#103507=AXIS2_PLACEMENT_3D('',#419961,#125869,#125870);
#103508=AXIS2_PLACEMENT_3D('',#419962,#125871,#125872);
#103509=AXIS2_PLACEMENT_3D('',#419963,#125873,#125874);
#103510=AXIS2_PLACEMENT_3D('',#419964,#125875,#125876);
#103511=AXIS2_PLACEMENT_3D('',#419965,#125877,#125878);
#103512=AXIS2_PLACEMENT_3D('',#419966,#125879,#125880);
#103513=AXIS2_PLACEMENT_3D('',#419967,#125881,#125882);
#103514=AXIS2_PLACEMENT_3D('',#419968,#125883,#125884);
#103515=AXIS2_PLACEMENT_3D('',#419969,#125885,#125886);
#103516=AXIS2_PLACEMENT_3D('',#419970,#125887,#125888);
#103517=AXIS2_PLACEMENT_3D('',#419971,#125889,#125890);
#103518=AXIS2_PLACEMENT_3D('',#419972,#125891,#125892);
#103519=AXIS2_PLACEMENT_3D('',#419973,#125893,#125894);
#103520=AXIS2_PLACEMENT_3D('',#419974,#125895,#125896);
#103521=AXIS2_PLACEMENT_3D('',#419975,#125897,#125898);
#103522=AXIS2_PLACEMENT_3D('',#419976,#125899,#125900);
#103523=AXIS2_PLACEMENT_3D('',#419977,#125901,#125902);
#103524=AXIS2_PLACEMENT_3D('',#419978,#125903,#125904);
#103525=AXIS2_PLACEMENT_3D('',#419979,#125905,#125906);
#103526=AXIS2_PLACEMENT_3D('',#419980,#125907,#125908);
#103527=AXIS2_PLACEMENT_3D('',#419981,#125909,#125910);
#103528=AXIS2_PLACEMENT_3D('',#419982,#125911,#125912);
#103529=AXIS2_PLACEMENT_3D('',#420056,#125915,#125916);
#103530=AXIS2_PLACEMENT_3D('',#420057,#125917,#125918);
#103531=AXIS2_PLACEMENT_3D('',#420058,#125919,#125920);
#103532=AXIS2_PLACEMENT_3D('',#420061,#125921,#125922);
#103533=AXIS2_PLACEMENT_3D('',#420069,#125925,#125926);
#103534=AXIS2_PLACEMENT_3D('',#420073,#125928,#125929);
#103535=AXIS2_PLACEMENT_3D('',#420080,#125931,#125932);
#103536=AXIS2_PLACEMENT_3D('',#420081,#125933,#125934);
#103537=AXIS2_PLACEMENT_3D('',#420085,#125937,#125938);
#103538=AXIS2_PLACEMENT_3D('',#420089,#125941,#125942);
#103539=AXIS2_PLACEMENT_3D('',#420093,#125945,#125946);
#103540=AXIS2_PLACEMENT_3D('',#420097,#125949,#125950);
#103541=AXIS2_PLACEMENT_3D('',#420101,#125953,#125954);
#103542=AXIS2_PLACEMENT_3D('',#420104,#125955,#125956);
#103543=AXIS2_PLACEMENT_3D('',#420105,#125957,#125958);
#103544=AXIS2_PLACEMENT_3D('',#420107,#125959,#125960);
#103545=AXIS2_PLACEMENT_3D('',#420109,#125961,#125962);
#103546=AXIS2_PLACEMENT_3D('',#420110,#125963,#125964);
#103547=AXIS2_PLACEMENT_3D('',#420111,#125965,#125966);
#103548=AXIS2_PLACEMENT_3D('',#420112,#125967,#125968);
#103549=AXIS2_PLACEMENT_3D('',#420113,#125969,#125970);
#103550=AXIS2_PLACEMENT_3D('',#420114,#125971,#125972);
#103551=AXIS2_PLACEMENT_3D('',#420122,#125976,#125977);
#103552=AXIS2_PLACEMENT_3D('',#420124,#125979,#125980);
#103553=AXIS2_PLACEMENT_3D('',#420129,#125982,#125983);
#103554=AXIS2_PLACEMENT_3D('',#420134,#125985,#125986);
#103555=AXIS2_PLACEMENT_3D('',#420139,#125988,#125989);
#103556=AXIS2_PLACEMENT_3D('',#420144,#125991,#125992);
#103557=AXIS2_PLACEMENT_3D('',#420145,#125993,#125994);
#103558=AXIS2_PLACEMENT_3D('',#420146,#125995,#125996);
#103559=AXIS2_PLACEMENT_3D('',#420147,#125997,#125998);
#103560=AXIS2_PLACEMENT_3D('',#420148,#125999,#126000);
#103561=AXIS2_PLACEMENT_3D('',#420149,#126001,#126002);
#103562=AXIS2_PLACEMENT_3D('',#420150,#126003,#126004);
#103563=AXIS2_PLACEMENT_3D('',#421382,#126005,#126006);
#103564=AXIS2_PLACEMENT_3D('',#422616,#126007,#126008);
#103565=AXIS2_PLACEMENT_3D('',#422653,#126009,#126010);
#103566=AXIS2_PLACEMENT_3D('',#422701,#126011,#126012);
#103567=AXIS2_PLACEMENT_3D('',#422702,#126013,#126014);
#103568=AXIS2_PLACEMENT_3D('',#422703,#126015,#126016);
#103569=AXIS2_PLACEMENT_3D('',#422704,#126017,#126018);
#103570=AXIS2_PLACEMENT_3D('',#422723,#126019,#126020);
#103571=AXIS2_PLACEMENT_3D('',#422748,#126021,#126022);
#103572=AXIS2_PLACEMENT_3D('',#422807,#126023,#126024);
#103573=AXIS2_PLACEMENT_3D('',#422820,#126025,#126026);
#103574=AXIS2_PLACEMENT_3D('',#422839,#126027,#126028);
#103575=AXIS2_PLACEMENT_3D('',#422840,#126029,#126030);
#103576=AXIS2_PLACEMENT_3D('',#422841,#126031,#126032);
#103577=AXIS2_PLACEMENT_3D('',#422854,#126033,#126034);
#103578=AXIS2_PLACEMENT_3D('',#422867,#126035,#126036);
#103579=AXIS2_PLACEMENT_3D('',#422874,#126039,#126040);
#103580=AXIS2_PLACEMENT_3D('',#422881,#126042,#126043);
#103581=AXIS2_PLACEMENT_3D('',#422884,#126044,#126045);
#103582=AXIS2_PLACEMENT_3D('',#422895,#126049,#126050);
#103583=AXIS2_PLACEMENT_3D('',#422963,#126051,#126052);
#103584=AXIS2_PLACEMENT_3D('',#422964,#126053,#126054);
#103585=AXIS2_PLACEMENT_3D('',#423006,#126055,#126056);
#103586=AXIS2_PLACEMENT_3D('',#423033,#126057,#126058);
#103587=AXIS2_PLACEMENT_3D('',#423114,#126059,#126060);
#103588=AXIS2_PLACEMENT_3D('',#423127,#126061,#126062);
#103589=AXIS2_PLACEMENT_3D('',#423128,#126063,#126064);
#103590=AXIS2_PLACEMENT_3D('',#423129,#126065,#126066);
#103591=AXIS2_PLACEMENT_3D('',#423142,#126067,#126068);
#103592=AXIS2_PLACEMENT_3D('',#423155,#126069,#126070);
#103593=AXIS2_PLACEMENT_3D('',#423174,#126071,#126072);
#103594=AXIS2_PLACEMENT_3D('',#423187,#126073,#126074);
#103595=AXIS2_PLACEMENT_3D('',#423200,#126075,#126076);
#103596=AXIS2_PLACEMENT_3D('',#423201,#126077,#126078);
#103597=AXIS2_PLACEMENT_3D('',#423202,#126079,#126080);
#103598=AXIS2_PLACEMENT_3D('',#423215,#126081,#126082);
#103599=AXIS2_PLACEMENT_3D('',#423216,#126083,#126084);
#103600=AXIS2_PLACEMENT_3D('',#423223,#126087,#126088);
#103601=AXIS2_PLACEMENT_3D('',#423230,#126090,#126091);
#103602=AXIS2_PLACEMENT_3D('',#423233,#126092,#126093);
#103603=AXIS2_PLACEMENT_3D('',#423244,#126097,#126098);
#103604=AXIS2_PLACEMENT_3D('',#423312,#126099,#126100);
#103605=AXIS2_PLACEMENT_3D('',#423313,#126101,#126102);
#103606=AXIS2_PLACEMENT_3D('',#423355,#126103,#126104);
#103607=AXIS2_PLACEMENT_3D('',#423382,#126105,#126106);
#103608=AXIS2_PLACEMENT_3D('',#423463,#126107,#126108);
#103609=AXIS2_PLACEMENT_3D('',#423476,#126109,#126110);
#103610=AXIS2_PLACEMENT_3D('',#423477,#126111,#126112);
#103611=AXIS2_PLACEMENT_3D('',#423478,#126113,#126114);
#103612=AXIS2_PLACEMENT_3D('',#423491,#126115,#126116);
#103613=AXIS2_PLACEMENT_3D('',#423504,#126117,#126118);
#103614=AXIS2_PLACEMENT_3D('',#423523,#126119,#126120);
#103615=AXIS2_PLACEMENT_3D('',#423536,#126121,#126122);
#103616=AXIS2_PLACEMENT_3D('',#423549,#126123,#126124);
#103617=AXIS2_PLACEMENT_3D('',#423550,#126125,#126126);
#103618=AXIS2_PLACEMENT_3D('',#423551,#126127,#126128);
#103619=AXIS2_PLACEMENT_3D('',#423564,#126129,#126130);
#103620=AXIS2_PLACEMENT_3D('',#423565,#126131,#126132);
#103621=AXIS2_PLACEMENT_3D('',#423572,#126135,#126136);
#103622=AXIS2_PLACEMENT_3D('',#423579,#126138,#126139);
#103623=AXIS2_PLACEMENT_3D('',#423582,#126140,#126141);
#103624=AXIS2_PLACEMENT_3D('',#423593,#126145,#126146);
#103625=AXIS2_PLACEMENT_3D('',#423661,#126147,#126148);
#103626=AXIS2_PLACEMENT_3D('',#423662,#126149,#126150);
#103627=AXIS2_PLACEMENT_3D('',#423704,#126151,#126152);
#103628=AXIS2_PLACEMENT_3D('',#423731,#126153,#126154);
#103629=AXIS2_PLACEMENT_3D('',#423812,#126155,#126156);
#103630=AXIS2_PLACEMENT_3D('',#423825,#126157,#126158);
#103631=AXIS2_PLACEMENT_3D('',#423826,#126159,#126160);
#103632=AXIS2_PLACEMENT_3D('',#423827,#126161,#126162);
#103633=AXIS2_PLACEMENT_3D('',#423840,#126163,#126164);
#103634=AXIS2_PLACEMENT_3D('',#423853,#126165,#126166);
#103635=AXIS2_PLACEMENT_3D('',#423872,#126167,#126168);
#103636=AXIS2_PLACEMENT_3D('',#423885,#126169,#126170);
#103637=AXIS2_PLACEMENT_3D('',#423898,#126171,#126172);
#103638=AXIS2_PLACEMENT_3D('',#423899,#126173,#126174);
#103639=AXIS2_PLACEMENT_3D('',#423900,#126175,#126176);
#103640=AXIS2_PLACEMENT_3D('',#423913,#126177,#126178);
#103641=AXIS2_PLACEMENT_3D('',#423914,#126179,#126180);
#103642=AXIS2_PLACEMENT_3D('',#423921,#126183,#126184);
#103643=AXIS2_PLACEMENT_3D('',#423928,#126186,#126187);
#103644=AXIS2_PLACEMENT_3D('',#423931,#126188,#126189);
#103645=AXIS2_PLACEMENT_3D('',#423942,#126193,#126194);
#103646=AXIS2_PLACEMENT_3D('',#424010,#126195,#126196);
#103647=AXIS2_PLACEMENT_3D('',#424011,#126197,#126198);
#103648=AXIS2_PLACEMENT_3D('',#424053,#126199,#126200);
#103649=AXIS2_PLACEMENT_3D('',#424080,#126201,#126202);
#103650=AXIS2_PLACEMENT_3D('',#424161,#126203,#126204);
#103651=AXIS2_PLACEMENT_3D('',#424174,#126205,#126206);
#103652=AXIS2_PLACEMENT_3D('',#424175,#126207,#126208);
#103653=AXIS2_PLACEMENT_3D('',#424176,#126209,#126210);
#103654=AXIS2_PLACEMENT_3D('',#424189,#126211,#126212);
#103655=AXIS2_PLACEMENT_3D('',#424202,#126213,#126214);
#103656=AXIS2_PLACEMENT_3D('',#424221,#126215,#126216);
#103657=AXIS2_PLACEMENT_3D('',#424234,#126217,#126218);
#103658=AXIS2_PLACEMENT_3D('',#424247,#126219,#126220);
#103659=AXIS2_PLACEMENT_3D('',#424248,#126221,#126222);
#103660=AXIS2_PLACEMENT_3D('',#424249,#126223,#126224);
#103661=AXIS2_PLACEMENT_3D('',#424262,#126225,#126226);
#103662=AXIS2_PLACEMENT_3D('',#424263,#126227,#126228);
#103663=AXIS2_PLACEMENT_3D('',#424270,#126231,#126232);
#103664=AXIS2_PLACEMENT_3D('',#424277,#126234,#126235);
#103665=AXIS2_PLACEMENT_3D('',#424280,#126236,#126237);
#103666=AXIS2_PLACEMENT_3D('',#424291,#126241,#126242);
#103667=AXIS2_PLACEMENT_3D('',#424359,#126243,#126244);
#103668=AXIS2_PLACEMENT_3D('',#424360,#126245,#126246);
#103669=AXIS2_PLACEMENT_3D('',#424402,#126247,#126248);
#103670=AXIS2_PLACEMENT_3D('',#424429,#126249,#126250);
#103671=AXIS2_PLACEMENT_3D('',#424510,#126251,#126252);
#103672=AXIS2_PLACEMENT_3D('',#424523,#126253,#126254);
#103673=AXIS2_PLACEMENT_3D('',#424524,#126255,#126256);
#103674=AXIS2_PLACEMENT_3D('',#424525,#126257,#126258);
#103675=AXIS2_PLACEMENT_3D('',#424538,#126259,#126260);
#103676=AXIS2_PLACEMENT_3D('',#424551,#126261,#126262);
#103677=AXIS2_PLACEMENT_3D('',#424570,#126263,#126264);
#103678=AXIS2_PLACEMENT_3D('',#424583,#126265,#126266);
#103679=AXIS2_PLACEMENT_3D('',#424596,#126267,#126268);
#103680=AXIS2_PLACEMENT_3D('',#424597,#126269,#126270);
#103681=AXIS2_PLACEMENT_3D('',#424598,#126271,#126272);
#103682=AXIS2_PLACEMENT_3D('',#424611,#126273,#126274);
#103683=AXIS2_PLACEMENT_3D('',#424612,#126275,#126276);
#103684=AXIS2_PLACEMENT_3D('',#424619,#126279,#126280);
#103685=AXIS2_PLACEMENT_3D('',#424626,#126282,#126283);
#103686=AXIS2_PLACEMENT_3D('',#424629,#126284,#126285);
#103687=AXIS2_PLACEMENT_3D('',#424640,#126289,#126290);
#103688=AXIS2_PLACEMENT_3D('',#424708,#126291,#126292);
#103689=AXIS2_PLACEMENT_3D('',#424709,#126293,#126294);
#103690=AXIS2_PLACEMENT_3D('',#424751,#126295,#126296);
#103691=AXIS2_PLACEMENT_3D('',#424778,#126297,#126298);
#103692=AXIS2_PLACEMENT_3D('',#424859,#126299,#126300);
#103693=AXIS2_PLACEMENT_3D('',#424872,#126301,#126302);
#103694=AXIS2_PLACEMENT_3D('',#424873,#126303,#126304);
#103695=AXIS2_PLACEMENT_3D('',#424874,#126305,#126306);
#103696=AXIS2_PLACEMENT_3D('',#424887,#126307,#126308);
#103697=AXIS2_PLACEMENT_3D('',#424900,#126309,#126310);
#103698=AXIS2_PLACEMENT_3D('',#424919,#126311,#126312);
#103699=AXIS2_PLACEMENT_3D('',#424932,#126313,#126314);
#103700=AXIS2_PLACEMENT_3D('',#424945,#126315,#126316);
#103701=AXIS2_PLACEMENT_3D('',#424946,#126317,#126318);
#103702=AXIS2_PLACEMENT_3D('',#424947,#126319,#126320);
#103703=AXIS2_PLACEMENT_3D('',#424960,#126321,#126322);
#103704=AXIS2_PLACEMENT_3D('',#424961,#126323,#126324);
#103705=AXIS2_PLACEMENT_3D('',#424968,#126327,#126328);
#103706=AXIS2_PLACEMENT_3D('',#424975,#126330,#126331);
#103707=AXIS2_PLACEMENT_3D('',#424978,#126332,#126333);
#103708=AXIS2_PLACEMENT_3D('',#424989,#126337,#126338);
#103709=AXIS2_PLACEMENT_3D('',#425057,#126339,#126340);
#103710=AXIS2_PLACEMENT_3D('',#425058,#126341,#126342);
#103711=AXIS2_PLACEMENT_3D('',#425100,#126343,#126344);
#103712=AXIS2_PLACEMENT_3D('',#425127,#126345,#126346);
#103713=AXIS2_PLACEMENT_3D('',#425208,#126347,#126348);
#103714=AXIS2_PLACEMENT_3D('',#425221,#126349,#126350);
#103715=AXIS2_PLACEMENT_3D('',#425222,#126351,#126352);
#103716=AXIS2_PLACEMENT_3D('',#425223,#126353,#126354);
#103717=AXIS2_PLACEMENT_3D('',#425236,#126355,#126356);
#103718=AXIS2_PLACEMENT_3D('',#425249,#126357,#126358);
#103719=AXIS2_PLACEMENT_3D('',#425268,#126359,#126360);
#103720=AXIS2_PLACEMENT_3D('',#425281,#126361,#126362);
#103721=AXIS2_PLACEMENT_3D('',#425294,#126363,#126364);
#103722=AXIS2_PLACEMENT_3D('',#425295,#126365,#126366);
#103723=AXIS2_PLACEMENT_3D('',#425296,#126367,#126368);
#103724=AXIS2_PLACEMENT_3D('',#425309,#126369,#126370);
#103725=AXIS2_PLACEMENT_3D('',#425310,#126371,#126372);
#103726=AXIS2_PLACEMENT_3D('',#425317,#126375,#126376);
#103727=AXIS2_PLACEMENT_3D('',#425324,#126378,#126379);
#103728=AXIS2_PLACEMENT_3D('',#425327,#126380,#126381);
#103729=AXIS2_PLACEMENT_3D('',#425338,#126385,#126386);
#103730=AXIS2_PLACEMENT_3D('',#425406,#126387,#126388);
#103731=AXIS2_PLACEMENT_3D('',#425407,#126389,#126390);
#103732=AXIS2_PLACEMENT_3D('',#425449,#126391,#126392);
#103733=AXIS2_PLACEMENT_3D('',#425476,#126393,#126394);
#103734=AXIS2_PLACEMENT_3D('',#425557,#126395,#126396);
#103735=AXIS2_PLACEMENT_3D('',#425570,#126397,#126398);
#103736=AXIS2_PLACEMENT_3D('',#425571,#126399,#126400);
#103737=AXIS2_PLACEMENT_3D('',#425572,#126401,#126402);
#103738=AXIS2_PLACEMENT_3D('',#425585,#126403,#126404);
#103739=AXIS2_PLACEMENT_3D('',#425598,#126405,#126406);
#103740=AXIS2_PLACEMENT_3D('',#425617,#126407,#126408);
#103741=AXIS2_PLACEMENT_3D('',#425630,#126409,#126410);
#103742=AXIS2_PLACEMENT_3D('',#425643,#126411,#126412);
#103743=AXIS2_PLACEMENT_3D('',#425644,#126413,#126414);
#103744=AXIS2_PLACEMENT_3D('',#425645,#126415,#126416);
#103745=AXIS2_PLACEMENT_3D('',#425658,#126417,#126418);
#103746=AXIS2_PLACEMENT_3D('',#425659,#126419,#126420);
#103747=AXIS2_PLACEMENT_3D('',#425666,#126423,#126424);
#103748=AXIS2_PLACEMENT_3D('',#425673,#126426,#126427);
#103749=AXIS2_PLACEMENT_3D('',#425676,#126428,#126429);
#103750=AXIS2_PLACEMENT_3D('',#425687,#126433,#126434);
#103751=AXIS2_PLACEMENT_3D('',#425755,#126435,#126436);
#103752=AXIS2_PLACEMENT_3D('',#425756,#126437,#126438);
#103753=AXIS2_PLACEMENT_3D('',#425798,#126439,#126440);
#103754=AXIS2_PLACEMENT_3D('',#425825,#126441,#126442);
#103755=AXIS2_PLACEMENT_3D('',#425906,#126443,#126444);
#103756=AXIS2_PLACEMENT_3D('',#425919,#126445,#126446);
#103757=AXIS2_PLACEMENT_3D('',#425920,#126447,#126448);
#103758=AXIS2_PLACEMENT_3D('',#425921,#126449,#126450);
#103759=AXIS2_PLACEMENT_3D('',#425934,#126451,#126452);
#103760=AXIS2_PLACEMENT_3D('',#425947,#126453,#126454);
#103761=AXIS2_PLACEMENT_3D('',#425966,#126455,#126456);
#103762=AXIS2_PLACEMENT_3D('',#425979,#126457,#126458);
#103763=AXIS2_PLACEMENT_3D('',#425992,#126459,#126460);
#103764=AXIS2_PLACEMENT_3D('',#425993,#126461,#126462);
#103765=AXIS2_PLACEMENT_3D('',#425994,#126463,#126464);
#103766=AXIS2_PLACEMENT_3D('',#426007,#126465,#126466);
#103767=AXIS2_PLACEMENT_3D('',#426008,#126467,#126468);
#103768=AXIS2_PLACEMENT_3D('',#426015,#126471,#126472);
#103769=AXIS2_PLACEMENT_3D('',#426022,#126474,#126475);
#103770=AXIS2_PLACEMENT_3D('',#426025,#126476,#126477);
#103771=AXIS2_PLACEMENT_3D('',#426036,#126481,#126482);
#103772=AXIS2_PLACEMENT_3D('',#426104,#126483,#126484);
#103773=AXIS2_PLACEMENT_3D('',#426105,#126485,#126486);
#103774=AXIS2_PLACEMENT_3D('',#426147,#126487,#126488);
#103775=AXIS2_PLACEMENT_3D('',#426174,#126489,#126490);
#103776=AXIS2_PLACEMENT_3D('',#426255,#126491,#126492);
#103777=AXIS2_PLACEMENT_3D('',#426268,#126493,#126494);
#103778=AXIS2_PLACEMENT_3D('',#426269,#126495,#126496);
#103779=AXIS2_PLACEMENT_3D('',#426270,#126497,#126498);
#103780=AXIS2_PLACEMENT_3D('',#426283,#126499,#126500);
#103781=AXIS2_PLACEMENT_3D('',#426296,#126501,#126502);
#103782=AXIS2_PLACEMENT_3D('',#426315,#126503,#126504);
#103783=AXIS2_PLACEMENT_3D('',#426328,#126505,#126506);
#103784=AXIS2_PLACEMENT_3D('',#426341,#126507,#126508);
#103785=AXIS2_PLACEMENT_3D('',#426342,#126509,#126510);
#103786=AXIS2_PLACEMENT_3D('',#426343,#126511,#126512);
#103787=AXIS2_PLACEMENT_3D('',#426356,#126513,#126514);
#103788=AXIS2_PLACEMENT_3D('',#426357,#126515,#126516);
#103789=AXIS2_PLACEMENT_3D('',#426364,#126519,#126520);
#103790=AXIS2_PLACEMENT_3D('',#426371,#126522,#126523);
#103791=AXIS2_PLACEMENT_3D('',#426374,#126524,#126525);
#103792=AXIS2_PLACEMENT_3D('',#426385,#126529,#126530);
#103793=AXIS2_PLACEMENT_3D('',#426453,#126531,#126532);
#103794=AXIS2_PLACEMENT_3D('',#426454,#126533,#126534);
#103795=AXIS2_PLACEMENT_3D('',#426496,#126535,#126536);
#103796=AXIS2_PLACEMENT_3D('',#426523,#126537,#126538);
#103797=AXIS2_PLACEMENT_3D('',#426604,#126539,#126540);
#103798=AXIS2_PLACEMENT_3D('',#426617,#126541,#126542);
#103799=AXIS2_PLACEMENT_3D('',#426618,#126543,#126544);
#103800=AXIS2_PLACEMENT_3D('',#426619,#126545,#126546);
#103801=AXIS2_PLACEMENT_3D('',#426632,#126547,#126548);
#103802=AXIS2_PLACEMENT_3D('',#426645,#126549,#126550);
#103803=AXIS2_PLACEMENT_3D('',#426664,#126551,#126552);
#103804=AXIS2_PLACEMENT_3D('',#426677,#126553,#126554);
#103805=AXIS2_PLACEMENT_3D('',#426690,#126555,#126556);
#103806=AXIS2_PLACEMENT_3D('',#426691,#126557,#126558);
#103807=AXIS2_PLACEMENT_3D('',#426692,#126559,#126560);
#103808=AXIS2_PLACEMENT_3D('',#426705,#126561,#126562);
#103809=AXIS2_PLACEMENT_3D('',#426706,#126563,#126564);
#103810=AXIS2_PLACEMENT_3D('',#426713,#126567,#126568);
#103811=AXIS2_PLACEMENT_3D('',#426720,#126570,#126571);
#103812=AXIS2_PLACEMENT_3D('',#426723,#126572,#126573);
#103813=AXIS2_PLACEMENT_3D('',#426734,#126577,#126578);
#103814=AXIS2_PLACEMENT_3D('',#426802,#126579,#126580);
#103815=AXIS2_PLACEMENT_3D('',#426803,#126581,#126582);
#103816=AXIS2_PLACEMENT_3D('',#426845,#126583,#126584);
#103817=AXIS2_PLACEMENT_3D('',#426872,#126585,#126586);
#103818=AXIS2_PLACEMENT_3D('',#426953,#126587,#126588);
#103819=AXIS2_PLACEMENT_3D('',#426966,#126589,#126590);
#103820=AXIS2_PLACEMENT_3D('',#426967,#126591,#126592);
#103821=AXIS2_PLACEMENT_3D('',#426968,#126593,#126594);
#103822=AXIS2_PLACEMENT_3D('',#426981,#126595,#126596);
#103823=AXIS2_PLACEMENT_3D('',#426994,#126597,#126598);
#103824=AXIS2_PLACEMENT_3D('',#427013,#126599,#126600);
#103825=AXIS2_PLACEMENT_3D('',#427026,#126601,#126602);
#103826=AXIS2_PLACEMENT_3D('',#427039,#126603,#126604);
#103827=AXIS2_PLACEMENT_3D('',#427040,#126605,#126606);
#103828=AXIS2_PLACEMENT_3D('',#427041,#126607,#126608);
#103829=AXIS2_PLACEMENT_3D('',#427054,#126609,#126610);
#103830=AXIS2_PLACEMENT_3D('',#427055,#126611,#126612);
#103831=AXIS2_PLACEMENT_3D('',#427062,#126615,#126616);
#103832=AXIS2_PLACEMENT_3D('',#427069,#126618,#126619);
#103833=AXIS2_PLACEMENT_3D('',#427072,#126620,#126621);
#103834=AXIS2_PLACEMENT_3D('',#427083,#126625,#126626);
#103835=AXIS2_PLACEMENT_3D('',#427151,#126627,#126628);
#103836=AXIS2_PLACEMENT_3D('',#427152,#126629,#126630);
#103837=AXIS2_PLACEMENT_3D('',#427194,#126631,#126632);
#103838=AXIS2_PLACEMENT_3D('',#427221,#126633,#126634);
#103839=AXIS2_PLACEMENT_3D('',#427302,#126635,#126636);
#103840=AXIS2_PLACEMENT_3D('',#427315,#126637,#126638);
#103841=AXIS2_PLACEMENT_3D('',#427316,#126639,#126640);
#103842=AXIS2_PLACEMENT_3D('',#427317,#126641,#126642);
#103843=AXIS2_PLACEMENT_3D('',#427330,#126643,#126644);
#103844=AXIS2_PLACEMENT_3D('',#427343,#126645,#126646);
#103845=AXIS2_PLACEMENT_3D('',#427362,#126647,#126648);
#103846=AXIS2_PLACEMENT_3D('',#427375,#126649,#126650);
#103847=AXIS2_PLACEMENT_3D('',#427388,#126651,#126652);
#103848=AXIS2_PLACEMENT_3D('',#427389,#126653,#126654);
#103849=AXIS2_PLACEMENT_3D('',#427390,#126655,#126656);
#103850=AXIS2_PLACEMENT_3D('',#427403,#126657,#126658);
#103851=AXIS2_PLACEMENT_3D('',#427404,#126659,#126660);
#103852=AXIS2_PLACEMENT_3D('',#427411,#126663,#126664);
#103853=AXIS2_PLACEMENT_3D('',#427418,#126666,#126667);
#103854=AXIS2_PLACEMENT_3D('',#427421,#126668,#126669);
#103855=AXIS2_PLACEMENT_3D('',#427432,#126673,#126674);
#103856=AXIS2_PLACEMENT_3D('',#427500,#126675,#126676);
#103857=AXIS2_PLACEMENT_3D('',#427501,#126677,#126678);
#103858=AXIS2_PLACEMENT_3D('',#427543,#126679,#126680);
#103859=AXIS2_PLACEMENT_3D('',#427570,#126681,#126682);
#103860=AXIS2_PLACEMENT_3D('',#427651,#126683,#126684);
#103861=AXIS2_PLACEMENT_3D('',#427664,#126685,#126686);
#103862=AXIS2_PLACEMENT_3D('',#427665,#126687,#126688);
#103863=AXIS2_PLACEMENT_3D('',#427666,#126689,#126690);
#103864=AXIS2_PLACEMENT_3D('',#427679,#126691,#126692);
#103865=AXIS2_PLACEMENT_3D('',#427692,#126693,#126694);
#103866=AXIS2_PLACEMENT_3D('',#427711,#126695,#126696);
#103867=AXIS2_PLACEMENT_3D('',#427724,#126697,#126698);
#103868=AXIS2_PLACEMENT_3D('',#427737,#126699,#126700);
#103869=AXIS2_PLACEMENT_3D('',#427738,#126701,#126702);
#103870=AXIS2_PLACEMENT_3D('',#427739,#126703,#126704);
#103871=AXIS2_PLACEMENT_3D('',#427752,#126705,#126706);
#103872=AXIS2_PLACEMENT_3D('',#427753,#126707,#126708);
#103873=AXIS2_PLACEMENT_3D('',#427760,#126711,#126712);
#103874=AXIS2_PLACEMENT_3D('',#427767,#126714,#126715);
#103875=AXIS2_PLACEMENT_3D('',#427770,#126716,#126717);
#103876=AXIS2_PLACEMENT_3D('',#427781,#126721,#126722);
#103877=AXIS2_PLACEMENT_3D('',#427849,#126723,#126724);
#103878=AXIS2_PLACEMENT_3D('',#427850,#126725,#126726);
#103879=AXIS2_PLACEMENT_3D('',#427892,#126727,#126728);
#103880=AXIS2_PLACEMENT_3D('',#427919,#126729,#126730);
#103881=AXIS2_PLACEMENT_3D('',#428000,#126731,#126732);
#103882=AXIS2_PLACEMENT_3D('',#428013,#126733,#126734);
#103883=AXIS2_PLACEMENT_3D('',#428014,#126735,#126736);
#103884=AXIS2_PLACEMENT_3D('',#428015,#126737,#126738);
#103885=AXIS2_PLACEMENT_3D('',#428028,#126739,#126740);
#103886=AXIS2_PLACEMENT_3D('',#428041,#126741,#126742);
#103887=AXIS2_PLACEMENT_3D('',#428060,#126743,#126744);
#103888=AXIS2_PLACEMENT_3D('',#428073,#126745,#126746);
#103889=AXIS2_PLACEMENT_3D('',#428086,#126747,#126748);
#103890=AXIS2_PLACEMENT_3D('',#428087,#126749,#126750);
#103891=AXIS2_PLACEMENT_3D('',#428088,#126751,#126752);
#103892=AXIS2_PLACEMENT_3D('',#428101,#126753,#126754);
#103893=AXIS2_PLACEMENT_3D('',#428102,#126755,#126756);
#103894=AXIS2_PLACEMENT_3D('',#428109,#126759,#126760);
#103895=AXIS2_PLACEMENT_3D('',#428116,#126762,#126763);
#103896=AXIS2_PLACEMENT_3D('',#428119,#126764,#126765);
#103897=AXIS2_PLACEMENT_3D('',#428130,#126769,#126770);
#103898=AXIS2_PLACEMENT_3D('',#428198,#126771,#126772);
#103899=AXIS2_PLACEMENT_3D('',#428199,#126773,#126774);
#103900=AXIS2_PLACEMENT_3D('',#428241,#126775,#126776);
#103901=AXIS2_PLACEMENT_3D('',#428268,#126777,#126778);
#103902=AXIS2_PLACEMENT_3D('',#428349,#126779,#126780);
#103903=AXIS2_PLACEMENT_3D('',#428362,#126781,#126782);
#103904=AXIS2_PLACEMENT_3D('',#428363,#126783,#126784);
#103905=AXIS2_PLACEMENT_3D('',#428364,#126785,#126786);
#103906=AXIS2_PLACEMENT_3D('',#428377,#126787,#126788);
#103907=AXIS2_PLACEMENT_3D('',#428390,#126789,#126790);
#103908=AXIS2_PLACEMENT_3D('',#428409,#126791,#126792);
#103909=AXIS2_PLACEMENT_3D('',#428422,#126793,#126794);
#103910=AXIS2_PLACEMENT_3D('',#428435,#126795,#126796);
#103911=AXIS2_PLACEMENT_3D('',#428436,#126797,#126798);
#103912=AXIS2_PLACEMENT_3D('',#428437,#126799,#126800);
#103913=AXIS2_PLACEMENT_3D('',#428450,#126801,#126802);
#103914=AXIS2_PLACEMENT_3D('',#428451,#126803,#126804);
#103915=AXIS2_PLACEMENT_3D('',#428458,#126807,#126808);
#103916=AXIS2_PLACEMENT_3D('',#428465,#126810,#126811);
#103917=AXIS2_PLACEMENT_3D('',#428468,#126812,#126813);
#103918=AXIS2_PLACEMENT_3D('',#428479,#126817,#126818);
#103919=AXIS2_PLACEMENT_3D('',#428547,#126819,#126820);
#103920=AXIS2_PLACEMENT_3D('',#428548,#126821,#126822);
#103921=AXIS2_PLACEMENT_3D('',#428590,#126823,#126824);
#103922=AXIS2_PLACEMENT_3D('',#428617,#126825,#126826);
#103923=AXIS2_PLACEMENT_3D('',#428698,#126827,#126828);
#103924=AXIS2_PLACEMENT_3D('',#428711,#126829,#126830);
#103925=AXIS2_PLACEMENT_3D('',#428712,#126831,#126832);
#103926=AXIS2_PLACEMENT_3D('',#428713,#126833,#126834);
#103927=AXIS2_PLACEMENT_3D('',#428726,#126835,#126836);
#103928=AXIS2_PLACEMENT_3D('',#428739,#126837,#126838);
#103929=AXIS2_PLACEMENT_3D('',#428758,#126839,#126840);
#103930=AXIS2_PLACEMENT_3D('',#428771,#126841,#126842);
#103931=AXIS2_PLACEMENT_3D('',#428784,#126843,#126844);
#103932=AXIS2_PLACEMENT_3D('',#428785,#126845,#126846);
#103933=AXIS2_PLACEMENT_3D('',#428786,#126847,#126848);
#103934=AXIS2_PLACEMENT_3D('',#428799,#126849,#126850);
#103935=AXIS2_PLACEMENT_3D('',#428800,#126851,#126852);
#103936=AXIS2_PLACEMENT_3D('',#428807,#126855,#126856);
#103937=AXIS2_PLACEMENT_3D('',#428814,#126858,#126859);
#103938=AXIS2_PLACEMENT_3D('',#428817,#126860,#126861);
#103939=AXIS2_PLACEMENT_3D('',#428828,#126865,#126866);
#103940=AXIS2_PLACEMENT_3D('',#428896,#126867,#126868);
#103941=AXIS2_PLACEMENT_3D('',#428897,#126869,#126870);
#103942=AXIS2_PLACEMENT_3D('',#428939,#126871,#126872);
#103943=AXIS2_PLACEMENT_3D('',#428966,#126873,#126874);
#103944=AXIS2_PLACEMENT_3D('',#429047,#126875,#126876);
#103945=AXIS2_PLACEMENT_3D('',#429060,#126877,#126878);
#103946=AXIS2_PLACEMENT_3D('',#429061,#126879,#126880);
#103947=AXIS2_PLACEMENT_3D('',#429062,#126881,#126882);
#103948=AXIS2_PLACEMENT_3D('',#429075,#126883,#126884);
#103949=AXIS2_PLACEMENT_3D('',#429088,#126885,#126886);
#103950=AXIS2_PLACEMENT_3D('',#429107,#126887,#126888);
#103951=AXIS2_PLACEMENT_3D('',#429120,#126889,#126890);
#103952=AXIS2_PLACEMENT_3D('',#429133,#126891,#126892);
#103953=AXIS2_PLACEMENT_3D('',#429134,#126893,#126894);
#103954=AXIS2_PLACEMENT_3D('',#429135,#126895,#126896);
#103955=AXIS2_PLACEMENT_3D('',#429148,#126897,#126898);
#103956=AXIS2_PLACEMENT_3D('',#429149,#126899,#126900);
#103957=AXIS2_PLACEMENT_3D('',#429156,#126903,#126904);
#103958=AXIS2_PLACEMENT_3D('',#429163,#126906,#126907);
#103959=AXIS2_PLACEMENT_3D('',#429166,#126908,#126909);
#103960=AXIS2_PLACEMENT_3D('',#429177,#126913,#126914);
#103961=AXIS2_PLACEMENT_3D('',#429245,#126915,#126916);
#103962=AXIS2_PLACEMENT_3D('',#429246,#126917,#126918);
#103963=AXIS2_PLACEMENT_3D('',#429288,#126919,#126920);
#103964=AXIS2_PLACEMENT_3D('',#429315,#126921,#126922);
#103965=AXIS2_PLACEMENT_3D('',#429396,#126923,#126924);
#103966=AXIS2_PLACEMENT_3D('',#429409,#126925,#126926);
#103967=AXIS2_PLACEMENT_3D('',#429410,#126927,#126928);
#103968=AXIS2_PLACEMENT_3D('',#429411,#126929,#126930);
#103969=AXIS2_PLACEMENT_3D('',#429424,#126931,#126932);
#103970=AXIS2_PLACEMENT_3D('',#429437,#126933,#126934);
#103971=AXIS2_PLACEMENT_3D('',#429456,#126935,#126936);
#103972=AXIS2_PLACEMENT_3D('',#429469,#126937,#126938);
#103973=AXIS2_PLACEMENT_3D('',#429482,#126939,#126940);
#103974=AXIS2_PLACEMENT_3D('',#429483,#126941,#126942);
#103975=AXIS2_PLACEMENT_3D('',#429484,#126943,#126944);
#103976=AXIS2_PLACEMENT_3D('',#429497,#126945,#126946);
#103977=AXIS2_PLACEMENT_3D('',#429498,#126947,#126948);
#103978=AXIS2_PLACEMENT_3D('',#429505,#126951,#126952);
#103979=AXIS2_PLACEMENT_3D('',#429512,#126954,#126955);
#103980=AXIS2_PLACEMENT_3D('',#429515,#126956,#126957);
#103981=AXIS2_PLACEMENT_3D('',#429526,#126961,#126962);
#103982=AXIS2_PLACEMENT_3D('',#429594,#126963,#126964);
#103983=AXIS2_PLACEMENT_3D('',#429595,#126965,#126966);
#103984=AXIS2_PLACEMENT_3D('',#429637,#126967,#126968);
#103985=AXIS2_PLACEMENT_3D('',#429664,#126969,#126970);
#103986=AXIS2_PLACEMENT_3D('',#429745,#126971,#126972);
#103987=AXIS2_PLACEMENT_3D('',#429758,#126973,#126974);
#103988=AXIS2_PLACEMENT_3D('',#429759,#126975,#126976);
#103989=AXIS2_PLACEMENT_3D('',#429760,#126977,#126978);
#103990=AXIS2_PLACEMENT_3D('',#429773,#126979,#126980);
#103991=AXIS2_PLACEMENT_3D('',#429786,#126981,#126982);
#103992=AXIS2_PLACEMENT_3D('',#429805,#126983,#126984);
#103993=AXIS2_PLACEMENT_3D('',#429818,#126985,#126986);
#103994=AXIS2_PLACEMENT_3D('',#429831,#126987,#126988);
#103995=AXIS2_PLACEMENT_3D('',#429832,#126989,#126990);
#103996=AXIS2_PLACEMENT_3D('',#429833,#126991,#126992);
#103997=AXIS2_PLACEMENT_3D('',#429846,#126993,#126994);
#103998=AXIS2_PLACEMENT_3D('',#429847,#126995,#126996);
#103999=AXIS2_PLACEMENT_3D('',#429854,#126999,#127000);
#104000=AXIS2_PLACEMENT_3D('',#429861,#127002,#127003);
#104001=AXIS2_PLACEMENT_3D('',#429864,#127004,#127005);
#104002=AXIS2_PLACEMENT_3D('',#429875,#127009,#127010);
#104003=AXIS2_PLACEMENT_3D('',#429943,#127011,#127012);
#104004=AXIS2_PLACEMENT_3D('',#429944,#127013,#127014);
#104005=AXIS2_PLACEMENT_3D('',#429986,#127015,#127016);
#104006=AXIS2_PLACEMENT_3D('',#430013,#127017,#127018);
#104007=AXIS2_PLACEMENT_3D('',#430094,#127019,#127020);
#104008=AXIS2_PLACEMENT_3D('',#430107,#127021,#127022);
#104009=AXIS2_PLACEMENT_3D('',#430108,#127023,#127024);
#104010=AXIS2_PLACEMENT_3D('',#430109,#127025,#127026);
#104011=AXIS2_PLACEMENT_3D('',#430122,#127027,#127028);
#104012=AXIS2_PLACEMENT_3D('',#430135,#127029,#127030);
#104013=AXIS2_PLACEMENT_3D('',#430154,#127031,#127032);
#104014=AXIS2_PLACEMENT_3D('',#430167,#127033,#127034);
#104015=AXIS2_PLACEMENT_3D('',#430180,#127035,#127036);
#104016=AXIS2_PLACEMENT_3D('',#430181,#127037,#127038);
#104017=AXIS2_PLACEMENT_3D('',#430182,#127039,#127040);
#104018=AXIS2_PLACEMENT_3D('',#430195,#127041,#127042);
#104019=AXIS2_PLACEMENT_3D('',#430196,#127043,#127044);
#104020=AXIS2_PLACEMENT_3D('',#430203,#127047,#127048);
#104021=AXIS2_PLACEMENT_3D('',#430210,#127050,#127051);
#104022=AXIS2_PLACEMENT_3D('',#430213,#127052,#127053);
#104023=AXIS2_PLACEMENT_3D('',#430224,#127057,#127058);
#104024=AXIS2_PLACEMENT_3D('',#430292,#127059,#127060);
#104025=AXIS2_PLACEMENT_3D('',#430293,#127061,#127062);
#104026=AXIS2_PLACEMENT_3D('',#430335,#127063,#127064);
#104027=AXIS2_PLACEMENT_3D('',#430362,#127065,#127066);
#104028=AXIS2_PLACEMENT_3D('',#430443,#127067,#127068);
#104029=AXIS2_PLACEMENT_3D('',#430456,#127069,#127070);
#104030=AXIS2_PLACEMENT_3D('',#430457,#127071,#127072);
#104031=AXIS2_PLACEMENT_3D('',#430458,#127073,#127074);
#104032=AXIS2_PLACEMENT_3D('',#430471,#127075,#127076);
#104033=AXIS2_PLACEMENT_3D('',#430484,#127077,#127078);
#104034=AXIS2_PLACEMENT_3D('',#430503,#127079,#127080);
#104035=AXIS2_PLACEMENT_3D('',#430516,#127081,#127082);
#104036=AXIS2_PLACEMENT_3D('',#430529,#127083,#127084);
#104037=AXIS2_PLACEMENT_3D('',#430530,#127085,#127086);
#104038=AXIS2_PLACEMENT_3D('',#430531,#127087,#127088);
#104039=AXIS2_PLACEMENT_3D('',#430544,#127089,#127090);
#104040=AXIS2_PLACEMENT_3D('',#430545,#127091,#127092);
#104041=AXIS2_PLACEMENT_3D('',#430552,#127095,#127096);
#104042=AXIS2_PLACEMENT_3D('',#430559,#127098,#127099);
#104043=AXIS2_PLACEMENT_3D('',#430562,#127100,#127101);
#104044=AXIS2_PLACEMENT_3D('',#430573,#127105,#127106);
#104045=AXIS2_PLACEMENT_3D('',#430641,#127107,#127108);
#104046=AXIS2_PLACEMENT_3D('',#430642,#127109,#127110);
#104047=AXIS2_PLACEMENT_3D('',#430684,#127111,#127112);
#104048=AXIS2_PLACEMENT_3D('',#430711,#127113,#127114);
#104049=AXIS2_PLACEMENT_3D('',#430792,#127115,#127116);
#104050=AXIS2_PLACEMENT_3D('',#430805,#127117,#127118);
#104051=AXIS2_PLACEMENT_3D('',#430806,#127119,#127120);
#104052=AXIS2_PLACEMENT_3D('',#430807,#127121,#127122);
#104053=AXIS2_PLACEMENT_3D('',#430820,#127123,#127124);
#104054=AXIS2_PLACEMENT_3D('',#430833,#127125,#127126);
#104055=AXIS2_PLACEMENT_3D('',#430852,#127127,#127128);
#104056=AXIS2_PLACEMENT_3D('',#430865,#127129,#127130);
#104057=AXIS2_PLACEMENT_3D('',#430878,#127131,#127132);
#104058=AXIS2_PLACEMENT_3D('',#430879,#127133,#127134);
#104059=AXIS2_PLACEMENT_3D('',#430880,#127135,#127136);
#104060=AXIS2_PLACEMENT_3D('',#430893,#127137,#127138);
#104061=AXIS2_PLACEMENT_3D('',#430894,#127139,#127140);
#104062=AXIS2_PLACEMENT_3D('',#430901,#127143,#127144);
#104063=AXIS2_PLACEMENT_3D('',#430908,#127146,#127147);
#104064=AXIS2_PLACEMENT_3D('',#430911,#127148,#127149);
#104065=AXIS2_PLACEMENT_3D('',#430922,#127153,#127154);
#104066=AXIS2_PLACEMENT_3D('',#430990,#127155,#127156);
#104067=AXIS2_PLACEMENT_3D('',#430991,#127157,#127158);
#104068=AXIS2_PLACEMENT_3D('',#431033,#127159,#127160);
#104069=AXIS2_PLACEMENT_3D('',#431060,#127161,#127162);
#104070=AXIS2_PLACEMENT_3D('',#431141,#127163,#127164);
#104071=AXIS2_PLACEMENT_3D('',#431154,#127165,#127166);
#104072=AXIS2_PLACEMENT_3D('',#431155,#127167,#127168);
#104073=AXIS2_PLACEMENT_3D('',#431156,#127169,#127170);
#104074=AXIS2_PLACEMENT_3D('',#431169,#127171,#127172);
#104075=AXIS2_PLACEMENT_3D('',#431182,#127173,#127174);
#104076=AXIS2_PLACEMENT_3D('',#431201,#127175,#127176);
#104077=AXIS2_PLACEMENT_3D('',#431214,#127177,#127178);
#104078=AXIS2_PLACEMENT_3D('',#431227,#127179,#127180);
#104079=AXIS2_PLACEMENT_3D('',#431228,#127181,#127182);
#104080=AXIS2_PLACEMENT_3D('',#431229,#127183,#127184);
#104081=AXIS2_PLACEMENT_3D('',#431242,#127185,#127186);
#104082=AXIS2_PLACEMENT_3D('',#431243,#127187,#127188);
#104083=AXIS2_PLACEMENT_3D('',#431250,#127191,#127192);
#104084=AXIS2_PLACEMENT_3D('',#431257,#127194,#127195);
#104085=AXIS2_PLACEMENT_3D('',#431260,#127196,#127197);
#104086=AXIS2_PLACEMENT_3D('',#431271,#127201,#127202);
#104087=AXIS2_PLACEMENT_3D('',#431339,#127203,#127204);
#104088=AXIS2_PLACEMENT_3D('',#431340,#127205,#127206);
#104089=AXIS2_PLACEMENT_3D('',#431382,#127207,#127208);
#104090=AXIS2_PLACEMENT_3D('',#431409,#127209,#127210);
#104091=AXIS2_PLACEMENT_3D('',#431490,#127211,#127212);
#104092=AXIS2_PLACEMENT_3D('',#431503,#127213,#127214);
#104093=AXIS2_PLACEMENT_3D('',#431504,#127215,#127216);
#104094=AXIS2_PLACEMENT_3D('',#431505,#127217,#127218);
#104095=AXIS2_PLACEMENT_3D('',#431518,#127219,#127220);
#104096=AXIS2_PLACEMENT_3D('',#431531,#127221,#127222);
#104097=AXIS2_PLACEMENT_3D('',#431550,#127223,#127224);
#104098=AXIS2_PLACEMENT_3D('',#431563,#127225,#127226);
#104099=AXIS2_PLACEMENT_3D('',#431576,#127227,#127228);
#104100=AXIS2_PLACEMENT_3D('',#431577,#127229,#127230);
#104101=AXIS2_PLACEMENT_3D('',#431578,#127231,#127232);
#104102=AXIS2_PLACEMENT_3D('',#431591,#127233,#127234);
#104103=AXIS2_PLACEMENT_3D('',#431592,#127235,#127236);
#104104=AXIS2_PLACEMENT_3D('',#431599,#127239,#127240);
#104105=AXIS2_PLACEMENT_3D('',#431606,#127242,#127243);
#104106=AXIS2_PLACEMENT_3D('',#431609,#127244,#127245);
#104107=AXIS2_PLACEMENT_3D('',#431620,#127249,#127250);
#104108=AXIS2_PLACEMENT_3D('',#431688,#127251,#127252);
#104109=AXIS2_PLACEMENT_3D('',#431689,#127253,#127254);
#104110=AXIS2_PLACEMENT_3D('',#431731,#127255,#127256);
#104111=AXIS2_PLACEMENT_3D('',#431758,#127257,#127258);
#104112=AXIS2_PLACEMENT_3D('',#431839,#127259,#127260);
#104113=AXIS2_PLACEMENT_3D('',#431852,#127261,#127262);
#104114=AXIS2_PLACEMENT_3D('',#431853,#127263,#127264);
#104115=AXIS2_PLACEMENT_3D('',#431854,#127265,#127266);
#104116=AXIS2_PLACEMENT_3D('',#431867,#127267,#127268);
#104117=AXIS2_PLACEMENT_3D('',#431880,#127269,#127270);
#104118=AXIS2_PLACEMENT_3D('',#431899,#127271,#127272);
#104119=AXIS2_PLACEMENT_3D('',#431912,#127273,#127274);
#104120=AXIS2_PLACEMENT_3D('',#431925,#127275,#127276);
#104121=AXIS2_PLACEMENT_3D('',#431926,#127277,#127278);
#104122=AXIS2_PLACEMENT_3D('',#431927,#127279,#127280);
#104123=AXIS2_PLACEMENT_3D('',#431940,#127281,#127282);
#104124=AXIS2_PLACEMENT_3D('',#431941,#127283,#127284);
#104125=AXIS2_PLACEMENT_3D('',#431948,#127287,#127288);
#104126=AXIS2_PLACEMENT_3D('',#431955,#127290,#127291);
#104127=AXIS2_PLACEMENT_3D('',#431958,#127292,#127293);
#104128=AXIS2_PLACEMENT_3D('',#431969,#127297,#127298);
#104129=AXIS2_PLACEMENT_3D('',#432037,#127299,#127300);
#104130=AXIS2_PLACEMENT_3D('',#432038,#127301,#127302);
#104131=AXIS2_PLACEMENT_3D('',#432080,#127303,#127304);
#104132=AXIS2_PLACEMENT_3D('',#432107,#127305,#127306);
#104133=AXIS2_PLACEMENT_3D('',#432188,#127307,#127308);
#104134=AXIS2_PLACEMENT_3D('',#432201,#127309,#127310);
#104135=AXIS2_PLACEMENT_3D('',#432202,#127311,#127312);
#104136=AXIS2_PLACEMENT_3D('',#432203,#127313,#127314);
#104137=AXIS2_PLACEMENT_3D('',#432216,#127315,#127316);
#104138=AXIS2_PLACEMENT_3D('',#432229,#127317,#127318);
#104139=AXIS2_PLACEMENT_3D('',#432248,#127319,#127320);
#104140=AXIS2_PLACEMENT_3D('',#432261,#127321,#127322);
#104141=AXIS2_PLACEMENT_3D('',#432274,#127323,#127324);
#104142=AXIS2_PLACEMENT_3D('',#432275,#127325,#127326);
#104143=AXIS2_PLACEMENT_3D('',#432276,#127327,#127328);
#104144=AXIS2_PLACEMENT_3D('',#432289,#127329,#127330);
#104145=AXIS2_PLACEMENT_3D('',#432290,#127331,#127332);
#104146=AXIS2_PLACEMENT_3D('',#432297,#127335,#127336);
#104147=AXIS2_PLACEMENT_3D('',#432304,#127338,#127339);
#104148=AXIS2_PLACEMENT_3D('',#432307,#127340,#127341);
#104149=AXIS2_PLACEMENT_3D('',#432318,#127345,#127346);
#104150=AXIS2_PLACEMENT_3D('',#432386,#127347,#127348);
#104151=AXIS2_PLACEMENT_3D('',#432387,#127349,#127350);
#104152=AXIS2_PLACEMENT_3D('',#432429,#127351,#127352);
#104153=AXIS2_PLACEMENT_3D('',#432456,#127353,#127354);
#104154=AXIS2_PLACEMENT_3D('',#432537,#127355,#127356);
#104155=AXIS2_PLACEMENT_3D('',#432550,#127357,#127358);
#104156=AXIS2_PLACEMENT_3D('',#432551,#127359,#127360);
#104157=AXIS2_PLACEMENT_3D('',#432552,#127361,#127362);
#104158=AXIS2_PLACEMENT_3D('',#432565,#127363,#127364);
#104159=AXIS2_PLACEMENT_3D('',#432578,#127365,#127366);
#104160=AXIS2_PLACEMENT_3D('',#432597,#127367,#127368);
#104161=AXIS2_PLACEMENT_3D('',#432610,#127369,#127370);
#104162=AXIS2_PLACEMENT_3D('',#432623,#127371,#127372);
#104163=AXIS2_PLACEMENT_3D('',#432624,#127373,#127374);
#104164=AXIS2_PLACEMENT_3D('',#432625,#127375,#127376);
#104165=AXIS2_PLACEMENT_3D('',#432638,#127377,#127378);
#104166=AXIS2_PLACEMENT_3D('',#432639,#127379,#127380);
#104167=AXIS2_PLACEMENT_3D('',#432646,#127383,#127384);
#104168=AXIS2_PLACEMENT_3D('',#432653,#127386,#127387);
#104169=AXIS2_PLACEMENT_3D('',#432656,#127388,#127389);
#104170=AXIS2_PLACEMENT_3D('',#432667,#127393,#127394);
#104171=AXIS2_PLACEMENT_3D('',#432735,#127395,#127396);
#104172=AXIS2_PLACEMENT_3D('',#432736,#127397,#127398);
#104173=AXIS2_PLACEMENT_3D('',#432778,#127399,#127400);
#104174=AXIS2_PLACEMENT_3D('',#432805,#127401,#127402);
#104175=AXIS2_PLACEMENT_3D('',#432886,#127403,#127404);
#104176=AXIS2_PLACEMENT_3D('',#432899,#127405,#127406);
#104177=AXIS2_PLACEMENT_3D('',#432900,#127407,#127408);
#104178=AXIS2_PLACEMENT_3D('',#432901,#127409,#127410);
#104179=AXIS2_PLACEMENT_3D('',#432914,#127411,#127412);
#104180=AXIS2_PLACEMENT_3D('',#432927,#127413,#127414);
#104181=AXIS2_PLACEMENT_3D('',#432946,#127415,#127416);
#104182=AXIS2_PLACEMENT_3D('',#432959,#127417,#127418);
#104183=AXIS2_PLACEMENT_3D('',#432972,#127419,#127420);
#104184=AXIS2_PLACEMENT_3D('',#432973,#127421,#127422);
#104185=AXIS2_PLACEMENT_3D('',#432974,#127423,#127424);
#104186=AXIS2_PLACEMENT_3D('',#432987,#127425,#127426);
#104187=AXIS2_PLACEMENT_3D('',#432988,#127427,#127428);
#104188=AXIS2_PLACEMENT_3D('',#432995,#127431,#127432);
#104189=AXIS2_PLACEMENT_3D('',#433002,#127434,#127435);
#104190=AXIS2_PLACEMENT_3D('',#433005,#127436,#127437);
#104191=AXIS2_PLACEMENT_3D('',#433016,#127441,#127442);
#104192=AXIS2_PLACEMENT_3D('',#433084,#127443,#127444);
#104193=AXIS2_PLACEMENT_3D('',#433085,#127445,#127446);
#104194=AXIS2_PLACEMENT_3D('',#433127,#127447,#127448);
#104195=AXIS2_PLACEMENT_3D('',#433154,#127449,#127450);
#104196=AXIS2_PLACEMENT_3D('',#433235,#127451,#127452);
#104197=AXIS2_PLACEMENT_3D('',#433248,#127453,#127454);
#104198=AXIS2_PLACEMENT_3D('',#433249,#127455,#127456);
#104199=AXIS2_PLACEMENT_3D('',#433250,#127457,#127458);
#104200=AXIS2_PLACEMENT_3D('',#433263,#127459,#127460);
#104201=AXIS2_PLACEMENT_3D('',#433276,#127461,#127462);
#104202=AXIS2_PLACEMENT_3D('',#433295,#127463,#127464);
#104203=AXIS2_PLACEMENT_3D('',#433308,#127465,#127466);
#104204=AXIS2_PLACEMENT_3D('',#433321,#127467,#127468);
#104205=AXIS2_PLACEMENT_3D('',#433322,#127469,#127470);
#104206=AXIS2_PLACEMENT_3D('',#433323,#127471,#127472);
#104207=AXIS2_PLACEMENT_3D('',#433336,#127473,#127474);
#104208=AXIS2_PLACEMENT_3D('',#433337,#127475,#127476);
#104209=AXIS2_PLACEMENT_3D('',#433344,#127479,#127480);
#104210=AXIS2_PLACEMENT_3D('',#433351,#127482,#127483);
#104211=AXIS2_PLACEMENT_3D('',#433354,#127484,#127485);
#104212=AXIS2_PLACEMENT_3D('',#433365,#127489,#127490);
#104213=AXIS2_PLACEMENT_3D('',#433433,#127491,#127492);
#104214=AXIS2_PLACEMENT_3D('',#433434,#127493,#127494);
#104215=AXIS2_PLACEMENT_3D('',#433476,#127495,#127496);
#104216=AXIS2_PLACEMENT_3D('',#433503,#127497,#127498);
#104217=AXIS2_PLACEMENT_3D('',#433584,#127499,#127500);
#104218=AXIS2_PLACEMENT_3D('',#433597,#127501,#127502);
#104219=AXIS2_PLACEMENT_3D('',#433598,#127503,#127504);
#104220=AXIS2_PLACEMENT_3D('',#433599,#127505,#127506);
#104221=AXIS2_PLACEMENT_3D('',#433612,#127507,#127508);
#104222=AXIS2_PLACEMENT_3D('',#433625,#127509,#127510);
#104223=AXIS2_PLACEMENT_3D('',#433644,#127511,#127512);
#104224=AXIS2_PLACEMENT_3D('',#433657,#127513,#127514);
#104225=AXIS2_PLACEMENT_3D('',#433670,#127515,#127516);
#104226=AXIS2_PLACEMENT_3D('',#433671,#127517,#127518);
#104227=AXIS2_PLACEMENT_3D('',#433672,#127519,#127520);
#104228=AXIS2_PLACEMENT_3D('',#433685,#127521,#127522);
#104229=AXIS2_PLACEMENT_3D('',#433686,#127523,#127524);
#104230=AXIS2_PLACEMENT_3D('',#433693,#127527,#127528);
#104231=AXIS2_PLACEMENT_3D('',#433700,#127530,#127531);
#104232=AXIS2_PLACEMENT_3D('',#433703,#127532,#127533);
#104233=AXIS2_PLACEMENT_3D('',#433714,#127537,#127538);
#104234=AXIS2_PLACEMENT_3D('',#433782,#127539,#127540);
#104235=AXIS2_PLACEMENT_3D('',#433783,#127541,#127542);
#104236=AXIS2_PLACEMENT_3D('',#433825,#127543,#127544);
#104237=AXIS2_PLACEMENT_3D('',#433852,#127545,#127546);
#104238=AXIS2_PLACEMENT_3D('',#433933,#127547,#127548);
#104239=AXIS2_PLACEMENT_3D('',#433946,#127549,#127550);
#104240=AXIS2_PLACEMENT_3D('',#433947,#127551,#127552);
#104241=AXIS2_PLACEMENT_3D('',#433948,#127553,#127554);
#104242=AXIS2_PLACEMENT_3D('',#433961,#127555,#127556);
#104243=AXIS2_PLACEMENT_3D('',#433974,#127557,#127558);
#104244=AXIS2_PLACEMENT_3D('',#433993,#127559,#127560);
#104245=AXIS2_PLACEMENT_3D('',#434006,#127561,#127562);
#104246=AXIS2_PLACEMENT_3D('',#434019,#127563,#127564);
#104247=AXIS2_PLACEMENT_3D('',#434020,#127565,#127566);
#104248=AXIS2_PLACEMENT_3D('',#434021,#127567,#127568);
#104249=AXIS2_PLACEMENT_3D('',#434034,#127569,#127570);
#104250=AXIS2_PLACEMENT_3D('',#434035,#127571,#127572);
#104251=AXIS2_PLACEMENT_3D('',#434042,#127575,#127576);
#104252=AXIS2_PLACEMENT_3D('',#434049,#127578,#127579);
#104253=AXIS2_PLACEMENT_3D('',#434052,#127580,#127581);
#104254=AXIS2_PLACEMENT_3D('',#434063,#127585,#127586);
#104255=AXIS2_PLACEMENT_3D('',#434131,#127587,#127588);
#104256=AXIS2_PLACEMENT_3D('',#434132,#127589,#127590);
#104257=AXIS2_PLACEMENT_3D('',#434174,#127591,#127592);
#104258=AXIS2_PLACEMENT_3D('',#434201,#127593,#127594);
#104259=AXIS2_PLACEMENT_3D('',#434282,#127595,#127596);
#104260=AXIS2_PLACEMENT_3D('',#434295,#127597,#127598);
#104261=AXIS2_PLACEMENT_3D('',#434296,#127599,#127600);
#104262=AXIS2_PLACEMENT_3D('',#434297,#127601,#127602);
#104263=AXIS2_PLACEMENT_3D('',#434310,#127603,#127604);
#104264=AXIS2_PLACEMENT_3D('',#434323,#127605,#127606);
#104265=AXIS2_PLACEMENT_3D('',#434342,#127607,#127608);
#104266=AXIS2_PLACEMENT_3D('',#434355,#127609,#127610);
#104267=AXIS2_PLACEMENT_3D('',#434368,#127611,#127612);
#104268=AXIS2_PLACEMENT_3D('',#434369,#127613,#127614);
#104269=AXIS2_PLACEMENT_3D('',#434370,#127615,#127616);
#104270=AXIS2_PLACEMENT_3D('',#434383,#127617,#127618);
#104271=AXIS2_PLACEMENT_3D('',#434384,#127619,#127620);
#104272=AXIS2_PLACEMENT_3D('',#434391,#127623,#127624);
#104273=AXIS2_PLACEMENT_3D('',#434398,#127626,#127627);
#104274=AXIS2_PLACEMENT_3D('',#434401,#127628,#127629);
#104275=AXIS2_PLACEMENT_3D('',#434412,#127633,#127634);
#104276=AXIS2_PLACEMENT_3D('',#434480,#127635,#127636);
#104277=AXIS2_PLACEMENT_3D('',#434481,#127637,#127638);
#104278=AXIS2_PLACEMENT_3D('',#434523,#127639,#127640);
#104279=AXIS2_PLACEMENT_3D('',#434550,#127641,#127642);
#104280=AXIS2_PLACEMENT_3D('',#434631,#127643,#127644);
#104281=AXIS2_PLACEMENT_3D('',#434644,#127645,#127646);
#104282=AXIS2_PLACEMENT_3D('',#434645,#127647,#127648);
#104283=AXIS2_PLACEMENT_3D('',#434646,#127649,#127650);
#104284=AXIS2_PLACEMENT_3D('',#434659,#127651,#127652);
#104285=AXIS2_PLACEMENT_3D('',#434672,#127653,#127654);
#104286=AXIS2_PLACEMENT_3D('',#434691,#127655,#127656);
#104287=AXIS2_PLACEMENT_3D('',#434704,#127657,#127658);
#104288=AXIS2_PLACEMENT_3D('',#434717,#127659,#127660);
#104289=AXIS2_PLACEMENT_3D('',#434718,#127661,#127662);
#104290=AXIS2_PLACEMENT_3D('',#434719,#127663,#127664);
#104291=AXIS2_PLACEMENT_3D('',#434732,#127665,#127666);
#104292=AXIS2_PLACEMENT_3D('',#434733,#127667,#127668);
#104293=AXIS2_PLACEMENT_3D('',#434740,#127671,#127672);
#104294=AXIS2_PLACEMENT_3D('',#434747,#127674,#127675);
#104295=AXIS2_PLACEMENT_3D('',#434750,#127676,#127677);
#104296=AXIS2_PLACEMENT_3D('',#434761,#127681,#127682);
#104297=AXIS2_PLACEMENT_3D('',#434829,#127683,#127684);
#104298=AXIS2_PLACEMENT_3D('',#434830,#127685,#127686);
#104299=AXIS2_PLACEMENT_3D('',#434872,#127687,#127688);
#104300=AXIS2_PLACEMENT_3D('',#434899,#127689,#127690);
#104301=AXIS2_PLACEMENT_3D('',#434980,#127691,#127692);
#104302=AXIS2_PLACEMENT_3D('',#434993,#127693,#127694);
#104303=AXIS2_PLACEMENT_3D('',#434994,#127695,#127696);
#104304=AXIS2_PLACEMENT_3D('',#434995,#127697,#127698);
#104305=AXIS2_PLACEMENT_3D('',#435008,#127699,#127700);
#104306=AXIS2_PLACEMENT_3D('',#435021,#127701,#127702);
#104307=AXIS2_PLACEMENT_3D('',#435040,#127703,#127704);
#104308=AXIS2_PLACEMENT_3D('',#435053,#127705,#127706);
#104309=AXIS2_PLACEMENT_3D('',#435066,#127707,#127708);
#104310=AXIS2_PLACEMENT_3D('',#435067,#127709,#127710);
#104311=AXIS2_PLACEMENT_3D('',#435068,#127711,#127712);
#104312=AXIS2_PLACEMENT_3D('',#435081,#127713,#127714);
#104313=AXIS2_PLACEMENT_3D('',#435082,#127715,#127716);
#104314=AXIS2_PLACEMENT_3D('',#435089,#127719,#127720);
#104315=AXIS2_PLACEMENT_3D('',#435096,#127722,#127723);
#104316=AXIS2_PLACEMENT_3D('',#435099,#127724,#127725);
#104317=AXIS2_PLACEMENT_3D('',#435110,#127729,#127730);
#104318=AXIS2_PLACEMENT_3D('',#435178,#127731,#127732);
#104319=AXIS2_PLACEMENT_3D('',#435179,#127733,#127734);
#104320=AXIS2_PLACEMENT_3D('',#435221,#127735,#127736);
#104321=AXIS2_PLACEMENT_3D('',#435248,#127737,#127738);
#104322=AXIS2_PLACEMENT_3D('',#435329,#127739,#127740);
#104323=AXIS2_PLACEMENT_3D('',#435342,#127741,#127742);
#104324=AXIS2_PLACEMENT_3D('',#435343,#127743,#127744);
#104325=AXIS2_PLACEMENT_3D('',#435344,#127745,#127746);
#104326=AXIS2_PLACEMENT_3D('',#435357,#127747,#127748);
#104327=AXIS2_PLACEMENT_3D('',#435370,#127749,#127750);
#104328=AXIS2_PLACEMENT_3D('',#435389,#127751,#127752);
#104329=AXIS2_PLACEMENT_3D('',#435402,#127753,#127754);
#104330=AXIS2_PLACEMENT_3D('',#435415,#127755,#127756);
#104331=AXIS2_PLACEMENT_3D('',#435416,#127757,#127758);
#104332=AXIS2_PLACEMENT_3D('',#435417,#127759,#127760);
#104333=AXIS2_PLACEMENT_3D('',#435430,#127761,#127762);
#104334=AXIS2_PLACEMENT_3D('',#435431,#127763,#127764);
#104335=AXIS2_PLACEMENT_3D('',#435438,#127767,#127768);
#104336=AXIS2_PLACEMENT_3D('',#435445,#127770,#127771);
#104337=AXIS2_PLACEMENT_3D('',#435448,#127772,#127773);
#104338=AXIS2_PLACEMENT_3D('',#435459,#127777,#127778);
#104339=AXIS2_PLACEMENT_3D('',#435527,#127779,#127780);
#104340=AXIS2_PLACEMENT_3D('',#435528,#127781,#127782);
#104341=AXIS2_PLACEMENT_3D('',#435570,#127783,#127784);
#104342=AXIS2_PLACEMENT_3D('',#435597,#127785,#127786);
#104343=AXIS2_PLACEMENT_3D('',#435678,#127787,#127788);
#104344=AXIS2_PLACEMENT_3D('',#435691,#127789,#127790);
#104345=AXIS2_PLACEMENT_3D('',#435692,#127791,#127792);
#104346=AXIS2_PLACEMENT_3D('',#435693,#127793,#127794);
#104347=AXIS2_PLACEMENT_3D('',#435706,#127795,#127796);
#104348=AXIS2_PLACEMENT_3D('',#435719,#127797,#127798);
#104349=AXIS2_PLACEMENT_3D('',#435738,#127799,#127800);
#104350=AXIS2_PLACEMENT_3D('',#435751,#127801,#127802);
#104351=AXIS2_PLACEMENT_3D('',#435764,#127803,#127804);
#104352=AXIS2_PLACEMENT_3D('',#435765,#127805,#127806);
#104353=AXIS2_PLACEMENT_3D('',#435766,#127807,#127808);
#104354=AXIS2_PLACEMENT_3D('',#435779,#127809,#127810);
#104355=AXIS2_PLACEMENT_3D('',#435780,#127811,#127812);
#104356=AXIS2_PLACEMENT_3D('',#435787,#127815,#127816);
#104357=AXIS2_PLACEMENT_3D('',#435794,#127818,#127819);
#104358=AXIS2_PLACEMENT_3D('',#435797,#127820,#127821);
#104359=AXIS2_PLACEMENT_3D('',#435808,#127825,#127826);
#104360=AXIS2_PLACEMENT_3D('',#435876,#127827,#127828);
#104361=AXIS2_PLACEMENT_3D('',#435877,#127829,#127830);
#104362=AXIS2_PLACEMENT_3D('',#435919,#127831,#127832);
#104363=AXIS2_PLACEMENT_3D('',#435946,#127833,#127834);
#104364=AXIS2_PLACEMENT_3D('',#436027,#127835,#127836);
#104365=AXIS2_PLACEMENT_3D('',#436040,#127837,#127838);
#104366=AXIS2_PLACEMENT_3D('',#436041,#127839,#127840);
#104367=AXIS2_PLACEMENT_3D('',#436042,#127841,#127842);
#104368=AXIS2_PLACEMENT_3D('',#436055,#127843,#127844);
#104369=AXIS2_PLACEMENT_3D('',#436068,#127845,#127846);
#104370=AXIS2_PLACEMENT_3D('',#436087,#127847,#127848);
#104371=AXIS2_PLACEMENT_3D('',#436100,#127849,#127850);
#104372=AXIS2_PLACEMENT_3D('',#436113,#127851,#127852);
#104373=AXIS2_PLACEMENT_3D('',#436114,#127853,#127854);
#104374=AXIS2_PLACEMENT_3D('',#436115,#127855,#127856);
#104375=AXIS2_PLACEMENT_3D('',#436128,#127857,#127858);
#104376=AXIS2_PLACEMENT_3D('',#436129,#127859,#127860);
#104377=AXIS2_PLACEMENT_3D('',#436136,#127863,#127864);
#104378=AXIS2_PLACEMENT_3D('',#436143,#127866,#127867);
#104379=AXIS2_PLACEMENT_3D('',#436146,#127868,#127869);
#104380=AXIS2_PLACEMENT_3D('',#436157,#127873,#127874);
#104381=AXIS2_PLACEMENT_3D('',#436225,#127875,#127876);
#104382=AXIS2_PLACEMENT_3D('',#436226,#127877,#127878);
#104383=AXIS2_PLACEMENT_3D('',#436268,#127879,#127880);
#104384=AXIS2_PLACEMENT_3D('',#436295,#127881,#127882);
#104385=AXIS2_PLACEMENT_3D('',#436376,#127883,#127884);
#104386=AXIS2_PLACEMENT_3D('',#436389,#127885,#127886);
#104387=AXIS2_PLACEMENT_3D('',#436390,#127887,#127888);
#104388=AXIS2_PLACEMENT_3D('',#436391,#127889,#127890);
#104389=AXIS2_PLACEMENT_3D('',#436404,#127891,#127892);
#104390=AXIS2_PLACEMENT_3D('',#436417,#127893,#127894);
#104391=AXIS2_PLACEMENT_3D('',#436436,#127895,#127896);
#104392=AXIS2_PLACEMENT_3D('',#436449,#127897,#127898);
#104393=AXIS2_PLACEMENT_3D('',#436462,#127899,#127900);
#104394=AXIS2_PLACEMENT_3D('',#436463,#127901,#127902);
#104395=AXIS2_PLACEMENT_3D('',#436464,#127903,#127904);
#104396=AXIS2_PLACEMENT_3D('',#436477,#127905,#127906);
#104397=AXIS2_PLACEMENT_3D('',#436478,#127907,#127908);
#104398=AXIS2_PLACEMENT_3D('',#436485,#127911,#127912);
#104399=AXIS2_PLACEMENT_3D('',#436492,#127914,#127915);
#104400=AXIS2_PLACEMENT_3D('',#436495,#127916,#127917);
#104401=AXIS2_PLACEMENT_3D('',#436506,#127921,#127922);
#104402=AXIS2_PLACEMENT_3D('',#436574,#127923,#127924);
#104403=AXIS2_PLACEMENT_3D('',#436575,#127925,#127926);
#104404=AXIS2_PLACEMENT_3D('',#436617,#127927,#127928);
#104405=AXIS2_PLACEMENT_3D('',#436644,#127929,#127930);
#104406=AXIS2_PLACEMENT_3D('',#436725,#127931,#127932);
#104407=AXIS2_PLACEMENT_3D('',#436738,#127933,#127934);
#104408=AXIS2_PLACEMENT_3D('',#436739,#127935,#127936);
#104409=AXIS2_PLACEMENT_3D('',#436740,#127937,#127938);
#104410=AXIS2_PLACEMENT_3D('',#436753,#127939,#127940);
#104411=AXIS2_PLACEMENT_3D('',#436766,#127941,#127942);
#104412=AXIS2_PLACEMENT_3D('',#436785,#127943,#127944);
#104413=AXIS2_PLACEMENT_3D('',#436798,#127945,#127946);
#104414=AXIS2_PLACEMENT_3D('',#436811,#127947,#127948);
#104415=AXIS2_PLACEMENT_3D('',#436812,#127949,#127950);
#104416=AXIS2_PLACEMENT_3D('',#436813,#127951,#127952);
#104417=AXIS2_PLACEMENT_3D('',#436826,#127953,#127954);
#104418=AXIS2_PLACEMENT_3D('',#436827,#127955,#127956);
#104419=AXIS2_PLACEMENT_3D('',#436834,#127959,#127960);
#104420=AXIS2_PLACEMENT_3D('',#436841,#127962,#127963);
#104421=AXIS2_PLACEMENT_3D('',#436844,#127964,#127965);
#104422=AXIS2_PLACEMENT_3D('',#436855,#127969,#127970);
#104423=AXIS2_PLACEMENT_3D('',#436923,#127971,#127972);
#104424=AXIS2_PLACEMENT_3D('',#436924,#127973,#127974);
#104425=AXIS2_PLACEMENT_3D('',#436966,#127975,#127976);
#104426=AXIS2_PLACEMENT_3D('',#436993,#127977,#127978);
#104427=AXIS2_PLACEMENT_3D('',#437074,#127979,#127980);
#104428=AXIS2_PLACEMENT_3D('',#437087,#127981,#127982);
#104429=AXIS2_PLACEMENT_3D('',#437088,#127983,#127984);
#104430=AXIS2_PLACEMENT_3D('',#437089,#127985,#127986);
#104431=AXIS2_PLACEMENT_3D('',#437102,#127987,#127988);
#104432=AXIS2_PLACEMENT_3D('',#437115,#127989,#127990);
#104433=AXIS2_PLACEMENT_3D('',#437134,#127991,#127992);
#104434=AXIS2_PLACEMENT_3D('',#437147,#127993,#127994);
#104435=AXIS2_PLACEMENT_3D('',#437160,#127995,#127996);
#104436=AXIS2_PLACEMENT_3D('',#437161,#127997,#127998);
#104437=AXIS2_PLACEMENT_3D('',#437162,#127999,#128000);
#104438=AXIS2_PLACEMENT_3D('',#437175,#128001,#128002);
#104439=AXIS2_PLACEMENT_3D('',#437176,#128003,#128004);
#104440=AXIS2_PLACEMENT_3D('',#437183,#128007,#128008);
#104441=AXIS2_PLACEMENT_3D('',#437190,#128010,#128011);
#104442=AXIS2_PLACEMENT_3D('',#437193,#128012,#128013);
#104443=AXIS2_PLACEMENT_3D('',#437204,#128017,#128018);
#104444=AXIS2_PLACEMENT_3D('',#437272,#128019,#128020);
#104445=AXIS2_PLACEMENT_3D('',#437273,#128021,#128022);
#104446=AXIS2_PLACEMENT_3D('',#437315,#128023,#128024);
#104447=AXIS2_PLACEMENT_3D('',#437342,#128025,#128026);
#104448=AXIS2_PLACEMENT_3D('',#437423,#128027,#128028);
#104449=AXIS2_PLACEMENT_3D('',#437436,#128029,#128030);
#104450=AXIS2_PLACEMENT_3D('',#437437,#128031,#128032);
#104451=AXIS2_PLACEMENT_3D('',#437438,#128033,#128034);
#104452=AXIS2_PLACEMENT_3D('',#437451,#128035,#128036);
#104453=AXIS2_PLACEMENT_3D('',#437464,#128037,#128038);
#104454=AXIS2_PLACEMENT_3D('',#437483,#128039,#128040);
#104455=AXIS2_PLACEMENT_3D('',#437496,#128041,#128042);
#104456=AXIS2_PLACEMENT_3D('',#437509,#128043,#128044);
#104457=AXIS2_PLACEMENT_3D('',#437510,#128045,#128046);
#104458=AXIS2_PLACEMENT_3D('',#437511,#128047,#128048);
#104459=AXIS2_PLACEMENT_3D('',#437524,#128049,#128050);
#104460=AXIS2_PLACEMENT_3D('',#437525,#128051,#128052);
#104461=AXIS2_PLACEMENT_3D('',#437532,#128055,#128056);
#104462=AXIS2_PLACEMENT_3D('',#437539,#128058,#128059);
#104463=AXIS2_PLACEMENT_3D('',#437542,#128060,#128061);
#104464=AXIS2_PLACEMENT_3D('',#437553,#128065,#128066);
#104465=AXIS2_PLACEMENT_3D('',#437621,#128067,#128068);
#104466=AXIS2_PLACEMENT_3D('',#437622,#128069,#128070);
#104467=AXIS2_PLACEMENT_3D('',#437664,#128071,#128072);
#104468=AXIS2_PLACEMENT_3D('',#437691,#128073,#128074);
#104469=AXIS2_PLACEMENT_3D('',#437772,#128075,#128076);
#104470=AXIS2_PLACEMENT_3D('',#437785,#128077,#128078);
#104471=AXIS2_PLACEMENT_3D('',#437786,#128079,#128080);
#104472=AXIS2_PLACEMENT_3D('',#437787,#128081,#128082);
#104473=AXIS2_PLACEMENT_3D('',#437800,#128083,#128084);
#104474=AXIS2_PLACEMENT_3D('',#437813,#128085,#128086);
#104475=AXIS2_PLACEMENT_3D('',#437832,#128087,#128088);
#104476=AXIS2_PLACEMENT_3D('',#437845,#128089,#128090);
#104477=AXIS2_PLACEMENT_3D('',#437858,#128091,#128092);
#104478=AXIS2_PLACEMENT_3D('',#437859,#128093,#128094);
#104479=AXIS2_PLACEMENT_3D('',#437860,#128095,#128096);
#104480=AXIS2_PLACEMENT_3D('',#437873,#128097,#128098);
#104481=AXIS2_PLACEMENT_3D('',#437874,#128099,#128100);
#104482=AXIS2_PLACEMENT_3D('',#437881,#128103,#128104);
#104483=AXIS2_PLACEMENT_3D('',#437888,#128106,#128107);
#104484=AXIS2_PLACEMENT_3D('',#437891,#128108,#128109);
#104485=AXIS2_PLACEMENT_3D('',#437902,#128113,#128114);
#104486=AXIS2_PLACEMENT_3D('',#437970,#128115,#128116);
#104487=AXIS2_PLACEMENT_3D('',#437971,#128117,#128118);
#104488=AXIS2_PLACEMENT_3D('',#438013,#128119,#128120);
#104489=AXIS2_PLACEMENT_3D('',#438040,#128121,#128122);
#104490=AXIS2_PLACEMENT_3D('',#438121,#128123,#128124);
#104491=AXIS2_PLACEMENT_3D('',#438134,#128125,#128126);
#104492=AXIS2_PLACEMENT_3D('',#438135,#128127,#128128);
#104493=AXIS2_PLACEMENT_3D('',#438136,#128129,#128130);
#104494=AXIS2_PLACEMENT_3D('',#438149,#128131,#128132);
#104495=AXIS2_PLACEMENT_3D('',#438162,#128133,#128134);
#104496=AXIS2_PLACEMENT_3D('',#438181,#128135,#128136);
#104497=AXIS2_PLACEMENT_3D('',#438194,#128137,#128138);
#104498=AXIS2_PLACEMENT_3D('',#438207,#128139,#128140);
#104499=AXIS2_PLACEMENT_3D('',#438208,#128141,#128142);
#104500=AXIS2_PLACEMENT_3D('',#438209,#128143,#128144);
#104501=AXIS2_PLACEMENT_3D('',#438222,#128145,#128146);
#104502=AXIS2_PLACEMENT_3D('',#438223,#128147,#128148);
#104503=AXIS2_PLACEMENT_3D('',#438230,#128151,#128152);
#104504=AXIS2_PLACEMENT_3D('',#438237,#128154,#128155);
#104505=AXIS2_PLACEMENT_3D('',#438240,#128156,#128157);
#104506=AXIS2_PLACEMENT_3D('',#438251,#128161,#128162);
#104507=AXIS2_PLACEMENT_3D('',#438319,#128163,#128164);
#104508=AXIS2_PLACEMENT_3D('',#438320,#128165,#128166);
#104509=AXIS2_PLACEMENT_3D('',#438362,#128167,#128168);
#104510=AXIS2_PLACEMENT_3D('',#438389,#128169,#128170);
#104511=AXIS2_PLACEMENT_3D('',#438470,#128171,#128172);
#104512=AXIS2_PLACEMENT_3D('',#438483,#128173,#128174);
#104513=AXIS2_PLACEMENT_3D('',#438484,#128175,#128176);
#104514=AXIS2_PLACEMENT_3D('',#438485,#128177,#128178);
#104515=AXIS2_PLACEMENT_3D('',#438498,#128179,#128180);
#104516=AXIS2_PLACEMENT_3D('',#438511,#128181,#128182);
#104517=AXIS2_PLACEMENT_3D('',#438530,#128183,#128184);
#104518=AXIS2_PLACEMENT_3D('',#438543,#128185,#128186);
#104519=AXIS2_PLACEMENT_3D('',#438556,#128187,#128188);
#104520=AXIS2_PLACEMENT_3D('',#438557,#128189,#128190);
#104521=AXIS2_PLACEMENT_3D('',#438558,#128191,#128192);
#104522=AXIS2_PLACEMENT_3D('',#438571,#128193,#128194);
#104523=AXIS2_PLACEMENT_3D('',#438572,#128195,#128196);
#104524=AXIS2_PLACEMENT_3D('',#438579,#128199,#128200);
#104525=AXIS2_PLACEMENT_3D('',#438586,#128202,#128203);
#104526=AXIS2_PLACEMENT_3D('',#438589,#128204,#128205);
#104527=AXIS2_PLACEMENT_3D('',#438600,#128209,#128210);
#104528=AXIS2_PLACEMENT_3D('',#438668,#128211,#128212);
#104529=AXIS2_PLACEMENT_3D('',#438669,#128213,#128214);
#104530=AXIS2_PLACEMENT_3D('',#438711,#128215,#128216);
#104531=AXIS2_PLACEMENT_3D('',#438738,#128217,#128218);
#104532=AXIS2_PLACEMENT_3D('',#438819,#128219,#128220);
#104533=AXIS2_PLACEMENT_3D('',#438832,#128221,#128222);
#104534=AXIS2_PLACEMENT_3D('',#438833,#128223,#128224);
#104535=AXIS2_PLACEMENT_3D('',#438834,#128225,#128226);
#104536=AXIS2_PLACEMENT_3D('',#438847,#128227,#128228);
#104537=AXIS2_PLACEMENT_3D('',#438860,#128229,#128230);
#104538=AXIS2_PLACEMENT_3D('',#438879,#128231,#128232);
#104539=AXIS2_PLACEMENT_3D('',#438892,#128233,#128234);
#104540=AXIS2_PLACEMENT_3D('',#438905,#128235,#128236);
#104541=AXIS2_PLACEMENT_3D('',#438906,#128237,#128238);
#104542=AXIS2_PLACEMENT_3D('',#438907,#128239,#128240);
#104543=AXIS2_PLACEMENT_3D('',#438920,#128241,#128242);
#104544=AXIS2_PLACEMENT_3D('',#438921,#128243,#128244);
#104545=AXIS2_PLACEMENT_3D('',#438928,#128247,#128248);
#104546=AXIS2_PLACEMENT_3D('',#438935,#128250,#128251);
#104547=AXIS2_PLACEMENT_3D('',#438938,#128252,#128253);
#104548=AXIS2_PLACEMENT_3D('',#438949,#128257,#128258);
#104549=AXIS2_PLACEMENT_3D('',#439017,#128259,#128260);
#104550=AXIS2_PLACEMENT_3D('',#439018,#128261,#128262);
#104551=AXIS2_PLACEMENT_3D('',#439060,#128263,#128264);
#104552=AXIS2_PLACEMENT_3D('',#439087,#128265,#128266);
#104553=AXIS2_PLACEMENT_3D('',#439168,#128267,#128268);
#104554=AXIS2_PLACEMENT_3D('',#439181,#128269,#128270);
#104555=AXIS2_PLACEMENT_3D('',#439182,#128271,#128272);
#104556=AXIS2_PLACEMENT_3D('',#439183,#128273,#128274);
#104557=AXIS2_PLACEMENT_3D('',#439196,#128275,#128276);
#104558=AXIS2_PLACEMENT_3D('',#439209,#128277,#128278);
#104559=AXIS2_PLACEMENT_3D('',#439228,#128279,#128280);
#104560=AXIS2_PLACEMENT_3D('',#439241,#128281,#128282);
#104561=AXIS2_PLACEMENT_3D('',#439254,#128283,#128284);
#104562=AXIS2_PLACEMENT_3D('',#439255,#128285,#128286);
#104563=AXIS2_PLACEMENT_3D('',#439256,#128287,#128288);
#104564=AXIS2_PLACEMENT_3D('',#439269,#128289,#128290);
#104565=AXIS2_PLACEMENT_3D('',#439270,#128291,#128292);
#104566=AXIS2_PLACEMENT_3D('',#439277,#128295,#128296);
#104567=AXIS2_PLACEMENT_3D('',#439284,#128298,#128299);
#104568=AXIS2_PLACEMENT_3D('',#439287,#128300,#128301);
#104569=AXIS2_PLACEMENT_3D('',#439298,#128305,#128306);
#104570=AXIS2_PLACEMENT_3D('',#439366,#128307,#128308);
#104571=AXIS2_PLACEMENT_3D('',#439367,#128309,#128310);
#104572=AXIS2_PLACEMENT_3D('',#439409,#128311,#128312);
#104573=AXIS2_PLACEMENT_3D('',#439436,#128313,#128314);
#104574=AXIS2_PLACEMENT_3D('',#439517,#128315,#128316);
#104575=AXIS2_PLACEMENT_3D('',#439530,#128317,#128318);
#104576=AXIS2_PLACEMENT_3D('',#439531,#128319,#128320);
#104577=AXIS2_PLACEMENT_3D('',#439532,#128321,#128322);
#104578=AXIS2_PLACEMENT_3D('',#439545,#128323,#128324);
#104579=AXIS2_PLACEMENT_3D('',#439558,#128325,#128326);
#104580=AXIS2_PLACEMENT_3D('',#439577,#128327,#128328);
#104581=AXIS2_PLACEMENT_3D('',#439590,#128329,#128330);
#104582=AXIS2_PLACEMENT_3D('',#439603,#128331,#128332);
#104583=AXIS2_PLACEMENT_3D('',#439604,#128333,#128334);
#104584=AXIS2_PLACEMENT_3D('',#439605,#128335,#128336);
#104585=AXIS2_PLACEMENT_3D('',#439618,#128337,#128338);
#104586=AXIS2_PLACEMENT_3D('',#439619,#128339,#128340);
#104587=AXIS2_PLACEMENT_3D('',#439626,#128343,#128344);
#104588=AXIS2_PLACEMENT_3D('',#439633,#128346,#128347);
#104589=AXIS2_PLACEMENT_3D('',#439636,#128348,#128349);
#104590=AXIS2_PLACEMENT_3D('',#439647,#128353,#128354);
#104591=AXIS2_PLACEMENT_3D('',#439715,#128355,#128356);
#104592=AXIS2_PLACEMENT_3D('',#439716,#128357,#128358);
#104593=AXIS2_PLACEMENT_3D('',#439758,#128359,#128360);
#104594=AXIS2_PLACEMENT_3D('',#439785,#128361,#128362);
#104595=AXIS2_PLACEMENT_3D('',#439866,#128363,#128364);
#104596=AXIS2_PLACEMENT_3D('',#439879,#128365,#128366);
#104597=AXIS2_PLACEMENT_3D('',#439880,#128367,#128368);
#104598=AXIS2_PLACEMENT_3D('',#439881,#128369,#128370);
#104599=AXIS2_PLACEMENT_3D('',#439894,#128371,#128372);
#104600=AXIS2_PLACEMENT_3D('',#439907,#128373,#128374);
#104601=AXIS2_PLACEMENT_3D('',#439926,#128375,#128376);
#104602=AXIS2_PLACEMENT_3D('',#439939,#128377,#128378);
#104603=AXIS2_PLACEMENT_3D('',#439952,#128379,#128380);
#104604=AXIS2_PLACEMENT_3D('',#439953,#128381,#128382);
#104605=AXIS2_PLACEMENT_3D('',#439954,#128383,#128384);
#104606=AXIS2_PLACEMENT_3D('',#439967,#128385,#128386);
#104607=AXIS2_PLACEMENT_3D('',#439968,#128387,#128388);
#104608=AXIS2_PLACEMENT_3D('',#439975,#128391,#128392);
#104609=AXIS2_PLACEMENT_3D('',#439982,#128394,#128395);
#104610=AXIS2_PLACEMENT_3D('',#439985,#128396,#128397);
#104611=AXIS2_PLACEMENT_3D('',#439996,#128401,#128402);
#104612=AXIS2_PLACEMENT_3D('',#440064,#128403,#128404);
#104613=AXIS2_PLACEMENT_3D('',#440065,#128405,#128406);
#104614=AXIS2_PLACEMENT_3D('',#440107,#128407,#128408);
#104615=AXIS2_PLACEMENT_3D('',#440134,#128409,#128410);
#104616=AXIS2_PLACEMENT_3D('',#440215,#128411,#128412);
#104617=AXIS2_PLACEMENT_3D('',#440228,#128413,#128414);
#104618=AXIS2_PLACEMENT_3D('',#440229,#128415,#128416);
#104619=AXIS2_PLACEMENT_3D('',#440230,#128417,#128418);
#104620=AXIS2_PLACEMENT_3D('',#440243,#128419,#128420);
#104621=AXIS2_PLACEMENT_3D('',#440256,#128421,#128422);
#104622=AXIS2_PLACEMENT_3D('',#440275,#128423,#128424);
#104623=AXIS2_PLACEMENT_3D('',#440288,#128425,#128426);
#104624=AXIS2_PLACEMENT_3D('',#440301,#128427,#128428);
#104625=AXIS2_PLACEMENT_3D('',#440302,#128429,#128430);
#104626=AXIS2_PLACEMENT_3D('',#440303,#128431,#128432);
#104627=AXIS2_PLACEMENT_3D('',#440316,#128433,#128434);
#104628=AXIS2_PLACEMENT_3D('',#440317,#128435,#128436);
#104629=AXIS2_PLACEMENT_3D('',#440324,#128439,#128440);
#104630=AXIS2_PLACEMENT_3D('',#440331,#128442,#128443);
#104631=AXIS2_PLACEMENT_3D('',#440334,#128444,#128445);
#104632=AXIS2_PLACEMENT_3D('',#440345,#128449,#128450);
#104633=AXIS2_PLACEMENT_3D('',#440413,#128451,#128452);
#104634=AXIS2_PLACEMENT_3D('',#440414,#128453,#128454);
#104635=AXIS2_PLACEMENT_3D('',#440456,#128455,#128456);
#104636=AXIS2_PLACEMENT_3D('',#440483,#128457,#128458);
#104637=AXIS2_PLACEMENT_3D('',#440564,#128459,#128460);
#104638=AXIS2_PLACEMENT_3D('',#440577,#128461,#128462);
#104639=AXIS2_PLACEMENT_3D('',#440578,#128463,#128464);
#104640=AXIS2_PLACEMENT_3D('',#440579,#128465,#128466);
#104641=AXIS2_PLACEMENT_3D('',#440592,#128467,#128468);
#104642=AXIS2_PLACEMENT_3D('',#440605,#128469,#128470);
#104643=AXIS2_PLACEMENT_3D('',#440624,#128471,#128472);
#104644=AXIS2_PLACEMENT_3D('',#440637,#128473,#128474);
#104645=AXIS2_PLACEMENT_3D('',#440650,#128475,#128476);
#104646=AXIS2_PLACEMENT_3D('',#440651,#128477,#128478);
#104647=AXIS2_PLACEMENT_3D('',#440652,#128479,#128480);
#104648=AXIS2_PLACEMENT_3D('',#440665,#128481,#128482);
#104649=AXIS2_PLACEMENT_3D('',#440666,#128483,#128484);
#104650=AXIS2_PLACEMENT_3D('',#440673,#128487,#128488);
#104651=AXIS2_PLACEMENT_3D('',#440680,#128490,#128491);
#104652=AXIS2_PLACEMENT_3D('',#440683,#128492,#128493);
#104653=AXIS2_PLACEMENT_3D('',#440694,#128497,#128498);
#104654=AXIS2_PLACEMENT_3D('',#440762,#128499,#128500);
#104655=AXIS2_PLACEMENT_3D('',#440763,#128501,#128502);
#104656=AXIS2_PLACEMENT_3D('',#440805,#128503,#128504);
#104657=AXIS2_PLACEMENT_3D('',#440832,#128505,#128506);
#104658=AXIS2_PLACEMENT_3D('',#440913,#128507,#128508);
#104659=AXIS2_PLACEMENT_3D('',#440926,#128509,#128510);
#104660=AXIS2_PLACEMENT_3D('',#440927,#128511,#128512);
#104661=AXIS2_PLACEMENT_3D('',#440928,#128513,#128514);
#104662=AXIS2_PLACEMENT_3D('',#440941,#128515,#128516);
#104663=AXIS2_PLACEMENT_3D('',#440954,#128517,#128518);
#104664=AXIS2_PLACEMENT_3D('',#440973,#128519,#128520);
#104665=AXIS2_PLACEMENT_3D('',#440986,#128521,#128522);
#104666=AXIS2_PLACEMENT_3D('',#440999,#128523,#128524);
#104667=AXIS2_PLACEMENT_3D('',#441000,#128525,#128526);
#104668=AXIS2_PLACEMENT_3D('',#441001,#128527,#128528);
#104669=AXIS2_PLACEMENT_3D('',#441014,#128529,#128530);
#104670=AXIS2_PLACEMENT_3D('',#441015,#128531,#128532);
#104671=AXIS2_PLACEMENT_3D('',#441022,#128535,#128536);
#104672=AXIS2_PLACEMENT_3D('',#441029,#128538,#128539);
#104673=AXIS2_PLACEMENT_3D('',#441032,#128540,#128541);
#104674=AXIS2_PLACEMENT_3D('',#441043,#128545,#128546);
#104675=AXIS2_PLACEMENT_3D('',#441111,#128547,#128548);
#104676=AXIS2_PLACEMENT_3D('',#441112,#128549,#128550);
#104677=AXIS2_PLACEMENT_3D('',#441154,#128551,#128552);
#104678=AXIS2_PLACEMENT_3D('',#441181,#128553,#128554);
#104679=AXIS2_PLACEMENT_3D('',#441262,#128555,#128556);
#104680=AXIS2_PLACEMENT_3D('',#441275,#128557,#128558);
#104681=AXIS2_PLACEMENT_3D('',#441276,#128559,#128560);
#104682=AXIS2_PLACEMENT_3D('',#441277,#128561,#128562);
#104683=AXIS2_PLACEMENT_3D('',#441290,#128563,#128564);
#104684=AXIS2_PLACEMENT_3D('',#441303,#128565,#128566);
#104685=AXIS2_PLACEMENT_3D('',#441322,#128567,#128568);
#104686=AXIS2_PLACEMENT_3D('',#441335,#128569,#128570);
#104687=AXIS2_PLACEMENT_3D('',#441348,#128571,#128572);
#104688=AXIS2_PLACEMENT_3D('',#441349,#128573,#128574);
#104689=AXIS2_PLACEMENT_3D('',#441350,#128575,#128576);
#104690=AXIS2_PLACEMENT_3D('',#441363,#128577,#128578);
#104691=AXIS2_PLACEMENT_3D('',#441364,#128579,#128580);
#104692=AXIS2_PLACEMENT_3D('',#441371,#128583,#128584);
#104693=AXIS2_PLACEMENT_3D('',#441378,#128586,#128587);
#104694=AXIS2_PLACEMENT_3D('',#441381,#128588,#128589);
#104695=AXIS2_PLACEMENT_3D('',#441392,#128593,#128594);
#104696=AXIS2_PLACEMENT_3D('',#441460,#128595,#128596);
#104697=AXIS2_PLACEMENT_3D('',#441461,#128597,#128598);
#104698=AXIS2_PLACEMENT_3D('',#441503,#128599,#128600);
#104699=AXIS2_PLACEMENT_3D('',#441530,#128601,#128602);
#104700=AXIS2_PLACEMENT_3D('',#441611,#128603,#128604);
#104701=AXIS2_PLACEMENT_3D('',#441624,#128605,#128606);
#104702=AXIS2_PLACEMENT_3D('',#441625,#128607,#128608);
#104703=AXIS2_PLACEMENT_3D('',#441626,#128609,#128610);
#104704=AXIS2_PLACEMENT_3D('',#441639,#128611,#128612);
#104705=AXIS2_PLACEMENT_3D('',#441652,#128613,#128614);
#104706=AXIS2_PLACEMENT_3D('',#441671,#128615,#128616);
#104707=AXIS2_PLACEMENT_3D('',#441684,#128617,#128618);
#104708=AXIS2_PLACEMENT_3D('',#441697,#128619,#128620);
#104709=AXIS2_PLACEMENT_3D('',#441698,#128621,#128622);
#104710=AXIS2_PLACEMENT_3D('',#441699,#128623,#128624);
#104711=AXIS2_PLACEMENT_3D('',#441712,#128625,#128626);
#104712=AXIS2_PLACEMENT_3D('',#441713,#128627,#128628);
#104713=AXIS2_PLACEMENT_3D('',#441720,#128631,#128632);
#104714=AXIS2_PLACEMENT_3D('',#441727,#128634,#128635);
#104715=AXIS2_PLACEMENT_3D('',#441730,#128636,#128637);
#104716=AXIS2_PLACEMENT_3D('',#441741,#128641,#128642);
#104717=AXIS2_PLACEMENT_3D('',#441809,#128643,#128644);
#104718=AXIS2_PLACEMENT_3D('',#441810,#128645,#128646);
#104719=AXIS2_PLACEMENT_3D('',#441852,#128647,#128648);
#104720=AXIS2_PLACEMENT_3D('',#441879,#128649,#128650);
#104721=AXIS2_PLACEMENT_3D('',#441960,#128651,#128652);
#104722=AXIS2_PLACEMENT_3D('',#441973,#128653,#128654);
#104723=AXIS2_PLACEMENT_3D('',#441974,#128655,#128656);
#104724=AXIS2_PLACEMENT_3D('',#441975,#128657,#128658);
#104725=AXIS2_PLACEMENT_3D('',#441988,#128659,#128660);
#104726=AXIS2_PLACEMENT_3D('',#442001,#128661,#128662);
#104727=AXIS2_PLACEMENT_3D('',#442020,#128663,#128664);
#104728=AXIS2_PLACEMENT_3D('',#442033,#128665,#128666);
#104729=AXIS2_PLACEMENT_3D('',#442046,#128667,#128668);
#104730=AXIS2_PLACEMENT_3D('',#442047,#128669,#128670);
#104731=AXIS2_PLACEMENT_3D('',#442048,#128671,#128672);
#104732=AXIS2_PLACEMENT_3D('',#442061,#128673,#128674);
#104733=AXIS2_PLACEMENT_3D('',#442062,#128675,#128676);
#104734=AXIS2_PLACEMENT_3D('',#442069,#128679,#128680);
#104735=AXIS2_PLACEMENT_3D('',#442076,#128682,#128683);
#104736=AXIS2_PLACEMENT_3D('',#442079,#128684,#128685);
#104737=AXIS2_PLACEMENT_3D('',#442090,#128689,#128690);
#104738=AXIS2_PLACEMENT_3D('',#442158,#128691,#128692);
#104739=AXIS2_PLACEMENT_3D('',#442159,#128693,#128694);
#104740=AXIS2_PLACEMENT_3D('',#442201,#128695,#128696);
#104741=AXIS2_PLACEMENT_3D('',#442228,#128697,#128698);
#104742=AXIS2_PLACEMENT_3D('',#442309,#128699,#128700);
#104743=AXIS2_PLACEMENT_3D('',#442322,#128701,#128702);
#104744=AXIS2_PLACEMENT_3D('',#442323,#128703,#128704);
#104745=AXIS2_PLACEMENT_3D('',#442324,#128705,#128706);
#104746=AXIS2_PLACEMENT_3D('',#442337,#128707,#128708);
#104747=AXIS2_PLACEMENT_3D('',#442350,#128709,#128710);
#104748=AXIS2_PLACEMENT_3D('',#442369,#128711,#128712);
#104749=AXIS2_PLACEMENT_3D('',#442382,#128713,#128714);
#104750=AXIS2_PLACEMENT_3D('',#442395,#128715,#128716);
#104751=AXIS2_PLACEMENT_3D('',#442396,#128717,#128718);
#104752=AXIS2_PLACEMENT_3D('',#442397,#128719,#128720);
#104753=AXIS2_PLACEMENT_3D('',#442410,#128721,#128722);
#104754=AXIS2_PLACEMENT_3D('',#442411,#128723,#128724);
#104755=AXIS2_PLACEMENT_3D('',#442418,#128727,#128728);
#104756=AXIS2_PLACEMENT_3D('',#442425,#128730,#128731);
#104757=AXIS2_PLACEMENT_3D('',#442428,#128732,#128733);
#104758=AXIS2_PLACEMENT_3D('',#442439,#128737,#128738);
#104759=AXIS2_PLACEMENT_3D('',#442507,#128739,#128740);
#104760=AXIS2_PLACEMENT_3D('',#442508,#128741,#128742);
#104761=AXIS2_PLACEMENT_3D('',#442550,#128743,#128744);
#104762=AXIS2_PLACEMENT_3D('',#442577,#128745,#128746);
#104763=AXIS2_PLACEMENT_3D('',#442658,#128747,#128748);
#104764=AXIS2_PLACEMENT_3D('',#442671,#128749,#128750);
#104765=AXIS2_PLACEMENT_3D('',#442672,#128751,#128752);
#104766=AXIS2_PLACEMENT_3D('',#442673,#128753,#128754);
#104767=AXIS2_PLACEMENT_3D('',#442686,#128755,#128756);
#104768=AXIS2_PLACEMENT_3D('',#442699,#128757,#128758);
#104769=AXIS2_PLACEMENT_3D('',#442718,#128759,#128760);
#104770=AXIS2_PLACEMENT_3D('',#442731,#128761,#128762);
#104771=AXIS2_PLACEMENT_3D('',#442744,#128763,#128764);
#104772=AXIS2_PLACEMENT_3D('',#442745,#128765,#128766);
#104773=AXIS2_PLACEMENT_3D('',#442746,#128767,#128768);
#104774=AXIS2_PLACEMENT_3D('',#442759,#128769,#128770);
#104775=AXIS2_PLACEMENT_3D('',#442760,#128771,#128772);
#104776=AXIS2_PLACEMENT_3D('',#442767,#128775,#128776);
#104777=AXIS2_PLACEMENT_3D('',#442774,#128778,#128779);
#104778=AXIS2_PLACEMENT_3D('',#442777,#128780,#128781);
#104779=AXIS2_PLACEMENT_3D('',#442788,#128785,#128786);
#104780=AXIS2_PLACEMENT_3D('',#442856,#128787,#128788);
#104781=AXIS2_PLACEMENT_3D('',#442857,#128789,#128790);
#104782=AXIS2_PLACEMENT_3D('',#442899,#128791,#128792);
#104783=AXIS2_PLACEMENT_3D('',#442926,#128793,#128794);
#104784=AXIS2_PLACEMENT_3D('',#443007,#128795,#128796);
#104785=AXIS2_PLACEMENT_3D('',#443020,#128797,#128798);
#104786=AXIS2_PLACEMENT_3D('',#443021,#128799,#128800);
#104787=AXIS2_PLACEMENT_3D('',#443022,#128801,#128802);
#104788=AXIS2_PLACEMENT_3D('',#443035,#128803,#128804);
#104789=AXIS2_PLACEMENT_3D('',#443048,#128805,#128806);
#104790=AXIS2_PLACEMENT_3D('',#443067,#128807,#128808);
#104791=AXIS2_PLACEMENT_3D('',#443080,#128809,#128810);
#104792=AXIS2_PLACEMENT_3D('',#443093,#128811,#128812);
#104793=AXIS2_PLACEMENT_3D('',#443094,#128813,#128814);
#104794=AXIS2_PLACEMENT_3D('',#443095,#128815,#128816);
#104795=AXIS2_PLACEMENT_3D('',#443108,#128817,#128818);
#104796=AXIS2_PLACEMENT_3D('',#443109,#128819,#128820);
#104797=AXIS2_PLACEMENT_3D('',#443116,#128823,#128824);
#104798=AXIS2_PLACEMENT_3D('',#443123,#128826,#128827);
#104799=AXIS2_PLACEMENT_3D('',#443126,#128828,#128829);
#104800=AXIS2_PLACEMENT_3D('',#443137,#128833,#128834);
#104801=AXIS2_PLACEMENT_3D('',#443205,#128835,#128836);
#104802=AXIS2_PLACEMENT_3D('',#443206,#128837,#128838);
#104803=AXIS2_PLACEMENT_3D('',#443248,#128839,#128840);
#104804=AXIS2_PLACEMENT_3D('',#443275,#128841,#128842);
#104805=AXIS2_PLACEMENT_3D('',#443356,#128843,#128844);
#104806=AXIS2_PLACEMENT_3D('',#443369,#128845,#128846);
#104807=AXIS2_PLACEMENT_3D('',#443370,#128847,#128848);
#104808=AXIS2_PLACEMENT_3D('',#443371,#128849,#128850);
#104809=AXIS2_PLACEMENT_3D('',#443384,#128851,#128852);
#104810=AXIS2_PLACEMENT_3D('',#443397,#128853,#128854);
#104811=AXIS2_PLACEMENT_3D('',#443416,#128855,#128856);
#104812=AXIS2_PLACEMENT_3D('',#443429,#128857,#128858);
#104813=AXIS2_PLACEMENT_3D('',#443442,#128859,#128860);
#104814=AXIS2_PLACEMENT_3D('',#443443,#128861,#128862);
#104815=AXIS2_PLACEMENT_3D('',#443444,#128863,#128864);
#104816=AXIS2_PLACEMENT_3D('',#443457,#128865,#128866);
#104817=AXIS2_PLACEMENT_3D('',#443458,#128867,#128868);
#104818=AXIS2_PLACEMENT_3D('',#443465,#128871,#128872);
#104819=AXIS2_PLACEMENT_3D('',#443472,#128874,#128875);
#104820=AXIS2_PLACEMENT_3D('',#443475,#128876,#128877);
#104821=AXIS2_PLACEMENT_3D('',#443486,#128881,#128882);
#104822=AXIS2_PLACEMENT_3D('',#443554,#128883,#128884);
#104823=AXIS2_PLACEMENT_3D('',#443555,#128885,#128886);
#104824=AXIS2_PLACEMENT_3D('',#443597,#128887,#128888);
#104825=AXIS2_PLACEMENT_3D('',#443624,#128889,#128890);
#104826=AXIS2_PLACEMENT_3D('',#443705,#128891,#128892);
#104827=AXIS2_PLACEMENT_3D('',#443718,#128893,#128894);
#104828=AXIS2_PLACEMENT_3D('',#443719,#128895,#128896);
#104829=AXIS2_PLACEMENT_3D('',#443720,#128897,#128898);
#104830=AXIS2_PLACEMENT_3D('',#443733,#128899,#128900);
#104831=AXIS2_PLACEMENT_3D('',#443746,#128901,#128902);
#104832=AXIS2_PLACEMENT_3D('',#443765,#128903,#128904);
#104833=AXIS2_PLACEMENT_3D('',#443778,#128905,#128906);
#104834=AXIS2_PLACEMENT_3D('',#443791,#128907,#128908);
#104835=AXIS2_PLACEMENT_3D('',#443792,#128909,#128910);
#104836=AXIS2_PLACEMENT_3D('',#443793,#128911,#128912);
#104837=AXIS2_PLACEMENT_3D('',#443806,#128913,#128914);
#104838=AXIS2_PLACEMENT_3D('',#443807,#128915,#128916);
#104839=AXIS2_PLACEMENT_3D('',#443814,#128919,#128920);
#104840=AXIS2_PLACEMENT_3D('',#443821,#128922,#128923);
#104841=AXIS2_PLACEMENT_3D('',#443824,#128924,#128925);
#104842=AXIS2_PLACEMENT_3D('',#443835,#128929,#128930);
#104843=AXIS2_PLACEMENT_3D('',#443903,#128931,#128932);
#104844=AXIS2_PLACEMENT_3D('',#443904,#128933,#128934);
#104845=AXIS2_PLACEMENT_3D('',#443946,#128935,#128936);
#104846=AXIS2_PLACEMENT_3D('',#443973,#128937,#128938);
#104847=AXIS2_PLACEMENT_3D('',#444054,#128939,#128940);
#104848=AXIS2_PLACEMENT_3D('',#444067,#128941,#128942);
#104849=AXIS2_PLACEMENT_3D('',#444068,#128943,#128944);
#104850=AXIS2_PLACEMENT_3D('',#444069,#128945,#128946);
#104851=AXIS2_PLACEMENT_3D('',#444082,#128947,#128948);
#104852=AXIS2_PLACEMENT_3D('',#444095,#128949,#128950);
#104853=AXIS2_PLACEMENT_3D('',#444114,#128951,#128952);
#104854=AXIS2_PLACEMENT_3D('',#444127,#128953,#128954);
#104855=AXIS2_PLACEMENT_3D('',#444140,#128955,#128956);
#104856=AXIS2_PLACEMENT_3D('',#444141,#128957,#128958);
#104857=AXIS2_PLACEMENT_3D('',#444142,#128959,#128960);
#104858=AXIS2_PLACEMENT_3D('',#444155,#128961,#128962);
#104859=AXIS2_PLACEMENT_3D('',#444156,#128963,#128964);
#104860=AXIS2_PLACEMENT_3D('',#444163,#128967,#128968);
#104861=AXIS2_PLACEMENT_3D('',#444170,#128970,#128971);
#104862=AXIS2_PLACEMENT_3D('',#444173,#128972,#128973);
#104863=AXIS2_PLACEMENT_3D('',#444184,#128977,#128978);
#104864=AXIS2_PLACEMENT_3D('',#444252,#128979,#128980);
#104865=AXIS2_PLACEMENT_3D('',#444253,#128981,#128982);
#104866=AXIS2_PLACEMENT_3D('',#444295,#128983,#128984);
#104867=AXIS2_PLACEMENT_3D('',#444322,#128985,#128986);
#104868=AXIS2_PLACEMENT_3D('',#444403,#128987,#128988);
#104869=AXIS2_PLACEMENT_3D('',#444416,#128989,#128990);
#104870=AXIS2_PLACEMENT_3D('',#444417,#128991,#128992);
#104871=AXIS2_PLACEMENT_3D('',#444418,#128993,#128994);
#104872=AXIS2_PLACEMENT_3D('',#444431,#128995,#128996);
#104873=AXIS2_PLACEMENT_3D('',#444444,#128997,#128998);
#104874=AXIS2_PLACEMENT_3D('',#444463,#128999,#129000);
#104875=AXIS2_PLACEMENT_3D('',#444476,#129001,#129002);
#104876=AXIS2_PLACEMENT_3D('',#444489,#129003,#129004);
#104877=AXIS2_PLACEMENT_3D('',#444490,#129005,#129006);
#104878=AXIS2_PLACEMENT_3D('',#444491,#129007,#129008);
#104879=AXIS2_PLACEMENT_3D('',#444504,#129009,#129010);
#104880=AXIS2_PLACEMENT_3D('',#444505,#129011,#129012);
#104881=AXIS2_PLACEMENT_3D('',#444512,#129015,#129016);
#104882=AXIS2_PLACEMENT_3D('',#444519,#129018,#129019);
#104883=AXIS2_PLACEMENT_3D('',#444522,#129020,#129021);
#104884=AXIS2_PLACEMENT_3D('',#444533,#129025,#129026);
#104885=AXIS2_PLACEMENT_3D('',#444601,#129027,#129028);
#104886=AXIS2_PLACEMENT_3D('',#444602,#129029,#129030);
#104887=AXIS2_PLACEMENT_3D('',#444644,#129031,#129032);
#104888=AXIS2_PLACEMENT_3D('',#444671,#129033,#129034);
#104889=AXIS2_PLACEMENT_3D('',#444752,#129035,#129036);
#104890=AXIS2_PLACEMENT_3D('',#444765,#129037,#129038);
#104891=AXIS2_PLACEMENT_3D('',#444766,#129039,#129040);
#104892=AXIS2_PLACEMENT_3D('',#444767,#129041,#129042);
#104893=AXIS2_PLACEMENT_3D('',#444780,#129043,#129044);
#104894=AXIS2_PLACEMENT_3D('',#444793,#129045,#129046);
#104895=AXIS2_PLACEMENT_3D('',#444812,#129047,#129048);
#104896=AXIS2_PLACEMENT_3D('',#444825,#129049,#129050);
#104897=AXIS2_PLACEMENT_3D('',#444838,#129051,#129052);
#104898=AXIS2_PLACEMENT_3D('',#444839,#129053,#129054);
#104899=AXIS2_PLACEMENT_3D('',#444840,#129055,#129056);
#104900=AXIS2_PLACEMENT_3D('',#444853,#129057,#129058);
#104901=AXIS2_PLACEMENT_3D('',#444854,#129059,#129060);
#104902=AXIS2_PLACEMENT_3D('',#444861,#129063,#129064);
#104903=AXIS2_PLACEMENT_3D('',#444868,#129066,#129067);
#104904=AXIS2_PLACEMENT_3D('',#444871,#129068,#129069);
#104905=AXIS2_PLACEMENT_3D('',#444882,#129073,#129074);
#104906=AXIS2_PLACEMENT_3D('',#444950,#129075,#129076);
#104907=AXIS2_PLACEMENT_3D('',#444951,#129077,#129078);
#104908=AXIS2_PLACEMENT_3D('',#444993,#129079,#129080);
#104909=AXIS2_PLACEMENT_3D('',#445020,#129081,#129082);
#104910=AXIS2_PLACEMENT_3D('',#445101,#129083,#129084);
#104911=AXIS2_PLACEMENT_3D('',#445114,#129085,#129086);
#104912=AXIS2_PLACEMENT_3D('',#445115,#129087,#129088);
#104913=AXIS2_PLACEMENT_3D('',#445116,#129089,#129090);
#104914=AXIS2_PLACEMENT_3D('',#445129,#129091,#129092);
#104915=AXIS2_PLACEMENT_3D('',#445142,#129093,#129094);
#104916=AXIS2_PLACEMENT_3D('',#445161,#129095,#129096);
#104917=AXIS2_PLACEMENT_3D('',#445174,#129097,#129098);
#104918=AXIS2_PLACEMENT_3D('',#445187,#129099,#129100);
#104919=AXIS2_PLACEMENT_3D('',#445188,#129101,#129102);
#104920=AXIS2_PLACEMENT_3D('',#445189,#129103,#129104);
#104921=AXIS2_PLACEMENT_3D('',#445202,#129105,#129106);
#104922=AXIS2_PLACEMENT_3D('',#445203,#129107,#129108);
#104923=AXIS2_PLACEMENT_3D('',#445210,#129111,#129112);
#104924=AXIS2_PLACEMENT_3D('',#445217,#129114,#129115);
#104925=AXIS2_PLACEMENT_3D('',#445220,#129116,#129117);
#104926=AXIS2_PLACEMENT_3D('',#445231,#129121,#129122);
#104927=AXIS2_PLACEMENT_3D('',#445299,#129123,#129124);
#104928=AXIS2_PLACEMENT_3D('',#445300,#129125,#129126);
#104929=AXIS2_PLACEMENT_3D('',#445342,#129127,#129128);
#104930=AXIS2_PLACEMENT_3D('',#445369,#129129,#129130);
#104931=AXIS2_PLACEMENT_3D('',#445450,#129131,#129132);
#104932=AXIS2_PLACEMENT_3D('',#445463,#129133,#129134);
#104933=AXIS2_PLACEMENT_3D('',#445464,#129135,#129136);
#104934=AXIS2_PLACEMENT_3D('',#445465,#129137,#129138);
#104935=AXIS2_PLACEMENT_3D('',#445478,#129139,#129140);
#104936=AXIS2_PLACEMENT_3D('',#445491,#129141,#129142);
#104937=AXIS2_PLACEMENT_3D('',#445510,#129143,#129144);
#104938=AXIS2_PLACEMENT_3D('',#445523,#129145,#129146);
#104939=AXIS2_PLACEMENT_3D('',#445536,#129147,#129148);
#104940=AXIS2_PLACEMENT_3D('',#445537,#129149,#129150);
#104941=AXIS2_PLACEMENT_3D('',#445538,#129151,#129152);
#104942=AXIS2_PLACEMENT_3D('',#445551,#129153,#129154);
#104943=AXIS2_PLACEMENT_3D('',#445552,#129155,#129156);
#104944=AXIS2_PLACEMENT_3D('',#445559,#129159,#129160);
#104945=AXIS2_PLACEMENT_3D('',#445566,#129162,#129163);
#104946=AXIS2_PLACEMENT_3D('',#445569,#129164,#129165);
#104947=AXIS2_PLACEMENT_3D('',#445580,#129169,#129170);
#104948=AXIS2_PLACEMENT_3D('',#445648,#129171,#129172);
#104949=AXIS2_PLACEMENT_3D('',#445649,#129173,#129174);
#104950=AXIS2_PLACEMENT_3D('',#445691,#129175,#129176);
#104951=AXIS2_PLACEMENT_3D('',#445718,#129177,#129178);
#104952=AXIS2_PLACEMENT_3D('',#445799,#129179,#129180);
#104953=AXIS2_PLACEMENT_3D('',#445812,#129181,#129182);
#104954=AXIS2_PLACEMENT_3D('',#445813,#129183,#129184);
#104955=AXIS2_PLACEMENT_3D('',#445814,#129185,#129186);
#104956=AXIS2_PLACEMENT_3D('',#445827,#129187,#129188);
#104957=AXIS2_PLACEMENT_3D('',#445840,#129189,#129190);
#104958=AXIS2_PLACEMENT_3D('',#445859,#129191,#129192);
#104959=AXIS2_PLACEMENT_3D('',#445872,#129193,#129194);
#104960=AXIS2_PLACEMENT_3D('',#445885,#129195,#129196);
#104961=AXIS2_PLACEMENT_3D('',#445886,#129197,#129198);
#104962=AXIS2_PLACEMENT_3D('',#445887,#129199,#129200);
#104963=AXIS2_PLACEMENT_3D('',#445900,#129201,#129202);
#104964=AXIS2_PLACEMENT_3D('',#445901,#129203,#129204);
#104965=AXIS2_PLACEMENT_3D('',#445908,#129207,#129208);
#104966=AXIS2_PLACEMENT_3D('',#445915,#129210,#129211);
#104967=AXIS2_PLACEMENT_3D('',#445918,#129212,#129213);
#104968=AXIS2_PLACEMENT_3D('',#445929,#129217,#129218);
#104969=AXIS2_PLACEMENT_3D('',#445997,#129219,#129220);
#104970=AXIS2_PLACEMENT_3D('',#445998,#129221,#129222);
#104971=AXIS2_PLACEMENT_3D('',#446040,#129223,#129224);
#104972=AXIS2_PLACEMENT_3D('',#446067,#129225,#129226);
#104973=AXIS2_PLACEMENT_3D('',#446148,#129227,#129228);
#104974=AXIS2_PLACEMENT_3D('',#446161,#129229,#129230);
#104975=AXIS2_PLACEMENT_3D('',#446162,#129231,#129232);
#104976=AXIS2_PLACEMENT_3D('',#446163,#129233,#129234);
#104977=AXIS2_PLACEMENT_3D('',#446176,#129235,#129236);
#104978=AXIS2_PLACEMENT_3D('',#446189,#129237,#129238);
#104979=AXIS2_PLACEMENT_3D('',#446208,#129239,#129240);
#104980=AXIS2_PLACEMENT_3D('',#446221,#129241,#129242);
#104981=AXIS2_PLACEMENT_3D('',#446234,#129243,#129244);
#104982=AXIS2_PLACEMENT_3D('',#446235,#129245,#129246);
#104983=AXIS2_PLACEMENT_3D('',#446236,#129247,#129248);
#104984=AXIS2_PLACEMENT_3D('',#446249,#129249,#129250);
#104985=AXIS2_PLACEMENT_3D('',#446250,#129251,#129252);
#104986=AXIS2_PLACEMENT_3D('',#446257,#129255,#129256);
#104987=AXIS2_PLACEMENT_3D('',#446264,#129258,#129259);
#104988=AXIS2_PLACEMENT_3D('',#446267,#129260,#129261);
#104989=AXIS2_PLACEMENT_3D('',#446278,#129265,#129266);
#104990=AXIS2_PLACEMENT_3D('',#446346,#129267,#129268);
#104991=AXIS2_PLACEMENT_3D('',#446347,#129269,#129270);
#104992=AXIS2_PLACEMENT_3D('',#446389,#129271,#129272);
#104993=AXIS2_PLACEMENT_3D('',#446416,#129273,#129274);
#104994=AXIS2_PLACEMENT_3D('',#446497,#129275,#129276);
#104995=AXIS2_PLACEMENT_3D('',#446510,#129277,#129278);
#104996=AXIS2_PLACEMENT_3D('',#446511,#129279,#129280);
#104997=AXIS2_PLACEMENT_3D('',#446512,#129281,#129282);
#104998=AXIS2_PLACEMENT_3D('',#446525,#129283,#129284);
#104999=AXIS2_PLACEMENT_3D('',#446538,#129285,#129286);
#105000=AXIS2_PLACEMENT_3D('',#446557,#129287,#129288);
#105001=AXIS2_PLACEMENT_3D('',#446570,#129289,#129290);
#105002=AXIS2_PLACEMENT_3D('',#446583,#129291,#129292);
#105003=AXIS2_PLACEMENT_3D('',#446584,#129293,#129294);
#105004=AXIS2_PLACEMENT_3D('',#446585,#129295,#129296);
#105005=AXIS2_PLACEMENT_3D('',#446598,#129297,#129298);
#105006=AXIS2_PLACEMENT_3D('',#446599,#129299,#129300);
#105007=AXIS2_PLACEMENT_3D('',#446606,#129303,#129304);
#105008=AXIS2_PLACEMENT_3D('',#446613,#129306,#129307);
#105009=AXIS2_PLACEMENT_3D('',#446616,#129308,#129309);
#105010=AXIS2_PLACEMENT_3D('',#446627,#129313,#129314);
#105011=AXIS2_PLACEMENT_3D('',#446695,#129315,#129316);
#105012=AXIS2_PLACEMENT_3D('',#446696,#129317,#129318);
#105013=AXIS2_PLACEMENT_3D('',#446738,#129319,#129320);
#105014=AXIS2_PLACEMENT_3D('',#446765,#129321,#129322);
#105015=AXIS2_PLACEMENT_3D('',#446846,#129323,#129324);
#105016=AXIS2_PLACEMENT_3D('',#446859,#129325,#129326);
#105017=AXIS2_PLACEMENT_3D('',#446860,#129327,#129328);
#105018=AXIS2_PLACEMENT_3D('',#446861,#129329,#129330);
#105019=AXIS2_PLACEMENT_3D('',#446874,#129331,#129332);
#105020=AXIS2_PLACEMENT_3D('',#446887,#129333,#129334);
#105021=AXIS2_PLACEMENT_3D('',#446906,#129335,#129336);
#105022=AXIS2_PLACEMENT_3D('',#446919,#129337,#129338);
#105023=AXIS2_PLACEMENT_3D('',#446932,#129339,#129340);
#105024=AXIS2_PLACEMENT_3D('',#446933,#129341,#129342);
#105025=AXIS2_PLACEMENT_3D('',#446934,#129343,#129344);
#105026=AXIS2_PLACEMENT_3D('',#446947,#129345,#129346);
#105027=AXIS2_PLACEMENT_3D('',#446948,#129347,#129348);
#105028=AXIS2_PLACEMENT_3D('',#446955,#129351,#129352);
#105029=AXIS2_PLACEMENT_3D('',#446962,#129354,#129355);
#105030=AXIS2_PLACEMENT_3D('',#446965,#129356,#129357);
#105031=AXIS2_PLACEMENT_3D('',#446976,#129361,#129362);
#105032=AXIS2_PLACEMENT_3D('',#447044,#129363,#129364);
#105033=AXIS2_PLACEMENT_3D('',#447045,#129365,#129366);
#105034=AXIS2_PLACEMENT_3D('',#447087,#129367,#129368);
#105035=AXIS2_PLACEMENT_3D('',#447114,#129369,#129370);
#105036=AXIS2_PLACEMENT_3D('',#447195,#129371,#129372);
#105037=AXIS2_PLACEMENT_3D('',#447208,#129373,#129374);
#105038=AXIS2_PLACEMENT_3D('',#447209,#129375,#129376);
#105039=AXIS2_PLACEMENT_3D('',#447210,#129377,#129378);
#105040=AXIS2_PLACEMENT_3D('',#447223,#129379,#129380);
#105041=AXIS2_PLACEMENT_3D('',#447236,#129381,#129382);
#105042=AXIS2_PLACEMENT_3D('',#447255,#129383,#129384);
#105043=AXIS2_PLACEMENT_3D('',#447268,#129385,#129386);
#105044=AXIS2_PLACEMENT_3D('',#447281,#129387,#129388);
#105045=AXIS2_PLACEMENT_3D('',#447282,#129389,#129390);
#105046=AXIS2_PLACEMENT_3D('',#447283,#129391,#129392);
#105047=AXIS2_PLACEMENT_3D('',#447296,#129393,#129394);
#105048=AXIS2_PLACEMENT_3D('',#447297,#129395,#129396);
#105049=AXIS2_PLACEMENT_3D('',#447304,#129399,#129400);
#105050=AXIS2_PLACEMENT_3D('',#447311,#129402,#129403);
#105051=AXIS2_PLACEMENT_3D('',#447314,#129404,#129405);
#105052=AXIS2_PLACEMENT_3D('',#447325,#129409,#129410);
#105053=AXIS2_PLACEMENT_3D('',#447393,#129411,#129412);
#105054=AXIS2_PLACEMENT_3D('',#447394,#129413,#129414);
#105055=AXIS2_PLACEMENT_3D('',#447436,#129415,#129416);
#105056=AXIS2_PLACEMENT_3D('',#447463,#129417,#129418);
#105057=AXIS2_PLACEMENT_3D('',#447544,#129419,#129420);
#105058=AXIS2_PLACEMENT_3D('',#447557,#129421,#129422);
#105059=AXIS2_PLACEMENT_3D('',#447558,#129423,#129424);
#105060=AXIS2_PLACEMENT_3D('',#447559,#129425,#129426);
#105061=AXIS2_PLACEMENT_3D('',#447572,#129427,#129428);
#105062=AXIS2_PLACEMENT_3D('',#447585,#129429,#129430);
#105063=AXIS2_PLACEMENT_3D('',#447604,#129431,#129432);
#105064=AXIS2_PLACEMENT_3D('',#447617,#129433,#129434);
#105065=AXIS2_PLACEMENT_3D('',#447630,#129435,#129436);
#105066=AXIS2_PLACEMENT_3D('',#447631,#129437,#129438);
#105067=AXIS2_PLACEMENT_3D('',#447632,#129439,#129440);
#105068=AXIS2_PLACEMENT_3D('',#447645,#129441,#129442);
#105069=AXIS2_PLACEMENT_3D('',#447646,#129443,#129444);
#105070=AXIS2_PLACEMENT_3D('',#447653,#129447,#129448);
#105071=AXIS2_PLACEMENT_3D('',#447660,#129450,#129451);
#105072=AXIS2_PLACEMENT_3D('',#447663,#129452,#129453);
#105073=AXIS2_PLACEMENT_3D('',#447674,#129457,#129458);
#105074=AXIS2_PLACEMENT_3D('',#447742,#129459,#129460);
#105075=AXIS2_PLACEMENT_3D('',#447743,#129461,#129462);
#105076=AXIS2_PLACEMENT_3D('',#447785,#129463,#129464);
#105077=AXIS2_PLACEMENT_3D('',#447812,#129465,#129466);
#105078=AXIS2_PLACEMENT_3D('',#447893,#129467,#129468);
#105079=AXIS2_PLACEMENT_3D('',#447906,#129469,#129470);
#105080=AXIS2_PLACEMENT_3D('',#447907,#129471,#129472);
#105081=AXIS2_PLACEMENT_3D('',#447908,#129473,#129474);
#105082=AXIS2_PLACEMENT_3D('',#447921,#129475,#129476);
#105083=AXIS2_PLACEMENT_3D('',#447934,#129477,#129478);
#105084=AXIS2_PLACEMENT_3D('',#447953,#129479,#129480);
#105085=AXIS2_PLACEMENT_3D('',#447966,#129481,#129482);
#105086=AXIS2_PLACEMENT_3D('',#447979,#129483,#129484);
#105087=AXIS2_PLACEMENT_3D('',#447980,#129485,#129486);
#105088=AXIS2_PLACEMENT_3D('',#447981,#129487,#129488);
#105089=AXIS2_PLACEMENT_3D('',#447994,#129489,#129490);
#105090=AXIS2_PLACEMENT_3D('',#447995,#129491,#129492);
#105091=AXIS2_PLACEMENT_3D('',#448002,#129495,#129496);
#105092=AXIS2_PLACEMENT_3D('',#448009,#129498,#129499);
#105093=AXIS2_PLACEMENT_3D('',#448012,#129500,#129501);
#105094=AXIS2_PLACEMENT_3D('',#448023,#129505,#129506);
#105095=AXIS2_PLACEMENT_3D('',#448091,#129507,#129508);
#105096=AXIS2_PLACEMENT_3D('',#448092,#129509,#129510);
#105097=AXIS2_PLACEMENT_3D('',#448134,#129511,#129512);
#105098=AXIS2_PLACEMENT_3D('',#448161,#129513,#129514);
#105099=AXIS2_PLACEMENT_3D('',#448242,#129515,#129516);
#105100=AXIS2_PLACEMENT_3D('',#448255,#129517,#129518);
#105101=AXIS2_PLACEMENT_3D('',#448256,#129519,#129520);
#105102=AXIS2_PLACEMENT_3D('',#448257,#129521,#129522);
#105103=AXIS2_PLACEMENT_3D('',#448270,#129523,#129524);
#105104=AXIS2_PLACEMENT_3D('',#448283,#129525,#129526);
#105105=AXIS2_PLACEMENT_3D('',#448302,#129527,#129528);
#105106=AXIS2_PLACEMENT_3D('',#448315,#129529,#129530);
#105107=AXIS2_PLACEMENT_3D('',#448328,#129531,#129532);
#105108=AXIS2_PLACEMENT_3D('',#448329,#129533,#129534);
#105109=AXIS2_PLACEMENT_3D('',#448330,#129535,#129536);
#105110=AXIS2_PLACEMENT_3D('',#448343,#129537,#129538);
#105111=AXIS2_PLACEMENT_3D('',#448344,#129539,#129540);
#105112=AXIS2_PLACEMENT_3D('',#448351,#129543,#129544);
#105113=AXIS2_PLACEMENT_3D('',#448358,#129546,#129547);
#105114=AXIS2_PLACEMENT_3D('',#448361,#129548,#129549);
#105115=AXIS2_PLACEMENT_3D('',#448372,#129553,#129554);
#105116=AXIS2_PLACEMENT_3D('',#448440,#129555,#129556);
#105117=AXIS2_PLACEMENT_3D('',#448441,#129557,#129558);
#105118=AXIS2_PLACEMENT_3D('',#448483,#129559,#129560);
#105119=AXIS2_PLACEMENT_3D('',#448510,#129561,#129562);
#105120=AXIS2_PLACEMENT_3D('',#448591,#129563,#129564);
#105121=AXIS2_PLACEMENT_3D('',#448604,#129565,#129566);
#105122=AXIS2_PLACEMENT_3D('',#448605,#129567,#129568);
#105123=AXIS2_PLACEMENT_3D('',#448606,#129569,#129570);
#105124=AXIS2_PLACEMENT_3D('',#448619,#129571,#129572);
#105125=AXIS2_PLACEMENT_3D('',#448632,#129573,#129574);
#105126=AXIS2_PLACEMENT_3D('',#448651,#129575,#129576);
#105127=AXIS2_PLACEMENT_3D('',#448664,#129577,#129578);
#105128=AXIS2_PLACEMENT_3D('',#448677,#129579,#129580);
#105129=AXIS2_PLACEMENT_3D('',#448678,#129581,#129582);
#105130=AXIS2_PLACEMENT_3D('',#448679,#129583,#129584);
#105131=AXIS2_PLACEMENT_3D('',#448692,#129585,#129586);
#105132=AXIS2_PLACEMENT_3D('',#448693,#129587,#129588);
#105133=AXIS2_PLACEMENT_3D('',#448700,#129591,#129592);
#105134=AXIS2_PLACEMENT_3D('',#448707,#129594,#129595);
#105135=AXIS2_PLACEMENT_3D('',#448710,#129596,#129597);
#105136=AXIS2_PLACEMENT_3D('',#448721,#129601,#129602);
#105137=AXIS2_PLACEMENT_3D('',#448789,#129603,#129604);
#105138=AXIS2_PLACEMENT_3D('',#448790,#129605,#129606);
#105139=AXIS2_PLACEMENT_3D('',#448832,#129607,#129608);
#105140=AXIS2_PLACEMENT_3D('',#448859,#129609,#129610);
#105141=AXIS2_PLACEMENT_3D('',#448940,#129611,#129612);
#105142=AXIS2_PLACEMENT_3D('',#448953,#129613,#129614);
#105143=AXIS2_PLACEMENT_3D('',#448954,#129615,#129616);
#105144=AXIS2_PLACEMENT_3D('',#448955,#129617,#129618);
#105145=AXIS2_PLACEMENT_3D('',#448968,#129619,#129620);
#105146=AXIS2_PLACEMENT_3D('',#448981,#129621,#129622);
#105147=AXIS2_PLACEMENT_3D('',#449000,#129623,#129624);
#105148=AXIS2_PLACEMENT_3D('',#449013,#129625,#129626);
#105149=AXIS2_PLACEMENT_3D('',#449026,#129627,#129628);
#105150=AXIS2_PLACEMENT_3D('',#449027,#129629,#129630);
#105151=AXIS2_PLACEMENT_3D('',#449028,#129631,#129632);
#105152=AXIS2_PLACEMENT_3D('',#449041,#129633,#129634);
#105153=AXIS2_PLACEMENT_3D('',#449042,#129635,#129636);
#105154=AXIS2_PLACEMENT_3D('',#449049,#129639,#129640);
#105155=AXIS2_PLACEMENT_3D('',#449056,#129642,#129643);
#105156=AXIS2_PLACEMENT_3D('',#449059,#129644,#129645);
#105157=AXIS2_PLACEMENT_3D('',#449070,#129649,#129650);
#105158=AXIS2_PLACEMENT_3D('',#449138,#129651,#129652);
#105159=AXIS2_PLACEMENT_3D('',#449139,#129653,#129654);
#105160=AXIS2_PLACEMENT_3D('',#449181,#129655,#129656);
#105161=AXIS2_PLACEMENT_3D('',#449208,#129657,#129658);
#105162=AXIS2_PLACEMENT_3D('',#449289,#129659,#129660);
#105163=AXIS2_PLACEMENT_3D('',#449302,#129661,#129662);
#105164=AXIS2_PLACEMENT_3D('',#449303,#129663,#129664);
#105165=AXIS2_PLACEMENT_3D('',#449304,#129665,#129666);
#105166=AXIS2_PLACEMENT_3D('',#449317,#129667,#129668);
#105167=AXIS2_PLACEMENT_3D('',#449330,#129669,#129670);
#105168=AXIS2_PLACEMENT_3D('',#449349,#129671,#129672);
#105169=AXIS2_PLACEMENT_3D('',#449362,#129673,#129674);
#105170=AXIS2_PLACEMENT_3D('',#449375,#129675,#129676);
#105171=AXIS2_PLACEMENT_3D('',#449376,#129677,#129678);
#105172=AXIS2_PLACEMENT_3D('',#449377,#129679,#129680);
#105173=AXIS2_PLACEMENT_3D('',#449390,#129681,#129682);
#105174=AXIS2_PLACEMENT_3D('',#449391,#129683,#129684);
#105175=AXIS2_PLACEMENT_3D('',#449392,#129685,#129686);
#105176=AXIS2_PLACEMENT_3D('',#449393,#129687,#129688);
#105177=AXIS2_PLACEMENT_3D('',#449398,#129690,#129691);
#105178=AXIS2_PLACEMENT_3D('',#449406,#129692,#129693);
#105179=AXIS2_PLACEMENT_3D('',#449430,#129695,#129696);
#105180=AXIS2_PLACEMENT_3D('',#449453,#129697,#129698);
#105181=AXIS2_PLACEMENT_3D('',#449501,#129700,#129701);
#105182=AXIS2_PLACEMENT_3D('',#449552,#129703,#129704);
#105183=AXIS2_PLACEMENT_3D('',#449603,#129706,#129707);
#105184=AXIS2_PLACEMENT_3D('',#449651,#129709,#129710);
#105185=AXIS2_PLACEMENT_3D('',#449702,#129712,#129713);
#105186=AXIS2_PLACEMENT_3D('',#449721,#129715,#129716);
#105187=AXIS2_PLACEMENT_3D('',#449741,#129717,#129718);
#105188=AXIS2_PLACEMENT_3D('',#449754,#129720,#129721);
#105189=AXIS2_PLACEMENT_3D('',#449762,#129722,#129723);
#105190=AXIS2_PLACEMENT_3D('',#449786,#129725,#129726);
#105191=AXIS2_PLACEMENT_3D('',#449811,#129728,#129729);
#105192=AXIS2_PLACEMENT_3D('',#449835,#129731,#129732);
#105193=AXIS2_PLACEMENT_3D('',#449860,#129734,#129735);
#105194=AXIS2_PLACEMENT_3D('',#449885,#129737,#129738);
#105195=AXIS2_PLACEMENT_3D('',#449909,#129740,#129741);
#105196=AXIS2_PLACEMENT_3D('',#449920,#129743,#129744);
#105197=AXIS2_PLACEMENT_3D('',#449926,#129745,#129746);
#105198=AXIS2_PLACEMENT_3D('',#449931,#129748,#129749);
#105199=AXIS2_PLACEMENT_3D('',#449939,#129750,#129751);
#105200=AXIS2_PLACEMENT_3D('',#449963,#129753,#129754);
#105201=AXIS2_PLACEMENT_3D('',#449986,#129755,#129756);
#105202=AXIS2_PLACEMENT_3D('',#450034,#129758,#129759);
#105203=AXIS2_PLACEMENT_3D('',#450085,#129761,#129762);
#105204=AXIS2_PLACEMENT_3D('',#450136,#129764,#129765);
#105205=AXIS2_PLACEMENT_3D('',#450184,#129767,#129768);
#105206=AXIS2_PLACEMENT_3D('',#450235,#129770,#129771);
#105207=AXIS2_PLACEMENT_3D('',#450254,#129773,#129774);
#105208=AXIS2_PLACEMENT_3D('',#450274,#129775,#129776);
#105209=AXIS2_PLACEMENT_3D('',#450287,#129778,#129779);
#105210=AXIS2_PLACEMENT_3D('',#450295,#129780,#129781);
#105211=AXIS2_PLACEMENT_3D('',#450319,#129783,#129784);
#105212=AXIS2_PLACEMENT_3D('',#450344,#129786,#129787);
#105213=AXIS2_PLACEMENT_3D('',#450368,#129789,#129790);
#105214=AXIS2_PLACEMENT_3D('',#450393,#129792,#129793);
#105215=AXIS2_PLACEMENT_3D('',#450418,#129795,#129796);
#105216=AXIS2_PLACEMENT_3D('',#450442,#129798,#129799);
#105217=AXIS2_PLACEMENT_3D('',#450453,#129801,#129802);
#105218=AXIS2_PLACEMENT_3D('',#450459,#129803,#129804);
#105219=AXIS2_PLACEMENT_3D('',#450464,#129806,#129807);
#105220=AXIS2_PLACEMENT_3D('',#450472,#129808,#129809);
#105221=AXIS2_PLACEMENT_3D('',#450496,#129811,#129812);
#105222=AXIS2_PLACEMENT_3D('',#450519,#129813,#129814);
#105223=AXIS2_PLACEMENT_3D('',#450567,#129816,#129817);
#105224=AXIS2_PLACEMENT_3D('',#450618,#129819,#129820);
#105225=AXIS2_PLACEMENT_3D('',#450669,#129822,#129823);
#105226=AXIS2_PLACEMENT_3D('',#450717,#129825,#129826);
#105227=AXIS2_PLACEMENT_3D('',#450768,#129828,#129829);
#105228=AXIS2_PLACEMENT_3D('',#450787,#129831,#129832);
#105229=AXIS2_PLACEMENT_3D('',#450807,#129833,#129834);
#105230=AXIS2_PLACEMENT_3D('',#450820,#129836,#129837);
#105231=AXIS2_PLACEMENT_3D('',#450828,#129838,#129839);
#105232=AXIS2_PLACEMENT_3D('',#450852,#129841,#129842);
#105233=AXIS2_PLACEMENT_3D('',#450877,#129844,#129845);
#105234=AXIS2_PLACEMENT_3D('',#450901,#129847,#129848);
#105235=AXIS2_PLACEMENT_3D('',#450926,#129850,#129851);
#105236=AXIS2_PLACEMENT_3D('',#450951,#129853,#129854);
#105237=AXIS2_PLACEMENT_3D('',#450975,#129856,#129857);
#105238=AXIS2_PLACEMENT_3D('',#450986,#129859,#129860);
#105239=AXIS2_PLACEMENT_3D('',#450992,#129861,#129862);
#105240=AXIS2_PLACEMENT_3D('',#450997,#129864,#129865);
#105241=AXIS2_PLACEMENT_3D('',#451005,#129866,#129867);
#105242=AXIS2_PLACEMENT_3D('',#451029,#129869,#129870);
#105243=AXIS2_PLACEMENT_3D('',#451052,#129871,#129872);
#105244=AXIS2_PLACEMENT_3D('',#451100,#129874,#129875);
#105245=AXIS2_PLACEMENT_3D('',#451151,#129877,#129878);
#105246=AXIS2_PLACEMENT_3D('',#451202,#129880,#129881);
#105247=AXIS2_PLACEMENT_3D('',#451250,#129883,#129884);
#105248=AXIS2_PLACEMENT_3D('',#451301,#129886,#129887);
#105249=AXIS2_PLACEMENT_3D('',#451320,#129889,#129890);
#105250=AXIS2_PLACEMENT_3D('',#451340,#129891,#129892);
#105251=AXIS2_PLACEMENT_3D('',#451353,#129894,#129895);
#105252=AXIS2_PLACEMENT_3D('',#451361,#129896,#129897);
#105253=AXIS2_PLACEMENT_3D('',#451385,#129899,#129900);
#105254=AXIS2_PLACEMENT_3D('',#451410,#129902,#129903);
#105255=AXIS2_PLACEMENT_3D('',#451434,#129905,#129906);
#105256=AXIS2_PLACEMENT_3D('',#451459,#129908,#129909);
#105257=AXIS2_PLACEMENT_3D('',#451484,#129911,#129912);
#105258=AXIS2_PLACEMENT_3D('',#451508,#129914,#129915);
#105259=AXIS2_PLACEMENT_3D('',#451519,#129917,#129918);
#105260=AXIS2_PLACEMENT_3D('',#451525,#129919,#129920);
#105261=AXIS2_PLACEMENT_3D('',#451527,#129921,#129922);
#105262=AXIS2_PLACEMENT_3D('',#451530,#129924,#129925);
#105263=AXIS2_PLACEMENT_3D('',#451531,#129926,#129927);
#105264=AXIS2_PLACEMENT_3D('',#451534,#129928,#129929);
#105265=AXIS2_PLACEMENT_3D('',#451535,#129930,#129931);
#105266=AXIS2_PLACEMENT_3D('',#451537,#129933,#129934);
#105267=AXIS2_PLACEMENT_3D('',#451539,#129935,#129936);
#105268=AXIS2_PLACEMENT_3D('',#452172,#129937,#129938);
#105269=AXIS2_PLACEMENT_3D('',#452831,#129939,#129940);
#105270=AXIS2_PLACEMENT_3D('',#452833,#129941,#129942);
#105271=AXIS2_PLACEMENT_3D('',#453309,#129943,#129944);
#105272=AXIS2_PLACEMENT_3D('',#453310,#129945,#129946);
#105273=AXIS2_PLACEMENT_3D('',#453311,#129947,#129948);
#105274=AXIS2_PLACEMENT_3D('',#453313,#129949,#129950);
#105275=AXIS2_PLACEMENT_3D('',#453316,#129952,#129953);
#105276=AXIS2_PLACEMENT_3D('',#453317,#129954,#129955);
#105277=AXIS2_PLACEMENT_3D('',#453320,#129957,#129958);
#105278=AXIS2_PLACEMENT_3D('',#453321,#129959,#129960);
#105279=AXIS2_PLACEMENT_3D('',#453324,#129962,#129963);
#105280=AXIS2_PLACEMENT_3D('',#453325,#129964,#129965);
#105281=AXIS2_PLACEMENT_3D('',#453327,#129966,#129967);
#105282=AXIS2_PLACEMENT_3D('',#453329,#129969,#129970);
#105283=AXIS2_PLACEMENT_3D('',#453332,#129972,#129973);
#105284=AXIS2_PLACEMENT_3D('',#453333,#129974,#129975);
#105285=AXIS2_PLACEMENT_3D('',#453335,#129976,#129977);
#105286=AXIS2_PLACEMENT_3D('',#453337,#129979,#129980);
#105287=AXIS2_PLACEMENT_3D('',#453339,#129981,#129982);
#105288=AXIS2_PLACEMENT_3D('',#453342,#129984,#129985);
#105289=AXIS2_PLACEMENT_3D('',#453343,#129986,#129987);
#105290=AXIS2_PLACEMENT_3D('',#453345,#129988,#129989);
#105291=AXIS2_PLACEMENT_3D('',#453348,#129991,#129992);
#105292=AXIS2_PLACEMENT_3D('',#453349,#129993,#129994);
#105293=AXIS2_PLACEMENT_3D('',#453351,#129995,#129996);
#105294=AXIS2_PLACEMENT_3D('',#453354,#129998,#129999);
#105295=AXIS2_PLACEMENT_3D('',#453355,#130000,#130001);
#105296=AXIS2_PLACEMENT_3D('',#453357,#130002,#130003);
#105297=AXIS2_PLACEMENT_3D('',#453360,#130005,#130006);
#105298=AXIS2_PLACEMENT_3D('',#453361,#130007,#130008);
#105299=AXIS2_PLACEMENT_3D('',#453363,#130009,#130010);
#105300=AXIS2_PLACEMENT_3D('',#453366,#130012,#130013);
#105301=AXIS2_PLACEMENT_3D('',#453367,#130014,#130015);
#105302=AXIS2_PLACEMENT_3D('',#453369,#130016,#130017);
#105303=AXIS2_PLACEMENT_3D('',#453372,#130019,#130020);
#105304=AXIS2_PLACEMENT_3D('',#453373,#130021,#130022);
#105305=AXIS2_PLACEMENT_3D('',#453375,#130023,#130024);
#105306=AXIS2_PLACEMENT_3D('',#453378,#130026,#130027);
#105307=AXIS2_PLACEMENT_3D('',#453379,#130028,#130029);
#105308=AXIS2_PLACEMENT_3D('',#453381,#130030,#130031);
#105309=AXIS2_PLACEMENT_3D('',#453384,#130033,#130034);
#105310=AXIS2_PLACEMENT_3D('',#453385,#130035,#130036);
#105311=AXIS2_PLACEMENT_3D('',#453387,#130037,#130038);
#105312=AXIS2_PLACEMENT_3D('',#453390,#130040,#130041);
#105313=AXIS2_PLACEMENT_3D('',#453391,#130042,#130043);
#105314=AXIS2_PLACEMENT_3D('',#453393,#130044,#130045);
#105315=AXIS2_PLACEMENT_3D('',#453396,#130047,#130048);
#105316=AXIS2_PLACEMENT_3D('',#453397,#130049,#130050);
#105317=AXIS2_PLACEMENT_3D('',#453399,#130051,#130052);
#105318=AXIS2_PLACEMENT_3D('',#453402,#130054,#130055);
#105319=AXIS2_PLACEMENT_3D('',#453403,#130056,#130057);
#105320=AXIS2_PLACEMENT_3D('',#453405,#130058,#130059);
#105321=AXIS2_PLACEMENT_3D('',#453408,#130061,#130062);
#105322=AXIS2_PLACEMENT_3D('',#453409,#130063,#130064);
#105323=AXIS2_PLACEMENT_3D('',#453411,#130065,#130066);
#105324=AXIS2_PLACEMENT_3D('',#453414,#130068,#130069);
#105325=AXIS2_PLACEMENT_3D('',#453415,#130070,#130071);
#105326=AXIS2_PLACEMENT_3D('',#453417,#130072,#130073);
#105327=AXIS2_PLACEMENT_3D('',#453420,#130075,#130076);
#105328=AXIS2_PLACEMENT_3D('',#453421,#130077,#130078);
#105329=AXIS2_PLACEMENT_3D('',#453423,#130079,#130080);
#105330=AXIS2_PLACEMENT_3D('',#453426,#130082,#130083);
#105331=AXIS2_PLACEMENT_3D('',#453427,#130084,#130085);
#105332=AXIS2_PLACEMENT_3D('',#453429,#130086,#130087);
#105333=AXIS2_PLACEMENT_3D('',#453432,#130089,#130090);
#105334=AXIS2_PLACEMENT_3D('',#453433,#130091,#130092);
#105335=AXIS2_PLACEMENT_3D('',#453435,#130093,#130094);
#105336=AXIS2_PLACEMENT_3D('',#453438,#130096,#130097);
#105337=AXIS2_PLACEMENT_3D('',#453439,#130098,#130099);
#105338=AXIS2_PLACEMENT_3D('',#453440,#130100,#130101);
#105339=AXIS2_PLACEMENT_3D('',#453441,#130102,#130103);
#105340=AXIS2_PLACEMENT_3D('',#453442,#130104,#130105);
#105341=AXIS2_PLACEMENT_3D('',#453443,#130106,#130107);
#105342=AXIS2_PLACEMENT_3D('',#453444,#130108,#130109);
#105343=AXIS2_PLACEMENT_3D('',#453445,#130110,#130111);
#105344=AXIS2_PLACEMENT_3D('',#453446,#130112,#130113);
#105345=AXIS2_PLACEMENT_3D('',#453447,#130114,#130115);
#105346=AXIS2_PLACEMENT_3D('',#453448,#130116,#130117);
#105347=AXIS2_PLACEMENT_3D('',#453449,#130118,#130119);
#105348=AXIS2_PLACEMENT_3D('',#453450,#130120,#130121);
#105349=AXIS2_PLACEMENT_3D('',#453451,#130122,#130123);
#105350=AXIS2_PLACEMENT_3D('',#453452,#130124,#130125);
#105351=AXIS2_PLACEMENT_3D('',#453453,#130126,#130127);
#105352=AXIS2_PLACEMENT_3D('',#453454,#130128,#130129);
#105353=AXIS2_PLACEMENT_3D('',#453455,#130130,#130131);
#105354=AXIS2_PLACEMENT_3D('',#453456,#130132,#130133);
#105355=AXIS2_PLACEMENT_3D('',#453457,#130134,#130135);
#105356=AXIS2_PLACEMENT_3D('',#453458,#130136,#130137);
#105357=AXIS2_PLACEMENT_3D('',#453459,#130138,#130139);
#105358=AXIS2_PLACEMENT_3D('',#453960,#130140,#130141);
#105359=AXIS2_PLACEMENT_3D('',#453961,#130142,#130143);
#105360=AXIS2_PLACEMENT_3D('',#454462,#130144,#130145);
#105361=AXIS2_PLACEMENT_3D('',#454463,#130146,#130147);
#105362=AXIS2_PLACEMENT_3D('',#454964,#130148,#130149);
#105363=AXIS2_PLACEMENT_3D('',#454965,#130150,#130151);
#105364=AXIS2_PLACEMENT_3D('',#454966,#130152,#130153);
#105365=AXIS2_PLACEMENT_3D('',#454982,#130155,#130156);
#105366=AXIS2_PLACEMENT_3D('',#454990,#130157,#130158);
#105367=AXIS2_PLACEMENT_3D('',#455038,#130160,#130161);
#105368=AXIS2_PLACEMENT_3D('',#455086,#130163,#130164);
#105369=AXIS2_PLACEMENT_3D('',#455140,#130166,#130167);
#105370=AXIS2_PLACEMENT_3D('',#455188,#130169,#130170);
#105371=AXIS2_PLACEMENT_3D('',#455236,#130172,#130173);
#105372=AXIS2_PLACEMENT_3D('',#455290,#130175,#130176);
#105373=AXIS2_PLACEMENT_3D('',#455338,#130178,#130179);
#105374=AXIS2_PLACEMENT_3D('',#455386,#130181,#130182);
#105375=AXIS2_PLACEMENT_3D('',#455434,#130184,#130185);
#105376=AXIS2_PLACEMENT_3D('',#455444,#130187,#130188);
#105377=AXIS2_PLACEMENT_3D('',#455445,#130189,#130190);
#105378=AXIS2_PLACEMENT_3D('',#455460,#130192,#130193);
#105379=AXIS2_PLACEMENT_3D('',#455471,#130194,#130195);
#105380=AXIS2_PLACEMENT_3D('',#455495,#130197,#130198);
#105381=AXIS2_PLACEMENT_3D('',#455519,#130200,#130201);
#105382=AXIS2_PLACEMENT_3D('',#455544,#130203,#130204);
#105383=AXIS2_PLACEMENT_3D('',#455569,#130206,#130207);
#105384=AXIS2_PLACEMENT_3D('',#455593,#130209,#130210);
#105385=AXIS2_PLACEMENT_3D('',#455618,#130212,#130213);
#105386=AXIS2_PLACEMENT_3D('',#455643,#130215,#130216);
#105387=AXIS2_PLACEMENT_3D('',#455667,#130218,#130219);
#105388=AXIS2_PLACEMENT_3D('',#455683,#130221,#130222);
#105389=AXIS2_PLACEMENT_3D('',#455691,#130223,#130224);
#105390=AXIS2_PLACEMENT_3D('',#455739,#130226,#130227);
#105391=AXIS2_PLACEMENT_3D('',#455787,#130229,#130230);
#105392=AXIS2_PLACEMENT_3D('',#455841,#130232,#130233);
#105393=AXIS2_PLACEMENT_3D('',#455889,#130235,#130236);
#105394=AXIS2_PLACEMENT_3D('',#455901,#130238,#130239);
#105395=AXIS2_PLACEMENT_3D('',#455906,#130240,#130241);
#105396=AXIS2_PLACEMENT_3D('',#455931,#130243,#130244);
#105397=AXIS2_PLACEMENT_3D('',#455956,#130246,#130247);
#105398=AXIS2_PLACEMENT_3D('',#455981,#130249,#130250);
#105399=AXIS2_PLACEMENT_3D('',#456365,#130252,#130253);
#105400=AXIS2_PLACEMENT_3D('',#456367,#130254,#130255);
#105401=AXIS2_PLACEMENT_3D('',#456723,#130256,#130257);
#105402=AXIS2_PLACEMENT_3D('',#456724,#130258,#130259);
#105403=AXIS2_PLACEMENT_3D('',#456726,#130260,#130261);
#105404=AXIS2_PLACEMENT_3D('',#456727,#130262,#130263);
#105405=AXIS2_PLACEMENT_3D('',#456728,#130264,#130265);
#105406=AXIS2_PLACEMENT_3D('',#456731,#130266,#130267);
#105407=AXIS2_PLACEMENT_3D('',#456774,#130268,#130269);
#105408=AXIS2_PLACEMENT_3D('',#457228,#130270,#130271);
#105409=AXIS2_PLACEMENT_3D('',#457230,#130272,#130273);
#105410=AXIS2_PLACEMENT_3D('',#457682,#130274,#130275);
#105411=AXIS2_PLACEMENT_3D('',#457685,#130276,#130277);
#105412=AXIS2_PLACEMENT_3D('',#457686,#130278,#130279);
#105413=AXIS2_PLACEMENT_3D('',#457689,#130281,#130282);
#105414=AXIS2_PLACEMENT_3D('',#457690,#130283,#130284);
#105415=AXIS2_PLACEMENT_3D('',#457692,#130285,#130286);
#105416=AXIS2_PLACEMENT_3D('',#457694,#130288,#130289);
#105417=AXIS2_PLACEMENT_3D('',#457695,#130290,#130291);
#105418=AXIS2_PLACEMENT_3D('',#457696,#130292,#130293);
#105419=AXIS2_PLACEMENT_3D('',#457698,#130295,#130296);
#105420=AXIS2_PLACEMENT_3D('',#457699,#130297,#130298);
#105421=AXIS2_PLACEMENT_3D('',#457701,#130299,#130300);
#105422=AXIS2_PLACEMENT_3D('',#457704,#130302,#130303);
#105423=AXIS2_PLACEMENT_3D('',#457705,#130304,#130305);
#105424=AXIS2_PLACEMENT_3D('',#457707,#130306,#130307);
#105425=AXIS2_PLACEMENT_3D('',#457709,#130309,#130310);
#105426=AXIS2_PLACEMENT_3D('',#457711,#130311,#130312);
#105427=AXIS2_PLACEMENT_3D('',#457713,#130314,#130315);
#105428=AXIS2_PLACEMENT_3D('',#457714,#130316,#130317);
#105429=AXIS2_PLACEMENT_3D('',#457715,#130318,#130319);
#105430=AXIS2_PLACEMENT_3D('',#457716,#130320,#130321);
#105431=AXIS2_PLACEMENT_3D('',#457717,#130322,#130323);
#105432=AXIS2_PLACEMENT_3D('',#457718,#130324,#130325);
#105433=AXIS2_PLACEMENT_3D('',#457720,#130326,#130327);
#105434=AXIS2_PLACEMENT_3D('',#457722,#130328,#130329);
#105435=AXIS2_PLACEMENT_3D('',#457723,#130330,#130331);
#105436=AXIS2_PLACEMENT_3D('',#457725,#130332,#130333);
#105437=AXIS2_PLACEMENT_3D('',#457727,#130335,#130336);
#105438=AXIS2_PLACEMENT_3D('',#457729,#130337,#130338);
#105439=AXIS2_PLACEMENT_3D('',#457731,#130340,#130341);
#105440=AXIS2_PLACEMENT_3D('',#457732,#130342,#130343);
#105441=AXIS2_PLACEMENT_3D('',#457733,#130344,#130345);
#105442=AXIS2_PLACEMENT_3D('',#457749,#130347,#130348);
#105443=AXIS2_PLACEMENT_3D('',#457757,#130349,#130350);
#105444=AXIS2_PLACEMENT_3D('',#457805,#130352,#130353);
#105445=AXIS2_PLACEMENT_3D('',#457853,#130355,#130356);
#105446=AXIS2_PLACEMENT_3D('',#457907,#130358,#130359);
#105447=AXIS2_PLACEMENT_3D('',#457955,#130361,#130362);
#105448=AXIS2_PLACEMENT_3D('',#458003,#130364,#130365);
#105449=AXIS2_PLACEMENT_3D('',#458015,#130367,#130368);
#105450=AXIS2_PLACEMENT_3D('',#458020,#130369,#130370);
#105451=AXIS2_PLACEMENT_3D('',#458045,#130372,#130373);
#105452=AXIS2_PLACEMENT_3D('',#458069,#130375,#130376);
#105453=AXIS2_PLACEMENT_3D('',#458094,#130378,#130379);
#105454=AXIS2_PLACEMENT_3D('',#458119,#130381,#130382);
#105455=AXIS2_PLACEMENT_3D('',#458529,#130384,#130385);
#105456=AXIS2_PLACEMENT_3D('',#458531,#130386,#130387);
#105457=AXIS2_PLACEMENT_3D('',#458555,#130388,#130389);
#105458=AXIS2_PLACEMENT_3D('',#458556,#130390,#130391);
#105459=AXIS2_PLACEMENT_3D('',#458909,#130392,#130393);
#105460=AXIS2_PLACEMENT_3D('',#458911,#130394,#130395);
#105461=AXIS2_PLACEMENT_3D('',#458912,#130396,#130397);
#105462=AXIS2_PLACEMENT_3D('',#458913,#130398,#130399);
#105463=AXIS2_PLACEMENT_3D('',#458914,#130400,#130401);
#105464=AXIS2_PLACEMENT_3D('',#458916,#130402,#130403);
#105465=AXIS2_PLACEMENT_3D('',#458917,#130404,#130405);
#105466=AXIS2_PLACEMENT_3D('',#458918,#130406,#130407);
#105467=AXIS2_PLACEMENT_3D('',#458920,#130408,#130409);
#105468=AXIS2_PLACEMENT_3D('',#458924,#130411,#130412);
#105469=AXIS2_PLACEMENT_3D('',#458925,#130413,#130414);
#105470=AXIS2_PLACEMENT_3D('',#458926,#130415,#130416);
#105471=AXIS2_PLACEMENT_3D('',#458928,#130417,#130418);
#105472=AXIS2_PLACEMENT_3D('',#458930,#130420,#130421);
#105473=AXIS2_PLACEMENT_3D('',#458932,#130422,#130423);
#105474=AXIS2_PLACEMENT_3D('',#458934,#130425,#130426);
#105475=AXIS2_PLACEMENT_3D('',#458936,#130427,#130428);
#105476=AXIS2_PLACEMENT_3D('',#458939,#130430,#130431);
#105477=AXIS2_PLACEMENT_3D('',#458940,#130432,#130433);
#105478=AXIS2_PLACEMENT_3D('',#458943,#130435,#130436);
#105479=AXIS2_PLACEMENT_3D('',#458944,#130437,#130438);
#105480=AXIS2_PLACEMENT_3D('',#458947,#130439,#130440);
#105481=AXIS2_PLACEMENT_3D('',#458948,#130441,#130442);
#105482=AXIS2_PLACEMENT_3D('',#458950,#130444,#130445);
#105483=AXIS2_PLACEMENT_3D('',#458952,#130447,#130448);
#105484=AXIS2_PLACEMENT_3D('',#458954,#130449,#130450);
#105485=AXIS2_PLACEMENT_3D('',#458956,#130452,#130453);
#105486=AXIS2_PLACEMENT_3D('',#458969,#130460,#130461);
#105487=AXIS2_PLACEMENT_3D('',#458982,#130468,#130469);
#105488=AXIS2_PLACEMENT_3D('',#458985,#130472,#130473);
#105489=AXIS2_PLACEMENT_3D('',#458987,#130475,#130476);
#105490=AXIS2_PLACEMENT_3D('',#458989,#130478,#130479);
#105491=AXIS2_PLACEMENT_3D('',#458991,#130481,#130482);
#105492=AXIS2_PLACEMENT_3D('',#458993,#130484,#130485);
#105493=AXIS2_PLACEMENT_3D('',#458994,#130486,#130487);
#105494=AXIS2_PLACEMENT_3D('',#458995,#130488,#130489);
#105495=AXIS2_PLACEMENT_3D('',#458996,#130490,#130491);
#105496=AXIS2_PLACEMENT_3D('',#458998,#130492,#130493);
#105497=AXIS2_PLACEMENT_3D('',#459001,#130495,#130496);
#105498=AXIS2_PLACEMENT_3D('',#459002,#130497,#130498);
#105499=AXIS2_PLACEMENT_3D('',#459004,#130499,#130500);
#105500=AXIS2_PLACEMENT_3D('',#459007,#130502,#130503);
#105501=AXIS2_PLACEMENT_3D('',#459008,#130504,#130505);
#105502=AXIS2_PLACEMENT_3D('',#459010,#130506,#130507);
#105503=AXIS2_PLACEMENT_3D('',#459013,#130509,#130510);
#105504=AXIS2_PLACEMENT_3D('',#459014,#130511,#130512);
#105505=AXIS2_PLACEMENT_3D('',#459016,#130513,#130514);
#105506=AXIS2_PLACEMENT_3D('',#459019,#130516,#130517);
#105507=AXIS2_PLACEMENT_3D('',#459020,#130518,#130519);
#105508=AXIS2_PLACEMENT_3D('',#459022,#130520,#130521);
#105509=AXIS2_PLACEMENT_3D('',#459025,#130523,#130524);
#105510=AXIS2_PLACEMENT_3D('',#459026,#130525,#130526);
#105511=AXIS2_PLACEMENT_3D('',#459029,#130527,#130528);
#105512=AXIS2_PLACEMENT_3D('',#459033,#130530,#130531);
#105513=AXIS2_PLACEMENT_3D('',#459035,#130533,#130534);
#105514=AXIS2_PLACEMENT_3D('',#459044,#130539,#130540);
#105515=AXIS2_PLACEMENT_3D('',#459053,#130545,#130546);
#105516=AXIS2_PLACEMENT_3D('',#459067,#130554,#130555);
#105517=AXIS2_PLACEMENT_3D('',#459076,#130560,#130561);
#105518=AXIS2_PLACEMENT_3D('',#459090,#130569,#130570);
#105519=AXIS2_PLACEMENT_3D('',#459099,#130575,#130576);
#105520=AXIS2_PLACEMENT_3D('',#459108,#130581,#130582);
#105521=AXIS2_PLACEMENT_3D('',#459111,#130585,#130586);
#105522=AXIS2_PLACEMENT_3D('',#459114,#130589,#130590);
#105523=AXIS2_PLACEMENT_3D('',#459115,#130591,#130592);
#105524=AXIS2_PLACEMENT_3D('',#459116,#130593,#130594);
#105525=AXIS2_PLACEMENT_3D('',#459118,#130596,#130597);
#105526=AXIS2_PLACEMENT_3D('',#459120,#130599,#130600);
#105527=AXIS2_PLACEMENT_3D('',#459123,#130603,#130604);
#105528=AXIS2_PLACEMENT_3D('',#459126,#130607,#130608);
#105529=AXIS2_PLACEMENT_3D('',#459128,#130610,#130611);
#105530=AXIS2_PLACEMENT_3D('',#459130,#130613,#130614);
#105531=AXIS2_PLACEMENT_3D('',#459132,#130616,#130617);
#105532=AXIS2_PLACEMENT_3D('',#459135,#130620,#130621);
#105533=AXIS2_PLACEMENT_3D('',#459137,#130623,#130624);
#105534=AXIS2_PLACEMENT_3D('',#459139,#130626,#130627);
#105535=AXIS2_PLACEMENT_3D('',#459141,#130629,#130630);
#105536=AXIS2_PLACEMENT_3D('',#459143,#130632,#130633);
#105537=AXIS2_PLACEMENT_3D('',#459145,#130635,#130636);
#105538=AXIS2_PLACEMENT_3D('',#459147,#130638,#130639);
#105539=AXIS2_PLACEMENT_3D('',#459149,#130641,#130642);
#105540=AXIS2_PLACEMENT_3D('',#459151,#130644,#130645);
#105541=AXIS2_PLACEMENT_3D('',#459153,#130647,#130648);
#105542=AXIS2_PLACEMENT_3D('',#459155,#130650,#130651);
#105543=AXIS2_PLACEMENT_3D('',#459157,#130653,#130654);
#105544=AXIS2_PLACEMENT_3D('',#459159,#130656,#130657);
#105545=AXIS2_PLACEMENT_3D('',#459161,#130659,#130660);
#105546=AXIS2_PLACEMENT_3D('',#459162,#130661,#130662);
#105547=AXIS2_PLACEMENT_3D('',#459163,#130663,#130664);
#105548=AXIS2_PLACEMENT_3D('',#459164,#130665,#130666);
#105549=AXIS2_PLACEMENT_3D('',#459165,#130667,#130668);
#105550=AXIS2_PLACEMENT_3D('',#459166,#130669,#130670);
#105551=AXIS2_PLACEMENT_3D('',#459167,#130671,#130672);
#105552=AXIS2_PLACEMENT_3D('',#459168,#130673,#130674);
#105553=AXIS2_PLACEMENT_3D('',#459169,#130675,#130676);
#105554=AXIS2_PLACEMENT_3D('',#459170,#130677,#130678);
#105555=AXIS2_PLACEMENT_3D('',#459171,#130679,#130680);
#105556=AXIS2_PLACEMENT_3D('',#459172,#130681,#130682);
#105557=AXIS2_PLACEMENT_3D('',#459173,#130683,#130684);
#105558=AXIS2_PLACEMENT_3D('',#459174,#130685,#130686);
#105559=AXIS2_PLACEMENT_3D('',#459175,#130687,#130688);
#105560=AXIS2_PLACEMENT_3D('',#459176,#130689,#130690);
#105561=AXIS2_PLACEMENT_3D('',#459177,#130691,#130692);
#105562=AXIS2_PLACEMENT_3D('',#459178,#130693,#130694);
#105563=AXIS2_PLACEMENT_3D('',#459179,#130695,#130696);
#105564=AXIS2_PLACEMENT_3D('',#459180,#130697,#130698);
#105565=AXIS2_PLACEMENT_3D('',#459181,#130699,#130700);
#105566=AXIS2_PLACEMENT_3D('',#459182,#130701,#130702);
#105567=AXIS2_PLACEMENT_3D('',#459183,#130703,#130704);
#105568=AXIS2_PLACEMENT_3D('',#459184,#130705,#130706);
#105569=AXIS2_PLACEMENT_3D('',#459185,#130707,#130708);
#105570=AXIS2_PLACEMENT_3D('',#459186,#130709,#130710);
#105571=AXIS2_PLACEMENT_3D('',#459187,#130711,#130712);
#105572=AXIS2_PLACEMENT_3D('',#459188,#130713,#130714);
#105573=AXIS2_PLACEMENT_3D('',#459189,#130715,#130716);
#105574=AXIS2_PLACEMENT_3D('',#459190,#130717,#130718);
#105575=DIRECTION('axis',(0.,0.,1.));
#105576=DIRECTION('refdir',(1.,0.,0.));
#105577=DIRECTION('axis',(0.,0.,1.));
#105578=DIRECTION('refdir',(1.,0.,0.));
#105579=DIRECTION('axis',(0.,0.,1.));
#105580=DIRECTION('refdir',(1.,0.,0.));
#105581=DIRECTION('center_axis',(4.93038065763132E-32,1.97215226305253E-31,
-1.));
#105582=DIRECTION('ref_axis',(-0.348448562526685,0.937327903816528,1.67675494144795E-31));
#105583=DIRECTION('',(4.93038065763132E-32,1.97215226305253E-31,-1.));
#105584=DIRECTION('center_axis',(4.93038065763132E-32,1.97215226305253E-31,
-1.));
#105585=DIRECTION('ref_axis',(1.,0.,4.93038065763132E-32));
#105586=DIRECTION('center_axis',(4.93038065763132E-32,1.97215226305253E-31,
-1.));
#105587=DIRECTION('ref_axis',(-0.348448562526685,0.937327903816528,1.67675494144795E-31));
#105588=DIRECTION('',(4.93038065763132E-32,1.97215226305253E-31,-1.));
#105589=DIRECTION('center_axis',(4.93038065763132E-32,1.97215226305253E-31,
-1.));
#105590=DIRECTION('ref_axis',(-0.348448562526685,0.937327903816528,1.67675494144795E-31));
#105591=DIRECTION('',(4.93038065763132E-32,1.97215226305253E-31,-1.));
#105592=DIRECTION('center_axis',(4.93038065763132E-32,1.97215226305253E-31,
-1.));
#105593=DIRECTION('ref_axis',(-0.348448562526685,0.937327903816528,1.67675494144795E-31));
#105594=DIRECTION('',(4.93038065763132E-32,1.97215226305253E-31,-1.));
#105595=DIRECTION('center_axis',(4.93038065763132E-32,1.97215226305253E-31,
-1.));
#105596=DIRECTION('ref_axis',(1.,0.,4.93038065763132E-32));
#105597=DIRECTION('center_axis',(4.93038065763132E-32,1.97215226305253E-31,
-1.));
#105598=DIRECTION('ref_axis',(-0.348448196221629,0.937328039989145,1.67675539060342E-31));
#105599=DIRECTION('',(4.93038065763132E-32,1.97215226305253E-31,-1.));
#105600=DIRECTION('center_axis',(4.93038065763132E-32,1.97215226305253E-31,
-1.));
#105601=DIRECTION('ref_axis',(1.,0.,4.93038065763132E-32));
#105602=DIRECTION('center_axis',(4.93038065763132E-32,1.97215226305253E-31,
-1.));
#105603=DIRECTION('ref_axis',(-0.348448196221629,0.937328039989145,1.67675539060342E-31));
#105604=DIRECTION('',(4.93038065763132E-32,1.97215226305253E-31,-1.));
#105605=DIRECTION('center_axis',(4.93038065763132E-32,1.97215226305253E-31,
-1.));
#105606=DIRECTION('ref_axis',(-0.348448196221629,0.937328039989145,1.67675539060342E-31));
#105607=DIRECTION('',(4.93038065763132E-32,1.97215226305253E-31,-1.));
#105608=DIRECTION('center_axis',(4.93038065763132E-32,1.97215226305253E-31,
-1.));
#105609=DIRECTION('ref_axis',(-0.348448196221629,0.937328039989145,1.67675539060342E-31));
#105610=DIRECTION('',(4.93038065763132E-32,1.97215226305253E-31,-1.));
#105611=DIRECTION('center_axis',(4.93038065763132E-32,1.97215226305253E-31,
-1.));
#105612=DIRECTION('ref_axis',(1.,0.,4.93038065763132E-32));
#105613=DIRECTION('center_axis',(4.93038065763132E-32,1.97215226305253E-31,
-1.));
#105614=DIRECTION('ref_axis',(-0.608873383780016,-0.793267421822095,-1.86464189658584E-31));
#105615=DIRECTION('',(4.93038065763132E-32,1.97215226305253E-31,-1.));
#105616=DIRECTION('center_axis',(-4.93038065763132E-32,-1.97215226305253E-31,
1.));
#105617=DIRECTION('ref_axis',(1.,5.75617900000082E-15,4.93038065763144E-32));
#105618=DIRECTION('center_axis',(4.93038065763132E-32,1.97215226305253E-31,
-1.));
#105619=DIRECTION('ref_axis',(-0.608873383780016,-0.793267421822095,-1.86464189658584E-31));
#105620=DIRECTION('',(4.93038065763132E-32,1.97215226305253E-31,-1.));
#105621=DIRECTION('center_axis',(4.93038065763132E-32,1.97215226305253E-31,
-1.));
#105622=DIRECTION('ref_axis',(-0.608873383780016,-0.793267421822095,-1.86464189658584E-31));
#105623=DIRECTION('',(4.93038065763132E-32,1.97215226305253E-31,-1.));
#105624=DIRECTION('center_axis',(4.93038065763132E-32,1.97215226305253E-31,
-1.));
#105625=DIRECTION('ref_axis',(-0.608873383780016,-0.793267421822095,-1.86464189658584E-31));
#105626=DIRECTION('',(4.93038065763132E-32,1.97215226305253E-31,-1.));
#105627=DIRECTION('center_axis',(4.93038065763132E-32,1.97215226305253E-31,
-1.));
#105628=DIRECTION('ref_axis',(1.,5.75617900000082E-15,4.93038065763144E-32));
#105629=DIRECTION('center_axis',(4.93038065763132E-32,1.97215226305253E-31,
-1.));
#105630=DIRECTION('ref_axis',(-0.608873392866957,-0.793267414847402,-1.86464188731089E-31));
#105631=DIRECTION('',(4.93038065763132E-32,1.97215226305253E-31,-1.));
#105632=DIRECTION('center_axis',(-4.93038065763132E-32,-1.97215226305253E-31,
1.));
#105633=DIRECTION('ref_axis',(1.,8.63426850000124E-15,4.93038065763149E-32));
#105634=DIRECTION('center_axis',(4.93038065763132E-32,1.97215226305253E-31,
-1.));
#105635=DIRECTION('ref_axis',(-0.608873392866957,-0.793267414847402,-1.86464188731089E-31));
#105636=DIRECTION('',(4.93038065763132E-32,1.97215226305253E-31,-1.));
#105637=DIRECTION('center_axis',(4.93038065763132E-32,1.97215226305253E-31,
-1.));
#105638=DIRECTION('ref_axis',(-0.608873392866957,-0.793267414847402,-1.86464188731089E-31));
#105639=DIRECTION('',(4.93038065763132E-32,1.97215226305253E-31,-1.));
#105640=DIRECTION('center_axis',(4.93038065763132E-32,1.97215226305253E-31,
-1.));
#105641=DIRECTION('ref_axis',(-0.608873392866957,-0.793267414847402,-1.86464188731089E-31));
#105642=DIRECTION('',(4.93038065763132E-32,1.97215226305253E-31,-1.));
#105643=DIRECTION('center_axis',(4.93038065763132E-32,1.97215226305253E-31,
-1.));
#105644=DIRECTION('ref_axis',(1.,8.63426850000124E-15,4.93038065763149E-32));
#105645=DIRECTION('center_axis',(4.93038065763132E-32,1.97215226305253E-31,
-1.));
#105646=DIRECTION('ref_axis',(-0.608873392866957,-0.793267414847402,-1.86464188731089E-31));
#105647=DIRECTION('center_axis',(4.93038065763132E-32,1.97215226305253E-31,
-1.));
#105648=DIRECTION('ref_axis',(-0.608873383780016,-0.793267421822095,-1.86464189658584E-31));
#105649=DIRECTION('center_axis',(4.93038065763132E-32,1.97215226305253E-31,
-1.));
#105650=DIRECTION('ref_axis',(-0.348448196221629,0.937328039989145,1.67675539060342E-31));
#105651=DIRECTION('center_axis',(4.93038065763132E-32,1.97215226305253E-31,
-1.));
#105652=DIRECTION('ref_axis',(-0.348448562526685,0.937327903816528,1.67675494144795E-31));
#105653=DIRECTION('center_axis',(4.93038065763132E-32,1.97215226305253E-31,
-1.));
#105654=DIRECTION('ref_axis',(-1.,0.,-4.93038065763132E-32));
#105655=DIRECTION('center_axis',(4.93038065763132E-32,1.97215226305253E-31,
-1.));
#105656=DIRECTION('ref_axis',(0.731712168750195,0.681613748469679,1.70500804894814E-31));
#105657=DIRECTION('',(0.909673749800079,-0.415323571356916,-3.70577535073674E-32));
#105658=DIRECTION('center_axis',(-4.93038065763132E-32,-1.97215226305253E-31,
1.));
#105659=DIRECTION('ref_axis',(-0.415323571356918,-0.909673749800078,-1.99878547459536E-31));
#105660=DIRECTION('',(-0.909673749800079,-0.415323571356916,-1.26758510722753E-31));
#105661=DIRECTION('center_axis',(4.93038065763132E-32,1.97215226305253E-31,
-1.));
#105662=DIRECTION('ref_axis',(0.731712168750193,-0.681613748469681,-9.83484144196257E-32));
#105663=DIRECTION('center_axis',(4.93038065763132E-32,1.97215226305253E-31,
-1.));
#105664=DIRECTION('ref_axis',(-1.,0.,-4.93038065763132E-32));
#105665=DIRECTION('center_axis',(4.93038065763132E-32,1.97215226305253E-31,
-1.));
#105666=DIRECTION('ref_axis',(-1.,0.,-4.93038065763132E-32));
#105667=DIRECTION('center_axis',(4.93038065763132E-32,1.97215226305253E-31,
-1.));
#105668=DIRECTION('ref_axis',(-0.731712168808585,-0.681613748406997,-1.70500804885331E-31));
#105669=DIRECTION('',(-0.909673749731055,0.415323571508098,3.70577535405859E-32));
#105670=DIRECTION('center_axis',(-4.93038065763132E-32,-1.97215226305253E-31,
1.));
#105671=DIRECTION('ref_axis',(0.415323571508097,0.909673749731055,1.99878547453377E-31));
#105672=DIRECTION('',(0.909673749731055,0.415323571508098,1.26758510749165E-31));
#105673=DIRECTION('center_axis',(4.93038065763132E-32,1.97215226305253E-31,
-1.));
#105674=DIRECTION('ref_axis',(-0.731712168808585,0.681613748406997,9.83484144043845E-32));
#105675=DIRECTION('center_axis',(4.93038065763132E-32,1.97215226305253E-31,
-1.));
#105676=DIRECTION('ref_axis',(-1.,0.,-4.93038065763132E-32));
#105677=DIRECTION('center_axis',(4.93038065763132E-32,1.97215226305253E-31,
-1.));
#105678=DIRECTION('ref_axis',(-1.,0.,-4.93038065763132E-32));
#105679=DIRECTION('center_axis',(4.93038065763132E-32,1.97215226305253E-31,
-1.));
#105680=DIRECTION('ref_axis',(-1.,0.,-4.93038065763132E-32));
#105681=DIRECTION('center_axis',(-4.93038065763132E-32,-1.97215226305253E-31,
1.));
#105682=DIRECTION('ref_axis',(-1.,0.,-4.93038065763132E-32));
#105683=DIRECTION('',(-0.707106781186547,8.65956056235491E-17,0.707106781186548));
#105684=DIRECTION('center_axis',(4.93038065763132E-32,1.97215226305253E-31,
-1.));
#105685=DIRECTION('ref_axis',(-1.,0.,-4.93038065763132E-32));
#105686=DIRECTION('center_axis',(-4.93038065763132E-32,-1.97215226305253E-31,
1.));
#105687=DIRECTION('ref_axis',(-1.,0.,-4.93038065763132E-32));
#105688=DIRECTION('',(4.93038065763132E-32,1.97215226305253E-31,-1.));
#105689=DIRECTION('center_axis',(4.93038065763132E-32,1.97215226305253E-31,
-1.));
#105690=DIRECTION('ref_axis',(-1.,0.,-4.93038065763132E-32));
#105691=DIRECTION('center_axis',(4.93038065763132E-32,1.97215226305253E-31,
-1.));
#105692=DIRECTION('ref_axis',(-1.,0.,-4.93038065763132E-32));
#105693=DIRECTION('center_axis',(4.93038065763132E-32,1.97215226305253E-31,
-1.));
#105694=DIRECTION('ref_axis',(1.,0.,4.93038065763132E-32));
#105695=DIRECTION('center_axis',(-4.93038065763132E-32,-1.97215226305253E-31,
1.));
#105696=DIRECTION('ref_axis',(1.,0.,4.93038065763132E-32));
#105697=DIRECTION('center_axis',(4.93038065763132E-32,1.97215226305253E-31,
-1.));
#105698=DIRECTION('ref_axis',(1.,0.,4.93038065763132E-32));
#105699=DIRECTION('',(0.707106781186547,8.65956056235494E-17,-0.707106781186548));
#105700=DIRECTION('center_axis',(-4.93038065763132E-32,-1.97215226305253E-31,
1.));
#105701=DIRECTION('ref_axis',(1.,0.,4.93038065763132E-32));
#105702=DIRECTION('center_axis',(4.93038065763132E-32,1.97215226305253E-31,
-1.));
#105703=DIRECTION('ref_axis',(1.,0.,4.93038065763132E-32));
#105704=DIRECTION('center_axis',(4.93038065763132E-32,1.97215226305253E-31,
-1.));
#105705=DIRECTION('ref_axis',(-1.,0.,-4.93038065763132E-32));
#105706=DIRECTION('',(-4.93038065763132E-32,-1.97215226305253E-31,1.));
#105707=DIRECTION('',(4.93038065763132E-32,1.97215226305253E-31,-1.));
#105708=DIRECTION('center_axis',(-4.93038065763132E-32,-1.97215226305253E-31,
1.));
#105709=DIRECTION('ref_axis',(-1.,0.,-4.93038065763132E-32));
#105710=DIRECTION('',(-4.93038065763132E-32,-1.97215226305253E-31,1.));
#105711=DIRECTION('',(4.93038065763132E-32,1.97215226305253E-31,-1.));
#105712=DIRECTION('center_axis',(-4.93038065763132E-32,-1.97215226305253E-31,
1.));
#105713=DIRECTION('ref_axis',(-1.,0.,-4.93038065763132E-32));
#105714=DIRECTION('',(-4.93038065763132E-32,-1.97215226305253E-31,1.));
#105715=DIRECTION('center_axis',(-4.93038065763132E-32,-1.97215226305253E-31,
1.));
#105716=DIRECTION('ref_axis',(1.,0.,4.93038065763132E-32));
#105717=DIRECTION('center_axis',(4.93038065763132E-32,1.97215226305253E-31,
-1.));
#105718=DIRECTION('ref_axis',(1.,0.,4.93038065763132E-32));
#105719=DIRECTION('center_axis',(4.93038065763132E-32,1.97215226305253E-31,
-1.));
#105720=DIRECTION('ref_axis',(1.,0.,4.93038065763132E-32));
#105721=DIRECTION('center_axis',(-4.93038065763132E-32,-1.97215226305253E-31,
1.));
#105722=DIRECTION('ref_axis',(1.,0.,4.93038065763132E-32));
#105723=DIRECTION('',(0.707106781186539,-8.65956056235485E-17,0.707106781186556));
#105724=DIRECTION('center_axis',(4.93038065763132E-32,1.97215226305253E-31,
-1.));
#105725=DIRECTION('ref_axis',(1.,0.,4.93038065763132E-32));
#105726=DIRECTION('center_axis',(-4.93038065763132E-32,-1.97215226305253E-31,
1.));
#105727=DIRECTION('ref_axis',(1.,0.,4.93038065763132E-32));
#105728=DIRECTION('center_axis',(4.93038065763132E-32,1.97215226305253E-31,
-1.));
#105729=DIRECTION('ref_axis',(-1.,0.,-4.93038065763132E-32));
#105730=DIRECTION('center_axis',(4.93038065763132E-32,1.97215226305253E-31,
-1.));
#105731=DIRECTION('ref_axis',(-1.,0.,-4.93038065763132E-32));
#105732=DIRECTION('',(-4.93038065763132E-32,-1.97215226305253E-31,1.));
#105733=DIRECTION('center_axis',(-4.93038065763132E-32,-1.97215226305253E-31,
1.));
#105734=DIRECTION('ref_axis',(1.,0.,4.93038065763132E-32));
#105735=DIRECTION('center_axis',(-4.93038065763132E-32,-1.97215226305253E-31,
1.));
#105736=DIRECTION('ref_axis',(1.,0.,4.93038065763132E-32));
#105737=DIRECTION('center_axis',(4.93038065763132E-32,1.97215226305253E-31,
-1.));
#105738=DIRECTION('ref_axis',(1.,0.,4.93038065763132E-32));
#105739=DIRECTION('center_axis',(-4.93038065763132E-32,-1.97215226305253E-31,
1.));
#105740=DIRECTION('ref_axis',(1.,0.,4.93038065763132E-32));
#105741=DIRECTION('',(-0.707106781186555,8.65956056235504E-17,-0.70710678118654));
#105742=DIRECTION('center_axis',(4.93038065763132E-32,1.97215226305253E-31,
-1.));
#105743=DIRECTION('ref_axis',(1.,0.,4.93038065763132E-32));
#105744=DIRECTION('center_axis',(4.93038065763132E-32,1.97215226305253E-31,
-1.));
#105745=DIRECTION('ref_axis',(-1.,0.,-4.93038065763132E-32));
#105746=DIRECTION('center_axis',(-4.93038065763132E-32,-1.97215226305253E-31,
1.));
#105747=DIRECTION('ref_axis',(-1.,0.,-4.93038065763132E-32));
#105748=DIRECTION('center_axis',(-4.93038065763132E-32,-1.97215226305253E-31,
1.));
#105749=DIRECTION('ref_axis',(1.,0.,4.93038065763132E-32));
#105750=DIRECTION('',(-4.93038065763132E-32,-1.97215226305253E-31,1.));
#105751=DIRECTION('center_axis',(-4.93038065763132E-32,-1.97215226305253E-31,
1.));
#105752=DIRECTION('ref_axis',(1.,0.,4.93038065763132E-32));
#105753=DIRECTION('center_axis',(-4.93038065763132E-32,-1.97215226305253E-31,
1.));
#105754=DIRECTION('ref_axis',(-1.,0.,-4.93038065763132E-32));
#105755=DIRECTION('',(-0.707106781186555,-8.65956056235501E-17,-0.70710678118654));
#105756=DIRECTION('center_axis',(4.93038065763132E-32,1.97215226305253E-31,
-1.));
#105757=DIRECTION('ref_axis',(0.731712168750192,-0.681613748469681,-9.83484144196258E-32));
#105758=DIRECTION('',(-0.293678113693067,0.643236477151022,0.707106781186565));
#105759=DIRECTION('center_axis',(-4.93038065763132E-32,-1.97215226305253E-31,
1.));
#105760=DIRECTION('ref_axis',(0.731712168750192,-0.681613748469682,-9.83484144196259E-32));
#105761=DIRECTION('center_axis',(-0.293678113693089,0.643236477151028,-0.707106781186551));
#105762=DIRECTION('ref_axis',(-0.923516686410398,2.4980018054066E-16,0.383558248407668));
#105763=DIRECTION('',(-0.29367811369309,0.643236477151034,0.707106781186544));
#105764=DIRECTION('',(0.909673749800079,0.415323571356916,1.26758510722753E-31));
#105765=DIRECTION('center_axis',(-4.93038065763132E-32,-1.97215226305253E-31,
1.));
#105766=DIRECTION('ref_axis',(-0.415323571356918,-0.909673749800078,-1.99878547459536E-31));
#105767=DIRECTION('',(-0.29367811369309,-0.643236477151034,0.707106781186544));
#105768=DIRECTION('center_axis',(4.93038065763132E-32,1.97215226305253E-31,
-1.));
#105769=DIRECTION('ref_axis',(-0.415323571356918,-0.909673749800078,-1.99878547459536E-31));
#105770=DIRECTION('center_axis',(-0.293678113693089,-0.643236477151028,
-0.707106781186551));
#105771=DIRECTION('ref_axis',(-0.923516686410398,-2.4980018054066E-16,0.383558248407668));
#105772=DIRECTION('',(-0.293678113693093,-0.643236477151025,0.707106781186552));
#105773=DIRECTION('',(-0.909673749800079,0.415323571356916,3.70577535073674E-32));
#105774=DIRECTION('center_axis',(4.93038065763132E-32,1.97215226305253E-31,
-1.));
#105775=DIRECTION('ref_axis',(0.731712168750195,0.681613748469679,1.70500804894814E-31));
#105776=DIRECTION('center_axis',(-4.93038065763132E-32,-1.97215226305253E-31,
1.));
#105777=DIRECTION('ref_axis',(0.731712168750195,0.681613748469679,1.70500804894814E-31));
#105778=DIRECTION('center_axis',(4.93038065763132E-32,1.97215226305253E-31,
-1.));
#105779=DIRECTION('ref_axis',(-0.731712168808585,0.681613748406997,9.83484144043845E-32));
#105780=DIRECTION('',(0.293678113799996,-0.643236477102231,0.707106781186539));
#105781=DIRECTION('center_axis',(-4.93038065763132E-32,-1.97215226305253E-31,
1.));
#105782=DIRECTION('ref_axis',(-0.731712168808585,0.681613748406997,9.83484144043845E-32));
#105783=DIRECTION('center_axis',(0.293678113799993,-0.643236477102225,-0.707106781186545));
#105784=DIRECTION('ref_axis',(-0.92351668636094,-5.55111512312577E-17,-0.383558248526752));
#105785=DIRECTION('',(0.293678113799987,-0.643236477102215,0.707106781186557));
#105786=DIRECTION('',(-0.909673749731055,-0.415323571508098,-1.26758510749165E-31));
#105787=DIRECTION('center_axis',(-4.93038065763132E-32,-1.97215226305253E-31,
1.));
#105788=DIRECTION('ref_axis',(0.415323571508097,0.909673749731055,1.99878547453377E-31));
#105789=DIRECTION('',(0.293678113799987,0.643236477102215,0.707106781186557));
#105790=DIRECTION('center_axis',(4.93038065763132E-32,1.97215226305253E-31,
-1.));
#105791=DIRECTION('ref_axis',(0.415323571508097,0.909673749731055,1.99878547453377E-31));
#105792=DIRECTION('center_axis',(0.293678113799988,0.643236477102216,-0.707106781186556));
#105793=DIRECTION('ref_axis',(-0.923516686360944,-5.27355936696949E-16,
-0.383558248526742));
#105794=DIRECTION('',(0.293678113799996,0.643236477102231,0.707106781186539));
#105795=DIRECTION('',(0.909673749731055,-0.415323571508098,-3.70577535405859E-32));
#105796=DIRECTION('center_axis',(4.93038065763132E-32,1.97215226305253E-31,
-1.));
#105797=DIRECTION('ref_axis',(-0.731712168808585,-0.681613748406997,-1.70500804885331E-31));
#105798=DIRECTION('center_axis',(-4.93038065763132E-32,-1.97215226305253E-31,
1.));
#105799=DIRECTION('ref_axis',(-0.731712168808585,-0.681613748406997,-1.70500804885331E-31));
#105800=DIRECTION('center_axis',(0.293678113799996,0.643236477102232,0.707106781186538));
#105801=DIRECTION('ref_axis',(0.923516686360937,-4.44089209850063E-16,-0.383558248526758));
#105802=DIRECTION('',(0.293678113799987,0.643236477102215,-0.707106781186557));
#105803=DIRECTION('',(-0.909673749731055,0.415323571508098,3.70577535405859E-32));
#105804=DIRECTION('',(-0.293678113799987,-0.643236477102215,0.707106781186557));
#105805=DIRECTION('',(0.909673749731055,-0.415323571508098,-3.70577535405859E-32));
#105806=DIRECTION('center_axis',(4.93038065763132E-32,1.97215226305253E-31,
-1.));
#105807=DIRECTION('ref_axis',(0.415323571508097,0.909673749731055,1.99878547453377E-31));
#105808=DIRECTION('',(0.29367811380001,-0.643236477102228,-0.707106781186536));
#105809=DIRECTION('center_axis',(-4.93038065763132E-32,-1.97215226305253E-31,
1.));
#105810=DIRECTION('ref_axis',(0.415323571508097,0.909673749731055,1.99878547453377E-31));
#105811=DIRECTION('center_axis',(4.93038065763132E-32,1.97215226305253E-31,
-1.));
#105812=DIRECTION('ref_axis',(0.415323571508097,0.909673749731055,1.99878547453377E-31));
#105813=DIRECTION('center_axis',(0.293678113799988,-0.643236477102216,0.707106781186556));
#105814=DIRECTION('ref_axis',(0.923516686360944,-5.27355936696949E-16,-0.383558248526742));
#105815=DIRECTION('',(0.293678113799996,-0.643236477102231,-0.707106781186539));
#105816=DIRECTION('',(0.909673749731055,0.415323571508098,1.26758510749165E-31));
#105817=DIRECTION('',(-0.909673749731055,-0.415323571508098,-1.26758510749165E-31));
#105818=DIRECTION('center_axis',(-4.93038065763132E-32,-1.97215226305253E-31,
1.));
#105819=DIRECTION('ref_axis',(-0.731712168808585,0.681613748406997,9.83484144043845E-32));
#105820=DIRECTION('',(0.662416044053367,-0.247396411818533,-0.707106781186549));
#105821=DIRECTION('center_axis',(4.93038065763132E-32,1.97215226305253E-31,
-1.));
#105822=DIRECTION('ref_axis',(-0.731712168808585,0.681613748406997,9.83484144043845E-32));
#105823=DIRECTION('center_axis',(-4.93038065763132E-32,-1.97215226305253E-31,
1.));
#105824=DIRECTION('ref_axis',(-0.731712168808585,0.681613748406997,9.83484144043845E-32));
#105825=DIRECTION('center_axis',(4.93038065763132E-32,1.97215226305253E-31,
-1.));
#105826=DIRECTION('ref_axis',(-1.,0.,-4.93038065763132E-32));
#105827=DIRECTION('',(-0.662416044052087,-0.247396411821942,-0.707106781186556));
#105828=DIRECTION('center_axis',(4.93038065763132E-32,1.97215226305253E-31,
-1.));
#105829=DIRECTION('ref_axis',(-1.,0.,-4.93038065763132E-32));
#105830=DIRECTION('center_axis',(-4.93038065763132E-32,-1.97215226305253E-31,
1.));
#105831=DIRECTION('ref_axis',(0.731712168750195,0.681613748469679,1.70500804894814E-31));
#105832=DIRECTION('',(-0.293678113693076,-0.643236477151037,-0.707106781186548));
#105833=DIRECTION('center_axis',(4.93038065763132E-32,1.97215226305253E-31,
-1.));
#105834=DIRECTION('ref_axis',(0.731712168750195,0.681613748469679,1.70500804894814E-31));
#105835=DIRECTION('center_axis',(-4.93038065763132E-32,-1.97215226305253E-31,
1.));
#105836=DIRECTION('ref_axis',(0.731712168750195,0.681613748469679,1.70500804894814E-31));
#105837=DIRECTION('center_axis',(-0.293678113693092,-0.643236477151034,
0.707106781186543));
#105838=DIRECTION('ref_axis',(0.923516686410395,-7.5643526760966E-32,0.383558248407675));
#105839=DIRECTION('',(-0.909673749800079,0.415323571356916,3.70577535073674E-32));
#105840=DIRECTION('',(-0.29367811369309,-0.643236477151034,-0.707106781186544));
#105841=DIRECTION('',(0.909673749800079,-0.415323571356916,-3.70577535073674E-32));
#105842=DIRECTION('center_axis',(4.93038065763132E-32,1.97215226305253E-31,
-1.));
#105843=DIRECTION('ref_axis',(-0.415323571356918,-0.909673749800078,-1.99878547459536E-31));
#105844=DIRECTION('',(-0.29367811369309,0.643236477151034,-0.707106781186544));
#105845=DIRECTION('center_axis',(-4.93038065763132E-32,-1.97215226305253E-31,
1.));
#105846=DIRECTION('ref_axis',(-0.415323571356918,-0.909673749800078,-1.99878547459536E-31));
#105847=DIRECTION('center_axis',(4.93038065763132E-32,1.97215226305253E-31,
-1.));
#105848=DIRECTION('ref_axis',(-0.415323571356918,-0.909673749800078,-1.99878547459536E-31));
#105849=DIRECTION('center_axis',(-0.293678113693089,0.643236477151028,0.707106781186551));
#105850=DIRECTION('ref_axis',(0.923516686410398,-2.4980018054066E-16,0.383558248407668));
#105851=DIRECTION('',(0.909673749800079,0.415323571356916,1.26758510722753E-31));
#105852=DIRECTION('',(-0.29367811369309,0.643236477151034,-0.707106781186544));
#105853=DIRECTION('',(-0.909673749800079,-0.415323571356916,-1.26758510722753E-31));
#105854=DIRECTION('center_axis',(-4.93038065763132E-32,-1.97215226305253E-31,
1.));
#105855=DIRECTION('ref_axis',(0.731712168750192,-0.681613748469681,-9.83484144196258E-32));
#105856=DIRECTION('',(-0.662416044052087,0.247396411821942,-0.707106781186556));
#105857=DIRECTION('center_axis',(4.93038065763132E-32,1.97215226305253E-31,
-1.));
#105858=DIRECTION('ref_axis',(0.731712168750192,-0.681613748469682,-9.83484144196259E-32));
#105859=DIRECTION('center_axis',(-4.93038065763132E-32,-1.97215226305253E-31,
1.));
#105860=DIRECTION('ref_axis',(0.731712168750193,-0.681613748469681,-9.83484144196257E-32));
#105861=DIRECTION('center_axis',(4.93038065763132E-32,1.97215226305253E-31,
-1.));
#105862=DIRECTION('ref_axis',(-1.,0.,-4.93038065763132E-32));
#105863=DIRECTION('',(0.662416044053361,0.247396411818521,-0.707106781186559));
#105864=DIRECTION('center_axis',(4.93038065763132E-32,1.97215226305253E-31,
-1.));
#105865=DIRECTION('ref_axis',(-1.,0.,-4.93038065763132E-32));
#105866=DIRECTION('center_axis',(-4.93038065763132E-32,-1.97215226305253E-31,
1.));
#105867=DIRECTION('ref_axis',(-0.731712168808585,-0.681613748406997,-1.70500804885331E-31));
#105868=DIRECTION('center_axis',(4.93038065763132E-32,1.97215226305253E-31,
-1.));
#105869=DIRECTION('ref_axis',(-0.731712168808585,-0.681613748406997,-1.70500804885331E-31));
#105870=DIRECTION('center_axis',(-4.93038065763132E-32,-1.97215226305253E-31,
1.));
#105871=DIRECTION('ref_axis',(-0.731712168808585,-0.681613748406997,-1.70500804885331E-31));
#105872=DIRECTION('center_axis',(4.93038065763132E-32,1.97215226305253E-31,
-1.));
#105873=DIRECTION('ref_axis',(-0.415323571356918,-0.909673749800078,-1.99878547459536E-31));
#105874=DIRECTION('',(4.93038065763132E-32,1.97215226305253E-31,-1.));
#105875=DIRECTION('',(4.93038065763132E-32,1.97215226305253E-31,-1.));
#105876=DIRECTION('center_axis',(-0.415323571356916,0.909673749800079,1.58924481402006E-31));
#105877=DIRECTION('ref_axis',(0.909673749800079,0.415323571356916,1.26758510722753E-31));
#105878=DIRECTION('',(-4.93038065763132E-32,-1.97215226305253E-31,1.));
#105879=DIRECTION('center_axis',(-4.93038065763132E-32,-1.97215226305253E-31,
1.));
#105880=DIRECTION('ref_axis',(0.731712168750192,-0.681613748469682,-9.83484144196259E-32));
#105881=DIRECTION('center_axis',(4.93038065763132E-32,1.97215226305253E-31,
-1.));
#105882=DIRECTION('ref_axis',(-0.731712168808585,-0.681613748406997,-1.70500804885331E-31));
#105883=DIRECTION('',(4.93038065763132E-32,1.97215226305253E-31,-1.));
#105884=DIRECTION('center_axis',(0.415323571508098,0.909673749731055,1.99878547453377E-31));
#105885=DIRECTION('ref_axis',(0.909673749731055,-0.415323571508098,-3.70577535405859E-32));
#105886=DIRECTION('',(4.93038065763132E-32,1.97215226305253E-31,-1.));
#105887=DIRECTION('center_axis',(4.93038065763132E-32,1.97215226305253E-31,
-1.));
#105888=DIRECTION('ref_axis',(-1.,0.,-4.93038065763132E-32));
#105889=DIRECTION('center_axis',(4.93038065763132E-32,1.97215226305253E-31,
-1.));
#105890=DIRECTION('ref_axis',(0.731712168750195,0.681613748469679,1.70500804894814E-31));
#105891=DIRECTION('',(4.93038065763132E-32,1.97215226305253E-31,-1.));
#105892=DIRECTION('center_axis',(-4.93038065763132E-32,-1.97215226305253E-31,
1.));
#105893=DIRECTION('ref_axis',(-0.731712168808585,0.681613748406997,9.83484144043845E-32));
#105894=DIRECTION('',(-4.93038065763132E-32,-1.97215226305253E-31,1.));
#105895=DIRECTION('center_axis',(0.415323571508098,-0.909673749731055,-1.58924481380939E-31));
#105896=DIRECTION('ref_axis',(-0.909673749731055,-0.415323571508098,-1.26758510749165E-31));
#105897=DIRECTION('',(4.93038065763132E-32,1.97215226305253E-31,-1.));
#105898=DIRECTION('center_axis',(-4.93038065763132E-32,-1.97215226305253E-31,
1.));
#105899=DIRECTION('ref_axis',(1.,0.,4.93038065763132E-32));
#105900=DIRECTION('center_axis',(4.93038065763132E-32,1.97215226305253E-31,
-1.));
#105901=DIRECTION('ref_axis',(1.,0.,4.93038065763132E-32));
#105902=DIRECTION('',(-0.707106781186547,-8.65956056235494E-17,0.707106781186548));
#105903=DIRECTION('center_axis',(-4.93038065763132E-32,-1.97215226305253E-31,
1.));
#105904=DIRECTION('ref_axis',(1.,0.,4.93038065763132E-32));
#105905=DIRECTION('center_axis',(4.93038065763132E-32,1.97215226305253E-31,
-1.));
#105906=DIRECTION('ref_axis',(1.,0.,4.93038065763132E-32));
#105907=DIRECTION('',(4.93038065763132E-32,1.97215226305253E-31,-1.));
#105908=DIRECTION('center_axis',(4.93038065763132E-32,1.97215226305253E-31,
-1.));
#105909=DIRECTION('ref_axis',(1.,0.,4.93038065763132E-32));
#105910=DIRECTION('center_axis',(-4.93038065763132E-32,-1.97215226305253E-31,
1.));
#105911=DIRECTION('ref_axis',(1.,0.,4.93038065763132E-32));
#105912=DIRECTION('center_axis',(-4.93038065763132E-32,-1.97215226305253E-31,
1.));
#105913=DIRECTION('ref_axis',(1.,0.,4.93038065763132E-32));
#105914=DIRECTION('',(0.980976649545336,-0.194125766055945,1.00813261006593E-32));
#105915=DIRECTION('center_axis',(4.93038065763132E-32,1.97215226305253E-31,
-1.));
#105916=DIRECTION('ref_axis',(0.999629431953048,-0.0272212926442944,4.39170827718369E-32));
#105917=DIRECTION('',(-0.980976649545336,-0.194125766055945,-8.66504398694668E-32));
#105918=DIRECTION('center_axis',(-4.93038065763132E-32,-1.97215226305253E-31,
1.));
#105919=DIRECTION('ref_axis',(1.,0.,4.93038065763132E-32));
#105920=DIRECTION('',(0.907731042944837,0.419552563660715,1.27496749553964E-31));
#105921=DIRECTION('center_axis',(4.93038065763132E-32,1.97215226305253E-31,
-1.));
#105922=DIRECTION('ref_axis',(0.824717472892045,0.565544949501416,1.5219578596529E-31));
#105923=DIRECTION('',(-0.67952251818951,-0.733654651231345,-1.78190914873556E-31));
#105924=DIRECTION('center_axis',(-4.93038065763132E-32,-1.97215226305253E-31,
1.));
#105925=DIRECTION('ref_axis',(1.,0.,4.93038065763132E-32));
#105926=DIRECTION('',(0.487763030582801,0.872976074126136,1.96212748132788E-31));
#105927=DIRECTION('center_axis',(4.93038065763132E-32,1.97215226305253E-31,
-1.));
#105928=DIRECTION('ref_axis',(0.334791470302201,0.942292243103428,2.02340871864506E-31));
#105929=DIRECTION('',(-0.11851388100621,-0.992952395640821,-2.01668516882386E-31));
#105930=DIRECTION('center_axis',(-4.93038065763132E-32,-1.97215226305253E-31,
1.));
#105931=DIRECTION('ref_axis',(1.,0.,4.93038065763132E-32));
#105932=DIRECTION('',(-0.118513881006211,0.992952395640821,1.89982145950909E-31));
#105933=DIRECTION('center_axis',(4.93038065763132E-32,1.97215226305253E-31,
-1.));
#105934=DIRECTION('ref_axis',(-0.283013494799533,0.95911592717531,1.75198622024769E-31));
#105935=DIRECTION('',(0.487763030582801,-0.872976074126136,-1.48115599902926E-31));
#105936=DIRECTION('center_axis',(-4.93038065763132E-32,-1.97215226305253E-31,
1.));
#105937=DIRECTION('ref_axis',(1.,0.,4.93038065763132E-32));
#105938=DIRECTION('',(-0.67952251818951,0.733654651231345,1.11184821271426E-31));
#105939=DIRECTION('center_axis',(4.93038065763132E-32,1.97215226305253E-31,
-1.));
#105940=DIRECTION('ref_axis',(-0.792716924162737,0.609589926217592,8.11364533537153E-32));
#105941=DIRECTION('',(0.907731042944837,-0.419552563660715,-3.79875580246296E-32));
#105942=DIRECTION('center_axis',(-4.93038065763132E-32,-1.97215226305253E-31,
1.));
#105943=DIRECTION('ref_axis',(1.,0.,4.93038065763132E-32));
#105944=DIRECTION('',(-0.980976649545336,0.194125766055945,-1.00813261006593E-32));
#105945=DIRECTION('center_axis',(4.93038065763132E-32,1.97215226305253E-31,
-1.));
#105946=DIRECTION('ref_axis',(-0.999629431953048,0.0272212926442945,-4.39170827718369E-32));
#105947=DIRECTION('',(0.980976649545336,0.194125766055945,8.66504398694668E-32));
#105948=DIRECTION('center_axis',(-4.93038065763132E-32,-1.97215226305253E-31,
1.));
#105949=DIRECTION('ref_axis',(1.,0.,4.93038065763132E-32));
#105950=DIRECTION('',(-0.907731042944837,-0.419552563660715,-1.27496749553964E-31));
#105951=DIRECTION('center_axis',(4.93038065763132E-32,1.97215226305253E-31,
-1.));
#105952=DIRECTION('ref_axis',(-0.824717472892045,-0.565544949501416,-1.5219578596529E-31));
#105953=DIRECTION('',(0.67952251818951,0.733654651231345,1.78190914873556E-31));
#105954=DIRECTION('center_axis',(-4.93038065763132E-32,-1.97215226305253E-31,
1.));
#105955=DIRECTION('ref_axis',(1.,0.,4.93038065763132E-32));
#105956=DIRECTION('',(-0.487763030582801,-0.872976074126136,-1.96212748132788E-31));
#105957=DIRECTION('center_axis',(4.93038065763132E-32,1.97215226305253E-31,
-1.));
#105958=DIRECTION('ref_axis',(-0.334791470302201,-0.942292243103428,-2.02340871864506E-31));
#105959=DIRECTION('',(0.11851388100621,0.992952395640821,2.01668516882386E-31));
#105960=DIRECTION('center_axis',(-4.93038065763132E-32,-1.97215226305253E-31,
1.));
#105961=DIRECTION('ref_axis',(1.,0.,4.93038065763132E-32));
#105962=DIRECTION('',(0.118513881006211,-0.992952395640821,-1.89982145950909E-31));
#105963=DIRECTION('center_axis',(4.93038065763132E-32,1.97215226305253E-31,
-1.));
#105964=DIRECTION('ref_axis',(0.283013494799533,-0.95911592717531,-1.75198622024769E-31));
#105965=DIRECTION('',(-0.487763030582801,0.872976074126136,1.48115599902926E-31));
#105966=DIRECTION('center_axis',(-4.93038065763132E-32,-1.97215226305253E-31,
1.));
#105967=DIRECTION('ref_axis',(1.,0.,4.93038065763132E-32));
#105968=DIRECTION('',(0.67952251818951,-0.733654651231345,-1.11184821271426E-31));
#105969=DIRECTION('center_axis',(4.93038065763132E-32,1.97215226305253E-31,
-1.));
#105970=DIRECTION('ref_axis',(0.792716924162737,-0.609589926217592,-8.11364533537153E-32));
#105971=DIRECTION('',(-0.907731042944837,0.419552563660715,3.79875580246296E-32));
#105972=DIRECTION('center_axis',(-4.93038065763132E-32,-1.97215226305253E-31,
1.));
#105973=DIRECTION('ref_axis',(1.,0.,4.93038065763132E-32));
#105974=DIRECTION('center_axis',(-4.93038065763132E-32,-1.97215226305253E-31,
1.));
#105975=DIRECTION('ref_axis',(1.,0.,4.93038065763132E-32));
#105976=DIRECTION('center_axis',(-4.93038065763132E-32,-1.97215226305253E-31,
1.));
#105977=DIRECTION('ref_axis',(1.,0.,4.93038065763132E-32));
#105978=DIRECTION('',(-0.487763030582801,0.872976074126136,1.48115599902926E-31));
#105979=DIRECTION('center_axis',(-4.93038065763132E-32,-1.97215226305253E-31,
1.));
#105980=DIRECTION('ref_axis',(0.283013494799533,-0.95911592717531,-1.75198622024769E-31));
#105981=DIRECTION('',(0.11851388100621,-0.992952395640821,-1.89982145950909E-31));
#105982=DIRECTION('center_axis',(-4.93038065763132E-32,-1.97215226305253E-31,
1.));
#105983=DIRECTION('ref_axis',(1.,0.,4.93038065763132E-32));
#105984=DIRECTION('',(0.11851388100621,0.992952395640821,2.01668516882386E-31));
#105985=DIRECTION('center_axis',(-4.93038065763132E-32,-1.97215226305253E-31,
1.));
#105986=DIRECTION('ref_axis',(-0.334791470302201,-0.942292243103428,-2.02340871864506E-31));
#105987=DIRECTION('',(-0.487763030582801,-0.872976074126136,-1.96212748132788E-31));
#105988=DIRECTION('center_axis',(-4.93038065763132E-32,-1.97215226305253E-31,
1.));
#105989=DIRECTION('ref_axis',(1.,0.,4.93038065763132E-32));
#105990=DIRECTION('',(0.67952251818951,0.733654651231345,1.78190914873556E-31));
#105991=DIRECTION('center_axis',(-4.93038065763132E-32,-1.97215226305253E-31,
1.));
#105992=DIRECTION('ref_axis',(-0.824717472892045,-0.565544949501416,-1.5219578596529E-31));
#105993=DIRECTION('',(-0.907731042944837,-0.419552563660715,-1.27496749553964E-31));
#105994=DIRECTION('center_axis',(-4.93038065763132E-32,-1.97215226305253E-31,
1.));
#105995=DIRECTION('ref_axis',(1.,0.,4.93038065763132E-32));
#105996=DIRECTION('',(0.980976649545336,0.194125766055945,8.66504398694668E-32));
#105997=DIRECTION('center_axis',(-4.93038065763132E-32,-1.97215226305253E-31,
1.));
#105998=DIRECTION('ref_axis',(-0.999629431953048,0.0272212926442946,-4.39170827718369E-32));
#105999=DIRECTION('',(-0.980976649545336,0.194125766055945,-1.00813261006593E-32));
#106000=DIRECTION('center_axis',(-4.93038065763132E-32,-1.97215226305253E-31,
1.));
#106001=DIRECTION('ref_axis',(1.,0.,4.93038065763132E-32));
#106002=DIRECTION('',(0.907731042944837,-0.419552563660715,-3.79875580246296E-32));
#106003=DIRECTION('center_axis',(-4.93038065763132E-32,-1.97215226305253E-31,
1.));
#106004=DIRECTION('ref_axis',(-0.792716924162737,0.609589926217592,8.11364533537153E-32));
#106005=DIRECTION('',(-0.67952251818951,0.733654651231345,1.11184821271426E-31));
#106006=DIRECTION('center_axis',(-4.93038065763132E-32,-1.97215226305253E-31,
1.));
#106007=DIRECTION('ref_axis',(1.,0.,4.93038065763132E-32));
#106008=DIRECTION('',(0.487763030582801,-0.872976074126136,-1.48115599902926E-31));
#106009=DIRECTION('center_axis',(-4.93038065763132E-32,-1.97215226305253E-31,
1.));
#106010=DIRECTION('ref_axis',(-0.283013494799533,0.95911592717531,1.75198622024769E-31));
#106011=DIRECTION('',(-0.118513881006211,0.992952395640821,1.89982145950909E-31));
#106012=DIRECTION('center_axis',(-4.93038065763132E-32,-1.97215226305253E-31,
1.));
#106013=DIRECTION('ref_axis',(1.,0.,4.93038065763132E-32));
#106014=DIRECTION('',(-0.11851388100621,-0.992952395640821,-2.01668516882386E-31));
#106015=DIRECTION('center_axis',(-4.93038065763132E-32,-1.97215226305253E-31,
1.));
#106016=DIRECTION('ref_axis',(0.334791470302201,0.942292243103428,2.02340871864506E-31));
#106017=DIRECTION('',(0.487763030582801,0.872976074126136,1.96212748132788E-31));
#106018=DIRECTION('center_axis',(-4.93038065763132E-32,-1.97215226305253E-31,
1.));
#106019=DIRECTION('ref_axis',(1.,0.,4.93038065763132E-32));
#106020=DIRECTION('',(-0.67952251818951,-0.733654651231345,-1.78190914873556E-31));
#106021=DIRECTION('center_axis',(-4.93038065763132E-32,-1.97215226305253E-31,
1.));
#106022=DIRECTION('ref_axis',(0.824717472892045,0.565544949501416,1.5219578596529E-31));
#106023=DIRECTION('',(0.907731042944837,0.419552563660715,1.27496749553964E-31));
#106024=DIRECTION('center_axis',(-4.93038065763132E-32,-1.97215226305253E-31,
1.));
#106025=DIRECTION('ref_axis',(1.,0.,4.93038065763132E-32));
#106026=DIRECTION('',(-0.980976649545336,-0.194125766055945,-8.66504398694668E-32));
#106027=DIRECTION('center_axis',(-4.93038065763132E-32,-1.97215226305253E-31,
1.));
#106028=DIRECTION('ref_axis',(0.999629431953048,-0.0272212926442945,4.39170827718369E-32));
#106029=DIRECTION('',(0.980976649545336,-0.194125766055945,1.00813261006593E-32));
#106030=DIRECTION('center_axis',(-4.93038065763132E-32,-1.97215226305253E-31,
1.));
#106031=DIRECTION('ref_axis',(1.,0.,4.93038065763132E-32));
#106032=DIRECTION('',(-0.907731042944837,0.419552563660715,3.79875580246296E-32));
#106033=DIRECTION('center_axis',(-4.93038065763132E-32,-1.97215226305253E-31,
1.));
#106034=DIRECTION('ref_axis',(0.792716924162737,-0.609589926217592,-8.11364533537153E-32));
#106035=DIRECTION('',(0.67952251818951,-0.733654651231345,-1.11184821271426E-31));
#106036=DIRECTION('center_axis',(4.93038065763132E-32,1.97215226305253E-31,
-1.));
#106037=DIRECTION('ref_axis',(1.,0.,4.93038065763132E-32));
#106038=DIRECTION('center_axis',(-0.733654651231345,-0.67952251818951,2.41113348070025E-17));
#106039=DIRECTION('ref_axis',(-1.44471196324713E-17,-1.98847542650175E-17,
-1.));
#106040=DIRECTION('',(-4.93038065763132E-32,-1.97215226305253E-31,1.));
#106041=DIRECTION('',(-4.93038065763132E-32,-1.97215226305253E-31,1.));
#106042=DIRECTION('',(-4.33349072293499E-17,-5.96453828357725E-17,-1.));
#106043=DIRECTION('center_axis',(-4.93038065763132E-32,-1.97215226305253E-31,
1.));
#106044=DIRECTION('ref_axis',(0.792716924162737,-0.609589926217592,-8.11364533537153E-32));
#106045=DIRECTION('',(-2.56739074444567E-15,-1.97215226305253E-31,1.));
#106046=DIRECTION('',(-4.93038065763132E-32,-1.97215226305253E-31,1.));
#106047=DIRECTION('center_axis',(0.419552563660715,0.907731042944837,-5.10516967005408E-17));
#106048=DIRECTION('ref_axis',(3.05893462795411E-17,4.21026231781923E-17,
1.));
#106049=DIRECTION('',(4.93038065763132E-32,1.97215226305253E-31,-1.));
#106050=DIRECTION('center_axis',(-4.93038065763132E-32,-1.97215226305253E-31,
1.));
#106051=DIRECTION('ref_axis',(1.,0.,4.93038065763132E-32));
#106052=DIRECTION('',(4.93038065763132E-32,1.97215226305253E-31,-1.));
#106053=DIRECTION('center_axis',(-4.93038065763132E-32,-1.97215226305253E-31,
1.));
#106054=DIRECTION('ref_axis',(1.,0.,4.93038065763132E-32));
#106055=DIRECTION('',(-4.93038065763132E-32,-1.97215226305253E-31,1.));
#106056=DIRECTION('center_axis',(-0.992952395640821,-0.118513881006211,
2.41113348070026E-17));
#106057=DIRECTION('ref_axis',(-2.33759306048745E-17,-7.59530027129711E-18,
-1.));
#106058=DIRECTION('',(-4.93038065763132E-32,-1.97215226305253E-31,1.));
#106059=DIRECTION('',(-4.93038065763132E-32,-1.97215226305253E-31,1.));
#106060=DIRECTION('',(-7.01173527964117E-17,-2.27825089712654E-17,-1.));
#106061=DIRECTION('center_axis',(-4.93038065763132E-32,-1.97215226305253E-31,
1.));
#106062=DIRECTION('ref_axis',(0.283013494799533,-0.95911592717531,-1.75198622024769E-31));
#106063=DIRECTION('',(-4.93038065763132E-32,-1.97215226305253E-31,1.));
#106064=DIRECTION('',(-4.93038065763132E-32,-1.97215226305253E-31,1.));
#106065=DIRECTION('center_axis',(0.872976074126136,0.487763030582801,-5.10516967005409E-17));
#106066=DIRECTION('ref_axis',(4.94946019739376E-17,1.60817710385402E-17,
1.));
#106067=DIRECTION('center_axis',(-4.93038065763132E-32,-1.97215226305253E-31,
1.));
#106068=DIRECTION('ref_axis',(1.,0.,4.93038065763132E-32));
#106069=DIRECTION('',(4.93038065763132E-32,1.97215226305253E-31,-1.));
#106070=DIRECTION('center_axis',(-0.872976074126136,0.487763030582801,2.41113348070028E-17));
#106071=DIRECTION('ref_axis',(-2.33759306048745E-17,7.59530027129753E-18,
-1.));
#106072=DIRECTION('',(-4.93038065763132E-32,-1.97215226305253E-31,1.));
#106073=DIRECTION('',(-4.93038065763132E-32,-1.97215226305253E-31,1.));
#106074=DIRECTION('',(-7.01173527964117E-17,2.27825089712658E-17,-1.));
#106075=DIRECTION('center_axis',(-4.93038065763132E-32,-1.97215226305253E-31,
1.));
#106076=DIRECTION('ref_axis',(-0.334791470302201,-0.942292243103428,-2.02340871864506E-31));
#106077=DIRECTION('',(2.42861286636753E-16,-1.97215226305253E-31,1.));
#106078=DIRECTION('',(-4.93038065763132E-32,-1.97215226305253E-31,1.));
#106079=DIRECTION('center_axis',(0.992952395640821,-0.118513881006211,-5.1051696700541E-17));
#106080=DIRECTION('ref_axis',(4.94946019739376E-17,-1.60817710385406E-17,
1.));
#106081=DIRECTION('center_axis',(-4.93038065763132E-32,-1.97215226305253E-31,
1.));
#106082=DIRECTION('ref_axis',(1.,0.,4.93038065763132E-32));
#106083=DIRECTION('',(4.93038065763132E-32,1.97215226305253E-31,-1.));
#106084=DIRECTION('center_axis',(-0.419552563660715,0.907731042944837,2.41113348070029E-17));
#106085=DIRECTION('ref_axis',(-1.44471196324713E-17,1.98847542650179E-17,
-1.));
#106086=DIRECTION('',(-4.93038065763132E-32,-1.97215226305253E-31,1.));
#106087=DIRECTION('',(-4.93038065763132E-32,-1.97215226305253E-31,1.));
#106088=DIRECTION('',(-4.33349072293499E-17,5.9645382835773E-17,-1.));
#106089=DIRECTION('center_axis',(-4.93038065763132E-32,-1.97215226305253E-31,
1.));
#106090=DIRECTION('ref_axis',(-0.824717472892045,-0.565544949501416,-1.5219578596529E-31));
#106091=DIRECTION('',(-4.93038065763132E-32,-1.97215226305253E-31,1.));
#106092=DIRECTION('',(-4.93038065763132E-32,-1.97215226305253E-31,1.));
#106093=DIRECTION('center_axis',(0.733654651231345,-0.67952251818951,-5.10516967005411E-17));
#106094=DIRECTION('ref_axis',(3.05893462795411E-17,-4.21026231781927E-17,
1.));
#106095=DIRECTION('center_axis',(-4.93038065763132E-32,-1.97215226305253E-31,
1.));
#106096=DIRECTION('ref_axis',(1.,0.,4.93038065763132E-32));
#106097=DIRECTION('',(4.93038065763132E-32,1.97215226305253E-31,-1.));
#106098=DIRECTION('center_axis',(0.194125766055945,0.980976649545336,2.41113348070029E-17));
#106099=DIRECTION('ref_axis',(6.16297582203915E-32,2.45789079874409E-17,
-1.));
#106100=DIRECTION('',(-4.93038065763132E-32,-1.97215226305253E-31,1.));
#106101=DIRECTION('',(-4.93038065763132E-32,-1.97215226305253E-31,1.));
#106102=DIRECTION('',(5.83326066734215E-32,7.37257477290145E-17,-1.));
#106103=DIRECTION('center_axis',(-4.93038065763132E-32,-1.97215226305253E-31,
1.));
#106104=DIRECTION('ref_axis',(-0.999629431953048,0.0272212926442946,-4.39170827718369E-32));
#106105=DIRECTION('',(2.4980018054066E-15,-1.97215226305253E-31,1.));
#106106=DIRECTION('',(-4.93038065763132E-32,-1.97215226305253E-31,1.));
#106107=DIRECTION('center_axis',(0.194125766055945,-0.980976649545336,-5.10516967005412E-17));
#106108=DIRECTION('ref_axis',(-5.8548270309372E-32,-5.20417042793044E-17,
1.));
#106109=DIRECTION('center_axis',(-4.93038065763132E-32,-1.97215226305253E-31,
1.));
#106110=DIRECTION('ref_axis',(1.,0.,4.93038065763132E-32));
#106111=DIRECTION('',(4.93038065763132E-32,1.97215226305253E-31,-1.));
#106112=DIRECTION('center_axis',(0.733654651231345,0.67952251818951,2.41113348070029E-17));
#106113=DIRECTION('ref_axis',(1.44471196324714E-17,1.98847542650179E-17,
-1.));
#106114=DIRECTION('',(-4.93038065763132E-32,-1.97215226305253E-31,1.));
#106115=DIRECTION('',(-4.93038065763132E-32,-1.97215226305253E-31,1.));
#106116=DIRECTION('',(4.33349072293499E-17,5.9645382835773E-17,-1.));
#106117=DIRECTION('center_axis',(-4.93038065763132E-32,-1.97215226305253E-31,
1.));
#106118=DIRECTION('ref_axis',(-0.792716924162737,0.609589926217592,8.11364533537153E-32));
#106119=DIRECTION('',(2.56739074444567E-15,-1.97215226305253E-31,1.));
#106120=DIRECTION('',(-4.93038065763132E-32,-1.97215226305253E-31,1.));
#106121=DIRECTION('center_axis',(-0.419552563660715,-0.907731042944837,
-5.10516967005412E-17));
#106122=DIRECTION('ref_axis',(-3.05893462795412E-17,-4.21026231781927E-17,
1.));
#106123=DIRECTION('center_axis',(-4.93038065763132E-32,-1.97215226305253E-31,
1.));
#106124=DIRECTION('ref_axis',(1.,0.,4.93038065763132E-32));
#106125=DIRECTION('',(4.93038065763132E-32,1.97215226305253E-31,-1.));
#106126=DIRECTION('center_axis',(0.992952395640821,0.118513881006211,2.41113348070028E-17));
#106127=DIRECTION('ref_axis',(2.33759306048746E-17,7.59530027129751E-18,
-1.));
#106128=DIRECTION('',(-4.93038065763132E-32,-1.97215226305253E-31,1.));
#106129=DIRECTION('',(-4.93038065763132E-32,-1.97215226305253E-31,1.));
#106130=DIRECTION('',(7.01173527964118E-17,2.27825089712658E-17,-1.));
#106131=DIRECTION('center_axis',(-4.93038065763132E-32,-1.97215226305253E-31,
1.));
#106132=DIRECTION('ref_axis',(-0.283013494799533,0.95911592717531,1.75198622024769E-31));
#106133=DIRECTION('',(-4.93038065763132E-32,-1.97215226305253E-31,1.));
#106134=DIRECTION('',(-2.4980018054066E-15,-1.97215226305253E-31,1.));
#106135=DIRECTION('center_axis',(-0.872976074126136,-0.487763030582801,
-5.10516967005412E-17));
#106136=DIRECTION('ref_axis',(-4.94946019739377E-17,-1.60817710385406E-17,
1.));
#106137=DIRECTION('center_axis',(-4.93038065763132E-32,-1.97215226305253E-31,
1.));
#106138=DIRECTION('ref_axis',(1.,0.,4.93038065763132E-32));
#106139=DIRECTION('',(4.93038065763132E-32,1.97215226305253E-31,-1.));
#106140=DIRECTION('center_axis',(0.872976074126137,-0.487763030582801,2.41113348070026E-17));
#106141=DIRECTION('ref_axis',(2.33759306048745E-17,-7.59530027129711E-18,
-1.));
#106142=DIRECTION('',(-4.93038065763132E-32,-1.97215226305253E-31,1.));
#106143=DIRECTION('',(-4.93038065763132E-32,2.44249065417534E-14,1.));
#106144=DIRECTION('',(7.01173527964118E-17,-2.27825089712654E-17,-1.));
#106145=DIRECTION('center_axis',(-4.93038065763132E-32,-1.97215226305253E-31,
1.));
#106146=DIRECTION('ref_axis',(0.334791470302201,0.942292243103428,2.02340871864506E-31));
#106147=DIRECTION('',(-4.93038065763132E-32,-1.97215226305253E-31,1.));
#106148=DIRECTION('',(-4.93038065763132E-32,-1.97215226305253E-31,1.));
#106149=DIRECTION('center_axis',(-0.992952395640821,0.118513881006211,-5.1051696700541E-17));
#106150=DIRECTION('ref_axis',(-4.94946019739377E-17,1.60817710385402E-17,
1.));
#106151=DIRECTION('center_axis',(-4.93038065763132E-32,-1.97215226305253E-31,
1.));
#106152=DIRECTION('ref_axis',(1.,0.,4.93038065763132E-32));
#106153=DIRECTION('',(4.93038065763132E-32,1.97215226305253E-31,-1.));
#106154=DIRECTION('center_axis',(0.419552563660715,-0.907731042944837,2.41113348070025E-17));
#106155=DIRECTION('ref_axis',(1.44471196324714E-17,-1.98847542650175E-17,
-1.));
#106156=DIRECTION('',(-4.93038065763132E-32,-1.97215226305253E-31,1.));
#106157=DIRECTION('',(-4.93038065763132E-32,-1.97215226305253E-31,1.));
#106158=DIRECTION('',(4.33349072293499E-17,-5.96453828357726E-17,-1.));
#106159=DIRECTION('center_axis',(-4.93038065763132E-32,-1.97215226305253E-31,
1.));
#106160=DIRECTION('ref_axis',(0.824717472892045,0.565544949501416,1.5219578596529E-31));
#106161=DIRECTION('',(-4.93038065763132E-32,-1.97215226305253E-31,1.));
#106162=DIRECTION('',(-4.93038065763132E-32,-1.97215226305253E-31,1.));
#106163=DIRECTION('center_axis',(-0.733654651231345,0.67952251818951,-5.10516967005409E-17));
#106164=DIRECTION('ref_axis',(-3.05893462795412E-17,4.21026231781923E-17,
1.));
#106165=DIRECTION('center_axis',(-4.93038065763132E-32,-1.97215226305253E-31,
1.));
#106166=DIRECTION('ref_axis',(1.,0.,4.93038065763132E-32));
#106167=DIRECTION('',(4.93038065763132E-32,1.97215226305253E-31,-1.));
#106168=DIRECTION('center_axis',(-0.194125766055945,-0.980976649545336,
2.41113348070025E-17));
#106169=DIRECTION('ref_axis',(4.00593428432545E-32,-2.45789079874405E-17,
-1.));
#106170=DIRECTION('',(-4.93038065763132E-32,-1.97215226305253E-31,1.));
#106171=DIRECTION('',(4.93038065763132E-32,-7.37257477290141E-17,-1.));
#106172=DIRECTION('center_axis',(-4.93038065763132E-32,-1.97215226305253E-31,
1.));
#106173=DIRECTION('ref_axis',(0.999629431953048,-0.0272212926442945,4.39170827718369E-32));
#106174=DIRECTION('',(-2.4980018054066E-15,-1.97215226305253E-31,1.));
#106175=DIRECTION('',(-4.93038065763132E-32,-1.97215226305253E-31,1.));
#106176=DIRECTION('center_axis',(-0.194125766055945,0.980976649545336,-5.10516967005408E-17));
#106177=DIRECTION('ref_axis',(-4.62223186652937E-32,5.2041704279304E-17,
1.));
#106178=DIRECTION('center_axis',(-4.93038065763132E-32,-1.97215226305253E-31,
1.));
#106179=DIRECTION('ref_axis',(-0.464722744083384,0.885456250264015,1.51712854493318E-31));
#106180=DIRECTION('center_axis',(4.93038065763132E-32,1.97215226305253E-31,
-1.));
#106181=DIRECTION('ref_axis',(1.,0.,4.93038065763132E-32));
#106182=DIRECTION('',(-0.415660658584274,0.791976146676961,-0.447213595499958));
#106183=DIRECTION('center_axis',(4.93038065763132E-32,1.97215226305253E-31,
-1.));
#106184=DIRECTION('ref_axis',(1.,7.65671051465626E-16,4.93038065763134E-32));
#106185=DIRECTION('center_axis',(4.93038065763132E-32,1.97215226305253E-31,
-1.));
#106186=DIRECTION('ref_axis',(1.,0.,4.93038065763132E-32));
#106187=DIRECTION('center_axis',(4.93038065763132E-32,1.97215226305253E-31,
-1.));
#106188=DIRECTION('ref_axis',(-0.464722744083384,0.885456250264015,1.51712854493318E-31));
#106189=DIRECTION('center_axis',(-4.93038065763132E-32,-1.97215226305253E-31,
1.));
#106190=DIRECTION('ref_axis',(1.,0.,4.93038065763132E-32));
#106191=DIRECTION('',(-0.415660658584278,0.791976146676969,0.447213595499941));
#106192=DIRECTION('center_axis',(-4.93038065763132E-32,-1.97215226305253E-31,
1.));
#106193=DIRECTION('ref_axis',(1.,0.,4.93038065763132E-32));
#106194=DIRECTION('center_axis',(4.93038065763132E-32,1.97215226305253E-31,
-1.));
#106195=DIRECTION('ref_axis',(1.,0.,4.93038065763132E-32));
#106196=DIRECTION('',(-4.93038065763132E-32,-1.97215226305253E-31,1.));
#106197=DIRECTION('center_axis',(-4.93038065763132E-32,-1.97215226305253E-31,
1.));
#106198=DIRECTION('ref_axis',(1.,0.,4.93038065763132E-32));
#106199=DIRECTION('center_axis',(-4.93038065763132E-32,-1.97215226305253E-31,
1.));
#106200=DIRECTION('ref_axis',(1.,0.,4.93038065763132E-32));
#106201=DIRECTION('center_axis',(4.93038065763132E-32,1.97215226305253E-31,
-1.));
#106202=DIRECTION('ref_axis',(1.,0.,4.93038065763132E-32));
#106203=DIRECTION('',(-4.93038065763132E-32,-1.97215226305253E-31,1.));
#106204=DIRECTION('center_axis',(-4.93038065763132E-32,-1.97215226305253E-31,
1.));
#106205=DIRECTION('ref_axis',(-0.464722744083384,0.885456250264015,1.51712854493318E-31));
#106206=DIRECTION('center_axis',(4.93038065763132E-32,1.97215226305253E-31,
-1.));
#106207=DIRECTION('ref_axis',(1.,0.,4.93038065763132E-32));
#106208=DIRECTION('',(-0.415660658584274,0.791976146676961,-0.447213595499958));
#106209=DIRECTION('center_axis',(4.93038065763132E-32,1.97215226305253E-31,
-1.));
#106210=DIRECTION('ref_axis',(1.,7.65671051465626E-16,4.93038065763134E-32));
#106211=DIRECTION('center_axis',(4.93038065763132E-32,1.97215226305253E-31,
-1.));
#106212=DIRECTION('ref_axis',(1.,0.,4.93038065763132E-32));
#106213=DIRECTION('center_axis',(4.93038065763132E-32,1.97215226305253E-31,
-1.));
#106214=DIRECTION('ref_axis',(-0.464722744083384,0.885456250264015,1.51712854493318E-31));
#106215=DIRECTION('',(-0.415660658584278,0.791976146676969,0.447213595499941));
#106216=DIRECTION('center_axis',(4.93038065763132E-32,1.97215226305253E-31,
-1.));
#106217=DIRECTION('ref_axis',(1.,0.,4.93038065763132E-32));
#106218=DIRECTION('',(-4.93038065763132E-32,-1.97215226305253E-31,1.));
#106219=DIRECTION('center_axis',(-4.93038065763132E-32,-1.97215226305253E-31,
1.));
#106220=DIRECTION('ref_axis',(1.,0.,4.93038065763132E-32));
#106221=DIRECTION('center_axis',(-4.93038065763132E-32,-1.97215226305253E-31,
1.));
#106222=DIRECTION('ref_axis',(1.,0.,4.93038065763132E-32));
#106223=DIRECTION('center_axis',(-4.93038065763132E-32,-1.97215226305253E-31,
1.));
#106224=DIRECTION('ref_axis',(-0.464722744083384,0.885456250264015,1.51712854493318E-31));
#106225=DIRECTION('center_axis',(4.93038065763132E-32,1.97215226305253E-31,
-1.));
#106226=DIRECTION('ref_axis',(1.,0.,4.93038065763132E-32));
#106227=DIRECTION('',(-0.415660658584274,0.791976146676961,-0.447213595499958));
#106228=DIRECTION('center_axis',(4.93038065763132E-32,1.97215226305253E-31,
-1.));
#106229=DIRECTION('ref_axis',(1.,7.65671051465626E-16,4.93038065763134E-32));
#106230=DIRECTION('center_axis',(4.93038065763132E-32,1.97215226305253E-31,
-1.));
#106231=DIRECTION('ref_axis',(1.,0.,4.93038065763132E-32));
#106232=DIRECTION('center_axis',(4.93038065763132E-32,1.97215226305253E-31,
-1.));
#106233=DIRECTION('ref_axis',(-0.464722744083384,0.885456250264015,1.51712854493318E-31));
#106234=DIRECTION('',(-0.415660658584278,0.791976146676969,0.447213595499941));
#106235=DIRECTION('center_axis',(4.93038065763132E-32,1.97215226305253E-31,
-1.));
#106236=DIRECTION('ref_axis',(1.,0.,4.93038065763132E-32));
#106237=DIRECTION('',(-4.93038065763132E-32,-1.97215226305253E-31,1.));
#106238=DIRECTION('center_axis',(-4.93038065763132E-32,-1.97215226305253E-31,
1.));
#106239=DIRECTION('ref_axis',(1.,0.,4.93038065763132E-32));
#106240=DIRECTION('center_axis',(-4.93038065763132E-32,-1.97215226305253E-31,
1.));
#106241=DIRECTION('ref_axis',(1.,0.,4.93038065763132E-32));
#106242=DIRECTION('center_axis',(-4.93038065763132E-32,-1.97215226305253E-31,
1.));
#106243=DIRECTION('ref_axis',(-0.464722744083384,0.885456250264015,1.51712854493318E-31));
#106244=DIRECTION('center_axis',(4.93038065763132E-32,1.97215226305253E-31,
-1.));
#106245=DIRECTION('ref_axis',(1.,0.,4.93038065763132E-32));
#106246=DIRECTION('',(-0.415660658584274,0.791976146676961,-0.447213595499958));
#106247=DIRECTION('center_axis',(4.93038065763132E-32,1.97215226305253E-31,
-1.));
#106248=DIRECTION('ref_axis',(1.,7.65671051465626E-16,4.93038065763134E-32));
#106249=DIRECTION('center_axis',(4.93038065763132E-32,1.97215226305253E-31,
-1.));
#106250=DIRECTION('ref_axis',(1.,0.,4.93038065763132E-32));
#106251=DIRECTION('center_axis',(4.93038065763132E-32,1.97215226305253E-31,
-1.));
#106252=DIRECTION('ref_axis',(-0.464722744083384,0.885456250264015,1.51712854493318E-31));
#106253=DIRECTION('',(-0.415660658584278,0.791976146676969,0.447213595499941));
#106254=DIRECTION('center_axis',(4.93038065763132E-32,1.97215226305253E-31,
-1.));
#106255=DIRECTION('ref_axis',(1.,0.,4.93038065763132E-32));
#106256=DIRECTION('',(-4.93038065763132E-32,-1.97215226305253E-31,1.));
#106257=DIRECTION('center_axis',(-4.93038065763132E-32,-1.97215226305253E-31,
1.));
#106258=DIRECTION('ref_axis',(1.,0.,4.93038065763132E-32));
#106259=DIRECTION('center_axis',(-4.93038065763132E-32,-1.97215226305253E-31,
1.));
#106260=DIRECTION('ref_axis',(1.,0.,4.93038065763132E-32));
#106261=DIRECTION('center_axis',(-4.93038065763132E-32,-1.97215226305253E-31,
1.));
#106262=DIRECTION('ref_axis',(-0.464722744083384,0.885456250264015,1.51712854493318E-31));
#106263=DIRECTION('center_axis',(4.93038065763132E-32,1.97215226305253E-31,
-1.));
#106264=DIRECTION('ref_axis',(1.,0.,4.93038065763132E-32));
#106265=DIRECTION('',(-0.415660658584274,0.791976146676961,-0.447213595499958));
#106266=DIRECTION('center_axis',(4.93038065763132E-32,1.97215226305253E-31,
-1.));
#106267=DIRECTION('ref_axis',(1.,7.65671051465626E-16,4.93038065763134E-32));
#106268=DIRECTION('center_axis',(4.93038065763132E-32,1.97215226305253E-31,
-1.));
#106269=DIRECTION('ref_axis',(1.,0.,4.93038065763132E-32));
#106270=DIRECTION('center_axis',(4.93038065763132E-32,1.97215226305253E-31,
-1.));
#106271=DIRECTION('ref_axis',(-0.464722744083384,0.885456250264015,1.51712854493318E-31));
#106272=DIRECTION('',(-0.415660658584278,0.791976146676969,0.447213595499941));
#106273=DIRECTION('center_axis',(4.93038065763132E-32,1.97215226305253E-31,
-1.));
#106274=DIRECTION('ref_axis',(1.,0.,4.93038065763132E-32));
#106275=DIRECTION('',(-4.93038065763132E-32,-1.97215226305253E-31,1.));
#106276=DIRECTION('center_axis',(-4.93038065763132E-32,-1.97215226305253E-31,
1.));
#106277=DIRECTION('ref_axis',(1.,0.,4.93038065763132E-32));
#106278=DIRECTION('center_axis',(-4.93038065763132E-32,-1.97215226305253E-31,
1.));
#106279=DIRECTION('ref_axis',(1.,0.,4.93038065763132E-32));
#106280=DIRECTION('center_axis',(-4.93038065763132E-32,-1.97215226305253E-31,
1.));
#106281=DIRECTION('ref_axis',(-0.464722744083384,0.885456250264015,1.51712854493318E-31));
#106282=DIRECTION('center_axis',(4.93038065763132E-32,1.97215226305253E-31,
-1.));
#106283=DIRECTION('ref_axis',(1.,0.,4.93038065763132E-32));
#106284=DIRECTION('',(-0.415660658584274,0.791976146676961,-0.447213595499958));
#106285=DIRECTION('center_axis',(4.93038065763132E-32,1.97215226305253E-31,
-1.));
#106286=DIRECTION('ref_axis',(1.,7.65671051465626E-16,4.93038065763134E-32));
#106287=DIRECTION('center_axis',(4.93038065763132E-32,1.97215226305253E-31,
-1.));
#106288=DIRECTION('ref_axis',(1.,0.,4.93038065763132E-32));
#106289=DIRECTION('center_axis',(4.93038065763132E-32,1.97215226305253E-31,
-1.));
#106290=DIRECTION('ref_axis',(-0.464722744083384,0.885456250264015,1.51712854493318E-31));
#106291=DIRECTION('',(-0.415660658584278,0.791976146676969,0.447213595499941));
#106292=DIRECTION('center_axis',(4.93038065763132E-32,1.97215226305253E-31,
-1.));
#106293=DIRECTION('ref_axis',(1.,0.,4.93038065763132E-32));
#106294=DIRECTION('',(-4.93038065763132E-32,-1.97215226305253E-31,1.));
#106295=DIRECTION('center_axis',(-4.93038065763132E-32,-1.97215226305253E-31,
1.));
#106296=DIRECTION('ref_axis',(1.,0.,4.93038065763132E-32));
#106297=DIRECTION('center_axis',(-4.93038065763132E-32,-1.97215226305253E-31,
1.));
#106298=DIRECTION('ref_axis',(1.,0.,4.93038065763132E-32));
#106299=DIRECTION('center_axis',(-4.93038065763132E-32,-1.97215226305253E-31,
1.));
#106300=DIRECTION('ref_axis',(-0.464722744083384,0.885456250264015,1.51712854493318E-31));
#106301=DIRECTION('center_axis',(4.93038065763132E-32,1.97215226305253E-31,
-1.));
#106302=DIRECTION('ref_axis',(1.,0.,4.93038065763132E-32));
#106303=DIRECTION('',(-0.415660658584274,0.791976146676961,-0.447213595499958));
#106304=DIRECTION('center_axis',(4.93038065763132E-32,1.97215226305253E-31,
-1.));
#106305=DIRECTION('ref_axis',(1.,7.65671051465626E-16,4.93038065763134E-32));
#106306=DIRECTION('center_axis',(4.93038065763132E-32,1.97215226305253E-31,
-1.));
#106307=DIRECTION('ref_axis',(1.,0.,4.93038065763132E-32));
#106308=DIRECTION('center_axis',(4.93038065763132E-32,1.97215226305253E-31,
-1.));
#106309=DIRECTION('ref_axis',(-0.464722744083384,0.885456250264015,1.51712854493318E-31));
#106310=DIRECTION('',(-0.415660658584278,0.791976146676969,0.447213595499941));
#106311=DIRECTION('center_axis',(4.93038065763132E-32,1.97215226305253E-31,
-1.));
#106312=DIRECTION('ref_axis',(1.,0.,4.93038065763132E-32));
#106313=DIRECTION('',(-4.93038065763132E-32,-1.97215226305253E-31,1.));
#106314=DIRECTION('center_axis',(-4.93038065763132E-32,-1.97215226305253E-31,
1.));
#106315=DIRECTION('ref_axis',(1.,0.,4.93038065763132E-32));
#106316=DIRECTION('center_axis',(-4.93038065763132E-32,-1.97215226305253E-31,
1.));
#106317=DIRECTION('ref_axis',(1.,0.,4.93038065763132E-32));
#106318=DIRECTION('center_axis',(-4.93038065763132E-32,-1.97215226305253E-31,
1.));
#106319=DIRECTION('ref_axis',(-0.464722744083384,0.885456250264015,1.51712854493318E-31));
#106320=DIRECTION('center_axis',(4.93038065763132E-32,1.97215226305253E-31,
-1.));
#106321=DIRECTION('ref_axis',(1.,0.,4.93038065763132E-32));
#106322=DIRECTION('',(-0.415660658584274,0.791976146676961,-0.447213595499958));
#106323=DIRECTION('center_axis',(4.93038065763132E-32,1.97215226305253E-31,
-1.));
#106324=DIRECTION('ref_axis',(1.,7.65671051465626E-16,4.93038065763134E-32));
#106325=DIRECTION('center_axis',(4.93038065763132E-32,1.97215226305253E-31,
-1.));
#106326=DIRECTION('ref_axis',(1.,0.,4.93038065763132E-32));
#106327=DIRECTION('center_axis',(4.93038065763132E-32,1.97215226305253E-31,
-1.));
#106328=DIRECTION('ref_axis',(-0.464722744083384,0.885456250264015,1.51712854493318E-31));
#106329=DIRECTION('',(-0.415660658584278,0.791976146676969,0.447213595499941));
#106330=DIRECTION('center_axis',(4.93038065763132E-32,1.97215226305253E-31,
-1.));
#106331=DIRECTION('ref_axis',(1.,0.,4.93038065763132E-32));
#106332=DIRECTION('',(-4.93038065763132E-32,-1.97215226305253E-31,1.));
#106333=DIRECTION('center_axis',(-4.93038065763132E-32,-1.97215226305253E-31,
1.));
#106334=DIRECTION('ref_axis',(1.,0.,4.93038065763132E-32));
#106335=DIRECTION('center_axis',(-4.93038065763132E-32,-1.97215226305253E-31,
1.));
#106336=DIRECTION('ref_axis',(1.,0.,4.93038065763132E-32));
#106337=DIRECTION('center_axis',(-4.93038065763132E-32,-1.97215226305253E-31,
1.));
#106338=DIRECTION('ref_axis',(-0.464722744083384,0.885456250264015,1.51712854493318E-31));
#106339=DIRECTION('center_axis',(4.93038065763132E-32,1.97215226305253E-31,
-1.));
#106340=DIRECTION('ref_axis',(1.,0.,4.93038065763132E-32));
#106341=DIRECTION('',(-0.415660658584274,0.791976146676961,-0.447213595499958));
#106342=DIRECTION('center_axis',(4.93038065763132E-32,1.97215226305253E-31,
-1.));
#106343=DIRECTION('ref_axis',(1.,7.65671051465626E-16,4.93038065763134E-32));
#106344=DIRECTION('center_axis',(4.93038065763132E-32,1.97215226305253E-31,
-1.));
#106345=DIRECTION('ref_axis',(1.,0.,4.93038065763132E-32));
#106346=DIRECTION('center_axis',(4.93038065763132E-32,1.97215226305253E-31,
-1.));
#106347=DIRECTION('ref_axis',(-0.464722744083384,0.885456250264015,1.51712854493318E-31));
#106348=DIRECTION('',(-0.415660658584278,0.791976146676969,0.447213595499941));
#106349=DIRECTION('center_axis',(4.93038065763132E-32,1.97215226305253E-31,
-1.));
#106350=DIRECTION('ref_axis',(1.,0.,4.93038065763132E-32));
#106351=DIRECTION('',(-4.93038065763132E-32,-1.97215226305253E-31,1.));
#106352=DIRECTION('center_axis',(-4.93038065763132E-32,-1.97215226305253E-31,
1.));
#106353=DIRECTION('ref_axis',(1.,0.,4.93038065763132E-32));
#106354=DIRECTION('center_axis',(-4.93038065763132E-32,-1.97215226305253E-31,
1.));
#106355=DIRECTION('ref_axis',(1.,0.,4.93038065763132E-32));
#106356=DIRECTION('center_axis',(-4.93038065763132E-32,-1.97215226305253E-31,
1.));
#106357=DIRECTION('ref_axis',(-0.464722744083384,0.885456250264015,1.51712854493318E-31));
#106358=DIRECTION('center_axis',(4.93038065763132E-32,1.97215226305253E-31,
-1.));
#106359=DIRECTION('ref_axis',(1.,0.,4.93038065763132E-32));
#106360=DIRECTION('',(-0.415660658584274,0.791976146676961,-0.447213595499958));
#106361=DIRECTION('center_axis',(4.93038065763132E-32,1.97215226305253E-31,
-1.));
#106362=DIRECTION('ref_axis',(1.,7.65671051465626E-16,4.93038065763134E-32));
#106363=DIRECTION('center_axis',(4.93038065763132E-32,1.97215226305253E-31,
-1.));
#106364=DIRECTION('ref_axis',(1.,0.,4.93038065763132E-32));
#106365=DIRECTION('center_axis',(4.93038065763132E-32,1.97215226305253E-31,
-1.));
#106366=DIRECTION('ref_axis',(-0.464722744083384,0.885456250264015,1.51712854493318E-31));
#106367=DIRECTION('',(-0.415660658584278,0.791976146676969,0.447213595499941));
#106368=DIRECTION('center_axis',(4.93038065763132E-32,1.97215226305253E-31,
-1.));
#106369=DIRECTION('ref_axis',(1.,0.,4.93038065763132E-32));
#106370=DIRECTION('',(-4.93038065763132E-32,-1.97215226305253E-31,1.));
#106371=DIRECTION('center_axis',(-4.93038065763132E-32,-1.97215226305253E-31,
1.));
#106372=DIRECTION('ref_axis',(1.,0.,4.93038065763132E-32));
#106373=DIRECTION('center_axis',(-4.93038065763132E-32,-1.97215226305253E-31,
1.));
#106374=DIRECTION('ref_axis',(1.,0.,4.93038065763132E-32));
#106375=DIRECTION('center_axis',(-4.93038065763132E-32,-1.97215226305253E-31,
1.));
#106376=DIRECTION('ref_axis',(-0.464722744083384,0.885456250264015,1.51712854493318E-31));
#106377=DIRECTION('center_axis',(4.93038065763132E-32,1.97215226305253E-31,
-1.));
#106378=DIRECTION('ref_axis',(1.,0.,4.93038065763132E-32));
#106379=DIRECTION('',(-0.415660658584274,0.791976146676961,-0.447213595499958));
#106380=DIRECTION('center_axis',(4.93038065763132E-32,1.97215226305253E-31,
-1.));
#106381=DIRECTION('ref_axis',(1.,7.65671051465626E-16,4.93038065763134E-32));
#106382=DIRECTION('center_axis',(4.93038065763132E-32,1.97215226305253E-31,
-1.));
#106383=DIRECTION('ref_axis',(1.,0.,4.93038065763132E-32));
#106384=DIRECTION('center_axis',(4.93038065763132E-32,1.97215226305253E-31,
-1.));
#106385=DIRECTION('ref_axis',(-0.464722744083384,0.885456250264015,1.51712854493318E-31));
#106386=DIRECTION('',(-0.415660658584278,0.791976146676969,0.447213595499941));
#106387=DIRECTION('center_axis',(4.93038065763132E-32,1.97215226305253E-31,
-1.));
#106388=DIRECTION('ref_axis',(1.,0.,4.93038065763132E-32));
#106389=DIRECTION('',(-4.93038065763132E-32,-1.97215226305253E-31,1.));
#106390=DIRECTION('center_axis',(-4.93038065763132E-32,-1.97215226305253E-31,
1.));
#106391=DIRECTION('ref_axis',(1.,0.,4.93038065763132E-32));
#106392=DIRECTION('center_axis',(-4.93038065763132E-32,-1.97215226305253E-31,
1.));
#106393=DIRECTION('ref_axis',(1.,0.,4.93038065763132E-32));
#106394=DIRECTION('center_axis',(-4.93038065763132E-32,-1.97215226305253E-31,
1.));
#106395=DIRECTION('ref_axis',(-0.464722744083384,0.885456250264015,1.51712854493318E-31));
#106396=DIRECTION('center_axis',(4.93038065763132E-32,1.97215226305253E-31,
-1.));
#106397=DIRECTION('ref_axis',(1.,0.,4.93038065763132E-32));
#106398=DIRECTION('',(-0.415660658584274,0.791976146676961,-0.447213595499958));
#106399=DIRECTION('center_axis',(4.93038065763132E-32,1.97215226305253E-31,
-1.));
#106400=DIRECTION('ref_axis',(1.,7.65671051465626E-16,4.93038065763134E-32));
#106401=DIRECTION('center_axis',(4.93038065763132E-32,1.97215226305253E-31,
-1.));
#106402=DIRECTION('ref_axis',(1.,0.,4.93038065763132E-32));
#106403=DIRECTION('center_axis',(4.93038065763132E-32,1.97215226305253E-31,
-1.));
#106404=DIRECTION('ref_axis',(-0.464722744083384,0.885456250264015,1.51712854493318E-31));
#106405=DIRECTION('',(-0.415660658584278,0.791976146676969,0.447213595499941));
#106406=DIRECTION('center_axis',(4.93038065763132E-32,1.97215226305253E-31,
-1.));
#106407=DIRECTION('ref_axis',(1.,0.,4.93038065763132E-32));
#106408=DIRECTION('',(-4.93038065763132E-32,-1.97215226305253E-31,1.));
#106409=DIRECTION('center_axis',(-4.93038065763132E-32,-1.97215226305253E-31,
1.));
#106410=DIRECTION('ref_axis',(1.,0.,4.93038065763132E-32));
#106411=DIRECTION('center_axis',(-4.93038065763132E-32,-1.97215226305253E-31,
1.));
#106412=DIRECTION('ref_axis',(1.,0.,4.93038065763132E-32));
#106413=DIRECTION('center_axis',(-4.93038065763132E-32,-1.97215226305253E-31,
1.));
#106414=DIRECTION('ref_axis',(-0.464722744083384,0.885456250264015,1.51712854493318E-31));
#106415=DIRECTION('center_axis',(4.93038065763132E-32,1.97215226305253E-31,
-1.));
#106416=DIRECTION('ref_axis',(1.,0.,4.93038065763132E-32));
#106417=DIRECTION('',(-0.415660658584274,0.791976146676961,-0.447213595499958));
#106418=DIRECTION('center_axis',(4.93038065763132E-32,1.97215226305253E-31,
-1.));
#106419=DIRECTION('ref_axis',(1.,7.65671051465626E-16,4.93038065763134E-32));
#106420=DIRECTION('center_axis',(4.93038065763132E-32,1.97215226305253E-31,
-1.));
#106421=DIRECTION('ref_axis',(1.,0.,4.93038065763132E-32));
#106422=DIRECTION('center_axis',(4.93038065763132E-32,1.97215226305253E-31,
-1.));
#106423=DIRECTION('ref_axis',(-0.464722744083384,0.885456250264015,1.51712854493318E-31));
#106424=DIRECTION('',(-0.415660658584278,0.791976146676969,0.447213595499941));
#106425=DIRECTION('center_axis',(4.93038065763132E-32,1.97215226305253E-31,
-1.));
#106426=DIRECTION('ref_axis',(1.,0.,4.93038065763132E-32));
#106427=DIRECTION('',(-4.93038065763132E-32,-1.97215226305253E-31,1.));
#106428=DIRECTION('center_axis',(-4.93038065763132E-32,-1.97215226305253E-31,
1.));
#106429=DIRECTION('ref_axis',(1.,0.,4.93038065763132E-32));
#106430=DIRECTION('center_axis',(-4.93038065763132E-32,-1.97215226305253E-31,
1.));
#106431=DIRECTION('ref_axis',(1.,0.,4.93038065763132E-32));
#106432=DIRECTION('center_axis',(-4.93038065763132E-32,-1.97215226305253E-31,
1.));
#106433=DIRECTION('ref_axis',(-0.464722744083384,0.885456250264015,1.51712854493318E-31));
#106434=DIRECTION('center_axis',(4.93038065763132E-32,1.97215226305253E-31,
-1.));
#106435=DIRECTION('ref_axis',(1.,0.,4.93038065763132E-32));
#106436=DIRECTION('',(-0.415660658584274,0.791976146676961,-0.447213595499958));
#106437=DIRECTION('center_axis',(4.93038065763132E-32,1.97215226305253E-31,
-1.));
#106438=DIRECTION('ref_axis',(1.,7.65671051465626E-16,4.93038065763134E-32));
#106439=DIRECTION('center_axis',(4.93038065763132E-32,1.97215226305253E-31,
-1.));
#106440=DIRECTION('ref_axis',(1.,0.,4.93038065763132E-32));
#106441=DIRECTION('center_axis',(4.93038065763132E-32,1.97215226305253E-31,
-1.));
#106442=DIRECTION('ref_axis',(-0.464722744083384,0.885456250264015,1.51712854493318E-31));
#106443=DIRECTION('',(-0.415660658584278,0.791976146676969,0.447213595499941));
#106444=DIRECTION('center_axis',(4.93038065763132E-32,1.97215226305253E-31,
-1.));
#106445=DIRECTION('ref_axis',(0.415323571508097,0.909673749731055,1.99878547453377E-31));
#106446=DIRECTION('center_axis',(4.93038065763132E-32,1.97215226305253E-31,
-1.));
#106447=DIRECTION('ref_axis',(1.,0.,4.93038065763132E-32));
#106448=DIRECTION('',(-4.93038065763132E-32,-1.97215226305253E-31,1.));
#106449=DIRECTION('center_axis',(4.93038065763132E-32,1.97215226305253E-31,
-1.));
#106450=DIRECTION('ref_axis',(1.,0.,4.93038065763132E-32));
#106451=DIRECTION('center_axis',(4.93038065763132E-32,1.97215226305253E-31,
-1.));
#106452=DIRECTION('ref_axis',(1.,0.,4.93038065763132E-32));
#106453=DIRECTION('center_axis',(-4.93038065763132E-32,-1.97215226305253E-31,
1.));
#106454=DIRECTION('ref_axis',(-0.464722744083384,0.885456250264015,1.51712854493318E-31));
#106455=DIRECTION('center_axis',(-4.93038065763132E-32,-1.97215226305253E-31,
1.));
#106456=DIRECTION('ref_axis',(1.,0.,4.93038065763132E-32));
#106457=DIRECTION('center_axis',(-4.93038065763132E-32,-1.97215226305253E-31,
1.));
#106458=DIRECTION('ref_axis',(1.,0.,4.93038065763132E-32));
#106459=DIRECTION('',(-0.415660658584274,0.791976146676961,-0.447213595499958));
#106460=DIRECTION('center_axis',(4.93038065763132E-32,1.97215226305253E-31,
-1.));
#106461=DIRECTION('ref_axis',(1.,7.65671051465626E-16,4.93038065763134E-32));
#106462=DIRECTION('center_axis',(4.93038065763132E-32,1.97215226305253E-31,
-1.));
#106463=DIRECTION('ref_axis',(-0.464722744083384,0.885456250264015,1.51712854493318E-31));
#106464=DIRECTION('',(-0.415660658584278,0.791976146676969,0.447213595499941));
#106465=DIRECTION('center_axis',(4.93038065763132E-32,1.97215226305253E-31,
-1.));
#106466=DIRECTION('ref_axis',(1.,0.,4.93038065763132E-32));
#106467=DIRECTION('',(-4.93038065763132E-32,-1.97215226305253E-31,1.));
#106468=DIRECTION('center_axis',(4.93038065763132E-32,1.97215226305253E-31,
-1.));
#106469=DIRECTION('ref_axis',(1.,0.,4.93038065763132E-32));
#106470=DIRECTION('',(-4.93038065763132E-32,-1.97215226305253E-31,1.));
#106471=DIRECTION('center_axis',(-0.415323571356916,-0.909673749800079,
-1.99878547459536E-31));
#106472=DIRECTION('ref_axis',(-0.909673749800079,0.415323571356916,3.70577535073674E-32));
#106473=DIRECTION('center_axis',(4.93038065763132E-32,1.97215226305253E-31,
-1.));
#106474=DIRECTION('ref_axis',(-1.,0.,-4.93038065763132E-32));
#106475=DIRECTION('axis',(0.,0.,1.));
#106476=DIRECTION('refdir',(1.,0.,0.));
#106477=DIRECTION('center_axis',(0.,0.,-1.));
#106478=DIRECTION('ref_axis',(-1.,0.,0.));
#106479=DIRECTION('',(1.,-1.05190123196885E-16,0.));
#106480=DIRECTION('center_axis',(0.,0.,-1.));
#106481=DIRECTION('ref_axis',(-1.,0.,0.));
#106482=DIRECTION('',(1.75316871994808E-16,1.,0.));
#106483=DIRECTION('center_axis',(0.,0.,-1.));
#106484=DIRECTION('ref_axis',(-1.,0.,0.));
#106485=DIRECTION('center_axis',(0.,0.,-1.));
#106486=DIRECTION('ref_axis',(-1.,0.,0.));
#106487=DIRECTION('',(-1.,1.75316871994808E-16,0.));
#106488=DIRECTION('center_axis',(0.,0.,-1.));
#106489=DIRECTION('ref_axis',(-1.,0.,0.));
#106490=DIRECTION('',(1.05190123196885E-16,1.,0.));
#106491=DIRECTION('center_axis',(0.,0.,-1.));
#106492=DIRECTION('ref_axis',(-1.,0.,0.));
#106493=DIRECTION('center_axis',(0.,0.,-1.));
#106494=DIRECTION('ref_axis',(-1.,0.,0.));
#106495=DIRECTION('',(-1.75316871994808E-16,-1.,0.));
#106496=DIRECTION('center_axis',(0.,0.,-1.));
#106497=DIRECTION('ref_axis',(-1.,0.,0.));
#106498=DIRECTION('',(-1.,1.05190123196885E-16,0.));
#106499=DIRECTION('center_axis',(0.,0.,-1.));
#106500=DIRECTION('ref_axis',(-1.,0.,0.));
#106501=DIRECTION('center_axis',(0.,0.,1.));
#106502=DIRECTION('ref_axis',(1.,0.,0.));
#106503=DIRECTION('center_axis',(0.,0.,-1.));
#106504=DIRECTION('ref_axis',(-1.,0.,0.));
#106505=DIRECTION('center_axis',(0.,0.,1.));
#106506=DIRECTION('ref_axis',(1.,0.,0.));
#106507=DIRECTION('center_axis',(0.,0.,-1.));
#106508=DIRECTION('ref_axis',(-1.,0.,0.));
#106509=DIRECTION('center_axis',(0.,0.,1.));
#106510=DIRECTION('ref_axis',(1.,0.,0.));
#106511=DIRECTION('center_axis',(0.,0.,-1.));
#106512=DIRECTION('ref_axis',(-1.,0.,0.));
#106513=DIRECTION('center_axis',(0.,0.,-1.));
#106514=DIRECTION('ref_axis',(-1.,0.,0.));
#106515=DIRECTION('center_axis',(0.,0.,-1.));
#106516=DIRECTION('ref_axis',(-1.,0.,0.));
#106517=DIRECTION('center_axis',(0.,0.,-1.));
#106518=DIRECTION('ref_axis',(-1.,0.,0.));
#106519=DIRECTION('center_axis',(0.,0.,-1.));
#106520=DIRECTION('ref_axis',(-1.,0.,0.));
#106521=DIRECTION('center_axis',(0.,0.,-1.));
#106522=DIRECTION('ref_axis',(-1.,0.,0.));
#106523=DIRECTION('center_axis',(0.,0.,-1.));
#106524=DIRECTION('ref_axis',(-1.,0.,0.));
#106525=DIRECTION('center_axis',(0.,0.,1.));
#106526=DIRECTION('ref_axis',(1.,0.,0.));
#106527=DIRECTION('',(-1.,1.05190123196885E-16,0.));
#106528=DIRECTION('center_axis',(0.,0.,-1.));
#106529=DIRECTION('ref_axis',(-1.,0.,0.));
#106530=DIRECTION('',(-1.75316871994808E-16,-1.,0.));
#106531=DIRECTION('center_axis',(0.,0.,1.));
#106532=DIRECTION('ref_axis',(1.,0.,0.));
#106533=DIRECTION('',(1.,-1.75316871994808E-16,0.));
#106534=DIRECTION('',(-1.05190123196885E-16,-1.,0.));
#106535=DIRECTION('center_axis',(0.,0.,-1.));
#106536=DIRECTION('ref_axis',(-1.,0.,0.));
#106537=DIRECTION('center_axis',(0.,0.,1.));
#106538=DIRECTION('ref_axis',(1.,0.,0.));
#106539=DIRECTION('',(1.75316871994808E-16,1.,0.));
#106540=DIRECTION('',(1.,-1.05190123196885E-16,0.));
#106541=DIRECTION('center_axis',(0.,0.,-1.));
#106542=DIRECTION('ref_axis',(-1.,0.,0.));
#106543=DIRECTION('center_axis',(0.,0.,-1.));
#106544=DIRECTION('ref_axis',(-1.,0.,0.));
#106545=DIRECTION('center_axis',(0.,0.,-1.));
#106546=DIRECTION('ref_axis',(-1.,0.,0.));
#106547=DIRECTION('',(0.,0.,-1.));
#106548=DIRECTION('center_axis',(0.,0.,-1.));
#106549=DIRECTION('ref_axis',(-1.,0.,0.));
#106550=DIRECTION('',(0.,0.,-1.));
#106551=DIRECTION('',(0.,0.,-1.));
#106552=DIRECTION('center_axis',(0.,0.,-1.));
#106553=DIRECTION('ref_axis',(-1.,0.,0.));
#106554=DIRECTION('',(0.,0.,-1.));
#106555=DIRECTION('',(0.,0.,-1.));
#106556=DIRECTION('center_axis',(0.,0.,-1.));
#106557=DIRECTION('ref_axis',(-1.,0.,0.));
#106558=DIRECTION('',(0.,0.,-1.));
#106559=DIRECTION('',(0.,0.,-1.));
#106560=DIRECTION('center_axis',(0.,0.,-1.));
#106561=DIRECTION('ref_axis',(-1.,0.,0.));
#106562=DIRECTION('',(0.,0.,-1.));
#106563=DIRECTION('center_axis',(0.,0.,-1.));
#106564=DIRECTION('ref_axis',(-1.,0.,0.));
#106565=DIRECTION('',(0.,0.,-1.));
#106566=DIRECTION('center_axis',(0.,0.,-1.));
#106567=DIRECTION('ref_axis',(-1.,0.,0.));
#106568=DIRECTION('center_axis',(0.,0.,-1.));
#106569=DIRECTION('ref_axis',(-1.,0.,0.));
#106570=DIRECTION('',(-1.05190123196885E-16,-1.,0.));
#106571=DIRECTION('center_axis',(0.,0.,-1.));
#106572=DIRECTION('ref_axis',(-1.,0.,0.));
#106573=DIRECTION('',(1.,-1.75316871994808E-16,0.));
#106574=DIRECTION('center_axis',(0.,0.,1.));
#106575=DIRECTION('ref_axis',(1.,0.,0.));
#106576=DIRECTION('center_axis',(0.,0.,-1.));
#106577=DIRECTION('ref_axis',(-1.,0.,0.));
#106578=DIRECTION('center_axis',(0.,0.,-1.));
#106579=DIRECTION('ref_axis',(-1.,0.,0.));
#106580=DIRECTION('center_axis',(0.,0.,-1.));
#106581=DIRECTION('ref_axis',(-1.,0.,0.));
#106582=DIRECTION('center_axis',(0.,0.,1.));
#106583=DIRECTION('ref_axis',(1.,0.,0.));
#106584=DIRECTION('',(1.05190123196885E-16,1.,0.));
#106585=DIRECTION('center_axis',(0.,0.,-1.));
#106586=DIRECTION('ref_axis',(-1.,0.,0.));
#106587=DIRECTION('',(-1.,1.75316871994808E-16,0.));
#106588=DIRECTION('center_axis',(0.,0.,-1.));
#106589=DIRECTION('ref_axis',(-1.,0.,0.));
#106590=DIRECTION('center_axis',(0.,0.,-1.));
#106591=DIRECTION('ref_axis',(-1.,0.,0.));
#106592=DIRECTION('',(0.,0.,1.));
#106593=DIRECTION('center_axis',(0.,0.,-1.));
#106594=DIRECTION('ref_axis',(-1.,0.,0.));
#106595=DIRECTION('center_axis',(0.,0.,-1.));
#106596=DIRECTION('ref_axis',(-1.,0.,0.));
#106597=DIRECTION('',(0.,0.,-1.));
#106598=DIRECTION('',(0.,0.,-1.));
#106599=DIRECTION('center_axis',(0.,0.,-1.));
#106600=DIRECTION('ref_axis',(-1.,0.,0.));
#106601=DIRECTION('',(0.,0.,-1.));
#106602=DIRECTION('',(0.,0.,-1.));
#106603=DIRECTION('center_axis',(0.,0.,-1.));
#106604=DIRECTION('ref_axis',(-1.,0.,0.));
#106605=DIRECTION('',(0.,0.,-1.));
#106606=DIRECTION('',(0.,0.,-1.));
#106607=DIRECTION('center_axis',(0.,0.,-1.));
#106608=DIRECTION('ref_axis',(-1.,0.,0.));
#106609=DIRECTION('',(0.,0.,-1.));
#106610=DIRECTION('',(0.,0.,-1.));
#106611=DIRECTION('center_axis',(0.,0.,-1.));
#106612=DIRECTION('ref_axis',(-1.,0.,0.));
#106613=DIRECTION('center_axis',(0.,0.,-1.));
#106614=DIRECTION('ref_axis',(-1.,0.,0.));
#106615=DIRECTION('center_axis',(0.,0.,-1.));
#106616=DIRECTION('ref_axis',(-1.,0.,0.));
#106617=DIRECTION('',(0.,0.,1.));
#106618=DIRECTION('center_axis',(0.,0.,-1.));
#106619=DIRECTION('ref_axis',(-1.,0.,0.));
#106620=DIRECTION('center_axis',(0.,0.,1.));
#106621=DIRECTION('ref_axis',(1.,0.,0.));
#106622=DIRECTION('center_axis',(1.75316871994808E-16,1.,0.));
#106623=DIRECTION('ref_axis',(-1.,1.75316871994808E-16,0.));
#106624=DIRECTION('',(1.,-1.75316871994808E-16,0.));
#106625=DIRECTION('center_axis',(-1.05190123196885E-16,-1.,0.));
#106626=DIRECTION('ref_axis',(1.,-1.05190123196885E-16,0.));
#106627=DIRECTION('',(-1.,1.05190123196885E-16,0.));
#106628=DIRECTION('center_axis',(0.,0.,-1.));
#106629=DIRECTION('ref_axis',(-1.,0.,0.));
#106630=DIRECTION('center_axis',(-1.,1.75316871994808E-16,0.));
#106631=DIRECTION('ref_axis',(-1.75316871994808E-16,-1.,0.));
#106632=DIRECTION('',(1.75316871994808E-16,1.,0.));
#106633=DIRECTION('center_axis',(1.,-1.05190123196885E-16,0.));
#106634=DIRECTION('ref_axis',(1.05190123196885E-16,1.,0.));
#106635=DIRECTION('',(-1.05190123196885E-16,-1.,0.));
#106636=DIRECTION('center_axis',(0.,0.,-1.));
#106637=DIRECTION('ref_axis',(-1.,0.,0.));
#106638=DIRECTION('center_axis',(-1.,1.05190123196885E-16,0.));
#106639=DIRECTION('ref_axis',(-1.05190123196885E-16,-1.,0.));
#106640=DIRECTION('',(1.05190123196885E-16,1.,0.));
#106641=DIRECTION('center_axis',(1.,-1.75316871994808E-16,0.));
#106642=DIRECTION('ref_axis',(1.75316871994808E-16,1.,0.));
#106643=DIRECTION('',(-1.75316871994808E-16,-1.,0.));
#106644=DIRECTION('center_axis',(0.,0.,-1.));
#106645=DIRECTION('ref_axis',(-1.,0.,0.));
#106646=DIRECTION('center_axis',(1.05190123196885E-16,1.,0.));
#106647=DIRECTION('ref_axis',(-1.,1.05190123196885E-16,0.));
#106648=DIRECTION('',(1.,-1.05190123196885E-16,0.));
#106649=DIRECTION('center_axis',(-1.75316871994808E-16,-1.,0.));
#106650=DIRECTION('ref_axis',(1.,-1.75316871994808E-16,0.));
#106651=DIRECTION('',(-1.,1.75316871994808E-16,0.));
#106652=DIRECTION('center_axis',(0.,0.,-1.));
#106653=DIRECTION('ref_axis',(-1.,0.,0.));
#106654=DIRECTION('center_axis',(0.,0.,-1.));
#106655=DIRECTION('ref_axis',(-0.953462589245592,-0.301511344577763,0.));
#106656=DIRECTION('center_axis',(1.66533453693558E-16,-1.98164517174841E-27,
1.));
#106657=DIRECTION('ref_axis',(-0.953462589245592,-0.301511344577763,0.));
#106658=DIRECTION('',(0.,0.,1.));
#106659=DIRECTION('center_axis',(-1.66533453693558E-16,1.98164517174841E-27,
-1.));
#106660=DIRECTION('ref_axis',(-0.953462589245592,-0.301511344577763,0.));
#106661=DIRECTION('',(0.,0.,-1.));
#106662=DIRECTION('center_axis',(-1.,4.69089087030665E-43,0.));
#106663=DIRECTION('ref_axis',(4.69089087030665E-43,1.,1.98164517174841E-27));
#106664=DIRECTION('',(4.69089087030665E-43,1.,1.98164517174841E-27));
#106665=DIRECTION('',(0.,0.,1.));
#106666=DIRECTION('',(4.69089087030665E-43,1.,1.98164517174841E-27));
#106667=DIRECTION('center_axis',(-1.66533453693558E-16,1.98164517174841E-27,
-1.));
#106668=DIRECTION('ref_axis',(1.,-1.39078872584238E-43,-1.66533453693558E-16));
#106669=DIRECTION('center_axis',(-1.66533453693558E-16,1.98164517174841E-27,
-1.));
#106670=DIRECTION('ref_axis',(0.793103448275862,0.609086956298473,-1.32078256376442E-16));
#106671=DIRECTION('center_axis',(-1.66533453693558E-16,1.98164517174841E-27,
-1.));
#106672=DIRECTION('ref_axis',(0.953462589245592,-0.301511344577763,0.));
#106673=DIRECTION('',(4.69089087030665E-43,1.,1.98164517174841E-27));
#106674=DIRECTION('center_axis',(-1.66533453693558E-16,1.98164517174841E-27,
-1.));
#106675=DIRECTION('ref_axis',(0.435494170355695,0.900191550497007,0.));
#106676=DIRECTION('center_axis',(-1.66533453693558E-16,1.98164517174841E-27,
-1.));
#106677=DIRECTION('ref_axis',(-0.589473684210526,-0.807787580755776,9.81670884914437E-17));
#106678=DIRECTION('',(4.69089087030665E-43,1.,1.98164517174841E-27));
#106679=DIRECTION('',(1.,-1.39078872584238E-43,-1.66533453693558E-16));
#106680=DIRECTION('',(4.69089087030665E-43,1.,1.98164517174841E-27));
#106681=DIRECTION('center_axis',(-1.66533453693558E-16,1.98164517174841E-27,
-1.));
#106682=DIRECTION('ref_axis',(0.484210526315789,0.874951522202794,-8.06372512604098E-17));
#106683=DIRECTION('center_axis',(-1.66533453693558E-16,1.98164517174841E-27,
-1.));
#106684=DIRECTION('ref_axis',(-0.435494170355695,0.900191550497007,0.));
#106685=DIRECTION('center_axis',(0.,0.,-1.));
#106686=DIRECTION('ref_axis',(-0.435494170355695,0.900191550497007,0.));
#106687=DIRECTION('center_axis',(1.66533453693558E-16,-1.98164517174841E-27,
1.));
#106688=DIRECTION('ref_axis',(-0.435494170355695,0.900191550497007,0.));
#106689=DIRECTION('',(0.,0.,-1.));
#106690=DIRECTION('center_axis',(0.,0.,-1.));
#106691=DIRECTION('ref_axis',(0.484210526315789,0.874951522202794,0.));
#106692=DIRECTION('',(0.,0.,-1.));
#106693=DIRECTION('center_axis',(-1.66533453693558E-16,1.98164517174841E-27,
-1.));
#106694=DIRECTION('ref_axis',(0.484210526315789,0.874951522202794,-8.06372512604098E-17));
#106695=DIRECTION('center_axis',(0.,0.,-1.));
#106696=DIRECTION('ref_axis',(0.953462589245592,-0.301511344577763,0.));
#106697=DIRECTION('center_axis',(1.66533453693558E-16,-1.98164517174841E-27,
1.));
#106698=DIRECTION('ref_axis',(0.953462589245592,-0.301511344577763,0.));
#106699=DIRECTION('',(0.,0.,1.));
#106700=DIRECTION('',(0.,0.,-1.));
#106701=DIRECTION('center_axis',(0.,0.,-1.));
#106702=DIRECTION('ref_axis',(1.91417762866406E-16,-1.,0.));
#106703=DIRECTION('center_axis',(1.66533453693558E-16,-1.98164517174841E-27,
1.));
#106704=DIRECTION('ref_axis',(0.793103448275862,0.609086956298473,-1.32078256376442E-16));
#106705=DIRECTION('center_axis',(0.,0.,-1.));
#106706=DIRECTION('ref_axis',(0.435494170355695,0.900191550497007,0.));
#106707=DIRECTION('center_axis',(1.66533453693558E-16,-1.98164517174841E-27,
1.));
#106708=DIRECTION('ref_axis',(0.435494170355695,0.900191550497007,0.));
#106709=DIRECTION('',(0.,0.,1.));
#106710=DIRECTION('',(0.,0.,-1.));
#106711=DIRECTION('center_axis',(0.,0.,-1.));
#106712=DIRECTION('ref_axis',(-0.589473684210526,-0.807787580755776,0.));
#106713=DIRECTION('center_axis',(-1.66533453693558E-16,1.98164517174841E-27,
-1.));
#106714=DIRECTION('ref_axis',(-0.589473684210526,-0.807787580755776,9.81670884914437E-17));
#106715=DIRECTION('',(0.,0.,-1.));
#106716=DIRECTION('center_axis',(1.39078872584238E-43,1.,-4.28912684949805E-59));
#106717=DIRECTION('ref_axis',(-1.,1.39078872584238E-43,1.66533453693558E-16));
#106718=DIRECTION('',(3.08395284618099E-16,0.,1.));
#106719=DIRECTION('',(-1.,1.39078872584238E-43,1.66533453693558E-16));
#106720=DIRECTION('',(3.08395284618099E-16,0.,1.));
#106721=DIRECTION('center_axis',(3.08395284618099E-16,0.,1.));
#106722=DIRECTION('ref_axis',(1.,0.,-3.08395284618099E-16));
#106723=DIRECTION('',(-4.69089087030665E-43,-1.,-1.98164517174841E-27));
#106724=DIRECTION('',(1.,-1.39078872584238E-43,-1.66533453693558E-16));
#106725=DIRECTION('',(4.69089087030665E-43,1.,1.98164517174841E-27));
#106726=DIRECTION('center_axis',(-1.39078872584238E-43,-1.,0.));
#106727=DIRECTION('ref_axis',(-1.,1.39078872584238E-43,1.66533453693558E-16));
#106728=DIRECTION('',(3.08395284618099E-16,0.,1.));
#106729=DIRECTION('',(-1.,1.39078872584238E-43,1.66533453693558E-16));
#106730=DIRECTION('',(0.,0.,-1.));
#106731=DIRECTION('center_axis',(1.,-4.69089087030665E-43,0.));
#106732=DIRECTION('ref_axis',(-4.69089087030665E-43,-1.,-1.98164517174841E-27));
#106733=DIRECTION('',(-4.69089087030665E-43,-1.,-1.98164517174841E-27));
#106734=DIRECTION('center_axis',(1.,-4.69089087030665E-43,0.));
#106735=DIRECTION('ref_axis',(-4.69089087030665E-43,-1.,-1.98164517174841E-27));
#106736=DIRECTION('',(-4.69089087030665E-43,-1.,-1.98164517174841E-27));
#106737=DIRECTION('center_axis',(-1.,4.69089087030665E-43,0.));
#106738=DIRECTION('ref_axis',(4.69089087030665E-43,1.,1.98164517174841E-27));
#106739=DIRECTION('',(4.69089087030665E-43,1.,1.98164517174841E-27));
#106740=DIRECTION('center_axis',(-1.66533453693558E-16,1.98164517174841E-27,
-1.));
#106741=DIRECTION('ref_axis',(1.,-1.39078872584238E-43,-1.66533453693558E-16));
#106742=DIRECTION('axis',(0.,0.,1.));
#106743=DIRECTION('refdir',(1.,0.,0.));
#106744=DIRECTION('center_axis',(0.707106781187368,-1.61919227945235E-16,
0.707106781185727));
#106745=DIRECTION('ref_axis',(-0.499999999999422,0.707106781186549,0.500000000000576));
#106746=DIRECTION('center_axis',(-0.707106781187366,0.,-0.707106781185729));
#106747=DIRECTION('ref_axis',(-0.707106781185729,0.,0.707106781187366));
#106748=DIRECTION('',(0.707106781187368,-1.61919227945235E-16,0.707106781185727));
#106749=DIRECTION('center_axis',(0.707106781187366,0.,0.707106781185729));
#106750=DIRECTION('ref_axis',(0.,1.,0.));
#106751=DIRECTION('',(-0.707106781187368,1.61919227945235E-16,-0.707106781185727));
#106752=DIRECTION('center_axis',(0.0231981048318895,0.,-0.999730887755404));
#106753=DIRECTION('ref_axis',(0.,1.,0.));
#106754=DIRECTION('center_axis',(-6.93889390390725E-18,-1.,-2.22049474265475E-16));
#106755=DIRECTION('ref_axis',(0.37194083714349,-1.73472347597681E-16,0.928256437448726));
#106756=DIRECTION('center_axis',(6.93889390390725E-18,1.,2.22049474265475E-16));
#106757=DIRECTION('ref_axis',(0.37194083714349,-2.08699711926501E-16,0.928256437448726));
#106758=DIRECTION('center_axis',(-6.93889390390725E-18,-1.,-2.22049474265475E-16));
#106759=DIRECTION('ref_axis',(0.,2.03710646720212E-16,-1.));
#106760=DIRECTION('center_axis',(0.978760432413326,0.,-0.205007355824322));
#106761=DIRECTION('ref_axis',(0.,1.,0.));
#106762=DIRECTION('center_axis',(6.93889390390725E-18,1.,2.22049474265475E-16));
#106763=DIRECTION('ref_axis',(-0.768845497716612,1.49223524815209E-16,-0.639434594498058));
#106764=DIRECTION('center_axis',(-6.93889390390725E-18,-1.,-2.22049474265475E-16));
#106765=DIRECTION('ref_axis',(-0.768845497716612,1.47321052872603E-16,-0.639434594498058));
#106766=DIRECTION('center_axis',(-0.474498912689989,0.,-0.880256088792357));
#106767=DIRECTION('ref_axis',(0.,1.,0.));
#106768=DIRECTION('center_axis',(-6.93889390390725E-18,-1.,-2.22049474265475E-16));
#106769=DIRECTION('ref_axis',(0.906884704407261,-8.67361737988403E-17,0.421378847252867));
#106770=DIRECTION('center_axis',(6.93889390390725E-18,1.,2.22049474265475E-16));
#106771=DIRECTION('ref_axis',(0.906884704407261,-9.98597282460494E-17,0.421378847252868));
#106772=DIRECTION('center_axis',(-6.93889390390725E-18,-1.,-2.22049474265475E-16));
#106773=DIRECTION('ref_axis',(0.,2.24081711397792E-16,-1.));
#106774=DIRECTION('center_axis',(0.0394929644100698,0.,-0.99921984856292));
#106775=DIRECTION('ref_axis',(0.,1.,0.));
#106776=DIRECTION('center_axis',(6.93889390390725E-18,1.,2.22049474265475E-16));
#106777=DIRECTION('ref_axis',(-0.974245534865613,-4.12211519055028E-17,
0.225489773148175));
#106778=DIRECTION('center_axis',(-6.93889390390725E-18,-1.,-2.22049474265475E-16));
#106779=DIRECTION('ref_axis',(-0.974245534865613,-4.33096991770057E-17,
0.225489773148175));
#106780=DIRECTION('center_axis',(-0.97649605508074,-1.49557640001864E-16,
0.215535274170498));
#106781=DIRECTION('ref_axis',(0.,1.,6.93889390390723E-16));
#106782=DIRECTION('center_axis',(-6.93889390390725E-18,-1.,-2.22049474265475E-16));
#106783=DIRECTION('ref_axis',(0.641559662047602,1.7347234759768E-16,-0.767073138646744));
#106784=DIRECTION('center_axis',(6.93889390390725E-18,1.,2.22049474265475E-16));
#106785=DIRECTION('ref_axis',(0.641559662047602,1.65876472731702E-16,-0.767073138646744));
#106786=DIRECTION('center_axis',(6.93889390390725E-18,1.,2.22049474265475E-16));
#106787=DIRECTION('ref_axis',(0.,-2.22044604925031E-16,1.));
#106788=DIRECTION('center_axis',(-0.864862503651722,0.,0.502008814441813));
#106789=DIRECTION('ref_axis',(0.,1.,0.));
#106790=DIRECTION('center_axis',(-6.93889390390725E-18,-1.,-2.22049474265475E-16));
#106791=DIRECTION('ref_axis',(-0.363087995156522,2.08166817117217E-16,-0.93175485390376));
#106792=DIRECTION('center_axis',(6.93889390390725E-18,1.,2.22049474265475E-16));
#106793=DIRECTION('ref_axis',(-0.363087995156523,2.09415104529808E-16,-0.93175485390376));
#106794=DIRECTION('center_axis',(1.88217497143483E-12,0.,1.));
#106795=DIRECTION('ref_axis',(0.,1.,0.));
#106796=DIRECTION('center_axis',(-6.93889390390725E-18,-1.,-2.22049474265475E-16));
#106797=DIRECTION('ref_axis',(-0.866605104544004,8.67361737988402E-17,-0.498994581912747));
#106798=DIRECTION('center_axis',(6.93889390390725E-18,1.,2.22049474265475E-16));
#106799=DIRECTION('ref_axis',(-0.866605104544003,1.16814765452061E-16,-0.498994581912747));
#106800=DIRECTION('center_axis',(1.88236169427837E-12,-2.22049474265488E-16,
1.));
#106801=DIRECTION('ref_axis',(-0.707106781186548,0.707106781186548,1.3306533587345E-12));
#106802=DIRECTION('center_axis',(1.88182802673964E-12,0.,1.));
#106803=DIRECTION('ref_axis',(0.,1.,0.));
#106804=DIRECTION('',(-1.88236169427837E-12,2.22049474265488E-16,-1.));
#106805=DIRECTION('',(1.88236169427837E-12,-2.22049474265488E-16,1.));
#106806=DIRECTION('center_axis',(-6.93889390390725E-18,-1.,-2.22049474265475E-16));
#106807=DIRECTION('ref_axis',(-0.923879532510704,-8.67361737988403E-17,
0.382683432366495));
#106808=DIRECTION('center_axis',(6.93889390390725E-18,1.,2.22049474265475E-16));
#106809=DIRECTION('ref_axis',(-0.923879532510704,-7.85639529110045E-17,
0.382683432366495));
#106810=DIRECTION('center_axis',(0.,-1.,-2.22044604925031E-16));
#106811=DIRECTION('ref_axis',(-1.,0.,0.));
#106812=DIRECTION('',(0.,1.,2.22044604925031E-16));
#106813=DIRECTION('center_axis',(-5.19732413453357E-17,1.,2.87905372759356E-16));
#106814=DIRECTION('ref_axis',(-1.,0.,0.));
#106815=DIRECTION('',(0.,1.,2.22044604925031E-16));
#106816=DIRECTION('center_axis',(4.16333634234434E-17,-1.,-2.28983498828938E-16));
#106817=DIRECTION('ref_axis',(-1.,0.,0.));
#106818=DIRECTION('',(0.,-1.,-2.22044604925031E-16));
#106819=DIRECTION('',(0.,-1.,-2.22044604925031E-16));
#106820=DIRECTION('center_axis',(0.,-1.,-2.22044604925031E-16));
#106821=DIRECTION('ref_axis',(-1.,0.,0.));
#106822=DIRECTION('',(0.,-1.,-2.22044604925031E-16));
#106823=DIRECTION('center_axis',(1.04492064682899E-28,-1.,-2.22044604925092E-16));
#106824=DIRECTION('ref_axis',(-0.866605104544003,0.,-0.498994581912747));
#106825=DIRECTION('',(1.04492064682899E-28,-1.,-2.22044604925092E-16));
#106826=DIRECTION('center_axis',(0.,-1.,-2.22044604925031E-16));
#106827=DIRECTION('ref_axis',(-0.866605104544003,0.,-0.498994581912747));
#106828=DIRECTION('center_axis',(1.,5.22460323415068E-28,-1.88236169427837E-12));
#106829=DIRECTION('ref_axis',(1.88236169427837E-12,-2.12407076745007E-16,
1.));
#106830=DIRECTION('',(-2.62675723349586E-44,1.,2.77555756156289E-16));
#106831=DIRECTION('',(1.88236169427837E-12,-2.12407076745007E-16,1.));
#106832=DIRECTION('center_axis',(-6.34155293818297E-44,-1.,-2.77555756156289E-16));
#106833=DIRECTION('ref_axis',(-0.923879532510704,-3.75530232012225E-16,
0.382683432366498));
#106834=DIRECTION('',(-6.34155293818297E-44,-1.,-2.77555756156289E-16));
#106835=DIRECTION('center_axis',(0.,-1.,-2.22044604925031E-16));
#106836=DIRECTION('ref_axis',(-0.923879532510704,-3.75530232012225E-16,
0.382683432366498));
#106837=DIRECTION('center_axis',(0.707106781185727,1.962615573357E-16,-0.707106781187368));
#106838=DIRECTION('ref_axis',(0.707106781187368,-1.66829210022371E-16,0.707106781185727));
#106839=DIRECTION('',(-1.38777878078145E-16,1.,1.38777878078467E-16));
#106840=DIRECTION('',(0.707106781187368,-1.66829210022371E-16,0.707106781185727));
#106841=DIRECTION('center_axis',(-6.93889390390725E-18,-1.,-2.22049474265475E-16));
#106842=DIRECTION('ref_axis',(1.,-6.93889390390725E-18,-1.83750175990301E-19));
#106843=DIRECTION('center_axis',(-0.442887523223796,1.9908012597496E-16,
-0.896577181157702));
#106844=DIRECTION('ref_axis',(0.633975804653729,0.70710678118655,-0.31316877097446));
#106845=DIRECTION('center_axis',(0.442887523223797,0.,0.896577181157702));
#106846=DIRECTION('ref_axis',(0.896577181157702,-1.38777878078145E-15,-0.442887523223797));
#106847=DIRECTION('',(-0.442887523223796,1.9908012597496E-16,-0.896577181157702));
#106848=DIRECTION('center_axis',(-0.442887523223799,0.,-0.896577181157701));
#106849=DIRECTION('ref_axis',(0.,1.,0.));
#106850=DIRECTION('',(0.442887523223796,-1.9908012597496E-16,0.896577181157702));
#106851=DIRECTION('center_axis',(-0.990557901827268,0.,0.137095014962474));
#106852=DIRECTION('ref_axis',(0.,1.,0.));
#106853=DIRECTION('center_axis',(3.42121385298657E-49,-1.,-2.22044604925031E-16));
#106854=DIRECTION('ref_axis',(0.468176250029909,2.31296463463574E-16,-0.883635105067659));
#106855=DIRECTION('center_axis',(-3.42121385298657E-49,1.,2.22044604925031E-16));
#106856=DIRECTION('ref_axis',(0.468176250029909,1.96206407802637E-16,-0.883635105067659));
#106857=DIRECTION('center_axis',(3.42121385298657E-49,-1.,-2.22044604925031E-16));
#106858=DIRECTION('ref_axis',(-0.0834849737561929,-2.22044604925031E-16,
0.996509036164213));
#106859=DIRECTION('center_axis',(-0.953939201414718,0.,-0.300000000007082));
#106860=DIRECTION('ref_axis',(0.,1.,0.));
#106861=DIRECTION('center_axis',(-3.42121385298657E-49,1.,2.22044604925031E-16));
#106862=DIRECTION('ref_axis',(-0.0834849737561933,-2.16840434497101E-16,
0.996509036164212));
#106863=DIRECTION('center_axis',(3.42121385298657E-49,-1.,-2.22044604925031E-16));
#106864=DIRECTION('ref_axis',(-0.0834849737561933,-2.21269455239306E-16,
0.996509036164212));
#106865=DIRECTION('center_axis',(-7.42739203474237E-12,0.,1.));
#106866=DIRECTION('ref_axis',(0.,1.,0.));
#106867=DIRECTION('center_axis',(3.42121385298657E-49,-1.,-2.22044604925031E-16));
#106868=DIRECTION('ref_axis',(-0.591607978303975,1.7347234759768E-16,-0.806225774834248));
#106869=DIRECTION('center_axis',(-3.42121385298657E-49,1.,2.22044604925031E-16));
#106870=DIRECTION('ref_axis',(-0.591607978303975,1.79018083653448E-16,-0.806225774834248));
#106871=DIRECTION('center_axis',(-7.42407262755995E-12,-2.22044604925031E-16,
1.));
#106872=DIRECTION('ref_axis',(-0.707106781186548,0.707106781186548,-5.2441088120038E-12));
#106873=DIRECTION('center_axis',(-7.42184091961917E-12,0.,1.));
#106874=DIRECTION('ref_axis',(0.,1.,0.));
#106875=DIRECTION('',(7.42407262755995E-12,2.22044604925031E-16,-1.));
#106876=DIRECTION('',(-7.42407262755995E-12,-2.22044604925031E-16,1.));
#106877=DIRECTION('center_axis',(0.707106781186548,0.,0.707106781186548));
#106878=DIRECTION('ref_axis',(0.,1.,0.));
#106879=DIRECTION('center_axis',(3.42121385298657E-49,-1.,-2.22044604925031E-16));
#106880=DIRECTION('ref_axis',(-0.923879532512707,-8.67361737988402E-17,
0.38268343236166));
#106881=DIRECTION('center_axis',(-3.42121385298657E-49,1.,2.22044604925031E-16));
#106882=DIRECTION('ref_axis',(-0.923879532512707,-8.49727915500997E-17,
0.38268343236166));
#106883=DIRECTION('center_axis',(0.707106781186547,-1.57009245868378E-16,
0.707106781186548));
#106884=DIRECTION('ref_axis',(-0.500000000000001,0.707106781186546,0.500000000000001));
#106885=DIRECTION('center_axis',(0.707106781186545,0.,0.70710678118655));
#106886=DIRECTION('ref_axis',(0.,1.,0.));
#106887=DIRECTION('',(-0.707106781186547,1.57009245868378E-16,-0.707106781186548));
#106888=DIRECTION('',(0.707106781186547,-1.57009245868378E-16,0.707106781186548));
#106889=DIRECTION('center_axis',(3.42121385298657E-49,-1.,-2.22044604925031E-16));
#106890=DIRECTION('ref_axis',(0.,1.38777878078145E-16,-1.));
#106891=DIRECTION('center_axis',(1.88182802673965E-12,0.,1.));
#106892=DIRECTION('ref_axis',(0.,1.,0.));
#106893=DIRECTION('center_axis',(-3.42121385298657E-49,1.,2.22044604925031E-16));
#106894=DIRECTION('ref_axis',(0.923879532510927,8.67361737988404E-17,-0.382683432365959));
#106895=DIRECTION('center_axis',(3.42121385298657E-49,-1.,-2.22044604925031E-16));
#106896=DIRECTION('ref_axis',(0.923879532510927,8.49727915510542E-17,-0.382683432365959));
#106897=DIRECTION('center_axis',(-1.88236169427837E-12,2.22044604925031E-16,
-1.));
#106898=DIRECTION('ref_axis',(-0.707106781186548,0.707106781186548,1.3306533587345E-12));
#106899=DIRECTION('center_axis',(1.88113413734926E-12,0.,1.));
#106900=DIRECTION('ref_axis',(0.,1.,0.));
#106901=DIRECTION('',(-1.88236169427837E-12,2.22044604925031E-16,-1.));
#106902=DIRECTION('',(1.88236169427837E-12,-2.22044604925031E-16,1.));
#106903=DIRECTION('center_axis',(0.915812085606104,0.,-0.401607051553878));
#106904=DIRECTION('ref_axis',(0.,1.,0.));
#106905=DIRECTION('center_axis',(3.42121385298657E-49,-1.,-2.22044604925031E-16));
#106906=DIRECTION('ref_axis',(-0.546988550357502,-1.73472347597681E-16,
0.837140087307852));
#106907=DIRECTION('center_axis',(-3.42121385298657E-49,1.,2.22044604925031E-16));
#106908=DIRECTION('ref_axis',(-0.546988550357502,-1.85882439953178E-16,
0.837140087307852));
#106909=DIRECTION('center_axis',(3.42121385298657E-49,-1.,-2.22044604925031E-16));
#106910=DIRECTION('ref_axis',(0.,2.22044604925031E-16,-1.));
#106911=DIRECTION('center_axis',(0.943231903981036,0.,-0.332134875182221));
#106912=DIRECTION('ref_axis',(0.,1.,0.));
#106913=DIRECTION('center_axis',(-3.42121385298657E-49,1.,2.22044604925031E-16));
#106914=DIRECTION('ref_axis',(-0.367127042551388,2.05012774433623E-16,-0.930170809382595));
#106915=DIRECTION('center_axis',(3.42121385298657E-49,-1.,-2.22044604925031E-16));
#106916=DIRECTION('ref_axis',(-0.367127042551388,2.06539409882155E-16,-0.930170809382595));
#106917=DIRECTION('center_axis',(-0.143915261386658,0.,-0.989590014874852));
#106918=DIRECTION('ref_axis',(0.,1.,0.));
#106919=DIRECTION('center_axis',(3.42121385298657E-49,-1.,-2.22044604925031E-16));
#106920=DIRECTION('ref_axis',(0.855693526352071,-1.15648231731787E-16,0.517482935911086));
#106921=DIRECTION('center_axis',(-3.42121385298657E-49,1.,2.22044604925031E-16));
#106922=DIRECTION('ref_axis',(0.855693526352071,-1.14904294059822E-16,0.517482935911086));
#106923=DIRECTION('center_axis',(3.42121385298657E-49,-1.,-2.22044604925031E-16));
#106924=DIRECTION('ref_axis',(0.,2.24855296126614E-16,-1.));
#106925=DIRECTION('center_axis',(0.681400754633201,0.,-0.731910521570297));
#106926=DIRECTION('ref_axis',(0.,1.,0.));
#106927=DIRECTION('center_axis',(-3.42121385298657E-49,1.,2.22044604925031E-16));
#106928=DIRECTION('ref_axis',(-0.954556261212484,6.60847038467355E-17,-0.29803077723625));
#106929=DIRECTION('center_axis',(-3.42121385298657E-49,1.,2.22044604925031E-16));
#106930=DIRECTION('ref_axis',(-0.954556261212484,6.60847038467355E-17,-0.29803077723625));
#106931=DIRECTION('center_axis',(3.42121385298657E-49,-1.,-2.22044604925031E-16));
#106932=DIRECTION('ref_axis',(-0.954556261212484,6.61761261869232E-17,-0.29803077723625));
#106933=DIRECTION('center_axis',(3.42121385298657E-49,-1.,-2.22044604925031E-16));
#106934=DIRECTION('ref_axis',(0.989443824790343,0.,0.144916933393781));
#106935=DIRECTION('center_axis',(-3.42121385298657E-49,1.,2.22044604925031E-16));
#106936=DIRECTION('ref_axis',(0.989443824790343,-3.21780232223691E-17,0.144916933393781));
#106937=DIRECTION('center_axis',(1.,-5.1044736764327E-16,-1.88236169427837E-12));
#106938=DIRECTION('ref_axis',(1.88236169427837E-12,-2.12407076745007E-16,
1.));
#106939=DIRECTION('',(5.10447367643583E-16,1.,1.6657509746718E-16));
#106940=DIRECTION('',(-1.88236169427837E-12,2.22044604925031E-16,-1.));
#106941=DIRECTION('',(-5.1044736764375E-16,-1.,-2.55223683821875E-16));
#106942=DIRECTION('center_axis',(0.,1.,1.6657509746814E-16));
#106943=DIRECTION('ref_axis',(-0.546988550357499,0.,0.837140087307854));
#106944=DIRECTION('',(0.,-1.,-1.6657509746814E-16));
#106945=DIRECTION('center_axis',(4.16333634234434E-17,-1.,-2.28983498828938E-16));
#106946=DIRECTION('ref_axis',(-0.546988550357499,0.,0.837140087307854));
#106947=DIRECTION('center_axis',(0.,1.,1.6657509746814E-16));
#106948=DIRECTION('ref_axis',(-0.91120908155642,6.86196423904955E-17,-0.411944182734877));
#106949=DIRECTION('',(0.,1.,1.6657509746814E-16));
#106950=DIRECTION('center_axis',(-4.16333634234434E-17,1.,2.28983498828938E-16));
#106951=DIRECTION('ref_axis',(-0.91120908155642,6.86196423904955E-17,-0.411944182734877));
#106952=DIRECTION('center_axis',(0.,-1.,-1.6657509746814E-16));
#106953=DIRECTION('ref_axis',(0.855693526352075,0.,0.517482935911081));
#106954=DIRECTION('',(0.,-1.,-1.6657509746814E-16));
#106955=DIRECTION('center_axis',(4.16333634234434E-17,-1.,-2.28983498828938E-16));
#106956=DIRECTION('ref_axis',(0.855693526352075,0.,0.517482935911081));
#106957=DIRECTION('center_axis',(0.,1.,1.6657509746814E-16));
#106958=DIRECTION('ref_axis',(1.,0.,1.15584692836443E-33));
#106959=DIRECTION('center_axis',(0.,1.,2.22044604925031E-16));
#106960=DIRECTION('ref_axis',(1.,0.,1.15584692836443E-33));
#106961=DIRECTION('',(0.,1.,1.6657509746814E-16));
#106962=DIRECTION('',(0.,1.,1.6657509746814E-16));
#106963=DIRECTION('center_axis',(4.16333634234434E-17,-1.,-2.28983498828938E-16));
#106964=DIRECTION('ref_axis',(1.,4.16333634234434E-17,6.93889390390723E-17));
#106965=DIRECTION('',(0.,-1.,-2.67523620391604E-16));
#106966=DIRECTION('center_axis',(-3.42121385298657E-49,1.,2.22044604925031E-16));
#106967=DIRECTION('ref_axis',(0.122670494314896,2.20282346155785E-16,-0.992447454440052));
#106968=DIRECTION('',(0.,1.,2.67523620391604E-16));
#106969=DIRECTION('center_axis',(4.16333634234434E-17,-1.,-2.28983498828938E-16));
#106970=DIRECTION('ref_axis',(1.,4.16333634234434E-17,6.93889390390723E-17));
#106971=DIRECTION('',(0.,-1.,-1.6657509746814E-16));
#106972=DIRECTION('center_axis',(-3.32156684755978E-49,1.,2.15577286334982E-16));
#106973=DIRECTION('ref_axis',(1.,0.,3.03664566131718E-33));
#106974=DIRECTION('',(0.,1.,1.6657509746814E-16));
#106975=DIRECTION('center_axis',(4.16333634234434E-17,-1.,-2.28983498828938E-16));
#106976=DIRECTION('ref_axis',(1.,4.16333634234434E-17,6.93889390390723E-17));
#106977=DIRECTION('center_axis',(0.,-1.,-1.6657509746814E-16));
#106978=DIRECTION('ref_axis',(0.989443824790343,0.,0.144916933393781));
#106979=DIRECTION('',(0.,-1.,-1.6657509746814E-16));
#106980=DIRECTION('center_axis',(4.16333634234434E-17,-1.,-2.28983498828938E-16));
#106981=DIRECTION('ref_axis',(0.989443824790343,0.,0.144916933393781));
#106982=DIRECTION('center_axis',(0.896577181157702,7.37740323484271E-17,
-0.442887523223796));
#106983=DIRECTION('ref_axis',(-0.442887523223796,2.02157641249503E-16,-0.896577181157702));
#106984=DIRECTION('',(0.,1.,1.6657509746814E-16));
#106985=DIRECTION('',(0.442887523223796,-1.86862482701593E-16,0.896577181157702));
#106986=DIRECTION('center_axis',(-3.42121385298657E-49,1.,2.22044604925031E-16));
#106987=DIRECTION('ref_axis',(-1.54077774334651E-33,-2.22044604925031E-16,
1.));
#106988=DIRECTION('center_axis',(3.42121385298657E-49,-1.,-2.22044604925031E-16));
#106989=DIRECTION('ref_axis',(0.,2.11471052009443E-16,-1.));
#106990=DIRECTION('center_axis',(-0.634351002555855,0.,0.77304515104642));
#106991=DIRECTION('ref_axis',(0.77304515104642,-1.38777878078145E-15,0.634351002555855));
#106992=DIRECTION('center_axis',(3.42121385298657E-49,-1.,-2.22044604925031E-16));
#106993=DIRECTION('ref_axis',(-0.487986704420985,1.93811869204134E-16,-0.872851061927719));
#106994=DIRECTION('center_axis',(0.990774955112549,0.,-0.135517483454076));
#106995=DIRECTION('ref_axis',(0.,1.,0.));
#106996=DIRECTION('center_axis',(-3.42121385298657E-49,1.,2.22044604925031E-16));
#106997=DIRECTION('ref_axis',(-0.487986704420985,1.93144469193492E-16,-0.872851061927719));
#106998=DIRECTION('center_axis',(0.000408627366271784,0.,-0.999999916511834));
#106999=DIRECTION('ref_axis',(0.,1.,0.));
#107000=DIRECTION('center_axis',(3.42121385298657E-49,-1.,-2.22044604925031E-16));
#107001=DIRECTION('ref_axis',(0.753363330133439,-1.15648231731787E-16,0.657604510941231));
#107002=DIRECTION('center_axis',(-3.42121385298657E-49,1.,2.22044604925031E-16));
#107003=DIRECTION('ref_axis',(0.753363330133439,-1.46017533828864E-16,0.657604510941231));
#107004=DIRECTION('center_axis',(0.000408627366273739,2.22044586386935E-16,
-0.999999916511834));
#107005=DIRECTION('ref_axis',(0.707106722151499,0.707106781186548,0.000288943181669179));
#107006=DIRECTION('center_axis',(0.000408627366277338,0.,-0.999999916511834));
#107007=DIRECTION('ref_axis',(0.,1.,0.));
#107008=DIRECTION('',(-0.000408627366273739,-2.22044586386934E-16,0.999999916511834));
#107009=DIRECTION('',(0.000408627366273739,2.22044586386934E-16,-0.999999916511834));
#107010=DIRECTION('center_axis',(-1.,0.,-1.30451205393456E-12));
#107011=DIRECTION('ref_axis',(0.,1.,0.));
#107012=DIRECTION('center_axis',(3.42121385298657E-49,-1.,-2.22044604925031E-16));
#107013=DIRECTION('ref_axis',(0.707251238022098,1.15648231731787E-16,-0.706962294833473));
#107014=DIRECTION('center_axis',(-3.42121385298657E-49,1.,2.22044604925031E-16));
#107015=DIRECTION('ref_axis',(0.707251238022098,1.56977163453192E-16,-0.706962294833473));
#107016=DIRECTION('center_axis',(-1.,2.89708077091569E-28,-1.30472918803582E-12));
#107017=DIRECTION('ref_axis',(9.22429319476718E-13,0.707106781186547,-0.707106781186548));
#107018=DIRECTION('center_axis',(-1.,0.,-1.30451205393456E-12));
#107019=DIRECTION('ref_axis',(0.,1.,0.));
#107020=DIRECTION('',(1.,-2.89708077091569E-28,1.30472918803582E-12));
#107021=DIRECTION('',(-1.,2.89708077091569E-28,-1.30472918803582E-12));
#107022=DIRECTION('center_axis',(0.368421052642242,0.,0.9296590385566));
#107023=DIRECTION('ref_axis',(0.,1.,0.));
#107024=DIRECTION('center_axis',(3.42121385298657E-49,-1.,-2.22044604925031E-16));
#107025=DIRECTION('ref_axis',(-0.827170191871368,1.15648231731787E-16,-0.561951486944811));
#107026=DIRECTION('center_axis',(-3.42121385298657E-49,1.,2.22044604925031E-16));
#107027=DIRECTION('ref_axis',(-0.827170191871368,1.24778295905694E-16,-0.561951486944811));
#107028=DIRECTION('center_axis',(3.42121385298657E-49,-1.,-2.22044604925031E-16));
#107029=DIRECTION('ref_axis',(0.,2.22044604925031E-16,-1.));
#107030=DIRECTION('center_axis',(-0.710839466106974,0.,0.703354287272603));
#107031=DIRECTION('ref_axis',(0.,1.,0.));
#107032=DIRECTION('center_axis',(-3.42121385298657E-49,1.,2.22044604925031E-16));
#107033=DIRECTION('ref_axis',(0.978715457840861,-4.33680868994202E-17,0.205221959310776));
#107034=DIRECTION('center_axis',(3.42121385298657E-49,-1.,-2.22044604925031E-16));
#107035=DIRECTION('ref_axis',(0.978715457840861,-4.5568428877102E-17,0.205221959310776));
#107036=DIRECTION('center_axis',(0.442887523223795,0.,0.896577181157703));
#107037=DIRECTION('ref_axis',(0.,1.,0.));
#107038=DIRECTION('center_axis',(3.42121385298657E-49,-1.,-2.22044604925031E-16));
#107039=DIRECTION('ref_axis',(-0.986263994778248,0.,-0.165176670883183));
#107040=DIRECTION('center_axis',(-3.42121385298657E-49,1.,2.22044604925031E-16));
#107041=DIRECTION('ref_axis',(-0.986263994778248,3.66765886290883E-17,-0.165176670883183));
#107042=DIRECTION('center_axis',(0.442887523223796,-1.9908012597496E-16,
0.896577181157703));
#107043=DIRECTION('ref_axis',(-0.633975804653731,0.707106781186549,0.313168770974457));
#107044=DIRECTION('center_axis',(0.442887523223795,0.,0.896577181157703));
#107045=DIRECTION('ref_axis',(0.,1.,0.));
#107046=DIRECTION('',(-0.442887523223796,1.9908012597496E-16,-0.896577181157703));
#107047=DIRECTION('',(0.442887523223796,-1.9908012597496E-16,0.896577181157703));
#107048=DIRECTION('center_axis',(0.991156957142872,0.,-0.132694710924297));
#107049=DIRECTION('ref_axis',(0.,1.,0.));
#107050=DIRECTION('center_axis',(3.42121385298657E-49,-1.,-2.22044604925031E-16));
#107051=DIRECTION('ref_axis',(-0.47013716097003,-2.31296463463574E-16,0.882593366095078));
#107052=DIRECTION('center_axis',(-3.42121385298657E-49,1.,2.22044604925031E-16));
#107053=DIRECTION('ref_axis',(-0.47013716097003,-1.95975095284035E-16,0.882593366095078));
#107054=DIRECTION('center_axis',(3.42121385298657E-49,-1.,-2.22044604925031E-16));
#107055=DIRECTION('ref_axis',(0.,2.24855296126614E-16,-1.));
#107056=DIRECTION('center_axis',(0.929017422864237,0.,0.370035982054031));
#107057=DIRECTION('ref_axis',(0.,1.,0.));
#107058=DIRECTION('center_axis',(3.42121385298657E-49,-1.,-2.22044604925031E-16));
#107059=DIRECTION('ref_axis',(0.122670494314896,2.20367602929994E-16,-0.992447454440052));
#107060=DIRECTION('center_axis',(3.42121385298657E-49,-1.,-2.22044604925031E-16));
#107061=DIRECTION('ref_axis',(0.249622059095992,-2.31296463463574E-16,0.968343341802213));
#107062=DIRECTION('center_axis',(-3.42121385298657E-49,1.,2.22044604925031E-16));
#107063=DIRECTION('ref_axis',(0.249622059095992,-2.15015414762257E-16,0.968343341802213));
#107064=DIRECTION('center_axis',(0.,1.,1.6657509746814E-16));
#107065=DIRECTION('ref_axis',(-0.986263994778249,0.,-0.165176670883179));
#107066=DIRECTION('',(4.0084926897219E-17,-1.,-1.86376085453573E-16));
#107067=DIRECTION('center_axis',(4.16333634234434E-17,-1.,-2.28983498828938E-16));
#107068=DIRECTION('ref_axis',(-0.986263994778249,0.,-0.165176670883179));
#107069=DIRECTION('',(0.,-1.,0.));
#107070=DIRECTION('center_axis',(0.,-1.,-2.22044604925031E-16));
#107071=DIRECTION('ref_axis',(-0.986263994778249,0.,-0.165176670883179));
#107072=DIRECTION('',(0.,1.,1.6657509746814E-16));
#107073=DIRECTION('center_axis',(-0.896577181157703,-1.184828736391E-16,
0.442887523223796));
#107074=DIRECTION('ref_axis',(0.442887523223796,-2.02157641249503E-16,0.896577181157703));
#107075=DIRECTION('',(0.,1.,2.67523620391604E-16));
#107076=DIRECTION('',(-0.442887523223796,1.86862482701593E-16,-0.896577181157703));
#107077=DIRECTION('center_axis',(0.,-1.,-2.67523620391604E-16));
#107078=DIRECTION('ref_axis',(-0.47013716097003,0.,0.882593366095077));
#107079=DIRECTION('center_axis',(4.16333634234434E-17,-1.,-2.28983498828938E-16));
#107080=DIRECTION('ref_axis',(-0.47013716097003,0.,0.882593366095077));
#107081=DIRECTION('center_axis',(0.,-1.,-2.67523620391604E-16));
#107082=DIRECTION('ref_axis',(0.24962205909599,0.,0.968343341802213));
#107083=DIRECTION('',(0.,-1.,-2.67523620391604E-16));
#107084=DIRECTION('center_axis',(1.35739377892777E-16,-1.,-3.84762012452445E-17));
#107085=DIRECTION('ref_axis',(0.24962205909599,0.,0.968343341802213));
#107086=DIRECTION('center_axis',(0.,1.,2.67523620391604E-16));
#107087=DIRECTION('ref_axis',(-0.984274724761795,4.72565661779708E-17,-0.176644462678832));
#107088=DIRECTION('',(0.,1.,2.67523620391604E-16));
#107089=DIRECTION('center_axis',(-1.35739377892777E-16,1.,3.84762012452445E-17));
#107090=DIRECTION('ref_axis',(-0.984274724761795,4.72565661779708E-17,-0.176644462678832));
#107091=DIRECTION('center_axis',(-3.42121385298657E-49,1.,2.22044604925031E-16));
#107092=DIRECTION('ref_axis',(-1.54077774334651E-33,-2.22044604925031E-16,
1.));
#107093=DIRECTION('center_axis',(-0.000408627366273673,-2.22046620305031E-16,
0.999999916511834));
#107094=DIRECTION('ref_axis',(-0.707106722151501,0.707106781186546,-0.000288943181673103));
#107095=DIRECTION('center_axis',(0.000408627366271784,0.,-0.999999916511834));
#107096=DIRECTION('ref_axis',(-0.999999916511834,-2.77555756156288E-15,
-0.000408627366271784));
#107097=DIRECTION('',(-0.000408627366273673,-2.22046620305031E-16,0.999999916511834));
#107098=DIRECTION('center_axis',(-0.000408627366277335,0.,0.999999916511834));
#107099=DIRECTION('ref_axis',(0.,1.,0.));
#107100=DIRECTION('',(0.000408627366273673,2.22046620305031E-16,-0.999999916511834));
#107101=DIRECTION('center_axis',(0.990663871945179,0.,0.136327153651006));
#107102=DIRECTION('ref_axis',(0.,1.,0.));
#107103=DIRECTION('center_axis',(-6.93889390390723E-18,-1.,-2.22049474265475E-16));
#107104=DIRECTION('ref_axis',(-0.753900508899602,-1.15648231731787E-16,
0.656988601636985));
#107105=DIRECTION('center_axis',(6.93889390390723E-18,1.,2.22049474265475E-16));
#107106=DIRECTION('ref_axis',(-0.753900508899602,-1.40652737946546E-16,
0.656988601636985));
#107107=DIRECTION('center_axis',(-6.93889390390723E-18,-1.,-2.22049474265475E-16));
#107108=DIRECTION('ref_axis',(0.,2.11471052009443E-16,-1.));
#107109=DIRECTION('center_axis',(0.829730454564779,0.,0.558164288330708));
#107110=DIRECTION('ref_axis',(0.,1.,0.));
#107111=DIRECTION('center_axis',(6.93889390390723E-18,1.,2.22049474265475E-16));
#107112=DIRECTION('ref_axis',(0.356447025452442,2.07451466911529E-16,-0.934315534520382));
#107113=DIRECTION('center_axis',(-6.93889390390723E-18,-1.,-2.22049474265475E-16));
#107114=DIRECTION('ref_axis',(0.356447025452442,2.04990925146339E-16,-0.934315534520382));
#107115=DIRECTION('center_axis',(0.748617784953237,0.,-0.663001819041026));
#107116=DIRECTION('ref_axis',(0.,1.,0.));
#107117=DIRECTION('center_axis',(-6.93889390390723E-18,-1.,-2.22049474265475E-16));
#107118=DIRECTION('ref_axis',(0.0662762646370237,-2.31296463463574E-16,
0.997801311256787));
#107119=DIRECTION('center_axis',(6.93889390390723E-18,1.,2.22049474265475E-16));
#107120=DIRECTION('ref_axis',(0.0662762646370237,-2.22021140554634E-16,
0.997801311256787));
#107121=DIRECTION('center_axis',(-6.93889390390723E-18,-1.,-2.22049474265475E-16));
#107122=DIRECTION('ref_axis',(0.,1.97372982155583E-16,-1.));
#107123=DIRECTION('center_axis',(0.939530312300397,0.,-0.342465753424659));
#107124=DIRECTION('ref_axis',(0.,1.,0.));
#107125=DIRECTION('center_axis',(6.93889390390723E-18,1.,2.22049474265475E-16));
#107126=DIRECTION('ref_axis',(-0.511715895878297,1.87537673078574E-16,-0.859154725241892));
#107127=DIRECTION('center_axis',(-6.93889390390723E-18,-1.,-2.22049474265475E-16));
#107128=DIRECTION('ref_axis',(-0.511715895878297,1.94325597363103E-16,-0.859154725241892));
#107129=DIRECTION('center_axis',(6.93889390390723E-18,1.,2.22049474265475E-16));
#107130=DIRECTION('ref_axis',(0.,-1.85037170770859E-16,1.));
#107131=DIRECTION('center_axis',(0.,0.,-1.));
#107132=DIRECTION('ref_axis',(0.,1.,0.));
#107133=DIRECTION('center_axis',(-6.93889390390723E-18,-1.,-2.22049474265475E-16));
#107134=DIRECTION('ref_axis',(0.819288030372914,-1.34922937020418E-16,0.573382179080996));
#107135=DIRECTION('center_axis',(6.93889390390723E-18,1.,2.22049474265475E-16));
#107136=DIRECTION('ref_axis',(0.819288030372914,-1.33004164137626E-16,0.573382179080996));
#107137=DIRECTION('center_axis',(7.61924092396395E-16,2.22049474265475E-16,
-1.));
#107138=DIRECTION('ref_axis',(0.707106781186548,0.707106781186547,0.));
#107139=DIRECTION('center_axis',(0.,0.,-1.));
#107140=DIRECTION('ref_axis',(0.,1.,0.));
#107141=DIRECTION('',(-7.61924092396395E-16,-2.22049474265475E-16,1.));
#107142=DIRECTION('',(7.61924092396395E-16,2.22049474265475E-16,-1.));
#107143=DIRECTION('center_axis',(-6.93889390390723E-18,-1.,-2.22049474265475E-16));
#107144=DIRECTION('ref_axis',(0.,2.14881875733901E-16,-1.));
#107145=DIRECTION('center_axis',(0.300000000002116,0.,-0.95393920141628));
#107146=DIRECTION('ref_axis',(0.,1.,0.));
#107147=DIRECTION('center_axis',(6.93889390390723E-18,1.,2.22049474265475E-16));
#107148=DIRECTION('ref_axis',(-0.988417725816438,5.13992141030164E-17,-0.151757699283627));
#107149=DIRECTION('center_axis',(-6.93889390390723E-18,-1.,-2.22049474265475E-16));
#107150=DIRECTION('ref_axis',(-0.988417725816438,4.0556243073849E-17,-0.151757699283627));
#107151=DIRECTION('center_axis',(-1.,0.,-1.30451205393454E-12));
#107152=DIRECTION('ref_axis',(0.,1.,0.));
#107153=DIRECTION('center_axis',(-6.93889390390723E-18,-1.,-2.22049474265475E-16));
#107154=DIRECTION('ref_axis',(0.806225774830896,1.15648231731787E-16,-0.591607978308543));
#107155=DIRECTION('center_axis',(6.93889390390723E-18,1.,2.22049474265475E-16));
#107156=DIRECTION('ref_axis',(0.806225774830896,1.25771925440525E-16,-0.591607978308543));
#107157=DIRECTION('center_axis',(-1.,6.93889390419694E-18,-1.30472918803582E-12));
#107158=DIRECTION('ref_axis',(9.22429319476717E-13,0.707106781186547,-0.707106781186548));
#107159=DIRECTION('center_axis',(-1.,0.,-1.30451205393456E-12));
#107160=DIRECTION('ref_axis',(0.,1.,0.));
#107161=DIRECTION('',(1.,-6.93889390419694E-18,1.30472918803582E-12));
#107162=DIRECTION('',(-1.,6.93889390419694E-18,-1.30472918803582E-12));
#107163=DIRECTION('center_axis',(-6.93889390390723E-18,-1.,-2.22049474265475E-16));
#107164=DIRECTION('ref_axis',(-0.706962294833474,1.15648231731787E-16,-0.707251238022097));
#107165=DIRECTION('center_axis',(6.93889390390723E-18,1.,2.22049474265475E-16));
#107166=DIRECTION('ref_axis',(-0.706962294833474,1.61950301934325E-16,-0.707251238022097));
#107167=DIRECTION('center_axis',(1.,-2.03832691661471E-31,7.61924092396395E-16));
#107168=DIRECTION('ref_axis',(7.61924092396395E-16,2.22049474265475E-16,
-1.));
#107169=DIRECTION('',(0.,1.,2.67523620391604E-16));
#107170=DIRECTION('',(7.61924092396395E-16,2.22044604925031E-16,-1.));
#107171=DIRECTION('',(-9.82764763367805E-32,1.,3.96508223080413E-16));
#107172=DIRECTION('',(7.61924092396395E-16,2.22044604925031E-16,-1.));
#107173=DIRECTION('',(0.,1.,2.67523620391604E-16));
#107174=DIRECTION('center_axis',(0.,1.,2.67523620391604E-16));
#107175=DIRECTION('ref_axis',(-1.,4.09094084738805E-31,-1.53134210293125E-15));
#107176=DIRECTION('',(0.,1.,2.67523620391604E-16));
#107177=DIRECTION('center_axis',(0.,-1.,-2.22044604925031E-16));
#107178=DIRECTION('ref_axis',(-1.,4.09094084738805E-31,-1.53134210293125E-15));
#107179=DIRECTION('center_axis',(0.,-1.,-2.67523620391604E-16));
#107180=DIRECTION('ref_axis',(0.806225774830893,0.,-0.591607978308547));
#107181=DIRECTION('',(0.,-1.,-2.67523620391604E-16));
#107182=DIRECTION('center_axis',(0.,-1.,-2.22044604925031E-16));
#107183=DIRECTION('ref_axis',(0.806225774830893,0.,-0.591607978308547));
#107184=DIRECTION('center_axis',(1.30472918803582E-12,2.67523620391604E-16,
-1.));
#107185=DIRECTION('ref_axis',(-1.,6.93889390419694E-18,-1.30472918803582E-12));
#107186=DIRECTION('',(0.,1.,2.67523620391604E-16));
#107187=DIRECTION('',(-1.,2.89708077091569E-28,-1.30472918803582E-12));
#107188=DIRECTION('center_axis',(0.,-1.,-2.67523620391604E-16));
#107189=DIRECTION('ref_axis',(-0.706962294833475,0.,-0.707251238022096));
#107190=DIRECTION('',(0.,-1.,-2.67523620391604E-16));
#107191=DIRECTION('center_axis',(0.,-1.,-2.22044604925031E-16));
#107192=DIRECTION('ref_axis',(-0.706962294833475,0.,-0.707251238022096));
#107193=DIRECTION('center_axis',(-0.999999916511834,1.09317472416619E-19,
-0.000408627366273673));
#107194=DIRECTION('ref_axis',(-0.000408627366273673,-2.22046620305031E-16,
0.999999916511834));
#107195=DIRECTION('',(0.,1.,2.67523620391604E-16));
#107196=DIRECTION('',(-0.000408627366274271,-2.29000492243171E-16,0.999999916511834));
#107197=DIRECTION('',(1.85839687592837E-20,1.,2.2204461251895E-16));
#107198=DIRECTION('',(-0.000408627366273673,-2.22044586386934E-16,0.999999916511834));
#107199=DIRECTION('center_axis',(-6.93889390390723E-18,-1.,-2.22049474265475E-16));
#107200=DIRECTION('ref_axis',(1.,-6.93889390390723E-18,1.54077774334651E-33));
#107201=DIRECTION('center_axis',(-6.93889390390723E-18,-1.,-2.22049474265475E-16));
#107202=DIRECTION('ref_axis',(0.,1.98254111540207E-16,-1.));
#107203=DIRECTION('center_axis',(-5.55111512312578E-15,0.,-1.));
#107204=DIRECTION('ref_axis',(-1.,0.,5.55111512312578E-15));
#107205=DIRECTION('center_axis',(-6.93889390390723E-18,-1.,-2.22049474265475E-16));
#107206=DIRECTION('ref_axis',(0.948334612654778,-7.70304532255269E-17,0.31727190616396));
#107207=DIRECTION('center_axis',(-0.60175986047648,0.,0.798677075118177));
#107208=DIRECTION('ref_axis',(0.,1.,0.));
#107209=DIRECTION('center_axis',(6.93889390390723E-18,1.,2.22049474265475E-16));
#107210=DIRECTION('ref_axis',(0.948334612654778,-7.2280144832367E-17,0.31727190616396));
#107211=DIRECTION('center_axis',(0.981039208710857,0.,0.193809367606358));
#107212=DIRECTION('ref_axis',(0.,1.,0.));
#107213=DIRECTION('center_axis',(-6.93889390390723E-18,-1.,-2.22049474265475E-16));
#107214=DIRECTION('ref_axis',(-0.934114852736577,-1.15648231731787E-16,
0.356972606647796));
#107215=DIRECTION('center_axis',(6.93889390390723E-18,1.,2.22049474265475E-16));
#107216=DIRECTION('ref_axis',(-0.934114852736577,-7.27838557761162E-17,
0.356972606647796));
#107217=DIRECTION('center_axis',(-6.93889390390723E-18,-1.,-2.22049474265475E-16));
#107218=DIRECTION('ref_axis',(0.,2.14881875733901E-16,-1.));
#107219=DIRECTION('center_axis',(0.899591968564469,0.,0.436731370632227));
#107220=DIRECTION('ref_axis',(0.,1.,0.));
#107221=DIRECTION('center_axis',(6.93889390390723E-18,1.,2.22049474265475E-16));
#107222=DIRECTION('ref_axis',(0.317889633169248,2.05596856412066E-16,-0.948127724055953));
#107223=DIRECTION('center_axis',(-6.93889390390723E-18,-1.,-2.22049474265475E-16));
#107224=DIRECTION('ref_axis',(0.317889633169248,2.08325460225432E-16,-0.948127724055953));
#107225=DIRECTION('center_axis',(6.93889390390723E-18,1.,2.22049474265475E-16));
#107226=DIRECTION('ref_axis',(0.,-2.22184532873183E-16,1.));
#107227=DIRECTION('center_axis',(0.990294325605679,0.,0.138986145616005));
#107228=DIRECTION('ref_axis',(0.,1.,0.));
#107229=DIRECTION('center_axis',(-6.93889390390723E-18,-1.,-2.22049474265475E-16));
#107230=DIRECTION('ref_axis',(-0.291409323841853,-2.08297999568609E-16,
0.956598455977237));
#107231=DIRECTION('center_axis',(6.93889390390723E-18,1.,2.22049474265475E-16));
#107232=DIRECTION('ref_axis',(-0.291409323841853,-2.10390125852163E-16,
0.956598455977237));
#107233=DIRECTION('center_axis',(-1.88182802673964E-12,0.,-1.));
#107234=DIRECTION('ref_axis',(0.,1.,0.));
#107235=DIRECTION('center_axis',(-6.93889390390723E-18,-1.,-2.22049474265475E-16));
#107236=DIRECTION('ref_axis',(0.656130266938607,-1.73472347597681E-16,0.754647648116041));
#107237=DIRECTION('center_axis',(6.93889390390723E-18,1.,2.22049474265475E-16));
#107238=DIRECTION('ref_axis',(0.656130266938607,-1.72121931829273E-16,0.754647648116041));
#107239=DIRECTION('center_axis',(-1.88215207428297E-12,2.22049474265488E-16,
-1.));
#107240=DIRECTION('ref_axis',(0.707106781186548,0.707106781186547,-1.3306533587345E-12));
#107241=DIRECTION('center_axis',(-1.88182802673964E-12,0.,-1.));
#107242=DIRECTION('ref_axis',(0.,1.,0.));
#107243=DIRECTION('',(1.88215207428297E-12,-2.22049474265488E-16,1.));
#107244=DIRECTION('',(-1.88215207428297E-12,2.22049474265488E-16,-1.));
#107245=DIRECTION('center_axis',(-6.93889390390723E-18,-1.,-2.22049474265475E-16));
#107246=DIRECTION('ref_axis',(0.,1.38777878078145E-16,-1.));
#107247=DIRECTION('center_axis',(0.707106781186549,0.,-0.707106781186546));
#107248=DIRECTION('ref_axis',(0.,1.,0.));
#107249=DIRECTION('center_axis',(6.93889390390723E-18,1.,2.22049474265475E-16));
#107250=DIRECTION('ref_axis',(-0.923879532511646,8.67361737988404E-17,-0.382683432364222));
#107251=DIRECTION('center_axis',(-6.93889390390723E-18,-1.,-2.22049474265475E-16));
#107252=DIRECTION('ref_axis',(-0.923879532511646,9.13853570226725E-17,-0.382683432364222));
#107253=DIRECTION('center_axis',(0.707106781186548,1.52106150078638E-16,
-0.707106781186547));
#107254=DIRECTION('ref_axis',(0.500000000000002,0.707106781186548,0.499999999999998));
#107255=DIRECTION('center_axis',(0.707106781186548,0.,-0.707106781186548));
#107256=DIRECTION('ref_axis',(0.,1.,0.));
#107257=DIRECTION('',(-0.707106781186548,-1.52106150078638E-16,0.707106781186547));
#107258=DIRECTION('',(0.707106781186548,1.52106150078638E-16,-0.707106781186547));
#107259=DIRECTION('center_axis',(0.,0.,-1.));
#107260=DIRECTION('ref_axis',(0.,1.,0.));
#107261=DIRECTION('center_axis',(-6.93889390390723E-18,-1.,-2.22049474265475E-16));
#107262=DIRECTION('ref_axis',(0.923879532511287,-8.67361737988403E-17,0.382683432365091));
#107263=DIRECTION('center_axis',(6.93889390390723E-18,1.,2.22049474265475E-16));
#107264=DIRECTION('ref_axis',(0.923879532511287,-9.1385357022863E-17,0.382683432365091));
#107265=DIRECTION('center_axis',(-8.32407533012986E-17,2.22049474265475E-16,
-1.));
#107266=DIRECTION('ref_axis',(0.707106781186551,0.707106781186544,0.));
#107267=DIRECTION('center_axis',(0.,0.,-1.));
#107268=DIRECTION('ref_axis',(0.,1.,0.));
#107269=DIRECTION('',(8.32407533012986E-17,-2.22049474265475E-16,1.));
#107270=DIRECTION('',(-8.32407533012986E-17,2.22049474265475E-16,-1.));
#107271=DIRECTION('center_axis',(-0.873688101364575,0.,0.486486486486485));
#107272=DIRECTION('ref_axis',(0.,1.,0.));
#107273=DIRECTION('center_axis',(-6.93889390390723E-18,-1.,-2.22049474265475E-16));
#107274=DIRECTION('ref_axis',(0.506711709709532,2.31296463463574E-16,-0.862115562580356));
#107275=DIRECTION('center_axis',(6.93889390390723E-18,1.,2.22049474265475E-16));
#107276=DIRECTION('ref_axis',(0.506711709709532,1.8791628863351E-16,-0.862115562580356));
#107277=DIRECTION('center_axis',(-6.93889390390723E-18,-1.,-2.22049474265475E-16));
#107278=DIRECTION('ref_axis',(-0.271927396983848,-1.70803542250024E-16,
0.962317770162013));
#107279=DIRECTION('center_axis',(-0.489871107039562,0.,-0.87179487179487));
#107280=DIRECTION('ref_axis',(0.,1.,0.));
#107281=DIRECTION('center_axis',(6.93889390390723E-18,1.,2.22049474265475E-16));
#107282=DIRECTION('ref_axis',(-0.271927396983848,-2.23835287222814E-16,
0.962317770162013));
#107283=DIRECTION('center_axis',(-6.93889390390723E-18,-1.,-2.22049474265475E-16));
#107284=DIRECTION('ref_axis',(-0.271927396983848,-2.11795279583562E-16,
0.962317770162013));
#107285=DIRECTION('center_axis',(0.,0.,1.));
#107286=DIRECTION('ref_axis',(0.,1.,0.));
#107287=DIRECTION('center_axis',(-6.93889390390723E-18,-1.,-2.22049474265475E-16));
#107288=DIRECTION('ref_axis',(-0.253184841770917,1.73472347597681E-16,-0.967417922046845));
#107289=DIRECTION('center_axis',(6.93889390390723E-18,1.,2.22049474265475E-16));
#107290=DIRECTION('ref_axis',(-0.253184841770917,2.16571463740626E-16,-0.967417922046845));
#107291=DIRECTION('center_axis',(0.,-2.22049474265475E-16,1.));
#107292=DIRECTION('ref_axis',(-0.707106781186548,0.707106781186547,0.));
#107293=DIRECTION('',(0.,2.22049474265475E-16,-1.));
#107294=DIRECTION('',(0.,-2.22049474265475E-16,1.));
#107295=DIRECTION('center_axis',(-1.13917782314015E-33,1.,1.88173394004264E-16));
#107296=DIRECTION('ref_axis',(0.923879532511287,0.,0.382683432365089));
#107297=DIRECTION('',(1.13917782314015E-33,-1.,-1.88173394004264E-16));
#107298=DIRECTION('center_axis',(0.,-1.,-2.22044604925031E-16));
#107299=DIRECTION('ref_axis',(0.923879532511287,0.,0.382683432365089));
#107300=DIRECTION('',(1.62923501610703E-32,1.,1.88173394004264E-16));
#107301=DIRECTION('center_axis',(1.,1.68028728913171E-32,-8.32407533012986E-17));
#107302=DIRECTION('ref_axis',(-8.32407533012986E-17,1.80520972702821E-16,
-1.));
#107303=DIRECTION('',(0.,1.,2.01858731750028E-16));
#107304=DIRECTION('',(-8.32407533012986E-17,2.22044604925031E-16,-1.));
#107305=DIRECTION('center_axis',(0.,-1.,-2.01858731750028E-16));
#107306=DIRECTION('ref_axis',(0.506711709709536,0.,-0.862115562580353));
#107307=DIRECTION('',(0.,-1.,-2.01858731750028E-16));
#107308=DIRECTION('center_axis',(0.,-1.,-2.22044604925031E-16));
#107309=DIRECTION('ref_axis',(0.506711709709536,0.,-0.862115562580353));
#107310=DIRECTION('center_axis',(0.,1.,2.01858731750028E-16));
#107311=DIRECTION('ref_axis',(1.,0.,-1.83750175990301E-19));
#107312=DIRECTION('',(0.,1.,0.));
#107313=DIRECTION('center_axis',(0.,-1.,-2.22044604925031E-16));
#107314=DIRECTION('ref_axis',(1.,0.,-1.83750175990301E-19));
#107315=DIRECTION('center_axis',(0.,-1.,0.));
#107316=DIRECTION('ref_axis',(1.,0.,0.));
#107317=DIRECTION('',(0.,-1.,0.));
#107318=DIRECTION('center_axis',(0.,-1.,-2.22044604925031E-16));
#107319=DIRECTION('ref_axis',(1.,0.,0.));
#107320=DIRECTION('center_axis',(-1.,0.,0.));
#107321=DIRECTION('ref_axis',(0.,-2.22044604925031E-16,1.));
#107322=DIRECTION('',(0.,1.,2.22044604925031E-16));
#107323=DIRECTION('',(0.,2.22049474265475E-16,-1.));
#107324=DIRECTION('center_axis',(0.,-1.,-2.22044604925031E-16));
#107325=DIRECTION('ref_axis',(0.707106781186548,-1.57009245868377E-16,0.707106781186548));
#107326=DIRECTION('',(0.,1.,2.22044604925031E-16));
#107327=DIRECTION('center_axis',(6.93889390390725E-18,1.,2.22049474265475E-16));
#107328=DIRECTION('ref_axis',(0.707106781186548,-1.57009245868377E-16,0.707106781186548));
#107329=DIRECTION('center_axis',(-6.93889390390723E-18,-1.,-2.22049474265475E-16));
#107330=DIRECTION('ref_axis',(1.,-6.93889390390723E-18,-1.83750175990301E-19));
#107331=DIRECTION('center_axis',(-6.93889390390721E-18,-1.,-2.22049474265475E-16));
#107332=DIRECTION('ref_axis',(0.,2.1779837001999E-16,-1.));
#107333=DIRECTION('center_axis',(0.995177777995763,0.,0.0980876658067449));
#107334=DIRECTION('ref_axis',(0.0980876658067449,-6.9388939039072E-16,-0.995177777995763));
#107335=DIRECTION('center_axis',(-6.93889390390721E-18,-1.,-2.22049474265475E-16));
#107336=DIRECTION('ref_axis',(-0.271646851952191,-2.11814819455226E-16,
0.962397001151014));
#107337=DIRECTION('center_axis',(-0.89959196856447,0.,-0.436731370632225));
#107338=DIRECTION('ref_axis',(0.,1.,0.));
#107339=DIRECTION('center_axis',(6.93889390390721E-18,1.,2.22049474265475E-16));
#107340=DIRECTION('ref_axis',(-0.271646851952191,-2.14187059826031E-16,
0.962397001151014));
#107341=DIRECTION('center_axis',(6.93889390390721E-18,1.,2.22049474265475E-16));
#107342=DIRECTION('ref_axis',(0.0641559653703721,2.22044604925031E-16,-0.997939884014762));
#107343=DIRECTION('center_axis',(-0.948108950182503,0.,0.317945622054827));
#107344=DIRECTION('ref_axis',(0.,1.,0.));
#107345=DIRECTION('center_axis',(-6.93889390390721E-18,-1.,-2.22049474265475E-16));
#107346=DIRECTION('ref_axis',(0.0641559653703722,2.25514051876985E-16,-0.997939884014762));
#107347=DIRECTION('center_axis',(6.93889390390721E-18,1.,2.22049474265475E-16));
#107348=DIRECTION('ref_axis',(0.0641559653703722,2.21146855157019E-16,-0.997939884014762));
#107349=DIRECTION('center_axis',(0.609084507830823,0.,0.793105328642094));
#107350=DIRECTION('ref_axis',(0.,1.,0.));
#107351=DIRECTION('center_axis',(-6.93889390390721E-18,-1.,-2.22049474265475E-16));
#107352=DIRECTION('ref_axis',(-0.956462973763756,1.15648231731787E-16,-0.291853695914566));
#107353=DIRECTION('center_axis',(6.93889390390721E-18,1.,2.22049474265475E-16));
#107354=DIRECTION('ref_axis',(-0.956462973763756,7.14427548382275E-17,-0.291853695914567));
#107355=DIRECTION('center_axis',(-6.93889390390721E-18,-1.,-2.22049474265475E-16));
#107356=DIRECTION('ref_axis',(0.,2.11471052309554E-16,-1.));
#107357=DIRECTION('center_axis',(-0.0951854606398691,0.,0.995459556226558));
#107358=DIRECTION('ref_axis',(0.,1.,0.));
#107359=DIRECTION('center_axis',(6.93889390390721E-18,1.,2.22049474265475E-16));
#107360=DIRECTION('ref_axis',(0.9611140067488,5.72279909600596E-17,-0.27615188942187));
#107361=DIRECTION('center_axis',(-6.93889390390721E-18,-1.,-2.22049474265475E-16));
#107362=DIRECTION('ref_axis',(0.961114006748799,5.46503137411547E-17,-0.27615188942187));
#107363=DIRECTION('center_axis',(0.957454413658976,-1.00122880701227E-16,
0.288584555659077));
#107364=DIRECTION('ref_axis',(0.,1.,3.46944695195361E-16));
#107365=DIRECTION('center_axis',(-6.93889390390721E-18,-1.,-2.22049474265475E-16));
#107366=DIRECTION('ref_axis',(-0.830183712534771,-1.15648231731787E-16,
0.557489913309635));
#107367=DIRECTION('center_axis',(6.93889390390721E-18,1.,2.22049474265475E-16));
#107368=DIRECTION('ref_axis',(-0.830183712534771,-1.18029785456679E-16,
0.557489913309635));
#107369=DIRECTION('center_axis',(6.93889390390721E-18,1.,2.22049474265475E-16));
#107370=DIRECTION('ref_axis',(0.,-2.17002965587602E-16,1.));
#107371=DIRECTION('center_axis',(0.998182760026068,0.,0.0602592531213423));
#107372=DIRECTION('ref_axis',(0.,1.,0.));
#107373=DIRECTION('center_axis',(-6.93889390390721E-18,-1.,-2.22049474265475E-16));
#107374=DIRECTION('ref_axis',(-0.17560666354258,-2.1939638064923E-16,0.984460410437841));
#107375=DIRECTION('center_axis',(6.93889390390721E-18,1.,2.22049474265475E-16));
#107376=DIRECTION('ref_axis',(-0.17560666354258,-2.17380400565755E-16,0.984460410437841));
#107377=DIRECTION('center_axis',(-1.88182802673964E-12,0.,-1.));
#107378=DIRECTION('ref_axis',(0.,1.,0.));
#107379=DIRECTION('center_axis',(-6.93889390390721E-18,-1.,-2.22049474265475E-16));
#107380=DIRECTION('ref_axis',(0.685470913635486,-1.73472347597681E-16,0.72810001137188));
#107381=DIRECTION('center_axis',(6.93889390390721E-18,1.,2.22049474265475E-16));
#107382=DIRECTION('ref_axis',(0.685470913635486,-1.66430634681743E-16,0.72810001137188));
#107383=DIRECTION('center_axis',(-1.88215207428297E-12,2.22049474265488E-16,
-1.));
#107384=DIRECTION('ref_axis',(0.707106781186544,0.707106781186551,-1.33071469047117E-12));
#107385=DIRECTION('center_axis',(-1.88182802673965E-12,1.38777878078145E-15,
-1.));
#107386=DIRECTION('ref_axis',(0.,1.,1.38777878078145E-15));
#107387=DIRECTION('',(1.88215207428297E-12,-2.22049474265488E-16,1.));
#107388=DIRECTION('',(-1.88215207428297E-12,2.22049474265488E-16,-1.));
#107389=DIRECTION('center_axis',(-6.93889390390721E-18,-1.,-2.22049474265475E-16));
#107390=DIRECTION('ref_axis',(0.740974920562387,1.73472347597681E-16,-0.671532699946595));
#107391=DIRECTION('center_axis',(6.93889390390721E-18,1.,2.22049474265475E-16));
#107392=DIRECTION('ref_axis',(0.740974920562387,1.43971936615978E-16,-0.671532699946595));
#107393=DIRECTION('center_axis',(0.,1.,2.01858731750028E-16));
#107394=DIRECTION('ref_axis',(0.229951641166733,-1.9644933285631E-16,0.973202056473745));
#107395=DIRECTION('',(0.,1.,2.01858731750028E-16));
#107396=DIRECTION('center_axis',(0.,-1.,-2.22044604925031E-16));
#107397=DIRECTION('ref_axis',(0.229951641166733,-1.9644933285631E-16,0.973202056473745));
#107398=DIRECTION('',(0.,-1.,-2.01858731750028E-16));
#107399=DIRECTION('center_axis',(3.79928830675489E-29,-1.,-2.01858731750026E-16));
#107400=DIRECTION('ref_axis',(0.685470913635487,0.,0.728100011371879));
#107401=DIRECTION('',(3.79928830675489E-29,-1.,-2.01858731750026E-16));
#107402=DIRECTION('center_axis',(-6.93889390390721E-18,-1.,-2.22049474265475E-16));
#107403=DIRECTION('ref_axis',(0.685470913635487,0.,0.728100011371879));
#107404=DIRECTION('center_axis',(-1.,-4.1792171374299E-28,1.88215207428297E-12));
#107405=DIRECTION('ref_axis',(-1.88215207428297E-12,2.22049474265488E-16,
-1.));
#107406=DIRECTION('',(-3.79928830675446E-29,1.,2.01858731750028E-16));
#107407=DIRECTION('',(-1.88215207428297E-12,2.22049474265488E-16,-1.));
#107408=DIRECTION('center_axis',(0.,1.,2.01858731750028E-16));
#107409=DIRECTION('ref_axis',(0.740974920562388,0.,-0.671532699946594));
#107410=DIRECTION('',(0.,-1.,-2.01858731750028E-16));
#107411=DIRECTION('center_axis',(-6.93889390390721E-18,-1.,-2.22049474265475E-16));
#107412=DIRECTION('ref_axis',(0.740974920562388,0.,-0.671532699946594));
#107413=DIRECTION('center_axis',(0.,1.,2.01858731750028E-16));
#107414=DIRECTION('ref_axis',(0.425760116003353,-1.82649062652652E-16,0.904836075552258));
#107415=DIRECTION('',(0.,1.,2.01858731750028E-16));
#107416=DIRECTION('center_axis',(0.,-1.,-2.22044604925031E-16));
#107417=DIRECTION('ref_axis',(0.89959196856447,-9.69738446503996E-17,0.436731370632224));
#107418=DIRECTION('center_axis',(-6.93889390390721E-18,-1.,-2.22049474265475E-16));
#107419=DIRECTION('ref_axis',(1.,-6.93889390390721E-18,-1.83750175990301E-19));
#107420=DIRECTION('center_axis',(-6.93889390390721E-18,-1.,-2.22049474265475E-16));
#107421=DIRECTION('ref_axis',(0.,2.01858731750028E-16,-1.));
#107422=DIRECTION('center_axis',(-0.961527331301806,0.,-0.274709284807824));
#107423=DIRECTION('ref_axis',(-0.274709284807824,0.,0.961527331301806));
#107424=DIRECTION('center_axis',(-6.93889390390721E-18,-1.,-2.22049474265475E-16));
#107425=DIRECTION('ref_axis',(0.544438391932684,1.82477483735409E-16,-0.838800832969158));
#107426=DIRECTION('center_axis',(0.642414549106759,0.,0.766357323378566));
#107427=DIRECTION('ref_axis',(0.,1.,0.));
#107428=DIRECTION('center_axis',(6.93889390390721E-18,1.,2.22049474265475E-16));
#107429=DIRECTION('ref_axis',(0.544438391932684,1.92747052886312E-16,-0.838800832969158));
#107430=DIRECTION('center_axis',(0.979447089047538,0.,0.201701263645781));
#107431=DIRECTION('ref_axis',(0.,1.,0.));
#107432=DIRECTION('center_axis',(-6.93889390390721E-18,-1.,-2.22049474265475E-16));
#107433=DIRECTION('ref_axis',(-0.512525209353285,-1.73472347597681E-16,
0.858672178294703));
#107434=DIRECTION('center_axis',(6.93889390390721E-18,1.,2.22049474265475E-16));
#107435=DIRECTION('ref_axis',(-0.512525209353286,-1.87111347705949E-16,
0.858672178294703));
#107436=DIRECTION('center_axis',(6.93889390390721E-18,1.,2.22049474265475E-16));
#107437=DIRECTION('ref_axis',(0.,-2.15078296159505E-16,1.));
#107438=DIRECTION('center_axis',(0.997789534013799,0.,0.0664533356012022));
#107439=DIRECTION('ref_axis',(0.,1.,0.));
#107440=DIRECTION('center_axis',(-6.93889390390721E-18,-1.,-2.22049474265475E-16));
#107441=DIRECTION('ref_axis',(-0.134390600847534,-2.1916945940167E-16,0.990928436570391));
#107442=DIRECTION('center_axis',(6.93889390390721E-18,1.,2.22049474265475E-16));
#107443=DIRECTION('ref_axis',(-0.134390600847534,-2.19102616254201E-16,
0.990928436570391));
#107444=DIRECTION('center_axis',(-6.93889390390721E-18,-1.,-2.22049474265475E-16));
#107445=DIRECTION('ref_axis',(0.,1.8503717077086E-16,-1.));
#107446=DIRECTION('center_axis',(0.0349202536836706,0.,0.999390101953521));
#107447=DIRECTION('ref_axis',(0.,1.,0.));
#107448=DIRECTION('center_axis',(6.93889390390721E-18,1.,2.22049474265475E-16));
#107449=DIRECTION('ref_axis',(0.718181642132044,1.73472347597681E-16,-0.695855681089492));
#107450=DIRECTION('center_axis',(-6.93889390390721E-18,-1.,-2.22049474265475E-16));
#107451=DIRECTION('ref_axis',(0.718181642132044,1.49531001932078E-16,-0.695855681089492));
#107452=DIRECTION('center_axis',(-6.93889390390721E-18,-1.,-2.22049474265475E-16));
#107453=DIRECTION('ref_axis',(0.,2.06553120860494E-16,-1.));
#107454=DIRECTION('center_axis',(0.0174573777538545,0.,0.999847608369375));
#107455=DIRECTION('ref_axis',(0.,1.,0.));
#107456=DIRECTION('center_axis',(6.93889390390721E-18,1.,2.22049474265475E-16));
#107457=DIRECTION('ref_axis',(0.999656987972984,0.,-0.0261898147527144));
#107458=DIRECTION('center_axis',(-6.93889390390721E-18,-1.,-2.22049474265475E-16));
#107459=DIRECTION('ref_axis',(0.999656987972984,-1.12107918289356E-18,-0.0261898147527144));
#107460=DIRECTION('center_axis',(0.999631786816462,0.,0.0271346786627047));
#107461=DIRECTION('ref_axis',(0.,1.,0.));
#107462=DIRECTION('center_axis',(-6.93889390390721E-18,-1.,-2.22049474265475E-16));
#107463=DIRECTION('ref_axis',(-0.71052079274556,-1.73472347597681E-16,0.703676206131926));
#107464=DIRECTION('center_axis',(6.93889390390721E-18,1.,2.22049474265475E-16));
#107465=DIRECTION('ref_axis',(-0.71052079274556,-1.51320703227337E-16,0.703676206131926));
#107466=DIRECTION('center_axis',(0.999631786816462,-1.29615800431083E-17,
0.0271346786627023));
#107467=DIRECTION('ref_axis',(-0.0191871152877203,0.707106781186547,0.706846415147545));
#107468=DIRECTION('center_axis',(0.999631786816462,0.,0.0271346786627047));
#107469=DIRECTION('ref_axis',(0.,1.,0.));
#107470=DIRECTION('',(-0.999631786816462,1.29615800431083E-17,-0.0271346786627023));
#107471=DIRECTION('',(0.999631786816462,-1.29615800431083E-17,0.0271346786627023));
#107472=DIRECTION('center_axis',(0.,0.,-1.));
#107473=DIRECTION('ref_axis',(0.,1.,0.));
#107474=DIRECTION('center_axis',(-6.93889390390721E-18,-1.,-2.22049474265475E-16));
#107475=DIRECTION('ref_axis',(0.697447245796159,-1.15648231731787E-16,0.716636127564995));
#107476=DIRECTION('center_axis',(6.93889390390721E-18,1.,2.22049474265475E-16));
#107477=DIRECTION('ref_axis',(0.69744724579616,-1.63968187807605E-16,0.716636127564995));
#107478=DIRECTION('center_axis',(-8.32407533012986E-17,2.22049474265475E-16,
-1.));
#107479=DIRECTION('ref_axis',(0.707106781186548,0.707106781186547,0.));
#107480=DIRECTION('center_axis',(0.,0.,-1.));
#107481=DIRECTION('ref_axis',(0.,1.,0.));
#107482=DIRECTION('',(8.32407533012986E-17,-2.22049474265475E-16,1.));
#107483=DIRECTION('',(-8.32407533012986E-17,2.22049474265475E-16,-1.));
#107484=DIRECTION('center_axis',(-0.70710678118655,0.,-0.707106781186545));
#107485=DIRECTION('ref_axis',(0.,1.,0.));
#107486=DIRECTION('center_axis',(-6.93889390390721E-18,-1.,-2.22049474265475E-16));
#107487=DIRECTION('ref_axis',(0.923879532511286,8.67361737988402E-17,-0.382683432365091));
#107488=DIRECTION('center_axis',(6.93889390390721E-18,1.,2.22049474265475E-16));
#107489=DIRECTION('ref_axis',(0.923879532511286,7.85639529106886E-17,-0.382683432365091));
#107490=DIRECTION('center_axis',(-0.707106781186547,1.61919227945412E-16,
-0.707106781186548));
#107491=DIRECTION('ref_axis',(0.500000000000001,0.707106781186546,-0.500000000000001));
#107492=DIRECTION('center_axis',(-0.707106781186548,0.,-0.707106781186548));
#107493=DIRECTION('ref_axis',(0.,1.,0.));
#107494=DIRECTION('',(0.707106781186547,-1.61919227945412E-16,0.707106781186548));
#107495=DIRECTION('',(-0.707106781186547,1.61919227945412E-16,-0.707106781186548));
#107496=DIRECTION('center_axis',(-0.999306434017034,0.,0.0372377621797867));
#107497=DIRECTION('ref_axis',(0.,1.,0.));
#107498=DIRECTION('center_axis',(-6.93889390390721E-18,-1.,-2.22049474265475E-16));
#107499=DIRECTION('ref_axis',(0.365412486013864,1.73472347597681E-16,-0.930845698848723));
#107500=DIRECTION('center_axis',(6.93889390390721E-18,1.,2.22049474265475E-16));
#107501=DIRECTION('ref_axis',(0.365412486013864,2.04158239580024E-16,-0.930845698848723));
#107502=DIRECTION('center_axis',(-6.93889390390721E-18,-1.,-2.22049474265475E-16));
#107503=DIRECTION('ref_axis',(-0.123085713533701,-2.13127337608609E-16,
0.992396043484606));
#107504=DIRECTION('center_axis',(-0.959930094890458,0.,-0.280239563451696));
#107505=DIRECTION('ref_axis',(0.,1.,0.));
#107506=DIRECTION('center_axis',(6.93889390390721E-18,1.,2.22049474265475E-16));
#107507=DIRECTION('ref_axis',(-0.1230857135337,-2.19181085988492E-16,0.992396043484606));
#107508=DIRECTION('center_axis',(-6.93889390390721E-18,-1.,-2.22049474265475E-16));
#107509=DIRECTION('ref_axis',(-0.1230857135337,-2.19506941011597E-16,0.992396043484606));
#107510=DIRECTION('center_axis',(-0.360174124451025,0.,0.932885094787101));
#107511=DIRECTION('ref_axis',(0.,1.,0.));
#107512=DIRECTION('center_axis',(-6.93889390390721E-18,-1.,-2.22049474265475E-16));
#107513=DIRECTION('ref_axis',(-0.44318546164383,2.31296463463574E-16,-0.896429945164454));
#107514=DIRECTION('center_axis',(6.93889390390721E-18,1.,2.22049474265475E-16));
#107515=DIRECTION('ref_axis',(-0.44318546164383,2.02127014937696E-16,-0.896429945164454));
#107516=DIRECTION('center_axis',(-6.93889390390721E-18,-1.,-2.22049474265475E-16));
#107517=DIRECTION('ref_axis',(0.,2.11471052309554E-16,-1.));
#107518=DIRECTION('center_axis',(-0.598212156168195,0.,0.801337766620667));
#107519=DIRECTION('ref_axis',(0.,1.,0.));
#107520=DIRECTION('center_axis',(6.93889390390721E-18,1.,2.22049474265475E-16));
#107521=DIRECTION('ref_axis',(0.875241543457166,-1.14455981920119E-16,0.483686097181549));
#107522=DIRECTION('center_axis',(-6.93889390390721E-18,-1.,-2.22049474265475E-16));
#107523=DIRECTION('ref_axis',(0.875241543457166,-1.13475451799024E-16,0.483686097181549));
#107524=DIRECTION('center_axis',(-6.93889390390721E-18,-1.,-2.22049474265475E-16));
#107525=DIRECTION('ref_axis',(-0.947452442825118,-1.15648231731787E-16,
0.319896652975169));
#107526=DIRECTION('center_axis',(6.93889390390721E-18,1.,2.22049474265475E-16));
#107527=DIRECTION('ref_axis',(-0.947452442825118,-6.44586116326602E-17,
0.319896652975169));
#107528=DIRECTION('center_axis',(1.13917782314015E-33,-1.,-1.88173394004264E-16));
#107529=DIRECTION('ref_axis',(0.923879532511287,0.,-0.382683432365089));
#107530=DIRECTION('',(-1.62923501610704E-32,-1.,-1.88173394004264E-16));
#107531=DIRECTION('center_axis',(0.,-1.,-2.22044604925031E-16));
#107532=DIRECTION('ref_axis',(0.923879532511287,0.,-0.382683432365089));
#107533=DIRECTION('',(-1.13917782314014E-33,1.,1.88173394004264E-16));
#107534=DIRECTION('center_axis',(-0.707106781186548,-1.33058682939303E-16,
0.707106781186547));
#107535=DIRECTION('ref_axis',(-0.707106781186547,1.61919227945412E-16,-0.707106781186548));
#107536=DIRECTION('',(0.,1.,1.88173394004264E-16));
#107537=DIRECTION('',(-0.707106781186547,1.61919227945412E-16,-0.707106781186548));
#107538=DIRECTION('center_axis',(0.,1.,1.88173394004264E-16));
#107539=DIRECTION('ref_axis',(0.365412486013864,0.,-0.930845698848723));
#107540=DIRECTION('',(0.,-1.,-1.88173394004264E-16));
#107541=DIRECTION('center_axis',(0.,-1.,-2.22044604925031E-16));
#107542=DIRECTION('ref_axis',(0.365412486013864,0.,-0.930845698848723));
#107543=DIRECTION('center_axis',(0.,1.,1.88173394004264E-16));
#107544=DIRECTION('ref_axis',(0.13797098470004,-1.86373754703504E-16,0.99043627123652));
#107545=DIRECTION('',(0.,1.,1.88173394004264E-16));
#107546=DIRECTION('center_axis',(0.,-1.,-2.22044604925031E-16));
#107547=DIRECTION('ref_axis',(0.13797098470004,-1.86373754703504E-16,0.99043627123652));
#107548=DIRECTION('center_axis',(0.,1.,2.01858731750028E-16));
#107549=DIRECTION('ref_axis',(-0.443185461643831,0.,-0.896429945164453));
#107550=DIRECTION('',(0.,-1.,-2.01858731750028E-16));
#107551=DIRECTION('center_axis',(0.,-1.,-2.22044604925031E-16));
#107552=DIRECTION('ref_axis',(-0.443185461643831,0.,-0.896429945164453));
#107553=DIRECTION('center_axis',(0.,1.,2.01858731750028E-16));
#107554=DIRECTION('ref_axis',(-0.984274724761795,3.56572272070144E-17,-0.176644462678833));
#107555=DIRECTION('',(0.,1.,2.01858731750028E-16));
#107556=DIRECTION('center_axis',(0.,-1.,-2.22044604925031E-16));
#107557=DIRECTION('ref_axis',(-0.984274724761795,3.56572272070144E-17,-0.176644462678833));
#107558=DIRECTION('center_axis',(0.,1.,2.00642715293703E-16));
#107559=DIRECTION('ref_axis',(-0.947452442825118,0.,0.319896652975169));
#107560=DIRECTION('',(0.,-1.,-2.00642715293703E-16));
#107561=DIRECTION('center_axis',(0.,-1.,-2.22044604925031E-16));
#107562=DIRECTION('ref_axis',(-0.947452442825118,0.,0.319896652975169));
#107563=DIRECTION('center_axis',(0.,1.,2.00642715293703E-16));
#107564=DIRECTION('ref_axis',(1.,0.,1.39223851401487E-33));
#107565=DIRECTION('',(0.,1.,2.00642715293703E-16));
#107566=DIRECTION('center_axis',(0.,-1.,-2.22044604925031E-16));
#107567=DIRECTION('ref_axis',(1.,0.,1.39223851401487E-33));
#107568=DIRECTION('',(0.,-1.,-2.00642715293703E-16));
#107569=DIRECTION('center_axis',(-6.93889390390723E-18,-1.,-2.22049474265475E-16));
#107570=DIRECTION('ref_axis',(1.,-6.93889390390723E-18,-1.83750175990302E-19));
#107571=DIRECTION('center_axis',(-6.93889390390721E-18,-1.,-2.22049474265475E-16));
#107572=DIRECTION('ref_axis',(1.,-6.93889390390721E-18,-1.83750175990301E-19));
#107573=DIRECTION('center_axis',(-6.93889390390725E-18,-1.,-2.22049474265475E-16));
#107574=DIRECTION('ref_axis',(0.,2.03710646720212E-16,-1.));
#107575=DIRECTION('center_axis',(-0.00645890109586822,0.,-0.99997914108077));
#107576=DIRECTION('ref_axis',(-0.99997914108077,0.,0.00645890109586822));
#107577=DIRECTION('center_axis',(-6.93889390390725E-18,-1.,-2.22049474265475E-16));
#107578=DIRECTION('ref_axis',(0.813766779597698,-1.34699921502175E-16,0.581191559146545));
#107579=DIRECTION('center_axis',(-0.947984515197821,0.,0.31831644466655));
#107580=DIRECTION('ref_axis',(0.,1.,0.));
#107581=DIRECTION('center_axis',(6.93889390390725E-18,1.,2.22049474265475E-16));
#107582=DIRECTION('ref_axis',(0.813766779597698,-1.34301172333688E-16,0.581191559146545));
#107583=DIRECTION('center_axis',(0.989904612137255,0.,0.141735171603208));
#107584=DIRECTION('ref_axis',(0.,1.,0.));
#107585=DIRECTION('center_axis',(-6.93889390390725E-18,-1.,-2.22049474265475E-16));
#107586=DIRECTION('ref_axis',(-0.995874208858217,0.,0.0907444771378411));
#107587=DIRECTION('center_axis',(6.93889390390725E-18,1.,2.22049474265475E-16));
#107588=DIRECTION('ref_axis',(-0.995874208858217,-1.32394979640483E-17,
0.0907444771378411));
#107589=DIRECTION('center_axis',(6.93889390390725E-18,1.,2.22049474265475E-16));
#107590=DIRECTION('ref_axis',(0.,-2.1541640776309E-16,1.));
#107591=DIRECTION('center_axis',(1.,0.,0.));
#107592=DIRECTION('ref_axis',(0.,1.,0.));
#107593=DIRECTION('center_axis',(-6.93889390390725E-18,-1.,-2.22049474265475E-16));
#107594=DIRECTION('ref_axis',(-0.0710471247227679,-2.22665998408963E-16,
0.997472960068907));
#107595=DIRECTION('center_axis',(6.93889390390725E-18,1.,2.22049474265475E-16));
#107596=DIRECTION('ref_axis',(-0.0710471247227679,-2.20995357916699E-16,
0.997472960068907));
#107597=DIRECTION('center_axis',(1.,-6.93889390390718E-18,-3.2590836004222E-16));
#107598=DIRECTION('ref_axis',(0.,0.707106781186547,0.707106781186548));
#107599=DIRECTION('center_axis',(1.,0.,1.38777878078144E-15));
#107600=DIRECTION('ref_axis',(0.,1.,0.));
#107601=DIRECTION('',(-1.,6.93889390390718E-18,3.2590836004222E-16));
#107602=DIRECTION('',(1.,-6.93889390390718E-18,-3.2590836004222E-16));
#107603=DIRECTION('center_axis',(0.472653347758817,0.,-0.881248439914865));
#107604=DIRECTION('ref_axis',(0.,1.,0.));
#107605=DIRECTION('center_axis',(-6.93889390390725E-18,-1.,-2.22049474265475E-16));
#107606=DIRECTION('ref_axis',(0.51349131065734,-1.73472347597681E-16,0.858094793061587));
#107607=DIRECTION('center_axis',(6.93889390390725E-18,1.,2.22049474265475E-16));
#107608=DIRECTION('ref_axis',(0.51349131065734,-1.94102559394496E-16,0.858094793061587));
#107609=DIRECTION('center_axis',(6.93889390390725E-18,1.,2.22049474265475E-16));
#107610=DIRECTION('ref_axis',(0.,-2.22044604925031E-16,1.));
#107611=DIRECTION('center_axis',(0.00430977270832746,0.,-0.999990712886476));
#107612=DIRECTION('ref_axis',(0.,1.,0.));
#107613=DIRECTION('center_axis',(-6.93889390390725E-18,-1.,-2.22049474265475E-16));
#107614=DIRECTION('ref_axis',(0.969330497601796,-5.78241158658936E-17,0.24576083174309));
#107615=DIRECTION('center_axis',(6.93889390390725E-18,1.,2.22049474265475E-16));
#107616=DIRECTION('ref_axis',(0.969330497601796,-6.12971449642794E-17,0.24576083174309));
#107617=DIRECTION('center_axis',(-0.96830751921471,0.,0.249760982205497));
#107618=DIRECTION('ref_axis',(0.,1.,0.));
#107619=DIRECTION('center_axis',(-6.93889390390725E-18,-1.,-2.22049474265475E-16));
#107620=DIRECTION('ref_axis',(0.614172012824047,1.73472347597681E-16,-0.789172185688053));
#107621=DIRECTION('center_axis',(6.93889390390725E-18,1.,2.22049474265475E-16));
#107622=DIRECTION('ref_axis',(0.614172012824046,1.70973594501233E-16,-0.789172185688053));
#107623=DIRECTION('center_axis',(-6.93889390390725E-18,-1.,-2.22049474265475E-16));
#107624=DIRECTION('ref_axis',(-0.0145150489551482,-2.03710646725265E-16,
0.999894651127722));
#107625=DIRECTION('center_axis',(-0.960649678360777,0.,-0.277762840324864));
#107626=DIRECTION('ref_axis',(0.,1.,0.));
#107627=DIRECTION('center_axis',(6.93889390390725E-18,1.,2.22049474265475E-16));
#107628=DIRECTION('ref_axis',(-0.0145150489551485,-2.19846143496015E-16,
0.999894651127722));
#107629=DIRECTION('center_axis',(-6.93889390390725E-18,-1.,-2.22049474265475E-16));
#107630=DIRECTION('ref_axis',(-0.0145150489551485,-2.21925363219061E-16,
0.999894651127722));
#107631=DIRECTION('center_axis',(-6.93889390390725E-18,-1.,-2.22049474265475E-16));
#107632=DIRECTION('ref_axis',(-0.603509608361002,1.73472347597681E-16,-0.797355725266929));
#107633=DIRECTION('center_axis',(6.93889390390725E-18,1.,2.22049474265475E-16));
#107634=DIRECTION('ref_axis',(-0.603509608361002,1.81240108740494E-16,-0.797355725266929));
#107635=DIRECTION('center_axis',(0.,-1.,-2.22044604925031E-16));
#107636=DIRECTION('ref_axis',(0.957056520812277,-6.43710396276775E-17,0.28990139008066));
#107637=DIRECTION('',(0.,1.,2.22044604925031E-16));
#107638=DIRECTION('center_axis',(0.,-1.,-2.22044604925031E-16));
#107639=DIRECTION('ref_axis',(-1.,0.,0.));
#107640=DIRECTION('',(0.,1.,2.22044604925031E-16));
#107641=DIRECTION('center_axis',(0.,1.,2.22044604925031E-16));
#107642=DIRECTION('ref_axis',(-1.,0.,0.));
#107643=DIRECTION('',(0.,-1.,-2.22044604925031E-16));
#107644=DIRECTION('center_axis',(0.,-1.,-2.22044604925031E-16));
#107645=DIRECTION('ref_axis',(-1.,0.,0.));
#107646=DIRECTION('',(0.,-1.,-2.22044604925031E-16));
#107647=DIRECTION('center_axis',(0.,1.,0.));
#107648=DIRECTION('ref_axis',(0.614172012824043,0.,-0.789172185688056));
#107649=DIRECTION('',(0.,-1.,0.));
#107650=DIRECTION('center_axis',(0.,-1.,-2.22044604925031E-16));
#107651=DIRECTION('ref_axis',(0.614172012824043,0.,-0.789172185688056));
#107652=DIRECTION('center_axis',(0.,1.,0.));
#107653=DIRECTION('ref_axis',(0.414254853160806,0.,0.910160928975046));
#107654=DIRECTION('',(0.,1.,0.));
#107655=DIRECTION('center_axis',(0.,-1.,-2.22044604925031E-16));
#107656=DIRECTION('ref_axis',(0.414254853160806,0.,0.910160928975046));
#107657=DIRECTION('center_axis',(0.,1.,0.));
#107658=DIRECTION('ref_axis',(-0.603509608361001,0.,-0.79735572526693));
#107659=DIRECTION('',(0.,-1.,0.));
#107660=DIRECTION('center_axis',(0.,-1.,-2.22044604925031E-16));
#107661=DIRECTION('ref_axis',(-0.603509608361001,0.,-0.79735572526693));
#107662=DIRECTION('center_axis',(0.,1.,0.));
#107663=DIRECTION('ref_axis',(1.,0.,-1.83750175990302E-19));
#107664=DIRECTION('',(0.,1.,0.));
#107665=DIRECTION('center_axis',(0.,-1.,-2.22044604925031E-16));
#107666=DIRECTION('ref_axis',(1.,0.,-1.83750175990302E-19));
#107667=DIRECTION('center_axis',(-6.93889390390725E-18,-1.,-2.22049474265475E-16));
#107668=DIRECTION('ref_axis',(1.,-6.93889390390725E-18,-1.83750175990301E-19));
#107669=DIRECTION('center_axis',(1.,-6.93889390390718E-18,-2.46926126761481E-16));
#107670=DIRECTION('ref_axis',(0.,0.707106781186548,0.707106781186548));
#107671=DIRECTION('center_axis',(-1.,0.,0.));
#107672=DIRECTION('ref_axis',(0.,0.,1.));
#107673=DIRECTION('',(1.,-6.93889390390718E-18,-2.46926126761481E-16));
#107674=DIRECTION('center_axis',(1.,0.,0.));
#107675=DIRECTION('ref_axis',(0.,1.,0.));
#107676=DIRECTION('',(-1.,6.93889390390718E-18,2.46926126761481E-16));
#107677=DIRECTION('center_axis',(0.,0.,-1.));
#107678=DIRECTION('ref_axis',(0.,1.,0.));
#107679=DIRECTION('center_axis',(-6.93889390390723E-18,-1.,-2.22049474265475E-16));
#107680=DIRECTION('ref_axis',(0.707106781186548,-1.15648231731787E-16,0.707106781186547));
#107681=DIRECTION('center_axis',(6.93889390390723E-18,1.,2.22049474265475E-16));
#107682=DIRECTION('ref_axis',(0.707106781186548,-1.61919227945412E-16,0.707106781186547));
#107683=DIRECTION('center_axis',(1.54077774334651E-33,2.22049474265475E-16,
-1.));
#107684=DIRECTION('ref_axis',(0.707106781186548,0.707106781186547,0.));
#107685=DIRECTION('center_axis',(0.,0.,-1.));
#107686=DIRECTION('ref_axis',(0.,1.,0.));
#107687=DIRECTION('',(-1.54077774334651E-33,-2.22049474265475E-16,1.));
#107688=DIRECTION('',(1.54077774334651E-33,2.22049474265475E-16,-1.));
#107689=DIRECTION('center_axis',(-0.845470457966937,0.,0.534022194955582));
#107690=DIRECTION('ref_axis',(0.,1.,0.));
#107691=DIRECTION('center_axis',(-6.93889390390723E-18,-1.,-2.22049474265475E-16));
#107692=DIRECTION('ref_axis',(0.482689240114392,2.31296463463574E-16,-0.875791697538741));
#107693=DIRECTION('center_axis',(6.93889390390723E-18,1.,2.22049474265475E-16));
#107694=DIRECTION('ref_axis',(0.482689240114392,1.91119756578834E-16,-0.875791697538742));
#107695=DIRECTION('center_axis',(-6.93889390390723E-18,-1.,-2.22049474265475E-16));
#107696=DIRECTION('ref_axis',(0.00955154174511641,-2.01858731750028E-16,
0.99995438298469));
#107697=DIRECTION('center_axis',(-0.855517195345567,0.,-0.517774399201095));
#107698=DIRECTION('ref_axis',(0.,1.,0.));
#107699=DIRECTION('center_axis',(6.93889390390723E-18,1.,2.22049474265475E-16));
#107700=DIRECTION('ref_axis',(0.00955154174511598,-2.31296463463574E-16,
0.99995438298469));
#107701=DIRECTION('center_axis',(-6.93889390390723E-18,-1.,-2.22049474265475E-16));
#107702=DIRECTION('ref_axis',(0.00955154174511598,-2.22105622165996E-16,
0.99995438298469));
#107703=DIRECTION('center_axis',(-0.238180414155802,0.,0.971220927653729));
#107704=DIRECTION('ref_axis',(0.,1.,0.));
#107705=DIRECTION('center_axis',(-6.93889390390723E-18,-1.,-2.22049474265475E-16));
#107706=DIRECTION('ref_axis',(-0.382987746401723,2.31296463463574E-16,-0.923753422784527));
#107707=DIRECTION('center_axis',(6.93889390390723E-18,1.,2.22049474265475E-16));
#107708=DIRECTION('ref_axis',(-0.382987746401723,2.07776473219015E-16,-0.923753422784527));
#107709=DIRECTION('center_axis',(-6.93889390390723E-18,-1.,-2.22049474265475E-16));
#107710=DIRECTION('ref_axis',(0.,2.22044604925031E-16,-1.));
#107711=DIRECTION('center_axis',(-0.369109963398455,0.,0.929385729888291));
#107712=DIRECTION('ref_axis',(0.,1.,0.));
#107713=DIRECTION('center_axis',(6.93889390390723E-18,1.,2.22049474265475E-16));
#107714=DIRECTION('ref_axis',(0.952555538217842,-7.35943292838645E-17,0.304364824857469));
#107715=DIRECTION('center_axis',(-6.93889390390723E-18,-1.,-2.22049474265475E-16));
#107716=DIRECTION('ref_axis',(0.952555538217842,-7.41937311617772E-17,0.304364824857469));
#107717=DIRECTION('center_axis',(-6.93889390390723E-18,-1.,-2.22049474265475E-16));
#107718=DIRECTION('ref_axis',(-0.82737837879608,-1.15648231731787E-16,0.561644921904196));
#107719=DIRECTION('center_axis',(6.93889390390723E-18,1.,2.22049474265475E-16));
#107720=DIRECTION('ref_axis',(-0.82737837879608,-1.18971868843848E-16,0.561644921904196));
#107721=DIRECTION('center_axis',(0.,-1.,-2.67523620391604E-16));
#107722=DIRECTION('ref_axis',(-0.382987746401723,0.,-0.923753422784527));
#107723=DIRECTION('',(0.,-1.,-2.67523620391604E-16));
#107724=DIRECTION('center_axis',(0.,-1.,-2.22044604925031E-16));
#107725=DIRECTION('ref_axis',(-0.382987746401723,0.,-0.923753422784527));
#107726=DIRECTION('',(0.,1.,2.67523620391604E-16));
#107727=DIRECTION('center_axis',(0.,1.,2.67523620391604E-16));
#107728=DIRECTION('ref_axis',(0.846680472137446,1.42349762883284E-16,-0.532101661434271));
#107729=DIRECTION('',(0.,1.,2.67523620391604E-16));
#107730=DIRECTION('center_axis',(0.,-1.,-2.22044604925031E-16));
#107731=DIRECTION('ref_axis',(0.846680472137446,1.42349762883284E-16,-0.532101661434271));
#107732=DIRECTION('center_axis',(0.,-1.,-2.67523620391604E-16));
#107733=DIRECTION('ref_axis',(-0.827378378796083,0.,0.561644921904192));
#107734=DIRECTION('',(0.,-1.,-2.67523620391604E-16));
#107735=DIRECTION('center_axis',(0.,-1.,-2.22044604925031E-16));
#107736=DIRECTION('ref_axis',(-0.827378378796083,0.,0.561644921904192));
#107737=DIRECTION('center_axis',(2.46926126761481E-16,-2.67523620391604E-16,
1.));
#107738=DIRECTION('ref_axis',(1.,-6.93889390390717E-18,-2.46926126761481E-16));
#107739=DIRECTION('',(0.,1.,2.67523620391604E-16));
#107740=DIRECTION('',(1.,5.48286142624213E-32,-2.46926126761481E-16));
#107741=DIRECTION('center_axis',(-6.93889390390723E-18,-1.,-2.22049474265475E-16));
#107742=DIRECTION('ref_axis',(1.,-6.93889390390723E-18,1.54077774334651E-33));
#107743=DIRECTION('center_axis',(-0.185783118407687,-0.485875683947296,
0.854054712921521));
#107744=DIRECTION('ref_axis',(-0.97714808085684,5.55111512312577E-15,-0.212559704736796));
#107745=DIRECTION('center_axis',(-0.947567167180116,0.319117547005372,0.0167467870209411));
#107746=DIRECTION('ref_axis',(-0.0176706968910312,0.,-0.999843861046006));
#107747=DIRECTION('center_axis',(0.,-1.,-2.22044604925031E-16));
#107748=DIRECTION('ref_axis',(0.634326560888794,-1.71654958451944E-16,0.773065206920474));
#107749=DIRECTION('',(0.,1.,2.22044604925031E-16));
#107750=DIRECTION('center_axis',(0.,1.,2.22044604925031E-16));
#107751=DIRECTION('ref_axis',(0.634326560888794,-1.71654958451944E-16,0.773065206920474));
#107752=DIRECTION('center_axis',(0.,-1.,-2.22044604925031E-16));
#107753=DIRECTION('ref_axis',(1.,0.,0.));
#107754=DIRECTION('',(0.,1.,2.22044604925031E-16));
#107755=DIRECTION('center_axis',(4.16333634234434E-17,-1.,-2.28983498828938E-16));
#107756=DIRECTION('ref_axis',(1.,0.,0.));
#107757=DIRECTION('',(0.,-1.,-2.22044604925031E-16));
#107758=DIRECTION('center_axis',(-6.93889390390725E-18,-1.,-2.22049474265475E-16));
#107759=DIRECTION('ref_axis',(1.,0.,0.));
#107760=DIRECTION('center_axis',(0.,1.,2.22044604925031E-16));
#107761=DIRECTION('ref_axis',(1.,0.,1.49586791797067E-33));
#107762=DIRECTION('center_axis',(0.,1.,2.22044604925031E-16));
#107763=DIRECTION('ref_axis',(1.,0.,0.));
#107764=DIRECTION('',(0.,1.,2.22044604925031E-16));
#107765=DIRECTION('center_axis',(0.,1.,2.22044604925031E-16));
#107766=DIRECTION('ref_axis',(1.,0.,1.49586791797067E-33));
#107767=DIRECTION('',(0.,-1.,-2.22044604925031E-16));
#107768=DIRECTION('center_axis',(0.,-1.,-2.22044604925031E-16));
#107769=DIRECTION('ref_axis',(1.,0.,0.));
#107770=DIRECTION('',(0.,1.,2.22044604925031E-16));
#107771=DIRECTION('center_axis',(0.,-1.,-2.22044604925031E-16));
#107772=DIRECTION('ref_axis',(1.,0.,0.));
#107773=DIRECTION('center_axis',(0.,-1.,-2.22044604925031E-16));
#107774=DIRECTION('ref_axis',(1.,0.,0.));
#107775=DIRECTION('center_axis',(3.42121385298657E-49,-1.,-2.22044604925031E-16));
#107776=DIRECTION('ref_axis',(1.,0.,1.54077774334651E-33));
#107777=DIRECTION('center_axis',(0.,-1.,-2.22044604925031E-16));
#107778=DIRECTION('ref_axis',(-0.438909080076843,0.,0.898531479374039));
#107779=DIRECTION('center_axis',(-4.16333634234434E-17,1.,2.28983498828938E-16));
#107780=DIRECTION('ref_axis',(-0.438909080076843,0.,0.898531479374039));
#107781=DIRECTION('center_axis',(0.,1.,2.22044604925031E-16));
#107782=DIRECTION('ref_axis',(-0.438909080076843,0.,0.898531479374039));
#107783=DIRECTION('',(1.02786322857718E-29,-1.,-2.22044604925031E-16));
#107784=DIRECTION('center_axis',(4.16333634234434E-17,-1.,-2.28983498828938E-16));
#107785=DIRECTION('ref_axis',(1.,4.16333634234434E-17,6.93889390390723E-17));
#107786=DIRECTION('',(-1.88249434430459E-12,2.2898349882886E-16,-1.));
#107787=DIRECTION('center_axis',(4.16333634234434E-17,-1.,-2.28983498828938E-16));
#107788=DIRECTION('ref_axis',(0.923879532510927,0.,-0.382683432365958));
#107789=DIRECTION('',(0.707106781186548,-1.57009245868377E-16,0.707106781186548));
#107790=DIRECTION('',(-0.707106781186548,-1.57009245868377E-16,0.707106781186547));
#107791=DIRECTION('',(-0.707106781186547,1.57009245868378E-16,-0.707106781186548));
#107792=DIRECTION('center_axis',(9.62964972189322E-33,1.,2.22044604925031E-16));
#107793=DIRECTION('ref_axis',(0.923879532510927,-3.75530232012134E-16,-0.382683432365958));
#107794=DIRECTION('center_axis',(4.16333634234434E-17,-1.,-2.28983498828938E-16));
#107795=DIRECTION('ref_axis',(0.226765259529559,0.,-0.973949442769229));
#107796=DIRECTION('center_axis',(1.,4.28276345240491E-28,-1.88249434430459E-12));
#107797=DIRECTION('ref_axis',(-1.88249434430459E-12,2.22049474265623E-16,
-1.));
#107798=DIRECTION('',(-1.8825923899717E-12,2.22054343606079E-16,-1.));
#107799=DIRECTION('',(8.56552690482593E-29,-1.,-1.82003774528629E-16));
#107800=DIRECTION('',(1.88250052083182E-12,-2.22044604925031E-16,1.));
#107801=DIRECTION('',(0.,1.,2.27504718160893E-16));
#107802=DIRECTION('center_axis',(0.,-1.,-2.22044604925031E-16));
#107803=DIRECTION('ref_axis',(0.905538513813742,0.,-0.424264068711928));
#107804=DIRECTION('center_axis',(0.,1.,2.22044604925031E-16));
#107805=DIRECTION('ref_axis',(0.905538513813742,0.,-0.424264068711928));
#107806=DIRECTION('',(0.,1.,2.22044604925031E-16));
#107807=DIRECTION('center_axis',(0.,1.,2.22044604925031E-16));
#107808=DIRECTION('ref_axis',(0.905538513813742,0.,-0.424264068711928));
#107809=DIRECTION('',(0.,-1.,-2.22044604925031E-16));
#107810=DIRECTION('center_axis',(0.,-1.,-2.22044604925031E-16));
#107811=DIRECTION('ref_axis',(-1.,0.,0.));
#107812=DIRECTION('center_axis',(0.,1.,2.22044604925031E-16));
#107813=DIRECTION('ref_axis',(-1.,0.,0.));
#107814=DIRECTION('',(0.,-2.22044604925031E-16,1.));
#107815=DIRECTION('center_axis',(0.,-1.,-2.22044604925031E-16));
#107816=DIRECTION('ref_axis',(1.,0.,-1.837501759903E-19));
#107817=DIRECTION('',(-1.,-4.08007352326711E-35,1.837501759903E-19));
#107818=DIRECTION('center_axis',(0.,-1.,-2.22044604925031E-16));
#107819=DIRECTION('ref_axis',(1.,0.,6.93889390390723E-17));
#107820=DIRECTION('',(0.000408627366273739,2.22044586386934E-16,-0.999999916511834));
#107821=DIRECTION('center_axis',(0.,-1.,-2.22044604925031E-16));
#107822=DIRECTION('ref_axis',(0.707251238022098,0.,-0.706962294833472));
#107823=DIRECTION('',(-1.,2.89708077091569E-28,-1.30472918803582E-12));
#107824=DIRECTION('center_axis',(0.,-1.,-2.22044604925031E-16));
#107825=DIRECTION('ref_axis',(-0.827170191871368,0.,-0.561951486944811));
#107826=DIRECTION('center_axis',(0.,-1.,-2.22044604925031E-16));
#107827=DIRECTION('ref_axis',(1.,0.,1.85631801868649E-33));
#107828=DIRECTION('center_axis',(0.,1.,2.22044604925031E-16));
#107829=DIRECTION('ref_axis',(-0.442887523223796,0.,-0.896577181157702));
#107830=DIRECTION('center_axis',(0.,-1.,-2.22044604925031E-16));
#107831=DIRECTION('ref_axis',(0.442887523223796,0.,0.896577181157703));
#107832=DIRECTION('center_axis',(0.,-1.,-2.22044604925031E-16));
#107833=DIRECTION('ref_axis',(0.468176250029908,0.,-0.883635105067659));
#107834=DIRECTION('center_axis',(0.,-1.,-2.22044604925031E-16));
#107835=DIRECTION('ref_axis',(1.,0.,1.15584692836443E-33));
#107836=DIRECTION('center_axis',(0.,-1.,-2.22044604925031E-16));
#107837=DIRECTION('ref_axis',(-0.591607978303977,0.,-0.806225774834246));
#107838=DIRECTION('',(-7.42407262755995E-12,-1.64826352645555E-16,1.));
#107839=DIRECTION('center_axis',(0.,-1.,-2.22044604925031E-16));
#107840=DIRECTION('ref_axis',(-0.923879532512709,3.75530232012858E-16,0.382683432361657));
#107841=DIRECTION('',(0.707106781186547,-2.82505968889577E-16,0.707106781186548));
#107842=DIRECTION('',(-0.707106781186548,-1.57009245868377E-16,0.707106781186547));
#107843=DIRECTION('',(-0.707106781186548,1.66829210022541E-16,-0.707106781186548));
#107844=DIRECTION('center_axis',(0.,1.,2.22044604925031E-16));
#107845=DIRECTION('ref_axis',(-0.923879532511288,0.,0.382683432365088));
#107846=DIRECTION('',(-4.61226199516842E-16,2.22044604925031E-16,-1.));
#107847=DIRECTION('center_axis',(0.,-1.,-2.22044604925031E-16));
#107848=DIRECTION('ref_axis',(-0.939690906904483,-7.59447731678524E-17,
0.342024852139477));
#107849=DIRECTION('',(1.,-2.8970973742862E-28,1.30473666552914E-12));
#107850=DIRECTION('center_axis',(0.,1.,2.22044604925031E-16));
#107851=DIRECTION('ref_axis',(-1.,0.,0.));
#107852=DIRECTION('center_axis',(0.,1.,2.22044604925031E-16));
#107853=DIRECTION('ref_axis',(-1.,0.,0.));
#107854=DIRECTION('center_axis',(0.,1.,2.22044604925031E-16));
#107855=DIRECTION('ref_axis',(-1.,0.,0.));
#107856=DIRECTION('',(0.,1.,2.22044604925031E-16));
#107857=DIRECTION('center_axis',(0.,-1.,-2.22044604925031E-16));
#107858=DIRECTION('ref_axis',(-1.,0.,0.));
#107859=DIRECTION('',(-1.,0.,0.));
#107860=DIRECTION('center_axis',(0.,1.,2.22044604925031E-16));
#107861=DIRECTION('ref_axis',(0.707106781186548,1.57009245868377E-16,-0.707106781186548));
#107862=DIRECTION('',(-1.190587693968E-16,2.22044604925031E-16,-1.));
#107863=DIRECTION('center_axis',(0.,1.,2.22044604925031E-16));
#107864=DIRECTION('ref_axis',(0.923879532511288,0.,0.382683432365088));
#107865=DIRECTION('',(-0.707106781186548,-1.52106150078638E-16,0.707106781186547));
#107866=DIRECTION('center_axis',(0.,-1.,-2.22044604925031E-16));
#107867=DIRECTION('ref_axis',(-0.923879532511647,0.,-0.382683432364221));
#107868=DIRECTION('',(1.88205007134457E-12,-2.22049474265488E-16,1.));
#107869=DIRECTION('center_axis',(0.,1.,2.22044604925031E-16));
#107870=DIRECTION('ref_axis',(0.89959196856447,-9.69738446503996E-17,0.436731370632224));
#107871=DIRECTION('center_axis',(0.,-1.,-2.22044604925031E-16));
#107872=DIRECTION('ref_axis',(-1.,0.,0.));
#107873=DIRECTION('center_axis',(0.,1.,2.22044604925031E-16));
#107874=DIRECTION('ref_axis',(0.706817778969831,-1.57073391034583E-16,0.707395665333168));
#107875=DIRECTION('center_axis',(0.,-1.,-2.22044604925031E-16));
#107876=DIRECTION('ref_axis',(-0.753900508899602,0.,0.656988601636985));
#107877=DIRECTION('center_axis',(-4.16333634234434E-17,1.,2.28983498828938E-16));
#107878=DIRECTION('ref_axis',(-0.984274724761795,4.72565661779708E-17,-0.176644462678832));
#107879=DIRECTION('center_axis',(0.,-1.,-2.22044604925031E-16));
#107880=DIRECTION('ref_axis',(0.0662762646370231,0.,0.997801311256787));
#107881=DIRECTION('center_axis',(0.,-1.,-2.22044604925031E-16));
#107882=DIRECTION('ref_axis',(-1.,0.,-1.85631801868649E-33));
#107883=DIRECTION('center_axis',(0.,1.,2.22044604925031E-16));
#107884=DIRECTION('ref_axis',(1.,1.85370757147271E-31,-6.93889390390722E-16));
#107885=DIRECTION('',(-1.,6.93889390390712E-18,1.83750175990302E-19));
#107886=DIRECTION('center_axis',(-6.93889390390723E-18,-1.,-2.22049474265475E-16));
#107887=DIRECTION('ref_axis',(1.,-6.93889390390723E-18,-1.83750175990302E-19));
#107888=DIRECTION('',(0.,-2.22044604925031E-16,1.));
#107889=DIRECTION('center_axis',(0.,1.,2.22044604925031E-16));
#107890=DIRECTION('ref_axis',(-0.923879532511647,0.,-0.382683432364221));
#107891=DIRECTION('',(0.707106781186548,1.52106150078638E-16,-0.707106781186547));
#107892=DIRECTION('center_axis',(0.,-1.,-2.22044604925031E-16));
#107893=DIRECTION('ref_axis',(-0.934114852736578,0.,0.356972606647795));
#107894=DIRECTION('center_axis',(0.,-1.,-2.22044604925031E-16));
#107895=DIRECTION('ref_axis',(-0.243728531198527,1.95771377718342E-16,-0.969843494116349));
#107896=DIRECTION('center_axis',(0.,1.,2.22044604925031E-16));
#107897=DIRECTION('ref_axis',(0.470867335571779,-1.78080586840007E-16,0.882204030988032));
#107898=DIRECTION('center_axis',(0.,-1.,-2.22044604925031E-16));
#107899=DIRECTION('ref_axis',(0.656130266938609,0.,0.754647648116039));
#107900=DIRECTION('',(-1.88215207428297E-12,2.22049474265488E-16,-1.));
#107901=DIRECTION('center_axis',(0.,-1.,-2.22044604925031E-16));
#107902=DIRECTION('ref_axis',(1.,0.,0.));
#107903=DIRECTION('center_axis',(0.,2.22044604925031E-16,-1.));
#107904=DIRECTION('ref_axis',(1.,0.,0.));
#107905=DIRECTION('',(0.,-1.,-2.22044604925031E-16));
#107906=DIRECTION('',(1.,0.,0.));
#107907=DIRECTION('',(0.,1.,2.22044604925031E-16));
#107908=DIRECTION('center_axis',(-6.50074362628841E-34,-1.,-2.27504718160893E-16));
#107909=DIRECTION('ref_axis',(0.923879532511288,0.,0.382683432365088));
#107910=DIRECTION('',(6.50074362628841E-34,1.,2.27504718160893E-16));
#107911=DIRECTION('center_axis',(0.,-1.,-2.22044604925031E-16));
#107912=DIRECTION('ref_axis',(0.923879532511288,0.,0.382683432365088));
#107913=DIRECTION('',(-6.50074362628841E-34,-1.,-2.27504718160893E-16));
#107914=DIRECTION('center_axis',(-0.707106781186547,1.60870128963502E-16,
-0.707106781186548));
#107915=DIRECTION('ref_axis',(-0.707106781186548,-1.52106150078733E-16,
0.707106781186547));
#107916=DIRECTION('',(0.707106781186548,1.57009245868377E-16,-0.707106781186547));
#107917=DIRECTION('',(0.,1.,2.27504718160893E-16));
#107918=DIRECTION('center_axis',(0.,-1.,-2.22044604925031E-16));
#107919=DIRECTION('ref_axis',(1.,0.,0.));
#107920=DIRECTION('',(1.190587693968E-16,-2.22044604925031E-16,1.));
#107921=DIRECTION('center_axis',(0.,-1.,-2.22044604925031E-16));
#107922=DIRECTION('ref_axis',(0.707106781186548,1.57009245868377E-16,-0.707106781186548));
#107923=DIRECTION('center_axis',(0.,-1.,-2.22044604925031E-16));
#107924=DIRECTION('ref_axis',(-0.939690906904483,-7.59447731678524E-17,
0.342024852139477));
#107925=DIRECTION('',(4.61226199516842E-16,-2.22044604925031E-16,1.));
#107926=DIRECTION('center_axis',(0.,-1.,-2.22044604925031E-16));
#107927=DIRECTION('ref_axis',(-0.923879532511288,0.,0.382683432365088));
#107928=DIRECTION('',(0.707106781186548,-1.57009245868377E-16,0.707106781186548));
#107929=DIRECTION('center_axis',(0.,1.,2.22044604925031E-16));
#107930=DIRECTION('ref_axis',(0.923879532510927,0.,-0.382683432365958));
#107931=DIRECTION('center_axis',(0.,-1.,-2.22044604925031E-16));
#107932=DIRECTION('ref_axis',(-0.923879532510705,0.,0.382683432366494));
#107933=DIRECTION('',(0.707106781187368,-1.57009245868195E-16,0.707106781185727));
#107934=DIRECTION('center_axis',(0.,-1.,-2.22044604925031E-16));
#107935=DIRECTION('ref_axis',(-0.382683432364552,0.,0.92387953251151));
#107936=DIRECTION('',(-1.,1.35429601616597E-31,-6.09920703375441E-16));
#107937=DIRECTION('center_axis',(0.,1.,2.22044604925031E-16));
#107938=DIRECTION('ref_axis',(0.360742674985292,2.07093317185659E-16,-0.932665386108253));
#107939=DIRECTION('center_axis',(0.,1.,2.22044604925031E-16));
#107940=DIRECTION('ref_axis',(0.707106781186547,-1.57009245868377E-16,0.707106781186547));
#107941=DIRECTION('',(0.707106781186548,1.57009245868377E-16,-0.707106781186548));
#107942=DIRECTION('center_axis',(0.,1.,2.22044604925031E-16));
#107943=DIRECTION('ref_axis',(-0.707106781186547,1.57009245868377E-16,-0.707106781186547));
#107944=DIRECTION('center_axis',(0.,1.,2.22044604925031E-16));
#107945=DIRECTION('ref_axis',(-0.993670662656293,-2.49428489271903E-17,
0.112332605134053));
#107946=DIRECTION('',(1.190587693968E-16,-2.22044604925031E-16,1.));
#107947=DIRECTION('center_axis',(0.,-1.,-2.22044604925031E-16));
#107948=DIRECTION('ref_axis',(0.923879532511287,0.,-0.38268343236509));
#107949=DIRECTION('',(-0.707106781186547,1.57009245868378E-16,-0.707106781186548));
#107950=DIRECTION('center_axis',(0.,1.,2.22044604925031E-16));
#107951=DIRECTION('ref_axis',(-0.923879532510926,0.,0.38268343236596));
#107952=DIRECTION('',(-1.88205025509474E-12,2.22044604925031E-16,-1.));
#107953=DIRECTION('center_axis',(0.,1.,2.22044604925031E-16));
#107954=DIRECTION('ref_axis',(-0.923879532511647,0.,-0.382683432364221));
#107955=DIRECTION('',(-0.707106781186548,-1.57009245868377E-16,0.707106781186548));
#107956=DIRECTION('center_axis',(0.,-1.,-2.22044604925031E-16));
#107957=DIRECTION('ref_axis',(0.707106781186548,-1.57009245868377E-16,0.707106781186548));
#107958=DIRECTION('',(0.707106781186548,1.57009245868377E-16,-0.707106781186548));
#107959=DIRECTION('center_axis',(0.,-1.,-2.22044604925031E-16));
#107960=DIRECTION('ref_axis',(-0.707106781186548,1.57009245868377E-16,-0.707106781186548));
#107961=DIRECTION('center_axis',(0.,1.,2.22044604925031E-16));
#107962=DIRECTION('ref_axis',(1.,0.,0.));
#107963=DIRECTION('center_axis',(0.,-1.,-2.22044604925031E-16));
#107964=DIRECTION('ref_axis',(1.,0.,0.));
#107965=DIRECTION('center_axis',(0.,1.,2.22044604925031E-16));
#107966=DIRECTION('ref_axis',(1.,0.,0.));
#107967=DIRECTION('center_axis',(0.,-1.,-2.27504718160893E-16));
#107968=DIRECTION('ref_axis',(-0.923879532511647,0.,-0.382683432364221));
#107969=DIRECTION('',(0.,-1.,-2.27504718160893E-16));
#107970=DIRECTION('center_axis',(-1.,-4.28175312849965E-28,1.88205025509474E-12));
#107971=DIRECTION('ref_axis',(1.88205025509474E-12,-2.22049474265623E-16,
1.));
#107972=DIRECTION('',(-2.6267572334885E-44,1.,2.27504718160893E-16));
#107973=DIRECTION('',(1.88205007134457E-12,-2.22049474265488E-16,1.));
#107974=DIRECTION('center_axis',(6.34155293819033E-44,1.,2.27504718160893E-16));
#107975=DIRECTION('ref_axis',(-0.923879532510926,0.,0.38268343236596));
#107976=DIRECTION('center_axis',(-6.93889390390721E-18,-1.,-2.22049474265475E-16));
#107977=DIRECTION('ref_axis',(-0.923879532510926,0.,0.38268343236596));
#107978=DIRECTION('',(-6.34155293819033E-44,-1.,-2.27504718160893E-16));
#107979=DIRECTION('center_axis',(6.50074362628842E-34,1.,2.27504718160893E-16));
#107980=DIRECTION('ref_axis',(0.923879532511287,0.,-0.38268343236509));
#107981=DIRECTION('',(-6.50074362628842E-34,-1.,-2.27504718160893E-16));
#107982=DIRECTION('center_axis',(0.,1.,2.22044604925031E-16));
#107983=DIRECTION('ref_axis',(0.923879532511287,0.,-0.38268343236509));
#107984=DIRECTION('',(6.50074362628842E-34,1.,2.27504718160893E-16));
#107985=DIRECTION('center_axis',(-0.707106781186548,-1.60870128963501E-16,
0.707106781186547));
#107986=DIRECTION('ref_axis',(0.707106781186547,-1.61919227945507E-16,0.707106781186548));
#107987=DIRECTION('',(0.707106781186547,-1.57009245868378E-16,0.707106781186548));
#107988=DIRECTION('',(0.707106781186547,-1.61919227945412E-16,0.707106781186548));
#107989=DIRECTION('center_axis',(0.,-1.,-2.22044604925031E-16));
#107990=DIRECTION('ref_axis',(-1.,0.,0.));
#107991=DIRECTION('',(-1.190587693968E-16,2.22044604925031E-16,-1.));
#107992=DIRECTION('center_axis',(0.,1.,2.22044604925031E-16));
#107993=DIRECTION('ref_axis',(0.69744724579616,-1.59125185820173E-16,0.716636127564994));
#107994=DIRECTION('',(-0.999631786816462,6.02510900342743E-18,-0.0271346786627024));
#107995=DIRECTION('center_axis',(0.,-1.,-2.22044604925031E-16));
#107996=DIRECTION('ref_axis',(-0.370112462344042,0.,-0.928986956430299));
#107997=DIRECTION('',(-0.707106781186548,-1.57009245868378E-16,0.707106781186548));
#107998=DIRECTION('',(-1.85435565520038E-14,-2.22044604925031E-16,1.));
#107999=DIRECTION('center_axis',(0.,-1.,-2.22044604925031E-16));
#108000=DIRECTION('ref_axis',(0.707106781186561,1.57009245868375E-16,-0.707106781186534));
#108001=DIRECTION('center_axis',(0.,-1.,-2.22044604925031E-16));
#108002=DIRECTION('ref_axis',(0.0271346786627019,0.,-0.999631786816462));
#108003=DIRECTION('',(0.999631786816462,-6.02510900342741E-18,0.0271346786627023));
#108004=DIRECTION('center_axis',(0.,-1.,-2.22044604925031E-16));
#108005=DIRECTION('ref_axis',(0.697447245796159,0.,0.716636127564995));
#108006=DIRECTION('',(-8.32407533012986E-17,2.22044604925031E-16,-1.));
#108007=DIRECTION('center_axis',(0.,-1.,-2.22044604925031E-16));
#108008=DIRECTION('ref_axis',(0.0595262816618969,-2.21650861813111E-16,
0.998226738667878));
#108009=DIRECTION('center_axis',(0.,1.,2.22044604925031E-16));
#108010=DIRECTION('ref_axis',(-0.157390971609958,2.19277123123827E-16,-0.98753636999134));
#108011=DIRECTION('center_axis',(0.,-1.,-2.22044604925031E-16));
#108012=DIRECTION('ref_axis',(0.89959196856447,-9.69738446503996E-17,0.436731370632224));
#108013=DIRECTION('center_axis',(4.004083039641E-17,1.,2.22044604925031E-16));
#108014=DIRECTION('ref_axis',(-0.382683432364552,0.,0.92387953251151));
#108015=DIRECTION('',(-4.004083039641E-17,-1.,-2.22044604925031E-16));
#108016=DIRECTION('center_axis',(0.,1.,2.22044604925031E-16));
#108017=DIRECTION('ref_axis',(-0.382683432364552,0.,0.92387953251151));
#108018=DIRECTION('',(4.004083039641E-17,1.,2.22044604925031E-16));
#108019=DIRECTION('center_axis',(0.707106781185727,1.28696103170951E-16,
-0.707106781187368));
#108020=DIRECTION('ref_axis',(-0.707106781187368,1.6191922794533E-16,-0.707106781185727));
#108021=DIRECTION('',(-8.56552690482593E-29,1.,1.82003774528629E-16));
#108022=DIRECTION('',(-0.707106781187368,1.57009245868195E-16,-0.707106781185727));
#108023=DIRECTION('center_axis',(-8.56552690482593E-29,1.,1.82003774528629E-16));
#108024=DIRECTION('ref_axis',(-0.923879532510705,0.,0.382683432366494));
#108025=DIRECTION('center_axis',(0.,1.,2.22044604925031E-16));
#108026=DIRECTION('ref_axis',(-0.923879532510705,0.,0.382683432366494));
#108027=DIRECTION('center_axis',(0.,-1.,-2.22044604925031E-16));
#108028=DIRECTION('ref_axis',(1.,0.,0.));
#108029=DIRECTION('center_axis',(0.,-1.,-2.22044604925031E-16));
#108030=DIRECTION('ref_axis',(0.371940837143492,0.,0.928256437448725));
#108031=DIRECTION('center_axis',(0.,-1.,-2.22044604925031E-16));
#108032=DIRECTION('ref_axis',(1.,0.,-1.83750175990302E-19));
#108033=DIRECTION('center_axis',(0.,-1.,-2.22044604925031E-16));
#108034=DIRECTION('ref_axis',(0.906884704407261,0.,0.421378847252866));
#108035=DIRECTION('center_axis',(0.,-1.,-2.22044604925031E-16));
#108036=DIRECTION('ref_axis',(0.414254853160806,0.,0.910160928975046));
#108037=DIRECTION('center_axis',(0.,-1.,-2.22044604925031E-16));
#108038=DIRECTION('ref_axis',(0.641559662047602,0.,-0.767073138646744));
#108039=DIRECTION('center_axis',(0.,1.,2.22044604925031E-16));
#108040=DIRECTION('ref_axis',(-0.901335144845703,0.,-0.433122334526835));
#108041=DIRECTION('center_axis',(0.,-1.,-2.22044604925031E-16));
#108042=DIRECTION('ref_axis',(0.141735171603208,0.,-0.989904612137255));
#108043=DIRECTION('center_axis',(0.,1.,2.22044604925031E-16));
#108044=DIRECTION('ref_axis',(2.48741143748787E-16,0.,1.));
#108045=DIRECTION('',(1.,7.23661930473396E-32,-3.2590836004222E-16));
#108046=DIRECTION('center_axis',(0.,-1.,-2.22044604925031E-16));
#108047=DIRECTION('ref_axis',(0.51349131065734,0.,0.858094793061586));
#108048=DIRECTION('center_axis',(0.,1.,2.22044604925031E-16));
#108049=DIRECTION('ref_axis',(-0.891123735454889,-1.00755045690416E-16,
0.453760386227053));
#108050=DIRECTION('',(-1.,-2.58135112964991E-32,1.16253719856037E-16));
#108051=DIRECTION('center_axis',(0.,1.,2.22044604925031E-16));
#108052=DIRECTION('ref_axis',(1.,0.,0.));
#108053=DIRECTION('center_axis',(0.,1.,2.27504718160893E-16));
#108054=DIRECTION('ref_axis',(0.923879532510927,0.,-0.382683432365958));
#108055=DIRECTION('',(0.,-1.,-2.27504718160893E-16));
#108056=DIRECTION('center_axis',(2.09862273058998E-32,1.,2.27504718160893E-16));
#108057=DIRECTION('ref_axis',(-0.923879532511288,0.,0.382683432365088));
#108058=DIRECTION('',(-2.09862273058998E-32,-1.,-2.27504718160893E-16));
#108059=DIRECTION('',(2.09862273058998E-32,1.,2.27504718160893E-16));
#108060=DIRECTION('center_axis',(0.707106781186548,1.60870128963502E-16,
-0.707106781186548));
#108061=DIRECTION('ref_axis',(-0.707106781186548,1.61919227945507E-16,-0.707106781186548));
#108062=DIRECTION('',(-5.33214183189602E-18,1.,2.22172576328997E-16));
#108063=DIRECTION('center_axis',(-0.707106781186547,1.53329341668337E-16,
-0.707106781186548));
#108064=DIRECTION('ref_axis',(-0.707106781186548,-1.57009245868377E-16,
0.707106781186547));
#108065=DIRECTION('',(-2.36032059159488E-16,-1.,1.91916246623874E-17));
#108066=DIRECTION('center_axis',(0.,1.,2.01858731750028E-16));
#108067=DIRECTION('ref_axis',(-0.243728531198527,1.95771377718342E-16,-0.969843494116349));
#108068=DIRECTION('',(0.,1.,2.01858731750028E-16));
#108069=DIRECTION('',(0.,-1.,-2.01858731750028E-16));
#108070=DIRECTION('center_axis',(0.,1.,2.01858731750028E-16));
#108071=DIRECTION('ref_axis',(0.470867335571779,-1.78080586840007E-16,0.882204030988032));
#108072=DIRECTION('',(0.,1.,2.01858731750028E-16));
#108073=DIRECTION('center_axis',(-2.57578868254608E-29,-1.,-2.01858731750032E-16));
#108074=DIRECTION('ref_axis',(0.656130266938609,0.,0.754647648116039));
#108075=DIRECTION('',(-2.57578868254608E-29,-1.,-2.01858731750032E-16));
#108076=DIRECTION('center_axis',(-1.,-3.54170943849992E-28,1.88215207428297E-12));
#108077=DIRECTION('ref_axis',(-1.88215207428297E-12,2.22049474265488E-16,
-1.));
#108078=DIRECTION('',(-4.48415508583941E-44,1.,1.88173394004264E-16));
#108079=DIRECTION('center_axis',(0.,-1.,-1.88173394004264E-16));
#108080=DIRECTION('ref_axis',(-0.923879532511647,0.,-0.382683432364221));
#108081=DIRECTION('',(0.,-1.,-1.88173394004264E-16));
#108082=DIRECTION('center_axis',(-0.707106781186547,1.33058682939303E-16,
-0.707106781186548));
#108083=DIRECTION('ref_axis',(0.707106781186548,1.52106150078638E-16,-0.707106781186547));
#108084=DIRECTION('center_axis',(0.,-1.,-2.01858731750028E-16));
#108085=DIRECTION('ref_axis',(-0.956462973763756,0.,-0.291853695914568));
#108086=DIRECTION('',(0.,-1.,-2.01858731750028E-16));
#108087=DIRECTION('center_axis',(0.,-1.,-2.22044604925031E-16));
#108088=DIRECTION('ref_axis',(-0.956462973763756,0.,-0.291853695914568));
#108089=DIRECTION('',(0.,1.,2.01858731750028E-16));
#108090=DIRECTION('center_axis',(0.,1.,2.01858731750028E-16));
#108091=DIRECTION('ref_axis',(-0.984274724761795,3.56572272070144E-17,-0.176644462678833));
#108092=DIRECTION('',(0.,1.,2.01858731750028E-16));
#108093=DIRECTION('center_axis',(0.,-1.,-2.22044604925031E-16));
#108094=DIRECTION('ref_axis',(-0.984274724761795,3.56572272070144E-17,-0.176644462678833));
#108095=DIRECTION('center_axis',(-3.14252774266953E-33,-1.,-2.01858731750028E-16));
#108096=DIRECTION('ref_axis',(-0.83018371253477,0.,0.557489913309636));
#108097=DIRECTION('center_axis',(0.,-1.,-2.22044604925031E-16));
#108098=DIRECTION('ref_axis',(-0.83018371253477,0.,0.557489913309636));
#108099=DIRECTION('center_axis',(0.,1.,3.96508223080413E-16));
#108100=DIRECTION('ref_axis',(-0.0664533356011988,-3.95631755140045E-16,
0.997789534013799));
#108101=DIRECTION('',(0.,1.,3.96508223080413E-16));
#108102=DIRECTION('center_axis',(0.,1.,2.22044604925031E-16));
#108103=DIRECTION('ref_axis',(-0.0664533356011988,-3.95631755140045E-16,
0.997789534013799));
#108104=DIRECTION('',(0.,-1.,-3.96508223080413E-16));
#108105=DIRECTION('center_axis',(0.,1.,3.96508223080413E-16));
#108106=DIRECTION('ref_axis',(0.0664533356011965,3.95631755140045E-16,-0.997789534013799));
#108107=DIRECTION('',(0.,1.,3.96508223080413E-16));
#108108=DIRECTION('center_axis',(0.,-1.,-2.22044604925031E-16));
#108109=DIRECTION('ref_axis',(0.0664533356011965,3.95631755140045E-16,-0.997789534013799));
#108110=DIRECTION('center_axis',(0.,-1.,-2.22044604925031E-16));
#108111=DIRECTION('ref_axis',(0.707106781186561,1.57009245868375E-16,-0.707106781186534));
#108112=DIRECTION('',(0.,1.,0.));
#108113=DIRECTION('',(0.,-1.,-2.22044604925031E-16));
#108114=DIRECTION('center_axis',(0.,1.,2.22044604925031E-16));
#108115=DIRECTION('ref_axis',(0.707106781186561,1.57009245868375E-16,-0.707106781186534));
#108116=DIRECTION('center_axis',(0.,-1.,0.));
#108117=DIRECTION('ref_axis',(0.0271346786627019,0.,-0.999631786816462));
#108118=DIRECTION('',(0.,-1.,0.));
#108119=DIRECTION('center_axis',(-0.0271346786627023,-2.01784404703786E-16,
0.999631786816462));
#108120=DIRECTION('ref_axis',(0.999631786816462,6.13206694458201E-17,0.0271346786627023));
#108121=DIRECTION('',(2.73791920107971E-48,1.,2.01858731750028E-16));
#108122=DIRECTION('center_axis',(-2.73791920107971E-48,-1.,-2.01858731750028E-16));
#108123=DIRECTION('ref_axis',(0.697447245796159,0.,0.716636127564995));
#108124=DIRECTION('',(-1.00813794530025E-51,-1.,-2.01858731750028E-16));
#108125=DIRECTION('center_axis',(1.,1.68028728913171E-32,-8.32407533012986E-17));
#108126=DIRECTION('ref_axis',(-8.32407533012986E-17,1.80520972702821E-16,
-1.));
#108127=DIRECTION('center_axis',(-6.93889390390721E-18,-1.,-2.22049474265475E-16));
#108128=DIRECTION('ref_axis',(1.,-6.93889390390721E-18,0.));
#108129=DIRECTION('center_axis',(0.,-1.,-2.22044604925031E-16));
#108130=DIRECTION('ref_axis',(0.229951641166733,-1.9644933285631E-16,0.973202056473745));
#108131=DIRECTION('center_axis',(0.,-1.,-2.22044604925031E-16));
#108132=DIRECTION('ref_axis',(0.89959196856447,-9.69738446503996E-17,0.436731370632224));
#108133=DIRECTION('center_axis',(0.,1.,1.6657509746814E-16));
#108134=DIRECTION('ref_axis',(1.,0.,1.15584692836443E-33));
#108135=DIRECTION('',(0.,1.,1.6657509746814E-16));
#108136=DIRECTION('',(0.,-1.,-1.6657509746814E-16));
#108137=DIRECTION('center_axis',(0.,-1.,-1.6657509746814E-16));
#108138=DIRECTION('ref_axis',(-0.591607978303977,0.,-0.806225774834246));
#108139=DIRECTION('',(-5.10447367644408E-16,-1.,-1.6657509747193E-16));
#108140=DIRECTION('center_axis',(1.,-5.10447367645645E-16,7.42407262755995E-12));
#108141=DIRECTION('ref_axis',(-7.42407262755995E-12,-1.64826352645555E-16,
1.));
#108142=DIRECTION('',(5.1044736764375E-16,1.,2.55223683821875E-16));
#108143=DIRECTION('center_axis',(-5.1044736764375E-16,-1.,-2.55223683821875E-16));
#108144=DIRECTION('ref_axis',(-0.923879532512709,3.75530232012858E-16,0.382683432361657));
#108145=DIRECTION('',(-5.1044736764375E-16,-1.,-2.55223683821875E-16));
#108146=DIRECTION('center_axis',(0.707106781186548,-1.8047039754986E-16,
-0.707106781186547));
#108147=DIRECTION('ref_axis',(0.707106781186547,-2.82505968889577E-16,0.707106781186548));
#108148=DIRECTION('',(5.1044736764375E-16,1.,2.55223683821875E-16));
#108149=DIRECTION('center_axis',(-5.1044736764375E-16,-1.,-2.55223683821875E-16));
#108150=DIRECTION('ref_axis',(0.923879532510927,-3.75530232012134E-16,-0.382683432365958));
#108151=DIRECTION('center_axis',(0.,1.,0.));
#108152=DIRECTION('ref_axis',(0.906884704407261,0.,0.421378847252866));
#108153=DIRECTION('',(0.,-1.,0.));
#108154=DIRECTION('',(0.,1.,0.));
#108155=DIRECTION('center_axis',(0.,1.,0.));
#108156=DIRECTION('ref_axis',(0.414254853160806,0.,0.910160928975046));
#108157=DIRECTION('',(0.,1.,0.));
#108158=DIRECTION('center_axis',(0.,1.,2.22044604925031E-16));
#108159=DIRECTION('ref_axis',(0.641559662047602,0.,-0.767073138646744));
#108160=DIRECTION('center_axis',(0.,1.,0.));
#108161=DIRECTION('ref_axis',(0.371940837143492,0.,0.928256437448725));
#108162=DIRECTION('',(0.,-1.,0.));
#108163=DIRECTION('center_axis',(0.,1.,0.));
#108164=DIRECTION('ref_axis',(1.,0.,-1.83750175990302E-19));
#108165=DIRECTION('center_axis',(1.,8.3944909223599E-32,-4.61226199516842E-16));
#108166=DIRECTION('ref_axis',(-4.61226199516842E-16,2.22049474265475E-16,
-1.));
#108167=DIRECTION('',(0.,-1.,-2.22044604925031E-16));
#108168=DIRECTION('center_axis',(0.,-1.,-2.22044604925031E-16));
#108169=DIRECTION('ref_axis',(0.89959196856447,-9.69738446503996E-17,0.436731370632224));
#108170=DIRECTION('center_axis',(0.,1.,2.22044604925031E-16));
#108171=DIRECTION('ref_axis',(0.89959196856447,-9.69738446503996E-17,0.436731370632224));
#108172=DIRECTION('center_axis',(1.,2.64363574135728E-32,-1.190587693968E-16));
#108173=DIRECTION('ref_axis',(1.190587693968E-16,-2.22044604925031E-16,
1.));
#108174=DIRECTION('',(0.,-1.,-2.22044604925031E-16));
#108175=DIRECTION('center_axis',(1.,2.64363574135728E-32,-1.190587693968E-16));
#108176=DIRECTION('ref_axis',(1.190587693968E-16,-2.22044604925031E-16,
1.));
#108177=DIRECTION('',(0.,1.,2.22044604925031E-16));
#108178=DIRECTION('',(1.190587693968E-16,-2.22044604925031E-16,1.));
#108179=DIRECTION('',(0.,1.,2.22044604925031E-16));
#108180=DIRECTION('center_axis',(0.,-1.,-2.22044604925031E-16));
#108181=DIRECTION('ref_axis',(-0.939690906904483,-7.59447731678524E-17,
0.342024852139477));
#108182=DIRECTION('center_axis',(1.35739377892777E-16,-1.,-3.84762012452445E-17));
#108183=DIRECTION('ref_axis',(1.,1.35739377892777E-16,6.93889390390723E-17));
#108184=DIRECTION('center_axis',(4.16333634234434E-17,-1.,-2.28983498828938E-16));
#108185=DIRECTION('ref_axis',(1.,4.16333634234434E-17,6.93889390390723E-17));
#108186=DIRECTION('center_axis',(1.35739377892777E-16,-1.,-3.84762012452445E-17));
#108187=DIRECTION('ref_axis',(-0.997493114923262,0.,-0.0707635900777229));
#108188=DIRECTION('center_axis',(4.16333634234434E-17,-1.,-2.28983498828939E-16));
#108189=DIRECTION('ref_axis',(0.753363330133441,0.,0.657604510941228));
#108190=DIRECTION('',(0.000408627363453739,2.29000492243054E-16,-0.999999916511835));
#108191=DIRECTION('center_axis',(0.,-1.,-2.67523620391604E-16));
#108192=DIRECTION('ref_axis',(0.753363330133441,0.,0.657604510941228));
#108193=DIRECTION('',(0.,-1.,-2.67523620391604E-16));
#108194=DIRECTION('center_axis',(0.,1.,1.6657509746814E-16));
#108195=DIRECTION('ref_axis',(-0.997493114923262,0.,-0.0707635900777229));
#108196=DIRECTION('center_axis',(0.,1.,2.22044604925031E-16));
#108197=DIRECTION('ref_axis',(0.226765259529559,0.,-0.973949442769229));
#108198=DIRECTION('center_axis',(0.,-1.,-2.22044604925031E-16));
#108199=DIRECTION('ref_axis',(-1.,0.,0.));
#108200=DIRECTION('center_axis',(0.,-1.,-2.22044604925031E-16));
#108201=DIRECTION('ref_axis',(-1.,0.,0.));
#108202=DIRECTION('center_axis',(0.,1.,0.));
#108203=DIRECTION('ref_axis',(0.442887523223796,0.,0.896577181157703));
#108204=DIRECTION('',(0.,1.,0.));
#108205=DIRECTION('center_axis',(4.16333634234434E-17,-1.,-2.28983498828938E-16));
#108206=DIRECTION('ref_axis',(0.442887523223796,-1.86862482701593E-16,0.896577181157703));
#108207=DIRECTION('',(0.,1.,0.));
#108208=DIRECTION('center_axis',(0.,1.,0.));
#108209=DIRECTION('ref_axis',(-0.442887523223796,0.,-0.896577181157702));
#108210=DIRECTION('center_axis',(-1.35739377892777E-16,1.,3.84762012452444E-17));
#108211=DIRECTION('ref_axis',(-0.442887523223796,-2.56203928247531E-17,
-0.896577181157702));
#108212=DIRECTION('center_axis',(4.16333634234434E-17,-1.,-2.28983498828938E-16));
#108213=DIRECTION('ref_axis',(1.,4.16333634234434E-17,6.93889390390723E-17));
#108214=DIRECTION('center_axis',(4.16333634234434E-17,-1.,-2.28983498828938E-16));
#108215=DIRECTION('ref_axis',(0.468176250029908,0.,-0.883635105067659));
#108216=DIRECTION('center_axis',(0.,-1.,-1.6657509746814E-16));
#108217=DIRECTION('ref_axis',(0.468176250029908,0.,-0.883635105067659));
#108218=DIRECTION('center_axis',(0.,-1.,-2.22044604925031E-16));
#108219=DIRECTION('ref_axis',(0.0595262816618969,-2.21650861813111E-16,
0.998226738667878));
#108220=DIRECTION('center_axis',(0.,-1.,-2.22044604925031E-16));
#108221=DIRECTION('ref_axis',(0.0595262816618969,-2.21650861813111E-16,
0.998226738667878));
#108222=DIRECTION('',(0.,1.,2.22044604925031E-16));
#108223=DIRECTION('center_axis',(0.,-1.,-2.22044604925031E-16));
#108224=DIRECTION('ref_axis',(-0.157390971609958,2.19277123123827E-16,-0.98753636999134));
#108225=DIRECTION('center_axis',(0.,1.,2.22044604925031E-16));
#108226=DIRECTION('ref_axis',(-0.157390971609958,2.19277123123827E-16,-0.98753636999134));
#108227=DIRECTION('center_axis',(1.,-4.12194440118864E-49,1.54077774334651E-33));
#108228=DIRECTION('ref_axis',(1.54077774334651E-33,2.22049474265475E-16,
-1.));
#108229=DIRECTION('',(0.,1.,2.67523620391604E-16));
#108230=DIRECTION('',(1.54077774334651E-33,2.22044604925031E-16,-1.));
#108231=DIRECTION('',(0.,-1.,-2.67523620391604E-16));
#108232=DIRECTION('center_axis',(0.,-1.,-2.67523620391604E-16));
#108233=DIRECTION('ref_axis',(0.482689240114392,0.,-0.875791697538742));
#108234=DIRECTION('',(0.,-1.,-2.67523620391604E-16));
#108235=DIRECTION('center_axis',(0.,-1.,-2.22044604925031E-16));
#108236=DIRECTION('ref_axis',(0.482689240114392,0.,-0.875791697538742));
#108237=DIRECTION('center_axis',(0.,1.,2.67523620391604E-16));
#108238=DIRECTION('ref_axis',(1.,0.,1.85631801868649E-33));
#108239=DIRECTION('center_axis',(0.,-1.,-2.22044604925031E-16));
#108240=DIRECTION('ref_axis',(1.,0.,1.85631801868649E-33));
#108241=DIRECTION('center_axis',(0.,1.,2.67523620391604E-16));
#108242=DIRECTION('ref_axis',(0.0662762646370231,0.,0.997801311256787));
#108243=DIRECTION('',(0.,-1.,-2.67523620391604E-16));
#108244=DIRECTION('',(0.,1.,2.67523620391604E-16));
#108245=DIRECTION('center_axis',(0.,1.,2.67523620391604E-16));
#108246=DIRECTION('ref_axis',(-1.,0.,-1.85631801868649E-33));
#108247=DIRECTION('',(0.,1.,2.67523620391604E-16));
#108248=DIRECTION('center_axis',(0.,1.,2.67523620391604E-16));
#108249=DIRECTION('ref_axis',(1.,1.85370757147271E-31,-6.93889390390722E-16));
#108250=DIRECTION('center_axis',(0.999999916511834,-1.09317472416637E-19,
0.000408627366273739));
#108251=DIRECTION('ref_axis',(0.000408627366273739,2.22046620305031E-16,
-0.999999916511834));
#108252=DIRECTION('',(0.,1.,2.67523620391604E-16));
#108253=DIRECTION('',(0.,1.,0.));
#108254=DIRECTION('center_axis',(0.,-1.,-2.67523620391604E-16));
#108255=DIRECTION('ref_axis',(0.707251238022098,0.,-0.706962294833472));
#108256=DIRECTION('',(0.,-1.,-2.67523620391604E-16));
#108257=DIRECTION('center_axis',(1.30472918803582E-12,2.67523620391604E-16,
-1.));
#108258=DIRECTION('ref_axis',(-1.,6.93889390419694E-18,-1.30472918803582E-12));
#108259=DIRECTION('',(-1.31710484347345E-28,1.,2.67523620391604E-16));
#108260=DIRECTION('center_axis',(0.,-1.,-1.6657509746814E-16));
#108261=DIRECTION('ref_axis',(-0.827170191871368,0.,-0.561951486944811));
#108262=DIRECTION('',(0.,-1.,-1.6657509746814E-16));
#108263=DIRECTION('center_axis',(0.,1.,1.6657509746814E-16));
#108264=DIRECTION('ref_axis',(1.,0.,1.15584692836443E-33));
#108265=DIRECTION('center_axis',(0.,-1.,0.));
#108266=DIRECTION('ref_axis',(0.141735171603208,0.,-0.989904612137255));
#108267=DIRECTION('',(0.,-1.,0.));
#108268=DIRECTION('center_axis',(0.,1.,0.));
#108269=DIRECTION('ref_axis',(2.48741143748787E-16,0.,1.));
#108270=DIRECTION('',(0.,1.,0.));
#108271=DIRECTION('center_axis',(3.2590836004222E-16,0.,1.));
#108272=DIRECTION('ref_axis',(1.,-6.93889390390704E-18,-3.2590836004222E-16));
#108273=DIRECTION('',(1.19092552242972E-16,1.,-3.88132583947496E-32));
#108274=DIRECTION('center_axis',(1.19092552242972E-16,1.,-3.88132583947496E-32));
#108275=DIRECTION('ref_axis',(0.51349131065734,0.,0.858094793061586));
#108276=DIRECTION('center_axis',(0.,1.,2.67523620391604E-16));
#108277=DIRECTION('ref_axis',(0.707106781186547,0.,0.707106781186547));
#108278=DIRECTION('center_axis',(0.,-1.,-2.22044604925031E-16));
#108279=DIRECTION('ref_axis',(0.707106781186547,0.,0.707106781186547));
#108280=DIRECTION('center_axis',(0.,-1.,-2.22044604925031E-16));
#108281=DIRECTION('ref_axis',(-0.934114852736578,0.,0.356972606647795));
#108282=DIRECTION('center_axis',(0.,1.,2.67523620391604E-16));
#108283=DIRECTION('ref_axis',(-0.984274724761795,4.72565661779708E-17,-0.176644462678832));
#108284=DIRECTION('',(0.,-1.,-2.67523620391604E-16));
#108285=DIRECTION('center_axis',(0.,-1.,-2.67523620391604E-16));
#108286=DIRECTION('ref_axis',(-0.753900508899602,0.,0.656988601636985));
#108287=DIRECTION('center_axis',(0.,1.,0.));
#108288=DIRECTION('ref_axis',(-0.000408627364868437,0.,0.999999916511835));
#108289=DIRECTION('center_axis',(0.,-1.,-2.22044604925031E-16));
#108290=DIRECTION('ref_axis',(-1.,0.,0.));
#108291=DIRECTION('center_axis',(0.,-1.,-2.22044604925031E-16));
#108292=DIRECTION('ref_axis',(-0.512525209353282,0.,0.858672178294705));
#108293=DIRECTION('',(-1.85435565520038E-14,-2.22044604925031E-16,1.));
#108294=DIRECTION('',(-0.707106781186548,-1.57009245868378E-16,0.707106781186548));
#108295=DIRECTION('center_axis',(0.,-1.,-2.22044604925031E-16));
#108296=DIRECTION('ref_axis',(-0.923879532511287,0.,-0.38268343236509));
#108297=DIRECTION('',(0.,-2.22044604925031E-16,1.));
#108298=DIRECTION('center_axis',(0.,1.,2.22044604925031E-16));
#108299=DIRECTION('ref_axis',(0.707106781186548,-1.57009245868377E-16,0.707106781186548));
#108300=DIRECTION('',(-1.,-2.58135112964991E-32,1.16253719856037E-16));
#108301=DIRECTION('center_axis',(0.,1.,2.22044604925031E-16));
#108302=DIRECTION('ref_axis',(-0.891123735454889,-1.00755045690416E-16,
0.453760386227053));
#108303=DIRECTION('center_axis',(0.,1.,2.22044604925031E-16));
#108304=DIRECTION('ref_axis',(-0.901335144845703,0.,-0.433122334526835));
#108305=DIRECTION('center_axis',(0.,-1.,-2.22044604925031E-16));
#108306=DIRECTION('ref_axis',(-1.,0.,0.));
#108307=DIRECTION('center_axis',(0.,-1.,-2.22044604925031E-16));
#108308=DIRECTION('ref_axis',(-1.,0.,0.));
#108309=DIRECTION('center_axis',(0.,1.,2.22044604925031E-16));
#108310=DIRECTION('ref_axis',(-0.785534661760763,1.24913747843662E-16,-0.618817659066387));
#108311=DIRECTION('center_axis',(0.,1.,2.22044604925031E-16));
#108312=DIRECTION('ref_axis',(-1.,0.,0.));
#108313=DIRECTION('',(0.308815713730941,-0.707106781186547,-0.636107581272893));
#108314=DIRECTION('center_axis',(0.,1.,2.01858731750028E-16));
#108315=DIRECTION('ref_axis',(-0.785534661760763,1.24913747843662E-16,-0.618817659066387));
#108316=DIRECTION('center_axis',(0.,-1.,-2.22044604925031E-16));
#108317=DIRECTION('ref_axis',(-0.901335144845703,0.,-0.433122334526835));
#108318=DIRECTION('center_axis',(-1.837501759903E-19,3.96508223080413E-16,
-1.));
#108319=DIRECTION('ref_axis',(-1.,6.93889390390712E-18,1.83750175990302E-19));
#108320=DIRECTION('',(0.,1.,3.96508223080413E-16));
#108321=DIRECTION('center_axis',(0.,1.,3.96508223080413E-16));
#108322=DIRECTION('ref_axis',(1.,0.,-1.837501759903E-19));
#108323=DIRECTION('',(0.,-1.,-3.96508223080413E-16));
#108324=DIRECTION('center_axis',(-1.,0.,0.));
#108325=DIRECTION('ref_axis',(0.,-2.22044604925031E-16,1.));
#108326=DIRECTION('center_axis',(-1.98445518114089E-16,-1.,-4.37374863265516E-16));
#108327=DIRECTION('ref_axis',(-0.512525209353282,0.,0.858672178294705));
#108328=DIRECTION('center_axis',(0.,-1.,-2.22044604925031E-16));
#108329=DIRECTION('ref_axis',(-1.,0.,0.));
#108330=DIRECTION('center_axis',(3.42121385298657E-49,-1.,-2.22044604925031E-16));
#108331=DIRECTION('ref_axis',(-1.,0.,-1.54077774334651E-33));
#108332=DIRECTION('center_axis',(3.42121385298657E-49,-1.,-2.22044604925031E-16));
#108333=DIRECTION('ref_axis',(-1.,0.,-1.54077774334651E-33));
#108334=DIRECTION('center_axis',(0.,1.,2.22044604925031E-16));
#108335=DIRECTION('ref_axis',(-1.,0.,0.));
#108336=DIRECTION('center_axis',(0.,-1.,-2.22044604925031E-16));
#108337=DIRECTION('ref_axis',(-1.,0.,0.));
#108338=DIRECTION('',(0.,1.,2.22044604925031E-16));
#108339=DIRECTION('center_axis',(0.,-1.,-2.22044604925031E-16));
#108340=DIRECTION('ref_axis',(1.,0.,0.));
#108341=DIRECTION('center_axis',(0.,1.,2.22044604925031E-16));
#108342=DIRECTION('ref_axis',(-1.,0.,0.));
#108343=DIRECTION('center_axis',(0.,-1.,-2.22044604925031E-16));
#108344=DIRECTION('ref_axis',(1.,0.,0.));
#108345=DIRECTION('',(0.,1.,2.22044604925031E-16));
#108346=DIRECTION('center_axis',(0.,1.,2.22044604925031E-16));
#108347=DIRECTION('ref_axis',(0.707106781186547,-1.57009245868377E-16,0.707106781186547));
#108348=DIRECTION('',(0.,1.,2.22044604925031E-16));
#108349=DIRECTION('center_axis',(0.,-1.,-2.22044604925031E-16));
#108350=DIRECTION('ref_axis',(0.707106781186547,-1.57009245868377E-16,0.707106781186547));
#108351=DIRECTION('',(0.,1.,2.22044604925031E-16));
#108352=DIRECTION('center_axis',(0.707106781186548,-1.57009245868377E-16,
0.707106781186548));
#108353=DIRECTION('ref_axis',(0.707106781186548,1.57009245868377E-16,-0.707106781186548));
#108354=DIRECTION('',(0.,1.,2.22044604925031E-16));
#108355=DIRECTION('',(-0.707106781186548,-1.57009245868377E-16,0.707106781186548));
#108356=DIRECTION('center_axis',(0.,1.,2.22044604925031E-16));
#108357=DIRECTION('ref_axis',(-0.707106781186547,1.57009245868377E-16,-0.707106781186547));
#108358=DIRECTION('',(0.,-1.,-2.22044604925031E-16));
#108359=DIRECTION('center_axis',(0.,-1.,-2.22044604925031E-16));
#108360=DIRECTION('ref_axis',(-0.707106781186547,1.57009245868377E-16,-0.707106781186547));
#108361=DIRECTION('center_axis',(0.,1.,2.22044604925031E-16));
#108362=DIRECTION('ref_axis',(0.707106781186548,-1.57009245868377E-16,0.707106781186548));
#108363=DIRECTION('center_axis',(0.,-1.,-2.22044604925031E-16));
#108364=DIRECTION('ref_axis',(0.707106781186548,-1.57009245868377E-16,0.707106781186548));
#108365=DIRECTION('',(0.,1.,2.22044604925031E-16));
#108366=DIRECTION('',(0.,1.,2.22044604925031E-16));
#108367=DIRECTION('center_axis',(-0.707106781186548,1.57009245868377E-16,
-0.707106781186548));
#108368=DIRECTION('ref_axis',(-0.707106781186548,-1.57009245868377E-16,
0.707106781186548));
#108369=DIRECTION('',(0.707106781186548,1.57009245868377E-16,-0.707106781186548));
#108370=DIRECTION('',(0.,1.,2.22044604925031E-16));
#108371=DIRECTION('center_axis',(0.,1.,2.22044604925031E-16));
#108372=DIRECTION('ref_axis',(-0.707106781186548,1.57009245868377E-16,-0.707106781186548));
#108373=DIRECTION('center_axis',(0.,-1.,-2.22044604925031E-16));
#108374=DIRECTION('ref_axis',(-0.707106781186548,1.57009245868377E-16,-0.707106781186548));
#108375=DIRECTION('',(0.,1.,2.22044604925031E-16));
#108376=DIRECTION('center_axis',(0.707106781186548,-1.57009245868377E-16,
0.707106781186548));
#108377=DIRECTION('ref_axis',(0.707106781186548,1.57009245868377E-16,-0.707106781186548));
#108378=DIRECTION('',(-0.707106781186548,-1.57009245868377E-16,0.707106781186548));
#108379=DIRECTION('center_axis',(3.42121385298657E-49,-1.,-2.22044604925031E-16));
#108380=DIRECTION('ref_axis',(-1.,0.,-1.54077774334651E-33));
#108381=DIRECTION('center_axis',(-3.42121385298657E-49,1.,2.22044604925031E-16));
#108382=DIRECTION('ref_axis',(-1.,0.,-1.54077774334651E-33));
#108383=DIRECTION('center_axis',(0.,-1.,-2.22044604925031E-16));
#108384=DIRECTION('ref_axis',(1.,0.,0.));
#108385=DIRECTION('',(0.,1.,2.22044604925031E-16));
#108386=DIRECTION('center_axis',(0.,1.,2.22044604925031E-16));
#108387=DIRECTION('ref_axis',(-1.,0.,0.));
#108388=DIRECTION('center_axis',(0.,1.,2.22044604925031E-16));
#108389=DIRECTION('ref_axis',(-1.,0.,0.));
#108390=DIRECTION('',(0.,1.,2.22044604925031E-16));
#108391=DIRECTION('center_axis',(0.,1.,2.22044604925031E-16));
#108392=DIRECTION('ref_axis',(0.360742674985292,2.07093317185659E-16,-0.932665386108253));
#108393=DIRECTION('center_axis',(0.,1.,2.22044604925031E-16));
#108394=DIRECTION('ref_axis',(0.360742674985292,2.07093317185659E-16,-0.932665386108253));
#108395=DIRECTION('',(0.,-1.,-2.22044604925031E-16));
#108396=DIRECTION('center_axis',(1.01862664414594E-31,1.,2.22044604925031E-16));
#108397=DIRECTION('ref_axis',(-0.370112462344042,0.,-0.928986956430299));
#108398=DIRECTION('center_axis',(0.,1.,2.22044604925031E-16));
#108399=DIRECTION('ref_axis',(-0.370112462344042,0.,-0.928986956430299));
#108400=DIRECTION('',(-1.01862664414594E-31,-1.,-2.22044604925031E-16));
#108401=DIRECTION('',(1.02531585888742E-31,1.,2.22044604925031E-16));
#108402=DIRECTION('center_axis',(0.0271346786627024,2.21962845174164E-16,
-0.999631786816462));
#108403=DIRECTION('ref_axis',(0.999631786816462,-6.02510900342743E-18,0.0271346786627024));
#108404=DIRECTION('',(0.,-1.,-2.22044604925031E-16));
#108405=DIRECTION('',(0.999631786816462,-6.02510900342743E-18,0.0271346786627024));
#108406=DIRECTION('center_axis',(0.,-1.,-2.22044604925031E-16));
#108407=DIRECTION('ref_axis',(-0.993670662656293,-2.49428489271903E-17,
0.112332605134053));
#108408=DIRECTION('center_axis',(0.,1.,2.22044604925031E-16));
#108409=DIRECTION('ref_axis',(-0.993670662656293,-2.49428489271903E-17,
0.112332605134053));
#108410=DIRECTION('center_axis',(0.,-1.,-2.22044604925031E-16));
#108411=DIRECTION('ref_axis',(0.707106781186548,1.57009245868377E-16,-0.707106781186548));
#108412=DIRECTION('center_axis',(0.,-1.,-2.22044604925031E-16));
#108413=DIRECTION('ref_axis',(0.69744724579616,-1.59125185820173E-16,0.716636127564994));
#108414=DIRECTION('center_axis',(0.,-1.,-2.22044604925031E-16));
#108415=DIRECTION('ref_axis',(0.69744724579616,-1.59125185820173E-16,0.716636127564994));
#108416=DIRECTION('center_axis',(0.,-1.,-2.22044604925031E-16));
#108417=DIRECTION('ref_axis',(-1.,0.,0.));
#108418=DIRECTION('center_axis',(0.,1.,2.22044604925031E-16));
#108419=DIRECTION('ref_axis',(-0.923879532511287,0.,-0.38268343236509));
#108420=DIRECTION('',(0.707106781186548,1.57009245868377E-16,-0.707106781186548));
#108421=DIRECTION('',(-1.,-2.58135112964991E-32,1.16253719856037E-16));
#108422=DIRECTION('center_axis',(0.,-1.,-2.22044604925031E-16));
#108423=DIRECTION('ref_axis',(0.707106781186548,-1.57009245868377E-16,0.707106781186548));
#108424=DIRECTION('',(0.,2.22044604925031E-16,-1.));
#108425=DIRECTION('center_axis',(0.,1.,2.22044604925031E-16));
#108426=DIRECTION('ref_axis',(0.89959196856447,-9.69738446503996E-17,0.436731370632224));
#108427=DIRECTION('center_axis',(0.,-1.,-2.22044604925031E-16));
#108428=DIRECTION('ref_axis',(1.,0.,0.));
#108429=DIRECTION('',(0.,1.,2.22044604925031E-16));
#108430=DIRECTION('center_axis',(0.,1.,2.22044604925031E-16));
#108431=DIRECTION('ref_axis',(-1.,0.,0.));
#108432=DIRECTION('',(0.,1.,2.22044604925031E-16));
#108433=DIRECTION('center_axis',(0.,-1.,-2.22044604925031E-16));
#108434=DIRECTION('ref_axis',(-1.,0.,0.));
#108435=DIRECTION('',(-0.707106781186547,0.707106781186547,7.04136402448281E-17));
#108436=DIRECTION('center_axis',(0.,-1.,-2.22044604925031E-16));
#108437=DIRECTION('ref_axis',(-0.891123735454889,-1.00755045690416E-16,
0.453760386227053));
#108438=DIRECTION('',(0.,1.,2.22044604925031E-16));
#108439=DIRECTION('center_axis',(1.16253719856037E-16,-2.22044604925031E-16,
1.));
#108440=DIRECTION('ref_axis',(-1.,-2.58135112964991E-32,1.16253719856037E-16));
#108441=DIRECTION('',(0.,-1.,-2.22044604925031E-16));
#108442=DIRECTION('center_axis',(0.,1.,2.22044604925031E-16));
#108443=DIRECTION('ref_axis',(0.707106781186548,-1.57009245868377E-16,0.707106781186548));
#108444=DIRECTION('',(0.,1.,2.22044604925031E-16));
#108445=DIRECTION('center_axis',(-1.,0.,0.));
#108446=DIRECTION('ref_axis',(0.,2.22044604925031E-16,-1.));
#108447=DIRECTION('',(0.,-1.,-2.22044604925031E-16));
#108448=DIRECTION('center_axis',(0.,-1.,-2.22044604925031E-16));
#108449=DIRECTION('ref_axis',(-0.923879532511287,0.,-0.38268343236509));
#108450=DIRECTION('',(1.74315279842105E-32,1.,2.22044604925031E-16));
#108451=DIRECTION('center_axis',(-0.707106781186548,1.57009245868378E-16,
-0.707106781186548));
#108452=DIRECTION('ref_axis',(0.707106781186548,1.57009245868378E-16,-0.707106781186548));
#108453=DIRECTION('',(-1.98173529318078E-45,1.,2.22044604925031E-16));
#108454=DIRECTION('center_axis',(-1.,4.11749668849466E-30,-1.85435565520038E-14));
#108455=DIRECTION('ref_axis',(1.85435565520038E-14,2.22044604925031E-16,
-1.));
#108456=DIRECTION('center_axis',(-1.11022302462516E-16,2.22044604925031E-16,
-1.));
#108457=DIRECTION('ref_axis',(-1.,-1.83750175990327E-19,1.11022302462516E-16));
#108458=DIRECTION('',(1.11022302462516E-16,-2.22044604925031E-16,1.));
#108459=DIRECTION('center_axis',(-1.,0.,-6.93889390390723E-17));
#108460=DIRECTION('ref_axis',(-6.93889390390723E-17,-6.93889390390724E-18,
1.));
#108461=DIRECTION('',(0.,-1.,0.));
#108462=DIRECTION('',(0.,1.,0.));
#108463=DIRECTION('',(6.93889390390723E-17,2.22049474265475E-16,-1.));
#108464=DIRECTION('center_axis',(6.93889390390722E-18,1.,2.22049474265475E-16));
#108465=DIRECTION('ref_axis',(-1.,6.93889390390721E-18,1.83750175990302E-19));
#108466=DIRECTION('center_axis',(-4.16333634234434E-17,1.,2.28983498828938E-16));
#108467=DIRECTION('ref_axis',(0.529831364669109,-1.72142934113367E-16,0.848103015566428));
#108468=DIRECTION('center_axis',(6.93889390390719E-18,1.,2.22049474265475E-16));
#108469=DIRECTION('ref_axis',(-0.805424049353576,1.37197252647342E-16,-0.59269899672843));
#108470=DIRECTION('center_axis',(0.,-1.,0.));
#108471=DIRECTION('ref_axis',(-0.805424049353576,0.,-0.59269899672843));
#108472=DIRECTION('',(0.,1.,0.));
#108473=DIRECTION('center_axis',(0.,-1.,0.));
#108474=DIRECTION('ref_axis',(0.456803537809492,0.,0.889567607236646));
#108475=DIRECTION('center_axis',(0.,1.,2.69144975666705E-16));
#108476=DIRECTION('ref_axis',(0.556470257418726,0.,-0.830867530120378));
#108477=DIRECTION('center_axis',(1.83750175990295E-19,-1.,-2.35922392732845E-16));
#108478=DIRECTION('ref_axis',(0.556470257418726,0.,-0.830867530120378));
#108479=DIRECTION('',(2.6329399793482E-17,-1.,-2.95474375460248E-16));
#108480=DIRECTION('center_axis',(0.,-1.,-2.22044604925031E-16));
#108481=DIRECTION('ref_axis',(0.556470257418726,0.,-0.830867530120378));
#108482=DIRECTION('',(0.,1.,2.69144975666705E-16));
#108483=DIRECTION('center_axis',(-1.83750175990295E-19,1.,2.35922392732845E-16));
#108484=DIRECTION('ref_axis',(1.,1.83750175990295E-19,4.08007322284045E-35));
#108485=DIRECTION('center_axis',(-1.83750175990295E-19,1.,2.35922392732845E-16));
#108486=DIRECTION('ref_axis',(-1.,0.,-1.86756843092096E-33));
#108487=DIRECTION('center_axis',(1.83750175990295E-19,-1.,-2.35922392732845E-16));
#108488=DIRECTION('ref_axis',(0.830867530119088,0.,-0.556470257420652));
#108489=DIRECTION('',(-0.707106781187368,1.6669239273947E-16,-0.707106781185727));
#108490=DIRECTION('center_axis',(1.83750175990295E-19,-1.,-2.35922392732845E-16));
#108491=DIRECTION('ref_axis',(-0.923879532510705,0.,0.382683432366495));
#108492=DIRECTION('',(-1.88260317010131E-12,2.35922392732845E-16,-1.));
#108493=DIRECTION('center_axis',(-1.83750175990295E-19,1.,2.35922392732845E-16));
#108494=DIRECTION('ref_axis',(0.877755401836952,0.,-0.479109021566127));
#108495=DIRECTION('center_axis',(1.83750175990295E-19,-1.,-2.35922392732845E-16));
#108496=DIRECTION('ref_axis',(-0.674528301887451,-1.98696006215612E-16,
0.738248989130924));
#108497=DIRECTION('center_axis',(-1.83750175990295E-19,1.,2.35922392732845E-16));
#108498=DIRECTION('ref_axis',(-0.439524536496337,0.,-0.898230583880153));
#108499=DIRECTION('',(-1.88249434430459E-12,2.35922392732845E-16,-1.));
#108500=DIRECTION('center_axis',(-1.83750175990295E-19,1.,2.35922392732845E-16));
#108501=DIRECTION('ref_axis',(-0.923879532510705,0.,0.382683432366494));
#108502=DIRECTION('',(-0.707106781187368,1.6669239273947E-16,-0.707106781185727));
#108503=DIRECTION('center_axis',(-1.83750175990295E-19,1.,2.35922392732845E-16));
#108504=DIRECTION('ref_axis',(-0.382683432364554,0.,0.923879532511509));
#108505=DIRECTION('',(1.,1.83750175990323E-19,-1.16253719856037E-16));
#108506=DIRECTION('center_axis',(-1.83750175990295E-19,1.,2.35922392732845E-16));
#108507=DIRECTION('ref_axis',(2.55004895630733E-36,-2.22044604925031E-16,
1.));
#108508=DIRECTION('',(-0.868387762761633,1.16830990166913E-16,-0.495885766569122));
#108509=DIRECTION('center_axis',(-1.83750175990295E-19,1.,2.35922392732845E-16));
#108510=DIRECTION('ref_axis',(0.157787733663648,2.19263064006667E-16,-0.987473053356541));
#108511=DIRECTION('',(1.,1.83750175990065E-19,9.76990079422698E-16));
#108512=DIRECTION('center_axis',(1.83750175990295E-19,-1.,-2.35922392732845E-16));
#108513=DIRECTION('ref_axis',(-0.382683432364555,0.,0.923879532511508));
#108514=DIRECTION('',(-0.707106781187368,1.6669239273947E-16,-0.707106781185727));
#108515=DIRECTION('center_axis',(0.,1.,2.69144975666705E-16));
#108516=DIRECTION('ref_axis',(-1.,0.,-1.86756843092096E-33));
#108517=DIRECTION('center_axis',(0.,1.,2.22044604925031E-16));
#108518=DIRECTION('ref_axis',(-1.,0.,-1.86756843092096E-33));
#108519=DIRECTION('',(0.,-1.,-2.69144975666705E-16));
#108520=DIRECTION('center_axis',(0.,-1.,-2.69144975666705E-16));
#108521=DIRECTION('ref_axis',(0.830867530119088,0.,-0.556470257420652));
#108522=DIRECTION('center_axis',(0.,-1.,-2.22044604925031E-16));
#108523=DIRECTION('ref_axis',(0.830867530119088,0.,-0.556470257420652));
#108524=DIRECTION('',(-2.6329399793482E-17,1.,2.95474375460248E-16));
#108525=DIRECTION('center_axis',(0.707106781185727,2.27549631693565E-16,
-0.707106781187368));
#108526=DIRECTION('ref_axis',(-0.707106781187368,1.61919227945235E-16,-0.707106781185727));
#108527=DIRECTION('',(0.707106781187368,-1.57009245868195E-16,0.707106781185727));
#108528=DIRECTION('',(0.,1.,0.));
#108529=DIRECTION('',(0.707106781187368,-1.61919227945235E-16,0.707106781185727));
#108530=DIRECTION('',(3.48630559683805E-32,-1.,-3.21803775253669E-16));
#108531=DIRECTION('center_axis',(6.93889390390724E-18,1.,2.22049474265475E-16));
#108532=DIRECTION('ref_axis',(0.,0.,1.));
#108533=DIRECTION('center_axis',(0.55526819475842,0.,-0.831671348484319));
#108534=DIRECTION('ref_axis',(0.831671348484319,0.,0.55526819475842));
#108535=DIRECTION('center_axis',(6.93889390390724E-18,1.,2.22049474265475E-16));
#108536=DIRECTION('ref_axis',(-0.953563413137572,7.34962729527946E-17,-0.301192325807655));
#108537=DIRECTION('center_axis',(-0.023198104831873,0.,0.999730887755405));
#108538=DIRECTION('ref_axis',(0.,-1.,0.));
#108539=DIRECTION('center_axis',(-6.93889390390724E-18,-1.,-2.22049474265475E-16));
#108540=DIRECTION('ref_axis',(-0.953563413137572,5.96894099260837E-17,-0.301192325807655));
#108541=DIRECTION('center_axis',(-0.707106781187369,0.,-0.707106781185726));
#108542=DIRECTION('ref_axis',(0.,-1.,0.));
#108543=DIRECTION('center_axis',(6.93889390390724E-18,1.,2.22049474265475E-16));
#108544=DIRECTION('ref_axis',(0.371940837143499,-1.7347234759768E-16,0.928256437448722));
#108545=DIRECTION('center_axis',(-6.93889390390724E-18,-1.,-2.22049474265475E-16));
#108546=DIRECTION('ref_axis',(0.371940837143499,-2.08699711926501E-16,0.928256437448722));
#108547=DIRECTION('center_axis',(-0.707106781187368,1.61919227945235E-16,
-0.707106781185727));
#108548=DIRECTION('ref_axis',(-0.499999999999422,-0.707106781186549,0.500000000000576));
#108549=DIRECTION('center_axis',(-0.707106781187366,0.,-0.707106781185729));
#108550=DIRECTION('ref_axis',(0.,-1.,0.));
#108551=DIRECTION('',(-0.707106781187368,1.61919227945235E-16,-0.707106781185727));
#108552=DIRECTION('center_axis',(-1.88182802673964E-12,0.,-1.));
#108553=DIRECTION('ref_axis',(0.,-1.,0.));
#108554=DIRECTION('center_axis',(6.93889390390724E-18,1.,2.22049474265475E-16));
#108555=DIRECTION('ref_axis',(-0.923879532510704,-8.67361737988403E-17,
0.382683432366496));
#108556=DIRECTION('center_axis',(-6.93889390390724E-18,-1.,-2.22049474265475E-16));
#108557=DIRECTION('ref_axis',(-0.923879532510704,-7.85639529110046E-17,
0.382683432366496));
#108558=DIRECTION('center_axis',(-1.88260317010131E-12,2.22049474265488E-16,
-1.));
#108559=DIRECTION('ref_axis',(-0.707106781186548,-0.707106781186548,1.3306533587345E-12));
#108560=DIRECTION('center_axis',(-1.88182802673964E-12,0.,-1.));
#108561=DIRECTION('ref_axis',(0.,-1.,0.));
#108562=DIRECTION('',(1.88260317010131E-12,-2.22049474265488E-16,1.));
#108563=DIRECTION('',(-1.88260317010131E-12,2.22049474265488E-16,-1.));
#108564=DIRECTION('center_axis',(0.909059342886221,0.,0.41666666666686));
#108565=DIRECTION('ref_axis',(0.,-1.,0.));
#108566=DIRECTION('center_axis',(6.93889390390724E-18,1.,2.22049474265475E-16));
#108567=DIRECTION('ref_axis',(-0.540061724868026,1.7347234759768E-16,-0.841625411529721));
#108568=DIRECTION('center_axis',(-6.93889390390724E-18,-1.,-2.22049474265475E-16));
#108569=DIRECTION('ref_axis',(-0.540061724868026,1.90629911169059E-16,-0.841625411529721));
#108570=DIRECTION('center_axis',(6.93889390390724E-18,1.,2.22049474265475E-16));
#108571=DIRECTION('ref_axis',(0.,-3.11641550771974E-16,1.));
#108572=DIRECTION('center_axis',(0.950100400237196,0.,0.311944273018627));
#108573=DIRECTION('ref_axis',(0.,-1.,0.));
#108574=DIRECTION('center_axis',(-6.93889390390724E-18,-1.,-2.22049474265475E-16));
#108575=DIRECTION('ref_axis',(-0.364882950347729,-2.09476042382105E-16,
0.931053399406036));
#108576=DIRECTION('center_axis',(6.93889390390724E-18,1.,2.22049474265475E-16));
#108577=DIRECTION('ref_axis',(-0.364882950347729,-2.04208033771386E-16,
0.931053399406036));
#108578=DIRECTION('center_axis',(6.93889390390724E-18,1.,2.22049474265475E-16));
#108579=DIRECTION('ref_axis',(0.945250138395208,1.15648231731787E-16,-0.326346711127658));
#108580=DIRECTION('center_axis',(-6.93889390390724E-18,-1.,-2.22049474265475E-16));
#108581=DIRECTION('ref_axis',(0.945250138395208,6.59061252111853E-17,-0.326346711127658));
#108582=DIRECTION('center_axis',(0.,-1.,-2.41352831440251E-16));
#108583=DIRECTION('ref_axis',(-0.540061724868023,0.,-0.841625411529723));
#108584=DIRECTION('',(0.,1.,2.41352831440251E-16));
#108585=DIRECTION('center_axis',(0.,1.,2.22044604925031E-16));
#108586=DIRECTION('ref_axis',(-0.540061724868023,0.,-0.841625411529723));
#108587=DIRECTION('',(1.51457201860782E-28,-1.,-2.41352831440251E-16));
#108588=DIRECTION('center_axis',(0.,-1.,-2.41352831440251E-16));
#108589=DIRECTION('ref_axis',(-1.,1.74423844019976E-32,-6.93889390390723E-17));
#108590=DIRECTION('',(0.,-1.,-2.41352831440251E-16));
#108591=DIRECTION('center_axis',(0.,1.,2.22044604925031E-16));
#108592=DIRECTION('ref_axis',(-1.,1.74423844019976E-32,-6.93889390390723E-17));
#108593=DIRECTION('center_axis',(0.,-1.,-1.60901887626834E-16));
#108594=DIRECTION('ref_axis',(0.945250138395209,0.,-0.326346711127656));
#108595=DIRECTION('',(0.,1.,1.60901887626834E-16));
#108596=DIRECTION('center_axis',(0.,1.,2.22044604925031E-16));
#108597=DIRECTION('ref_axis',(0.945250138395209,0.,-0.326346711127656));
#108598=DIRECTION('center_axis',(0.,-1.,-1.60901887626834E-16));
#108599=DIRECTION('ref_axis',(-1.,1.32537114452455E-32,-6.93889390390723E-17));
#108600=DIRECTION('',(0.,-1.,-1.60901887626834E-16));
#108601=DIRECTION('center_axis',(0.,1.,2.22044604925031E-16));
#108602=DIRECTION('ref_axis',(-1.,0.,0.));
#108603=DIRECTION('',(0.,1.,1.60901887626834E-16));
#108604=DIRECTION('center_axis',(0.,1.,2.22044604925031E-16));
#108605=DIRECTION('ref_axis',(-1.,0.,0.));
#108606=DIRECTION('center_axis',(6.93889390390724E-18,1.,2.22049474265475E-16));
#108607=DIRECTION('ref_axis',(-1.,6.93889390390724E-18,1.83750175990302E-19));
#108608=DIRECTION('center_axis',(0.,-1.,-2.22044604925031E-16));
#108609=DIRECTION('ref_axis',(0.,0.,-1.));
#108610=DIRECTION('center_axis',(0.,-1.,-2.22044604925031E-16));
#108611=DIRECTION('ref_axis',(-0.223884986531161,2.16408129595356E-16,-0.974615571805592));
#108612=DIRECTION('center_axis',(0.89959196856447,0.,0.436731370632225));
#108613=DIRECTION('ref_axis',(0.,-1.,0.));
#108614=DIRECTION('center_axis',(0.,1.,2.22044604925031E-16));
#108615=DIRECTION('ref_axis',(-0.223884986531161,2.08166817117217E-16,-0.974615571805592));
#108616=DIRECTION('center_axis',(0.,-1.,-2.22044604925031E-16));
#108617=DIRECTION('ref_axis',(0.,0.,-1.));
#108618=DIRECTION('center_axis',(0.,-1.,-2.22044604925031E-16));
#108619=DIRECTION('ref_axis',(-0.999460488335693,-7.29284625413709E-18,
0.0328440596726021));
#108620=DIRECTION('center_axis',(3.46944695195253E-16,3.46944695195361E-16,
-1.));
#108621=DIRECTION('ref_axis',(0.,-1.,-3.46944695195361E-16));
#108622=DIRECTION('center_axis',(0.,1.,2.22044604925031E-16));
#108623=DIRECTION('ref_axis',(-0.999460488335693,0.,0.0328440596726021));
#108624=DIRECTION('center_axis',(2.22628932034678E-16,2.22044604925031E-16,
-1.));
#108625=DIRECTION('ref_axis',(-0.707106781186549,-0.707106781186546,-4.90653893338678E-16));
#108626=DIRECTION('center_axis',(0.,0.,-1.));
#108627=DIRECTION('ref_axis',(0.,-1.,0.));
#108628=DIRECTION('',(-2.22628932034678E-16,-2.22044604925031E-16,1.));
#108629=DIRECTION('',(2.22628932034678E-16,2.22044604925031E-16,-1.));
#108630=DIRECTION('center_axis',(0.,-1.,-2.22044604925031E-16));
#108631=DIRECTION('ref_axis',(0.,0.,-1.));
#108632=DIRECTION('center_axis',(0.,1.,2.22044604925031E-16));
#108633=DIRECTION('ref_axis',(-0.999213555456797,0.,-0.0396518674388288));
#108634=DIRECTION('center_axis',(0.,-1.,-2.22044604925031E-16));
#108635=DIRECTION('ref_axis',(-0.999213555456797,8.80448323999446E-18,-0.0396518674388288));
#108636=DIRECTION('center_axis',(0.,-1.,-2.22044604925031E-16));
#108637=DIRECTION('ref_axis',(0.,2.04238085258919E-16,-1.));
#108638=DIRECTION('center_axis',(0.,-1.,-2.22044604925031E-16));
#108639=DIRECTION('ref_axis',(-0.229661543013825,-2.16109476147391E-16,
0.973270556248625));
#108640=DIRECTION('center_axis',(-0.899591968564469,0.,-0.436731370632226));
#108641=DIRECTION('ref_axis',(0.,-1.,0.));
#108642=DIRECTION('center_axis',(0.,1.,2.22044604925031E-16));
#108643=DIRECTION('ref_axis',(-0.229661543013825,-2.15407355546517E-16,
0.973270556248625));
#108644=DIRECTION('center_axis',(0.,-1.,-2.22044604925031E-16));
#108645=DIRECTION('ref_axis',(0.,0.,-1.));
#108646=DIRECTION('center_axis',(0.,1.,2.22044604925031E-16));
#108647=DIRECTION('ref_axis',(-0.627438795144384,-1.73472347597681E-16,
0.778665883641863));
#108648=DIRECTION('center_axis',(0.,-1.,-2.22044604925031E-16));
#108649=DIRECTION('ref_axis',(-0.627438795144384,-1.72898558501858E-16,
0.778665883641863));
#108650=DIRECTION('center_axis',(0.,1.,2.22044604925031E-16));
#108651=DIRECTION('ref_axis',(0.,-3.48477392031983E-16,1.));
#108652=DIRECTION('center_axis',(0.,-1.,-2.22044604925031E-16));
#108653=DIRECTION('ref_axis',(-0.234423796430946,-2.14187059826031E-16,
0.972134498753595));
#108654=DIRECTION('center_axis',(0.,1.,2.22044604925031E-16));
#108655=DIRECTION('ref_axis',(-0.234423796430946,-2.15857220709735E-16,
0.972134498753594));
#108656=DIRECTION('center_axis',(1.88212241265405E-12,-2.22044604925031E-16,
1.));
#108657=DIRECTION('ref_axis',(0.707106781186548,-0.707106781186548,-1.3306533587345E-12));
#108658=DIRECTION('',(-1.88212241265405E-12,2.22044604925031E-16,-1.));
#108659=DIRECTION('',(1.88212241265405E-12,-2.22044604925031E-16,1.));
#108660=DIRECTION('center_axis',(0.,-1.,-2.77555756156289E-16));
#108661=DIRECTION('ref_axis',(-1.,0.,0.));
#108662=DIRECTION('',(0.,-1.,-2.77555756156289E-16));
#108663=DIRECTION('center_axis',(0.,-1.,-2.22044604925031E-16));
#108664=DIRECTION('ref_axis',(-1.,0.,0.));
#108665=DIRECTION('',(0.,1.,2.77555756156289E-16));
#108666=DIRECTION('center_axis',(0.,-1.,-2.77555756156289E-16));
#108667=DIRECTION('ref_axis',(0.89959196856447,-1.21217305812999E-16,0.436731370632224));
#108668=DIRECTION('',(0.,1.,2.77555756156289E-16));
#108669=DIRECTION('center_axis',(0.,1.,2.22044604925031E-16));
#108670=DIRECTION('ref_axis',(0.89959196856447,-9.69738446503996E-17,0.436731370632224));
#108671=DIRECTION('center_axis',(-1.,-5.22393909422894E-28,1.88212241265405E-12));
#108672=DIRECTION('ref_axis',(1.88212241265405E-12,-2.22044604925031E-16,
1.));
#108673=DIRECTION('',(0.,-1.,-2.77555756156289E-16));
#108674=DIRECTION('',(1.88212241265405E-12,-2.22044604925031E-16,1.));
#108675=DIRECTION('center_axis',(0.,-1.,-2.77555756156289E-16));
#108676=DIRECTION('ref_axis',(0.89959196856447,-1.21217305812999E-16,0.436731370632224));
#108677=DIRECTION('',(0.,-1.,-2.77555756156289E-16));
#108678=DIRECTION('center_axis',(0.,-1.,-2.22044604925031E-16));
#108679=DIRECTION('ref_axis',(0.89959196856447,-9.69738446503996E-17,0.436731370632224));
#108680=DIRECTION('center_axis',(0.,1.,2.22044604925031E-16));
#108681=DIRECTION('ref_axis',(-1.,0.,0.));
#108682=DIRECTION('center_axis',(6.93889390390722E-18,1.,2.22049474265475E-16));
#108683=DIRECTION('ref_axis',(0.,-2.87669123789514E-16,1.));
#108684=DIRECTION('center_axis',(6.93889390390722E-18,1.,2.22049474265475E-16));
#108685=DIRECTION('ref_axis',(-0.540572225751839,-1.83058718699731E-16,
0.84129761009152));
#108686=DIRECTION('center_axis',(0.881309715225975,0.,0.472539083937308));
#108687=DIRECTION('ref_axis',(0.,-1.,0.));
#108688=DIRECTION('center_axis',(-6.93889390390722E-18,-1.,-2.22049474265475E-16));
#108689=DIRECTION('ref_axis',(-0.540572225751839,-1.80231010491097E-16,
0.84129761009152));
#108690=DIRECTION('center_axis',(-0.577747036373043,0.,0.816215879508703));
#108691=DIRECTION('ref_axis',(0.,-1.,0.));
#108692=DIRECTION('center_axis',(6.93889390390722E-18,1.,2.22049474265475E-16));
#108693=DIRECTION('ref_axis',(0.973362209071398,0.,-0.229272785021789));
#108694=DIRECTION('center_axis',(-6.93889390390722E-18,-1.,-2.22049474265475E-16));
#108695=DIRECTION('ref_axis',(0.973362209071398,4.41558442786504E-17,-0.229272785021789));
#108696=DIRECTION('center_axis',(6.93889390390722E-18,1.,2.22049474265475E-16));
#108697=DIRECTION('ref_axis',(0.,0.,1.));
#108698=DIRECTION('center_axis',(6.93889390390722E-18,1.,2.22049474265475E-16));
#108699=DIRECTION('ref_axis',(-0.98001004047213,-3.73761208507432E-17,0.198948034857887));
#108700=DIRECTION('center_axis',(-6.93889390390722E-18,-1.,-2.22049474265475E-16));
#108701=DIRECTION('ref_axis',(-0.98001004047213,-3.65204942310907E-17,0.198948034857887));
#108702=DIRECTION('center_axis',(6.93889390390722E-18,1.,2.22049474265475E-16));
#108703=DIRECTION('ref_axis',(-0.98001004047213,-3.73761208507432E-17,0.198948034857887));
#108704=DIRECTION('center_axis',(0.,-1.,0.));
#108705=DIRECTION('ref_axis',(-0.832437275985664,0.,0.55411928458552));
#108706=DIRECTION('',(0.,-1.,0.));
#108707=DIRECTION('',(4.44089209850063E-17,-1.,-2.66453525910038E-16));
#108708=DIRECTION('',(0.,-1.,0.));
#108709=DIRECTION('center_axis',(0.,1.,2.22044604925031E-16));
#108710=DIRECTION('ref_axis',(-0.832437275985664,0.,0.55411928458552));
#108711=DIRECTION('',(0.,1.,0.));
#108712=DIRECTION('',(0.,-1.,0.));
#108713=DIRECTION('center_axis',(0.,-1.,0.));
#108714=DIRECTION('ref_axis',(-0.472539083937309,0.,0.881309715225975));
#108715=DIRECTION('',(0.,1.,0.));
#108716=DIRECTION('center_axis',(0.,1.,2.22044604925031E-16));
#108717=DIRECTION('ref_axis',(-1.,0.,0.));
#108718=DIRECTION('',(0.,1.,2.22044604925031E-16));
#108719=DIRECTION('center_axis',(0.,1.,2.22044604925031E-16));
#108720=DIRECTION('ref_axis',(-1.,0.,0.));
#108721=DIRECTION('center_axis',(0.,1.,2.22044604925031E-16));
#108722=DIRECTION('ref_axis',(-1.,0.,0.));
#108723=DIRECTION('center_axis',(-1.88016196282748E-14,-2.22049474265475E-16,
1.));
#108724=DIRECTION('ref_axis',(0.707106781186548,-0.707106781186548,1.57009245868377E-14));
#108725=DIRECTION('',(-1.88016196282748E-14,-2.22049474265475E-16,1.));
#108726=DIRECTION('center_axis',(-1.66533453693773E-14,0.,1.));
#108727=DIRECTION('ref_axis',(0.,-1.,0.));
#108728=DIRECTION('',(1.88016196282748E-14,2.22049474265475E-16,-1.));
#108729=DIRECTION('center_axis',(6.93889390390722E-18,1.,2.22049474265475E-16));
#108730=DIRECTION('ref_axis',(-1.,6.93889390390721E-18,1.83750175990302E-19));
#108731=DIRECTION('',(0.,2.22049474265475E-16,-1.));
#108732=DIRECTION('',(-1.,6.93889390390743E-18,-9.76990079422698E-16));
#108733=DIRECTION('center_axis',(-6.93889390390722E-18,-1.,-2.22049474265475E-16));
#108734=DIRECTION('ref_axis',(0.70710678118654,-1.61919227945413E-16,0.707106781186555));
#108735=DIRECTION('center_axis',(1.,0.,0.));
#108736=DIRECTION('ref_axis',(0.,3.08148791101958E-33,-1.));
#108737=DIRECTION('center_axis',(1.,0.,0.));
#108738=DIRECTION('ref_axis',(1.9854940640545E-17,-2.52712137005744E-16,
1.));
#108739=DIRECTION('',(0.,1.,0.));
#108740=DIRECTION('',(2.22044604925031E-16,-2.22044604925031E-16,1.));
#108741=DIRECTION('',(0.,1.,2.77555756156289E-16));
#108742=DIRECTION('center_axis',(1.,0.,0.));
#108743=DIRECTION('ref_axis',(-4.90653893338679E-16,-0.707106781186548,
0.707106781186548));
#108744=DIRECTION('center_axis',(-1.,0.,-1.38777878078144E-15));
#108745=DIRECTION('ref_axis',(0.,-1.,0.));
#108746=DIRECTION('center_axis',(6.93889390390722E-18,1.,2.22049474265475E-16));
#108747=DIRECTION('ref_axis',(0.70710678118654,-1.15648231731787E-16,0.707106781186555));
#108748=DIRECTION('center_axis',(-1.,6.93889390390743E-18,-9.76990079422698E-16));
#108749=DIRECTION('ref_axis',(-4.90653893338679E-16,-0.707106781186548,
0.707106781186548));
#108750=DIRECTION('',(1.,-6.93889390390743E-18,9.76990079422698E-16));
#108751=DIRECTION('center_axis',(1.,-4.17479820231099E-30,1.88016196282748E-14));
#108752=DIRECTION('ref_axis',(1.88016196282748E-14,0.,-1.));
#108753=DIRECTION('',(1.04369955057775E-30,-1.,-2.77555756156289E-16));
#108754=DIRECTION('center_axis',(-1.,4.17479820231099E-30,-1.88016196282748E-14));
#108755=DIRECTION('ref_axis',(-1.26584900907556E-14,-0.898717034276078,
0.438529009647037));
#108756=DIRECTION('center_axis',(-1.,4.17479820231099E-30,-1.88016196282748E-14));
#108757=DIRECTION('ref_axis',(-1.85037170770859E-14,-2.22044604925031E-16,
1.));
#108758=DIRECTION('',(0.,1.,2.22044604925031E-16));
#108759=DIRECTION('center_axis',(1.,-4.17479820231099E-30,1.88016196282748E-14));
#108760=DIRECTION('ref_axis',(-1.85037170770859E-14,-2.22044604925031E-16,
1.));
#108761=DIRECTION('center_axis',(1.04369955057775E-30,-1.,-2.77555756156289E-16));
#108762=DIRECTION('ref_axis',(0.707106781186538,0.,0.707106781186557));
#108763=DIRECTION('',(-1.04369955057775E-30,1.,2.77555756156289E-16));
#108764=DIRECTION('center_axis',(-9.76990079422698E-16,-2.77555756156289E-16,
1.));
#108765=DIRECTION('ref_axis',(1.,-6.93889390390734E-18,9.76990079422698E-16));
#108766=DIRECTION('center_axis',(-1.26161707343768E-16,2.22044604925031E-16,
-1.));
#108767=DIRECTION('ref_axis',(-0.674310247716091,-0.738448163262029,-7.46314788228609E-17));
#108768=DIRECTION('',(2.53017617534078E-17,-1.,-2.77555756156289E-16));
#108769=DIRECTION('',(-1.,2.16935376201088E-31,-9.76990079422698E-16));
#108770=DIRECTION('',(1.27117486340087E-16,1.,2.77555756156289E-16));
#108771=DIRECTION('',(1.,-1.13108869885842E-30,5.02293560613052E-15));
#108772=DIRECTION('',(-8.41078048960409E-18,-1.,-2.77555756156289E-16));
#108773=DIRECTION('',(0.,1.,2.22044604925031E-16));
#108774=DIRECTION('',(-1.,4.69398999576592E-31,-2.11398515958123E-15));
#108775=DIRECTION('',(2.63976927864639E-32,1.,2.77555756156289E-16));
#108776=DIRECTION('',(1.,-2.7116922025136E-31,9.76990079422698E-16));
#108777=DIRECTION('',(1.,7.55993416755167E-31,9.76990079422697E-16));
#108778=DIRECTION('center_axis',(-0.323730285810082,2.12338308705133E-16,
-0.946149407889326));
#108779=DIRECTION('ref_axis',(-0.669028662334179,-0.707106781186547,0.228911880371771));
#108780=DIRECTION('',(-0.323730285810082,2.12338308705133E-16,-0.946149407889326));
#108781=DIRECTION('center_axis',(-0.164089292933262,0.,-0.986445489596188));
#108782=DIRECTION('ref_axis',(0.986445489596187,-1.2940412193226E-15,-0.164089292933262));
#108783=DIRECTION('',(0.323730285810082,-2.12338308705133E-16,0.946149407889326));
#108784=DIRECTION('center_axis',(6.93889390390723E-17,2.22049474265475E-16,
-1.));
#108785=DIRECTION('ref_axis',(-0.707106781186548,-0.707106781186548,0.));
#108786=DIRECTION('center_axis',(0.808736084303188,0.,-0.588171697675047));
#108787=DIRECTION('ref_axis',(-0.588171697675047,2.04063050372407E-16,-0.808736084303188));
#108788=DIRECTION('',(-6.93889390390723E-17,-2.22049474265475E-16,1.));
#108789=DIRECTION('',(6.93889390390723E-17,2.22049474265475E-16,-1.));
#108790=DIRECTION('center_axis',(0.946149407889326,0.,-0.323730285810082));
#108791=DIRECTION('ref_axis',(-0.323730285810082,5.66263013082985E-17,-0.946149407889326));
#108792=DIRECTION('',(0.,1.,0.));
#108793=DIRECTION('center_axis',(1.,0.,6.93889390390723E-17));
#108794=DIRECTION('ref_axis',(6.93889390390723E-17,6.93889390390724E-18,
-1.));
#108795=DIRECTION('',(0.,1.,0.));
#108796=DIRECTION('',(-1.11022302462516E-16,2.22044604925031E-16,-1.));
#108797=DIRECTION('center_axis',(6.93889390390722E-18,1.,2.22049474265475E-16));
#108798=DIRECTION('ref_axis',(0.,0.,1.));
#108799=DIRECTION('center_axis',(6.93889390390722E-18,1.,2.22049474265475E-16));
#108800=DIRECTION('ref_axis',(0.973489193493256,-5.75449829877939E-17,0.22873301062997));
#108801=DIRECTION('center_axis',(-0.00226873389465586,0.,-0.999997426419946));
#108802=DIRECTION('ref_axis',(0.,-1.,0.));
#108803=DIRECTION('center_axis',(-6.93889390390722E-18,-1.,-2.22049474265475E-16));
#108804=DIRECTION('ref_axis',(0.973489193493256,-5.4780741346636E-17,0.22873301062997));
#108805=DIRECTION('center_axis',(0.990019786637194,0.,0.140928428880923));
#108806=DIRECTION('ref_axis',(0.,-1.,0.));
#108807=DIRECTION('center_axis',(6.93889390390722E-18,1.,2.22049474265475E-16));
#108808=DIRECTION('ref_axis',(-0.656246152467199,1.15648231731787E-16,-0.754546875529942));
#108809=DIRECTION('center_axis',(-6.93889390390722E-18,-1.,-2.22049474265475E-16));
#108810=DIRECTION('ref_axis',(-0.656246152467199,1.72100359446898E-16,-0.754546875529942));
#108811=DIRECTION('center_axis',(6.93889390390722E-18,1.,2.22049474265475E-16));
#108812=DIRECTION('ref_axis',(0.,-2.75992927452516E-16,1.));
#108813=DIRECTION('center_axis',(0.991102794140644,0.,0.133098653060836));
#108814=DIRECTION('ref_axis',(0.,-1.,0.));
#108815=DIRECTION('center_axis',(-6.93889390390722E-18,-1.,-2.22049474265475E-16));
#108816=DIRECTION('ref_axis',(-0.137014611029961,-2.19752839926614E-16,
0.990569026552066));
#108817=DIRECTION('center_axis',(6.93889390390722E-18,1.,2.22049474265475E-16));
#108818=DIRECTION('ref_axis',(-0.137014611029961,-2.19004601720328E-16,
0.990569026552066));
#108819=DIRECTION('center_axis',(-2.22044604925031E-14,0.,1.));
#108820=DIRECTION('ref_axis',(0.,-1.,0.));
#108821=DIRECTION('center_axis',(6.93889390390722E-18,1.,2.22049474265475E-16));
#108822=DIRECTION('ref_axis',(0.752694710045468,1.15648231731787E-16,-0.658369708803168));
#108823=DIRECTION('center_axis',(-6.93889390390722E-18,-1.,-2.22049474265475E-16));
#108824=DIRECTION('ref_axis',(0.752694710045468,1.4096777897702E-16,-0.658369708803168));
#108825=DIRECTION('center_axis',(-2.57651168044591E-14,-2.22049474265475E-16,
1.));
#108826=DIRECTION('ref_axis',(0.707106781186548,-0.707106781186548,1.57009245868377E-14));
#108827=DIRECTION('',(2.57651168044591E-14,2.22049474265475E-16,-1.));
#108828=DIRECTION('',(-2.57651168044591E-14,-2.22049474265475E-16,1.));
#108829=DIRECTION('center_axis',(-0.707106781186563,0.,0.707106781186532));
#108830=DIRECTION('ref_axis',(-0.707106781186532,3.14025378024051E-16,-0.707106781186563));
#108831=DIRECTION('center_axis',(-1.,6.9388939039087E-18,-6.67785932371251E-15));
#108832=DIRECTION('ref_axis',(-3.92523114670943E-15,-0.707106781186548,
0.707106781186548));
#108833=DIRECTION('',(1.,-6.9388939039087E-18,6.67785932371251E-15));
#108834=DIRECTION('',(-1.,6.9388939039087E-18,-6.67785932371251E-15));
#108835=DIRECTION('center_axis',(1.,-6.86520621803209E-30,2.57651168044591E-14));
#108836=DIRECTION('ref_axis',(-2.57651168044591E-14,-2.2898349882894E-16,
1.));
#108837=DIRECTION('',(6.86520621803209E-30,1.,4.58448813522947E-44));
#108838=DIRECTION('center_axis',(-1.,6.86520621803209E-30,-2.57651168044591E-14));
#108839=DIRECTION('ref_axis',(1.97111506292388E-14,0.643991722633251,-0.765032457598929));
#108840=DIRECTION('',(8.62629387613302E-31,-1.,-2.99934041219171E-16));
#108841=DIRECTION('',(-2.57651168044591E-14,-2.22044604925031E-16,1.));
#108842=DIRECTION('',(0.,1.,2.66453525910038E-16));
#108843=DIRECTION('center_axis',(6.67785932371251E-15,0.,-1.));
#108844=DIRECTION('ref_axis',(-1.,-3.76269782527349E-17,-6.67785932371251E-15));
#108845=DIRECTION('',(0.,1.,2.22044604925031E-16));
#108846=DIRECTION('',(0.,-1.,-2.22044604925031E-16));
#108847=DIRECTION('',(-1.,0.,0.));
#108848=DIRECTION('center_axis',(0.,1.,2.22044604925031E-16));
#108849=DIRECTION('ref_axis',(0.973489193493256,-5.07889309786447E-17,0.22873301062997));
#108850=DIRECTION('',(0.,-1.,-2.22044604925031E-16));
#108851=DIRECTION('center_axis',(0.,1.,2.22044604925031E-16));
#108852=DIRECTION('ref_axis',(-1.,0.,0.));
#108853=DIRECTION('center_axis',(6.93889390390722E-18,1.,2.22049474265475E-16));
#108854=DIRECTION('ref_axis',(-1.,6.93889390390721E-18,1.83750175990302E-19));
#108855=DIRECTION('center_axis',(6.93889390390723E-18,1.,2.22049474265475E-16));
#108856=DIRECTION('ref_axis',(0.,0.,1.));
#108857=DIRECTION('center_axis',(-6.93889390390723E-18,-1.,-2.22049474265475E-16));
#108858=DIRECTION('ref_axis',(0.33866857591881,-2.08550719155025E-16,0.940905731561417));
#108859=DIRECTION('center_axis',(6.93889390390723E-18,1.,2.22049474265475E-16));
#108860=DIRECTION('ref_axis',(0.33866857591881,-2.11277608343473E-16,0.940905731561417));
#108861=DIRECTION('center_axis',(-0.17934429547033,0.,0.983786370957766));
#108862=DIRECTION('ref_axis',(0.,-1.,0.));
#108863=DIRECTION('center_axis',(6.93889390390723E-18,1.,2.22049474265475E-16));
#108864=DIRECTION('ref_axis',(0.865342368165252,1.15648231731787E-16,-0.50118119064681));
#108865=DIRECTION('center_axis',(-6.93889390390723E-18,-1.,-2.22049474265475E-16));
#108866=DIRECTION('ref_axis',(0.,0.,-1.));
#108867=DIRECTION('center_axis',(-0.939530312300397,0.,0.342465753424658));
#108868=DIRECTION('ref_axis',(0.,-1.,0.));
#108869=DIRECTION('center_axis',(6.93889390390723E-18,1.,2.22049474265475E-16));
#108870=DIRECTION('ref_axis',(0.764334265490702,-1.34922937020418E-16,0.644820231224787));
#108871=DIRECTION('center_axis',(6.93889390390723E-18,1.,2.22049474265475E-16));
#108872=DIRECTION('ref_axis',(0.,0.,1.));
#108873=DIRECTION('center_axis',(6.93889390390723E-18,1.,2.22049474265475E-16));
#108874=DIRECTION('ref_axis',(-0.819288030372914,1.33004164137626E-16,-0.573382179080996));
#108875=DIRECTION('center_axis',(0.,0.,1.));
#108876=DIRECTION('ref_axis',(0.,-1.,0.));
#108877=DIRECTION('center_axis',(-6.93889390390723E-18,-1.,-2.22049474265475E-16));
#108878=DIRECTION('ref_axis',(-0.819288030372914,1.31276371155002E-16,-0.573382179080996));
#108879=DIRECTION('center_axis',(6.93889390390723E-18,1.,2.22049474265475E-16));
#108880=DIRECTION('ref_axis',(-1.,6.93889390390723E-18,1.83750175990302E-19));
#108881=DIRECTION('center_axis',(-6.93889390390723E-18,-1.,-2.22049474265475E-16));
#108882=DIRECTION('ref_axis',(-0.816812386473668,1.33768869693028E-16,-0.576903393388521));
#108883=DIRECTION('center_axis',(-6.93889390390723E-18,-1.,-2.22049474265475E-16));
#108884=DIRECTION('ref_axis',(-0.983881728593356,4.65340321282978E-17,-0.178820424281317));
#108885=DIRECTION('',(-2.04853783127104E-16,2.22049474265475E-16,-1.));
#108886=DIRECTION('center_axis',(-6.93889390390723E-18,-1.,-2.22049474265475E-16));
#108887=DIRECTION('ref_axis',(-0.707106781186547,-1.52106150078638E-16,
0.707106781186548));
#108888=DIRECTION('',(-1.,6.93889390390728E-18,-2.40389762145677E-16));
#108889=DIRECTION('center_axis',(-6.93889390390723E-18,-1.,-2.22049474265475E-16));
#108890=DIRECTION('ref_axis',(0.707106781186547,-1.61919227945412E-16,0.707106781186548));
#108891=DIRECTION('',(-2.41949676183277E-16,-2.22049474265475E-16,1.));
#108892=DIRECTION('center_axis',(-2.41949676183277E-16,-2.22049474265475E-16,
1.));
#108893=DIRECTION('ref_axis',(0.707106781186548,-0.707106781186548,0.));
#108894=DIRECTION('center_axis',(0.,0.,1.));
#108895=DIRECTION('ref_axis',(0.,-1.,0.));
#108896=DIRECTION('',(2.41949676183277E-16,2.22049474265475E-16,-1.));
#108897=DIRECTION('center_axis',(-1.,0.,0.));
#108898=DIRECTION('ref_axis',(0.,-1.,0.));
#108899=DIRECTION('center_axis',(6.93889390390723E-18,1.,2.22049474265475E-16));
#108900=DIRECTION('ref_axis',(0.707106781186547,-1.15648231731787E-16,0.707106781186548));
#108901=DIRECTION('center_axis',(-1.,6.93889390390728E-18,-2.40389762145677E-16));
#108902=DIRECTION('ref_axis',(0.,-0.707106781186548,0.707106781186548));
#108903=DIRECTION('center_axis',(-1.,0.,0.));
#108904=DIRECTION('ref_axis',(0.,-1.,0.));
#108905=DIRECTION('',(1.,-6.93889390390728E-18,2.40389762145677E-16));
#108906=DIRECTION('center_axis',(0.,0.,-1.));
#108907=DIRECTION('ref_axis',(0.,-1.,0.));
#108908=DIRECTION('center_axis',(6.93889390390723E-18,1.,2.22049474265475E-16));
#108909=DIRECTION('ref_axis',(-0.707106781186547,-1.15648231731787E-16,
0.707106781186548));
#108910=DIRECTION('center_axis',(-2.04853783127104E-16,2.22049474265475E-16,
-1.));
#108911=DIRECTION('ref_axis',(-0.707106781186547,-0.707106781186548,0.));
#108912=DIRECTION('center_axis',(0.,0.,-1.));
#108913=DIRECTION('ref_axis',(0.,-1.,0.));
#108914=DIRECTION('',(2.04853783127104E-16,-2.22049474265475E-16,1.));
#108915=DIRECTION('center_axis',(0.351876296299398,0.,-0.9360465117197));
#108916=DIRECTION('ref_axis',(0.,-1.,0.));
#108917=DIRECTION('center_axis',(6.93889390390723E-18,1.,2.22049474265475E-16));
#108918=DIRECTION('ref_axis',(-0.983881728593356,0.,-0.178820424281317));
#108919=DIRECTION('center_axis',(6.93889390390723E-18,1.,2.22049474265475E-16));
#108920=DIRECTION('ref_axis',(0.,-3.86164530304402E-16,1.));
#108921=DIRECTION('center_axis',(6.93889390390723E-18,1.,2.22049474265475E-16));
#108922=DIRECTION('ref_axis',(-0.816812386473668,1.35760967685141E-16,-0.576903393388521));
#108923=DIRECTION('center_axis',(0.,1.,0.));
#108924=DIRECTION('ref_axis',(-0.983786370957765,0.,-0.179344295470333));
#108925=DIRECTION('',(0.,1.,0.));
#108926=DIRECTION('center_axis',(0.,1.,2.22044604925031E-16));
#108927=DIRECTION('ref_axis',(-0.983786370957765,0.,-0.179344295470333));
#108928=DIRECTION('',(0.,-1.,0.));
#108929=DIRECTION('center_axis',(0.,-1.,-2.39272203583008E-16));
#108930=DIRECTION('ref_axis',(0.342465753424657,-2.24803488157148E-16,0.939530312300397));
#108931=DIRECTION('',(0.,-1.,-2.39272203583008E-16));
#108932=DIRECTION('center_axis',(0.,1.,2.22044604925031E-16));
#108933=DIRECTION('ref_axis',(0.342465753424657,-2.24803488157148E-16,0.939530312300397));
#108934=DIRECTION('center_axis',(0.,-1.,-2.39272203583008E-16));
#108935=DIRECTION('ref_axis',(-0.342465753424657,2.24803488157148E-16,-0.939530312300397));
#108936=DIRECTION('',(0.,-1.,-2.39272203583008E-16));
#108937=DIRECTION('center_axis',(0.,-1.,-2.22044604925031E-16));
#108938=DIRECTION('ref_axis',(-0.342465753424657,2.24803488157148E-16,-0.939530312300397));
#108939=DIRECTION('center_axis',(1.,-5.78918321765678E-32,2.41949676183277E-16));
#108940=DIRECTION('ref_axis',(-2.41949676183277E-16,-2.22049474265475E-16,
1.));
#108941=DIRECTION('',(3.24194260188779E-33,-1.,-2.52671446983656E-16));
#108942=DIRECTION('',(2.41949676183277E-16,2.22044604925031E-16,-1.));
#108943=DIRECTION('center_axis',(-3.24194260188779E-33,1.,2.52671446983656E-16));
#108944=DIRECTION('ref_axis',(0.707106781186548,0.,0.707106781186548));
#108945=DIRECTION('',(-3.24194260188779E-33,1.,2.52671446983656E-16));
#108946=DIRECTION('center_axis',(0.,-1.,-2.22044604925031E-16));
#108947=DIRECTION('ref_axis',(0.707106781186548,0.,0.707106781186548));
#108948=DIRECTION('center_axis',(-2.40389762145677E-16,-2.52671446983656E-16,
1.));
#108949=DIRECTION('ref_axis',(-1.,-6.93889390390718E-18,-2.40389762145677E-16));
#108950=DIRECTION('',(4.78544407166016E-17,-1.,-2.52671446983656E-16));
#108951=DIRECTION('',(1.,-5.3377249763659E-32,2.40389762145677E-16));
#108952=DIRECTION('center_axis',(-4.78544407166016E-17,1.,2.52671446983656E-16));
#108953=DIRECTION('ref_axis',(-0.707106781186548,0.,0.707106781186547));
#108954=DIRECTION('',(-4.78544407166016E-17,1.,2.52671446983656E-16));
#108955=DIRECTION('center_axis',(0.,1.,2.22044604925031E-16));
#108956=DIRECTION('ref_axis',(-0.707106781186548,0.,0.707106781186547));
#108957=DIRECTION('center_axis',(1.,4.78544407166016E-17,-2.04853783127104E-16));
#108958=DIRECTION('ref_axis',(2.04853783127104E-16,-2.28983498828938E-16,
1.));
#108959=DIRECTION('',(4.78544407166015E-17,-1.,-3.49344973759647E-16));
#108960=DIRECTION('',(-2.04853783127104E-16,2.22044604925031E-16,-1.));
#108961=DIRECTION('center_axis',(-4.78544407166016E-17,1.,3.49344973759647E-16));
#108962=DIRECTION('ref_axis',(-0.983881728593356,0.,-0.178820424281317));
#108963=DIRECTION('',(0.,1.,2.22044604925031E-16));
#108964=DIRECTION('center_axis',(0.,1.,2.22044604925031E-16));
#108965=DIRECTION('ref_axis',(-0.983881728593356,0.,-0.178820424281317));
#108966=DIRECTION('center_axis',(0.,1.,2.22044604925031E-16));
#108967=DIRECTION('ref_axis',(0.17741935483871,2.18521943337466E-16,-0.98413534258689));
#108968=DIRECTION('center_axis',(0.,-1.,-2.22044604925031E-16));
#108969=DIRECTION('ref_axis',(-0.994623655913978,-2.29939845948218E-17,
0.103555700453002));
#108970=DIRECTION('',(0.,1.,2.22044604925031E-16));
#108971=DIRECTION('center_axis',(0.,1.,2.22044604925031E-16));
#108972=DIRECTION('ref_axis',(0.17741935483871,2.18521943337466E-16,-0.98413534258689));
#108973=DIRECTION('',(0.,1.,2.22044604925031E-16));
#108974=DIRECTION('center_axis',(1.51594548245566E-16,-0.819152044288998,
0.573576436351038));
#108975=DIRECTION('ref_axis',(-1.9770466526922E-16,-0.573576436351038,-0.819152044288998));
#108976=DIRECTION('',(0.,1.,2.22044604925031E-16));
#108977=DIRECTION('center_axis',(0.,-1.,-2.22044604925031E-16));
#108978=DIRECTION('ref_axis',(0.17741935483871,2.18521943337466E-16,-0.98413534258689));
#108979=DIRECTION('center_axis',(1.,0.,0.));
#108980=DIRECTION('ref_axis',(0.,-1.,0.));
#108981=DIRECTION('center_axis',(6.93889390390723E-18,1.,2.22049474265475E-16));
#108982=DIRECTION('ref_axis',(0.,0.,1.));
#108983=DIRECTION('center_axis',(-0.563542669426771,0.,-0.826086956521739));
#108984=DIRECTION('ref_axis',(0.826086956521739,0.,-0.563542669426771));
#108985=DIRECTION('center_axis',(6.93889390390723E-18,1.,2.22049474265475E-16));
#108986=DIRECTION('ref_axis',(-0.462172675917159,-1.93704275295193E-16,
0.886789951248644));
#108987=DIRECTION('center_axis',(0.999936821691632,0.,-0.0112406683625832));
#108988=DIRECTION('ref_axis',(0.,-1.,0.));
#108989=DIRECTION('center_axis',(-6.93889390390723E-18,-1.,-2.22049474265475E-16));
#108990=DIRECTION('ref_axis',(-0.462172675917159,-1.98254111540207E-16,
0.886789951248644));
#108991=DIRECTION('center_axis',(-0.707106781186548,0.,0.707106781186548));
#108992=DIRECTION('ref_axis',(0.,-1.,0.));
#108993=DIRECTION('center_axis',(6.93889390390723E-18,1.,2.22049474265475E-16));
#108994=DIRECTION('ref_axis',(0.921714097362088,8.67361737988403E-17,-0.387869981725824));
#108995=DIRECTION('center_axis',(-6.93889390390723E-18,-1.,-2.22049474265475E-16));
#108996=DIRECTION('ref_axis',(0.921714097362088,7.97306491942474E-17,-0.387869981725824));
#108997=DIRECTION('center_axis',(-0.707106781186548,-1.52106150078638E-16,
0.707106781186547));
#108998=DIRECTION('ref_axis',(0.500000000000002,-0.707106781186548,0.499999999999998));
#108999=DIRECTION('center_axis',(-0.707106781186549,0.,0.707106781186546));
#109000=DIRECTION('ref_axis',(0.,-1.,0.));
#109001=DIRECTION('',(0.707106781186548,1.52106150078638E-16,-0.707106781186547));
#109002=DIRECTION('',(-0.707106781186548,-1.52106150078638E-16,0.707106781186547));
#109003=DIRECTION('center_axis',(6.93889390390723E-18,1.,2.22049474265475E-16));
#109004=DIRECTION('ref_axis',(0.,0.,1.));
#109005=DIRECTION('center_axis',(1.88182802673964E-12,0.,1.));
#109006=DIRECTION('ref_axis',(0.,-1.,0.));
#109007=DIRECTION('center_axis',(-6.93889390390723E-18,-1.,-2.22049474265475E-16));
#109008=DIRECTION('ref_axis',(-0.923879532511647,8.67361737988402E-17,-0.38268343236422));
#109009=DIRECTION('center_axis',(6.93889390390723E-18,1.,2.22049474265475E-16));
#109010=DIRECTION('ref_axis',(-0.923879532511647,9.13853570226723E-17,-0.38268343236422));
#109011=DIRECTION('center_axis',(1.88212241265405E-12,-2.22049474265488E-16,
1.));
#109012=DIRECTION('ref_axis',(0.707106781186548,-0.707106781186548,-1.3306533587345E-12));
#109013=DIRECTION('center_axis',(1.88182802673964E-12,0.,1.));
#109014=DIRECTION('ref_axis',(0.,-1.,0.));
#109015=DIRECTION('',(-1.88212241265405E-12,2.22049474265488E-16,-1.));
#109016=DIRECTION('',(1.88212241265405E-12,-2.22049474265488E-16,1.));
#109017=DIRECTION('center_axis',(-0.989426754293278,0.,-0.14503343714009));
#109018=DIRECTION('ref_axis',(0.,-1.,0.));
#109019=DIRECTION('center_axis',(6.93889390390723E-18,1.,2.22049474265475E-16));
#109020=DIRECTION('ref_axis',(0.653822056396758,-1.73472347597681E-16,0.756648345381865));
#109021=DIRECTION('center_axis',(-6.93889390390723E-18,-1.,-2.22049474265475E-16));
#109022=DIRECTION('ref_axis',(0.653822056396758,-1.72550169177256E-16,0.756648345381865));
#109023=DIRECTION('center_axis',(6.93889390390723E-18,1.,2.22049474265475E-16));
#109024=DIRECTION('ref_axis',(0.,0.,1.));
#109025=DIRECTION('center_axis',(0.89959196856447,0.,0.436731370632225));
#109026=DIRECTION('ref_axis',(-0.436731370632225,0.,0.89959196856447));
#109027=DIRECTION('center_axis',(6.93889390390723E-18,1.,2.22049474265475E-16));
#109028=DIRECTION('ref_axis',(0.327915980784702,2.07496294239519E-16,-0.944706890811116));
#109029=DIRECTION('center_axis',(-0.976712922996695,0.,-0.214550381149164));
#109030=DIRECTION('ref_axis',(0.,-1.,0.));
#109031=DIRECTION('center_axis',(-6.93889390390723E-18,-1.,-2.22049474265475E-16));
#109032=DIRECTION('ref_axis',(0.327915980784702,2.06949467309514E-16,-0.944706890811116));
#109033=DIRECTION('center_axis',(0.55230501554796,0.,-0.833642111340693));
#109034=DIRECTION('ref_axis',(0.,-1.,0.));
#109035=DIRECTION('center_axis',(6.93889390390723E-18,1.,2.22049474265475E-16));
#109036=DIRECTION('ref_axis',(-0.926903899779186,-1.15648231731787E-16,
0.375298761754069));
#109037=DIRECTION('center_axis',(-6.93889390390723E-18,-1.,-2.22049474265475E-16));
#109038=DIRECTION('ref_axis',(-0.926903899779186,-7.69032049202891E-17,
0.375298761754069));
#109039=DIRECTION('center_axis',(6.93889390390723E-18,1.,2.22049474265475E-16));
#109040=DIRECTION('ref_axis',(0.,0.,1.));
#109041=DIRECTION('center_axis',(0.,0.,-1.));
#109042=DIRECTION('ref_axis',(0.,-1.,0.));
#109043=DIRECTION('center_axis',(-6.93889390390723E-18,-1.,-2.22049474265475E-16));
#109044=DIRECTION('ref_axis',(0.957507731389333,-5.78241158658936E-17,0.288407601026141));
#109045=DIRECTION('center_axis',(6.93889390390723E-18,1.,2.22049474265475E-16));
#109046=DIRECTION('ref_axis',(0.957507731389333,-7.06848007423029E-17,0.288407601026141));
#109047=DIRECTION('center_axis',(0.,2.22049474265475E-16,-1.));
#109048=DIRECTION('ref_axis',(-0.707106781186548,-0.707106781186548,0.));
#109049=DIRECTION('center_axis',(0.,0.,-1.));
#109050=DIRECTION('ref_axis',(0.,-1.,0.));
#109051=DIRECTION('',(0.,-2.22049474265475E-16,1.));
#109052=DIRECTION('',(0.,2.22049474265475E-16,-1.));
#109053=DIRECTION('center_axis',(-6.93889390390723E-18,-1.,-2.22049474265475E-16));
#109054=DIRECTION('ref_axis',(0.,0.,-1.));
#109055=DIRECTION('center_axis',(6.93889390390723E-18,1.,2.22049474265475E-16));
#109056=DIRECTION('ref_axis',(-0.294329993497647,-2.16418819656757E-16,
0.955703853151003));
#109057=DIRECTION('center_axis',(-6.93889390390723E-18,-1.,-2.22049474265475E-16));
#109058=DIRECTION('ref_axis',(-0.294329993497647,-2.10171213548051E-16,
0.955703853151004));
#109059=DIRECTION('center_axis',(-0.988716140908567,0.130504856475735,0.0735450551914906));
#109060=DIRECTION('ref_axis',(-0.149801177254627,-0.861356769214109,-0.485411293051738));
#109061=DIRECTION('center_axis',(0.,1.,0.));
#109062=DIRECTION('ref_axis',(-0.294883912309791,0.,-0.95553308590591));
#109063=DIRECTION('center_axis',(-0.707106781186547,0.,-0.707106781186548));
#109064=DIRECTION('ref_axis',(-0.707106781186548,-1.57009245868377E-16,
0.707106781186547));
#109065=DIRECTION('',(0.,-1.,0.));
#109066=DIRECTION('',(-0.707106781186548,-1.57009245868377E-16,0.707106781186547));
#109067=DIRECTION('',(0.,1.,0.));
#109068=DIRECTION('center_axis',(0.,1.,0.));
#109069=DIRECTION('ref_axis',(-0.923879532511647,0.,-0.38268343236422));
#109070=DIRECTION('',(0.,1.,0.));
#109071=DIRECTION('center_axis',(0.,-1.,-2.22044604925031E-16));
#109072=DIRECTION('ref_axis',(-0.923879532511647,0.,-0.38268343236422));
#109073=DIRECTION('center_axis',(-1.,-5.22393909422894E-28,1.88212241265405E-12));
#109074=DIRECTION('ref_axis',(1.88212241265405E-12,-2.22044604925031E-16,
1.));
#109075=DIRECTION('',(0.,-1.,0.));
#109076=DIRECTION('',(1.88215207428297E-12,-2.22044604925031E-16,1.));
#109077=DIRECTION('center_axis',(0.,-1.,0.));
#109078=DIRECTION('ref_axis',(0.653822056396758,0.,0.756648345381865));
#109079=DIRECTION('',(0.,1.,0.));
#109080=DIRECTION('center_axis',(0.,1.,2.22044604925031E-16));
#109081=DIRECTION('ref_axis',(0.653822056396758,0.,0.756648345381865));
#109082=DIRECTION('center_axis',(0.,-1.,0.));
#109083=DIRECTION('ref_axis',(-0.436731370632224,0.,0.899591968564471));
#109084=DIRECTION('',(0.,-1.,0.));
#109085=DIRECTION('center_axis',(0.,-1.,-2.22044604925031E-16));
#109086=DIRECTION('ref_axis',(-0.436731370632224,0.,0.899591968564471));
#109087=DIRECTION('center_axis',(0.,-1.,0.));
#109088=DIRECTION('ref_axis',(0.436731370632225,0.,-0.89959196856447));
#109089=DIRECTION('',(0.,-1.,0.));
#109090=DIRECTION('center_axis',(0.,1.,2.22044604925031E-16));
#109091=DIRECTION('ref_axis',(0.436731370632225,0.,-0.89959196856447));
#109092=DIRECTION('center_axis',(6.93889390390723E-18,1.,2.22049474265475E-16));
#109093=DIRECTION('ref_axis',(-1.,6.93889390390723E-18,1.83750175990302E-19));
#109094=DIRECTION('center_axis',(1.65636802248512E-16,-2.22049474265475E-16,
1.));
#109095=DIRECTION('ref_axis',(0.707106781186548,-0.707106781186548,-2.4532694666934E-16));
#109096=DIRECTION('center_axis',(0.,0.,-1.));
#109097=DIRECTION('ref_axis',(1.,0.,0.));
#109098=DIRECTION('',(1.65636802248512E-16,-2.22049474265475E-16,1.));
#109099=DIRECTION('center_axis',(0.,0.,1.));
#109100=DIRECTION('ref_axis',(0.,-1.,0.));
#109101=DIRECTION('',(-1.65636802248512E-16,2.22049474265475E-16,-1.));
#109102=DIRECTION('center_axis',(-1.,0.,0.));
#109103=DIRECTION('ref_axis',(0.,-1.,0.));
#109104=DIRECTION('center_axis',(6.93889390390723E-18,1.,2.22049474265475E-16));
#109105=DIRECTION('ref_axis',(0.707106781186547,-1.15648231731787E-16,0.707106781186548));
#109106=DIRECTION('center_axis',(-6.93889390390723E-18,-1.,-2.22049474265475E-16));
#109107=DIRECTION('ref_axis',(0.707106781186547,-1.61919227945412E-16,0.707106781186548));
#109108=DIRECTION('center_axis',(-1.,6.93889390390724E-18,-6.93889390390729E-17));
#109109=DIRECTION('ref_axis',(0.,-0.707106781186548,0.707106781186548));
#109110=DIRECTION('center_axis',(-1.,0.,0.));
#109111=DIRECTION('ref_axis',(0.,-1.,0.));
#109112=DIRECTION('',(1.,-6.93889390390724E-18,6.93889390390729E-17));
#109113=DIRECTION('',(-1.,6.93889390390724E-18,-6.93889390390729E-17));
#109114=DIRECTION('center_axis',(6.93889390390723E-18,1.,2.22049474265475E-16));
#109115=DIRECTION('ref_axis',(0.,0.,1.));
#109116=DIRECTION('center_axis',(-0.914646181285313,0.,0.40425531914892));
#109117=DIRECTION('ref_axis',(0.,-1.,0.));
#109118=DIRECTION('center_axis',(-6.93889390390723E-18,-1.,-2.22049474265475E-16));
#109119=DIRECTION('ref_axis',(-0.206583903916408,2.20013709148278E-16,-0.978428888904379));
#109120=DIRECTION('center_axis',(6.93889390390723E-18,1.,2.22049474265475E-16));
#109121=DIRECTION('ref_axis',(-0.206583903916408,2.18693084178901E-16,-0.978428888904378));
#109122=DIRECTION('center_axis',(1.66533453693774E-14,0.,-1.));
#109123=DIRECTION('ref_axis',(0.,-1.,0.));
#109124=DIRECTION('center_axis',(6.93889390390723E-18,1.,2.22049474265475E-16));
#109125=DIRECTION('ref_axis',(-0.54577682290983,-2.31296463463574E-16,0.837930581596383));
#109126=DIRECTION('center_axis',(-6.93889390390723E-18,-1.,-2.22049474265475E-16));
#109127=DIRECTION('ref_axis',(-0.54577682290983,-1.82274957645058E-16,0.837930581596383));
#109128=DIRECTION('center_axis',(1.88016196282748E-14,2.22049474265475E-16,
-1.));
#109129=DIRECTION('ref_axis',(-0.707106781186548,-0.707106781186548,-1.3738309013483E-14));
#109130=DIRECTION('center_axis',(1.94289029309402E-14,0.,-1.));
#109131=DIRECTION('ref_axis',(0.,-1.,0.));
#109132=DIRECTION('',(-1.88016196282748E-14,-2.22049474265475E-16,1.));
#109133=DIRECTION('',(1.88016196282748E-14,2.22049474265475E-16,-1.));
#109134=DIRECTION('center_axis',(6.93889390390723E-18,1.,2.22049474265475E-16));
#109135=DIRECTION('ref_axis',(0.,-4.13106241720989E-16,1.));
#109136=DIRECTION('center_axis',(-0.567316408958496,0.,-0.823499904144765));
#109137=DIRECTION('ref_axis',(0.,-1.,0.));
#109138=DIRECTION('center_axis',(-6.93889390390723E-18,-1.,-2.22049474265475E-16));
#109139=DIRECTION('ref_axis',(0.95485598499061,5.33761069531325E-17,-0.297069096217718));
#109140=DIRECTION('center_axis',(6.93889390390723E-18,1.,2.22049474265475E-16));
#109141=DIRECTION('ref_axis',(0.95485598499061,5.93383922623034E-17,-0.297069096217718));
#109142=DIRECTION('center_axis',(0.994393511593655,0.,0.105742820562149));
#109143=DIRECTION('ref_axis',(0.,-1.,0.));
#109144=DIRECTION('center_axis',(6.93889390390723E-18,1.,2.22049474265475E-16));
#109145=DIRECTION('ref_axis',(-0.859376679196035,1.15648231731787E-16,-0.511343058282788));
#109146=DIRECTION('center_axis',(-6.93889390390723E-18,-1.,-2.22049474265475E-16));
#109147=DIRECTION('ref_axis',(-0.859376679196035,1.19506580861427E-16,-0.511343058282788));
#109148=DIRECTION('center_axis',(6.93889390390723E-18,1.,2.22049474265475E-16));
#109149=DIRECTION('ref_axis',(0.,-1.78573536624128E-16,1.));
#109150=DIRECTION('center_axis',(0.999122256992311,0.,-0.0418893254014727));
#109151=DIRECTION('ref_axis',(0.,-1.,0.));
#109152=DIRECTION('center_axis',(-6.93889390390723E-18,-1.,-2.22049474265475E-16));
#109153=DIRECTION('ref_axis',(-0.0320141760681106,-2.21667125556843E-16,
0.999487414893594));
#109154=DIRECTION('center_axis',(6.93889390390723E-18,1.,2.22049474265475E-16));
#109155=DIRECTION('ref_axis',(-0.0320141760681106,-2.21713512040924E-16,
0.999487414893594));
#109156=DIRECTION('center_axis',(0.707106781186548,0.,0.707106781186547));
#109157=DIRECTION('ref_axis',(0.,-1.,0.));
#109158=DIRECTION('center_axis',(6.93889390390723E-18,1.,2.22049474265475E-16));
#109159=DIRECTION('ref_axis',(0.363244855982583,1.73472347597681E-16,-0.931693712870379));
#109160=DIRECTION('center_axis',(-6.93889390390723E-18,-1.,-2.22049474265475E-16));
#109161=DIRECTION('ref_axis',(0.363244855982583,2.04361581602513E-16,-0.931693712870379));
#109162=DIRECTION('center_axis',(0.707106781186547,-1.61919227945412E-16,
0.707106781186548));
#109163=DIRECTION('ref_axis',(0.500000000000001,-0.707106781186547,-0.499999999999999));
#109164=DIRECTION('center_axis',(0.707106781186552,0.,0.707106781186543));
#109165=DIRECTION('ref_axis',(0.,-1.,0.));
#109166=DIRECTION('',(-0.707106781186547,1.61919227945412E-16,-0.707106781186548));
#109167=DIRECTION('',(0.707106781186547,-1.61919227945412E-16,0.707106781186548));
#109168=DIRECTION('center_axis',(6.93889390390723E-18,1.,2.22049474265475E-16));
#109169=DIRECTION('ref_axis',(0.923879532511287,8.67361737988403E-17,-0.38268343236509));
#109170=DIRECTION('center_axis',(-6.93889390390723E-18,-1.,-2.22049474265475E-16));
#109171=DIRECTION('ref_axis',(0.923879532511287,7.85639529106883E-17,-0.38268343236509));
#109172=DIRECTION('center_axis',(0.,-1.,0.));
#109173=DIRECTION('ref_axis',(-0.859376679196034,0.,-0.51134305828279));
#109174=DIRECTION('',(0.,1.,0.));
#109175=DIRECTION('center_axis',(0.,1.,2.22044604925031E-16));
#109176=DIRECTION('ref_axis',(-0.859376679196034,0.,-0.51134305828279));
#109177=DIRECTION('',(0.,-1.,-2.22044604925031E-16));
#109178=DIRECTION('center_axis',(0.,-1.,0.));
#109179=DIRECTION('ref_axis',(-0.28378257126716,0.,0.958888654769155));
#109180=DIRECTION('',(0.,-1.,0.));
#109181=DIRECTION('center_axis',(0.,1.,2.22044604925031E-16));
#109182=DIRECTION('ref_axis',(-0.28378257126716,0.,0.958888654769155));
#109183=DIRECTION('center_axis',(0.,1.,0.));
#109184=DIRECTION('ref_axis',(0.363244855982583,0.,-0.931693712870379));
#109185=DIRECTION('',(0.,1.,0.));
#109186=DIRECTION('center_axis',(0.,1.,2.22044604925031E-16));
#109187=DIRECTION('ref_axis',(0.363244855982583,0.,-0.931693712870379));
#109188=DIRECTION('center_axis',(-0.707106781186548,0.,0.707106781186547));
#109189=DIRECTION('ref_axis',(0.707106781186547,-1.57009245868378E-16,0.707106781186548));
#109190=DIRECTION('',(0.,-1.,0.));
#109191=DIRECTION('',(0.707106781186547,-1.57009245868378E-16,0.707106781186548));
#109192=DIRECTION('center_axis',(0.,-1.,0.));
#109193=DIRECTION('ref_axis',(0.923879532511287,0.,-0.382683432365089));
#109194=DIRECTION('',(0.,1.,0.));
#109195=DIRECTION('center_axis',(0.,1.,2.22044604925031E-16));
#109196=DIRECTION('ref_axis',(0.923879532511287,0.,-0.382683432365089));
#109197=DIRECTION('center_axis',(1.,0.,-1.65636802248512E-16));
#109198=DIRECTION('ref_axis',(1.65636802248512E-16,-2.28983498828938E-16,
1.));
#109199=DIRECTION('',(0.,-1.,0.));
#109200=DIRECTION('',(1.65636802248512E-16,-2.22044604925031E-16,1.));
#109201=DIRECTION('center_axis',(6.93889390390723E-18,1.,2.22049474265475E-16));
#109202=DIRECTION('ref_axis',(-1.,6.93889390390723E-18,1.83750175990302E-19));
#109203=DIRECTION('center_axis',(-2.04853783127104E-16,2.22049474265475E-16,
-1.));
#109204=DIRECTION('ref_axis',(-0.707106781186547,-0.707106781186548,0.));
#109205=DIRECTION('center_axis',(-3.79470760369927E-16,0.,1.));
#109206=DIRECTION('ref_axis',(-1.,0.,-3.79470760369927E-16));
#109207=DIRECTION('',(-2.04853783127104E-16,2.22049474265475E-16,-1.));
#109208=DIRECTION('center_axis',(0.,0.,-1.));
#109209=DIRECTION('ref_axis',(0.,-1.,0.));
#109210=DIRECTION('',(2.04853783127104E-16,-2.22049474265475E-16,1.));
#109211=DIRECTION('center_axis',(1.,0.,3.46944695195362E-16));
#109212=DIRECTION('ref_axis',(0.,-1.,0.));
#109213=DIRECTION('center_axis',(6.93889390390723E-18,1.,2.22049474265475E-16));
#109214=DIRECTION('ref_axis',(-0.707106781186547,1.15648231731787E-16,-0.707106781186548));
#109215=DIRECTION('center_axis',(-6.93889390390723E-18,-1.,-2.22049474265475E-16));
#109216=DIRECTION('ref_axis',(-0.707106781186547,1.61919227945412E-16,-0.707106781186548));
#109217=DIRECTION('center_axis',(1.,-6.93889390390728E-18,2.40389762145677E-16));
#109218=DIRECTION('ref_axis',(0.,-0.707106781186548,-0.707106781186547));
#109219=DIRECTION('center_axis',(1.,0.,1.38777878078145E-15));
#109220=DIRECTION('ref_axis',(0.,-1.,0.));
#109221=DIRECTION('',(-1.,6.93889390390728E-18,-2.40389762145677E-16));
#109222=DIRECTION('',(1.,-6.93889390390728E-18,2.40389762145677E-16));
#109223=DIRECTION('center_axis',(0.,0.,1.));
#109224=DIRECTION('ref_axis',(0.,-1.,0.));
#109225=DIRECTION('center_axis',(6.93889390390723E-18,1.,2.22049474265475E-16));
#109226=DIRECTION('ref_axis',(0.707106781186548,1.15648231731787E-16,-0.707106781186547));
#109227=DIRECTION('center_axis',(-6.93889390390723E-18,-1.,-2.22049474265475E-16));
#109228=DIRECTION('ref_axis',(0.707106781186548,1.52106150078638E-16,-0.707106781186547));
#109229=DIRECTION('center_axis',(-2.41949676183277E-16,-2.22049474265475E-16,
1.));
#109230=DIRECTION('ref_axis',(0.707106781186548,-0.707106781186548,0.));
#109231=DIRECTION('center_axis',(0.,0.,1.));
#109232=DIRECTION('ref_axis',(0.,-1.,0.));
#109233=DIRECTION('',(2.41949676183277E-16,2.22049474265475E-16,-1.));
#109234=DIRECTION('',(-2.41949676183277E-16,-2.22049474265475E-16,1.));
#109235=DIRECTION('center_axis',(6.93889390390723E-18,1.,2.22049474265475E-16));
#109236=DIRECTION('ref_axis',(0.,0.,1.));
#109237=DIRECTION('center_axis',(0.970096776450229,0.,0.242718446601972));
#109238=DIRECTION('ref_axis',(0.,-1.,0.));
#109239=DIRECTION('center_axis',(-6.93889390390723E-18,-1.,-2.22049474265475E-16));
#109240=DIRECTION('ref_axis',(-0.788263422531444,-1.31276371155002E-16,
0.615337936989922));
#109241=DIRECTION('center_axis',(6.93889390390723E-18,1.,2.22049474265475E-16));
#109242=DIRECTION('ref_axis',(-0.788263422531444,-1.31165789146938E-16,
0.615337936989922));
#109243=DIRECTION('center_axis',(-6.93889390390723E-18,-1.,-2.22049474265475E-16));
#109244=DIRECTION('ref_axis',(0.,0.,-1.));
#109245=DIRECTION('center_axis',(0.442477646994526,0.,0.896779533614694));
#109246=DIRECTION('ref_axis',(0.,-1.,0.));
#109247=DIRECTION('center_axis',(6.93889390390723E-18,1.,2.22049474265475E-16));
#109248=DIRECTION('ref_axis',(0.627860970415715,1.6821560979169E-16,-0.77832551148516));
#109249=DIRECTION('center_axis',(-6.93889390390723E-18,-1.,-2.22049474265475E-16));
#109250=DIRECTION('ref_axis',(0.627860970415715,1.68470109972568E-16,-0.77832551148516));
#109251=DIRECTION('center_axis',(-0.98636834994651,0.,-0.164552357089771));
#109252=DIRECTION('ref_axis',(0.,-1.,0.));
#109253=DIRECTION('center_axis',(6.93889390390723E-18,1.,2.22049474265475E-16));
#109254=DIRECTION('ref_axis',(0.802769817727363,-1.15648231731787E-16,0.596289040437585));
#109255=DIRECTION('center_axis',(-6.93889390390723E-18,-1.,-2.22049474265475E-16));
#109256=DIRECTION('ref_axis',(0.802769817727363,-1.37976002533899E-16,0.596289040437585));
#109257=DIRECTION('center_axis',(-6.93889390390723E-18,-1.,-2.22049474265475E-16));
#109258=DIRECTION('ref_axis',(0.,1.57234772945449E-16,-1.));
#109259=DIRECTION('center_axis',(-0.899591968564471,0.,-0.436731370632223));
#109260=DIRECTION('ref_axis',(0.,-1.,0.));
#109261=DIRECTION('center_axis',(6.93889390390723E-18,1.,2.22049474265475E-16));
#109262=DIRECTION('ref_axis',(-0.303756589059817,-2.08827432818175E-16,
0.952749670481573));
#109263=DIRECTION('center_axis',(-6.93889390390723E-18,-1.,-2.22049474265475E-16));
#109264=DIRECTION('ref_axis',(-0.303756589059817,-2.09449828692939E-16,
0.952749670481573));
#109265=DIRECTION('center_axis',(-6.93889390390723E-18,-1.,-2.22049474265475E-16));
#109266=DIRECTION('ref_axis',(0.,3.86164530304402E-16,-1.));
#109267=DIRECTION('center_axis',(-0.351876296299399,0.,-0.9360465117197));
#109268=DIRECTION('ref_axis',(0.,-1.,0.));
#109269=DIRECTION('center_axis',(6.93889390390723E-18,1.,2.22049474265475E-16));
#109270=DIRECTION('ref_axis',(-0.739004663706429,-1.43303243667649E-16,
0.673700309499815));
#109271=DIRECTION('center_axis',(-6.93889390390723E-18,-1.,-2.22049474265475E-16));
#109272=DIRECTION('ref_axis',(-0.739004663706429,-1.4446692458097E-16,0.673700309499816));
#109273=DIRECTION('center_axis',(6.93889390390723E-18,1.,2.22049474265475E-16));
#109274=DIRECTION('ref_axis',(-0.983881728593356,0.,0.178820424281317));
#109275=DIRECTION('center_axis',(-6.93889390390723E-18,-1.,-2.22049474265475E-16));
#109276=DIRECTION('ref_axis',(-0.983881728593356,-3.28799302708935E-17,
0.178820424281317));
#109277=DIRECTION('center_axis',(0.,-1.,-2.39272203583008E-16));
#109278=DIRECTION('ref_axis',(0.983984869082392,4.26507501169509E-17,-0.178252005365741));
#109279=DIRECTION('',(0.,-1.,-2.39272203583008E-16));
#109280=DIRECTION('center_axis',(0.,1.,2.22044604925031E-16));
#109281=DIRECTION('ref_axis',(0.983984869082392,4.26507501169509E-17,-0.178252005365741));
#109282=DIRECTION('',(0.,-1.,-2.39272203583008E-16));
#109283=DIRECTION('center_axis',(0.,1.,2.39272203583008E-16));
#109284=DIRECTION('ref_axis',(0.802769817727364,0.,0.596289040437585));
#109285=DIRECTION('',(0.,1.,2.22044604925031E-16));
#109286=DIRECTION('center_axis',(0.,1.,2.22044604925031E-16));
#109287=DIRECTION('ref_axis',(0.802769817727364,0.,0.596289040437585));
#109288=DIRECTION('center_axis',(0.,1.,2.22044604925031E-16));
#109289=DIRECTION('ref_axis',(-0.436731370632224,-1.99749543253629E-16,
0.89959196856447));
#109290=DIRECTION('',(0.,1.,3.21803775253669E-16));
#109291=DIRECTION('center_axis',(0.,-1.,-2.22044604925031E-16));
#109292=DIRECTION('ref_axis',(-0.436731370632224,-1.99749543253629E-16,
0.89959196856447));
#109293=DIRECTION('',(0.,1.,2.22044604925031E-16));
#109294=DIRECTION('center_axis',(0.,-1.,-2.22044604925031E-16));
#109295=DIRECTION('ref_axis',(-0.436731370632224,-1.99749543253629E-16,
0.89959196856447));
#109296=DIRECTION('center_axis',(0.,1.,2.22044604925031E-16));
#109297=DIRECTION('ref_axis',(0.17741935483871,2.18521943337466E-16,-0.98413534258689));
#109298=DIRECTION('',(0.,-1.,-2.22044604925031E-16));
#109299=DIRECTION('center_axis',(0.,1.,2.22044604925031E-16));
#109300=DIRECTION('ref_axis',(0.17741935483871,2.18521943337466E-16,-0.98413534258689));
#109301=DIRECTION('',(0.,-1.,-2.22044604925031E-16));
#109302=DIRECTION('center_axis',(1.00839335745948E-17,-0.819152044288994,
-0.573576436351042));
#109303=DIRECTION('ref_axis',(4.94261663173048E-17,0.573576436351042,-0.819152044288994));
#109304=DIRECTION('',(0.,-1.,-2.22044604925031E-16));
#109305=DIRECTION('center_axis',(0.,1.,2.22044604925031E-16));
#109306=DIRECTION('ref_axis',(0.17741935483871,2.18521943337466E-16,-0.98413534258689));
#109307=DIRECTION('center_axis',(-4.78544407166016E-17,1.,9.47442360904155E-17));
#109308=DIRECTION('ref_axis',(-0.983881728593356,0.,0.178820424281317));
#109309=DIRECTION('',(-4.78544407166016E-17,1.,9.47442360904155E-17));
#109310=DIRECTION('center_axis',(0.,1.,2.22044604925031E-16));
#109311=DIRECTION('ref_axis',(-0.983881728593356,0.,0.178820424281317));
#109312=DIRECTION('center_axis',(1.,4.78544407166016E-17,-2.04853783127104E-16));
#109313=DIRECTION('ref_axis',(2.04853783127104E-16,-2.28983498828938E-16,
1.));
#109314=DIRECTION('',(4.78544407166016E-17,-1.,-6.12536841172497E-17));
#109315=DIRECTION('',(-2.04853783127104E-16,2.22044604925031E-16,-1.));
#109316=DIRECTION('center_axis',(6.93889390390723E-18,1.,2.22049474265475E-16));
#109317=DIRECTION('ref_axis',(-1.,6.93889390390723E-18,1.83750175990302E-19));
#109318=DIRECTION('center_axis',(2.21497401043431E-17,-1.,-2.22049474265426E-16));
#109319=DIRECTION('ref_axis',(0.,2.85358528417711E-16,-1.));
#109320=DIRECTION('center_axis',(-2.21497401043431E-17,1.,2.22049474265426E-16));
#109321=DIRECTION('ref_axis',(-0.095969134594036,2.18898871406418E-16,-0.995384310306965));
#109322=DIRECTION('center_axis',(-0.981030928551421,0.,0.193851276048257));
#109323=DIRECTION('ref_axis',(0.,-1.,0.));
#109324=DIRECTION('center_axis',(2.21497401043431E-17,-1.,-2.22049474265426E-16));
#109325=DIRECTION('ref_axis',(-0.095969134594036,2.20376887935251E-16,-0.995384310306965));
#109326=DIRECTION('center_axis',(0.113781875054763,0.,-0.993505754844441));
#109327=DIRECTION('ref_axis',(0.,-1.,0.));
#109328=DIRECTION('center_axis',(-2.21497401043431E-17,1.,2.22049474265426E-16));
#109329=DIRECTION('ref_axis',(-0.677875792531132,-1.15648231731787E-16,
0.73517644814037));
#109330=DIRECTION('center_axis',(2.21497401043431E-17,-1.,-2.22049474265426E-16));
#109331=DIRECTION('ref_axis',(-0.677875792531132,-1.78260316429482E-16,
0.73517644814037));
#109332=DIRECTION('center_axis',(-2.21497401043431E-17,1.,2.22049474265426E-16));
#109333=DIRECTION('ref_axis',(0.,0.,1.));
#109334=DIRECTION('center_axis',(-0.368421052641889,0.,-0.92965903855674));
#109335=DIRECTION('ref_axis',(0.,-1.,0.));
#109336=DIRECTION('center_axis',(2.21497401043431E-17,-1.,-2.22049474265426E-16));
#109337=DIRECTION('ref_axis',(0.991347881177066,4.33680868994202E-17,-0.131260727126366));
#109338=DIRECTION('center_axis',(-2.21497401043431E-17,1.,2.22049474265426E-16));
#109339=DIRECTION('ref_axis',(0.991347881177066,5.11044733711702E-17,-0.131260727126366));
#109340=DIRECTION('center_axis',(1.,0.,1.68753899743024E-12));
#109341=DIRECTION('ref_axis',(0.,-1.,0.));
#109342=DIRECTION('center_axis',(-2.21497401043431E-17,1.,2.22049474265426E-16));
#109343=DIRECTION('ref_axis',(-0.827170191871152,1.15648231731787E-16,-0.56195148694513));
#109344=DIRECTION('center_axis',(2.21497401043431E-17,-1.,-2.22049474265426E-16));
#109345=DIRECTION('ref_axis',(-0.827170191871151,1.06459427466835E-16,-0.56195148694513));
#109346=DIRECTION('center_axis',(1.,2.21497401039684E-17,1.68718058920808E-12));
#109347=DIRECTION('ref_axis',(1.19327026859967E-12,-0.707106781186548,-0.707106781186548));
#109348=DIRECTION('',(-1.,-2.21497401039684E-17,-1.68718058920808E-12));
#109349=DIRECTION('',(1.,2.21497401039684E-17,1.68718058920808E-12));
#109350=DIRECTION('center_axis',(-0.707106781185951,0.,-0.707106781187144));
#109351=DIRECTION('ref_axis',(-0.707106781187144,0.,0.707106781185951));
#109352=DIRECTION('center_axis',(0.,0.,-1.));
#109353=DIRECTION('ref_axis',(0.719344700989996,-0.694653295650148,0.));
#109354=DIRECTION('',(4.9183381452852E-33,-2.22049474265426E-16,1.));
#109355=DIRECTION('',(0.,0.,-1.));
#109356=DIRECTION('center_axis',(-1.68718058920808E-12,-1.77635683940025E-16,
1.));
#109357=DIRECTION('ref_axis',(0.719344700989996,-0.694653295650148,0.));
#109358=DIRECTION('center_axis',(0.,1.,1.77635683940025E-16));
#109359=DIRECTION('ref_axis',(-0.827170191871152,0.,-0.561951486945128));
#109360=DIRECTION('',(0.,1.,1.77635683940025E-16));
#109361=DIRECTION('center_axis',(0.,1.,2.22044604925031E-16));
#109362=DIRECTION('ref_axis',(-0.827170191871152,0.,-0.561951486945128));
#109363=DIRECTION('',(0.,-1.,-1.77635683940025E-16));
#109364=DIRECTION('center_axis',(1.68718058920808E-12,1.77635683940025E-16,
-1.));
#109365=DIRECTION('ref_axis',(1.,2.21497401039684E-17,1.68718058920808E-12));
#109366=DIRECTION('center_axis',(1.68718058920808E-12,1.77635683940025E-16,
-1.));
#109367=DIRECTION('ref_axis',(-1.,-1.20024110770287E-15,-1.68709743142951E-12));
#109368=DIRECTION('',(0.,1.,1.77635683940025E-16));
#109369=DIRECTION('center_axis',(-1.68718058920808E-12,-1.77635683940025E-16,
1.));
#109370=DIRECTION('ref_axis',(1.,1.49541069999345E-33,0.));
#109371=DIRECTION('',(-3.81426075461834E-28,-1.,-1.77635683940025E-16));
#109372=DIRECTION('',(1.,-3.7462934736789E-28,1.68718058920808E-12));
#109373=DIRECTION('center_axis',(-1.68718058920808E-12,-1.77635683940025E-16,
1.));
#109374=DIRECTION('ref_axis',(-0.441505993976003,-0.897258300203047,-7.45059728147161E-13));
#109375=DIRECTION('',(1.,-3.7462934736789E-28,1.68718058920808E-12));
#109376=DIRECTION('center_axis',(0.,0.,1.));
#109377=DIRECTION('ref_axis',(-1.,-1.20024110770287E-15,0.));
#109378=DIRECTION('',(0.,0.,1.));
#109379=DIRECTION('center_axis',(-2.21497401043431E-17,1.,2.22049474265426E-16));
#109380=DIRECTION('ref_axis',(-1.,-2.21497401043431E-17,1.83750175990296E-19));
#109381=DIRECTION('center_axis',(0.,-1.,-1.77635683940025E-16));
#109382=DIRECTION('ref_axis',(0.835709485407066,9.75525066900838E-17,-0.549171790973149));
#109383=DIRECTION('',(0.,-1.,-1.77635683940025E-16));
#109384=DIRECTION('center_axis',(0.,1.,2.22044604925031E-16));
#109385=DIRECTION('ref_axis',(0.835709485407066,9.75525066900838E-17,-0.549171790973149));
#109386=DIRECTION('',(0.,-1.,-1.77635683940025E-16));
#109387=DIRECTION('',(0.,1.,1.77635683940025E-16));
#109388=DIRECTION('center_axis',(0.,1.,2.22044604925031E-16));
#109389=DIRECTION('ref_axis',(0.835709485407066,9.75525066900838E-17,-0.549171790973149));
#109390=DIRECTION('',(0.,-1.,-1.77635683940025E-16));
#109391=DIRECTION('',(0.,-1.,-1.77635683940025E-16));
#109392=DIRECTION('center_axis',(-1.88260317010131E-12,2.22049474265488E-16,
-1.));
#109393=DIRECTION('ref_axis',(-0.707106781186548,-0.707106781186548,1.33114401262784E-12));
#109394=DIRECTION('center_axis',(1.88321580552043E-12,0.,1.));
#109395=DIRECTION('ref_axis',(-1.,0.,1.88321580552043E-12));
#109396=DIRECTION('',(-1.88260317010131E-12,2.22049474265488E-16,-1.));
#109397=DIRECTION('center_axis',(-1.88182802673963E-12,2.77555756156289E-15,
-1.));
#109398=DIRECTION('ref_axis',(0.,-1.,-2.77555756156289E-15));
#109399=DIRECTION('',(1.88260317010131E-12,-2.22049474265488E-16,1.));
#109400=DIRECTION('center_axis',(6.93889390390723E-18,1.,2.22049474265475E-16));
#109401=DIRECTION('ref_axis',(0.,0.,1.));
#109402=DIRECTION('center_axis',(-0.707106781186549,0.,-0.707106781186546));
#109403=DIRECTION('ref_axis',(0.,-1.,0.));
#109404=DIRECTION('center_axis',(-6.93889390390723E-18,-1.,-2.22049474265475E-16));
#109405=DIRECTION('ref_axis',(0.923879532510926,8.67361737988403E-17,-0.382683432365961));
#109406=DIRECTION('center_axis',(6.93889390390723E-18,1.,2.22049474265475E-16));
#109407=DIRECTION('ref_axis',(0.923879532510926,7.85639529108843E-17,-0.382683432365961));
#109408=DIRECTION('center_axis',(-0.707106781186548,1.61919227945412E-16,
-0.707106781186548));
#109409=DIRECTION('ref_axis',(-0.500000000000002,-0.707106781186548,0.499999999999998));
#109410=DIRECTION('center_axis',(-0.707106781186548,0.,-0.707106781186548));
#109411=DIRECTION('ref_axis',(0.,-1.,0.));
#109412=DIRECTION('',(0.707106781186548,-1.61919227945412E-16,0.707106781186548));
#109413=DIRECTION('',(-0.707106781186548,1.61919227945412E-16,-0.707106781186548));
#109414=DIRECTION('center_axis',(0.760782493872049,0.,-0.649006931409693));
#109415=DIRECTION('ref_axis',(0.,-1.,0.));
#109416=DIRECTION('center_axis',(6.93889390390723E-18,1.,2.22049474265475E-16));
#109417=DIRECTION('ref_axis',(-0.999217609598081,0.,-0.0395495722998017));
#109418=DIRECTION('center_axis',(-6.93889390390723E-18,-1.,-2.22049474265475E-16));
#109419=DIRECTION('ref_axis',(-0.999217609598081,1.57154267165122E-17,-0.0395495722998017));
#109420=DIRECTION('center_axis',(-6.93889390390723E-18,-1.,-2.22049474265475E-16));
#109421=DIRECTION('ref_axis',(0.,3.86164530304402E-16,-1.));
#109422=DIRECTION('center_axis',(0.787785770581038,0.,-0.615949332063962));
#109423=DIRECTION('ref_axis',(0.,-1.,0.));
#109424=DIRECTION('center_axis',(6.93889390390723E-18,1.,2.22049474265475E-16));
#109425=DIRECTION('ref_axis',(-0.632622226422346,1.81014623580189E-16,-0.774460533943747));
#109426=DIRECTION('center_axis',(-6.93889390390723E-18,-1.,-2.22049474265475E-16));
#109427=DIRECTION('ref_axis',(-0.632622226422346,1.76358252911966E-16,-0.774460533943748));
#109428=DIRECTION('center_axis',(0.499999999999996,0.,0.866025403784441));
#109429=DIRECTION('ref_axis',(0.,-1.,0.));
#109430=DIRECTION('center_axis',(6.93889390390723E-18,1.,2.22049474265475E-16));
#109431=DIRECTION('ref_axis',(0.190629674628629,2.31296463463575E-16,-0.981662022872935));
#109432=DIRECTION('center_axis',(-6.93889390390723E-18,-1.,-2.22049474265475E-16));
#109433=DIRECTION('ref_axis',(0.190629674628629,2.16654776998133E-16,-0.981662022872935));
#109434=DIRECTION('center_axis',(0.5,-1.95769932562834E-16,0.866025403784439));
#109435=DIRECTION('ref_axis',(0.612372435695796,-0.707106781186546,-0.353553390593273));
#109436=DIRECTION('center_axis',(0.500000000000001,0.,0.866025403784438));
#109437=DIRECTION('ref_axis',(0.,-1.,0.));
#109438=DIRECTION('',(-0.5,1.95769932562834E-16,-0.866025403784439));
#109439=DIRECTION('',(0.5,-1.95769932562834E-16,0.866025403784439));
#109440=DIRECTION('center_axis',(-0.681760298603169,0.,0.73157562510551));
#109441=DIRECTION('ref_axis',(0.,-1.,0.));
#109442=DIRECTION('center_axis',(6.93889390390723E-18,1.,2.22049474265475E-16));
#109443=DIRECTION('ref_axis',(0.993590264000317,0.,0.113041529022662));
#109444=DIRECTION('center_axis',(-6.93889390390723E-18,-1.,-2.22049474265475E-16));
#109445=DIRECTION('ref_axis',(0.993590264000317,-3.19952295155008E-17,0.113041529022662));
#109446=DIRECTION('center_axis',(6.93889390390723E-18,1.,2.22049474265475E-16));
#109447=DIRECTION('ref_axis',(0.,0.,1.));
#109448=DIRECTION('center_axis',(0.681760298603169,0.,0.73157562510551));
#109449=DIRECTION('ref_axis',(0.,-1.,0.));
#109450=DIRECTION('center_axis',(-6.93889390390723E-18,-1.,-2.22049474265475E-16));
#109451=DIRECTION('ref_axis',(-1.,0.,-1.33226206458968E-16));
#109452=DIRECTION('center_axis',(-6.93889390390723E-18,-1.,-2.22049474265475E-16));
#109453=DIRECTION('ref_axis',(-1.,0.,-1.33226206458968E-16));
#109454=DIRECTION('center_axis',(6.93889390390723E-18,1.,2.22049474265475E-16));
#109455=DIRECTION('ref_axis',(-1.,6.93889390390726E-18,-1.33226206458968E-16));
#109456=DIRECTION('center_axis',(-0.500000000000002,-2.25347189810573E-16,
0.866025403784438));
#109457=DIRECTION('ref_axis',(0.,-1.,-2.60208521396521E-16));
#109458=DIRECTION('center_axis',(6.93889390390723E-18,1.,2.22049474265475E-16));
#109459=DIRECTION('ref_axis',(0.993590264000317,0.,-0.113041529022662));
#109460=DIRECTION('center_axis',(-6.93889390390723E-18,-1.,-2.22049474265475E-16));
#109461=DIRECTION('ref_axis',(0.993590264000316,1.82063946637941E-17,-0.113041529022662));
#109462=DIRECTION('center_axis',(-0.5,-1.88831038658927E-16,0.866025403784439));
#109463=DIRECTION('ref_axis',(0.612372435695792,-0.70710678118655,0.353553390593273));
#109464=DIRECTION('center_axis',(-0.500000000000002,0.,0.866025403784438));
#109465=DIRECTION('ref_axis',(0.,-1.,0.));
#109466=DIRECTION('',(0.5,1.88831038658927E-16,-0.866025403784439));
#109467=DIRECTION('',(-0.5,-1.88831038658927E-16,0.866025403784439));
#109468=DIRECTION('center_axis',(6.93889390390723E-18,1.,2.22049474265475E-16));
#109469=DIRECTION('ref_axis',(-0.258819045101613,-1.7347234759768E-16,0.965925826289312));
#109470=DIRECTION('center_axis',(-6.93889390390723E-18,-1.,-2.22049474265475E-16));
#109471=DIRECTION('ref_axis',(-0.258819045101613,-2.12687404012715E-16,
0.965925826289312));
#109472=DIRECTION('center_axis',(0.,-1.,-2.22044604925031E-16));
#109473=DIRECTION('ref_axis',(0.993590264000317,0.,0.113041529022661));
#109474=DIRECTION('',(0.,1.,2.22044604925031E-16));
#109475=DIRECTION('center_axis',(0.,-1.,-2.22044604925031E-16));
#109476=DIRECTION('ref_axis',(0.993590264000317,0.,0.113041529022661));
#109477=DIRECTION('',(1.32618116302315E-17,-1.,-2.29701315439687E-16));
#109478=DIRECTION('center_axis',(0.,1.,2.22044604925031E-16));
#109479=DIRECTION('ref_axis',(1.,0.,0.));
#109480=DIRECTION('center_axis',(0.,1.,2.22044604925031E-16));
#109481=DIRECTION('ref_axis',(1.,0.,0.));
#109482=DIRECTION('',(0.,-1.,-2.22044604925031E-16));
#109483=DIRECTION('',(0.,-1.,-2.22044604925031E-16));
#109484=DIRECTION('center_axis',(0.,1.,2.22044604925031E-16));
#109485=DIRECTION('ref_axis',(1.,0.,0.));
#109486=DIRECTION('',(0.,1.,2.22044604925031E-16));
#109487=DIRECTION('center_axis',(-6.93889390390723E-18,-1.,-2.22049474265475E-16));
#109488=DIRECTION('ref_axis',(0.5,-1.98254111540207E-16,0.866025403784439));
#109489=DIRECTION('',(0.,-1.,-2.22044604925031E-16));
#109490=DIRECTION('center_axis',(0.,1.,2.22044604925031E-16));
#109491=DIRECTION('ref_axis',(1.,0.,0.));
#109492=DIRECTION('',(0.,1.,2.22044604925031E-16));
#109493=DIRECTION('center_axis',(-6.93889390390723E-18,-1.,-2.22049474265475E-16));
#109494=DIRECTION('ref_axis',(0.5,1.98254111540207E-16,-0.866025403784438));
#109495=DIRECTION('',(0.,-1.,-2.22044604925031E-16));
#109496=DIRECTION('center_axis',(0.,1.,2.22044604925031E-16));
#109497=DIRECTION('ref_axis',(1.,0.,0.));
#109498=DIRECTION('center_axis',(0.,-1.,-2.22044604925031E-16));
#109499=DIRECTION('ref_axis',(0.993590264000316,0.,-0.113041529022664));
#109500=DIRECTION('',(1.32618116302315E-17,1.,2.29701315439688E-16));
#109501=DIRECTION('center_axis',(0.,-1.,-2.22044604925031E-16));
#109502=DIRECTION('ref_axis',(0.993590264000316,0.,-0.113041529022664));
#109503=DIRECTION('center_axis',(0.866025403784439,-1.26335723491828E-16,
0.5));
#109504=DIRECTION('ref_axis',(-0.5,-1.95761498617786E-16,0.866025403784439));
#109505=DIRECTION('',(-1.15316379899143E-28,-1.,-2.52671446983456E-16));
#109506=DIRECTION('',(0.5,1.92296268638356E-16,-0.866025403784439));
#109507=DIRECTION('center_axis',(-1.15316379899143E-28,-1.,-2.52671446983456E-16));
#109508=DIRECTION('ref_axis',(0.866025403784439,0.,0.5));
#109509=DIRECTION('',(1.15316379899143E-28,1.,2.52671446983456E-16));
#109510=DIRECTION('center_axis',(0.,-1.,-2.22044604925031E-16));
#109511=DIRECTION('ref_axis',(0.866025403784439,0.,0.5));
#109512=DIRECTION('center_axis',(1.,3.60363687185997E-28,-1.88260317010131E-12));
#109513=DIRECTION('ref_axis',(-1.88260317010131E-12,2.22049474265488E-16,
-1.));
#109514=DIRECTION('',(0.,1.,1.91417762866406E-16));
#109515=DIRECTION('',(-1.88260317010131E-12,2.22044604925031E-16,-1.));
#109516=DIRECTION('center_axis',(6.93889390390723E-18,1.,2.22049474265475E-16));
#109517=DIRECTION('ref_axis',(-1.,6.93889390390723E-18,1.83750175990302E-19));
#109518=DIRECTION('center_axis',(-6.93889390390723E-18,-1.,-2.22049474265475E-16));
#109519=DIRECTION('ref_axis',(0.,3.86164530304402E-16,-1.));
#109520=DIRECTION('center_axis',(-6.93889390390723E-18,-1.,-2.22049474265475E-16));
#109521=DIRECTION('ref_axis',(0.828643266372963,1.18548330240756E-16,-0.559777042307691));
#109522=DIRECTION('center_axis',(0.319238463372312,0.,0.947674418512859));
#109523=DIRECTION('ref_axis',(0.,-1.,0.));
#109524=DIRECTION('center_axis',(6.93889390390723E-18,1.,2.22049474265475E-16));
#109525=DIRECTION('ref_axis',(0.828643266372963,1.13134139737618E-16,-0.559777042307691));
#109526=DIRECTION('center_axis',(0.,0.,1.));
#109527=DIRECTION('ref_axis',(0.,-1.,0.));
#109528=DIRECTION('center_axis',(6.93889390390723E-18,1.,2.22049474265475E-16));
#109529=DIRECTION('ref_axis',(0.98683190526879,0.,-0.161749159947031));
#109530=DIRECTION('center_axis',(-6.93889390390723E-18,-1.,-2.22049474265475E-16));
#109531=DIRECTION('ref_axis',(0.98683190526879,2.90687940374697E-17,-0.161749159947031));
#109532=DIRECTION('center_axis',(-2.10803227901262E-16,-2.22049474265475E-16,
1.));
#109533=DIRECTION('ref_axis',(0.707106781186547,-0.707106781186548,0.));
#109534=DIRECTION('center_axis',(0.,0.,1.));
#109535=DIRECTION('ref_axis',(0.,-1.,0.));
#109536=DIRECTION('',(2.10803227901262E-16,2.22049474265475E-16,-1.));
#109537=DIRECTION('',(-2.10803227901262E-16,-2.22049474265475E-16,1.));
#109538=DIRECTION('center_axis',(-1.,0.,-3.46944695195361E-16));
#109539=DIRECTION('ref_axis',(0.,-1.,0.));
#109540=DIRECTION('center_axis',(6.93889390390723E-18,1.,2.22049474265475E-16));
#109541=DIRECTION('ref_axis',(0.707106781186548,-1.15648231731787E-16,0.707106781186547));
#109542=DIRECTION('center_axis',(-6.93889390390723E-18,-1.,-2.22049474265475E-16));
#109543=DIRECTION('ref_axis',(0.707106781186548,-1.61919227945412E-16,0.707106781186547));
#109544=DIRECTION('center_axis',(-1.,6.93889390390728E-18,-2.40389762145677E-16));
#109545=DIRECTION('ref_axis',(0.,-0.707106781186548,0.707106781186548));
#109546=DIRECTION('center_axis',(-1.,0.,0.));
#109547=DIRECTION('ref_axis',(0.,-1.,0.));
#109548=DIRECTION('',(1.,-6.93889390390728E-18,2.40389762145677E-16));
#109549=DIRECTION('',(-1.,6.93889390390728E-18,-2.40389762145677E-16));
#109550=DIRECTION('center_axis',(-0.292682926829268,0.,-0.956209550434764));
#109551=DIRECTION('ref_axis',(0.,-1.,0.));
#109552=DIRECTION('center_axis',(6.93889390390723E-18,1.,2.22049474265475E-16));
#109553=DIRECTION('ref_axis',(-0.594691967816421,-2.31296463463574E-16,
0.803953645065829));
#109554=DIRECTION('center_axis',(-6.93889390390723E-18,-1.,-2.22049474265475E-16));
#109555=DIRECTION('ref_axis',(-0.59469196781642,-1.74390979750496E-16,0.803953645065829));
#109556=DIRECTION('center_axis',(6.93889390390723E-18,1.,2.22049474265475E-16));
#109557=DIRECTION('ref_axis',(0.5,0.,-0.866025403784439));
#109558=DIRECTION('center_axis',(-0.974443225432437,0.,0.224633925329253));
#109559=DIRECTION('ref_axis',(0.,-1.,0.));
#109560=DIRECTION('center_axis',(6.93889390390723E-18,1.,2.22049474265475E-16));
#109561=DIRECTION('ref_axis',(0.5,1.88831038658927E-16,-0.866025403784438));
#109562=DIRECTION('center_axis',(-0.500000000000001,0.,-0.866025403784438));
#109563=DIRECTION('ref_axis',(0.,-1.,0.));
#109564=DIRECTION('center_axis',(6.93889390390723E-18,1.,2.22049474265475E-16));
#109565=DIRECTION('ref_axis',(-0.398898296183895,-2.31296463463574E-16,
0.916995174088493));
#109566=DIRECTION('center_axis',(-6.93889390390723E-18,-1.,-2.22049474265475E-16));
#109567=DIRECTION('ref_axis',(-0.398898296183895,-2.00850383354658E-16,
0.916995174088493));
#109568=DIRECTION('center_axis',(-0.5,1.95769932562834E-16,-0.866025403784439));
#109569=DIRECTION('ref_axis',(-0.612372435695794,-0.707106781186549,0.353553390593272));
#109570=DIRECTION('center_axis',(-0.500000000000001,0.,-0.866025403784438));
#109571=DIRECTION('ref_axis',(0.,-1.,0.));
#109572=DIRECTION('',(0.5,-1.95769932562834E-16,0.866025403784439));
#109573=DIRECTION('',(-0.5,1.95769932562834E-16,-0.866025403784439));
#109574=DIRECTION('center_axis',(0.927320654301968,0.,-0.374267824031094));
#109575=DIRECTION('ref_axis',(0.,-1.,0.));
#109576=DIRECTION('center_axis',(6.93889390390723E-18,1.,2.22049474265475E-16));
#109577=DIRECTION('ref_axis',(-0.945459087052697,1.15648231731787E-16,-0.325740870492914));
#109578=DIRECTION('center_axis',(-6.93889390390723E-18,-1.,-2.22049474265475E-16));
#109579=DIRECTION('ref_axis',(-0.945459087052697,7.88910293352734E-17,-0.325740870492914));
#109580=DIRECTION('center_axis',(-6.93889390390723E-18,-1.,-2.22049474265475E-16));
#109581=DIRECTION('ref_axis',(0.,3.86164530304402E-16,-1.));
#109582=DIRECTION('center_axis',(6.93889390390723E-18,1.,2.22049474265475E-16));
#109583=DIRECTION('ref_axis',(-0.185745985401917,2.18726003492728E-16,-0.982597796103304));
#109584=DIRECTION('center_axis',(-6.93889390390723E-18,-1.,-2.22049474265475E-16));
#109585=DIRECTION('ref_axis',(-0.185745985401917,2.19474195724934E-16,-0.982597796103304));
#109586=DIRECTION('center_axis',(6.93889390390723E-18,1.,2.22049474265475E-16));
#109587=DIRECTION('ref_axis',(0.,0.,1.));
#109588=DIRECTION('center_axis',(-6.93889390390723E-18,-1.,-2.22049474265475E-16));
#109589=DIRECTION('ref_axis',(-0.351073082383137,-2.08550719155025E-16,
0.936348060726354));
#109590=DIRECTION('center_axis',(6.93889390390723E-18,1.,2.22049474265475E-16));
#109591=DIRECTION('ref_axis',(-0.351073082383137,-2.05479535742609E-16,
0.936348060726354));
#109592=DIRECTION('center_axis',(-0.866025403784439,-1.26335723491828E-16,
0.5));
#109593=DIRECTION('ref_axis',(-0.5,1.88822604713879E-16,-0.866025403784439));
#109594=DIRECTION('',(1.4340744877117E-17,-1.,-2.27832548238107E-16));
#109595=DIRECTION('',(0.5,-1.92296268638356E-16,0.866025403784439));
#109596=DIRECTION('',(-1.32618116302315E-17,1.,2.29701315439687E-16));
#109597=DIRECTION('center_axis',(-1.4340744877117E-17,1.,2.27832548238107E-16));
#109598=DIRECTION('ref_axis',(-0.945459087052698,0.,-0.325740870492911));
#109599=DIRECTION('',(0.,1.,2.22044604925031E-16));
#109600=DIRECTION('center_axis',(0.,1.,2.22044604925031E-16));
#109601=DIRECTION('ref_axis',(-0.945459087052698,0.,-0.325740870492911));
#109602=DIRECTION('center_axis',(1.,0.,0.));
#109603=DIRECTION('ref_axis',(0.,-1.,0.));
#109604=DIRECTION('center_axis',(0.,1.,2.22044604925031E-16));
#109605=DIRECTION('ref_axis',(1.,0.,0.));
#109606=DIRECTION('',(0.,-1.,-2.22044604925031E-16));
#109607=DIRECTION('center_axis',(0.,1.,2.22044604925031E-16));
#109608=DIRECTION('ref_axis',(1.,0.,0.));
#109609=DIRECTION('',(0.,-1.,-2.22044604925031E-16));
#109610=DIRECTION('center_axis',(0.,-1.,-2.22044604925031E-16));
#109611=DIRECTION('ref_axis',(1.,0.,0.));
#109612=DIRECTION('',(0.,-1.,-2.22044604925031E-16));
#109613=DIRECTION('center_axis',(-2.37859513600921E-17,0.866025403784432,
0.500000000000011));
#109614=DIRECTION('ref_axis',(0.,0.500000000000011,-0.866025403784432));
#109615=DIRECTION('center_axis',(1.51594548245566E-16,-0.819152044288998,
0.573576436351038));
#109616=DIRECTION('ref_axis',(0.,-0.573576436351038,-0.819152044288998));
#109617=DIRECTION('center_axis',(1.51594548245566E-16,-0.819152044288998,
0.573576436351038));
#109618=DIRECTION('ref_axis',(0.,-0.573576436351038,-0.819152044288998));
#109619=DIRECTION('',(0.,-1.,-2.22044604925031E-16));
#109620=DIRECTION('center_axis',(0.,-1.,-2.22044604925031E-16));
#109621=DIRECTION('ref_axis',(1.,0.,0.));
#109622=DIRECTION('',(0.,1.,2.22044604925031E-16));
#109623=DIRECTION('center_axis',(0.,-1.,-2.22044604925031E-16));
#109624=DIRECTION('ref_axis',(1.,0.,0.));
#109625=DIRECTION('',(0.,1.,2.22044604925031E-16));
#109626=DIRECTION('center_axis',(6.93889390390723E-18,1.,2.22049474265475E-16));
#109627=DIRECTION('ref_axis',(-1.,6.93889390390723E-18,1.83750175990302E-19));
#109628=DIRECTION('center_axis',(-6.93889390390723E-18,-1.,-2.22049474265475E-16));
#109629=DIRECTION('ref_axis',(0.417899232327897,-3.86164530304402E-16,0.908493385567421));
#109630=DIRECTION('center_axis',(0.319238463372311,0.,-0.947674418512859));
#109631=DIRECTION('ref_axis',(0.947674418512859,0.,0.319238463372311));
#109632=DIRECTION('center_axis',(-6.93889390390723E-18,-1.,-2.22049474265475E-16));
#109633=DIRECTION('ref_axis',(0.417899232327897,-2.04630237074555E-16,0.908493385567421));
#109634=DIRECTION('center_axis',(-0.927320654301968,0.,-0.374267824031094));
#109635=DIRECTION('ref_axis',(0.,-1.,0.));
#109636=DIRECTION('center_axis',(6.93889390390723E-18,1.,2.22049474265475E-16));
#109637=DIRECTION('ref_axis',(0.417899232327897,-2.03641451527712E-16,0.908493385567421));
#109638=DIRECTION('center_axis',(0.500000000000001,0.,-0.866025403784438));
#109639=DIRECTION('ref_axis',(0.,-1.,0.));
#109640=DIRECTION('center_axis',(6.93889390390723E-18,1.,2.22049474265475E-16));
#109641=DIRECTION('ref_axis',(-0.945459087052697,-1.15648231731787E-16,
0.325740870492914));
#109642=DIRECTION('center_axis',(-6.93889390390723E-18,-1.,-2.22049474265475E-16));
#109643=DIRECTION('ref_axis',(-0.945459087052697,-6.5770148744186E-17,0.325740870492914));
#109644=DIRECTION('center_axis',(0.5,1.88831038658927E-16,-0.866025403784439));
#109645=DIRECTION('ref_axis',(-0.612372435695796,-0.707106781186547,-0.353553390593273));
#109646=DIRECTION('center_axis',(0.499999999999999,3.00462919747432E-16,
-0.866025403784439));
#109647=DIRECTION('ref_axis',(0.,-1.,-3.46944695195361E-16));
#109648=DIRECTION('',(-0.5,-1.88831038658927E-16,0.866025403784439));
#109649=DIRECTION('',(0.5,1.88831038658927E-16,-0.866025403784439));
#109650=DIRECTION('center_axis',(0.974443225432437,-1.55871097507791E-16,
0.224633925329254));
#109651=DIRECTION('ref_axis',(0.,-1.,-6.93889390390722E-16));
#109652=DIRECTION('center_axis',(6.93889390390723E-18,1.,2.22049474265475E-16));
#109653=DIRECTION('ref_axis',(-0.398898296183895,2.31296463463574E-16,-0.916995174088493));
#109654=DIRECTION('center_axis',(-6.93889390390723E-18,-1.,-2.22049474265475E-16));
#109655=DIRECTION('ref_axis',(-0.398898296183895,2.06386209265997E-16,-0.916995174088493));
#109656=DIRECTION('center_axis',(6.93889390390723E-18,1.,2.22049474265475E-16));
#109657=DIRECTION('ref_axis',(0.,0.,1.));
#109658=DIRECTION('center_axis',(0.292682926829268,0.,-0.956209550434764));
#109659=DIRECTION('ref_axis',(0.,-1.,0.));
#109660=DIRECTION('center_axis',(6.93889390390723E-18,1.,2.22049474265475E-16));
#109661=DIRECTION('ref_axis',(0.5,-1.95769932562834E-16,0.866025403784439));
#109662=DIRECTION('center_axis',(1.,0.,0.));
#109663=DIRECTION('ref_axis',(0.,-1.,0.));
#109664=DIRECTION('center_axis',(6.93889390390723E-18,1.,2.22049474265475E-16));
#109665=DIRECTION('ref_axis',(-0.59469196781642,2.31296463463574E-16,-0.80395364506583));
#109666=DIRECTION('center_axis',(-6.93889390390723E-18,-1.,-2.22049474265475E-16));
#109667=DIRECTION('ref_axis',(-0.59469196781642,1.82643988690864E-16,-0.80395364506583));
#109668=DIRECTION('center_axis',(1.,-6.93889390390728E-18,2.40389762145677E-16));
#109669=DIRECTION('ref_axis',(0.,-0.707106781186548,-0.707106781186547));
#109670=DIRECTION('center_axis',(1.,0.,6.93889390390723E-16));
#109671=DIRECTION('ref_axis',(0.,-1.,0.));
#109672=DIRECTION('',(-1.,6.93889390390728E-18,-2.40389762145677E-16));
#109673=DIRECTION('',(1.,-6.93889390390728E-18,2.40389762145677E-16));
#109674=DIRECTION('center_axis',(0.,0.,1.));
#109675=DIRECTION('ref_axis',(0.,-1.,0.));
#109676=DIRECTION('center_axis',(6.93889390390723E-18,1.,2.22049474265475E-16));
#109677=DIRECTION('ref_axis',(0.707106781186548,1.15648231731787E-16,-0.707106781186547));
#109678=DIRECTION('center_axis',(-6.93889390390723E-18,-1.,-2.22049474265475E-16));
#109679=DIRECTION('ref_axis',(0.707106781186548,1.52106150078638E-16,-0.707106781186547));
#109680=DIRECTION('center_axis',(-2.10803227901262E-16,-2.22049474265475E-16,
1.));
#109681=DIRECTION('ref_axis',(0.707106781186547,-0.707106781186548,0.));
#109682=DIRECTION('center_axis',(-8.67361737988403E-17,0.,1.));
#109683=DIRECTION('ref_axis',(0.,-1.,0.));
#109684=DIRECTION('',(2.10803227901262E-16,2.22049474265475E-16,-1.));
#109685=DIRECTION('',(-2.10803227901262E-16,-2.22049474265475E-16,1.));
#109686=DIRECTION('center_axis',(6.93889390390723E-18,1.,2.22049474265475E-16));
#109687=DIRECTION('ref_axis',(0.986831905268789,0.,0.161749159947033));
#109688=DIRECTION('center_axis',(-6.93889390390723E-18,-1.,-2.22049474265475E-16));
#109689=DIRECTION('ref_axis',(0.986831905268789,-4.27638378207716E-17,0.161749159947033));
#109690=DIRECTION('center_axis',(2.40389762145677E-16,6.12536841172497E-17,
-1.));
#109691=DIRECTION('ref_axis',(1.,6.93889390390718E-18,2.40389762145677E-16));
#109692=DIRECTION('',(4.78544407166015E-17,-1.,-6.12536841172497E-17));
#109693=DIRECTION('',(-1.,5.3377249763659E-32,-2.40389762145677E-16));
#109694=DIRECTION('',(3.86524912081669E-32,1.,6.12536841172497E-17));
#109695=DIRECTION('center_axis',(-4.78544407166015E-17,1.,6.12536841172497E-17));
#109696=DIRECTION('ref_axis',(0.707106781186548,0.,-0.707106781186548));
#109697=DIRECTION('',(-4.78544407166015E-17,1.,6.12536841172497E-17));
#109698=DIRECTION('center_axis',(0.,1.,2.22044604925031E-16));
#109699=DIRECTION('ref_axis',(0.707106781186548,0.,-0.707106781186548));
#109700=DIRECTION('center_axis',(-1.,-4.78544407166015E-17,-2.10803227901262E-16));
#109701=DIRECTION('ref_axis',(2.10803227901262E-16,2.28983498828939E-16,
-1.));
#109702=DIRECTION('',(4.78544407166016E-17,-1.,-3.64102766715121E-16));
#109703=DIRECTION('',(-2.10803227901262E-16,-2.22044604925031E-16,1.));
#109704=DIRECTION('center_axis',(-4.78544407166016E-17,1.,3.64102766715121E-16));
#109705=DIRECTION('ref_axis',(0.98683190526879,0.,0.161749159947033));
#109706=DIRECTION('',(0.,1.,2.22044604925031E-16));
#109707=DIRECTION('center_axis',(0.,1.,2.22044604925031E-16));
#109708=DIRECTION('ref_axis',(0.98683190526879,0.,0.161749159947033));
#109709=DIRECTION('center_axis',(0.,1.,2.22044604925031E-16));
#109710=DIRECTION('ref_axis',(1.,0.,0.));
#109711=DIRECTION('',(0.,-1.,-2.22044604925031E-16));
#109712=DIRECTION('center_axis',(0.,-1.,-2.22044604925031E-16));
#109713=DIRECTION('ref_axis',(1.,0.,0.));
#109714=DIRECTION('',(0.,-1.,-2.22044604925031E-16));
#109715=DIRECTION('center_axis',(0.,-1.,-2.22044604925031E-16));
#109716=DIRECTION('ref_axis',(1.,0.,0.));
#109717=DIRECTION('',(0.,1.,2.22044604925031E-16));
#109718=DIRECTION('center_axis',(1.00839335745948E-17,-0.819152044288994,
-0.573576436351042));
#109719=DIRECTION('ref_axis',(0.,0.573576436351042,-0.819152044288994));
#109720=DIRECTION('center_axis',(-1.47144065207334E-16,0.866025403784436,
-0.500000000000005));
#109721=DIRECTION('ref_axis',(0.,-0.500000000000005,-0.866025403784436));
#109722=DIRECTION('',(0.,1.,2.22044604925031E-16));
#109723=DIRECTION('center_axis',(0.,-1.,-2.22044604925031E-16));
#109724=DIRECTION('ref_axis',(1.,0.,0.));
#109725=DIRECTION('center_axis',(6.93889390390723E-18,1.,2.22049474265475E-16));
#109726=DIRECTION('ref_axis',(-1.,6.93889390390723E-18,1.83750175990302E-19));
#109727=DIRECTION('center_axis',(0.,1.,1.91417762866406E-16));
#109728=DIRECTION('ref_axis',(0.923879532510926,0.,-0.38268343236596));
#109729=DIRECTION('',(-1.74315279842105E-32,1.,1.91417762866406E-16));
#109730=DIRECTION('center_axis',(0.,1.,2.22044604925031E-16));
#109731=DIRECTION('ref_axis',(0.923879532510926,0.,-0.38268343236596));
#109732=DIRECTION('center_axis',(0.707106781186548,1.35352798162394E-16,
-0.707106781186548));
#109733=DIRECTION('ref_axis',(-0.707106781186548,1.61919227945412E-16,-0.707106781186548));
#109734=DIRECTION('',(-1.65275500460854E-17,-1.,-2.07945312912492E-16));
#109735=DIRECTION('',(-0.707106781186548,1.57009245868377E-16,-0.707106781186548));
#109736=DIRECTION('center_axis',(1.65275500460854E-17,1.,2.07945312912492E-16));
#109737=DIRECTION('ref_axis',(-0.999217609598081,0.,-0.0395495722997975));
#109738=DIRECTION('center_axis',(0.,1.,2.22044604925031E-16));
#109739=DIRECTION('ref_axis',(-0.999217609598081,0.,-0.0395495722997975));
#109740=DIRECTION('center_axis',(0.,1.,1.77635683940025E-16));
#109741=DIRECTION('ref_axis',(-0.677875792531128,0.,0.735176448140373));
#109742=DIRECTION('',(0.,1.,1.77635683940025E-16));
#109743=DIRECTION('center_axis',(0.,1.,2.22044604925031E-16));
#109744=DIRECTION('ref_axis',(-0.677875792531128,0.,0.735176448140373));
#109745=DIRECTION('center_axis',(0.,-1.,-1.77635683940025E-16));
#109746=DIRECTION('ref_axis',(0.991347881177066,2.3316589037557E-17,-0.131260727126366));
#109747=DIRECTION('center_axis',(0.,1.,2.22044604925031E-16));
#109748=DIRECTION('ref_axis',(-1.,0.,1.83750175990301E-19));
#109749=DIRECTION('center_axis',(2.89174624745853E-28,1.,2.27504718161182E-16));
#109750=DIRECTION('ref_axis',(-0.707106781186546,0.,0.707106781186549));
#109751=DIRECTION('center_axis',(0.,-1.,-2.22044604925031E-16));
#109752=DIRECTION('ref_axis',(-0.707106781186546,0.,0.707106781186549));
#109753=DIRECTION('',(2.89174624745853E-28,1.,2.27504718161182E-16));
#109754=DIRECTION('center_axis',(0.,-1.,-2.22044604925031E-16));
#109755=DIRECTION('ref_axis',(-0.707106781186546,0.,0.707106781186549));
#109756=DIRECTION('',(-2.89174624745853E-28,-1.,-2.27504718161182E-16));
#109757=DIRECTION('center_axis',(0.707106781186548,1.60870128963502E-16,
-0.707106781186548));
#109758=DIRECTION('ref_axis',(-0.707106781186548,1.61919227945507E-16,-0.707106781186548));
#109759=DIRECTION('',(0.707106781186548,-1.57009245868377E-16,0.707106781186548));
#109760=DIRECTION('',(0.707106781186548,-1.57009245868377E-16,0.707106781186548));
#109761=DIRECTION('',(2.09862273058998E-32,1.,2.27504718160893E-16));
#109762=DIRECTION('',(0.707106781186548,-1.57009245868377E-16,0.707106781186548));
#109763=DIRECTION('',(0.,-1.,-2.27504718160893E-16));
#109764=DIRECTION('',(0.707106781186548,-1.57009245868377E-16,0.707106781186548));
#109765=DIRECTION('',(2.73005661793073E-18,-1.,-2.24774661542962E-16));
#109766=DIRECTION('center_axis',(1.,-1.97827874126669E-27,7.42447950166969E-12));
#109767=DIRECTION('ref_axis',(7.42447950166969E-12,2.22049474265423E-16,
-1.));
#109768=DIRECTION('',(-7.42447950166969E-12,-2.22044604925031E-16,1.));
#109769=DIRECTION('',(9.65588433237313E-28,-1.,-3.96508223080413E-16));
#109770=DIRECTION('',(7.42447950166969E-12,2.22049474265423E-16,-1.));
#109771=DIRECTION('center_axis',(0.,-1.,-2.22044604925031E-16));
#109772=DIRECTION('ref_axis',(0.0584478133347438,0.,0.998290465303755));
#109773=DIRECTION('center_axis',(0.,-1.,-2.22044604925031E-16));
#109774=DIRECTION('ref_axis',(0.0584478133347438,0.,0.998290465303755));
#109775=DIRECTION('center_axis',(0.,-1.,-2.22044604925031E-16));
#109776=DIRECTION('ref_axis',(0.0584478133347438,0.,0.998290465303755));
#109777=DIRECTION('center_axis',(1.21828783833459E-17,-1.,-2.31570082641268E-16));
#109778=DIRECTION('ref_axis',(0.190629674628636,0.,-0.981662022872934));
#109779=DIRECTION('',(-1.21828783833459E-17,1.,2.31570082641268E-16));
#109780=DIRECTION('center_axis',(0.,1.,2.22044604925031E-16));
#109781=DIRECTION('ref_axis',(0.190629674628636,0.,-0.981662022872934));
#109782=DIRECTION('center_axis',(2.09862273058998E-32,1.,2.27504718160893E-16));
#109783=DIRECTION('ref_axis',(-0.923879532511288,0.,0.382683432365088));
#109784=DIRECTION('center_axis',(0.,-1.,-2.22044604925031E-16));
#109785=DIRECTION('ref_axis',(-0.923879532511288,0.,0.382683432365088));
#109786=DIRECTION('',(-2.09862273058998E-32,-1.,-2.27504718160893E-16));
#109787=DIRECTION('center_axis',(0.,-1.,-2.22044604925031E-16));
#109788=DIRECTION('ref_axis',(-0.923879532511288,0.,0.382683432365088));
#109789=DIRECTION('center_axis',(0.,-1.,-3.96508223080413E-16));
#109790=DIRECTION('ref_axis',(-0.598633244308989,0.,-0.80102324486128));
#109791=DIRECTION('center_axis',(0.,1.,2.22044604925031E-16));
#109792=DIRECTION('ref_axis',(-0.598633244308989,0.,-0.80102324486128));
#109793=DIRECTION('',(0.,1.,3.96508223080413E-16));
#109794=DIRECTION('center_axis',(0.,1.,2.22044604925031E-16));
#109795=DIRECTION('ref_axis',(-0.598633244308989,0.,-0.80102324486128));
#109796=DIRECTION('center_axis',(0.,-1.,-3.96508223080413E-16));
#109797=DIRECTION('ref_axis',(-1.,0.,1.837501759903E-19));
#109798=DIRECTION('center_axis',(6.93889390390723E-18,1.,2.22049474265475E-16));
#109799=DIRECTION('ref_axis',(-1.,6.93889390390723E-18,1.83750175990302E-19));
#109800=DIRECTION('',(0.,-1.,-3.96508223080413E-16));
#109801=DIRECTION('center_axis',(0.,1.,2.22044604925031E-16));
#109802=DIRECTION('ref_axis',(-1.,0.,1.837501759903E-19));
#109803=DIRECTION('center_axis',(1.,8.3944909223599E-32,-4.61226199516842E-16));
#109804=DIRECTION('ref_axis',(-4.61226199516842E-16,2.22049474265475E-16,
-1.));
#109805=DIRECTION('',(4.61226199516842E-16,-2.22044604925031E-16,1.));
#109806=DIRECTION('',(0.,1.,2.22044604925031E-16));
#109807=DIRECTION('',(4.61226199516842E-16,-2.22044604925031E-16,1.));
#109808=DIRECTION('center_axis',(0.,1.,2.22044604925031E-16));
#109809=DIRECTION('ref_axis',(-0.939690906904483,-7.59447731678524E-17,
0.342024852139477));
#109810=DIRECTION('center_axis',(0.,-1.,-2.22044604925031E-16));
#109811=DIRECTION('ref_axis',(-0.939690906904483,-7.59447731678524E-17,
0.342024852139477));
#109812=DIRECTION('center_axis',(0.,1.,2.22044604925031E-16));
#109813=DIRECTION('ref_axis',(0.,2.22044604925031E-16,-1.));
#109814=DIRECTION('',(0.,1.,2.22044604925031E-16));
#109815=DIRECTION('center_axis',(0.,-1.,-2.22044604925031E-16));
#109816=DIRECTION('ref_axis',(-1.,0.,0.));
#109817=DIRECTION('center_axis',(0.,-1.,-2.22044604925031E-16));
#109818=DIRECTION('ref_axis',(-1.,0.,0.));
#109819=DIRECTION('center_axis',(0.,1.,2.22044604925031E-16));
#109820=DIRECTION('ref_axis',(1.,0.,0.));
#109821=DIRECTION('center_axis',(0.,1.,2.22044604925031E-16));
#109822=DIRECTION('ref_axis',(1.,0.,0.));
#109823=DIRECTION('center_axis',(0.,-1.,-2.22044604925031E-16));
#109824=DIRECTION('ref_axis',(1.,0.,0.));
#109825=DIRECTION('',(0.,-1.,-2.22044604925031E-16));
#109826=DIRECTION('center_axis',(0.,1.,2.22044604925031E-16));
#109827=DIRECTION('ref_axis',(-1.,0.,0.));
#109828=DIRECTION('center_axis',(0.,-1.,-2.22044604925031E-16));
#109829=DIRECTION('ref_axis',(-1.,0.,0.));
#109830=DIRECTION('',(0.,1.,2.22044604925031E-16));
#109831=DIRECTION('center_axis',(1.,0.,0.));
#109832=DIRECTION('ref_axis',(0.,2.22044604925031E-16,-1.));
#109833=DIRECTION('',(0.,-1.,0.));
#109834=DIRECTION('',(0.,2.22044604925031E-16,-1.));
#109835=DIRECTION('',(0.,1.,2.22044604925031E-16));
#109836=DIRECTION('',(-6.34413156931604E-16,2.22044604925031E-16,-1.));
#109837=DIRECTION('',(0.,1.,2.22044604925031E-16));
#109838=DIRECTION('',(0.,2.22044604925031E-16,-1.));
#109839=DIRECTION('',(0.,1.,2.22044604925031E-16));
#109840=DIRECTION('',(0.,-2.22044604925031E-16,1.));
#109841=DIRECTION('',(0.,1.,2.22044604925031E-16));
#109842=DIRECTION('center_axis',(0.,-1.,0.));
#109843=DIRECTION('ref_axis',(-0.294883912309792,0.,-0.95553308590591));
#109844=DIRECTION('',(0.,1.,0.));
#109845=DIRECTION('center_axis',(0.,1.,2.22044604925031E-16));
#109846=DIRECTION('ref_axis',(-0.294883912309792,0.,-0.95553308590591));
#109847=DIRECTION('center_axis',(0.,-1.,0.));
#109848=DIRECTION('ref_axis',(-1.,0.,-6.93889390390723E-17));
#109849=DIRECTION('',(0.,-1.,0.));
#109850=DIRECTION('center_axis',(0.,1.,2.22044604925031E-16));
#109851=DIRECTION('ref_axis',(-1.,0.,-6.93889390390723E-17));
#109852=DIRECTION('center_axis',(0.,1.,0.));
#109853=DIRECTION('ref_axis',(-0.707106781186547,0.,-0.707106781186548));
#109854=DIRECTION('center_axis',(0.,1.,2.22044604925031E-16));
#109855=DIRECTION('ref_axis',(-0.707106781186547,0.,-0.707106781186548));
#109856=DIRECTION('center_axis',(0.,1.,2.22044604925031E-16));
#109857=DIRECTION('ref_axis',(0.707106781186548,0.,0.707106781186548));
#109858=DIRECTION('center_axis',(0.,-1.,-2.22044604925031E-16));
#109859=DIRECTION('ref_axis',(0.707106781186548,0.,0.707106781186548));
#109860=DIRECTION('',(0.,-1.,-2.22044604925031E-16));
#109861=DIRECTION('center_axis',(0.,-1.,-2.22044604925031E-16));
#109862=DIRECTION('ref_axis',(0.707106781186548,0.,0.707106781186548));
#109863=DIRECTION('center_axis',(-6.50074362628841E-34,-1.,-2.27504718160893E-16));
#109864=DIRECTION('ref_axis',(0.923879532511286,0.,0.382683432365092));
#109865=DIRECTION('center_axis',(0.,-1.,-2.22044604925031E-16));
#109866=DIRECTION('ref_axis',(0.923879532511286,0.,0.382683432365092));
#109867=DIRECTION('',(6.50074362628841E-34,1.,2.27504718160893E-16));
#109868=DIRECTION('center_axis',(0.,-1.,-2.22044604925031E-16));
#109869=DIRECTION('ref_axis',(0.923879532511286,0.,0.382683432365092));
#109870=DIRECTION('',(-6.50074362628841E-34,-1.,-2.27504718160893E-16));
#109871=DIRECTION('center_axis',(-0.707106781186547,1.60870128963502E-16,
-0.707106781186548));
#109872=DIRECTION('ref_axis',(-0.707106781186548,-1.52106150078733E-16,
0.707106781186547));
#109873=DIRECTION('',(0.707106781186548,1.57009245868377E-16,-0.707106781186547));
#109874=DIRECTION('',(0.,1.,2.27504718160893E-16));
#109875=DIRECTION('',(0.707106781186548,1.57009245868377E-16,-0.707106781186547));
#109876=DIRECTION('center_axis',(0.,-1.,-2.22044604925031E-16));
#109877=DIRECTION('ref_axis',(-0.926903899779187,0.,0.375298761754066));
#109878=DIRECTION('',(0.,1.,2.22044604925031E-16));
#109879=DIRECTION('center_axis',(0.,1.,2.22044604925031E-16));
#109880=DIRECTION('ref_axis',(-0.926903899779187,0.,0.375298761754066));
#109881=DIRECTION('center_axis',(1.,2.64363574135728E-32,-1.190587693968E-16));
#109882=DIRECTION('ref_axis',(-1.190587693968E-16,2.22044604925031E-16,
-1.));
#109883=DIRECTION('',(1.190587693968E-16,-2.22044604925031E-16,1.));
#109884=DIRECTION('',(0.,-1.,-2.22044604925031E-16));
#109885=DIRECTION('',(-1.190587693968E-16,2.22044604925031E-16,-1.));
#109886=DIRECTION('center_axis',(0.,1.,2.22044604925031E-16));
#109887=DIRECTION('ref_axis',(0.707106781186548,1.57009245868377E-16,-0.707106781186548));
#109888=DIRECTION('center_axis',(0.,-1.,-2.22044604925031E-16));
#109889=DIRECTION('ref_axis',(0.707106781186548,1.57009245868377E-16,-0.707106781186548));
#109890=DIRECTION('',(0.,1.,2.22044604925031E-16));
#109891=DIRECTION('center_axis',(0.,-1.,-2.22044604925031E-16));
#109892=DIRECTION('ref_axis',(0.707106781186548,1.57009245868377E-16,-0.707106781186548));
#109893=DIRECTION('center_axis',(0.,1.,2.22044604925031E-16));
#109894=DIRECTION('ref_axis',(0.905538513813742,0.,-0.424264068711928));
#109895=DIRECTION('center_axis',(0.,-1.,-2.22044604925031E-16));
#109896=DIRECTION('ref_axis',(0.905538513813742,0.,-0.424264068711928));
#109897=DIRECTION('',(0.,-1.,-2.22044604925031E-16));
#109898=DIRECTION('center_axis',(0.,-1.,-2.22044604925031E-16));
#109899=DIRECTION('ref_axis',(0.905538513813742,0.,-0.424264068711928));
#109900=DIRECTION('',(0.,1.,2.22044604925031E-16));
#109901=DIRECTION('center_axis',(0.,1.,2.22044604925031E-16));
#109902=DIRECTION('ref_axis',(-0.30491067796787,2.11471052309918E-16,-0.952380952382592));
#109903=DIRECTION('center_axis',(0.,-1.,-2.22044604925031E-16));
#109904=DIRECTION('ref_axis',(-0.30491067796787,2.11471052309918E-16,-0.952380952382592));
#109905=DIRECTION('center_axis',(0.,1.,2.22044604925031E-16));
#109906=DIRECTION('ref_axis',(-0.30491067796787,2.11471052309918E-16,-0.952380952382592));
#109907=DIRECTION('center_axis',(0.,1.,2.22044604925031E-16));
#109908=DIRECTION('ref_axis',(1.,0.,0.));
#109909=DIRECTION('center_axis',(0.,-1.,-2.22044604925031E-16));
#109910=DIRECTION('ref_axis',(1.,0.,0.));
#109911=DIRECTION('',(0.,-1.,-2.22044604925031E-16));
#109912=DIRECTION('center_axis',(0.,-1.,-2.22044604925031E-16));
#109913=DIRECTION('ref_axis',(1.,0.,0.));
#109914=DIRECTION('center_axis',(0.,-1.,-2.22044604925031E-16));
#109915=DIRECTION('ref_axis',(0.707106781186548,-1.57009245868377E-16,0.707106781186548));
#109916=DIRECTION('center_axis',(0.,-1.,-2.22044604925031E-16));
#109917=DIRECTION('ref_axis',(0.707106781186548,-1.57009245868377E-16,0.707106781186548));
#109918=DIRECTION('',(0.,-1.,-2.22044604925031E-16));
#109919=DIRECTION('center_axis',(0.,-1.,-2.22044604925031E-16));
#109920=DIRECTION('ref_axis',(0.707106781186548,-1.57009245868377E-16,0.707106781186548));
#109921=DIRECTION('center_axis',(0.,-1.,-2.22044604925031E-16));
#109922=DIRECTION('ref_axis',(-0.00296584926884181,-2.22043628341636E-16,
0.999995601859386));
#109923=DIRECTION('',(0.,1.,2.22044604925031E-16));
#109924=DIRECTION('center_axis',(0.,-1.,-2.22044604925031E-16));
#109925=DIRECTION('ref_axis',(-0.00296584926884181,-2.22043628341636E-16,
0.999995601859386));
#109926=DIRECTION('',(0.,-1.,-2.22044604925031E-16));
#109927=DIRECTION('center_axis',(0.,1.,2.22044604925031E-16));
#109928=DIRECTION('ref_axis',(-0.00296584926884181,-2.22043628341636E-16,
0.999995601859386));
#109929=DIRECTION('center_axis',(-7.93016446160826E-17,-3.1720657846433E-16,
1.));
#109930=DIRECTION('ref_axis',(1.33226762955019E-15,-1.,-3.1720657846433E-16));
#109931=DIRECTION('',(-7.93016446160826E-17,-3.1720657846433E-16,1.));
#109932=DIRECTION('',(-7.93016446160826E-17,-3.1720657846433E-16,1.));
#109933=DIRECTION('center_axis',(-1.58603289232165E-16,-3.1720657846433E-16,
1.));
#109934=DIRECTION('ref_axis',(-1.27675647831893E-15,-1.,-3.1720657846433E-16));
#109935=DIRECTION('',(-1.58603289232165E-16,-3.1720657846433E-16,1.));
#109936=DIRECTION('',(-1.58603289232165E-16,-3.1720657846433E-16,1.));
#109937=DIRECTION('center_axis',(0.,0.,1.));
#109938=DIRECTION('ref_axis',(1.,-7.0059776216349E-34,0.));
#109939=DIRECTION('center_axis',(0.,-2.22044604925031E-16,1.));
#109940=DIRECTION('ref_axis',(1.,-7.0059776216349E-34,0.));
#109941=DIRECTION('',(0.,0.,1.));
#109942=DIRECTION('center_axis',(1.68718058920808E-12,1.77635683940025E-16,
-1.));
#109943=DIRECTION('ref_axis',(1.,-7.0059776216349E-34,0.));
#109944=DIRECTION('center_axis',(-1.68718058920808E-12,-1.77635683940025E-16,
1.));
#109945=DIRECTION('ref_axis',(1.,0.,1.68718058920808E-12));
#109946=DIRECTION('',(-1.,7.0059776216349E-34,-1.68718058920808E-12));
#109947=DIRECTION('center_axis',(-1.68718058920808E-12,-1.77635683940025E-16,
1.));
#109948=DIRECTION('ref_axis',(0.441505993976003,0.897258300203047,0.));
#109949=DIRECTION('center_axis',(-1.68718058920808E-12,-1.77635683940025E-16,
1.));
#109950=DIRECTION('ref_axis',(1.,-2.99704178492074E-28,1.68718058920808E-12));
#109951=DIRECTION('center_axis',(-1.68753899746303E-12,0.,1.));
#109952=DIRECTION('ref_axis',(1.,-1.85111672238412E-28,1.04208212862878E-12));
#109953=DIRECTION('',(0.707106781194979,8.65956056243049E-17,-0.707106781178116));
#109954=DIRECTION('center_axis',(0.,0.,1.));
#109955=DIRECTION('ref_axis',(1.,-7.0059776216349E-34,0.));
#109956=DIRECTION('center_axis',(0.,-2.22044604925031E-16,1.));
#109957=DIRECTION('ref_axis',(1.,-7.0059776216349E-34,0.));
#109958=DIRECTION('',(0.,0.,1.));
#109959=DIRECTION('center_axis',(1.68718058920808E-12,1.77635683940025E-16,
-1.));
#109960=DIRECTION('ref_axis',(1.,-7.0059776216349E-34,0.));
#109961=DIRECTION('center_axis',(-1.68718058920808E-12,-1.77635683940025E-16,
1.));
#109962=DIRECTION('ref_axis',(1.,0.,1.68718058920808E-12));
#109963=DIRECTION('',(-1.,7.0059776216349E-34,-1.68718058920808E-12));
#109964=DIRECTION('center_axis',(-1.68718058920808E-12,-1.77635683940025E-16,
1.));
#109965=DIRECTION('ref_axis',(0.441505993976003,0.897258300203047,0.));
#109966=DIRECTION('center_axis',(-1.68718058920808E-12,-1.77635683940025E-16,
1.));
#109967=DIRECTION('ref_axis',(1.,-2.99704178492074E-28,1.68718058920808E-12));
#109968=DIRECTION('center_axis',(-1.6875389973825E-12,0.,1.));
#109969=DIRECTION('ref_axis',(1.,-1.85111672238412E-28,1.04208212862878E-12));
#109970=DIRECTION('',(0.707106781178108,8.65956056222387E-17,-0.707106781194987));
#109971=DIRECTION('center_axis',(1.68684510806422E-12,0.,-1.));
#109972=DIRECTION('ref_axis',(-0.441505993976003,-0.897258300203047,-4.62840134152024E-13));
#109973=DIRECTION('center_axis',(-1.68718058920808E-12,-1.77635683940025E-16,
1.));
#109974=DIRECTION('ref_axis',(1.,0.,1.68718058920808E-12));
#109975=DIRECTION('center_axis',(1.68718058920808E-12,1.77635683940025E-16,
-1.));
#109976=DIRECTION('ref_axis',(-1.,0.,0.));
#109977=DIRECTION('',(-1.,3.7462934736789E-28,-1.68718058920808E-12));
#109978=DIRECTION('',(-1.79863670155429E-15,-1.,-1.7763568394306E-16));
#109979=DIRECTION('center_axis',(-1.68718058920808E-12,-1.77635683940025E-16,
1.));
#109980=DIRECTION('ref_axis',(-1.,-1.77635683940025E-15,0.));
#109981=DIRECTION('',(-1.43890936124343E-15,1.,1.77635683937597E-16));
#109982=DIRECTION('',(-1.,3.7462934736789E-28,-1.68718058920808E-12));
#109983=DIRECTION('center_axis',(-1.68718058920808E-12,-1.77635683940025E-16,
1.));
#109984=DIRECTION('ref_axis',(1.,0.,1.68718058920808E-12));
#109985=DIRECTION('center_axis',(1.68718058920808E-12,1.77635683940025E-16,
-1.));
#109986=DIRECTION('ref_axis',(-1.,0.,0.));
#109987=DIRECTION('',(-1.,3.7462934736789E-28,-1.68718058920808E-12));
#109988=DIRECTION('',(1.61669403717014E-32,-1.,-1.77635683940025E-16));
#109989=DIRECTION('center_axis',(-1.68718058920808E-12,-1.77635683940025E-16,
1.));
#109990=DIRECTION('ref_axis',(-1.,7.0059776216349E-34,0.));
#109991=DIRECTION('',(-1.61669403717014E-32,1.,1.77635683940025E-16));
#109992=DIRECTION('',(-1.,3.7462934736789E-28,-1.68718058920808E-12));
#109993=DIRECTION('center_axis',(1.,-1.79863670155429E-15,1.85037170770859E-16));
#109994=DIRECTION('ref_axis',(1.79863670155429E-15,1.,1.7763568394306E-16));
#109995=DIRECTION('',(1.8503717077086E-16,2.22044604925031E-16,-1.));
#109996=DIRECTION('',(1.79863670155429E-15,1.,1.7763568394306E-16));
#109997=DIRECTION('',(-1.85037170770859E-16,0.,1.));
#109998=DIRECTION('center_axis',(-1.85037170770859E-16,0.,1.));
#109999=DIRECTION('ref_axis',(-1.,-1.77635683940025E-15,-1.85037170770859E-16));
#110000=DIRECTION('center_axis',(-1.68718058920808E-12,-1.77635683940025E-16,
1.));
#110001=DIRECTION('ref_axis',(-1.,-1.77635683940025E-15,0.));
#110002=DIRECTION('center_axis',(-1.68718058920808E-12,-1.77635683940025E-16,
1.));
#110003=DIRECTION('ref_axis',(-1.,-1.77635683940025E-15,0.));
#110004=DIRECTION('',(-1.85037170770859E-16,0.,1.));
#110005=DIRECTION('center_axis',(-1.,-1.43890936124343E-15,-1.85037170770859E-16));
#110006=DIRECTION('ref_axis',(1.43890936124343E-15,-1.,-1.77635683937597E-16));
#110007=DIRECTION('',(1.43890936124343E-15,-1.,-1.77635683937597E-16));
#110008=DIRECTION('',(-1.85037170770859E-16,-2.22044604925031E-16,1.));
#110009=DIRECTION('center_axis',(1.,1.61669403717014E-32,0.));
#110010=DIRECTION('ref_axis',(-1.61669403717014E-32,1.,1.77635683940025E-16));
#110011=DIRECTION('',(-3.58978188768097E-48,2.22044604925031E-16,-1.));
#110012=DIRECTION('',(-1.61669403717014E-32,1.,1.77635683940025E-16));
#110013=DIRECTION('',(0.,0.,1.));
#110014=DIRECTION('center_axis',(0.,0.,1.));
#110015=DIRECTION('ref_axis',(-1.,7.0059776216349E-34,0.));
#110016=DIRECTION('center_axis',(-1.68718058920808E-12,-1.77635683940025E-16,
1.));
#110017=DIRECTION('ref_axis',(-1.,7.0059776216349E-34,-1.57702134180175E-16));
#110018=DIRECTION('center_axis',(-1.68718058920808E-12,-1.77635683940025E-16,
1.));
#110019=DIRECTION('ref_axis',(-1.,7.0059776216349E-34,-1.57702134180175E-16));
#110020=DIRECTION('',(0.,0.,1.));
#110021=DIRECTION('center_axis',(-1.,-1.61669403717014E-32,0.));
#110022=DIRECTION('ref_axis',(1.61669403717014E-32,-1.,-1.77635683940025E-16));
#110023=DIRECTION('',(1.61669403717014E-32,-1.,-1.77635683940025E-16));
#110024=DIRECTION('',(3.58978188768097E-48,-2.22044604925031E-16,1.));
#110025=DIRECTION('center_axis',(0.577350269189626,0.577350269189625,0.577350269189626));
#110026=DIRECTION('ref_axis',(-0.707106781186548,0.,0.707106781186547));
#110027=DIRECTION('center_axis',(2.77555756159287E-17,-1.,-1.78063851184191E-16));
#110028=DIRECTION('ref_axis',(1.,2.77555756159287E-17,4.9422646860063E-33));
#110029=DIRECTION('center_axis',(0.408248290463863,-0.816496580927726,0.408248290463863));
#110030=DIRECTION('ref_axis',(0.707106781186547,0.,-0.707106781186548));
#110031=DIRECTION('center_axis',(2.77555756159287E-17,-1.,-1.78063851184191E-16));
#110032=DIRECTION('ref_axis',(-1.,0.,-1.68830924263176E-12));
#110033=DIRECTION('center_axis',(0.,1.,2.22044604925031E-16));
#110034=DIRECTION('ref_axis',(-1.,0.,-1.68830924263176E-12));
#110035=DIRECTION('center_axis',(0.577350269189626,0.577350269189626,0.577350269189626));
#110036=DIRECTION('ref_axis',(-0.707106781186547,0.,0.707106781186548));
#110037=DIRECTION('center_axis',(1.72173578928287E-15,-1.,-1.78063851181333E-16));
#110038=DIRECTION('ref_axis',(1.,1.72173578928287E-15,3.06578905356441E-31));
#110039=DIRECTION('center_axis',(0.408248290463863,-0.816496580927726,0.408248290463863));
#110040=DIRECTION('ref_axis',(0.707106781186548,0.,-0.707106781186548));
#110041=DIRECTION('center_axis',(1.72173578928287E-15,-1.,-1.78063851181333E-16));
#110042=DIRECTION('ref_axis',(-1.,-1.77635683940025E-15,-1.68779887675753E-12));
#110043=DIRECTION('center_axis',(0.,1.,2.22044604925031E-16));
#110044=DIRECTION('ref_axis',(-1.,-1.77635683940025E-15,-1.68779887675753E-12));
#110045=DIRECTION('center_axis',(-1.,1.5355029188888E-32,-1.73472347597681E-16));
#110046=DIRECTION('ref_axis',(2.32378448758667E-32,-1.,-2.22472772169198E-16));
#110047=DIRECTION('',(-1.73472347597681E-16,-2.22044604925031E-16,1.));
#110048=DIRECTION('',(2.31635696988567E-32,-1.,-2.22044604925031E-16));
#110049=DIRECTION('',(-1.73472347597681E-16,0.,1.));
#110050=DIRECTION('center_axis',(-1.73472347597681E-16,0.,1.));
#110051=DIRECTION('ref_axis',(-1.,7.0059776216349E-34,-1.73472347597681E-16));
#110052=DIRECTION('center_axis',(-1.73472347597681E-16,0.,1.));
#110053=DIRECTION('ref_axis',(-1.,7.0059776216349E-34,-1.73472347597681E-16));
#110054=DIRECTION('center_axis',(0.,-2.22044604925031E-16,1.));
#110055=DIRECTION('ref_axis',(-1.,7.0059776216349E-34,-1.73472347597681E-16));
#110056=DIRECTION('',(-1.73472347597681E-16,0.,1.));
#110057=DIRECTION('center_axis',(1.,-1.5355029188888E-32,1.73472347597681E-16));
#110058=DIRECTION('ref_axis',(-2.32378448758667E-32,1.,2.22472772169198E-16));
#110059=DIRECTION('',(-2.31635696988567E-32,1.,2.22044604925031E-16));
#110060=DIRECTION('',(1.73472347597681E-16,2.22044604925031E-16,-1.));
#110061=DIRECTION('center_axis',(0.,0.,1.));
#110062=DIRECTION('ref_axis',(1.96005385927235E-15,1.,0.));
#110063=DIRECTION('center_axis',(-1.,-3.59727340310858E-15,-1.73472347597681E-16));
#110064=DIRECTION('ref_axis',(3.59727340310858E-15,-1.,-2.22472772169197E-16));
#110065=DIRECTION('',(-1.7347234759768E-16,-2.22044604925031E-16,1.));
#110066=DIRECTION('',(3.59727340310858E-15,-1.,-2.22044604925031E-16));
#110067=DIRECTION('',(-1.73472347597681E-16,0.,1.));
#110068=DIRECTION('center_axis',(-1.73472347597681E-16,0.,1.));
#110069=DIRECTION('ref_axis',(1.,-7.0059776216349E-34,1.73472347597681E-16));
#110070=DIRECTION('center_axis',(-1.73472347597681E-16,0.,1.));
#110071=DIRECTION('ref_axis',(1.,-7.0059776216349E-34,1.73472347597681E-16));
#110072=DIRECTION('center_axis',(0.,-2.22044604925031E-16,1.));
#110073=DIRECTION('ref_axis',(1.,-7.0059776216349E-34,1.73472347597681E-16));
#110074=DIRECTION('',(-1.73472347597681E-16,0.,1.));
#110075=DIRECTION('center_axis',(1.,-3.23754606279772E-15,1.73472347597681E-16));
#110076=DIRECTION('ref_axis',(3.23754606279772E-15,1.,2.22472772169198E-16));
#110077=DIRECTION('',(3.23754606279772E-15,1.,2.22044604925031E-16));
#110078=DIRECTION('',(1.73472347597681E-16,2.22044604925031E-16,-1.));
#110079=DIRECTION('center_axis',(0.,0.,1.));
#110080=DIRECTION('ref_axis',(1.83697019872103E-16,1.,0.));
#110081=DIRECTION('center_axis',(0.,2.22044604925031E-16,-1.));
#110082=DIRECTION('ref_axis',(-1.,0.,0.));
#110083=DIRECTION('',(1.,0.,0.));
#110084=DIRECTION('',(0.,-1.,-2.22044604925031E-16));
#110085=DIRECTION('',(-1.,0.,0.));
#110086=DIRECTION('center_axis',(0.,2.22044604925031E-16,-1.));
#110087=DIRECTION('ref_axis',(-1.,0.,0.));
#110088=DIRECTION('',(1.,0.,0.));
#110089=DIRECTION('',(1.,0.,0.));
#110090=DIRECTION('center_axis',(0.,-2.46716227694479E-16,1.));
#110091=DIRECTION('ref_axis',(-0.803531498237542,0.595262237455166,1.46860853713914E-16));
#110092=DIRECTION('',(0.,2.46716227694479E-16,-1.));
#110093=DIRECTION('',(0.,2.46716227694479E-16,-1.));
#110094=DIRECTION('center_axis',(1.,-2.99689426160925E-28,1.68710148498153E-12));
#110095=DIRECTION('ref_axis',(-1.68710148498153E-12,-2.22049474265463E-16,
1.));
#110096=DIRECTION('center_axis',(1.,-6.81117991896132E-28,1.68711550397432E-12));
#110097=DIRECTION('ref_axis',(-1.68711550397432E-12,-2.22049474265463E-16,
1.));
#110098=DIRECTION('',(3.81426075461834E-28,1.,1.77635683940025E-16));
#110099=DIRECTION('',(-3.81426075461834E-28,-1.,-1.77635683940025E-16));
#110100=DIRECTION('',(-1.68711550397432E-12,-2.22044604925031E-16,1.));
#110101=DIRECTION('center_axis',(0.,1.,1.77635683940025E-16));
#110102=DIRECTION('ref_axis',(-0.421146106069637,0.,0.906992809972815));
#110103=DIRECTION('center_axis',(0.,1.,2.22044604925031E-16));
#110104=DIRECTION('ref_axis',(-0.421146106069637,0.,0.906992809972815));
#110105=DIRECTION('',(0.,-1.,-1.77635683940025E-16));
#110106=DIRECTION('',(3.81426075461834E-28,1.,1.77635683940025E-16));
#110107=DIRECTION('center_axis',(6.93889390390723E-18,1.,2.22049474265475E-16));
#110108=DIRECTION('ref_axis',(-1.,6.93889390390723E-18,1.83750175990302E-19));
#110109=DIRECTION('',(1.,-6.93889390428186E-18,1.68718058920808E-12));
#110110=DIRECTION('',(0.,-2.46716227694479E-16,1.));
#110111=DIRECTION('center_axis',(-6.93889390390723E-18,-1.,-2.22049474265475E-16));
#110112=DIRECTION('ref_axis',(0.004256401731842,1.77634074823828E-16,-0.99999094148112));
#110113=DIRECTION('',(1.68710148498153E-12,2.22049474265463E-16,-1.));
#110114=DIRECTION('center_axis',(-1.,2.99689426160925E-28,-1.68710148498153E-12));
#110115=DIRECTION('ref_axis',(1.68710148498153E-12,2.22049474265463E-16,
-1.));
#110116=DIRECTION('',(-8.96831017167883E-44,-1.,-1.77635683940025E-16));
#110117=DIRECTION('',(0.,1.,1.77635683940025E-16));
#110118=DIRECTION('',(9.25185853854297E-17,0.,-1.));
#110119=DIRECTION('center_axis',(0.,-2.46716227694479E-16,1.));
#110120=DIRECTION('ref_axis',(1.,1.49541069999345E-33,0.));
#110121=DIRECTION('',(0.,-2.46716227694479E-16,1.));
#110122=DIRECTION('center_axis',(-1.68718058920808E-12,-1.77635683940025E-16,
1.));
#110123=DIRECTION('ref_axis',(1.,1.49541069999345E-33,0.));
#110124=DIRECTION('center_axis',(0.,2.22044604925031E-16,-1.));
#110125=DIRECTION('ref_axis',(1.,0.,0.));
#110126=DIRECTION('center_axis',(0.,-2.22044604925031E-16,1.));
#110127=DIRECTION('ref_axis',(1.,0.,0.));
#110128=DIRECTION('center_axis',(0.,2.22044604925031E-16,-1.));
#110129=DIRECTION('ref_axis',(1.,0.,0.));
#110130=DIRECTION('center_axis',(0.,-3.1720657846433E-16,1.));
#110131=DIRECTION('ref_axis',(1.,0.,0.));
#110132=DIRECTION('center_axis',(0.,-2.22044604925031E-16,1.));
#110133=DIRECTION('ref_axis',(1.,0.,0.));
#110134=DIRECTION('',(0.,-3.1720657846433E-16,1.));
#110135=DIRECTION('center_axis',(1.68684510810446E-12,0.,-1.));
#110136=DIRECTION('ref_axis',(-0.441505993976003,-0.897258300203047,-4.62840134152023E-13));
#110137=DIRECTION('center_axis',(-1.68718058920808E-12,-1.77635683940025E-16,
1.));
#110138=DIRECTION('ref_axis',(-0.441505993976003,-0.897258300203047,-7.45059728147159E-13));
#110139=DIRECTION('center_axis',(-1.,6.81117991896132E-28,-1.68711550397432E-12));
#110140=DIRECTION('ref_axis',(1.68711550397432E-12,2.22049474265463E-16,
-1.));
#110141=DIRECTION('',(-3.81426075461834E-28,-1.,-1.77635683940025E-16));
#110142=DIRECTION('',(1.68711550397432E-12,2.22044604925031E-16,-1.));
#110143=DIRECTION('center_axis',(3.81426075461834E-28,1.,1.77635683940025E-16));
#110144=DIRECTION('ref_axis',(-0.707106781185354,0.,-0.707106781187741));
#110145=DIRECTION('',(3.81426075461834E-28,1.,1.77635683940025E-16));
#110146=DIRECTION('center_axis',(0.,1.,2.22044604925031E-16));
#110147=DIRECTION('ref_axis',(-0.707106781185354,0.,-0.707106781187741));
#110148=DIRECTION('center_axis',(1.68718058920808E-12,1.77635683940025E-16,
-1.));
#110149=DIRECTION('ref_axis',(1.,2.21497401039684E-17,1.68718058920808E-12));
#110150=DIRECTION('',(-8.31844254296254E-44,-1.,-1.77635683940025E-16));
#110151=DIRECTION('',(1.,-3.7462934736789E-28,1.68718058920808E-12));
#110152=DIRECTION('center_axis',(1.68718058920808E-12,1.77635683940025E-16,
-1.));
#110153=DIRECTION('ref_axis',(-1.,7.0059776216349E-34,-1.68741283569787E-12));
#110154=DIRECTION('center_axis',(-9.25185853854297E-17,0.,1.));
#110155=DIRECTION('ref_axis',(-1.,7.0059776216349E-34,-9.25185853854297E-17));
#110156=DIRECTION('',(9.25185853854297E-17,0.,-1.));
#110157=DIRECTION('center_axis',(0.,-1.,-1.77635683940025E-16));
#110158=DIRECTION('ref_axis',(0.8003905296798,0.,-0.599478940413164));
#110159=DIRECTION('center_axis',(0.,-1.,-2.22044604925031E-16));
#110160=DIRECTION('ref_axis',(0.8003905296798,0.,-0.599478940413164));
#110161=DIRECTION('',(0.,1.,1.77635683940025E-16));
#110162=DIRECTION('center_axis',(0.,1.,2.22044604925031E-16));
#110163=DIRECTION('ref_axis',(0.8003905296798,0.,-0.599478940413164));
#110164=DIRECTION('center_axis',(0.,1.,2.22044604925031E-16));
#110165=DIRECTION('ref_axis',(-1.,0.,0.));
#110166=DIRECTION('center_axis',(0.,1.,2.22044604925031E-16));
#110167=DIRECTION('ref_axis',(0.718172954054269,0.,0.695864647805135));
#110168=DIRECTION('center_axis',(0.,-1.,-2.22044604925031E-16));
#110169=DIRECTION('ref_axis',(-0.910370950513196,7.3504420940774E-17,-0.413793103448693));
#110170=DIRECTION('center_axis',(3.81426075461834E-28,1.,1.77635683940025E-16));
#110171=DIRECTION('ref_axis',(0.70710678118774,0.,-0.707106781185355));
#110172=DIRECTION('center_axis',(0.,1.,2.22044604925031E-16));
#110173=DIRECTION('ref_axis',(0.70710678118774,0.,-0.707106781185355));
#110174=DIRECTION('center_axis',(0.,-1.,-1.77635683940025E-16));
#110175=DIRECTION('ref_axis',(-0.910370950513196,7.3504420940774E-17,-0.413793103448693));
#110176=DIRECTION('center_axis',(0.,1.,2.22044604925031E-16));
#110177=DIRECTION('ref_axis',(-0.910370950513196,7.3504420940774E-17,-0.413793103448693));
#110178=DIRECTION('',(0.,-1.,-1.77635683940025E-16));
#110179=DIRECTION('center_axis',(0.,-1.,-1.77635683940025E-16));
#110180=DIRECTION('ref_axis',(0.718172954054269,0.,0.695864647805135));
#110181=DIRECTION('center_axis',(0.,-1.,-2.22044604925031E-16));
#110182=DIRECTION('ref_axis',(0.718172954054269,0.,0.695864647805135));
#110183=DIRECTION('',(0.,1.,1.77635683940025E-16));
#110184=DIRECTION('center_axis',(1.,9.15104299692007E-33,7.93016446160826E-17));
#110185=DIRECTION('ref_axis',(-2.32378448758667E-32,1.,1.77635683940025E-16));
#110186=DIRECTION('',(-7.93016446160826E-17,-2.22044604925031E-16,1.));
#110187=DIRECTION('',(0.,1.,1.77635683940025E-16));
#110188=DIRECTION('',(0.,-1.,-2.22044604925031E-16));
#110189=DIRECTION('center_axis',(-7.93016446160826E-17,-2.22044604925031E-16,
1.));
#110190=DIRECTION('ref_axis',(-0.707106781186547,0.707106781186548,0.));
#110191=DIRECTION('',(7.93016446160826E-17,2.22044604925031E-16,-1.));
#110192=DIRECTION('center_axis',(-1.,-9.15104299692007E-33,-7.93016446160826E-17));
#110193=DIRECTION('ref_axis',(2.32378448758667E-32,-1.,-1.77635683940025E-16));
#110194=DIRECTION('',(7.93016446160826E-17,2.22044604925031E-16,-1.));
#110195=DIRECTION('',(0.,1.,2.22044604925031E-16));
#110196=DIRECTION('',(0.,-1.,-1.77635683940025E-16));
#110197=DIRECTION('center_axis',(0.,-1.,-1.77635683940025E-16));
#110198=DIRECTION('ref_axis',(0.004256401731842,1.77634074823828E-16,-0.99999094148112));
#110199=DIRECTION('center_axis',(0.,-1.,-2.22044604925031E-16));
#110200=DIRECTION('ref_axis',(0.004256401731842,1.77634074823828E-16,-0.99999094148112));
#110201=DIRECTION('center_axis',(0.,1.,1.77635683940025E-16));
#110202=DIRECTION('ref_axis',(0.418454579663818,0.,0.908237724804678));
#110203=DIRECTION('center_axis',(0.,1.,2.22044604925031E-16));
#110204=DIRECTION('ref_axis',(0.418454579663818,0.,0.908237724804678));
#110205=DIRECTION('center_axis',(1.,-4.93575888202656E-33,1.58603289232165E-16));
#110206=DIRECTION('ref_axis',(-2.32378448758667E-32,1.,1.77635683940025E-16));
#110207=DIRECTION('',(-1.58603289232165E-16,-2.22044604925031E-16,1.));
#110208=DIRECTION('',(0.,-1.,-2.22044604925031E-16));
#110209=DIRECTION('center_axis',(0.,1.,2.22044604925031E-16));
#110210=DIRECTION('ref_axis',(1.,-3.42114081564477E-49,1.54074485025198E-33));
#110211=DIRECTION('center_axis',(0.,1.,2.22044604925031E-16));
#110212=DIRECTION('ref_axis',(1.,0.,0.));
#110213=DIRECTION('center_axis',(1.83750175990302E-19,-1.,-2.22039735584453E-16));
#110214=DIRECTION('ref_axis',(1.,1.83750175990302E-19,1.58154558548465E-33));
#110215=DIRECTION('',(0.,1.,2.22044604925031E-16));
#110216=DIRECTION('center_axis',(1.83750175990302E-19,-1.,-2.22039735584453E-16));
#110217=DIRECTION('ref_axis',(1.,1.83750175990302E-19,1.58154558548465E-33));
#110218=DIRECTION('center_axis',(-1.,4.93575888202656E-33,-1.58603289232165E-16));
#110219=DIRECTION('ref_axis',(2.32378448758667E-32,-1.,-1.77635683940025E-16));
#110220=DIRECTION('',(1.58603289232165E-16,2.22044604925031E-16,-1.));
#110221=DIRECTION('center_axis',(0.,1.,2.22044604925031E-16));
#110222=DIRECTION('ref_axis',(0.16256157635468,2.19091056557869E-16,-0.986698400674229));
#110223=DIRECTION('center_axis',(0.,1.,2.22044604925031E-16));
#110224=DIRECTION('ref_axis',(0.16256157635468,2.19091056557869E-16,-0.986698400674229));
#110225=DIRECTION('center_axis',(0.,-1.,-2.22044604925031E-16));
#110226=DIRECTION('ref_axis',(0.16256157635468,2.19091056557869E-16,-0.986698400674229));
#110227=DIRECTION('center_axis',(0.,-1.,-2.22044604925031E-16));
#110228=DIRECTION('ref_axis',(0.16256157635468,2.19091056557869E-16,-0.986698400674229));
#110229=DIRECTION('center_axis',(-7.93016446160826E-17,-2.22044604925031E-16,
1.));
#110230=DIRECTION('ref_axis',(0.707106781186547,0.707106781186548,0.));
#110231=DIRECTION('',(-7.93016446160826E-17,-2.22044604925031E-16,1.));
#110232=DIRECTION('center_axis',(-1.58603289232165E-16,-2.22044604925031E-16,
1.));
#110233=DIRECTION('ref_axis',(-0.707106781186547,0.707106781186548,0.));
#110234=DIRECTION('',(1.58603289232165E-16,2.22044604925031E-16,-1.));
#110235=DIRECTION('center_axis',(1.58603289232165E-16,2.22044604925031E-16,
-1.));
#110236=DIRECTION('ref_axis',(0.707106781186548,0.707106781186548,0.));
#110237=DIRECTION('',(-1.58603289232165E-16,-2.22044604925031E-16,1.));
#110238=DIRECTION('center_axis',(0.,1.,2.22044604925031E-16));
#110239=DIRECTION('ref_axis',(1.,0.,0.));
#110240=DIRECTION('',(-1.,2.89708077091569E-28,-1.30472918803582E-12));
#110241=DIRECTION('center_axis',(0.,2.22044604925031E-16,-1.));
#110242=DIRECTION('ref_axis',(-1.,0.,0.));
#110243=DIRECTION('',(1.,0.,0.));
#110244=DIRECTION('',(1.,0.,0.));
#110245=DIRECTION('',(1.,0.,0.));
#110246=DIRECTION('',(-1.,0.,0.));
#110247=DIRECTION('center_axis',(0.,-1.,-2.66453525910038E-16));
#110248=DIRECTION('ref_axis',(-0.655931289920099,0.,-0.75482060312617));
#110249=DIRECTION('',(0.,1.,2.66453525910038E-16));
#110250=DIRECTION('center_axis',(0.,1.,2.22044604925031E-16));
#110251=DIRECTION('ref_axis',(-0.655931289920099,0.,-0.75482060312617));
#110252=DIRECTION('',(0.,-1.,0.));
#110253=DIRECTION('center_axis',(0.,-1.,0.));
#110254=DIRECTION('ref_axis',(-0.457833560950813,0.,0.889037924088224));
#110255=DIRECTION('',(0.,1.,0.));
#110256=DIRECTION('center_axis',(0.,1.,2.22044604925031E-16));
#110257=DIRECTION('ref_axis',(-0.457833560950813,0.,0.889037924088224));
#110258=DIRECTION('center_axis',(1.,0.,1.90323947078569E-14));
#110259=DIRECTION('ref_axis',(-8.85696131249311E-15,-2.22044604925031E-16,
1.));
#110260=DIRECTION('center_axis',(1.,-4.17479820231099E-30,1.88016196282748E-14));
#110261=DIRECTION('ref_axis',(-1.85037170770859E-14,-2.22044604925031E-16,
1.));
#110262=DIRECTION('center_axis',(-1.,4.17479820231099E-30,-1.88016196282748E-14));
#110263=DIRECTION('ref_axis',(0.,-2.22044604925031E-16,1.));
#110264=DIRECTION('center_axis',(0.,1.,2.22044604925031E-16));
#110265=DIRECTION('ref_axis',(0.900018102197426,-9.67786997242177E-17,0.435852516015388));
#110266=DIRECTION('',(0.,-1.,-2.22044604925031E-16));
#110267=DIRECTION('center_axis',(-4.16333634234434E-17,1.,2.28983498828938E-16));
#110268=DIRECTION('ref_axis',(-1.,0.,0.));
#110269=DIRECTION('center_axis',(0.,1.,2.22044604925031E-16));
#110270=DIRECTION('ref_axis',(-1.,0.,0.));
#110271=DIRECTION('center_axis',(0.,-1.,0.));
#110272=DIRECTION('ref_axis',(-0.301695932343328,0.,0.953404197813021));
#110273=DIRECTION('center_axis',(-4.16333634234434E-17,1.,2.28983498828938E-16));
#110274=DIRECTION('ref_axis',(-1.,-4.16333634234434E-17,-6.93889390390723E-17));
#110275=DIRECTION('center_axis',(4.16333634234434E-17,-1.,-2.28983498828938E-16));
#110276=DIRECTION('ref_axis',(-1.,-4.16333634234434E-17,-6.93889390390723E-17));
#110277=DIRECTION('center_axis',(-1.,4.1086505480261E-30,-1.85037170770859E-14));
#110278=DIRECTION('ref_axis',(-1.26584900907556E-14,-0.898717034276078,
0.438529009647037));
#110279=DIRECTION('',(-1.,4.1086505480261E-30,-1.85037170770859E-14));
#110280=DIRECTION('center_axis',(0.,-1.,-2.66453525910038E-16));
#110281=DIRECTION('ref_axis',(-0.436731370632223,-2.39699451904355E-16,
0.899591968564471));
#110282=DIRECTION('',(0.,-1.,-2.66453525910038E-16));
#110283=DIRECTION('center_axis',(0.,1.,0.));
#110284=DIRECTION('ref_axis',(-0.975463667519713,0.,-0.220160471813156));
#110285=DIRECTION('',(0.,1.,0.));
#110286=DIRECTION('center_axis',(0.,1.,2.22044604925031E-16));
#110287=DIRECTION('ref_axis',(-0.975463667519713,0.,-0.220160471813156));
#110288=DIRECTION('',(0.,-1.,0.));
#110289=DIRECTION('center_axis',(0.,-1.,0.));
#110290=DIRECTION('ref_axis',(0.988823617405683,0.,0.14909008572249));
#110291=DIRECTION('center_axis',(0.,1.,2.22044604925031E-16));
#110292=DIRECTION('ref_axis',(-0.805424049353576,0.,-0.59269899672843));
#110293=DIRECTION('',(0.,1.,0.));
#110294=DIRECTION('center_axis',(0.,-1.,0.));
#110295=DIRECTION('ref_axis',(-0.00362742930711492,0.,-0.999993420856668));
#110296=DIRECTION('center_axis',(0.,1.,2.22044604925031E-16));
#110297=DIRECTION('ref_axis',(-0.00362742930711492,0.,-0.999993420856668));
#110298=DIRECTION('',(0.,-1.,0.));
#110299=DIRECTION('center_axis',(0.,-1.,0.));
#110300=DIRECTION('ref_axis',(0.456803537809492,0.,0.889567607236646));
#110301=DIRECTION('center_axis',(0.,1.,2.22044604925031E-16));
#110302=DIRECTION('ref_axis',(0.456803537809492,0.,0.889567607236646));
#110303=DIRECTION('center_axis',(1.23192613759945E-16,0.,1.));
#110304=DIRECTION('ref_axis',(-1.,-1.83750175990341E-19,1.751211913973E-16));
#110305=DIRECTION('center_axis',(1.23192613759945E-16,-2.22049474265475E-16,
1.));
#110306=DIRECTION('ref_axis',(-1.,-1.83750175990352E-19,2.22044604925031E-16));
#110307=DIRECTION('',(-0.707106781186548,-8.67255366190364E-17,-0.707106781186547));
#110308=DIRECTION('center_axis',(-1.23192613759945E-16,2.22049474265475E-16,
-1.));
#110309=DIRECTION('ref_axis',(-1.,-1.8375017599033E-19,1.23192613759945E-16));
#110310=DIRECTION('center_axis',(1.23192613759945E-16,-2.22049474265475E-16,
1.));
#110311=DIRECTION('ref_axis',(-1.,-1.8375017599033E-19,1.23192613759945E-16));
#110312=DIRECTION('center_axis',(1.23192613759945E-16,-2.22049474265475E-16,
1.));
#110313=DIRECTION('ref_axis',(-1.,-1.8375017599033E-19,1.23192613759945E-16));
#110314=DIRECTION('center_axis',(2.22044604925031E-16,-2.22044604925031E-16,
1.));
#110315=DIRECTION('ref_axis',(-1.,-1.83750175990352E-19,2.22044604925031E-16));
#110316=DIRECTION('',(2.22044604925031E-16,-2.22044604925031E-16,1.));
#110317=DIRECTION('center_axis',(1.23192613759945E-16,-2.22049474265475E-16,
1.));
#110318=DIRECTION('ref_axis',(-1.,-1.83750175990336E-19,1.52923281628809E-16));
#110319=DIRECTION('center_axis',(1.23192613759944E-16,-2.22044604925031E-16,
1.));
#110320=DIRECTION('ref_axis',(-1.,-1.83750175990329E-19,1.17513135154478E-16));
#110321=DIRECTION('',(-0.832050294337844,2.11185235656057E-17,-0.554700196225229));
#110322=DIRECTION('center_axis',(-1.23192613759945E-16,2.22049474265475E-16,
-1.));
#110323=DIRECTION('ref_axis',(-1.,-1.83750175990327E-19,1.11022302462516E-16));
#110324=DIRECTION('center_axis',(0.,1.,2.22044604925031E-16));
#110325=DIRECTION('ref_axis',(-1.,0.,0.));
#110326=DIRECTION('center_axis',(0.,-1.,-2.22044604925031E-16));
#110327=DIRECTION('ref_axis',(-1.,0.,0.));
#110328=DIRECTION('',(0.,1.,2.22044604925031E-16));
#110329=DIRECTION('center_axis',(0.,-1.,-2.22044604925031E-16));
#110330=DIRECTION('ref_axis',(-1.,0.,0.));
#110331=DIRECTION('center_axis',(-1.,4.1086505480261E-30,-1.85037170770859E-14));
#110332=DIRECTION('ref_axis',(-1.85037170770859E-14,-2.22044604925031E-16,
1.));
#110333=DIRECTION('center_axis',(0.,1.,2.22044604925031E-16));
#110334=DIRECTION('ref_axis',(-1.,0.,0.));
#110335=DIRECTION('center_axis',(0.,-1.,-2.22044604925031E-16));
#110336=DIRECTION('ref_axis',(-1.,0.,0.));
#110337=DIRECTION('',(0.,1.,2.22044604925031E-16));
#110338=DIRECTION('center_axis',(4.16333634234434E-17,-1.,-2.28983498828938E-16));
#110339=DIRECTION('ref_axis',(-1.,0.,0.));
#110340=DIRECTION('center_axis',(0.,-1.,-2.66453525910038E-16));
#110341=DIRECTION('ref_axis',(-0.6562461524672,0.,-0.754546875529941));
#110342=DIRECTION('',(0.,1.,2.66453525910038E-16));
#110343=DIRECTION('center_axis',(1.,0.,2.2204460492513E-14));
#110344=DIRECTION('ref_axis',(-1.00566802662866E-14,-2.22044604925031E-16,
1.));
#110345=DIRECTION('center_axis',(1.,-4.17479820231099E-30,1.88016196282748E-14));
#110346=DIRECTION('ref_axis',(-1.88016196282748E-14,-2.22044604925031E-16,
1.));
#110347=DIRECTION('',(-0.707106781186359,-2.43604851491997E-16,0.707106781186736));
#110348=DIRECTION('center_axis',(-1.,4.17479820231099E-30,-1.88016196282748E-14));
#110349=DIRECTION('ref_axis',(0.,-2.22044604925031E-16,1.));
#110350=DIRECTION('center_axis',(-1.,0.,0.));
#110351=DIRECTION('ref_axis',(0.,-2.22044604925031E-16,1.));
#110352=DIRECTION('',(-1.,0.,0.));
#110353=DIRECTION('center_axis',(-1.,4.17479820231099E-30,-1.88016196282748E-14));
#110354=DIRECTION('ref_axis',(0.,-2.22044604925031E-16,1.));
#110355=DIRECTION('center_axis',(0.,1.,2.22044604925031E-16));
#110356=DIRECTION('ref_axis',(0.718181642132044,1.54510999792355E-16,-0.695855681089492));
#110357=DIRECTION('center_axis',(0.,-1.,-2.22044604925031E-16));
#110358=DIRECTION('ref_axis',(0.718181642132044,1.54510999792355E-16,-0.695855681089492));
#110359=DIRECTION('',(0.,-1.,-2.22044604925031E-16));
#110360=DIRECTION('center_axis',(0.,-1.,-2.22044604925031E-16));
#110361=DIRECTION('ref_axis',(0.718181642132044,1.54510999792355E-16,-0.695855681089492));
#110362=DIRECTION('',(0.,1.,2.22044604925031E-16));
#110363=DIRECTION('center_axis',(0.,1.,2.22044604925031E-16));
#110364=DIRECTION('ref_axis',(-0.911330049261084,-9.14105459778262E-17,
0.411676500803472));
#110365=DIRECTION('',(0.,-1.,-2.22044604925031E-16));
#110366=DIRECTION('center_axis',(0.,1.,2.22044604925031E-16));
#110367=DIRECTION('ref_axis',(-0.911330049261084,-9.14105459778262E-17,
0.411676500803472));
#110368=DIRECTION('',(0.,1.,2.22044604925031E-16));
#110369=DIRECTION('center_axis',(0.,-1.,-2.22044604925031E-16));
#110370=DIRECTION('ref_axis',(-0.911330049261084,-9.14105459778262E-17,
0.411676500803472));
#110371=DIRECTION('center_axis',(0.,1.,2.22044604925031E-16));
#110372=DIRECTION('ref_axis',(-0.0029658492688445,2.22043628341636E-16,
-0.999995601859385));
#110373=DIRECTION('',(0.,1.,2.22044604925031E-16));
#110374=DIRECTION('center_axis',(0.,-1.,-2.22044604925031E-16));
#110375=DIRECTION('ref_axis',(-0.0029658492688445,2.22043628341636E-16,
-0.999995601859385));
#110376=DIRECTION('center_axis',(0.,1.,2.22044604925031E-16));
#110377=DIRECTION('ref_axis',(-0.0029658492688445,2.22043628341636E-16,
-0.999995601859385));
#110378=DIRECTION('center_axis',(0.,1.,2.22044604925031E-16));
#110379=DIRECTION('ref_axis',(0.157787733663648,2.19263064006667E-16,-0.987473053356541));
#110380=DIRECTION('',(0.,-1.,-2.22044604925031E-16));
#110381=DIRECTION('center_axis',(0.,-1.,-2.22044604925031E-16));
#110382=DIRECTION('ref_axis',(0.157787733663648,2.19263064006667E-16,-0.987473053356541));
#110383=DIRECTION('center_axis',(0.495885766569122,1.92820817704139E-16,
-0.868387762761633));
#110384=DIRECTION('ref_axis',(-0.868387762761633,1.16830990166913E-16,-0.495885766569122));
#110385=DIRECTION('',(0.,1.,2.22044604925031E-16));
#110386=DIRECTION('',(0.868387762761633,-1.10108759125787E-16,0.495885766569122));
#110387=DIRECTION('center_axis',(0.,1.,2.22044604925031E-16));
#110388=DIRECTION('ref_axis',(2.55004895630733E-36,-2.22044604925031E-16,
1.));
#110389=DIRECTION('center_axis',(0.,-1.,-2.22044604925031E-16));
#110390=DIRECTION('ref_axis',(2.55004895630733E-36,-2.22044604925031E-16,
1.));
#110391=DIRECTION('',(0.,1.,2.22044604925031E-16));
#110392=DIRECTION('center_axis',(0.,-1.,-2.22044604925031E-16));
#110393=DIRECTION('ref_axis',(-0.788263422531444,-1.36632469114311E-16,
0.615337936989922));
#110394=DIRECTION('',(0.,-1.,-2.77555756156289E-16));
#110395=DIRECTION('center_axis',(0.,-1.,-2.22044604925031E-16));
#110396=DIRECTION('ref_axis',(-0.788263422531444,-1.36632469114311E-16,
0.615337936989922));
#110397=DIRECTION('',(0.,-1.,-2.22044604925031E-16));
#110398=DIRECTION('',(0.,-1.,-2.77555756156289E-16));
#110399=DIRECTION('center_axis',(-1.26161707343768E-16,2.22044604925031E-16,
-1.));
#110400=DIRECTION('ref_axis',(-1.,-1.8375017599033E-19,1.26161707343768E-16));
#110401=DIRECTION('center_axis',(-1.16253719856037E-16,2.22044604925031E-16,
-1.));
#110402=DIRECTION('ref_axis',(-1.,-1.8375017599033E-19,1.26161707343768E-16));
#110403=DIRECTION('',(-1.26161707343768E-16,2.22044604925031E-16,-1.));
#110404=DIRECTION('center_axis',(1.23192613759945E-16,-2.22049474265475E-16,
1.));
#110405=DIRECTION('ref_axis',(-1.,-1.8375017599033E-19,1.26161707343768E-16));
#110406=DIRECTION('center_axis',(1.,-4.94335532585216E-32,2.22628932034678E-16));
#110407=DIRECTION('ref_axis',(2.22628932034678E-16,2.22044604925031E-16,
-1.));
#110408=DIRECTION('',(0.,-1.,-2.77555756156289E-16));
#110409=DIRECTION('',(2.22628932034678E-16,2.22044604925031E-16,-1.));
#110410=DIRECTION('center_axis',(0.,1.,2.22044604925031E-16));
#110411=DIRECTION('ref_axis',(-0.819288030372914,1.27316419425093E-16,-0.573382179080996));
#110412=DIRECTION('',(0.,1.,2.22044604925031E-16));
#110413=DIRECTION('center_axis',(0.,-1.,-2.22044604925031E-16));
#110414=DIRECTION('ref_axis',(-0.819288030372914,1.27316419425093E-16,-0.573382179080996));
#110415=DIRECTION('center_axis',(0.,-1.,-2.22044604925031E-16));
#110416=DIRECTION('ref_axis',(-0.59469196781642,0.,0.80395364506583));
#110417=DIRECTION('center_axis',(0.,-1.,-2.22044604925031E-16));
#110418=DIRECTION('ref_axis',(-0.59469196781642,0.,0.80395364506583));
#110419=DIRECTION('',(7.36237927774606E-33,-1.,-2.52671446983656E-16));
#110420=DIRECTION('center_axis',(0.,1.,2.22044604925031E-16));
#110421=DIRECTION('ref_axis',(-1.,0.,0.));
#110422=DIRECTION('',(-0.308815713730942,0.707106781186545,0.636107581272894));
#110423=DIRECTION('center_axis',(0.,-1.,-2.22044604925031E-16));
#110424=DIRECTION('ref_axis',(-1.,0.,0.));
#110425=DIRECTION('center_axis',(0.,1.,2.22044604925031E-16));
#110426=DIRECTION('ref_axis',(-1.,0.,0.));
#110427=DIRECTION('',(0.308815713730941,0.707106781186548,-0.636107581272892));
#110428=DIRECTION('center_axis',(0.,1.,2.22044604925031E-16));
#110429=DIRECTION('ref_axis',(-1.,0.,0.));
#110430=DIRECTION('center_axis',(0.,-1.,-2.22044604925031E-16));
#110431=DIRECTION('ref_axis',(-0.398898296183895,0.,0.916995174088493));
#110432=DIRECTION('center_axis',(0.,-1.,-2.22044604925031E-16));
#110433=DIRECTION('ref_axis',(-0.398898296183895,0.,0.916995174088493));
#110434=DIRECTION('center_axis',(0.,1.,2.22044604925031E-16));
#110435=DIRECTION('ref_axis',(1.,0.,0.));
#110436=DIRECTION('center_axis',(0.,-1.,-2.22044604925031E-16));
#110437=DIRECTION('ref_axis',(1.,0.,0.));
#110438=DIRECTION('center_axis',(0.,1.,2.22044604925031E-16));
#110439=DIRECTION('ref_axis',(1.,0.,0.));
#110440=DIRECTION('center_axis',(0.,-1.,-2.22044604925031E-16));
#110441=DIRECTION('ref_axis',(1.,0.,0.));
#110442=DIRECTION('center_axis',(0.,-1.,-2.22044604925031E-16));
#110443=DIRECTION('ref_axis',(-1.,0.,-6.93889390390723E-17));
#110444=DIRECTION('center_axis',(0.,1.,2.22044604925031E-16));
#110445=DIRECTION('ref_axis',(1.,0.,0.));
#110446=DIRECTION('',(0.,-1.,-2.22044604925031E-16));
#110447=DIRECTION('center_axis',(0.,1.,2.22044604925031E-16));
#110448=DIRECTION('ref_axis',(1.,0.,0.));
#110449=DIRECTION('center_axis',(0.,-1.,0.));
#110450=DIRECTION('ref_axis',(-1.,0.,-6.93889390390723E-17));
#110451=DIRECTION('',(0.,-1.,0.));
#110452=DIRECTION('center_axis',(-4.16333634234434E-17,1.,2.28983498828938E-16));
#110453=DIRECTION('ref_axis',(-1.,0.,-6.93889390390723E-17));
#110454=DIRECTION('center_axis',(0.,-1.,-2.22044604925031E-16));
#110455=DIRECTION('ref_axis',(1.,0.,0.));
#110456=DIRECTION('center_axis',(-4.16333634234434E-17,1.,2.28983498828938E-16));
#110457=DIRECTION('ref_axis',(-1.,-4.16333634234434E-17,-6.93889390390723E-17));
#110458=DIRECTION('center_axis',(0.,-1.,-2.22044604925031E-16));
#110459=DIRECTION('ref_axis',(0.89959196856447,-9.69738446503996E-17,0.436731370632224));
#110460=DIRECTION('center_axis',(0.,-1.,-2.22044604925031E-16));
#110461=DIRECTION('ref_axis',(0.89959196856447,-9.69738446503996E-17,0.436731370632224));
#110462=DIRECTION('center_axis',(0.,1.,2.22044604925031E-16));
#110463=DIRECTION('ref_axis',(0.89959196856447,-9.69738446503996E-17,0.436731370632224));
#110464=DIRECTION('center_axis',(0.,1.,2.22044604925031E-16));
#110465=DIRECTION('ref_axis',(-0.436731370632224,-1.99749543253629E-16,
0.89959196856447));
#110466=DIRECTION('center_axis',(0.,-1.,-2.22044604925031E-16));
#110467=DIRECTION('ref_axis',(-0.436731370632224,-1.99749543253629E-16,
0.89959196856447));
#110468=DIRECTION('center_axis',(0.,1.,2.22044604925031E-16));
#110469=DIRECTION('ref_axis',(-0.436731370632224,-1.99749543253629E-16,
0.89959196856447));
#110470=DIRECTION('center_axis',(-1.,4.1086505480261E-30,-1.85037170770859E-14));
#110471=DIRECTION('ref_axis',(-1.85037170770859E-14,-2.22044604925031E-16,
1.));
#110472=DIRECTION('center_axis',(-1.,4.17479820231099E-30,-1.88016196282748E-14));
#110473=DIRECTION('ref_axis',(-1.85037170770859E-14,-2.22044604925031E-16,
1.));
#110474=DIRECTION('',(-1.,4.1086505480261E-30,-1.85037170770859E-14));
#110475=DIRECTION('center_axis',(1.,-4.17479820231099E-30,1.88016196282748E-14));
#110476=DIRECTION('ref_axis',(0.,1.,2.22044604925031E-16));
#110477=DIRECTION('center_axis',(-1.23192613759945E-16,2.22044604925031E-16,
-1.));
#110478=DIRECTION('ref_axis',(-1.,-1.8375017599033E-19,1.24462157223372E-16));
#110479=DIRECTION('',(0.464833898989921,2.53608975501167E-16,-0.885397902837944));
#110480=DIRECTION('center_axis',(1.23192613759945E-16,-2.22049474265475E-16,
1.));
#110481=DIRECTION('ref_axis',(0.,-1.,-2.22049474265475E-16));
#110482=DIRECTION('center_axis',(-1.23192613759945E-16,2.22049474265475E-16,
-1.));
#110483=DIRECTION('ref_axis',(-1.,-1.83750175990328E-19,1.14692461221607E-16));
#110484=DIRECTION('center_axis',(1.23192613759945E-16,-2.22049474265475E-16,
1.));
#110485=DIRECTION('ref_axis',(-1.,-2.73548551187854E-32,1.23192613759945E-16));
#110486=DIRECTION('center_axis',(1.23192613759945E-16,-2.22044604925031E-16,
1.));
#110487=DIRECTION('ref_axis',(-1.,-1.4920830064792E-32,6.7195971141788E-17));
#110488=DIRECTION('center_axis',(-1.23192613759945E-16,2.22049474265475E-16,
-1.));
#110489=DIRECTION('ref_axis',(-1.,0.,0.));
#110490=DIRECTION('',(0.554700196225232,-2.52683460863366E-16,0.832050294337842));
#110491=DIRECTION('center_axis',(-1.23192613759945E-16,2.22049474265475E-16,
-1.));
#110492=DIRECTION('ref_axis',(-1.,0.,0.));
#110493=DIRECTION('center_axis',(0.,-1.,0.));
#110494=DIRECTION('ref_axis',(-1.,0.,0.));
#110495=DIRECTION('center_axis',(0.,1.,2.22044604925031E-16));
#110496=DIRECTION('ref_axis',(-1.,0.,0.));
#110497=DIRECTION('center_axis',(0.,-1.,0.));
#110498=DIRECTION('ref_axis',(-1.,0.,0.));
#110499=DIRECTION('center_axis',(0.,1.,2.22044604925031E-16));
#110500=DIRECTION('ref_axis',(-1.,0.,0.));
#110501=DIRECTION('center_axis',(0.,-1.,0.));
#110502=DIRECTION('ref_axis',(0.97760907194103,0.,0.210429328893571));
#110503=DIRECTION('center_axis',(0.,-1.,-2.22044604925031E-16));
#110504=DIRECTION('ref_axis',(-1.,0.,0.));
#110505=DIRECTION('center_axis',(-1.11022302462516E-16,2.22044604925031E-16,
-1.));
#110506=DIRECTION('ref_axis',(-1.,-1.83750175990327E-19,1.11022302462516E-16));
#110507=DIRECTION('',(-1.11022302462516E-16,2.22044604925031E-16,-1.));
#110508=DIRECTION('center_axis',(2.22044604925031E-16,-2.22044604925031E-16,
1.));
#110509=DIRECTION('ref_axis',(0.805763256495856,0.592237768536584,-4.74121826153412E-17));
#110510=DIRECTION('center_axis',(1.23192613759945E-16,-2.22049474265475E-16,
1.));
#110511=DIRECTION('ref_axis',(-1.,-1.83750175990352E-19,2.22044604925031E-16));
#110512=DIRECTION('center_axis',(-2.22044604925031E-16,2.22044604925031E-16,
-1.));
#110513=DIRECTION('ref_axis',(-1.,-1.83750175990352E-19,2.22044604925031E-16));
#110514=DIRECTION('center_axis',(1.23192613759945E-16,-2.22049474265475E-16,
1.));
#110515=DIRECTION('ref_axis',(-1.,-1.83750175990352E-19,2.22044604925031E-16));
#110516=DIRECTION('center_axis',(-1.11022302462516E-16,2.22044604925031E-16,
-1.));
#110517=DIRECTION('ref_axis',(0.589037115720846,0.808105980860968,1.14039316434621E-16));
#110518=DIRECTION('center_axis',(1.23192613759945E-16,-2.22049474265475E-16,
1.));
#110519=DIRECTION('ref_axis',(-1.,-1.83750175990327E-19,1.11022302462516E-16));
#110520=DIRECTION('center_axis',(1.23192613759945E-16,-2.22049474265475E-16,
1.));
#110521=DIRECTION('ref_axis',(-1.,-1.83750175990327E-19,1.11022302462516E-16));
#110522=DIRECTION('center_axis',(1.23192613759945E-16,-2.22049474265475E-16,
1.));
#110523=DIRECTION('ref_axis',(-1.,-1.83750175990327E-19,1.11022302462516E-16));
#110524=DIRECTION('center_axis',(1.23192613759945E-16,0.,1.));
#110525=DIRECTION('ref_axis',(1.,1.64129130712712E-32,-7.39155682559668E-17));
#110526=DIRECTION('center_axis',(1.23192613759945E-16,0.,1.));
#110527=DIRECTION('ref_axis',(1.,1.64129130712712E-32,-7.39155682559668E-17));
#110528=DIRECTION('center_axis',(1.23192613759945E-16,-2.22049474265475E-16,
1.));
#110529=DIRECTION('ref_axis',(1.,0.,0.));
#110530=DIRECTION('center_axis',(0.,-2.22044604925031E-16,1.));
#110531=DIRECTION('ref_axis',(1.,0.,0.));
#110532=DIRECTION('center_axis',(-0.683267731943171,1.85374434656938E-16,
-0.730167930331944));
#110533=DIRECTION('ref_axis',(0.730167930331944,1.86856382700914E-16,-0.683267731943171));
#110534=DIRECTION('',(-2.53017617534078E-17,1.,2.77555756156289E-16));
#110535=DIRECTION('center_axis',(-0.683267731943171,1.85374434656938E-16,
-0.730167930331944));
#110536=DIRECTION('ref_axis',(0.730167930331944,-1.90208386519252E-14,-0.683267731943171));
#110537=DIRECTION('',(0.730167930331944,1.51715913597344E-16,-0.683267731943171));
#110538=DIRECTION('center_axis',(-2.53017617534078E-17,1.,2.77555756156289E-16));
#110539=DIRECTION('ref_axis',(-0.683267731943172,0.,-0.730167930331943));
#110540=DIRECTION('center_axis',(0.,1.,2.22044604925031E-16));
#110541=DIRECTION('ref_axis',(-0.683267731943172,0.,-0.730167930331943));
#110542=DIRECTION('center_axis',(2.44942954807913E-14,2.99934041219171E-16,
-1.));
#110543=DIRECTION('ref_axis',(1.,4.16333634234378E-17,2.44942954807913E-14));
#110544=DIRECTION('',(1.,-7.34667303037021E-30,2.44942954807913E-14));
#110545=DIRECTION('',(0.,-1.,-2.99934041219171E-16));
#110546=DIRECTION('',(1.,4.16333634234378E-17,2.44942954807913E-14));
#110547=DIRECTION('',(-8.62629387613302E-31,1.,2.99934041219171E-16));
#110548=DIRECTION('center_axis',(-1.,3.53805783332294E-31,-1.17961196366423E-15));
#110549=DIRECTION('ref_axis',(1.17961196366423E-15,2.28983498828939E-16,
-1.));
#110550=DIRECTION('',(-2.63976927864639E-32,-1.,-2.77555756156289E-16));
#110551=DIRECTION('',(1.17961196366423E-15,2.28983498828939E-16,-1.));
#110552=DIRECTION('',(0.,1.,2.99934041219171E-16));
#110553=DIRECTION('center_axis',(-1.,3.53805783332294E-31,-1.17961196366423E-15));
#110554=DIRECTION('ref_axis',(-1.40115152357497E-16,0.992920511302924,0.118780714907517));
#110555=DIRECTION('center_axis',(0.,-1.,-2.99934041219171E-16));
#110556=DIRECTION('ref_axis',(-0.707106781186541,0.,-0.707106781186554));
#110557=DIRECTION('center_axis',(0.,-1.,-2.22044604925031E-16));
#110558=DIRECTION('ref_axis',(-0.707106781186541,0.,-0.707106781186554));
#110559=DIRECTION('center_axis',(1.,-6.86520621803209E-30,2.57651168044591E-14));
#110560=DIRECTION('ref_axis',(2.57571741713036E-14,0.,-1.));
#110561=DIRECTION('center_axis',(2.14231643585101E-14,-0.555555555545262,
-0.831479419289976));
#110562=DIRECTION('ref_axis',(-1.41861830924326E-14,-0.831479419289976,
0.555555555545262));
#110563=DIRECTION('center_axis',(1.,-6.86520621803209E-30,2.57651168044591E-14));
#110564=DIRECTION('ref_axis',(1.97107954957864E-14,0.643991722633251,-0.765032457598929));
#110565=DIRECTION('center_axis',(-1.,0.,0.));
#110566=DIRECTION('ref_axis',(0.,0.640782340939398,-0.767722600644416));
#110567=DIRECTION('center_axis',(1.,-3.53805783332294E-31,1.17961196366423E-15));
#110568=DIRECTION('ref_axis',(-1.30104260698261E-16,0.992920511302924,0.118780714907517));
#110569=DIRECTION('',(-1.,0.,0.));
#110570=DIRECTION('',(-1.,0.,0.));
#110571=DIRECTION('center_axis',(-1.,0.,0.));
#110572=DIRECTION('ref_axis',(0.,-0.881917103691109,0.471404520785583));
#110573=DIRECTION('center_axis',(-1.,0.,0.));
#110574=DIRECTION('ref_axis',(0.,-0.881917103691109,0.471404520785584));
#110575=DIRECTION('center_axis',(-0.221755562098149,-0.912048152143364,
-0.344953096594898));
#110576=DIRECTION('ref_axis',(0.493196961917217,-0.410083123490685,0.767195274088514));
#110577=DIRECTION('center_axis',(0.,-1.,0.));
#110578=DIRECTION('ref_axis',(1.,0.,2.77555756156286E-14));
#110579=DIRECTION('center_axis',(1.,1.48359792176586E-14,2.22044604925059E-14));
#110580=DIRECTION('ref_axis',(-2.22044604925059E-14,0.,1.));
#110581=DIRECTION('center_axis',(-8.62629387613302E-31,1.,2.99934041219171E-16));
#110582=DIRECTION('ref_axis',(0.707106781186528,0.,0.707106781186567));
#110583=DIRECTION('center_axis',(0.,1.,2.22044604925031E-16));
#110584=DIRECTION('ref_axis',(0.707106781186528,0.,0.707106781186567));
#110585=DIRECTION('center_axis',(0.248654602219127,-0.206751184253524,-0.94626890290499));
#110586=DIRECTION('ref_axis',(0.72760687511296,-0.604990141980321,0.323380833376045));
#110587=DIRECTION('center_axis',(0.,-0.555555555565834,0.831479419276231));
#110588=DIRECTION('ref_axis',(0.,-0.831479419276231,-0.555555555565833));
#110589=DIRECTION('center_axis',(0.,-1.,0.));
#110590=DIRECTION('ref_axis',(1.,0.,0.));
#110591=DIRECTION('center_axis',(1.,0.,0.));
#110592=DIRECTION('ref_axis',(0.,-0.471404520796493,0.881917103685277));
#110593=DIRECTION('center_axis',(1.,1.85449740220717E-14,2.77555756156289E-14));
#110594=DIRECTION('ref_axis',(-2.77555756156289E-14,0.,1.));
#110595=DIRECTION('center_axis',(0.,-0.305555555545279,-0.952174250058998));
#110596=DIRECTION('ref_axis',(1.,0.,0.));
#110597=DIRECTION('center_axis',(-1.,3.53805783332294E-31,-1.17961196366423E-15));
#110598=DIRECTION('ref_axis',(-8.88178419700126E-16,0.,1.));
#110599=DIRECTION('center_axis',(-2.63976927864639E-32,-1.,-2.77555756156289E-16));
#110600=DIRECTION('ref_axis',(0.707106781186544,0.,0.707106781186551));
#110601=DIRECTION('center_axis',(0.,1.,2.22044604925031E-16));
#110602=DIRECTION('ref_axis',(0.707106781186544,0.,0.707106781186551));
#110603=DIRECTION('center_axis',(0.,1.,2.22044604925031E-16));
#110604=DIRECTION('ref_axis',(-1.,0.,0.));
#110605=DIRECTION('',(0.,1.,2.22044604925031E-16));
#110606=DIRECTION('center_axis',(-4.16333634234434E-17,1.,2.28983498828938E-16));
#110607=DIRECTION('ref_axis',(-1.,0.,0.));
#110608=DIRECTION('center_axis',(0.,1.,2.66453525910038E-16));
#110609=DIRECTION('ref_axis',(0.971814489841705,0.,-0.235746892521843));
#110610=DIRECTION('center_axis',(0.,-1.,-2.66453525910038E-16));
#110611=DIRECTION('ref_axis',(-0.436731370632223,-2.39699451904355E-16,
0.899591968564471));
#110612=DIRECTION('',(0.,-1.,-2.66453525910038E-16));
#110613=DIRECTION('center_axis',(0.,1.,2.22044604925031E-16));
#110614=DIRECTION('ref_axis',(-0.436731370632223,-2.39699451904355E-16,
0.899591968564471));
#110615=DIRECTION('',(0.,1.,2.66453525910038E-16));
#110616=DIRECTION('center_axis',(0.,1.,0.));
#110617=DIRECTION('ref_axis',(-0.301492073683253,-2.34187669256869E-17,
0.953468683023292));
#110618=DIRECTION('center_axis',(0.,-1.,-2.66453525910038E-16));
#110619=DIRECTION('ref_axis',(-0.659606396000608,0.,-0.751611204250635));
#110620=DIRECTION('center_axis',(-0.619186432486295,-0.785244014192337,
6.07756750723163E-15));
#110621=DIRECTION('ref_axis',(0.684676922246484,-0.539886523461806,0.489632570329433));
#110622=DIRECTION('center_axis',(1.26161707343768E-16,-2.22044604925031E-16,
1.));
#110623=DIRECTION('ref_axis',(-1.,-1.8375017599033E-19,1.26161707343768E-16));
#110624=DIRECTION('center_axis',(-1.26161707343768E-16,2.22044604925031E-16,
-1.));
#110625=DIRECTION('ref_axis',(0.69507377161985,0.718938420176691,0.));
#110626=DIRECTION('center_axis',(1.26161707343768E-16,-2.22044604925031E-16,
1.));
#110627=DIRECTION('ref_axis',(-1.,-1.8375017599033E-19,1.26161707343768E-16));
#110628=DIRECTION('center_axis',(-6.93889390390729E-17,0.,1.));
#110629=DIRECTION('ref_axis',(-1.,-2.65392283312903E-15,-6.93889390390729E-17));
#110630=DIRECTION('',(0.,-1.,0.));
#110631=DIRECTION('',(-1.,1.5407439555098E-32,-6.93889390390729E-17));
#110632=DIRECTION('',(0.,1.,0.));
#110633=DIRECTION('center_axis',(0.,-1.,0.));
#110634=DIRECTION('ref_axis',(0.707106781186547,0.,0.707106781186547));
#110635=DIRECTION('center_axis',(0.,1.,2.22044604925031E-16));
#110636=DIRECTION('ref_axis',(0.707106781186547,0.,0.707106781186547));
#110637=DIRECTION('center_axis',(0.,-1.,0.));
#110638=DIRECTION('ref_axis',(6.93889390390723E-17,0.,-1.));
#110639=DIRECTION('',(0.,-1.,0.));
#110640=DIRECTION('center_axis',(0.,1.,2.22044604925031E-16));
#110641=DIRECTION('ref_axis',(6.93889390390723E-17,0.,-1.));
#110642=DIRECTION('center_axis',(0.,-1.,-2.66453525910038E-16));
#110643=DIRECTION('ref_axis',(0.752694710045468,0.,-0.658369708803169));
#110644=DIRECTION('center_axis',(0.,1.,2.22044604925031E-16));
#110645=DIRECTION('ref_axis',(0.752694710045468,0.,-0.658369708803169));
#110646=DIRECTION('center_axis',(1.16253719856037E-16,-2.22044604925031E-16,
1.));
#110647=DIRECTION('ref_axis',(1.,2.58135112964991E-32,-1.16253719856037E-16));
#110648=DIRECTION('',(4.004083039641E-17,1.,2.22044604925031E-16));
#110649=DIRECTION('',(-1.,-2.58135112964991E-32,1.16253719856037E-16));
#110650=DIRECTION('',(0.,-1.,-2.22044604925031E-16));
#110651=DIRECTION('',(-1.,-1.83750175990151E-19,-6.09920703375441E-16));
#110652=DIRECTION('center_axis',(0.,1.,2.22044604925031E-16));
#110653=DIRECTION('ref_axis',(0.707106781186543,-1.57009245868379E-16,0.707106781186552));
#110654=DIRECTION('center_axis',(0.,-1.,-2.22044604925031E-16));
#110655=DIRECTION('ref_axis',(0.707106781186543,-1.57009245868379E-16,0.707106781186552));
#110656=DIRECTION('',(0.,1.,2.22044604925031E-16));
#110657=DIRECTION('center_axis',(0.,-1.,-2.22044604925031E-16));
#110658=DIRECTION('ref_axis',(0.707106781186543,-1.57009245868379E-16,0.707106781186552));
#110659=DIRECTION('center_axis',(0.,1.,2.22044604925031E-16));
#110660=DIRECTION('ref_axis',(-0.707106781186541,1.57009245868379E-16,-0.707106781186554));
#110661=DIRECTION('center_axis',(0.,1.,2.22044604925031E-16));
#110662=DIRECTION('ref_axis',(-0.707106781186541,1.57009245868379E-16,-0.707106781186554));
#110663=DIRECTION('',(0.,1.,2.22044604925031E-16));
#110664=DIRECTION('center_axis',(0.,1.,2.22044604925031E-16));
#110665=DIRECTION('ref_axis',(-0.707106781186541,1.57009245868379E-16,-0.707106781186554));
#110666=DIRECTION('',(0.,-1.,-2.22044604925031E-16));
#110667=DIRECTION('center_axis',(0.,2.22044604925031E-16,-1.));
#110668=DIRECTION('ref_axis',(-1.,0.,0.));
#110669=DIRECTION('',(1.,0.,0.));
#110670=DIRECTION('',(0.,-1.,-2.22044604925031E-16));
#110671=DIRECTION('',(1.,0.,0.));
#110672=DIRECTION('center_axis',(0.,-1.,-2.22044604925031E-16));
#110673=DIRECTION('ref_axis',(0.707106781186548,-1.57009245868377E-16,0.707106781186548));
#110674=DIRECTION('center_axis',(0.,-1.,-2.22044604925031E-16));
#110675=DIRECTION('ref_axis',(0.707106781186548,-1.57009245868377E-16,0.707106781186548));
#110676=DIRECTION('',(0.,1.,2.22044604925031E-16));
#110677=DIRECTION('center_axis',(0.,-1.,-2.22044604925031E-16));
#110678=DIRECTION('ref_axis',(0.707106781186548,-1.57009245868377E-16,0.707106781186548));
#110679=DIRECTION('center_axis',(0.,1.,2.22044604925031E-16));
#110680=DIRECTION('ref_axis',(0.89959196856447,-9.69738446503996E-17,0.436731370632224));
#110681=DIRECTION('center_axis',(0.,-1.,-2.22044604925031E-16));
#110682=DIRECTION('ref_axis',(0.89959196856447,-9.69738446503996E-17,0.436731370632224));
#110683=DIRECTION('center_axis',(0.,1.,2.22044604925031E-16));
#110684=DIRECTION('ref_axis',(0.89959196856447,-9.69738446503996E-17,0.436731370632224));
#110685=DIRECTION('center_axis',(0.,-1.,-2.22044604925031E-16));
#110686=DIRECTION('ref_axis',(1.,0.,0.));
#110687=DIRECTION('center_axis',(0.,1.,2.22044604925031E-16));
#110688=DIRECTION('ref_axis',(0.707106781186548,-1.57009245868377E-16,0.707106781186548));
#110689=DIRECTION('',(-1.88205007134457E-12,2.22044604925031E-16,-1.));
#110690=DIRECTION('center_axis',(0.,1.,2.22044604925031E-16));
#110691=DIRECTION('ref_axis',(-0.923879532511647,0.,-0.382683432364221));
#110692=DIRECTION('center_axis',(0.,-1.,0.));
#110693=DIRECTION('ref_axis',(-0.545776822909828,0.,0.837930581596384));
#110694=DIRECTION('',(4.17479820231099E-30,1.,7.84929678246568E-44));
#110695=DIRECTION('center_axis',(0.,1.,2.22044604925031E-16));
#110696=DIRECTION('ref_axis',(-0.545776822909828,0.,0.837930581596384));
#110697=DIRECTION('center_axis',(0.,1.,1.60901887626834E-16));
#110698=DIRECTION('ref_axis',(0.371940837143503,0.,0.92825643744872));
#110699=DIRECTION('center_axis',(4.05090206454524E-44,-1.,-2.22044604925031E-16));
#110700=DIRECTION('ref_axis',(-0.707106781185726,-1.5700924586856E-16,0.707106781187369));
#110701=DIRECTION('center_axis',(0.707106781185727,2.27549631693565E-16,
-0.707106781187368));
#110702=DIRECTION('ref_axis',(-0.707106781187368,1.61919227945235E-16,-0.707106781185727));
#110703=DIRECTION('',(8.41078048960407E-18,1.,2.77555756156289E-16));
#110704=DIRECTION('',(0.707106781187368,-1.57009245868195E-16,0.707106781185727));
#110705=DIRECTION('center_axis',(8.41078048960409E-18,1.,2.77555756156289E-16));
#110706=DIRECTION('ref_axis',(-0.382683432364555,0.,0.923879532511508));
#110707=DIRECTION('center_axis',(1.93528837224907E-48,1.,2.22044604925031E-16));
#110708=DIRECTION('ref_axis',(-0.707106781185727,-1.5700924586856E-16,0.707106781187368));
#110709=DIRECTION('center_axis',(0.683267731942997,-2.89517588606287E-16,
0.730167930332108));
#110710=DIRECTION('ref_axis',(-0.730167930332108,-1.86856382700881E-16,
0.683267731942997));
#110711=DIRECTION('',(0.730167930332109,1.51715913597305E-16,-0.683267731942995));
#110712=DIRECTION('',(-1.27117486340087E-16,-1.,-2.77555756156289E-16));
#110713=DIRECTION('',(-0.730167930332108,-1.51715913597305E-16,0.683267731942997));
#110714=DIRECTION('',(0.,-1.,-2.22044604925031E-16));
#110715=DIRECTION('center_axis',(-1.27117486340087E-16,-1.,-2.77555756156289E-16));
#110716=DIRECTION('ref_axis',(0.367309181526879,0.,0.930098900744461));
#110717=DIRECTION('center_axis',(-1.069105884037E-48,1.,2.22044604925031E-16));
#110718=DIRECTION('ref_axis',(-1.38777878078144E-15,-2.22044604925031E-16,
1.));
#110719=DIRECTION('center_axis',(0.,1.,2.22044604925031E-16));
#110720=DIRECTION('ref_axis',(0.367309181526879,0.,0.930098900744461));
#110721=DIRECTION('center_axis',(1.,4.28276345240491E-28,-1.88249434430459E-12));
#110722=DIRECTION('ref_axis',(-1.88249434430459E-12,2.22049474265623E-16,
-1.));
#110723=DIRECTION('',(1.88249434430459E-12,-2.22044604925031E-16,1.));
#110724=DIRECTION('',(0.,1.,2.27504718160893E-16));
#110725=DIRECTION('',(1.88249434430459E-12,-2.22044604925031E-16,1.));
#110726=DIRECTION('',(8.56552690482593E-29,-1.,-1.82003774528629E-16));
#110727=DIRECTION('',(7.83875492500777E-29,1.,2.69144975666705E-16));
#110728=DIRECTION('',(1.88259220622152E-12,-2.22049474265488E-16,1.));
#110729=DIRECTION('',(-1.02786322857718E-29,1.,2.22044604925031E-16));
#110730=DIRECTION('center_axis',(-8.56552690482593E-29,1.,1.82003774528629E-16));
#110731=DIRECTION('ref_axis',(-0.923879532510705,0.,0.382683432366494));
#110732=DIRECTION('center_axis',(0.,-1.,-2.22044604925031E-16));
#110733=DIRECTION('ref_axis',(-0.923879532510705,0.,0.382683432366494));
#110734=DIRECTION('',(-8.56552690482593E-29,1.,1.82003774528629E-16));
#110735=DIRECTION('center_axis',(0.707106781185727,1.28696103170951E-16,
-0.707106781187368));
#110736=DIRECTION('ref_axis',(-0.707106781187368,1.6191922794533E-16,-0.707106781185727));
#110737=DIRECTION('',(-4.004083039641E-17,-1.,-2.22044604925031E-16));
#110738=DIRECTION('',(0.707106781187368,-1.57009245868195E-16,0.707106781185727));
#110739=DIRECTION('center_axis',(4.004083039641E-17,1.,2.22044604925031E-16));
#110740=DIRECTION('ref_axis',(-0.382683432364554,0.,0.923879532511509));
#110741=DIRECTION('center_axis',(0.,-1.,-2.22044604925031E-16));
#110742=DIRECTION('ref_axis',(-0.382683432364554,0.,0.923879532511509));
#110743=DIRECTION('center_axis',(0.,-1.,-2.22044604925031E-16));
#110744=DIRECTION('ref_axis',(1.,0.,0.));
#110745=DIRECTION('center_axis',(0.,-1.,-2.22044604925031E-16));
#110746=DIRECTION('ref_axis',(0.923879532511287,0.,-0.38268343236509));
#110747=DIRECTION('',(-0.707106781186547,1.57009245868378E-16,-0.707106781186548));
#110748=DIRECTION('center_axis',(0.,-1.,-2.22044604925031E-16));
#110749=DIRECTION('ref_axis',(0.707106781186561,1.57009245868375E-16,-0.707106781186534));
#110750=DIRECTION('',(-3.65372513458554E-16,-2.22044604925031E-16,1.));
#110751=DIRECTION('',(-1.190587693968E-16,2.22044604925031E-16,-1.));
#110752=DIRECTION('center_axis',(1.,2.64363574135728E-32,-1.190587693968E-16));
#110753=DIRECTION('ref_axis',(-1.190587693968E-16,2.22044604925031E-16,
-1.));
#110754=DIRECTION('',(-6.50074362628842E-34,-1.,-2.27504718160893E-16));
#110755=DIRECTION('',(1.190587693968E-16,-2.22044604925031E-16,1.));
#110756=DIRECTION('center_axis',(6.50074362628842E-34,1.,2.27504718160893E-16));
#110757=DIRECTION('ref_axis',(0.923879532511287,0.,-0.38268343236509));
#110758=DIRECTION('center_axis',(0.,-1.,-2.22044604925031E-16));
#110759=DIRECTION('ref_axis',(0.923879532511287,0.,-0.38268343236509));
#110760=DIRECTION('',(6.50074362628842E-34,1.,2.27504718160893E-16));
#110761=DIRECTION('center_axis',(0.,1.,2.27504718160893E-16));
#110762=DIRECTION('ref_axis',(-0.923879532511647,0.,-0.382683432364221));
#110763=DIRECTION('',(0.,-1.,-2.27504718160893E-16));
#110764=DIRECTION('center_axis',(0.,1.,2.22044604925031E-16));
#110765=DIRECTION('ref_axis',(-0.923879532511647,0.,-0.382683432364221));
#110766=DIRECTION('center_axis',(0.,1.,2.22044604925031E-16));
#110767=DIRECTION('ref_axis',(-0.136414717731255,-2.19968891577408E-16,
0.990651818141118));
#110768=DIRECTION('',(0.,1.,2.22044604925031E-16));
#110769=DIRECTION('center_axis',(0.,1.,2.22044604925031E-16));
#110770=DIRECTION('ref_axis',(0.683267731942997,-1.62129849619521E-16,0.730167930332107));
#110771=DIRECTION('center_axis',(0.,-1.,-2.22044604925031E-16));
#110772=DIRECTION('ref_axis',(-0.136414717731255,-2.19968891577408E-16,
0.990651818141118));
#110773=DIRECTION('center_axis',(0.,1.,2.22044604925031E-16));
#110774=DIRECTION('ref_axis',(1.,0.,0.));
#110775=DIRECTION('center_axis',(0.,-1.,-2.22044604925031E-16));
#110776=DIRECTION('ref_axis',(-0.986133812836816,0.,-0.165952111104148));
#110777=DIRECTION('',(3.65372513458554E-16,2.22044604925031E-16,-1.));
#110778=DIRECTION('center_axis',(0.,-1.,-2.22044604925031E-16));
#110779=DIRECTION('ref_axis',(0.707106781186561,1.57009245868375E-16,-0.707106781186534));
#110780=DIRECTION('center_axis',(0.,-1.,-2.22044604925031E-16));
#110781=DIRECTION('ref_axis',(1.,0.,0.));
#110782=DIRECTION('center_axis',(0.,1.,2.22044604925031E-16));
#110783=DIRECTION('ref_axis',(-0.986133812836816,0.,-0.165952111104148));
#110784=DIRECTION('',(0.,-1.,-2.22044604925031E-16));
#110785=DIRECTION('center_axis',(0.,-1.,-2.22044604925031E-16));
#110786=DIRECTION('ref_axis',(-0.986133812836816,0.,-0.165952111104148));
#110787=DIRECTION('center_axis',(0.,1.,2.22044604925031E-16));
#110788=DIRECTION('ref_axis',(1.,0.,0.));
#110789=DIRECTION('center_axis',(0.,-1.,-2.22044604925031E-16));
#110790=DIRECTION('ref_axis',(-1.,0.,0.));
#110791=DIRECTION('center_axis',(0.,1.,2.22044604925031E-16));
#110792=DIRECTION('ref_axis',(1.,0.,0.));
#110793=DIRECTION('',(0.,-1.,-2.22044604925031E-16));
#110794=DIRECTION('center_axis',(0.,-1.,-2.22044604925031E-16));
#110795=DIRECTION('ref_axis',(-1.,0.,0.));
#110796=DIRECTION('center_axis',(0.,1.,2.22044604925031E-16));
#110797=DIRECTION('ref_axis',(-0.297808776285592,0.,-0.954625545838408));
#110798=DIRECTION('center_axis',(0.,-1.,-2.22044604925031E-16));
#110799=DIRECTION('ref_axis',(-0.297808776285592,0.,-0.954625545838408));
#110800=DIRECTION('center_axis',(0.,-1.,-2.22044604925031E-16));
#110801=DIRECTION('ref_axis',(-0.297808776285592,0.,-0.954625545838408));
#110802=DIRECTION('center_axis',(0.,1.,2.22044604925031E-16));
#110803=DIRECTION('ref_axis',(1.,0.,0.));
#110804=DIRECTION('center_axis',(0.,-1.,-2.22044604925031E-16));
#110805=DIRECTION('ref_axis',(-1.,0.,0.));
#110806=DIRECTION('center_axis',(0.,-1.,-2.22044604925031E-16));
#110807=DIRECTION('ref_axis',(-1.,0.,0.));
#110808=DIRECTION('',(0.,-1.,-2.22044604925031E-16));
#110809=DIRECTION('center_axis',(0.,1.,2.22044604925031E-16));
#110810=DIRECTION('ref_axis',(-1.,0.,0.));
#110811=DIRECTION('center_axis',(0.,1.,2.22044604925031E-16));
#110812=DIRECTION('ref_axis',(-1.,0.,0.));
#110813=DIRECTION('center_axis',(0.,1.,2.22044604925031E-16));
#110814=DIRECTION('ref_axis',(-1.,0.,0.));
#110815=DIRECTION('center_axis',(0.,1.,0.));
#110816=DIRECTION('ref_axis',(-1.,0.,0.));
#110817=DIRECTION('',(-0.707106781186548,-0.707106781186548,8.65956056235493E-17));
#110818=DIRECTION('center_axis',(-0.866025403784439,3.06268420586249E-17,
-0.5));
#110819=DIRECTION('ref_axis',(0.5,1.95761498617786E-16,-0.866025403784439));
#110820=DIRECTION('',(6.96245110587154E-17,-1.,-1.81846874723086E-16));
#110821=DIRECTION('',(-0.5,-1.92296268638356E-16,0.866025403784439));
#110822=DIRECTION('',(-7.52889106048643E-17,1.,1.91657902531386E-16));
#110823=DIRECTION('center_axis',(0.,1.,2.22044604925031E-16));
#110824=DIRECTION('ref_axis',(1.,0.,0.));
#110825=DIRECTION('center_axis',(0.,-1.,-2.22044604925031E-16));
#110826=DIRECTION('ref_axis',(0.641711497466635,0.,0.766946121979327));
#110827=DIRECTION('',(1.,2.73910036535074E-32,-1.2335811384724E-16));
#110828=DIRECTION('center_axis',(0.,-1.,-2.22044604925031E-16));
#110829=DIRECTION('ref_axis',(-0.641711497466635,0.,0.766946121979327));
#110830=DIRECTION('center_axis',(0.,1.,2.22044604925031E-16));
#110831=DIRECTION('ref_axis',(0.98683190526879,0.,-0.161749159947031));
#110832=DIRECTION('',(-2.10803227901262E-16,-2.22044604925031E-16,1.));
#110833=DIRECTION('center_axis',(0.,1.,2.22044604925031E-16));
#110834=DIRECTION('ref_axis',(0.707106781186547,0.,0.707106781186548));
#110835=DIRECTION('',(1.,-5.3377249763659E-32,2.40389762145677E-16));
#110836=DIRECTION('center_axis',(0.,-1.,-2.22044604925031E-16));
#110837=DIRECTION('ref_axis',(-0.59469196781642,0.,-0.80395364506583));
#110838=DIRECTION('center_axis',(0.,-1.,-2.22044604925031E-16));
#110839=DIRECTION('ref_axis',(-0.650397979794319,0.,-0.759593620220357));
#110840=DIRECTION('',(-1.,-2.73910036535074E-32,1.2335811384724E-16));
#110841=DIRECTION('center_axis',(0.,-1.,-2.22044604925031E-16));
#110842=DIRECTION('ref_axis',(0.650397979794315,0.,-0.759593620220361));
#110843=DIRECTION('center_axis',(0.,1.,2.22044604925031E-16));
#110844=DIRECTION('ref_axis',(-0.707106781186548,0.,-0.707106781186548));
#110845=DIRECTION('',(-1.,5.3377249763659E-32,-2.40389762145677E-16));
#110846=DIRECTION('center_axis',(0.,-1.,-2.22044604925031E-16));
#110847=DIRECTION('ref_axis',(0.707106781186547,0.,-0.707106781186548));
#110848=DIRECTION('',(2.41949676183277E-16,2.22044604925031E-16,-1.));
#110849=DIRECTION('center_axis',(0.,-1.,-2.22044604925031E-16));
#110850=DIRECTION('ref_axis',(-1.,1.45619093356108E-31,-6.0908498285001E-16));
#110851=DIRECTION('center_axis',(0.,-1.,-2.22044604925031E-16));
#110852=DIRECTION('ref_axis',(0.664346409066274,0.,-0.747424811443096));
#110853=DIRECTION('center_axis',(0.,-1.,-2.22044604925031E-16));
#110854=DIRECTION('ref_axis',(0.707106781186561,1.57009245868375E-16,-0.707106781186534));
#110855=DIRECTION('center_axis',(0.,1.,2.22044604925031E-16));
#110856=DIRECTION('ref_axis',(0.707106781186548,-1.57009245868377E-16,0.707106781186548));
#110857=DIRECTION('center_axis',(7.52889106048643E-17,-1.,-1.91657902531386E-16));
#110858=DIRECTION('ref_axis',(-0.945459087052696,0.,0.325740870492916));
#110859=DIRECTION('center_axis',(0.,1.,2.22044604925031E-16));
#110860=DIRECTION('ref_axis',(-0.945459087052696,0.,0.325740870492916));
#110861=DIRECTION('center_axis',(0.,-2.22044604925031E-16,1.));
#110862=DIRECTION('ref_axis',(1.,0.,0.));
#110863=DIRECTION('center_axis',(0.,0.880412421871567,0.474208780406102));
#110864=DIRECTION('ref_axis',(0.,0.474208780406102,-0.880412421871567));
#110865=DIRECTION('center_axis',(-3.94297421746172E-16,-0.913923057046371,
0.405887479234104));
#110866=DIRECTION('ref_axis',(0.,-0.405887479234104,-0.913923057046371));
#110867=DIRECTION('',(0.,-2.22044604925031E-16,1.));
#110868=DIRECTION('center_axis',(2.37859513600921E-17,-0.866025403784432,
-0.500000000000011));
#110869=DIRECTION('ref_axis',(1.586190700722E-16,-0.500000000000011,0.866025403784432));
#110870=DIRECTION('center_axis',(-2.37859513600921E-17,0.866025403784432,
0.500000000000011));
#110871=DIRECTION('ref_axis',(0.,-0.500000000000011,0.866025403784432));
#110872=DIRECTION('center_axis',(2.37859513600921E-17,-0.866025403784432,
-0.500000000000011));
#110873=DIRECTION('ref_axis',(0.,-0.500000000000011,0.866025403784432));
#110874=DIRECTION('',(-1.,-9.86864910777917E-17,1.2335811384724E-16));
#110875=DIRECTION('center_axis',(2.37859513600921E-17,-0.866025403784432,
-0.500000000000011));
#110876=DIRECTION('ref_axis',(-3.0046291974743E-16,-0.500000000000011,0.866025403784432));
#110877=DIRECTION('center_axis',(1.2335811384724E-16,1.06734344607313E-15,
1.));
#110878=DIRECTION('ref_axis',(-1.11022302462516E-16,1.,-1.06734344607313E-15));
#110879=DIRECTION('',(1.59056477988302E-31,-1.,1.06734344607313E-15));
#110880=DIRECTION('',(-1.,-2.73910036535073E-32,1.2335811384724E-16));
#110881=DIRECTION('',(-1.59056477988302E-31,1.,-1.06734344607313E-15));
#110882=DIRECTION('',(-1.,-9.86864910777917E-17,1.2335811384724E-16));
#110883=DIRECTION('center_axis',(-1.2335811384724E-16,4.26937378429254E-16,
-1.));
#110884=DIRECTION('ref_axis',(1.11022302462516E-16,-1.,-4.26937378429254E-16));
#110885=DIRECTION('',(2.52751860804106E-32,1.,4.26937378429254E-16));
#110886=DIRECTION('',(-1.,-9.86864910777917E-17,1.2335811384724E-16));
#110887=DIRECTION('',(-2.52751860804106E-32,-1.,-4.26937378429254E-16));
#110888=DIRECTION('',(1.,2.73910036535074E-32,-1.2335811384724E-16));
#110889=DIRECTION('center_axis',(-1.51594548245566E-16,0.819152044288998,
-0.573576436351038));
#110890=DIRECTION('ref_axis',(-3.3847457739984E-17,-0.573576436351038,-0.819152044288998));
#110891=DIRECTION('center_axis',(1.51594548245566E-16,-0.819152044288998,
0.573576436351038));
#110892=DIRECTION('ref_axis',(9.28221823687422E-33,0.573576436351038,0.819152044288998));
#110893=DIRECTION('center_axis',(-1.51594548245566E-16,0.819152044288998,
-0.573576436351038));
#110894=DIRECTION('ref_axis',(2.13150342243378E-16,0.573576436351038,0.819152044288998));
#110895=DIRECTION('center_axis',(-1.51594548245566E-16,0.819152044288998,
-0.573576436351038));
#110896=DIRECTION('ref_axis',(2.13150342243378E-16,0.573576436351038,0.819152044288998));
#110897=DIRECTION('center_axis',(-1.2335811384724E-16,6.93700665664735E-16,
-1.));
#110898=DIRECTION('ref_axis',(1.11022302462516E-16,-1.,-6.93700665664735E-16));
#110899=DIRECTION('',(-5.8182602037469E-32,-1.,-6.93700665664735E-16));
#110900=DIRECTION('',(5.8182602037469E-32,1.,6.93700665664735E-16));
#110901=DIRECTION('center_axis',(0.,1.,2.22044604925031E-16));
#110902=DIRECTION('ref_axis',(-0.641711497466635,0.,0.766946121979327));
#110903=DIRECTION('center_axis',(0.,-1.,-2.22044604925031E-16));
#110904=DIRECTION('ref_axis',(0.641711497466635,0.,0.766946121979327));
#110905=DIRECTION('center_axis',(0.,-1.,-2.22044604925031E-16));
#110906=DIRECTION('ref_axis',(0.641711497466635,0.,0.766946121979327));
#110907=DIRECTION('center_axis',(0.,-1.,-2.22044604925031E-16));
#110908=DIRECTION('ref_axis',(0.641711497466635,0.,0.766946121979327));
#110909=DIRECTION('center_axis',(0.,1.,2.22044604925031E-16));
#110910=DIRECTION('ref_axis',(-0.641711497466633,0.,0.766946121979329));
#110911=DIRECTION('center_axis',(0.,-1.,-2.22044604925031E-16));
#110912=DIRECTION('ref_axis',(-0.641711497466633,0.,0.766946121979329));
#110913=DIRECTION('center_axis',(0.,1.,2.22044604925031E-16));
#110914=DIRECTION('ref_axis',(0.650397979794315,0.,-0.759593620220361));
#110915=DIRECTION('center_axis',(0.,-1.,-2.22044604925031E-16));
#110916=DIRECTION('ref_axis',(0.650397979794315,0.,-0.759593620220361));
#110917=DIRECTION('center_axis',(-1.00839335745948E-17,0.819152044288994,
0.573576436351042));
#110918=DIRECTION('ref_axis',(0.,0.573576436351042,-0.819152044288994));
#110919=DIRECTION('center_axis',(0.,-1.,-2.22044604925031E-16));
#110920=DIRECTION('ref_axis',(-0.650397979794316,0.,-0.75959362022036));
#110921=DIRECTION('center_axis',(0.,-1.,-2.22044604925031E-16));
#110922=DIRECTION('ref_axis',(-0.650397979794316,0.,-0.75959362022036));
#110923=DIRECTION('center_axis',(-1.00839335745948E-17,0.819152044288994,
0.573576436351042));
#110924=DIRECTION('ref_axis',(-1.42100228162251E-16,0.573576436351042,-0.819152044288995));
#110925=DIRECTION('center_axis',(1.2335811384724E-16,-1.72794927465785E-15,
1.));
#110926=DIRECTION('ref_axis',(-1.11022302462516E-16,1.,1.72794927465785E-15));
#110927=DIRECTION('',(-1.85765559691991E-31,-1.,-1.72794927465785E-15));
#110928=DIRECTION('',(-1.,-9.86864910777917E-17,1.2335811384724E-16));
#110929=DIRECTION('',(1.85765559691991E-31,1.,1.72794927465785E-15));
#110930=DIRECTION('center_axis',(0.,-1.,-2.22044604925031E-16));
#110931=DIRECTION('ref_axis',(-0.650397979794319,0.,-0.759593620220357));
#110932=DIRECTION('center_axis',(1.47144065207334E-16,-0.866025403784436,
0.500000000000005));
#110933=DIRECTION('ref_axis',(-3.75578649684289E-16,-0.500000000000005,
-0.866025403784436));
#110934=DIRECTION('center_axis',(0.,1.,2.22044604925031E-16));
#110935=DIRECTION('ref_axis',(0.650397979794315,0.,-0.759593620220361));
#110936=DIRECTION('center_axis',(1.47144065207334E-16,-0.866025403784436,
0.500000000000005));
#110937=DIRECTION('ref_axis',(-7.51157299368577E-17,-0.500000000000005,
-0.866025403784436));
#110938=DIRECTION('center_axis',(1.47144065207334E-16,-0.866025403784436,
0.500000000000005));
#110939=DIRECTION('ref_axis',(4.7596767609683E-17,0.500000000000005,0.866025403784436));
#110940=DIRECTION('center_axis',(-1.47144065207334E-16,0.866025403784436,
-0.500000000000005));
#110941=DIRECTION('ref_axis',(0.,-0.500000000000005,-0.866025403784436));
#110942=DIRECTION('center_axis',(0.,-0.913923057046369,-0.40588747923411));
#110943=DIRECTION('ref_axis',(0.,-0.40588747923411,0.913923057046369));
#110944=DIRECTION('center_axis',(0.736991631393267,0.387681384808809,0.553666396965732));
#110945=DIRECTION('ref_axis',(0.,-0.819152044288996,0.57357643635104));
#110946=DIRECTION('center_axis',(0.,0.880412421871569,-0.474208780406097));
#110947=DIRECTION('ref_axis',(0.,0.474208780406097,0.880412421871569));
#110948=DIRECTION('center_axis',(-1.00839335745948E-17,0.819152044288994,
0.573576436351042));
#110949=DIRECTION('ref_axis',(-1.61207010943858E-16,0.573576436351042,-0.819152044288994));
#110950=DIRECTION('center_axis',(1.00839335745948E-17,-0.819152044288994,
-0.573576436351042));
#110951=DIRECTION('ref_axis',(-6.17444843556704E-34,0.573576436351042,-0.819152044288995));
#110952=DIRECTION('center_axis',(0.,1.,2.22044604925031E-16));
#110953=DIRECTION('ref_axis',(0.664346409066274,0.,-0.747424811443096));
#110954=DIRECTION('center_axis',(0.,-1.,-2.22044604925031E-16));
#110955=DIRECTION('ref_axis',(0.664346409066274,0.,-0.747424811443096));
#110956=DIRECTION('',(0.,-1.,-2.22044604925031E-16));
#110957=DIRECTION('center_axis',(4.78544407166016E-17,-1.,-6.12536841172497E-17));
#110958=DIRECTION('ref_axis',(-0.707106781186548,0.,-0.707106781186548));
#110959=DIRECTION('',(-4.78544407166016E-17,1.,6.12536841172497E-17));
#110960=DIRECTION('center_axis',(-4.30715231393665E-32,-1.,-6.12536841172497E-17));
#110961=DIRECTION('ref_axis',(0.707106781186547,0.,-0.707106781186548));
#110962=DIRECTION('',(4.30715231393665E-32,1.,6.12536841172497E-17));
#110963=DIRECTION('',(-4.30715231393665E-32,-1.,-6.12536841172497E-17));
#110964=DIRECTION('center_axis',(2.40389762145677E-16,6.12536841172497E-17,
-1.));
#110965=DIRECTION('ref_axis',(1.,6.93889390390718E-18,2.40389762145677E-16));
#110966=DIRECTION('center_axis',(0.,-1.,-2.22044604925031E-16));
#110967=DIRECTION('ref_axis',(-0.398898296183895,0.,-0.916995174088493));
#110968=DIRECTION('center_axis',(0.,-1.,-2.22044604925031E-16));
#110969=DIRECTION('ref_axis',(-0.398898296183895,0.,-0.916995174088493));
#110970=DIRECTION('center_axis',(0.,1.,2.69144975666705E-16));
#110971=DIRECTION('ref_axis',(0.877755401836952,0.,-0.479109021566127));
#110972=DIRECTION('',(9.91356230361479E-29,-1.,-2.69144975666705E-16));
#110973=DIRECTION('center_axis',(0.,-1.,-2.22044604925031E-16));
#110974=DIRECTION('ref_axis',(0.877755401836952,0.,-0.479109021566127));
#110975=DIRECTION('',(0.,1.,2.69144975666705E-16));
#110976=DIRECTION('center_axis',(0.,1.,2.69144975666705E-16));
#110977=DIRECTION('ref_axis',(-0.674528301887451,-1.98696006215612E-16,
0.738248989130924));
#110978=DIRECTION('',(0.,-1.,-2.69144975666705E-16));
#110979=DIRECTION('center_axis',(0.,1.,2.22044604925031E-16));
#110980=DIRECTION('ref_axis',(-0.674528301887451,-1.98696006215612E-16,
0.738248989130924));
#110981=DIRECTION('center_axis',(0.,1.,2.69144975666705E-16));
#110982=DIRECTION('ref_axis',(-0.439524536496337,0.,-0.898230583880153));
#110983=DIRECTION('center_axis',(0.,-1.,-2.22044604925031E-16));
#110984=DIRECTION('ref_axis',(-0.439524536496337,0.,-0.898230583880153));
#110985=DIRECTION('center_axis',(0.,1.,2.22044604925031E-16));
#110986=DIRECTION('ref_axis',(1.,0.,0.));
#110987=DIRECTION('center_axis',(0.,-1.,-2.22044604925031E-16));
#110988=DIRECTION('ref_axis',(-0.385275875185828,0.,-0.922801441264476));
#110989=DIRECTION('',(-1.88260317010131E-12,2.22044604925031E-16,-1.));
#110990=DIRECTION('center_axis',(0.,1.,2.22044604925031E-16));
#110991=DIRECTION('ref_axis',(0.707106781186561,1.57009245868375E-16,-0.707106781186534));
#110992=DIRECTION('center_axis',(0.,1.,2.22044604925031E-16));
#110993=DIRECTION('ref_axis',(-0.385275875185828,0.,-0.922801441264476));
#110994=DIRECTION('center_axis',(0.,-1.,-2.22044604925031E-16));
#110995=DIRECTION('ref_axis',(-0.385275875185828,0.,-0.922801441264476));
#110996=DIRECTION('center_axis',(0.,-1.,-2.22044604925031E-16));
#110997=DIRECTION('ref_axis',(-0.59469196781642,0.,-0.80395364506583));
#110998=DIRECTION('center_axis',(-2.40389762145677E-16,-2.52671446983656E-16,
1.));
#110999=DIRECTION('ref_axis',(-1.,-6.93889390390718E-18,-2.40389762145677E-16));
#111000=DIRECTION('',(-4.78544407166016E-17,1.,2.52671446983656E-16));
#111001=DIRECTION('center_axis',(4.78544407166016E-17,-1.,-2.52671446983656E-16));
#111002=DIRECTION('ref_axis',(0.707106781186547,0.,0.707106781186548));
#111003=DIRECTION('',(4.78544407166016E-17,-1.,-2.52671446983656E-16));
#111004=DIRECTION('center_axis',(-1.,-4.78544407166015E-17,-2.10803227901262E-16));
#111005=DIRECTION('ref_axis',(2.10803227901262E-16,2.28983498828939E-16,
-1.));
#111006=DIRECTION('',(-4.78544407166015E-17,1.,7.99864431349418E-17));
#111007=DIRECTION('center_axis',(-4.78544407166015E-17,1.,7.99864431349418E-17));
#111008=DIRECTION('ref_axis',(0.98683190526879,0.,-0.161749159947031));
#111009=DIRECTION('center_axis',(0.,-1.,-2.22044604925031E-16));
#111010=DIRECTION('ref_axis',(0.707106781186548,-1.57009245868377E-16,0.707106781186548));
#111011=DIRECTION('center_axis',(0.,-1.,-2.39272203583008E-16));
#111012=DIRECTION('ref_axis',(-1.,1.45619093356108E-31,-6.0908498285001E-16));
#111013=DIRECTION('',(0.,-1.,-2.39272203583008E-16));
#111014=DIRECTION('center_axis',(1.,-5.78918321765678E-32,2.41949676183277E-16));
#111015=DIRECTION('ref_axis',(-2.41949676183277E-16,-2.22049474265475E-16,
1.));
#111016=DIRECTION('center_axis',(0.,-1.,-2.22044604925031E-16));
#111017=DIRECTION('ref_axis',(0.707106781186561,1.57009245868375E-16,-0.707106781186534));
#111018=DIRECTION('',(0.,-1.,-2.22044604925031E-16));
#111019=DIRECTION('center_axis',(1.,-4.17479820231099E-30,1.88016196282748E-14));
#111020=DIRECTION('ref_axis',(-1.88016196282748E-14,-2.22044604925031E-16,
1.));
#111021=DIRECTION('',(-1.88016196282748E-14,-2.22044604925031E-16,1.));
#111022=DIRECTION('center_axis',(1.,6.05828807443126E-28,-1.88260317010131E-12));
#111023=DIRECTION('ref_axis',(-1.88260317010131E-12,2.22049474265488E-16,
-1.));
#111024=DIRECTION('',(-8.96831017167883E-44,1.,3.21803775253669E-16));
#111025=DIRECTION('center_axis',(0.,1.,3.21803775253669E-16));
#111026=DIRECTION('ref_axis',(-0.923879532510705,0.,0.382683432366495));
#111027=DIRECTION('center_axis',(-1.23192613759945E-16,2.22044604925031E-16,
-1.));
#111028=DIRECTION('ref_axis',(0.555094454892529,0.831787320261355,1.17579893590648E-16));
#111029=DIRECTION('center_axis',(1.23192613759945E-16,0.,1.));
#111030=DIRECTION('ref_axis',(0.791958354931176,0.610575109265604,-1.02206428667277E-16));
#111031=DIRECTION('center_axis',(6.93889390390722E-18,1.,2.22049474265475E-16));
#111032=DIRECTION('ref_axis',(-1.,6.93889390390721E-18,1.83750175990302E-19));
#111033=DIRECTION('center_axis',(0.808736084303188,0.,-0.588171697675047));
#111034=DIRECTION('ref_axis',(-0.588171697675046,-5.25462354708949E-17,
-0.808736084303188));
#111035=DIRECTION('center_axis',(-0.707106781186548,-1.60870128963501E-16,
0.707106781186547));
#111036=DIRECTION('ref_axis',(0.707106781186547,-1.61919227945507E-16,0.707106781186548));
#111037=DIRECTION('',(-0.707106781186547,1.57009245868378E-16,-0.707106781186548));
#111038=DIRECTION('',(-6.34155293819033E-44,-1.,-2.27504718160893E-16));
#111039=DIRECTION('',(-0.707106781186547,1.57009245868378E-16,-0.707106781186547));
#111040=DIRECTION('center_axis',(6.34155293819033E-44,1.,2.27504718160893E-16));
#111041=DIRECTION('ref_axis',(-0.923879532510926,0.,0.38268343236596));
#111042=DIRECTION('center_axis',(0.,1.,2.22044604925031E-16));
#111043=DIRECTION('ref_axis',(-0.923879532510926,0.,0.38268343236596));
#111044=DIRECTION('',(0.,1.,2.77555756156289E-16));
#111045=DIRECTION('center_axis',(4.32964835625641E-44,-1.,-2.22044604925031E-16));
#111046=DIRECTION('ref_axis',(-1.,-4.17772723536479E-28,1.88148108204444E-12));
#111047=DIRECTION('center_axis',(-1.,-4.28175312849965E-28,1.88205025509474E-12));
#111048=DIRECTION('ref_axis',(1.88205025509474E-12,-2.22049474265623E-16,
1.));
#111049=DIRECTION('',(-1.88205025509474E-12,2.22044604925031E-16,-1.));
#111050=DIRECTION('',(-1.88221415680549E-12,2.22044604925031E-16,-1.));
#111051=DIRECTION('center_axis',(0.,-1.,-2.77555756156289E-16));
#111052=DIRECTION('ref_axis',(-1.,0.,0.));
#111053=DIRECTION('center_axis',(-4.3296825676447E-44,1.,2.22044604925031E-16));
#111054=DIRECTION('ref_axis',(-1.,-4.3296825676447E-44,-9.61382655183462E-60));
#111055=DIRECTION('center_axis',(0.,-2.22044604925031E-16,1.));
#111056=DIRECTION('ref_axis',(1.,0.,0.));
#111057=DIRECTION('',(0.,-2.22044604925031E-16,1.));
#111058=DIRECTION('center_axis',(0.,-1.,-2.22044604925031E-16));
#111059=DIRECTION('ref_axis',(1.,0.,0.));
#111060=DIRECTION('center_axis',(0.,1.,2.22044604925031E-16));
#111061=DIRECTION('ref_axis',(0.923879532510927,0.,-0.382683432365958));
#111062=DIRECTION('center_axis',(0.,1.,2.27504718160893E-16));
#111063=DIRECTION('ref_axis',(0.923879532510927,0.,-0.382683432365958));
#111064=DIRECTION('center_axis',(0.,-1.,-2.22044604925031E-16));
#111065=DIRECTION('ref_axis',(0.923879532510927,0.,-0.382683432365958));
#111066=DIRECTION('center_axis',(0.,1.,2.22044604925031E-16));
#111067=DIRECTION('ref_axis',(-1.,2.71926214689378E-32,-1.22464679914735E-16));
#111068=DIRECTION('center_axis',(0.866025403784439,1.26335723491828E-16,
-0.5));
#111069=DIRECTION('ref_axis',(0.5,-1.88822604713879E-16,0.866025403784439));
#111070=DIRECTION('',(-0.5,1.92296268638356E-16,-0.866025403784439));
#111071=DIRECTION('center_axis',(0.,1.,2.22044604925031E-16));
#111072=DIRECTION('ref_axis',(-1.,2.71926214689378E-32,-1.22464679914735E-16));
#111073=DIRECTION('center_axis',(0.,1.,2.22044604925031E-16));
#111074=DIRECTION('ref_axis',(1.,0.,0.));
#111075=DIRECTION('axis',(0.,0.,1.));
#111076=DIRECTION('refdir',(1.,0.,0.));
#111077=DIRECTION('center_axis',(-0.707106781186547,8.2927418592453E-17,
-0.707106781186548));
#111078=DIRECTION('ref_axis',(-0.707106781186548,-7.08402960210301E-17,
0.707106781186547));
#111079=DIRECTION('',(-0.707106781186548,-7.04136402448282E-17,0.707106781186547));
#111080=DIRECTION('',(8.39504102067944E-47,-1.,-1.17277080066038E-16));
#111081=DIRECTION('',(0.707106781186548,7.04136402448282E-17,-0.707106781186547));
#111082=DIRECTION('',(0.,1.,1.17277080066038E-16));
#111083=DIRECTION('center_axis',(-0.707106781186547,8.2927418592453E-17,
-0.707106781186548));
#111084=DIRECTION('ref_axis',(-0.707106781186548,-7.08402960210301E-17,
0.707106781186547));
#111085=DIRECTION('',(0.707106781186548,7.04136402448282E-17,-0.707106781186547));
#111086=DIRECTION('',(0.,1.,1.17277080066038E-16));
#111087=DIRECTION('',(-0.707106781186548,-7.04136402448282E-17,0.707106781186547));
#111088=DIRECTION('',(8.39504102067944E-47,-1.,-1.17277080066038E-16));
#111089=DIRECTION('center_axis',(8.40594773455218E-47,-1.,-9.9579925010296E-17));
#111090=DIRECTION('ref_axis',(-1.,-8.46731860157208E-47,6.16297582203915E-33));
#111091=DIRECTION('',(1.55426471955831E-12,9.9579925010296E-17,-1.));
#111092=DIRECTION('',(6.16297582203915E-33,-9.9579925010296E-17,1.));
#111093=DIRECTION('center_axis',(8.40594773455218E-47,-1.,-9.9579925010296E-17));
#111094=DIRECTION('ref_axis',(-1.,-8.46731860157208E-47,6.16297582203915E-33));
#111095=DIRECTION('',(6.16297582203915E-33,-9.9579925010296E-17,1.));
#111096=DIRECTION('center_axis',(-8.40594773455218E-47,1.,9.9579925010296E-17));
#111097=DIRECTION('ref_axis',(0.12,-9.88603496856012E-17,0.992773891679268));
#111098=DIRECTION('center_axis',(-8.40594773455218E-47,1.,9.9579925010296E-17));
#111099=DIRECTION('ref_axis',(1.,8.46731860157208E-47,-6.16297582203915E-33));
#111100=DIRECTION('center_axis',(-8.40594773455218E-47,1.,9.9579925010296E-17));
#111101=DIRECTION('ref_axis',(0.0625000000000002,9.93852426637541E-17,-0.998044963916957));
#111102=DIRECTION('',(6.16297582203915E-33,-9.9579925010296E-17,1.));
#111103=DIRECTION('',(0.707106781186551,-7.04136402448278E-17,0.707106781186544));
#111104=DIRECTION('',(-8.88178419700125E-16,-9.9579925010296E-17,1.));
#111105=DIRECTION('center_axis',(8.40594773455218E-47,-1.,-9.9579925010296E-17));
#111106=DIRECTION('ref_axis',(-0.923879532511287,-3.81075874975982E-17,
0.382683432365088));
#111107=DIRECTION('',(-0.707106781186546,7.04136402448283E-17,-0.707106781186548));
#111108=DIRECTION('center_axis',(8.40594773455218E-47,-1.,-9.9579925010296E-17));
#111109=DIRECTION('ref_axis',(-0.38268343236509,-9.19998545660213E-17,0.923879532511287));
#111110=DIRECTION('',(1.,8.46731860157208E-47,-6.16297582203915E-33));
#111111=DIRECTION('',(6.16297582203915E-33,-9.9579925010296E-17,1.));
#111112=DIRECTION('',(-0.707106781186547,7.04136402448282E-17,-0.707106781186548));
#111113=DIRECTION('center_axis',(8.40594773455218E-47,-1.,-9.9579925010296E-17));
#111114=DIRECTION('ref_axis',(-1.,-8.46731860157208E-47,6.16297582203915E-33));
#111115=DIRECTION('',(1.55426471955831E-12,9.9579925010296E-17,-1.));
#111116=DIRECTION('',(-0.899167304897951,-4.35766755619441E-17,0.437605024882661));
#111117=DIRECTION('center_axis',(6.9388939039071E-18,1.,9.95799250102971E-17));
#111118=DIRECTION('ref_axis',(0.999999893270433,-6.98490071851115E-18,0.000462016367098532));
#111119=DIRECTION('center_axis',(8.40594773455218E-47,-1.,-9.9579925010296E-17));
#111120=DIRECTION('ref_axis',(-1.,-8.46731860157208E-47,6.16297582203915E-33));
#111121=DIRECTION('center_axis',(6.9388939039071E-18,1.,9.95799250102971E-17));
#111122=DIRECTION('ref_axis',(0.999999893270433,-6.98490071851115E-18,0.000462016367098532));
#111123=DIRECTION('',(-6.16297582203915E-33,9.95799250102971E-17,-1.));
#111124=DIRECTION('center_axis',(-8.40594773455218E-47,1.,9.9579925010296E-17));
#111125=DIRECTION('ref_axis',(0.12,-9.88603496856012E-17,0.992773891679268));
#111126=DIRECTION('center_axis',(8.40594773455218E-47,-1.,-9.9579925010296E-17));
#111127=DIRECTION('ref_axis',(-0.85146931829632,5.22201532254593E-17,-0.524404424085075));
#111128=DIRECTION('center_axis',(-8.40594773455218E-47,1.,9.9579925010296E-17));
#111129=DIRECTION('ref_axis',(1.,8.46731860157208E-47,-6.16297582203915E-33));
#111130=DIRECTION('center_axis',(8.40594773455218E-47,-1.,-9.9579925010296E-17));
#111131=DIRECTION('ref_axis',(-0.811844140885989,-5.81421498601493E-17,
0.583874208121142));
#111132=DIRECTION('center_axis',(6.9388939039071E-18,1.,9.95799250102971E-17));
#111133=DIRECTION('ref_axis',(0.0625000000000002,9.93852426637541E-17,-0.998044963916957));
#111134=DIRECTION('',(6.16297582203915E-33,-9.9579925010296E-17,1.));
#111135=DIRECTION('',(0.707106781186547,7.04136402448282E-17,-0.707106781186548));
#111136=DIRECTION('',(1.,0.,0.));
#111137=DIRECTION('',(6.16297582203915E-33,-1.14933685332317E-16,1.));
#111138=DIRECTION('',(0.707106781186547,-8.12703882852425E-17,0.707106781186548));
#111139=DIRECTION('center_axis',(0.437605024882661,-8.53227559733209E-17,
0.899167304897951));
#111140=DIRECTION('ref_axis',(0.899167304897951,3.73374490313955E-17,-0.437605024882661));
#111141=DIRECTION('',(8.40384663814132E-47,-1.,-1.02989148852055E-16));
#111142=DIRECTION('',(-0.899167304897951,-4.35766755619441E-17,0.437605024882661));
#111143=DIRECTION('',(0.,-1.,0.));
#111144=DIRECTION('center_axis',(8.40594773455218E-47,-1.,-9.9579925010296E-17));
#111145=DIRECTION('ref_axis',(-1.,-8.46731860157208E-47,6.16297582203915E-33));
#111146=DIRECTION('',(-1.55426471955831E-12,-9.9579925010296E-17,1.));
#111147=DIRECTION('',(-0.707106781186547,8.12703882852425E-17,-0.707106781186548));
#111148=DIRECTION('',(-6.16297582203915E-33,1.14933685332317E-16,-1.));
#111149=DIRECTION('',(-1.,1.15873958031682E-16,1.83750175990223E-19));
#111150=DIRECTION('',(-0.707106781186547,-7.04136402448282E-17,0.707106781186548));
#111151=DIRECTION('',(-6.16297582203915E-33,9.9579925010296E-17,-1.));
#111152=DIRECTION('center_axis',(-6.9388939039071E-18,-1.,-9.95799250102971E-17));
#111153=DIRECTION('ref_axis',(0.0625000000000002,9.93852426637541E-17,-0.998044963916957));
#111154=DIRECTION('center_axis',(-8.40594773455218E-47,1.,9.9579925010296E-17));
#111155=DIRECTION('ref_axis',(-0.811844140885989,-5.81421498601493E-17,
0.583874208121142));
#111156=DIRECTION('center_axis',(8.40594773455218E-47,-1.,-9.9579925010296E-17));
#111157=DIRECTION('ref_axis',(1.,8.46731860157208E-47,-6.16297582203915E-33));
#111158=DIRECTION('center_axis',(-8.40594773455218E-47,1.,9.9579925010296E-17));
#111159=DIRECTION('ref_axis',(-0.85146931829632,5.22201532254593E-17,-0.524404424085075));
#111160=DIRECTION('center_axis',(8.40594773455218E-47,-1.,-9.9579925010296E-17));
#111161=DIRECTION('ref_axis',(0.12,-9.88603496856012E-17,0.992773891679268));
#111162=DIRECTION('',(6.16297582203915E-33,-9.95799250102971E-17,1.));
#111163=DIRECTION('center_axis',(-6.9388939039071E-18,-1.,-9.95799250102971E-17));
#111164=DIRECTION('ref_axis',(0.999999893270433,-6.98490071851115E-18,0.000462016367098532));
#111165=DIRECTION('center_axis',(-8.40594773455218E-47,1.,9.9579925010296E-17));
#111166=DIRECTION('ref_axis',(-1.,-8.46731860157208E-47,6.16297582203915E-33));
#111167=DIRECTION('center_axis',(-6.9388939039071E-18,-1.,-9.95799250102971E-17));
#111168=DIRECTION('ref_axis',(0.999999893270433,-6.98490071851115E-18,0.000462016367098532));
#111169=DIRECTION('center_axis',(-0.707106781186548,-5.98729840163861E-47,
-0.707106781186547));
#111170=DIRECTION('ref_axis',(-0.707106781186547,0.,0.707106781186548));
#111171=DIRECTION('',(8.46731860157208E-47,-1.,-1.55587128320416E-65));
#111172=DIRECTION('',(-8.46731860157208E-47,1.,1.55587128320416E-65));
#111173=DIRECTION('center_axis',(-1.,-8.46731860157208E-47,6.16297582203915E-33));
#111174=DIRECTION('ref_axis',(-6.16297582203915E-33,9.9579925010296E-17,
-1.));
#111175=DIRECTION('',(-8.40594773455218E-47,1.,9.9579925010296E-17));
#111176=DIRECTION('',(6.16297582203915E-33,-9.9579925010296E-17,1.));
#111177=DIRECTION('',(-8.40594773455218E-47,1.,9.9579925010296E-17));
#111178=DIRECTION('center_axis',(1.,8.46731860157208E-47,-6.16297582203915E-33));
#111179=DIRECTION('ref_axis',(-8.40594773455218E-47,1.,9.9579925010296E-17));
#111180=DIRECTION('',(-6.16297582203915E-33,9.9579925010296E-17,-1.));
#111181=DIRECTION('center_axis',(1.,8.46731860157208E-47,-6.16297582203915E-33));
#111182=DIRECTION('ref_axis',(8.40594773455218E-47,-1.,-9.9579925010296E-17));
#111183=DIRECTION('',(6.16297582203915E-33,-9.9579925010296E-17,1.));
#111184=DIRECTION('center_axis',(1.,8.46731860157208E-47,-6.16297582203915E-33));
#111185=DIRECTION('ref_axis',(-8.40594773455218E-47,1.,9.9579925010296E-17));
#111186=DIRECTION('',(-8.40594773455218E-47,1.,9.9579925010296E-17));
#111187=DIRECTION('',(-8.40594773455218E-47,1.,9.9579925010296E-17));
#111188=DIRECTION('center_axis',(1.,8.46731860157208E-47,-6.16297582203915E-33));
#111189=DIRECTION('ref_axis',(6.16297582203915E-33,-9.9579925010296E-17,
1.));
#111190=DIRECTION('',(-8.46731860157208E-47,1.,0.));
#111191=DIRECTION('',(-8.13081314298998E-47,1.,5.46011323586143E-16));
#111192=DIRECTION('',(-8.40594773455218E-47,1.,9.9579925010296E-17));
#111193=DIRECTION('',(-6.16297582203915E-33,9.9579925010296E-17,-1.));
#111194=DIRECTION('',(-8.13081314298998E-47,1.,5.46011323586143E-16));
#111195=DIRECTION('center_axis',(1.,8.46731860157208E-47,-6.16297582203915E-33));
#111196=DIRECTION('ref_axis',(-8.40594773455218E-47,1.,9.9579925010296E-17));
#111197=DIRECTION('',(6.16297582203915E-33,-9.9579925010296E-17,1.));
#111198=DIRECTION('center_axis',(1.,8.46731860157208E-47,-6.16297582203915E-33));
#111199=DIRECTION('ref_axis',(8.40594773455218E-47,-1.,-9.9579925010296E-17));
#111200=DIRECTION('',(-6.16297582203915E-33,9.9579925010296E-17,-1.));
#111201=DIRECTION('center_axis',(-0.707106781186548,-3.86088309512404E-16,
0.707106781186547));
#111202=DIRECTION('ref_axis',(0.707106781186547,-4.12156156691976E-16,0.707106781186548));
#111203=DIRECTION('',(1.26831058763807E-43,1.,5.46011323586143E-16));
#111204=DIRECTION('center_axis',(1.83750175990223E-19,0.,1.));
#111205=DIRECTION('ref_axis',(-1.,1.15873958031682E-16,1.83750175990223E-19));
#111206=DIRECTION('center_axis',(8.40594773455218E-47,-1.,-9.9579925010296E-17));
#111207=DIRECTION('ref_axis',(0.0625000000000002,9.93852426637541E-17,-0.998044963916957));
#111208=DIRECTION('',(-8.40594773455218E-47,1.,9.9579925010296E-17));
#111209=DIRECTION('center_axis',(0.,-1.,0.));
#111210=DIRECTION('ref_axis',(0.999999893270433,0.,0.000462016367098532));
#111211=DIRECTION('',(0.,1.,0.));
#111212=DIRECTION('center_axis',(-1.,-8.46731860157208E-47,6.16297582203915E-33));
#111213=DIRECTION('ref_axis',(-6.16297582203915E-33,9.9579925010296E-17,
-1.));
#111214=DIRECTION('',(8.40594773455218E-47,-1.,-9.9579925010296E-17));
#111215=DIRECTION('',(8.40594773455218E-47,-1.,-9.9579925010296E-17));
#111216=DIRECTION('center_axis',(8.40594773455218E-47,-1.,-9.9579925010296E-17));
#111217=DIRECTION('ref_axis',(-1.,-8.46731860157208E-47,6.16297582203915E-33));
#111218=DIRECTION('',(0.,-1.,0.));
#111219=DIRECTION('center_axis',(-0.707106781186548,-3.86088309512404E-16,
0.707106781186547));
#111220=DIRECTION('ref_axis',(0.707106781186547,-4.12156156691976E-16,0.707106781186548));
#111221=DIRECTION('',(0.707106781186547,-7.04136402448282E-17,0.707106781186548));
#111222=DIRECTION('',(1.26831058763807E-43,1.,5.46011323586143E-16));
#111223=DIRECTION('center_axis',(-1.,-1.02762453955456E-27,1.88205719398865E-12));
#111224=DIRECTION('ref_axis',(1.88205719398865E-12,-5.82876826609362E-16,
1.));
#111225=DIRECTION('',(-1.55426471955831E-12,-9.9579925010296E-17,1.));
#111226=DIRECTION('center_axis',(-1.,-1.02762453955456E-27,1.88205719398865E-12));
#111227=DIRECTION('ref_axis',(1.88205719398865E-12,-5.82876826609362E-16,
1.));
#111228=DIRECTION('center_axis',(1.,8.46731860157208E-47,-6.16297582203915E-33));
#111229=DIRECTION('ref_axis',(6.16297582203915E-33,-9.9579925010296E-17,
1.));
#111230=DIRECTION('',(-6.16297582203915E-33,9.9579925010296E-17,-1.));
#111231=DIRECTION('',(-6.16297582203915E-33,9.9579925010296E-17,-1.));
#111232=DIRECTION('',(-6.16297582203915E-33,9.9579925010296E-17,-1.));
#111233=DIRECTION('',(8.40594773455218E-47,-1.,-9.9579925010296E-17));
#111234=DIRECTION('',(6.16297582203915E-33,-9.9579925010296E-17,1.));
#111235=DIRECTION('center_axis',(8.40594773455218E-47,-1.,-9.9579925010296E-17));
#111236=DIRECTION('ref_axis',(-1.,-8.46731860157208E-47,6.16297582203915E-33));
#111237=DIRECTION('center_axis',(8.40594773455218E-47,-1.,-9.9579925010296E-17));
#111238=DIRECTION('ref_axis',(-0.923879532511287,-3.81075874975982E-17,
0.382683432365088));
#111239=DIRECTION('center_axis',(-8.40594773455218E-47,1.,9.9579925010296E-17));
#111240=DIRECTION('ref_axis',(-0.923879532511287,-3.81075874975982E-17,
0.382683432365088));
#111241=DIRECTION('',(-8.40594773455218E-47,1.,9.9579925010296E-17));
#111242=DIRECTION('',(8.40594773455218E-47,-1.,-9.9579925010296E-17));
#111243=DIRECTION('center_axis',(-0.707106781186549,-7.04136402448281E-17,
0.707106781186547));
#111244=DIRECTION('ref_axis',(8.40594773455218E-47,-1.,-9.9579925010296E-17));
#111245=DIRECTION('',(0.707106781186546,-7.04136402448283E-17,0.707106781186548));
#111246=DIRECTION('',(8.40594773455218E-47,-1.,-9.9579925010296E-17));
#111247=DIRECTION('center_axis',(-8.40594773455218E-47,1.,9.9579925010296E-17));
#111248=DIRECTION('ref_axis',(-1.,-8.46731860157208E-47,6.16297582203915E-33));
#111249=DIRECTION('',(-1.,-8.46731860157208E-47,6.16297582203915E-33));
#111250=DIRECTION('center_axis',(-8.40594773455218E-47,1.,9.9579925010296E-17));
#111251=DIRECTION('ref_axis',(-0.38268343236509,-9.19998545660213E-17,0.923879532511287));
#111252=DIRECTION('',(8.88178419700125E-16,9.9579925010296E-17,-1.));
#111253=DIRECTION('',(-0.707106781186551,7.04136402448278E-17,-0.707106781186544));
#111254=DIRECTION('center_axis',(8.40594773455218E-47,-1.,-9.9579925010296E-17));
#111255=DIRECTION('ref_axis',(0.0625000000000002,9.93852426637541E-17,-0.998044963916957));
#111256=DIRECTION('center_axis',(8.40594773455218E-47,-1.,-9.9579925010296E-17));
#111257=DIRECTION('ref_axis',(1.,8.46731860157208E-47,-6.16297582203915E-33));
#111258=DIRECTION('center_axis',(8.40594773455218E-47,-1.,-9.9579925010296E-17));
#111259=DIRECTION('ref_axis',(0.12,-9.88603496856012E-17,0.992773891679268));
#111260=DIRECTION('',(6.16297582203915E-33,-9.9579925010296E-17,1.));
#111261=DIRECTION('center_axis',(-8.40594773455218E-47,1.,9.9579925010296E-17));
#111262=DIRECTION('ref_axis',(-1.,-8.46731860157208E-47,6.16297582203915E-33));
#111263=DIRECTION('center_axis',(-8.40594773455218E-47,1.,9.9579925010296E-17));
#111264=DIRECTION('ref_axis',(-0.38268343236509,-9.19998545660213E-17,0.923879532511287));
#111265=DIRECTION('',(-8.40594773455218E-47,1.,9.9579925010296E-17));
#111266=DIRECTION('center_axis',(1.,-8.84447404295016E-32,8.88178419700125E-16));
#111267=DIRECTION('ref_axis',(8.88178419700125E-16,9.9579925010296E-17,
-1.));
#111268=DIRECTION('',(-8.40594773455218E-47,1.,9.9579925010296E-17));
#111269=DIRECTION('center_axis',(0.707106781186544,7.04136402448285E-17,
-0.707106781186551));
#111270=DIRECTION('ref_axis',(-0.707106781186551,7.04136402448278E-17,-0.707106781186544));
#111271=DIRECTION('center_axis',(-0.707106781186544,-7.04136402448285E-17,
0.707106781186551));
#111272=DIRECTION('ref_axis',(-0.707106781186551,7.04136402448278E-17,-0.707106781186544));
#111273=DIRECTION('center_axis',(-1.,-8.46731860157208E-47,6.16297582203915E-33));
#111274=DIRECTION('ref_axis',(-8.40594773455218E-47,1.,9.9579925010296E-17));
#111275=DIRECTION('',(-1.,-8.46731860157208E-47,6.16297582203915E-33));
#111276=DIRECTION('center_axis',(1.,8.46731860157208E-47,-6.16297582203915E-33));
#111277=DIRECTION('ref_axis',(-8.40594773455218E-47,1.,9.9579925010296E-17));
#111278=DIRECTION('',(-1.,-8.46731860157208E-47,6.16297582203915E-33));
#111279=DIRECTION('center_axis',(1.,8.46731860157208E-47,-6.16297582203915E-33));
#111280=DIRECTION('ref_axis',(-8.40594773455218E-47,1.,9.9579925010296E-17));
#111281=DIRECTION('',(0.707106781186548,0.707106781186548,7.04136402448282E-17));
#111282=DIRECTION('',(-0.707106781186548,0.707106781186548,7.04136402448282E-17));
#111283=DIRECTION('center_axis',(-1.,-8.46731860157208E-47,6.16297582203915E-33));
#111284=DIRECTION('ref_axis',(-8.40594773455218E-47,1.,9.9579925010296E-17));
#111285=DIRECTION('center_axis',(0.707106781186548,-0.707106781186548,-7.04136402448282E-17));
#111286=DIRECTION('ref_axis',(0.707106781186548,0.707106781186548,7.04136402448282E-17));
#111287=DIRECTION('',(0.707106781186548,0.707106781186548,7.04136402448282E-17));
#111288=DIRECTION('',(-6.16297582203915E-33,9.9579925010296E-17,-1.));
#111289=DIRECTION('center_axis',(1.,8.46731860157208E-47,-6.16297582203915E-33));
#111290=DIRECTION('ref_axis',(8.40594773455218E-47,-1.,-9.9579925010296E-17));
#111291=DIRECTION('',(0.707106781186548,-0.707106781186548,-7.04136402448282E-17));
#111292=DIRECTION('center_axis',(-1.,-8.46731860157208E-47,6.16297582203915E-33));
#111293=DIRECTION('ref_axis',(8.40594773455218E-47,-1.,-9.9579925010296E-17));
#111294=DIRECTION('center_axis',(0.707106781186544,0.707106781186551,7.04136402448286E-17));
#111295=DIRECTION('ref_axis',(-0.707106781186551,0.707106781186544,7.04136402448278E-17));
#111296=DIRECTION('',(6.16297582203915E-33,-9.9579925010296E-17,1.));
#111297=DIRECTION('center_axis',(-8.40594773455218E-47,1.,9.9579925010296E-17));
#111298=DIRECTION('ref_axis',(-6.16297582203915E-33,9.9579925010296E-17,
-1.));
#111299=DIRECTION('',(-1.,-8.46731860157208E-47,6.16297582203915E-33));
#111300=DIRECTION('',(-6.16297582203915E-33,9.9579925010296E-17,-1.));
#111301=DIRECTION('',(-1.,-8.46731860157208E-47,6.16297582203915E-33));
#111302=DIRECTION('center_axis',(-1.,-8.46731860157208E-47,6.16297582203915E-33));
#111303=DIRECTION('ref_axis',(-8.40594773455218E-47,1.,9.9579925010296E-17));
#111304=DIRECTION('',(-1.,-8.46731860157208E-47,6.16297582203915E-33));
#111305=DIRECTION('center_axis',(-1.,-8.46731860157208E-47,6.16297582203915E-33));
#111306=DIRECTION('ref_axis',(-8.40594773455218E-47,1.,9.9579925010296E-17));
#111307=DIRECTION('center_axis',(8.40594773455218E-47,-1.,-9.9579925010296E-17));
#111308=DIRECTION('ref_axis',(6.16297582203915E-33,-9.9579925010296E-17,
1.));
#111309=DIRECTION('',(-1.,-8.46731860157208E-47,6.16297582203915E-33));
#111310=DIRECTION('',(6.16297582203915E-33,-9.9579925010296E-17,1.));
#111311=DIRECTION('center_axis',(-1.,-8.46731860157208E-47,6.16297582203915E-33));
#111312=DIRECTION('ref_axis',(8.40594773455218E-47,-1.,-9.9579925010296E-17));
#111313=DIRECTION('center_axis',(-1.,-8.46731860157208E-47,6.16297582203915E-33));
#111314=DIRECTION('ref_axis',(8.40594773455218E-47,-1.,-9.9579925010296E-17));
#111315=DIRECTION('center_axis',(1.,8.46731860157208E-47,-6.16297582203915E-33));
#111316=DIRECTION('ref_axis',(6.16297582203915E-33,-9.9579925010296E-17,
1.));
#111317=DIRECTION('',(6.16297582203915E-33,-9.9579925010296E-17,1.));
#111318=DIRECTION('center_axis',(1.,8.46731860157208E-47,-6.16297582203915E-33));
#111319=DIRECTION('ref_axis',(8.40594773455218E-47,-1.,-9.9579925010296E-17));
#111320=DIRECTION('',(-6.16297582203915E-33,9.9579925010296E-17,-1.));
#111321=DIRECTION('center_axis',(-8.40594773455218E-47,1.,9.9579925010296E-17));
#111322=DIRECTION('ref_axis',(-6.16297582203915E-33,9.9579925010296E-17,
-1.));
#111323=DIRECTION('',(-1.,-8.46731860157208E-47,6.16297582203915E-33));
#111324=DIRECTION('center_axis',(8.40594773455218E-47,-1.,-9.9579925010296E-17));
#111325=DIRECTION('ref_axis',(6.16297582203915E-33,-9.9579925010296E-17,
1.));
#111326=DIRECTION('',(-1.,-8.46731860157208E-47,6.16297582203915E-33));
#111327=DIRECTION('center_axis',(-1.,-8.46731860157208E-47,6.16297582203915E-33));
#111328=DIRECTION('ref_axis',(8.40594773455218E-47,-1.,-9.9579925010296E-17));
#111329=DIRECTION('center_axis',(8.40594773455218E-47,-1.,-9.9579925010296E-17));
#111330=DIRECTION('ref_axis',(1.,8.46731860157208E-47,-6.16297582203915E-33));
#111331=DIRECTION('center_axis',(-8.40594773455218E-47,1.,9.9579925010296E-17));
#111332=DIRECTION('ref_axis',(1.,8.46731860157208E-47,-6.16297582203915E-33));
#111333=DIRECTION('center_axis',(-8.40594773455218E-47,1.,9.9579925010296E-17));
#111334=DIRECTION('ref_axis',(1.,8.46731860157208E-47,-6.16297582203915E-33));
#111335=DIRECTION('center_axis',(8.40594773455218E-47,-1.,-9.9579925010296E-17));
#111336=DIRECTION('ref_axis',(1.,8.46731860157208E-47,-6.16297582203915E-33));
#111337=DIRECTION('center_axis',(-8.40594773455218E-47,1.,9.9579925010296E-17));
#111338=DIRECTION('ref_axis',(-1.,-8.46731860157208E-47,6.16297582203915E-33));
#111339=DIRECTION('',(6.16297582203915E-33,-9.9579925010296E-17,1.));
#111340=DIRECTION('center_axis',(-8.40594773455218E-47,1.,9.9579925010296E-17));
#111341=DIRECTION('ref_axis',(-1.,-1.56620894510576E-31,1.5728159515523E-15));
#111342=DIRECTION('center_axis',(-8.40594773455218E-47,1.,9.9579925010296E-17));
#111343=DIRECTION('ref_axis',(-0.449999999999999,8.89277165364225E-17,-0.893028554974588));
#111344=DIRECTION('center_axis',(8.40594773455218E-47,-1.,-9.9579925010296E-17));
#111345=DIRECTION('ref_axis',(1.,8.46731860157207E-47,-6.16297582203915E-33));
#111346=DIRECTION('center_axis',(8.40594773455218E-47,-1.,-9.9579925010296E-17));
#111347=DIRECTION('ref_axis',(1.,8.46731860157208E-47,-6.16297582203915E-33));
#111348=DIRECTION('center_axis',(8.40594773455218E-47,-1.,-9.9579925010296E-17));
#111349=DIRECTION('ref_axis',(-1.,-1.56620894510576E-31,1.5728159515523E-15));
#111350=DIRECTION('',(-6.16297582203915E-33,9.9579925010296E-17,-1.));
#111351=DIRECTION('center_axis',(8.40594773455218E-47,-1.,-9.9579925010296E-17));
#111352=DIRECTION('ref_axis',(-0.449999999999999,8.89277165364225E-17,-0.893028554974588));
#111353=DIRECTION('center_axis',(-8.40594773455218E-47,1.,9.9579925010296E-17));
#111354=DIRECTION('ref_axis',(1.,8.46731860157207E-47,-6.16297582203915E-33));
#111355=DIRECTION('center_axis',(8.40594773455218E-47,-1.,-9.9579925010296E-17));
#111356=DIRECTION('ref_axis',(1.,8.46731860157208E-47,-6.16297582203915E-33));
#111357=DIRECTION('center_axis',(-8.40594773455218E-47,1.,9.9579925010296E-17));
#111358=DIRECTION('ref_axis',(1.,8.46731860157208E-47,-6.16297582203915E-33));
#111359=DIRECTION('center_axis',(-8.40594773455218E-47,1.,9.9579925010296E-17));
#111360=DIRECTION('ref_axis',(1.,8.46731860157208E-47,-6.16297582203915E-33));
#111361=DIRECTION('center_axis',(8.40594773455218E-47,-1.,-9.9579925010296E-17));
#111362=DIRECTION('ref_axis',(1.,8.46731860157208E-47,-6.16297582203915E-33));
#111363=DIRECTION('center_axis',(8.40594773455218E-47,-1.,-9.9579925010296E-17));
#111364=DIRECTION('ref_axis',(1.,8.46731860157208E-47,-6.16297582203915E-33));
#111365=DIRECTION('',(-6.16297582203915E-33,9.9579925010296E-17,-1.));
#111366=DIRECTION('center_axis',(8.40594773455218E-47,-1.,-9.9579925010296E-17));
#111367=DIRECTION('ref_axis',(-0.449999999999999,8.89277165364225E-17,-0.893028554974588));
#111368=DIRECTION('center_axis',(8.40594773455218E-47,-1.,-9.9579925010296E-17));
#111369=DIRECTION('ref_axis',(-1.,-1.56620894510576E-31,1.5728159515523E-15));
#111370=DIRECTION('center_axis',(-8.40594773455218E-47,1.,9.9579925010296E-17));
#111371=DIRECTION('ref_axis',(1.,8.46731860157207E-47,-6.16297582203915E-33));
#111372=DIRECTION('center_axis',(-8.40594773455218E-47,1.,9.9579925010296E-17));
#111373=DIRECTION('ref_axis',(1.,8.46731860157208E-47,-6.16297582203915E-33));
#111374=DIRECTION('center_axis',(-8.40594773455218E-47,1.,9.9579925010296E-17));
#111375=DIRECTION('ref_axis',(-1.,-1.56620894510576E-31,1.5728159515523E-15));
#111376=DIRECTION('center_axis',(-8.40594773455218E-47,1.,9.9579925010296E-17));
#111377=DIRECTION('ref_axis',(-0.449999999999999,8.89277165364225E-17,-0.893028554974588));
#111378=DIRECTION('',(6.16297582203915E-33,-9.9579925010296E-17,1.));
#111379=DIRECTION('center_axis',(8.40594773455218E-47,-1.,-9.9579925010296E-17));
#111380=DIRECTION('ref_axis',(1.,8.46731860157207E-47,-6.16297582203915E-33));
#111381=DIRECTION('center_axis',(8.40594773455218E-47,-1.,-9.9579925010296E-17));
#111382=DIRECTION('ref_axis',(0.0625000000000002,9.93852426637541E-17,-0.998044963916957));
#111383=DIRECTION('',(8.40594773455218E-47,-1.,-9.9579925010296E-17));
#111384=DIRECTION('center_axis',(8.40594773455218E-47,-1.,-9.9579925010296E-17));
#111385=DIRECTION('ref_axis',(-0.85146931829632,5.22201532254593E-17,-0.524404424085075));
#111386=DIRECTION('',(-8.40594773455218E-47,1.,9.9579925010296E-17));
#111387=DIRECTION('',(8.40594773455218E-47,-1.,-9.9579925010296E-17));
#111388=DIRECTION('center_axis',(-1.,-8.46731860157208E-47,6.16297582203915E-33));
#111389=DIRECTION('ref_axis',(-6.16297582203915E-33,9.9579925010296E-17,
-1.));
#111390=DIRECTION('',(8.40594773455218E-47,-1.,-9.9579925010296E-17));
#111391=DIRECTION('center_axis',(8.40594773455218E-47,-1.,-9.9579925010296E-17));
#111392=DIRECTION('ref_axis',(-0.811844140885989,-5.81421498601493E-17,
0.583874208121142));
#111393=DIRECTION('center_axis',(8.40594773455218E-47,-1.,-9.9579925010296E-17));
#111394=DIRECTION('ref_axis',(1.,8.46731860157208E-47,-6.16297582203915E-33));
#111395=DIRECTION('center_axis',(8.40594773455218E-47,-1.,-9.9579925010296E-17));
#111396=DIRECTION('ref_axis',(-1.,-8.46731860157208E-47,6.16297582203915E-33));
#111397=DIRECTION('center_axis',(-8.40594773455218E-47,1.,9.9579925010296E-17));
#111398=DIRECTION('ref_axis',(-1.,-8.46731860157207E-47,6.16297582203915E-33));
#111399=DIRECTION('center_axis',(-8.40594773455218E-47,1.,9.9579925010296E-17));
#111400=DIRECTION('ref_axis',(-1.,-8.46731860157208E-47,6.16297582203915E-33));
#111401=DIRECTION('center_axis',(-8.40594773455218E-47,1.,9.9579925010296E-17));
#111402=DIRECTION('ref_axis',(-1.,-8.46731860157208E-47,6.16297582203915E-33));
#111403=DIRECTION('',(-0.898876371703422,4.36361536127186E-17,-0.438202314454514));
#111404=DIRECTION('center_axis',(-8.40594773455218E-47,1.,9.9579925010296E-17));
#111405=DIRECTION('ref_axis',(-1.,-8.46731860157208E-47,6.16297582203915E-33));
#111406=DIRECTION('center_axis',(-8.40594773455218E-47,1.,9.9579925010296E-17));
#111407=DIRECTION('ref_axis',(-1.,-8.46731860157208E-47,6.16297582203915E-33));
#111408=DIRECTION('center_axis',(8.40594773455218E-47,-1.,-9.9579925010296E-17));
#111409=DIRECTION('ref_axis',(-1.,-8.46731860157207E-47,6.16297582203915E-33));
#111410=DIRECTION('center_axis',(8.40594773455218E-47,-1.,-9.9579925010296E-17));
#111411=DIRECTION('ref_axis',(-1.,-8.46731860157208E-47,6.16297582203915E-33));
#111412=DIRECTION('center_axis',(8.40594773455218E-47,-1.,-9.9579925010296E-17));
#111413=DIRECTION('ref_axis',(-1.,-8.46731860157208E-47,6.16297582203915E-33));
#111414=DIRECTION('',(-0.898876371703422,4.36361536127186E-17,-0.438202314454514));
#111415=DIRECTION('center_axis',(-1.,-8.46731860157208E-47,6.16297582203915E-33));
#111416=DIRECTION('ref_axis',(-6.16297582203915E-33,9.9579925010296E-17,
-1.));
#111417=DIRECTION('',(8.40594773455218E-47,-1.,-9.9579925010296E-17));
#111418=DIRECTION('',(8.40594773455218E-47,-1.,-9.9579925010296E-17));
#111419=DIRECTION('center_axis',(-1.,-8.46731860157208E-47,6.16297582203915E-33));
#111420=DIRECTION('ref_axis',(-6.16297582203915E-33,9.9579925010296E-17,
-1.));
#111421=DIRECTION('',(-8.40594773455218E-47,1.,9.9579925010296E-17));
#111422=DIRECTION('',(8.40594773455218E-47,-1.,-9.9579925010296E-17));
#111423=DIRECTION('center_axis',(-8.40594773455218E-47,1.,9.9579925010296E-17));
#111424=DIRECTION('ref_axis',(0.12,-9.88603496856012E-17,0.992773891679268));
#111425=DIRECTION('center_axis',(-8.40594773455218E-47,1.,9.9579925010296E-17));
#111426=DIRECTION('ref_axis',(0.12,-9.88603496856012E-17,0.992773891679268));
#111427=DIRECTION('',(8.40594773455218E-47,-1.,-9.9579925010296E-17));
#111428=DIRECTION('center_axis',(8.40594773455218E-47,-1.,-9.9579925010296E-17));
#111429=DIRECTION('ref_axis',(-0.85146931829632,5.22201532254593E-17,-0.524404424085075));
#111430=DIRECTION('center_axis',(8.40594773455218E-47,-1.,-9.9579925010296E-17));
#111431=DIRECTION('ref_axis',(-1.,-8.46731860157207E-47,6.16297582203915E-33));
#111432=DIRECTION('',(-8.40594773455218E-47,1.,9.9579925010296E-17));
#111433=DIRECTION('center_axis',(8.40594773455218E-47,-1.,-9.9579925010296E-17));
#111434=DIRECTION('ref_axis',(-0.811844140885989,-5.81421498601493E-17,
0.583874208121142));
#111435=DIRECTION('center_axis',(6.16297582203915E-33,-9.9579925010296E-17,
1.));
#111436=DIRECTION('ref_axis',(-1.,-8.46731860157208E-47,6.16297582203915E-33));
#111437=DIRECTION('center_axis',(0.438202314454514,8.95100416877536E-17,
-0.898876371703421));
#111438=DIRECTION('ref_axis',(0.898876371703422,-4.36361536127186E-17,0.438202314454514));
#111439=DIRECTION('',(8.40594773455218E-47,-1.,-9.9579925010296E-17));
#111440=DIRECTION('center_axis',(8.40594773455218E-47,-1.,-9.9579925010296E-17));
#111441=DIRECTION('ref_axis',(-1.,-8.46731860157207E-47,6.16297582203915E-33));
#111442=DIRECTION('',(-8.40594773455218E-47,1.,9.9579925010296E-17));
#111443=DIRECTION('center_axis',(8.40594773455218E-47,-1.,-9.9579925010296E-17));
#111444=DIRECTION('ref_axis',(-1.,-8.46731860157207E-47,6.16297582203915E-33));
#111445=DIRECTION('',(-8.40594773455218E-47,1.,9.9579925010296E-17));
#111446=DIRECTION('center_axis',(8.40594773455218E-47,-1.,-9.9579925010296E-17));
#111447=DIRECTION('ref_axis',(-1.,-8.46731860157208E-47,6.16297582203915E-33));
#111448=DIRECTION('',(-8.40594773455218E-47,1.,9.9579925010296E-17));
#111449=DIRECTION('',(-8.40594773455218E-47,1.,9.9579925010296E-17));
#111450=DIRECTION('axis',(0.,0.,1.));
#111451=DIRECTION('refdir',(1.,0.,0.));
#111452=DIRECTION('center_axis',(-1.17238944502697E-33,1.22459810574157E-16,
1.));
#111453=DIRECTION('ref_axis',(-1.,-1.07747590158145E-32,8.53125817097821E-20));
#111454=DIRECTION('center_axis',(1.83750175990301E-19,1.22464679914735E-16,
1.));
#111455=DIRECTION('ref_axis',(-1.,-1.07627038873394E-32,1.83750175990301E-19));
#111456=DIRECTION('',(0.707106781186548,-3.4431437427623E-21,0.707106781186548));
#111457=DIRECTION('center_axis',(-1.83750175990301E-19,-1.22464679914735E-16,
-1.));
#111458=DIRECTION('ref_axis',(-1.,-1.07852067938263E-32,-1.17238944502697E-33));
#111459=DIRECTION('center_axis',(1.17238944502697E-33,-1.22459810574157E-16,
-1.));
#111460=DIRECTION('ref_axis',(-1.,-1.07852067938263E-32,-1.17238944502697E-33));
#111461=DIRECTION('',(-1.17238944502697E-33,1.22459810574157E-16,1.));
#111462=DIRECTION('center_axis',(1.83750175990301E-19,1.22464679914735E-16,
1.));
#111463=DIRECTION('ref_axis',(-1.,-1.07852067938263E-32,-1.17238944502697E-33));
#111464=DIRECTION('center_axis',(1.83750175990301E-19,1.22464679914735E-16,
1.));
#111465=DIRECTION('ref_axis',(-1.,-1.07627047820816E-32,1.83750175990301E-19));
#111466=DIRECTION('center_axis',(1.17238944502697E-33,-1.22459810574157E-16,
-1.));
#111467=DIRECTION('ref_axis',(-1.,-1.07747590158145E-32,8.53125817097821E-20));
#111468=DIRECTION('center_axis',(-1.83750175990301E-19,-1.22464679914735E-16,
-1.));
#111469=DIRECTION('ref_axis',(-1.,-1.07627038873394E-32,1.83750175990301E-19));
#111470=DIRECTION('',(0.707106781186548,3.4431437427623E-21,-0.707106781186548));
#111471=DIRECTION('center_axis',(1.83750175990301E-19,1.22464679914735E-16,
1.));
#111472=DIRECTION('ref_axis',(-1.,-1.07627047820816E-32,1.83750175990301E-19));
#111473=DIRECTION('axis',(0.,0.,1.));
#111474=DIRECTION('refdir',(1.,0.,0.));
#111475=DIRECTION('center_axis',(-3.56297039712382E-33,-1.,4.0245584642662E-16));
#111476=DIRECTION('ref_axis',(1.,-5.96129604355379E-16,3.46944695195422E-17));
#111477=DIRECTION('center_axis',(-5.55111512312578E-16,-1.,4.02455846426619E-16));
#111478=DIRECTION('ref_axis',(1.,-5.55111512312577E-16,3.46944695195422E-17));
#111479=DIRECTION('',(-0.707106781186552,-0.707106781186543,3.46642169093045E-16));
#111480=DIRECTION('center_axis',(5.55111512312578E-16,1.,-4.02455846426619E-16));
#111481=DIRECTION('ref_axis',(1.,-6.34413156928661E-16,3.46944695195423E-17));
#111482=DIRECTION('center_axis',(-6.34413156928661E-16,-1.,4.0245584642662E-16));
#111483=DIRECTION('ref_axis',(1.,-6.34413156928661E-16,3.46944695195423E-17));
#111484=DIRECTION('center_axis',(-5.55111512312578E-16,-1.,4.02455846426619E-16));
#111485=DIRECTION('ref_axis',(1.,-6.34413156928661E-16,3.46944695195423E-17));
#111486=DIRECTION('',(6.34413156928661E-16,1.,-4.0245584642662E-16));
#111487=DIRECTION('center_axis',(-5.55111512312578E-16,-1.,4.02455846426619E-16));
#111488=DIRECTION('ref_axis',(1.,-5.55111512312578E-16,3.46944695195422E-17));
#111489=DIRECTION('center_axis',(3.56297039712382E-33,1.,-4.0245584642662E-16));
#111490=DIRECTION('ref_axis',(1.,-5.96129604355379E-16,3.46944695195422E-17));
#111491=DIRECTION('center_axis',(5.55111512312578E-16,1.,-4.02455846426619E-16));
#111492=DIRECTION('ref_axis',(1.,-5.55111512312578E-16,3.46944695195422E-17));
#111493=DIRECTION('',(-0.707106781186547,0.707106781186548,-3.95707558426922E-16));
#111494=DIRECTION('center_axis',(-5.55111512312578E-16,-1.,4.02455846426619E-16));
#111495=DIRECTION('ref_axis',(1.,-5.55111512312578E-16,3.46944695195422E-17));
#111496=DIRECTION('axis',(0.,0.,1.));
#111497=DIRECTION('refdir',(1.,0.,0.));
#111498=DIRECTION('center_axis',(-3.85185988875507E-34,1.,0.));
#111499=DIRECTION('ref_axis',(1.,0.,0.));
#111500=DIRECTION('center_axis',(-3.85185988875507E-34,1.,0.));
#111501=DIRECTION('ref_axis',(0.,0.,1.));
#111502=DIRECTION('center_axis',(-3.85185988875507E-34,1.,0.));
#111503=DIRECTION('ref_axis',(0.,0.,1.));
#111504=DIRECTION('center_axis',(-3.85185988875507E-34,1.,0.));
#111505=DIRECTION('ref_axis',(1.,0.,0.));
#111506=DIRECTION('center_axis',(-3.85185988875507E-34,1.,0.));
#111507=DIRECTION('ref_axis',(0.,0.,1.));
#111508=DIRECTION('center_axis',(-3.85185988875507E-34,1.,0.));
#111509=DIRECTION('ref_axis',(0.,0.,1.));
#111510=DIRECTION('center_axis',(-3.85185988875507E-34,1.,0.));
#111511=DIRECTION('ref_axis',(1.,0.,0.));
#111512=DIRECTION('center_axis',(-3.85185988875507E-34,1.,0.));
#111513=DIRECTION('ref_axis',(0.,0.,1.));
#111514=DIRECTION('center_axis',(-3.85185988875507E-34,1.,0.));
#111515=DIRECTION('ref_axis',(0.,0.,1.));
#111516=DIRECTION('center_axis',(-3.85185988875507E-34,1.,0.));
#111517=DIRECTION('ref_axis',(1.,0.,0.));
#111518=DIRECTION('center_axis',(-3.85185988875507E-34,1.,0.));
#111519=DIRECTION('ref_axis',(0.,0.,1.));
#111520=DIRECTION('center_axis',(-3.85185988875507E-34,1.,0.));
#111521=DIRECTION('ref_axis',(0.,0.,1.));
#111522=DIRECTION('center_axis',(-3.85185988875507E-34,1.,0.));
#111523=DIRECTION('ref_axis',(1.,0.,0.));
#111524=DIRECTION('center_axis',(-3.85185988875507E-34,1.,0.));
#111525=DIRECTION('ref_axis',(0.,0.,1.));
#111526=DIRECTION('center_axis',(-3.85185988875507E-34,1.,0.));
#111527=DIRECTION('ref_axis',(0.,0.,1.));
#111528=DIRECTION('center_axis',(-3.85185988875507E-34,1.,0.));
#111529=DIRECTION('ref_axis',(1.,0.,0.));
#111530=DIRECTION('center_axis',(-3.85185988875507E-34,1.,0.));
#111531=DIRECTION('ref_axis',(0.,0.,1.));
#111532=DIRECTION('center_axis',(-3.85185988875507E-34,1.,0.));
#111533=DIRECTION('ref_axis',(0.,0.,1.));
#111534=DIRECTION('center_axis',(-3.85185988875507E-34,1.,0.));
#111535=DIRECTION('ref_axis',(1.,0.,0.));
#111536=DIRECTION('center_axis',(-3.85185988875507E-34,1.,0.));
#111537=DIRECTION('ref_axis',(0.,0.,1.));
#111538=DIRECTION('center_axis',(-3.85185988875507E-34,1.,0.));
#111539=DIRECTION('ref_axis',(0.,0.,1.));
#111540=DIRECTION('center_axis',(-3.85185988875507E-34,1.,0.));
#111541=DIRECTION('ref_axis',(1.,0.,0.));
#111542=DIRECTION('center_axis',(-3.85185988875507E-34,1.,0.));
#111543=DIRECTION('ref_axis',(0.,0.,1.));
#111544=DIRECTION('center_axis',(-3.85185988875507E-34,1.,0.));
#111545=DIRECTION('ref_axis',(0.,0.,1.));
#111546=DIRECTION('center_axis',(-3.85185988875507E-34,1.,0.));
#111547=DIRECTION('ref_axis',(1.,0.,0.));
#111548=DIRECTION('center_axis',(-3.85185988875507E-34,1.,0.));
#111549=DIRECTION('ref_axis',(0.,0.,1.));
#111550=DIRECTION('center_axis',(-3.85185988875507E-34,1.,0.));
#111551=DIRECTION('ref_axis',(0.,0.,1.));
#111552=DIRECTION('center_axis',(-3.85185988875507E-34,1.,0.));
#111553=DIRECTION('ref_axis',(1.,0.,0.));
#111554=DIRECTION('center_axis',(-3.85185988875507E-34,1.,0.));
#111555=DIRECTION('ref_axis',(0.,0.,1.));
#111556=DIRECTION('center_axis',(-3.85185988875507E-34,1.,0.));
#111557=DIRECTION('ref_axis',(0.,0.,1.));
#111558=DIRECTION('center_axis',(-3.85185988875507E-34,1.,0.));
#111559=DIRECTION('ref_axis',(1.,0.,0.));
#111560=DIRECTION('center_axis',(-3.85185988875507E-34,1.,0.));
#111561=DIRECTION('ref_axis',(0.,0.,1.));
#111562=DIRECTION('center_axis',(-3.85185988875507E-34,1.,0.));
#111563=DIRECTION('ref_axis',(0.,0.,1.));
#111564=DIRECTION('center_axis',(-3.85185988875507E-34,1.,0.));
#111565=DIRECTION('ref_axis',(1.,0.,0.));
#111566=DIRECTION('center_axis',(-3.85185988875507E-34,1.,0.));
#111567=DIRECTION('ref_axis',(0.,0.,1.));
#111568=DIRECTION('center_axis',(-3.85185988875507E-34,1.,0.));
#111569=DIRECTION('ref_axis',(0.,0.,1.));
#111570=DIRECTION('center_axis',(-3.85185988875507E-34,1.,0.));
#111571=DIRECTION('ref_axis',(1.,0.,0.));
#111572=DIRECTION('center_axis',(-3.85185988875507E-34,1.,0.));
#111573=DIRECTION('ref_axis',(0.,0.,1.));
#111574=DIRECTION('center_axis',(-3.85185988875507E-34,1.,0.));
#111575=DIRECTION('ref_axis',(0.,0.,1.));
#111576=DIRECTION('center_axis',(-3.85185988875507E-34,1.,0.));
#111577=DIRECTION('ref_axis',(1.,0.,0.));
#111578=DIRECTION('center_axis',(-3.85185988875507E-34,1.,0.));
#111579=DIRECTION('ref_axis',(0.,0.,1.));
#111580=DIRECTION('center_axis',(-3.85185988875507E-34,1.,0.));
#111581=DIRECTION('ref_axis',(0.,0.,1.));
#111582=DIRECTION('center_axis',(-3.85185988875507E-34,1.,0.));
#111583=DIRECTION('ref_axis',(1.,0.,0.));
#111584=DIRECTION('center_axis',(-3.85185988875507E-34,1.,0.));
#111585=DIRECTION('ref_axis',(0.,0.,1.));
#111586=DIRECTION('center_axis',(-3.85185988875507E-34,1.,0.));
#111587=DIRECTION('ref_axis',(0.,0.,1.));
#111588=DIRECTION('center_axis',(-3.85185988875507E-34,1.,0.));
#111589=DIRECTION('ref_axis',(1.,0.,0.));
#111590=DIRECTION('center_axis',(-3.85185988875507E-34,1.,0.));
#111591=DIRECTION('ref_axis',(0.,0.,1.));
#111592=DIRECTION('center_axis',(-3.85185988875507E-34,1.,0.));
#111593=DIRECTION('ref_axis',(0.,0.,1.));
#111594=DIRECTION('center_axis',(-3.85185988875507E-34,1.,0.));
#111595=DIRECTION('ref_axis',(1.,0.,0.));
#111596=DIRECTION('center_axis',(-3.85185988875507E-34,1.,0.));
#111597=DIRECTION('ref_axis',(0.,0.,1.));
#111598=DIRECTION('center_axis',(-3.85185988875507E-34,1.,0.));
#111599=DIRECTION('ref_axis',(0.,0.,1.));
#111600=DIRECTION('center_axis',(-3.85185988875507E-34,1.,0.));
#111601=DIRECTION('ref_axis',(1.,0.,0.));
#111602=DIRECTION('center_axis',(-3.85185988875507E-34,1.,0.));
#111603=DIRECTION('ref_axis',(0.,0.,1.));
#111604=DIRECTION('center_axis',(-3.85185988875507E-34,1.,0.));
#111605=DIRECTION('ref_axis',(0.,0.,1.));
#111606=DIRECTION('center_axis',(-3.85185988875507E-34,1.,0.));
#111607=DIRECTION('ref_axis',(1.,0.,0.));
#111608=DIRECTION('center_axis',(-3.85185988875507E-34,1.,0.));
#111609=DIRECTION('ref_axis',(0.,0.,1.));
#111610=DIRECTION('center_axis',(-3.85185988875507E-34,1.,0.));
#111611=DIRECTION('ref_axis',(0.,0.,1.));
#111612=DIRECTION('center_axis',(-3.85185988875507E-34,1.,0.));
#111613=DIRECTION('ref_axis',(1.,0.,0.));
#111614=DIRECTION('center_axis',(-3.85185988875507E-34,1.,0.));
#111615=DIRECTION('ref_axis',(0.,0.,1.));
#111616=DIRECTION('center_axis',(-3.85185988875507E-34,1.,0.));
#111617=DIRECTION('ref_axis',(0.,0.,1.));
#111618=DIRECTION('center_axis',(-3.85185988875507E-34,1.,0.));
#111619=DIRECTION('ref_axis',(1.,0.,0.));
#111620=DIRECTION('center_axis',(-3.85185988875507E-34,1.,0.));
#111621=DIRECTION('ref_axis',(0.,0.,1.));
#111622=DIRECTION('center_axis',(-3.85185988875507E-34,1.,0.));
#111623=DIRECTION('ref_axis',(0.,0.,1.));
#111624=DIRECTION('center_axis',(-3.85185988875507E-34,1.,0.));
#111625=DIRECTION('ref_axis',(1.,0.,0.));
#111626=DIRECTION('center_axis',(-3.85185988875507E-34,1.,0.));
#111627=DIRECTION('ref_axis',(0.,0.,1.));
#111628=DIRECTION('center_axis',(-3.85185988875507E-34,1.,0.));
#111629=DIRECTION('ref_axis',(0.,0.,1.));
#111630=DIRECTION('center_axis',(-3.85185988875507E-34,1.,0.));
#111631=DIRECTION('ref_axis',(1.,0.,0.));
#111632=DIRECTION('center_axis',(-3.85185988875507E-34,1.,0.));
#111633=DIRECTION('ref_axis',(0.,0.,1.));
#111634=DIRECTION('center_axis',(-3.85185988875507E-34,1.,0.));
#111635=DIRECTION('ref_axis',(0.,0.,1.));
#111636=DIRECTION('center_axis',(-3.85185988875507E-34,1.,0.));
#111637=DIRECTION('ref_axis',(1.,0.,0.));
#111638=DIRECTION('center_axis',(-3.85185988875507E-34,1.,0.));
#111639=DIRECTION('ref_axis',(0.,0.,1.));
#111640=DIRECTION('center_axis',(-3.85185988875507E-34,1.,0.));
#111641=DIRECTION('ref_axis',(0.,0.,1.));
#111642=DIRECTION('center_axis',(-3.85185988875507E-34,1.,0.));
#111643=DIRECTION('ref_axis',(1.,0.,0.));
#111644=DIRECTION('center_axis',(-3.85185988875507E-34,1.,0.));
#111645=DIRECTION('ref_axis',(0.,0.,1.));
#111646=DIRECTION('center_axis',(-3.85185988875507E-34,1.,0.));
#111647=DIRECTION('ref_axis',(0.,0.,1.));
#111648=DIRECTION('center_axis',(-3.85185988875507E-34,1.,0.));
#111649=DIRECTION('ref_axis',(1.,0.,0.));
#111650=DIRECTION('center_axis',(-3.85185988875507E-34,1.,0.));
#111651=DIRECTION('ref_axis',(0.,0.,1.));
#111652=DIRECTION('center_axis',(-3.85185988875507E-34,1.,0.));
#111653=DIRECTION('ref_axis',(0.,0.,1.));
#111654=DIRECTION('center_axis',(-3.85185988875507E-34,1.,0.));
#111655=DIRECTION('ref_axis',(1.,0.,0.));
#111656=DIRECTION('center_axis',(-3.85185988875507E-34,1.,0.));
#111657=DIRECTION('ref_axis',(0.,0.,1.));
#111658=DIRECTION('center_axis',(-3.85185988875507E-34,1.,0.));
#111659=DIRECTION('ref_axis',(0.,0.,1.));
#111660=DIRECTION('center_axis',(-3.85185988875507E-34,1.,0.));
#111661=DIRECTION('ref_axis',(1.,0.,0.));
#111662=DIRECTION('center_axis',(-3.85185988875507E-34,1.,0.));
#111663=DIRECTION('ref_axis',(0.,0.,1.));
#111664=DIRECTION('center_axis',(-3.85185988875507E-34,1.,0.));
#111665=DIRECTION('ref_axis',(0.,0.,1.));
#111666=DIRECTION('center_axis',(-3.85185988875507E-34,1.,0.));
#111667=DIRECTION('ref_axis',(1.,0.,0.));
#111668=DIRECTION('center_axis',(-3.85185988875507E-34,1.,0.));
#111669=DIRECTION('ref_axis',(0.,0.,1.));
#111670=DIRECTION('center_axis',(-3.85185988875507E-34,1.,0.));
#111671=DIRECTION('ref_axis',(0.,0.,1.));
#111672=DIRECTION('center_axis',(-3.85185988875507E-34,1.,0.));
#111673=DIRECTION('ref_axis',(1.,0.,0.));
#111674=DIRECTION('center_axis',(-3.85185988875507E-34,1.,0.));
#111675=DIRECTION('ref_axis',(0.,0.,1.));
#111676=DIRECTION('center_axis',(-3.85185988875507E-34,1.,0.));
#111677=DIRECTION('ref_axis',(0.,0.,1.));
#111678=DIRECTION('center_axis',(-3.85185988875507E-34,1.,0.));
#111679=DIRECTION('ref_axis',(1.,0.,0.));
#111680=DIRECTION('center_axis',(-3.85185988875507E-34,1.,0.));
#111681=DIRECTION('ref_axis',(0.,0.,1.));
#111682=DIRECTION('center_axis',(-3.85185988875507E-34,1.,0.));
#111683=DIRECTION('ref_axis',(0.,0.,1.));
#111684=DIRECTION('center_axis',(-3.85185988875507E-34,1.,0.));
#111685=DIRECTION('ref_axis',(1.,0.,0.));
#111686=DIRECTION('center_axis',(-3.85185988875507E-34,1.,0.));
#111687=DIRECTION('ref_axis',(0.,0.,1.));
#111688=DIRECTION('center_axis',(-3.85185988875507E-34,1.,0.));
#111689=DIRECTION('ref_axis',(0.,0.,1.));
#111690=DIRECTION('center_axis',(-3.85185988875507E-34,1.,0.));
#111691=DIRECTION('ref_axis',(1.,0.,0.));
#111692=DIRECTION('center_axis',(-3.85185988875507E-34,1.,0.));
#111693=DIRECTION('ref_axis',(0.,0.,1.));
#111694=DIRECTION('center_axis',(-3.85185988875507E-34,1.,0.));
#111695=DIRECTION('ref_axis',(0.,0.,1.));
#111696=DIRECTION('center_axis',(-3.85185988875507E-34,1.,0.));
#111697=DIRECTION('ref_axis',(1.,0.,0.));
#111698=DIRECTION('center_axis',(-3.85185988875507E-34,1.,0.));
#111699=DIRECTION('ref_axis',(0.,0.,1.));
#111700=DIRECTION('center_axis',(-3.85185988875507E-34,1.,0.));
#111701=DIRECTION('ref_axis',(0.,0.,1.));
#111702=DIRECTION('center_axis',(-3.85185988875507E-34,1.,0.));
#111703=DIRECTION('ref_axis',(1.,0.,0.));
#111704=DIRECTION('center_axis',(-3.85185988875507E-34,1.,0.));
#111705=DIRECTION('ref_axis',(0.,0.,1.));
#111706=DIRECTION('center_axis',(-3.85185988875507E-34,1.,0.));
#111707=DIRECTION('ref_axis',(0.,0.,1.));
#111708=DIRECTION('center_axis',(-3.85185988875507E-34,1.,0.));
#111709=DIRECTION('ref_axis',(1.,0.,0.));
#111710=DIRECTION('center_axis',(-3.85185988875507E-34,1.,0.));
#111711=DIRECTION('ref_axis',(0.,0.,1.));
#111712=DIRECTION('center_axis',(-3.85185988875507E-34,1.,0.));
#111713=DIRECTION('ref_axis',(0.,0.,1.));
#111714=DIRECTION('center_axis',(-3.85185988875507E-34,1.,0.));
#111715=DIRECTION('ref_axis',(1.,0.,0.));
#111716=DIRECTION('center_axis',(-3.85185988875507E-34,1.,0.));
#111717=DIRECTION('ref_axis',(0.,0.,1.));
#111718=DIRECTION('center_axis',(-3.85185988875507E-34,1.,0.));
#111719=DIRECTION('ref_axis',(0.,0.,1.));
#111720=DIRECTION('center_axis',(-3.85185988875507E-34,1.,0.));
#111721=DIRECTION('ref_axis',(1.,0.,0.));
#111722=DIRECTION('center_axis',(-3.85185988875507E-34,1.,0.));
#111723=DIRECTION('ref_axis',(0.,0.,1.));
#111724=DIRECTION('center_axis',(-3.85185988875507E-34,1.,0.));
#111725=DIRECTION('ref_axis',(0.,0.,1.));
#111726=DIRECTION('center_axis',(-3.85185988875507E-34,1.,0.));
#111727=DIRECTION('ref_axis',(1.,0.,0.));
#111728=DIRECTION('center_axis',(-3.85185988875507E-34,1.,0.));
#111729=DIRECTION('ref_axis',(0.,0.,1.));
#111730=DIRECTION('center_axis',(-3.85185988875507E-34,1.,0.));
#111731=DIRECTION('ref_axis',(0.,0.,1.));
#111732=DIRECTION('center_axis',(-3.85185988875507E-34,1.,0.));
#111733=DIRECTION('ref_axis',(1.,0.,0.));
#111734=DIRECTION('center_axis',(-3.85185988875507E-34,1.,0.));
#111735=DIRECTION('ref_axis',(0.,0.,1.));
#111736=DIRECTION('center_axis',(-3.85185988875507E-34,1.,0.));
#111737=DIRECTION('ref_axis',(0.,0.,1.));
#111738=DIRECTION('center_axis',(-3.85185988875507E-34,1.,0.));
#111739=DIRECTION('ref_axis',(1.,0.,0.));
#111740=DIRECTION('center_axis',(-3.85185988875507E-34,1.,0.));
#111741=DIRECTION('ref_axis',(0.,0.,1.));
#111742=DIRECTION('center_axis',(-3.85185988875507E-34,1.,0.));
#111743=DIRECTION('ref_axis',(0.,0.,1.));
#111744=DIRECTION('center_axis',(-3.85185988875507E-34,1.,0.));
#111745=DIRECTION('ref_axis',(1.,0.,0.));
#111746=DIRECTION('center_axis',(-3.85185988875507E-34,1.,0.));
#111747=DIRECTION('ref_axis',(0.,0.,1.));
#111748=DIRECTION('center_axis',(-3.85185988875507E-34,1.,0.));
#111749=DIRECTION('ref_axis',(0.,0.,1.));
#111750=DIRECTION('center_axis',(-3.85185988875507E-34,1.,0.));
#111751=DIRECTION('ref_axis',(1.,0.,0.));
#111752=DIRECTION('center_axis',(-3.85185988875507E-34,1.,0.));
#111753=DIRECTION('ref_axis',(0.,0.,1.));
#111754=DIRECTION('center_axis',(-3.85185988875507E-34,1.,0.));
#111755=DIRECTION('ref_axis',(0.,0.,1.));
#111756=DIRECTION('center_axis',(-3.85185988875507E-34,1.,0.));
#111757=DIRECTION('ref_axis',(1.,0.,0.));
#111758=DIRECTION('center_axis',(-3.85185988875507E-34,1.,0.));
#111759=DIRECTION('ref_axis',(0.,0.,1.));
#111760=DIRECTION('center_axis',(-3.85185988875507E-34,1.,0.));
#111761=DIRECTION('ref_axis',(0.,0.,1.));
#111762=DIRECTION('center_axis',(-3.85185988875507E-34,1.,0.));
#111763=DIRECTION('ref_axis',(1.,0.,0.));
#111764=DIRECTION('center_axis',(-3.85185988875507E-34,1.,0.));
#111765=DIRECTION('ref_axis',(0.,0.,1.));
#111766=DIRECTION('center_axis',(-3.85185988875507E-34,1.,0.));
#111767=DIRECTION('ref_axis',(0.,0.,1.));
#111768=DIRECTION('center_axis',(-3.85185988875507E-34,1.,0.));
#111769=DIRECTION('ref_axis',(1.,0.,0.));
#111770=DIRECTION('center_axis',(-3.85185988875507E-34,1.,0.));
#111771=DIRECTION('ref_axis',(0.,0.,1.));
#111772=DIRECTION('center_axis',(-3.85185988875507E-34,1.,0.));
#111773=DIRECTION('ref_axis',(0.,0.,1.));
#111774=DIRECTION('center_axis',(-3.85185988875507E-34,1.,0.));
#111775=DIRECTION('ref_axis',(1.,0.,0.));
#111776=DIRECTION('center_axis',(-3.85185988875507E-34,1.,0.));
#111777=DIRECTION('ref_axis',(0.,0.,1.));
#111778=DIRECTION('center_axis',(-3.85185988875507E-34,1.,0.));
#111779=DIRECTION('ref_axis',(0.,0.,1.));
#111780=DIRECTION('center_axis',(-3.85185988875507E-34,1.,0.));
#111781=DIRECTION('ref_axis',(1.,0.,0.));
#111782=DIRECTION('center_axis',(-3.85185988875507E-34,1.,0.));
#111783=DIRECTION('ref_axis',(0.,0.,1.));
#111784=DIRECTION('center_axis',(-3.85185988875507E-34,1.,0.));
#111785=DIRECTION('ref_axis',(0.,0.,1.));
#111786=DIRECTION('center_axis',(-3.85185988875507E-34,1.,0.));
#111787=DIRECTION('ref_axis',(1.,0.,0.));
#111788=DIRECTION('center_axis',(-3.85185988875507E-34,1.,0.));
#111789=DIRECTION('ref_axis',(0.,0.,1.));
#111790=DIRECTION('center_axis',(-3.85185988875507E-34,1.,0.));
#111791=DIRECTION('ref_axis',(0.,0.,1.));
#111792=DIRECTION('center_axis',(-3.85185988875507E-34,1.,0.));
#111793=DIRECTION('ref_axis',(1.,0.,0.));
#111794=DIRECTION('center_axis',(-3.85185988875507E-34,1.,0.));
#111795=DIRECTION('ref_axis',(0.,0.,1.));
#111796=DIRECTION('center_axis',(-3.85185988875507E-34,1.,0.));
#111797=DIRECTION('ref_axis',(0.,0.,1.));
#111798=DIRECTION('center_axis',(-3.85185988875507E-34,1.,0.));
#111799=DIRECTION('ref_axis',(1.,0.,0.));
#111800=DIRECTION('center_axis',(-3.85185988875507E-34,1.,0.));
#111801=DIRECTION('ref_axis',(0.,0.,1.));
#111802=DIRECTION('center_axis',(-3.85185988875507E-34,1.,0.));
#111803=DIRECTION('ref_axis',(0.,0.,1.));
#111804=DIRECTION('center_axis',(-3.85185988875507E-34,1.,0.));
#111805=DIRECTION('ref_axis',(1.,0.,0.));
#111806=DIRECTION('center_axis',(-3.85185988875507E-34,1.,0.));
#111807=DIRECTION('ref_axis',(0.,0.,1.));
#111808=DIRECTION('center_axis',(-3.85185988875507E-34,1.,0.));
#111809=DIRECTION('ref_axis',(0.,0.,1.));
#111810=DIRECTION('center_axis',(-3.85185988875507E-34,1.,0.));
#111811=DIRECTION('ref_axis',(1.,0.,0.));
#111812=DIRECTION('center_axis',(-3.85185988875507E-34,1.,0.));
#111813=DIRECTION('ref_axis',(0.,0.,1.));
#111814=DIRECTION('center_axis',(-3.85185988875507E-34,1.,0.));
#111815=DIRECTION('ref_axis',(0.,0.,1.));
#111816=DIRECTION('center_axis',(-3.85185988875507E-34,1.,0.));
#111817=DIRECTION('ref_axis',(1.,0.,0.));
#111818=DIRECTION('center_axis',(-3.85185988875507E-34,1.,0.));
#111819=DIRECTION('ref_axis',(0.,0.,1.));
#111820=DIRECTION('center_axis',(-3.85185988875507E-34,1.,0.));
#111821=DIRECTION('ref_axis',(0.,0.,1.));
#111822=DIRECTION('center_axis',(-3.85185988875507E-34,1.,0.));
#111823=DIRECTION('ref_axis',(1.,0.,0.));
#111824=DIRECTION('center_axis',(-3.85185988875507E-34,1.,0.));
#111825=DIRECTION('ref_axis',(0.,0.,1.));
#111826=DIRECTION('center_axis',(-3.85185988875507E-34,1.,0.));
#111827=DIRECTION('ref_axis',(0.,0.,1.));
#111828=DIRECTION('center_axis',(-3.85185988875507E-34,1.,0.));
#111829=DIRECTION('ref_axis',(1.,0.,0.));
#111830=DIRECTION('center_axis',(-3.85185988875507E-34,1.,0.));
#111831=DIRECTION('ref_axis',(0.,0.,1.));
#111832=DIRECTION('center_axis',(-3.85185988875507E-34,1.,0.));
#111833=DIRECTION('ref_axis',(0.,0.,1.));
#111834=DIRECTION('center_axis',(-3.85185988875507E-34,1.,0.));
#111835=DIRECTION('ref_axis',(1.,0.,0.));
#111836=DIRECTION('center_axis',(-3.85185988875507E-34,1.,0.));
#111837=DIRECTION('ref_axis',(0.,0.,1.));
#111838=DIRECTION('center_axis',(-3.85185988875507E-34,1.,0.));
#111839=DIRECTION('ref_axis',(0.,0.,1.));
#111840=DIRECTION('center_axis',(-3.85185988875507E-34,1.,0.));
#111841=DIRECTION('ref_axis',(1.,0.,0.));
#111842=DIRECTION('center_axis',(-3.85185988875507E-34,1.,0.));
#111843=DIRECTION('ref_axis',(0.,0.,1.));
#111844=DIRECTION('center_axis',(-3.85185988875507E-34,1.,0.));
#111845=DIRECTION('ref_axis',(0.,0.,1.));
#111846=DIRECTION('center_axis',(-3.85185988875507E-34,1.,0.));
#111847=DIRECTION('ref_axis',(1.,0.,0.));
#111848=DIRECTION('center_axis',(-3.85185988875507E-34,1.,0.));
#111849=DIRECTION('ref_axis',(0.,0.,1.));
#111850=DIRECTION('center_axis',(-3.85185988875507E-34,1.,0.));
#111851=DIRECTION('ref_axis',(0.,0.,1.));
#111852=DIRECTION('center_axis',(-3.85185988875507E-34,1.,0.));
#111853=DIRECTION('ref_axis',(1.,0.,0.));
#111854=DIRECTION('center_axis',(-3.85185988875507E-34,1.,0.));
#111855=DIRECTION('ref_axis',(0.,0.,1.));
#111856=DIRECTION('center_axis',(-3.85185988875507E-34,1.,0.));
#111857=DIRECTION('ref_axis',(0.,0.,1.));
#111858=DIRECTION('center_axis',(-3.85185988875507E-34,1.,0.));
#111859=DIRECTION('ref_axis',(1.,0.,0.));
#111860=DIRECTION('center_axis',(-3.85185988875507E-34,1.,0.));
#111861=DIRECTION('ref_axis',(0.,0.,1.));
#111862=DIRECTION('center_axis',(-3.85185988875507E-34,1.,0.));
#111863=DIRECTION('ref_axis',(0.,0.,1.));
#111864=DIRECTION('center_axis',(-3.85185988875507E-34,1.,0.));
#111865=DIRECTION('ref_axis',(1.,0.,0.));
#111866=DIRECTION('center_axis',(-3.85185988875507E-34,1.,0.));
#111867=DIRECTION('ref_axis',(0.,0.,1.));
#111868=DIRECTION('center_axis',(-3.85185988875507E-34,1.,0.));
#111869=DIRECTION('ref_axis',(0.,0.,1.));
#111870=DIRECTION('center_axis',(-3.85185988875507E-34,1.,0.));
#111871=DIRECTION('ref_axis',(1.,0.,0.));
#111872=DIRECTION('center_axis',(-3.85185988875507E-34,1.,0.));
#111873=DIRECTION('ref_axis',(0.,0.,1.));
#111874=DIRECTION('center_axis',(-3.85185988875507E-34,1.,0.));
#111875=DIRECTION('ref_axis',(0.,0.,1.));
#111876=DIRECTION('center_axis',(-3.85185988875507E-34,1.,0.));
#111877=DIRECTION('ref_axis',(1.,0.,0.));
#111878=DIRECTION('center_axis',(-3.85185988875507E-34,1.,0.));
#111879=DIRECTION('ref_axis',(0.,0.,1.));
#111880=DIRECTION('center_axis',(-3.85185988875507E-34,1.,0.));
#111881=DIRECTION('ref_axis',(0.,0.,1.));
#111882=DIRECTION('center_axis',(-3.85185988875507E-34,1.,0.));
#111883=DIRECTION('ref_axis',(1.,0.,0.));
#111884=DIRECTION('center_axis',(-3.85185988875507E-34,1.,0.));
#111885=DIRECTION('ref_axis',(0.,0.,1.));
#111886=DIRECTION('center_axis',(-3.85185988875507E-34,1.,0.));
#111887=DIRECTION('ref_axis',(0.,0.,1.));
#111888=DIRECTION('center_axis',(-3.85185988875507E-34,1.,0.));
#111889=DIRECTION('ref_axis',(1.,0.,0.));
#111890=DIRECTION('center_axis',(-3.85185988875507E-34,1.,0.));
#111891=DIRECTION('ref_axis',(0.,0.,1.));
#111892=DIRECTION('center_axis',(-3.85185988875507E-34,1.,0.));
#111893=DIRECTION('ref_axis',(0.,0.,1.));
#111894=DIRECTION('center_axis',(-3.85185988875507E-34,1.,0.));
#111895=DIRECTION('ref_axis',(1.,0.,0.));
#111896=DIRECTION('center_axis',(-3.85185988875507E-34,1.,0.));
#111897=DIRECTION('ref_axis',(0.,0.,1.));
#111898=DIRECTION('center_axis',(-3.85185988875507E-34,1.,0.));
#111899=DIRECTION('ref_axis',(0.,0.,1.));
#111900=DIRECTION('center_axis',(-3.85185988875507E-34,1.,0.));
#111901=DIRECTION('ref_axis',(1.,0.,0.));
#111902=DIRECTION('center_axis',(-3.85185988875507E-34,1.,0.));
#111903=DIRECTION('ref_axis',(0.,0.,1.));
#111904=DIRECTION('center_axis',(-3.85185988875507E-34,1.,0.));
#111905=DIRECTION('ref_axis',(0.,0.,1.));
#111906=DIRECTION('center_axis',(-3.85185988875507E-34,1.,0.));
#111907=DIRECTION('ref_axis',(1.,0.,0.));
#111908=DIRECTION('center_axis',(-3.85185988875507E-34,1.,0.));
#111909=DIRECTION('ref_axis',(0.,0.,1.));
#111910=DIRECTION('center_axis',(-3.85185988875507E-34,1.,0.));
#111911=DIRECTION('ref_axis',(0.,0.,1.));
#111912=DIRECTION('center_axis',(-3.85185988875507E-34,1.,0.));
#111913=DIRECTION('ref_axis',(1.,0.,0.));
#111914=DIRECTION('center_axis',(-3.85185988875507E-34,1.,0.));
#111915=DIRECTION('ref_axis',(0.,0.,1.));
#111916=DIRECTION('center_axis',(-3.85185988875507E-34,1.,0.));
#111917=DIRECTION('ref_axis',(0.,0.,1.));
#111918=DIRECTION('center_axis',(3.85185988875507E-34,-1.,0.));
#111919=DIRECTION('ref_axis',(-1.,-3.85185988875507E-34,0.));
#111920=DIRECTION('center_axis',(3.85185988875507E-34,-1.,0.));
#111921=DIRECTION('ref_axis',(0.,0.,1.));
#111922=DIRECTION('',(0.707106780557139,-0.707106781815956,8.6595605546469E-17));
#111923=DIRECTION('center_axis',(-3.85185988875507E-34,1.,0.));
#111924=DIRECTION('ref_axis',(0.,0.,-1.));
#111925=DIRECTION('center_axis',(3.85185988875507E-34,-1.,0.));
#111926=DIRECTION('ref_axis',(0.,0.,1.));
#111927=DIRECTION('center_axis',(3.85185988875507E-34,-1.,0.));
#111928=DIRECTION('ref_axis',(-1.,-3.85185988875507E-34,0.));
#111929=DIRECTION('center_axis',(3.85185988875507E-34,-1.,0.));
#111930=DIRECTION('ref_axis',(0.,0.,1.));
#111931=DIRECTION('',(0.707106780557139,-0.707106781815956,8.6595605546469E-17));
#111932=DIRECTION('center_axis',(-3.85185988875507E-34,1.,0.));
#111933=DIRECTION('ref_axis',(0.,0.,-1.));
#111934=DIRECTION('center_axis',(3.85185988875507E-34,-1.,0.));
#111935=DIRECTION('ref_axis',(0.,0.,1.));
#111936=DIRECTION('center_axis',(3.85185988875507E-34,-1.,0.));
#111937=DIRECTION('ref_axis',(-1.,-3.85185988875507E-34,0.));
#111938=DIRECTION('center_axis',(3.85185988875507E-34,-1.,0.));
#111939=DIRECTION('ref_axis',(0.,0.,1.));
#111940=DIRECTION('',(0.707106780557139,-0.707106781815956,8.6595605546469E-17));
#111941=DIRECTION('center_axis',(-3.85185988875507E-34,1.,0.));
#111942=DIRECTION('ref_axis',(0.,0.,-1.));
#111943=DIRECTION('center_axis',(3.85185988875507E-34,-1.,0.));
#111944=DIRECTION('ref_axis',(0.,0.,1.));
#111945=DIRECTION('center_axis',(3.85185988875507E-34,-1.,0.));
#111946=DIRECTION('ref_axis',(-1.,-3.85185988875507E-34,0.));
#111947=DIRECTION('center_axis',(3.85185988875507E-34,-1.,0.));
#111948=DIRECTION('ref_axis',(0.,0.,1.));
#111949=DIRECTION('',(-0.707106780557139,0.707106781815956,-8.65956055464691E-17));
#111950=DIRECTION('center_axis',(-3.85185988875507E-34,1.,0.));
#111951=DIRECTION('ref_axis',(0.,0.,-1.));
#111952=DIRECTION('center_axis',(3.85185988875507E-34,-1.,0.));
#111953=DIRECTION('ref_axis',(0.,0.,1.));
#111954=DIRECTION('center_axis',(-3.85185988875507E-34,1.,0.));
#111955=DIRECTION('ref_axis',(1.,3.85185988875507E-34,0.));
#111956=DIRECTION('center_axis',(-3.85185988875507E-34,1.,0.));
#111957=DIRECTION('ref_axis',(0.,0.,1.));
#111958=DIRECTION('',(-0.707106780557139,0.707106781815956,8.6595605546469E-17));
#111959=DIRECTION('center_axis',(3.85185988875507E-34,-1.,0.));
#111960=DIRECTION('ref_axis',(0.,0.,1.));
#111961=DIRECTION('center_axis',(-3.85185988875507E-34,1.,0.));
#111962=DIRECTION('ref_axis',(1.,3.85185988875507E-34,0.));
#111963=DIRECTION('center_axis',(-3.85185988875507E-34,1.,0.));
#111964=DIRECTION('ref_axis',(0.,0.,1.));
#111965=DIRECTION('',(-0.707106780557139,0.707106781815956,8.6595605546469E-17));
#111966=DIRECTION('center_axis',(3.85185988875507E-34,-1.,0.));
#111967=DIRECTION('ref_axis',(0.,0.,1.));
#111968=DIRECTION('center_axis',(3.85185988875507E-34,-1.,0.));
#111969=DIRECTION('ref_axis',(-1.,-3.85185988875507E-34,0.));
#111970=DIRECTION('center_axis',(3.85185988875507E-34,-1.,0.));
#111971=DIRECTION('ref_axis',(0.,0.,1.));
#111972=DIRECTION('',(-0.707106780557139,0.707106781815956,-8.65956055464691E-17));
#111973=DIRECTION('center_axis',(-3.85185988875507E-34,1.,0.));
#111974=DIRECTION('ref_axis',(0.,0.,-1.));
#111975=DIRECTION('center_axis',(3.85185988875507E-34,-1.,0.));
#111976=DIRECTION('ref_axis',(0.,0.,1.));
#111977=DIRECTION('center_axis',(-3.85185988875507E-34,1.,0.));
#111978=DIRECTION('ref_axis',(1.,3.85185988875507E-34,0.));
#111979=DIRECTION('center_axis',(-3.85185988875507E-34,1.,0.));
#111980=DIRECTION('ref_axis',(0.,0.,1.));
#111981=DIRECTION('',(-0.707106780557139,0.707106781815956,8.6595605546469E-17));
#111982=DIRECTION('center_axis',(3.85185988875507E-34,-1.,0.));
#111983=DIRECTION('ref_axis',(0.,0.,1.));
#111984=DIRECTION('center_axis',(-3.85185988875507E-34,1.,0.));
#111985=DIRECTION('ref_axis',(1.,3.85185988875507E-34,0.));
#111986=DIRECTION('',(-3.85185988875507E-34,1.,0.));
#111987=DIRECTION('center_axis',(-3.85185988875507E-34,1.,0.));
#111988=DIRECTION('ref_axis',(1.,3.85185988875507E-34,0.));
#111989=DIRECTION('',(-3.85185988875507E-34,1.,0.));
#111990=DIRECTION('center_axis',(-3.85185988875507E-34,1.,0.));
#111991=DIRECTION('ref_axis',(1.,3.85185988875507E-34,0.));
#111992=DIRECTION('',(0.707106780557139,-0.707106781815956,-8.6595605546469E-17));
#111993=DIRECTION('center_axis',(-3.85185988875507E-34,1.,0.));
#111994=DIRECTION('ref_axis',(0.,0.,1.));
#111995=DIRECTION('center_axis',(-3.85185988875507E-34,1.,0.));
#111996=DIRECTION('ref_axis',(1.,3.85185988875507E-34,0.));
#111997=DIRECTION('',(3.85185988875507E-34,-1.,0.));
#111998=DIRECTION('center_axis',(-3.85185988875507E-34,1.,0.));
#111999=DIRECTION('ref_axis',(1.,3.85185988875507E-34,0.));
#112000=DIRECTION('',(3.85185988875507E-34,-1.,0.));
#112001=DIRECTION('center_axis',(-3.85185988875507E-34,1.,0.));
#112002=DIRECTION('ref_axis',(0.,0.,1.));
#112003=DIRECTION('center_axis',(-3.85185988875507E-34,1.,0.));
#112004=DIRECTION('ref_axis',(1.,3.85185988875507E-34,0.));
#112005=DIRECTION('',(-3.85185988875507E-34,1.,0.));
#112006=DIRECTION('center_axis',(-3.85185988875507E-34,1.,0.));
#112007=DIRECTION('ref_axis',(1.,3.85185988875507E-34,0.));
#112008=DIRECTION('center_axis',(-3.85185988875507E-34,1.,0.));
#112009=DIRECTION('ref_axis',(1.,3.85185988875507E-34,0.));
#112010=DIRECTION('center_axis',(3.85185988875507E-34,-1.,0.));
#112011=DIRECTION('ref_axis',(-1.,-3.85185988875507E-34,0.));
#112012=DIRECTION('center_axis',(0.,0.,-1.));
#112013=DIRECTION('ref_axis',(-3.85185988875507E-34,1.,0.));
#112014=DIRECTION('center_axis',(0.,0.,-1.));
#112015=DIRECTION('ref_axis',(-1.,-3.85185988875507E-34,0.));
#112016=DIRECTION('center_axis',(0.,0.,-1.));
#112017=DIRECTION('ref_axis',(0.,1.,0.));
#112018=DIRECTION('center_axis',(0.,0.,-1.));
#112019=DIRECTION('ref_axis',(-1.,-3.85185988875507E-34,0.));
#112020=DIRECTION('center_axis',(0.,0.,1.));
#112021=DIRECTION('ref_axis',(3.85185988875507E-34,-1.,0.));
#112022=DIRECTION('center_axis',(-0.089639308998799,-3.45278058788195E-35,
-0.995974293986656));
#112023=DIRECTION('ref_axis',(-3.85185988875507E-34,1.,0.));
#112024=DIRECTION('center_axis',(-0.089639308998799,-3.45278058788195E-35,
-0.995974293986656));
#112025=DIRECTION('ref_axis',(-0.995974293986656,-3.83635343323835E-34,
0.089639308998799));
#112026=DIRECTION('center_axis',(-0.089639308998799,-3.45278058788195E-35,
-0.995974293986656));
#112027=DIRECTION('ref_axis',(0.,1.,0.));
#112028=DIRECTION('center_axis',(-0.089639308998799,-3.45278058788195E-35,
-0.995974293986656));
#112029=DIRECTION('ref_axis',(-0.995974293986656,-3.83635343323835E-34,
0.089639308998799));
#112030=DIRECTION('center_axis',(0.089639308998799,3.45278058788195E-35,
0.995974293986656));
#112031=DIRECTION('ref_axis',(3.85185988875507E-34,-1.,0.));
#112032=DIRECTION('center_axis',(-0.178556894923064,-6.87776141414805E-35,
-0.98392958857605));
#112033=DIRECTION('ref_axis',(-3.85185988875507E-34,1.,0.));
#112034=DIRECTION('center_axis',(-0.178556894923064,-6.87776141414805E-35,
-0.98392958857605));
#112035=DIRECTION('ref_axis',(-0.983929588576049,-3.78995891559536E-34,
0.178556894923064));
#112036=DIRECTION('center_axis',(-0.178556894923064,-6.87776141414805E-35,
-0.98392958857605));
#112037=DIRECTION('ref_axis',(0.,1.,0.));
#112038=DIRECTION('center_axis',(-0.178556894923064,-6.87776141414805E-35,
-0.98392958857605));
#112039=DIRECTION('ref_axis',(-0.983929588576049,-3.78995891559536E-34,
0.178556894923064));
#112040=DIRECTION('center_axis',(0.178556894923064,6.87776141414805E-35,
0.98392958857605));
#112041=DIRECTION('ref_axis',(3.85185988875507E-34,-1.,0.));
#112042=DIRECTION('center_axis',(-0.266036845891333,-1.02473665561974E-34,
-0.963962860606254));
#112043=DIRECTION('ref_axis',(-3.85185988875507E-34,1.,0.));
#112044=DIRECTION('center_axis',(-0.266036845891333,-1.02473665561974E-34,
-0.963962860606254));
#112045=DIRECTION('ref_axis',(-0.963962860606253,-3.71304987701882E-34,
0.266036845891333));
#112046=DIRECTION('center_axis',(-0.266036845891333,-1.02473665561974E-34,
-0.963962860606254));
#112047=DIRECTION('ref_axis',(0.,1.,0.));
#112048=DIRECTION('center_axis',(-0.266036845891333,-1.02473665561974E-34,
-0.963962860606254));
#112049=DIRECTION('ref_axis',(-0.963962860606253,-3.71304987701882E-34,
0.266036845891333));
#112050=DIRECTION('center_axis',(0.266036845891333,1.02473665561974E-34,
0.963962860606254));
#112051=DIRECTION('ref_axis',(3.85185988875507E-34,-1.,0.));
#112052=DIRECTION('center_axis',(-0.351374823891528,-1.35344659006615E-34,
-0.936234870710976));
#112053=DIRECTION('ref_axis',(-3.85185988875507E-34,1.,0.));
#112054=DIRECTION('center_axis',(-0.351374823891528,-1.35344659006615E-34,
-0.936234870710976));
#112055=DIRECTION('ref_axis',(-0.936234870710976,-3.60624554494539E-34,
0.351374823891528));
#112056=DIRECTION('center_axis',(-0.351374823891528,-1.35344659006615E-34,
-0.936234870710976));
#112057=DIRECTION('ref_axis',(0.,1.,0.));
#112058=DIRECTION('center_axis',(-0.351374823891528,-1.35344659006615E-34,
-0.936234870710976));
#112059=DIRECTION('ref_axis',(-0.936234870710976,-3.60624554494539E-34,
0.351374823891528));
#112060=DIRECTION('center_axis',(0.351374823891528,1.35344659006615E-34,
0.936234870710976));
#112061=DIRECTION('ref_axis',(3.85185988875507E-34,-1.,0.));
#112062=DIRECTION('center_axis',(-0.433883738983985,-1.67125937057549E-34,
-0.900968867966745));
#112063=DIRECTION('ref_axis',(-3.85185988875507E-34,1.,0.));
#112064=DIRECTION('center_axis',(-0.433883738983985,-1.67125937057549E-34,
-0.900968867966745));
#112065=DIRECTION('ref_axis',(-0.900968867966744,-3.47040584353816E-34,
0.433883738983985));
#112066=DIRECTION('center_axis',(-0.433883738983985,-1.67125937057549E-34,
-0.900968867966745));
#112067=DIRECTION('ref_axis',(0.,1.,0.));
#112068=DIRECTION('center_axis',(-0.433883738983985,-1.67125937057549E-34,
-0.900968867966745));
#112069=DIRECTION('ref_axis',(-0.900968867966744,-3.47040584353816E-34,
0.433883738983985));
#112070=DIRECTION('center_axis',(0.433883738983985,1.67125937057549E-34,
0.900968867966745));
#112071=DIRECTION('ref_axis',(3.85185988875507E-34,-1.,0.));
#112072=DIRECTION('center_axis',(-0.512899276931483,-1.97561615178386E-34,
-0.858448793885321));
#112073=DIRECTION('ref_axis',(-3.85185988875507E-34,1.,0.));
#112074=DIRECTION('center_axis',(-0.512899276931483,-1.97561615178386E-34,
-0.858448793885321));
#112075=DIRECTION('ref_axis',(-0.858448793885321,-3.30662447571703E-34,
0.512899276931483));
#112076=DIRECTION('center_axis',(-0.512899276931483,-1.97561615178386E-34,
-0.858448793885321));
#112077=DIRECTION('ref_axis',(0.,1.,0.));
#112078=DIRECTION('center_axis',(-0.512899276931483,-1.97561615178386E-34,
-0.858448793885321));
#112079=DIRECTION('ref_axis',(-0.858448793885321,-3.30662447571703E-34,
0.512899276931483));
#112080=DIRECTION('center_axis',(0.512899276931483,1.97561615178386E-34,
0.858448793885321));
#112081=DIRECTION('ref_axis',(3.85185988875507E-34,-1.,0.));
#112082=DIRECTION('center_axis',(-0.587785252279345,-2.26406643645659E-34,
-0.809016994384486));
#112083=DIRECTION('ref_axis',(-3.85185988875507E-34,1.,0.));
#112084=DIRECTION('center_axis',(-0.587785252279345,-2.26406643645659E-34,
-0.809016994384486));
#112085=DIRECTION('ref_axis',(-0.809016994384486,-3.11622010999078E-34,
0.587785252279345));
#112086=DIRECTION('center_axis',(-0.587785252279345,-2.26406643645659E-34,
-0.809016994384486));
#112087=DIRECTION('ref_axis',(0.,1.,0.));
#112088=DIRECTION('center_axis',(-0.587785252279345,-2.26406643645659E-34,
-0.809016994384486));
#112089=DIRECTION('ref_axis',(-0.809016994384486,-3.11622010999078E-34,
0.587785252279345));
#112090=DIRECTION('center_axis',(0.587785252279345,2.26406643645659E-34,
0.809016994384486));
#112091=DIRECTION('ref_axis',(3.85185988875507E-34,-1.,0.));
#112092=DIRECTION('center_axis',(-0.657938725975692,-2.53428778784438E-34,
-0.753071465972177));
#112093=DIRECTION('ref_axis',(-3.85185988875507E-34,1.,0.));
#112094=DIRECTION('center_axis',(-0.657938725975692,-2.53428778784438E-34,
-0.753071465972177));
#112095=DIRECTION('ref_axis',(-0.753071465972177,-2.9007257731442E-34,0.657938725975692));
#112096=DIRECTION('center_axis',(-0.657938725975692,-2.53428778784438E-34,
-0.753071465972177));
#112097=DIRECTION('ref_axis',(0.,1.,0.));
#112098=DIRECTION('center_axis',(-0.657938725975692,-2.53428778784438E-34,
-0.753071465972177));
#112099=DIRECTION('ref_axis',(-0.753071465972177,-2.9007257731442E-34,0.657938725975692));
#112100=DIRECTION('center_axis',(0.657938725975692,2.53428778784438E-34,
0.753071465972177));
#112101=DIRECTION('ref_axis',(3.85185988875507E-34,-1.,0.));
#112102=DIRECTION('center_axis',(-0.722794863903263,-2.78410454406716E-34,
-0.69106264890751));
#112103=DIRECTION('ref_axis',(-3.85185988875507E-34,1.,0.));
#112104=DIRECTION('center_axis',(-0.722794863903263,-2.78410454406716E-34,
-0.69106264890751));
#112105=DIRECTION('ref_axis',(-0.69106264890751,-2.66187649794366E-34,0.722794863903263));
#112106=DIRECTION('center_axis',(-0.722794863903263,-2.78410454406716E-34,
-0.69106264890751));
#112107=DIRECTION('ref_axis',(0.,1.,0.));
#112108=DIRECTION('center_axis',(-0.722794863903263,-2.78410454406716E-34,
-0.69106264890751));
#112109=DIRECTION('ref_axis',(-0.69106264890751,-2.66187649794366E-34,0.722794863903263));
#112110=DIRECTION('center_axis',(0.722794863903263,2.78410454406716E-34,
0.69106264890751));
#112111=DIRECTION('ref_axis',(3.85185988875507E-34,-1.,0.));
#112112=DIRECTION('center_axis',(-0.781831482217226,-3.01150532611845E-34,
-0.623489802173232));
#112113=DIRECTION('ref_axis',(-3.85185988875507E-34,1.,0.));
#112114=DIRECTION('center_axis',(-0.781831482217226,-3.01150532611845E-34,
-0.623489802173232));
#112115=DIRECTION('ref_axis',(-0.623489802173232,-2.4015953600389E-34,0.781831482217226));
#112116=DIRECTION('center_axis',(-0.781831482217226,-3.01150532611845E-34,
-0.623489802173232));
#112117=DIRECTION('ref_axis',(0.,1.,0.));
#112118=DIRECTION('center_axis',(-0.781831482217226,-3.01150532611845E-34,
-0.623489802173232));
#112119=DIRECTION('ref_axis',(-0.623489802173232,-2.4015953600389E-34,0.781831482217226));
#112120=DIRECTION('center_axis',(0.781831482217226,3.01150532611845E-34,
0.623489802173232));
#112121=DIRECTION('ref_axis',(3.85185988875507E-34,-1.,0.));
#112122=DIRECTION('center_axis',(-0.834573254013744,-3.21465924136334E-34,
-0.550896981009072));
#112123=DIRECTION('ref_axis',(-3.85185988875507E-34,1.,0.));
#112124=DIRECTION('center_axis',(-0.834573254013744,-3.21465924136334E-34,
-0.550896981009072));
#112125=DIRECTION('ref_axis',(-0.550896981009072,-2.12197798398511E-34,
0.834573254013744));
#112126=DIRECTION('center_axis',(-0.834573254013744,-3.21465924136334E-34,
-0.550896981009072));
#112127=DIRECTION('ref_axis',(0.,1.,0.));
#112128=DIRECTION('center_axis',(-0.834573254013744,-3.21465924136334E-34,
-0.550896981009072));
#112129=DIRECTION('ref_axis',(-0.550896981009072,-2.12197798398511E-34,
0.834573254013744));
#112130=DIRECTION('center_axis',(0.834573254013744,3.21465924136334E-34,
0.550896981009072));
#112131=DIRECTION('ref_axis',(3.85185988875507E-34,-1.,0.));
#112132=DIRECTION('center_axis',(-0.880595532086284,-3.39193060826008E-34,
-0.473868662046431));
#112133=DIRECTION('ref_axis',(-3.85185988875507E-34,1.,0.));
#112134=DIRECTION('center_axis',(-0.880595532086284,-3.39193060826008E-34,
-0.473868662046431));
#112135=DIRECTION('ref_axis',(-0.473868662046431,-1.82527569187468E-34,
0.880595532086284));
#112136=DIRECTION('center_axis',(-0.880595532086284,-3.39193060826008E-34,
-0.473868662046431));
#112137=DIRECTION('ref_axis',(0.,1.,0.));
#112138=DIRECTION('center_axis',(-0.880595532086284,-3.39193060826008E-34,
-0.473868662046431));
#112139=DIRECTION('ref_axis',(-0.473868662046431,-1.82527569187468E-34,
0.880595532086284));
#112140=DIRECTION('center_axis',(0.880595532086284,3.39193060826008E-34,
0.473868662046431));
#112141=DIRECTION('ref_axis',(3.85185988875507E-34,-1.,0.));
#112142=DIRECTION('center_axis',(-0.919527772341198,-3.54189214287736E-34,
-0.393025032145835));
#112143=DIRECTION('ref_axis',(-3.85185988875507E-34,1.,0.));
#112144=DIRECTION('center_axis',(-0.919527772341198,-3.54189214287736E-34,
-0.393025032145835));
#112145=DIRECTION('ref_axis',(-0.393025032145835,-1.51387735659921E-34,
0.919527772341198));
#112146=DIRECTION('center_axis',(-0.919527772341198,-3.54189214287736E-34,
-0.393025032145835));
#112147=DIRECTION('ref_axis',(0.,1.,0.));
#112148=DIRECTION('center_axis',(-0.919527772341198,-3.54189214287736E-34,
-0.393025032145835));
#112149=DIRECTION('ref_axis',(-0.393025032145835,-1.51387735659921E-34,
0.919527772341198));
#112150=DIRECTION('center_axis',(0.919527772341198,3.54189214287736E-34,
0.393025032145835));
#112151=DIRECTION('ref_axis',(3.85185988875507E-34,-1.,0.));
#112152=DIRECTION('center_axis',(-0.951056516377163,-3.66333644737232E-34,
-0.309016994122548));
#112153=DIRECTION('ref_axis',(-3.85185988875507E-34,1.,0.));
#112154=DIRECTION('center_axis',(-0.951056516377163,-3.66333644737232E-34,
-0.309016994122548));
#112155=DIRECTION('ref_axis',(-0.309016994122548,-1.1902901646043E-34,0.951056516377163));
#112156=DIRECTION('center_axis',(-0.951056516377163,-3.66333644737232E-34,
-0.309016994122548));
#112157=DIRECTION('ref_axis',(0.,1.,0.));
#112158=DIRECTION('center_axis',(-0.951056516377163,-3.66333644737232E-34,
-0.309016994122548));
#112159=DIRECTION('ref_axis',(-0.309016994122548,-1.1902901646043E-34,0.951056516377163));
#112160=DIRECTION('center_axis',(0.951056516377163,3.66333644737232E-34,
0.309016994122548));
#112161=DIRECTION('ref_axis',(3.85185988875507E-34,-1.,0.));
#112162=DIRECTION('center_axis',(-0.974927912163343,-3.75528571928971E-34,
-0.222520934037282));
#112163=DIRECTION('ref_axis',(-3.85185988875507E-34,1.,0.));
#112164=DIRECTION('center_axis',(-0.974927912163343,-3.75528571928971E-34,
-0.222520934037282));
#112165=DIRECTION('ref_axis',(-0.222520934037282,-8.57119460226519E-35,
0.974927912163343));
#112166=DIRECTION('center_axis',(-0.974927912163343,-3.75528571928971E-34,
-0.222520934037282));
#112167=DIRECTION('ref_axis',(0.,1.,0.));
#112168=DIRECTION('center_axis',(-0.974927912163343,-3.75528571928971E-34,
-0.222520934037282));
#112169=DIRECTION('ref_axis',(-0.222520934037282,-8.57119460226519E-35,
0.974927912163343));
#112170=DIRECTION('center_axis',(0.974927912163343,3.75528571928971E-34,
0.222520934037282));
#112171=DIRECTION('ref_axis',(3.85185988875507E-34,-1.,0.));
#112172=DIRECTION('center_axis',(-0.990949761747861,-3.81699963904798E-34,
-0.134233265965845));
#112173=DIRECTION('ref_axis',(-3.85185988875507E-34,1.,0.));
#112174=DIRECTION('center_axis',(-0.990949761747861,-3.81699963904798E-34,
-0.134233265965845));
#112175=DIRECTION('ref_axis',(-0.134233265965845,-5.17047732910431E-35,
0.990949761747861));
#112176=DIRECTION('center_axis',(-0.990949761747861,-3.81699963904798E-34,
-0.134233265965845));
#112177=DIRECTION('ref_axis',(0.,1.,0.));
#112178=DIRECTION('center_axis',(-0.990949761747861,-3.81699963904798E-34,
-0.134233265965845));
#112179=DIRECTION('ref_axis',(-0.134233265965845,-5.17047732910431E-35,
0.990949761747861));
#112180=DIRECTION('center_axis',(0.990949761747861,3.81699963904798E-34,
0.134233265965845));
#112181=DIRECTION('ref_axis',(3.85185988875507E-34,-1.,0.));
#112182=DIRECTION('center_axis',(-0.998993066557948,-3.84798132221898E-34,
-0.0448648299801474));
#112183=DIRECTION('ref_axis',(-3.85185988875507E-34,1.,0.));
#112184=DIRECTION('center_axis',(-0.998993066557948,-3.84798132221898E-34,
-0.0448648299801474));
#112185=DIRECTION('ref_axis',(-0.0448648299801474,-1.72813039016346E-35,
0.998993066557948));
#112186=DIRECTION('center_axis',(-0.998993066557948,-3.84798132221898E-34,
-0.0448648299801474));
#112187=DIRECTION('ref_axis',(0.,1.,0.));
#112188=DIRECTION('center_axis',(-0.998993066557948,-3.84798132221898E-34,
-0.0448648299801474));
#112189=DIRECTION('ref_axis',(-0.0448648299801474,-1.72813039016346E-35,
0.998993066557948));
#112190=DIRECTION('center_axis',(0.998993066557948,3.84798132221898E-34,
0.0448648299801474));
#112191=DIRECTION('ref_axis',(3.85185988875507E-34,-1.,0.));
#112192=DIRECTION('center_axis',(-0.998993066557948,-3.84798132221898E-34,
0.0448648299801474));
#112193=DIRECTION('ref_axis',(-3.85185988875507E-34,1.,0.));
#112194=DIRECTION('center_axis',(-0.998993066557948,-3.84798132221898E-34,
0.0448648299801474));
#112195=DIRECTION('ref_axis',(0.0448648299801474,1.72813039016346E-35,0.998993066557948));
#112196=DIRECTION('center_axis',(-0.998993066557948,-3.84798132221898E-34,
0.0448648299801474));
#112197=DIRECTION('ref_axis',(0.,1.,0.));
#112198=DIRECTION('center_axis',(-0.998993066557948,-3.84798132221898E-34,
0.0448648299801474));
#112199=DIRECTION('ref_axis',(0.0448648299801474,1.72813039016346E-35,0.998993066557948));
#112200=DIRECTION('center_axis',(0.998993066557948,3.84798132221898E-34,
-0.0448648299801474));
#112201=DIRECTION('ref_axis',(3.85185988875507E-34,-1.,0.));
#112202=DIRECTION('center_axis',(-0.990949761747861,-3.81699963904798E-34,
0.134233265965845));
#112203=DIRECTION('ref_axis',(-3.85185988875507E-34,1.,0.));
#112204=DIRECTION('center_axis',(-0.990949761747861,-3.81699963904798E-34,
0.134233265965845));
#112205=DIRECTION('ref_axis',(0.134233265965845,5.17047732910431E-35,0.990949761747861));
#112206=DIRECTION('center_axis',(-0.990949761747861,-3.81699963904798E-34,
0.134233265965845));
#112207=DIRECTION('ref_axis',(0.,1.,0.));
#112208=DIRECTION('center_axis',(-0.990949761747861,-3.81699963904798E-34,
0.134233265965845));
#112209=DIRECTION('ref_axis',(0.134233265965845,5.17047732910431E-35,0.990949761747861));
#112210=DIRECTION('center_axis',(0.990949761747861,3.81699963904798E-34,
-0.134233265965845));
#112211=DIRECTION('ref_axis',(3.85185988875507E-34,-1.,0.));
#112212=DIRECTION('center_axis',(-0.974927912163343,-3.75528571928971E-34,
0.222520934037282));
#112213=DIRECTION('ref_axis',(-3.85185988875507E-34,1.,0.));
#112214=DIRECTION('center_axis',(-0.974927912163343,-3.75528571928971E-34,
0.222520934037282));
#112215=DIRECTION('ref_axis',(0.222520934037282,8.57119460226519E-35,0.974927912163343));
#112216=DIRECTION('center_axis',(-0.974927912163343,-3.75528571928971E-34,
0.222520934037282));
#112217=DIRECTION('ref_axis',(0.,1.,0.));
#112218=DIRECTION('center_axis',(-0.974927912163343,-3.75528571928971E-34,
0.222520934037282));
#112219=DIRECTION('ref_axis',(0.222520934037282,8.57119460226519E-35,0.974927912163343));
#112220=DIRECTION('center_axis',(0.974927912163343,3.75528571928971E-34,
-0.222520934037282));
#112221=DIRECTION('ref_axis',(3.85185988875507E-34,-1.,0.));
#112222=DIRECTION('center_axis',(-0.951056516377163,-3.66333644737232E-34,
0.309016994122548));
#112223=DIRECTION('ref_axis',(-3.85185988875507E-34,1.,0.));
#112224=DIRECTION('center_axis',(-0.951056516377163,-3.66333644737232E-34,
0.309016994122548));
#112225=DIRECTION('ref_axis',(0.309016994122548,1.1902901646043E-34,0.951056516377163));
#112226=DIRECTION('center_axis',(-0.951056516377163,-3.66333644737232E-34,
0.309016994122548));
#112227=DIRECTION('ref_axis',(0.,1.,0.));
#112228=DIRECTION('center_axis',(-0.951056516377163,-3.66333644737232E-34,
0.309016994122548));
#112229=DIRECTION('ref_axis',(0.309016994122548,1.1902901646043E-34,0.951056516377163));
#112230=DIRECTION('center_axis',(0.951056516377163,3.66333644737232E-34,
-0.309016994122548));
#112231=DIRECTION('ref_axis',(3.85185988875507E-34,-1.,0.));
#112232=DIRECTION('center_axis',(-0.919527772341198,-3.54189214287736E-34,
0.393025032145835));
#112233=DIRECTION('ref_axis',(-3.85185988875507E-34,1.,0.));
#112234=DIRECTION('center_axis',(-0.919527772341198,-3.54189214287736E-34,
0.393025032145835));
#112235=DIRECTION('ref_axis',(0.393025032145835,1.51387735659921E-34,0.919527772341198));
#112236=DIRECTION('center_axis',(-0.919527772341198,-3.54189214287736E-34,
0.393025032145835));
#112237=DIRECTION('ref_axis',(0.,1.,0.));
#112238=DIRECTION('center_axis',(-0.919527772341198,-3.54189214287736E-34,
0.393025032145835));
#112239=DIRECTION('ref_axis',(0.393025032145835,1.51387735659921E-34,0.919527772341198));
#112240=DIRECTION('center_axis',(0.919527772341198,3.54189214287736E-34,
-0.393025032145835));
#112241=DIRECTION('ref_axis',(3.85185988875507E-34,-1.,0.));
#112242=DIRECTION('center_axis',(-0.880595532086284,-3.39193060826008E-34,
0.473868662046431));
#112243=DIRECTION('ref_axis',(-3.85185988875507E-34,1.,0.));
#112244=DIRECTION('center_axis',(-0.880595532086284,-3.39193060826008E-34,
0.473868662046431));
#112245=DIRECTION('ref_axis',(0.473868662046431,1.82527569187468E-34,0.880595532086284));
#112246=DIRECTION('center_axis',(-0.880595532086284,-3.39193060826008E-34,
0.473868662046431));
#112247=DIRECTION('ref_axis',(0.,1.,0.));
#112248=DIRECTION('center_axis',(-0.880595532086284,-3.39193060826008E-34,
0.473868662046431));
#112249=DIRECTION('ref_axis',(0.473868662046431,1.82527569187468E-34,0.880595532086284));
#112250=DIRECTION('center_axis',(0.880595532086284,3.39193060826008E-34,
-0.473868662046431));
#112251=DIRECTION('ref_axis',(3.85185988875507E-34,-1.,0.));
#112252=DIRECTION('center_axis',(-0.834573254013744,-3.21465924136334E-34,
0.550896981009072));
#112253=DIRECTION('ref_axis',(-3.85185988875507E-34,1.,0.));
#112254=DIRECTION('center_axis',(-0.834573254013744,-3.21465924136334E-34,
0.550896981009072));
#112255=DIRECTION('ref_axis',(0.550896981009072,2.12197798398511E-34,0.834573254013744));
#112256=DIRECTION('center_axis',(-0.834573254013744,-3.21465924136334E-34,
0.550896981009072));
#112257=DIRECTION('ref_axis',(0.,1.,0.));
#112258=DIRECTION('center_axis',(-0.834573254013744,-3.21465924136334E-34,
0.550896981009072));
#112259=DIRECTION('ref_axis',(0.550896981009072,2.12197798398511E-34,0.834573254013744));
#112260=DIRECTION('center_axis',(0.834573254013744,3.21465924136334E-34,
-0.550896981009072));
#112261=DIRECTION('ref_axis',(3.85185988875507E-34,-1.,0.));
#112262=DIRECTION('center_axis',(-0.781831482217226,-3.01150532611845E-34,
0.623489802173232));
#112263=DIRECTION('ref_axis',(-3.85185988875507E-34,1.,0.));
#112264=DIRECTION('center_axis',(-0.781831482217226,-3.01150532611845E-34,
0.623489802173232));
#112265=DIRECTION('ref_axis',(0.623489802173232,2.4015953600389E-34,0.781831482217226));
#112266=DIRECTION('center_axis',(-0.781831482217226,-3.01150532611845E-34,
0.623489802173232));
#112267=DIRECTION('ref_axis',(0.,1.,0.));
#112268=DIRECTION('center_axis',(-0.781831482217226,-3.01150532611845E-34,
0.623489802173232));
#112269=DIRECTION('ref_axis',(0.623489802173232,2.4015953600389E-34,0.781831482217226));
#112270=DIRECTION('center_axis',(0.781831482217226,3.01150532611845E-34,
-0.623489802173232));
#112271=DIRECTION('ref_axis',(3.85185988875507E-34,-1.,0.));
#112272=DIRECTION('center_axis',(-0.722794863903263,-2.78410454406716E-34,
0.69106264890751));
#112273=DIRECTION('ref_axis',(-3.85185988875507E-34,1.,0.));
#112274=DIRECTION('center_axis',(-0.722794863903263,-2.78410454406716E-34,
0.69106264890751));
#112275=DIRECTION('ref_axis',(0.69106264890751,2.66187649794366E-34,0.722794863903263));
#112276=DIRECTION('center_axis',(-0.722794863903263,-2.78410454406716E-34,
0.69106264890751));
#112277=DIRECTION('ref_axis',(0.,1.,0.));
#112278=DIRECTION('center_axis',(-0.722794863903263,-2.78410454406716E-34,
0.69106264890751));
#112279=DIRECTION('ref_axis',(0.69106264890751,2.66187649794366E-34,0.722794863903263));
#112280=DIRECTION('center_axis',(0.722794863903263,2.78410454406716E-34,
-0.69106264890751));
#112281=DIRECTION('ref_axis',(3.85185988875507E-34,-1.,0.));
#112282=DIRECTION('center_axis',(-0.657938725975692,-2.53428778784438E-34,
0.753071465972177));
#112283=DIRECTION('ref_axis',(-3.85185988875507E-34,1.,0.));
#112284=DIRECTION('center_axis',(-0.657938725975692,-2.53428778784438E-34,
0.753071465972177));
#112285=DIRECTION('ref_axis',(0.753071465972177,2.9007257731442E-34,0.657938725975692));
#112286=DIRECTION('center_axis',(-0.657938725975692,-2.53428778784438E-34,
0.753071465972177));
#112287=DIRECTION('ref_axis',(0.,1.,0.));
#112288=DIRECTION('center_axis',(-0.657938725975692,-2.53428778784438E-34,
0.753071465972177));
#112289=DIRECTION('ref_axis',(0.753071465972177,2.9007257731442E-34,0.657938725975692));
#112290=DIRECTION('center_axis',(0.657938725975692,2.53428778784438E-34,
-0.753071465972177));
#112291=DIRECTION('ref_axis',(3.85185988875507E-34,-1.,0.));
#112292=DIRECTION('center_axis',(-0.587785252279345,-2.26406643645659E-34,
0.809016994384486));
#112293=DIRECTION('ref_axis',(-3.85185988875507E-34,1.,0.));
#112294=DIRECTION('center_axis',(-0.587785252279345,-2.26406643645659E-34,
0.809016994384486));
#112295=DIRECTION('ref_axis',(0.809016994384486,3.11622010999078E-34,0.587785252279345));
#112296=DIRECTION('center_axis',(-0.587785252279345,-2.26406643645659E-34,
0.809016994384486));
#112297=DIRECTION('ref_axis',(0.,1.,0.));
#112298=DIRECTION('center_axis',(-0.587785252279345,-2.26406643645659E-34,
0.809016994384486));
#112299=DIRECTION('ref_axis',(0.809016994384486,3.11622010999078E-34,0.587785252279345));
#112300=DIRECTION('center_axis',(0.587785252279345,2.26406643645659E-34,
-0.809016994384486));
#112301=DIRECTION('ref_axis',(3.85185988875507E-34,-1.,0.));
#112302=DIRECTION('center_axis',(-0.512899276931483,-1.97561615178386E-34,
0.858448793885321));
#112303=DIRECTION('ref_axis',(-3.85185988875507E-34,1.,0.));
#112304=DIRECTION('center_axis',(-0.512899276931483,-1.97561615178386E-34,
0.858448793885321));
#112305=DIRECTION('ref_axis',(0.858448793885321,3.30662447571703E-34,0.512899276931483));
#112306=DIRECTION('center_axis',(-0.512899276931483,-1.97561615178386E-34,
0.858448793885321));
#112307=DIRECTION('ref_axis',(0.,1.,0.));
#112308=DIRECTION('center_axis',(-0.512899276931483,-1.97561615178386E-34,
0.858448793885321));
#112309=DIRECTION('ref_axis',(0.858448793885321,3.30662447571703E-34,0.512899276931483));
#112310=DIRECTION('center_axis',(0.512899276931483,1.97561615178386E-34,
-0.858448793885321));
#112311=DIRECTION('ref_axis',(3.85185988875507E-34,-1.,0.));
#112312=DIRECTION('center_axis',(-0.433883738983985,-1.67125937057549E-34,
0.900968867966745));
#112313=DIRECTION('ref_axis',(-3.85185988875507E-34,1.,0.));
#112314=DIRECTION('center_axis',(-0.433883738983985,-1.67125937057549E-34,
0.900968867966745));
#112315=DIRECTION('ref_axis',(0.900968867966744,3.47040584353816E-34,0.433883738983985));
#112316=DIRECTION('center_axis',(-0.433883738983985,-1.67125937057549E-34,
0.900968867966745));
#112317=DIRECTION('ref_axis',(0.,1.,0.));
#112318=DIRECTION('center_axis',(-0.433883738983985,-1.67125937057549E-34,
0.900968867966745));
#112319=DIRECTION('ref_axis',(0.900968867966744,3.47040584353816E-34,0.433883738983985));
#112320=DIRECTION('center_axis',(0.433883738983985,1.67125937057549E-34,
-0.900968867966745));
#112321=DIRECTION('ref_axis',(3.85185988875507E-34,-1.,0.));
#112322=DIRECTION('center_axis',(-0.351374823891528,-1.35344659006615E-34,
0.936234870710976));
#112323=DIRECTION('ref_axis',(-3.85185988875507E-34,1.,0.));
#112324=DIRECTION('center_axis',(-0.351374823891528,-1.35344659006615E-34,
0.936234870710976));
#112325=DIRECTION('ref_axis',(0.936234870710976,3.60624554494539E-34,0.351374823891528));
#112326=DIRECTION('center_axis',(-0.351374823891528,-1.35344659006615E-34,
0.936234870710976));
#112327=DIRECTION('ref_axis',(0.,1.,0.));
#112328=DIRECTION('center_axis',(-0.351374823891528,-1.35344659006615E-34,
0.936234870710976));
#112329=DIRECTION('ref_axis',(0.936234870710976,3.60624554494539E-34,0.351374823891528));
#112330=DIRECTION('center_axis',(0.351374823891528,1.35344659006615E-34,
-0.936234870710976));
#112331=DIRECTION('ref_axis',(3.85185988875507E-34,-1.,0.));
#112332=DIRECTION('center_axis',(-0.266036845891333,-1.02473665561974E-34,
0.963962860606254));
#112333=DIRECTION('ref_axis',(-3.85185988875507E-34,1.,0.));
#112334=DIRECTION('center_axis',(-0.266036845891333,-1.02473665561974E-34,
0.963962860606254));
#112335=DIRECTION('ref_axis',(0.963962860606253,3.71304987701882E-34,0.266036845891333));
#112336=DIRECTION('center_axis',(-0.266036845891333,-1.02473665561974E-34,
0.963962860606254));
#112337=DIRECTION('ref_axis',(0.,1.,0.));
#112338=DIRECTION('center_axis',(-0.266036845891333,-1.02473665561974E-34,
0.963962860606254));
#112339=DIRECTION('ref_axis',(0.963962860606253,3.71304987701882E-34,0.266036845891333));
#112340=DIRECTION('center_axis',(0.266036845891333,1.02473665561974E-34,
-0.963962860606254));
#112341=DIRECTION('ref_axis',(3.85185988875507E-34,-1.,0.));
#112342=DIRECTION('center_axis',(-0.178556894923064,-6.87776141414805E-35,
0.98392958857605));
#112343=DIRECTION('ref_axis',(-3.85185988875507E-34,1.,0.));
#112344=DIRECTION('center_axis',(-0.178556894923064,-6.87776141414805E-35,
0.98392958857605));
#112345=DIRECTION('ref_axis',(0.983929588576049,3.78995891559536E-34,0.178556894923064));
#112346=DIRECTION('center_axis',(-0.178556894923064,-6.87776141414805E-35,
0.98392958857605));
#112347=DIRECTION('ref_axis',(0.,1.,0.));
#112348=DIRECTION('center_axis',(-0.178556894923064,-6.87776141414805E-35,
0.98392958857605));
#112349=DIRECTION('ref_axis',(0.983929588576049,3.78995891559536E-34,0.178556894923064));
#112350=DIRECTION('center_axis',(0.178556894923064,6.87776141414805E-35,
-0.98392958857605));
#112351=DIRECTION('ref_axis',(3.85185988875507E-34,-1.,0.));
#112352=DIRECTION('center_axis',(-0.089639308998799,-3.45278058788195E-35,
0.995974293986656));
#112353=DIRECTION('ref_axis',(-3.85185988875507E-34,1.,0.));
#112354=DIRECTION('center_axis',(-0.089639308998799,-3.45278058788195E-35,
0.995974293986656));
#112355=DIRECTION('ref_axis',(0.995974293986656,3.83635343323835E-34,0.089639308998799));
#112356=DIRECTION('center_axis',(-0.089639308998799,-3.45278058788195E-35,
0.995974293986656));
#112357=DIRECTION('ref_axis',(0.,1.,0.));
#112358=DIRECTION('center_axis',(-0.089639308998799,-3.45278058788195E-35,
0.995974293986656));
#112359=DIRECTION('ref_axis',(0.995974293986656,3.83635343323835E-34,0.089639308998799));
#112360=DIRECTION('center_axis',(0.089639308998799,3.45278058788195E-35,
-0.995974293986656));
#112361=DIRECTION('ref_axis',(3.85185988875507E-34,-1.,0.));
#112362=DIRECTION('center_axis',(0.,0.,1.));
#112363=DIRECTION('ref_axis',(-3.85185988875507E-34,1.,0.));
#112364=DIRECTION('center_axis',(0.,0.,1.));
#112365=DIRECTION('ref_axis',(1.,3.85185988875507E-34,0.));
#112366=DIRECTION('center_axis',(0.,0.,1.));
#112367=DIRECTION('ref_axis',(0.,1.,0.));
#112368=DIRECTION('center_axis',(0.,0.,1.));
#112369=DIRECTION('ref_axis',(1.,3.85185988875507E-34,0.));
#112370=DIRECTION('center_axis',(0.,0.,-1.));
#112371=DIRECTION('ref_axis',(3.85185988875507E-34,-1.,0.));
#112372=DIRECTION('center_axis',(0.089639308998799,3.45278058788195E-35,
0.995974293986656));
#112373=DIRECTION('ref_axis',(-3.85185988875507E-34,1.,0.));
#112374=DIRECTION('center_axis',(0.089639308998799,3.45278058788195E-35,
0.995974293986656));
#112375=DIRECTION('ref_axis',(0.995974293986656,3.83635343323835E-34,-0.089639308998799));
#112376=DIRECTION('center_axis',(0.089639308998799,3.45278058788195E-35,
0.995974293986656));
#112377=DIRECTION('ref_axis',(0.,1.,0.));
#112378=DIRECTION('center_axis',(0.089639308998799,3.45278058788195E-35,
0.995974293986656));
#112379=DIRECTION('ref_axis',(0.995974293986656,3.83635343323835E-34,-0.089639308998799));
#112380=DIRECTION('center_axis',(-0.089639308998799,-3.45278058788195E-35,
-0.995974293986656));
#112381=DIRECTION('ref_axis',(3.85185988875507E-34,-1.,0.));
#112382=DIRECTION('center_axis',(0.178556894923064,6.87776141414805E-35,
0.98392958857605));
#112383=DIRECTION('ref_axis',(-3.85185988875507E-34,1.,0.));
#112384=DIRECTION('center_axis',(0.178556894923064,6.87776141414805E-35,
0.98392958857605));
#112385=DIRECTION('ref_axis',(0.983929588576049,3.78995891559536E-34,-0.178556894923064));
#112386=DIRECTION('center_axis',(0.178556894923064,6.87776141414805E-35,
0.98392958857605));
#112387=DIRECTION('ref_axis',(0.,1.,0.));
#112388=DIRECTION('center_axis',(0.178556894923064,6.87776141414805E-35,
0.98392958857605));
#112389=DIRECTION('ref_axis',(0.983929588576049,3.78995891559536E-34,-0.178556894923064));
#112390=DIRECTION('center_axis',(-0.178556894923064,-6.87776141414805E-35,
-0.98392958857605));
#112391=DIRECTION('ref_axis',(3.85185988875507E-34,-1.,0.));
#112392=DIRECTION('center_axis',(0.266036845891333,1.02473665561974E-34,
0.963962860606254));
#112393=DIRECTION('ref_axis',(-3.85185988875507E-34,1.,0.));
#112394=DIRECTION('center_axis',(0.266036845891333,1.02473665561974E-34,
0.963962860606254));
#112395=DIRECTION('ref_axis',(0.963962860606253,3.71304987701882E-34,-0.266036845891333));
#112396=DIRECTION('center_axis',(0.266036845891333,1.02473665561974E-34,
0.963962860606254));
#112397=DIRECTION('ref_axis',(0.,1.,0.));
#112398=DIRECTION('center_axis',(0.266036845891333,1.02473665561974E-34,
0.963962860606254));
#112399=DIRECTION('ref_axis',(0.963962860606253,3.71304987701882E-34,-0.266036845891333));
#112400=DIRECTION('center_axis',(-0.266036845891333,-1.02473665561974E-34,
-0.963962860606254));
#112401=DIRECTION('ref_axis',(3.85185988875507E-34,-1.,0.));
#112402=DIRECTION('center_axis',(0.351374823891528,1.35344659006615E-34,
0.936234870710976));
#112403=DIRECTION('ref_axis',(-3.85185988875507E-34,1.,0.));
#112404=DIRECTION('center_axis',(0.351374823891528,1.35344659006615E-34,
0.936234870710976));
#112405=DIRECTION('ref_axis',(0.936234870710976,3.60624554494539E-34,-0.351374823891528));
#112406=DIRECTION('center_axis',(0.351374823891528,1.35344659006615E-34,
0.936234870710976));
#112407=DIRECTION('ref_axis',(0.,1.,0.));
#112408=DIRECTION('center_axis',(0.351374823891528,1.35344659006615E-34,
0.936234870710976));
#112409=DIRECTION('ref_axis',(0.936234870710976,3.60624554494539E-34,-0.351374823891528));
#112410=DIRECTION('center_axis',(-0.351374823891528,-1.35344659006615E-34,
-0.936234870710976));
#112411=DIRECTION('ref_axis',(3.85185988875507E-34,-1.,0.));
#112412=DIRECTION('center_axis',(0.433883738983985,1.67125937057549E-34,
0.900968867966745));
#112413=DIRECTION('ref_axis',(-3.85185988875507E-34,1.,0.));
#112414=DIRECTION('center_axis',(0.433883738983985,1.67125937057549E-34,
0.900968867966745));
#112415=DIRECTION('ref_axis',(0.900968867966744,3.47040584353816E-34,-0.433883738983985));
#112416=DIRECTION('center_axis',(0.433883738983985,1.67125937057549E-34,
0.900968867966745));
#112417=DIRECTION('ref_axis',(0.,1.,0.));
#112418=DIRECTION('center_axis',(0.433883738983985,1.67125937057549E-34,
0.900968867966745));
#112419=DIRECTION('ref_axis',(0.900968867966744,3.47040584353816E-34,-0.433883738983985));
#112420=DIRECTION('center_axis',(-0.433883738983985,-1.67125937057549E-34,
-0.900968867966745));
#112421=DIRECTION('ref_axis',(3.85185988875507E-34,-1.,0.));
#112422=DIRECTION('center_axis',(0.512899276931483,1.97561615178386E-34,
0.858448793885321));
#112423=DIRECTION('ref_axis',(-3.85185988875507E-34,1.,0.));
#112424=DIRECTION('center_axis',(0.512899276931483,1.97561615178386E-34,
0.858448793885321));
#112425=DIRECTION('ref_axis',(0.858448793885321,3.30662447571703E-34,-0.512899276931483));
#112426=DIRECTION('center_axis',(0.512899276931483,1.97561615178386E-34,
0.858448793885321));
#112427=DIRECTION('ref_axis',(0.,1.,0.));
#112428=DIRECTION('center_axis',(0.512899276931483,1.97561615178386E-34,
0.858448793885321));
#112429=DIRECTION('ref_axis',(0.858448793885321,3.30662447571703E-34,-0.512899276931483));
#112430=DIRECTION('center_axis',(-0.512899276931483,-1.97561615178386E-34,
-0.858448793885321));
#112431=DIRECTION('ref_axis',(3.85185988875507E-34,-1.,0.));
#112432=DIRECTION('center_axis',(0.587785252279345,2.26406643645659E-34,
0.809016994384486));
#112433=DIRECTION('ref_axis',(-3.85185988875507E-34,1.,0.));
#112434=DIRECTION('center_axis',(0.587785252279345,2.26406643645659E-34,
0.809016994384486));
#112435=DIRECTION('ref_axis',(0.809016994384486,3.11622010999078E-34,-0.587785252279345));
#112436=DIRECTION('center_axis',(0.587785252279345,2.26406643645659E-34,
0.809016994384486));
#112437=DIRECTION('ref_axis',(0.,1.,0.));
#112438=DIRECTION('center_axis',(0.587785252279345,2.26406643645659E-34,
0.809016994384486));
#112439=DIRECTION('ref_axis',(0.809016994384486,3.11622010999078E-34,-0.587785252279345));
#112440=DIRECTION('center_axis',(-0.587785252279345,-2.26406643645659E-34,
-0.809016994384486));
#112441=DIRECTION('ref_axis',(3.85185988875507E-34,-1.,0.));
#112442=DIRECTION('center_axis',(0.657938725975692,2.53428778784438E-34,
0.753071465972177));
#112443=DIRECTION('ref_axis',(-3.85185988875507E-34,1.,0.));
#112444=DIRECTION('center_axis',(0.657938725975692,2.53428778784438E-34,
0.753071465972177));
#112445=DIRECTION('ref_axis',(0.753071465972177,2.9007257731442E-34,-0.657938725975692));
#112446=DIRECTION('center_axis',(0.657938725975692,2.53428778784438E-34,
0.753071465972177));
#112447=DIRECTION('ref_axis',(0.,1.,0.));
#112448=DIRECTION('center_axis',(0.657938725975692,2.53428778784438E-34,
0.753071465972177));
#112449=DIRECTION('ref_axis',(0.753071465972177,2.9007257731442E-34,-0.657938725975692));
#112450=DIRECTION('center_axis',(-0.657938725975692,-2.53428778784438E-34,
-0.753071465972177));
#112451=DIRECTION('ref_axis',(3.85185988875507E-34,-1.,0.));
#112452=DIRECTION('center_axis',(0.722794863903263,2.78410454406716E-34,
0.69106264890751));
#112453=DIRECTION('ref_axis',(-3.85185988875507E-34,1.,0.));
#112454=DIRECTION('center_axis',(0.722794863903263,2.78410454406716E-34,
0.69106264890751));
#112455=DIRECTION('ref_axis',(0.69106264890751,2.66187649794366E-34,-0.722794863903263));
#112456=DIRECTION('center_axis',(0.722794863903263,2.78410454406716E-34,
0.69106264890751));
#112457=DIRECTION('ref_axis',(0.,1.,0.));
#112458=DIRECTION('center_axis',(0.722794863903263,2.78410454406716E-34,
0.69106264890751));
#112459=DIRECTION('ref_axis',(0.69106264890751,2.66187649794366E-34,-0.722794863903263));
#112460=DIRECTION('center_axis',(-0.722794863903263,-2.78410454406716E-34,
-0.69106264890751));
#112461=DIRECTION('ref_axis',(3.85185988875507E-34,-1.,0.));
#112462=DIRECTION('center_axis',(0.781831482217226,3.01150532611845E-34,
0.623489802173232));
#112463=DIRECTION('ref_axis',(-3.85185988875507E-34,1.,0.));
#112464=DIRECTION('center_axis',(0.781831482217226,3.01150532611845E-34,
0.623489802173232));
#112465=DIRECTION('ref_axis',(0.623489802173232,2.4015953600389E-34,-0.781831482217226));
#112466=DIRECTION('center_axis',(0.781831482217226,3.01150532611845E-34,
0.623489802173232));
#112467=DIRECTION('ref_axis',(0.,1.,0.));
#112468=DIRECTION('center_axis',(0.781831482217226,3.01150532611845E-34,
0.623489802173232));
#112469=DIRECTION('ref_axis',(0.623489802173232,2.4015953600389E-34,-0.781831482217226));
#112470=DIRECTION('center_axis',(-0.781831482217226,-3.01150532611845E-34,
-0.623489802173232));
#112471=DIRECTION('ref_axis',(3.85185988875507E-34,-1.,0.));
#112472=DIRECTION('center_axis',(0.834573254013744,3.21465924136334E-34,
0.550896981009072));
#112473=DIRECTION('ref_axis',(-3.85185988875507E-34,1.,0.));
#112474=DIRECTION('center_axis',(0.834573254013744,3.21465924136334E-34,
0.550896981009072));
#112475=DIRECTION('ref_axis',(0.550896981009072,2.12197798398511E-34,-0.834573254013744));
#112476=DIRECTION('center_axis',(0.834573254013744,3.21465924136334E-34,
0.550896981009072));
#112477=DIRECTION('ref_axis',(0.,1.,0.));
#112478=DIRECTION('center_axis',(0.834573254013744,3.21465924136334E-34,
0.550896981009072));
#112479=DIRECTION('ref_axis',(0.550896981009072,2.12197798398511E-34,-0.834573254013744));
#112480=DIRECTION('center_axis',(-0.834573254013744,-3.21465924136334E-34,
-0.550896981009072));
#112481=DIRECTION('ref_axis',(3.85185988875507E-34,-1.,0.));
#112482=DIRECTION('center_axis',(0.880595532086284,3.39193060826008E-34,
0.473868662046431));
#112483=DIRECTION('ref_axis',(-3.85185988875507E-34,1.,0.));
#112484=DIRECTION('center_axis',(0.880595532086284,3.39193060826008E-34,
0.473868662046431));
#112485=DIRECTION('ref_axis',(0.473868662046431,1.82527569187468E-34,-0.880595532086284));
#112486=DIRECTION('center_axis',(0.880595532086284,3.39193060826008E-34,
0.473868662046431));
#112487=DIRECTION('ref_axis',(0.,1.,0.));
#112488=DIRECTION('center_axis',(0.880595532086284,3.39193060826008E-34,
0.473868662046431));
#112489=DIRECTION('ref_axis',(0.473868662046431,1.82527569187468E-34,-0.880595532086284));
#112490=DIRECTION('center_axis',(-0.880595532086284,-3.39193060826008E-34,
-0.473868662046431));
#112491=DIRECTION('ref_axis',(3.85185988875507E-34,-1.,0.));
#112492=DIRECTION('center_axis',(0.919527772341198,3.54189214287736E-34,
0.393025032145835));
#112493=DIRECTION('ref_axis',(-3.85185988875507E-34,1.,0.));
#112494=DIRECTION('center_axis',(0.919527772341198,3.54189214287736E-34,
0.393025032145835));
#112495=DIRECTION('ref_axis',(0.393025032145835,1.51387735659921E-34,-0.919527772341198));
#112496=DIRECTION('center_axis',(0.919527772341198,3.54189214287736E-34,
0.393025032145835));
#112497=DIRECTION('ref_axis',(0.,1.,0.));
#112498=DIRECTION('center_axis',(0.919527772341198,3.54189214287736E-34,
0.393025032145835));
#112499=DIRECTION('ref_axis',(0.393025032145835,1.51387735659921E-34,-0.919527772341198));
#112500=DIRECTION('center_axis',(-0.919527772341198,-3.54189214287736E-34,
-0.393025032145835));
#112501=DIRECTION('ref_axis',(3.85185988875507E-34,-1.,0.));
#112502=DIRECTION('center_axis',(0.951056516377163,3.66333644737232E-34,
0.309016994122548));
#112503=DIRECTION('ref_axis',(-3.85185988875507E-34,1.,0.));
#112504=DIRECTION('center_axis',(0.951056516377163,3.66333644737232E-34,
0.309016994122548));
#112505=DIRECTION('ref_axis',(0.309016994122548,1.1902901646043E-34,-0.951056516377163));
#112506=DIRECTION('center_axis',(0.951056516377163,3.66333644737232E-34,
0.309016994122548));
#112507=DIRECTION('ref_axis',(0.,1.,0.));
#112508=DIRECTION('center_axis',(0.951056516377163,3.66333644737232E-34,
0.309016994122548));
#112509=DIRECTION('ref_axis',(0.309016994122548,1.1902901646043E-34,-0.951056516377163));
#112510=DIRECTION('center_axis',(-0.951056516377163,-3.66333644737232E-34,
-0.309016994122548));
#112511=DIRECTION('ref_axis',(3.85185988875507E-34,-1.,0.));
#112512=DIRECTION('center_axis',(0.974927912163343,3.75528571928971E-34,
0.222520934037282));
#112513=DIRECTION('ref_axis',(-3.85185988875507E-34,1.,0.));
#112514=DIRECTION('center_axis',(0.974927912163343,3.75528571928971E-34,
0.222520934037282));
#112515=DIRECTION('ref_axis',(0.222520934037282,8.57119460226519E-35,-0.974927912163343));
#112516=DIRECTION('center_axis',(0.974927912163343,3.75528571928971E-34,
0.222520934037282));
#112517=DIRECTION('ref_axis',(0.,1.,0.));
#112518=DIRECTION('center_axis',(0.974927912163343,3.75528571928971E-34,
0.222520934037282));
#112519=DIRECTION('ref_axis',(0.222520934037282,8.57119460226519E-35,-0.974927912163343));
#112520=DIRECTION('center_axis',(-0.974927912163343,-3.75528571928971E-34,
-0.222520934037282));
#112521=DIRECTION('ref_axis',(3.85185988875507E-34,-1.,0.));
#112522=DIRECTION('center_axis',(0.990949761747861,3.81699963904798E-34,
0.134233265965845));
#112523=DIRECTION('ref_axis',(-3.85185988875507E-34,1.,0.));
#112524=DIRECTION('center_axis',(0.990949761747861,3.81699963904798E-34,
0.134233265965845));
#112525=DIRECTION('ref_axis',(0.134233265965845,5.17047732910431E-35,-0.990949761747861));
#112526=DIRECTION('center_axis',(0.990949761747861,3.81699963904798E-34,
0.134233265965845));
#112527=DIRECTION('ref_axis',(0.,1.,0.));
#112528=DIRECTION('center_axis',(0.990949761747861,3.81699963904798E-34,
0.134233265965845));
#112529=DIRECTION('ref_axis',(0.134233265965845,5.17047732910431E-35,-0.990949761747861));
#112530=DIRECTION('center_axis',(-0.990949761747861,-3.81699963904798E-34,
-0.134233265965845));
#112531=DIRECTION('ref_axis',(3.85185988875507E-34,-1.,0.));
#112532=DIRECTION('center_axis',(0.998993066557948,3.84798132221898E-34,
0.0448648299801474));
#112533=DIRECTION('ref_axis',(-3.85185988875507E-34,1.,0.));
#112534=DIRECTION('center_axis',(0.998993066557948,3.84798132221898E-34,
0.0448648299801474));
#112535=DIRECTION('ref_axis',(0.0448648299801474,1.72813039016346E-35,-0.998993066557948));
#112536=DIRECTION('center_axis',(0.998993066557948,3.84798132221898E-34,
0.0448648299801474));
#112537=DIRECTION('ref_axis',(0.,1.,0.));
#112538=DIRECTION('center_axis',(0.998993066557948,3.84798132221898E-34,
0.0448648299801474));
#112539=DIRECTION('ref_axis',(0.0448648299801474,1.72813039016346E-35,-0.998993066557948));
#112540=DIRECTION('center_axis',(-0.998993066557948,-3.84798132221898E-34,
-0.0448648299801474));
#112541=DIRECTION('ref_axis',(3.85185988875507E-34,-1.,0.));
#112542=DIRECTION('center_axis',(0.998993066557948,3.84798132221898E-34,
-0.0448648299801474));
#112543=DIRECTION('ref_axis',(-3.85185988875507E-34,1.,0.));
#112544=DIRECTION('center_axis',(0.998993066557948,3.84798132221898E-34,
-0.0448648299801474));
#112545=DIRECTION('ref_axis',(-0.0448648299801474,-1.72813039016346E-35,
-0.998993066557948));
#112546=DIRECTION('center_axis',(0.998993066557948,3.84798132221898E-34,
-0.0448648299801474));
#112547=DIRECTION('ref_axis',(0.,1.,0.));
#112548=DIRECTION('center_axis',(0.998993066557948,3.84798132221898E-34,
-0.0448648299801474));
#112549=DIRECTION('ref_axis',(-0.0448648299801474,-1.72813039016346E-35,
-0.998993066557948));
#112550=DIRECTION('center_axis',(-0.998993066557948,-3.84798132221898E-34,
0.0448648299801474));
#112551=DIRECTION('ref_axis',(3.85185988875507E-34,-1.,0.));
#112552=DIRECTION('center_axis',(0.990949761747861,3.81699963904798E-34,
-0.134233265965845));
#112553=DIRECTION('ref_axis',(-3.85185988875507E-34,1.,0.));
#112554=DIRECTION('center_axis',(0.990949761747861,3.81699963904798E-34,
-0.134233265965845));
#112555=DIRECTION('ref_axis',(-0.134233265965845,-5.17047732910431E-35,
-0.990949761747861));
#112556=DIRECTION('center_axis',(0.990949761747861,3.81699963904798E-34,
-0.134233265965845));
#112557=DIRECTION('ref_axis',(0.,1.,0.));
#112558=DIRECTION('center_axis',(0.990949761747861,3.81699963904798E-34,
-0.134233265965845));
#112559=DIRECTION('ref_axis',(-0.134233265965845,-5.17047732910431E-35,
-0.990949761747861));
#112560=DIRECTION('center_axis',(-0.990949761747861,-3.81699963904798E-34,
0.134233265965845));
#112561=DIRECTION('ref_axis',(3.85185988875507E-34,-1.,0.));
#112562=DIRECTION('center_axis',(0.974927912163343,3.75528571928971E-34,
-0.222520934037282));
#112563=DIRECTION('ref_axis',(-3.85185988875507E-34,1.,0.));
#112564=DIRECTION('center_axis',(0.974927912163343,3.75528571928971E-34,
-0.222520934037282));
#112565=DIRECTION('ref_axis',(-0.222520934037282,-8.57119460226519E-35,
-0.974927912163343));
#112566=DIRECTION('center_axis',(0.974927912163343,3.75528571928971E-34,
-0.222520934037282));
#112567=DIRECTION('ref_axis',(0.,1.,0.));
#112568=DIRECTION('center_axis',(0.974927912163343,3.75528571928971E-34,
-0.222520934037282));
#112569=DIRECTION('ref_axis',(-0.222520934037282,-8.57119460226519E-35,
-0.974927912163343));
#112570=DIRECTION('center_axis',(-0.974927912163343,-3.75528571928971E-34,
0.222520934037282));
#112571=DIRECTION('ref_axis',(3.85185988875507E-34,-1.,0.));
#112572=DIRECTION('center_axis',(0.951056516377163,3.66333644737232E-34,
-0.309016994122548));
#112573=DIRECTION('ref_axis',(-3.85185988875507E-34,1.,0.));
#112574=DIRECTION('center_axis',(0.951056516377163,3.66333644737232E-34,
-0.309016994122548));
#112575=DIRECTION('ref_axis',(-0.309016994122548,-1.1902901646043E-34,-0.951056516377163));
#112576=DIRECTION('center_axis',(0.951056516377163,3.66333644737232E-34,
-0.309016994122548));
#112577=DIRECTION('ref_axis',(0.,1.,0.));
#112578=DIRECTION('center_axis',(0.951056516377163,3.66333644737232E-34,
-0.309016994122548));
#112579=DIRECTION('ref_axis',(-0.309016994122548,-1.1902901646043E-34,-0.951056516377163));
#112580=DIRECTION('center_axis',(-0.951056516377163,-3.66333644737232E-34,
0.309016994122548));
#112581=DIRECTION('ref_axis',(3.85185988875507E-34,-1.,0.));
#112582=DIRECTION('center_axis',(0.919527772341198,3.54189214287736E-34,
-0.393025032145835));
#112583=DIRECTION('ref_axis',(-3.85185988875507E-34,1.,0.));
#112584=DIRECTION('center_axis',(0.919527772341198,3.54189214287736E-34,
-0.393025032145835));
#112585=DIRECTION('ref_axis',(-0.393025032145835,-1.51387735659921E-34,
-0.919527772341198));
#112586=DIRECTION('center_axis',(0.919527772341198,3.54189214287736E-34,
-0.393025032145835));
#112587=DIRECTION('ref_axis',(0.,1.,0.));
#112588=DIRECTION('center_axis',(0.919527772341198,3.54189214287736E-34,
-0.393025032145835));
#112589=DIRECTION('ref_axis',(-0.393025032145835,-1.51387735659921E-34,
-0.919527772341198));
#112590=DIRECTION('center_axis',(-0.919527772341198,-3.54189214287736E-34,
0.393025032145835));
#112591=DIRECTION('ref_axis',(3.85185988875507E-34,-1.,0.));
#112592=DIRECTION('center_axis',(0.880595532086284,3.39193060826008E-34,
-0.473868662046431));
#112593=DIRECTION('ref_axis',(-3.85185988875507E-34,1.,0.));
#112594=DIRECTION('center_axis',(0.880595532086284,3.39193060826008E-34,
-0.473868662046431));
#112595=DIRECTION('ref_axis',(-0.473868662046431,-1.82527569187468E-34,
-0.880595532086284));
#112596=DIRECTION('center_axis',(0.880595532086284,3.39193060826008E-34,
-0.473868662046431));
#112597=DIRECTION('ref_axis',(0.,1.,0.));
#112598=DIRECTION('center_axis',(0.880595532086284,3.39193060826008E-34,
-0.473868662046431));
#112599=DIRECTION('ref_axis',(-0.473868662046431,-1.82527569187468E-34,
-0.880595532086284));
#112600=DIRECTION('center_axis',(-0.880595532086284,-3.39193060826008E-34,
0.473868662046431));
#112601=DIRECTION('ref_axis',(3.85185988875507E-34,-1.,0.));
#112602=DIRECTION('center_axis',(0.834573254013744,3.21465924136334E-34,
-0.550896981009072));
#112603=DIRECTION('ref_axis',(-3.85185988875507E-34,1.,0.));
#112604=DIRECTION('center_axis',(0.834573254013744,3.21465924136334E-34,
-0.550896981009072));
#112605=DIRECTION('ref_axis',(-0.550896981009072,-2.12197798398511E-34,
-0.834573254013744));
#112606=DIRECTION('center_axis',(0.834573254013744,3.21465924136334E-34,
-0.550896981009072));
#112607=DIRECTION('ref_axis',(0.,1.,0.));
#112608=DIRECTION('center_axis',(0.834573254013744,3.21465924136334E-34,
-0.550896981009072));
#112609=DIRECTION('ref_axis',(-0.550896981009072,-2.12197798398511E-34,
-0.834573254013744));
#112610=DIRECTION('center_axis',(-0.834573254013744,-3.21465924136334E-34,
0.550896981009072));
#112611=DIRECTION('ref_axis',(3.85185988875507E-34,-1.,0.));
#112612=DIRECTION('center_axis',(0.781831482217226,3.01150532611845E-34,
-0.623489802173232));
#112613=DIRECTION('ref_axis',(-3.85185988875507E-34,1.,0.));
#112614=DIRECTION('center_axis',(0.781831482217226,3.01150532611845E-34,
-0.623489802173232));
#112615=DIRECTION('ref_axis',(-0.623489802173232,-2.4015953600389E-34,-0.781831482217226));
#112616=DIRECTION('center_axis',(0.781831482217226,3.01150532611845E-34,
-0.623489802173232));
#112617=DIRECTION('ref_axis',(0.,1.,0.));
#112618=DIRECTION('center_axis',(0.781831482217226,3.01150532611845E-34,
-0.623489802173232));
#112619=DIRECTION('ref_axis',(-0.623489802173232,-2.4015953600389E-34,-0.781831482217226));
#112620=DIRECTION('center_axis',(-0.781831482217226,-3.01150532611845E-34,
0.623489802173232));
#112621=DIRECTION('ref_axis',(3.85185988875507E-34,-1.,0.));
#112622=DIRECTION('center_axis',(0.722794863903263,2.78410454406716E-34,
-0.69106264890751));
#112623=DIRECTION('ref_axis',(-3.85185988875507E-34,1.,0.));
#112624=DIRECTION('center_axis',(0.722794863903263,2.78410454406716E-34,
-0.69106264890751));
#112625=DIRECTION('ref_axis',(-0.69106264890751,-2.66187649794366E-34,-0.722794863903263));
#112626=DIRECTION('center_axis',(0.722794863903263,2.78410454406716E-34,
-0.69106264890751));
#112627=DIRECTION('ref_axis',(0.,1.,0.));
#112628=DIRECTION('center_axis',(0.722794863903263,2.78410454406716E-34,
-0.69106264890751));
#112629=DIRECTION('ref_axis',(-0.69106264890751,-2.66187649794366E-34,-0.722794863903263));
#112630=DIRECTION('center_axis',(-0.722794863903263,-2.78410454406716E-34,
0.69106264890751));
#112631=DIRECTION('ref_axis',(3.85185988875507E-34,-1.,0.));
#112632=DIRECTION('center_axis',(0.657938725975692,2.53428778784438E-34,
-0.753071465972177));
#112633=DIRECTION('ref_axis',(-3.85185988875507E-34,1.,0.));
#112634=DIRECTION('center_axis',(0.657938725975692,2.53428778784438E-34,
-0.753071465972177));
#112635=DIRECTION('ref_axis',(-0.753071465972177,-2.9007257731442E-34,-0.657938725975692));
#112636=DIRECTION('center_axis',(0.657938725975692,2.53428778784438E-34,
-0.753071465972177));
#112637=DIRECTION('ref_axis',(0.,1.,0.));
#112638=DIRECTION('center_axis',(0.657938725975692,2.53428778784438E-34,
-0.753071465972177));
#112639=DIRECTION('ref_axis',(-0.753071465972177,-2.9007257731442E-34,-0.657938725975692));
#112640=DIRECTION('center_axis',(-0.657938725975692,-2.53428778784438E-34,
0.753071465972177));
#112641=DIRECTION('ref_axis',(3.85185988875507E-34,-1.,0.));
#112642=DIRECTION('center_axis',(0.587785252279345,2.26406643645659E-34,
-0.809016994384486));
#112643=DIRECTION('ref_axis',(-3.85185988875507E-34,1.,0.));
#112644=DIRECTION('center_axis',(0.587785252279345,2.26406643645659E-34,
-0.809016994384486));
#112645=DIRECTION('ref_axis',(-0.809016994384486,-3.11622010999078E-34,
-0.587785252279345));
#112646=DIRECTION('center_axis',(0.587785252279345,2.26406643645659E-34,
-0.809016994384486));
#112647=DIRECTION('ref_axis',(0.,1.,0.));
#112648=DIRECTION('center_axis',(0.587785252279345,2.26406643645659E-34,
-0.809016994384486));
#112649=DIRECTION('ref_axis',(-0.809016994384486,-3.11622010999078E-34,
-0.587785252279345));
#112650=DIRECTION('center_axis',(-0.587785252279345,-2.26406643645659E-34,
0.809016994384486));
#112651=DIRECTION('ref_axis',(3.85185988875507E-34,-1.,0.));
#112652=DIRECTION('center_axis',(0.512899276931483,1.97561615178386E-34,
-0.858448793885321));
#112653=DIRECTION('ref_axis',(-3.85185988875507E-34,1.,0.));
#112654=DIRECTION('center_axis',(0.512899276931483,1.97561615178386E-34,
-0.858448793885321));
#112655=DIRECTION('ref_axis',(-0.858448793885321,-3.30662447571703E-34,
-0.512899276931483));
#112656=DIRECTION('center_axis',(0.512899276931483,1.97561615178386E-34,
-0.858448793885321));
#112657=DIRECTION('ref_axis',(0.,1.,0.));
#112658=DIRECTION('center_axis',(0.512899276931483,1.97561615178386E-34,
-0.858448793885321));
#112659=DIRECTION('ref_axis',(-0.858448793885321,-3.30662447571703E-34,
-0.512899276931483));
#112660=DIRECTION('center_axis',(-0.512899276931483,-1.97561615178386E-34,
0.858448793885321));
#112661=DIRECTION('ref_axis',(3.85185988875507E-34,-1.,0.));
#112662=DIRECTION('center_axis',(0.433883738983985,1.67125937057549E-34,
-0.900968867966745));
#112663=DIRECTION('ref_axis',(-3.85185988875507E-34,1.,0.));
#112664=DIRECTION('center_axis',(0.433883738983985,1.67125937057549E-34,
-0.900968867966745));
#112665=DIRECTION('ref_axis',(-0.900968867966744,-3.47040584353816E-34,
-0.433883738983985));
#112666=DIRECTION('center_axis',(0.433883738983985,1.67125937057549E-34,
-0.900968867966745));
#112667=DIRECTION('ref_axis',(0.,1.,0.));
#112668=DIRECTION('center_axis',(0.433883738983985,1.67125937057549E-34,
-0.900968867966745));
#112669=DIRECTION('ref_axis',(-0.900968867966744,-3.47040584353816E-34,
-0.433883738983985));
#112670=DIRECTION('center_axis',(-0.433883738983985,-1.67125937057549E-34,
0.900968867966745));
#112671=DIRECTION('ref_axis',(3.85185988875507E-34,-1.,0.));
#112672=DIRECTION('center_axis',(0.351374823891528,1.35344659006615E-34,
-0.936234870710976));
#112673=DIRECTION('ref_axis',(-3.85185988875507E-34,1.,0.));
#112674=DIRECTION('center_axis',(0.351374823891528,1.35344659006615E-34,
-0.936234870710976));
#112675=DIRECTION('ref_axis',(-0.936234870710976,-3.60624554494539E-34,
-0.351374823891528));
#112676=DIRECTION('center_axis',(0.351374823891528,1.35344659006615E-34,
-0.936234870710976));
#112677=DIRECTION('ref_axis',(0.,1.,0.));
#112678=DIRECTION('center_axis',(0.351374823891528,1.35344659006615E-34,
-0.936234870710976));
#112679=DIRECTION('ref_axis',(-0.936234870710976,-3.60624554494539E-34,
-0.351374823891528));
#112680=DIRECTION('center_axis',(-0.351374823891528,-1.35344659006615E-34,
0.936234870710976));
#112681=DIRECTION('ref_axis',(3.85185988875507E-34,-1.,0.));
#112682=DIRECTION('center_axis',(0.266036845891333,1.02473665561974E-34,
-0.963962860606254));
#112683=DIRECTION('ref_axis',(-3.85185988875507E-34,1.,0.));
#112684=DIRECTION('center_axis',(0.266036845891333,1.02473665561974E-34,
-0.963962860606254));
#112685=DIRECTION('ref_axis',(-0.963962860606253,-3.71304987701882E-34,
-0.266036845891333));
#112686=DIRECTION('center_axis',(0.266036845891333,1.02473665561974E-34,
-0.963962860606254));
#112687=DIRECTION('ref_axis',(0.,1.,0.));
#112688=DIRECTION('center_axis',(0.266036845891333,1.02473665561974E-34,
-0.963962860606254));
#112689=DIRECTION('ref_axis',(-0.963962860606253,-3.71304987701882E-34,
-0.266036845891333));
#112690=DIRECTION('center_axis',(-0.266036845891333,-1.02473665561974E-34,
0.963962860606254));
#112691=DIRECTION('ref_axis',(3.85185988875507E-34,-1.,0.));
#112692=DIRECTION('center_axis',(0.178556894923064,6.87776141414805E-35,
-0.98392958857605));
#112693=DIRECTION('ref_axis',(-3.85185988875507E-34,1.,0.));
#112694=DIRECTION('center_axis',(0.178556894923064,6.87776141414805E-35,
-0.98392958857605));
#112695=DIRECTION('ref_axis',(-0.983929588576049,-3.78995891559536E-34,
-0.178556894923064));
#112696=DIRECTION('center_axis',(0.178556894923064,6.87776141414805E-35,
-0.98392958857605));
#112697=DIRECTION('ref_axis',(0.,1.,0.));
#112698=DIRECTION('center_axis',(0.178556894923064,6.87776141414805E-35,
-0.98392958857605));
#112699=DIRECTION('ref_axis',(-0.983929588576049,-3.78995891559536E-34,
-0.178556894923064));
#112700=DIRECTION('center_axis',(-0.178556894923064,-6.87776141414805E-35,
0.98392958857605));
#112701=DIRECTION('ref_axis',(3.85185988875507E-34,-1.,0.));
#112702=DIRECTION('center_axis',(0.089639308998799,3.45278058788195E-35,
-0.995974293986656));
#112703=DIRECTION('ref_axis',(-3.85185988875507E-34,1.,0.));
#112704=DIRECTION('center_axis',(0.089639308998799,3.45278058788195E-35,
-0.995974293986656));
#112705=DIRECTION('ref_axis',(-0.995974293986656,-3.83635343323835E-34,
-0.089639308998799));
#112706=DIRECTION('center_axis',(0.089639308998799,3.45278058788195E-35,
-0.995974293986656));
#112707=DIRECTION('ref_axis',(0.,1.,0.));
#112708=DIRECTION('center_axis',(0.089639308998799,3.45278058788195E-35,
-0.995974293986656));
#112709=DIRECTION('ref_axis',(-0.995974293986656,-3.83635343323835E-34,
-0.089639308998799));
#112710=DIRECTION('center_axis',(-0.089639308998799,-3.45278058788195E-35,
0.995974293986656));
#112711=DIRECTION('ref_axis',(3.85185988875507E-34,-1.,0.));
#112712=DIRECTION('center_axis',(-3.85185988875507E-34,1.,0.));
#112713=DIRECTION('ref_axis',(1.,3.85185988875507E-34,0.));
#112714=DIRECTION('center_axis',(-3.85185988875507E-34,1.,0.));
#112715=DIRECTION('ref_axis',(0.,0.,1.));
#112716=DIRECTION('',(-3.85185988875507E-34,1.,0.));
#112717=DIRECTION('center_axis',(-3.85185988875507E-34,1.,0.));
#112718=DIRECTION('ref_axis',(0.,0.,1.));
#112719=DIRECTION('center_axis',(-3.85185988875507E-34,1.,0.));
#112720=DIRECTION('ref_axis',(1.,3.85185988875507E-34,0.));
#112721=DIRECTION('center_axis',(-3.85185988875507E-34,1.,0.));
#112722=DIRECTION('ref_axis',(0.,0.,1.));
#112723=DIRECTION('',(-3.85185988875507E-34,1.,0.));
#112724=DIRECTION('center_axis',(-3.85185988875507E-34,1.,0.));
#112725=DIRECTION('ref_axis',(0.,0.,1.));
#112726=DIRECTION('center_axis',(-3.85185988875507E-34,1.,0.));
#112727=DIRECTION('ref_axis',(1.,0.,0.));
#112728=DIRECTION('center_axis',(-3.85185988875507E-34,1.,0.));
#112729=DIRECTION('ref_axis',(0.,0.,1.));
#112730=DIRECTION('center_axis',(-1.22464679914735E-16,-4.71716788352798E-50,
-1.));
#112731=DIRECTION('ref_axis',(-1.,0.,1.22464679914735E-16));
#112732=DIRECTION('center_axis',(3.85185988875507E-34,-1.,0.));
#112733=DIRECTION('ref_axis',(0.,0.,1.));
#112734=DIRECTION('center_axis',(-3.85185988875507E-34,1.,0.));
#112735=DIRECTION('ref_axis',(1.,0.,0.));
#112736=DIRECTION('center_axis',(-3.85185988875507E-34,1.,0.));
#112737=DIRECTION('ref_axis',(0.,0.,1.));
#112738=DIRECTION('center_axis',(-1.22464679914735E-16,-4.71716788352798E-50,
-1.));
#112739=DIRECTION('ref_axis',(-1.,0.,1.22464679914735E-16));
#112740=DIRECTION('center_axis',(3.85185988875507E-34,-1.,0.));
#112741=DIRECTION('ref_axis',(0.,0.,1.));
#112742=DIRECTION('center_axis',(3.85185988875507E-34,-1.,0.));
#112743=DIRECTION('ref_axis',(-1.,0.,0.));
#112744=DIRECTION('center_axis',(3.85185988875507E-34,-1.,0.));
#112745=DIRECTION('ref_axis',(0.,0.,1.));
#112746=DIRECTION('center_axis',(-1.22464679914735E-16,-4.71716788352798E-50,
1.));
#112747=DIRECTION('ref_axis',(1.,0.,1.22464679914735E-16));
#112748=DIRECTION('center_axis',(-3.85185988875507E-34,1.,0.));
#112749=DIRECTION('ref_axis',(0.,0.,-1.));
#112750=DIRECTION('center_axis',(3.85185988875507E-34,-1.,0.));
#112751=DIRECTION('ref_axis',(0.,0.,1.));
#112752=DIRECTION('center_axis',(-3.85185988875507E-34,1.,0.));
#112753=DIRECTION('ref_axis',(1.,0.,0.));
#112754=DIRECTION('center_axis',(-3.85185988875507E-34,1.,0.));
#112755=DIRECTION('ref_axis',(0.,0.,1.));
#112756=DIRECTION('center_axis',(1.22464679914735E-16,4.71716788352798E-50,
1.));
#112757=DIRECTION('ref_axis',(-1.,0.,1.22464679914735E-16));
#112758=DIRECTION('center_axis',(3.85185988875507E-34,-1.,0.));
#112759=DIRECTION('ref_axis',(0.,0.,1.));
#112760=DIRECTION('center_axis',(-3.85185988875507E-34,1.,0.));
#112761=DIRECTION('ref_axis',(1.,0.,0.));
#112762=DIRECTION('center_axis',(-3.85185988875507E-34,1.,0.));
#112763=DIRECTION('ref_axis',(0.,0.,1.));
#112764=DIRECTION('center_axis',(1.22464679914735E-16,4.71716788352798E-50,
1.));
#112765=DIRECTION('ref_axis',(-1.,0.,1.22464679914735E-16));
#112766=DIRECTION('center_axis',(3.85185988875507E-34,-1.,0.));
#112767=DIRECTION('ref_axis',(0.,0.,-1.));
#112768=DIRECTION('center_axis',(3.85185988875507E-34,-1.,0.));
#112769=DIRECTION('ref_axis',(0.,0.,-1.));
#112770=DIRECTION('center_axis',(-3.85185988875507E-34,1.,0.));
#112771=DIRECTION('ref_axis',(1.,0.,0.));
#112772=DIRECTION('center_axis',(3.85185988875507E-34,-1.,0.));
#112773=DIRECTION('ref_axis',(0.,0.,-1.));
#112774=DIRECTION('center_axis',(0.942809041733257,3.63156833060794E-34,
0.333333332905692));
#112775=DIRECTION('ref_axis',(0.333333332905692,1.28395329460448E-34,-0.942809041733257));
#112776=DIRECTION('center_axis',(-3.85185988875507E-34,1.,0.));
#112777=DIRECTION('ref_axis',(0.,0.,1.));
#112778=DIRECTION('center_axis',(-0.388215488117679,-1.49535166687396E-34,
0.921568627279354));
#112779=DIRECTION('ref_axis',(0.921568627279354,3.54975323015241E-34,0.388215488117679));
#112780=DIRECTION('center_axis',(-3.85185988875507E-34,1.,0.));
#112781=DIRECTION('ref_axis',(1.,0.,0.));
#112782=DIRECTION('center_axis',(3.85185988875507E-34,-1.,0.));
#112783=DIRECTION('ref_axis',(0.,0.,-1.));
#112784=DIRECTION('center_axis',(0.388215488966968,1.4953516701453E-34,
0.921568626921586));
#112785=DIRECTION('ref_axis',(0.921568626921586,3.54975322877434E-34,-0.388215488966968));
#112786=DIRECTION('center_axis',(-3.85185988875507E-34,1.,0.));
#112787=DIRECTION('ref_axis',(0.,0.,1.));
#112788=DIRECTION('center_axis',(-0.942809041733257,-3.63156833060794E-34,
0.333333332905692));
#112789=DIRECTION('ref_axis',(0.333333332905692,1.28395329460448E-34,0.942809041733257));
#112790=DIRECTION('center_axis',(-3.85185988875507E-34,1.,0.));
#112791=DIRECTION('ref_axis',(1.,0.,0.));
#112792=DIRECTION('center_axis',(-3.85185988875507E-34,1.,0.));
#112793=DIRECTION('ref_axis',(0.,0.,1.));
#112794=DIRECTION('center_axis',(1.22464679914735E-16,4.71716788352797E-50,
1.));
#112795=DIRECTION('ref_axis',(-1.,0.,1.22464679914735E-16));
#112796=DIRECTION('center_axis',(3.85185988875507E-34,-1.,0.));
#112797=DIRECTION('ref_axis',(0.,0.,-1.));
#112798=DIRECTION('center_axis',(3.85185988875507E-34,-1.,0.));
#112799=DIRECTION('ref_axis',(0.,0.,-1.));
#112800=DIRECTION('center_axis',(3.85185988875507E-34,-1.,0.));
#112801=DIRECTION('ref_axis',(-1.,0.,0.));
#112802=DIRECTION('center_axis',(3.85185988875507E-34,-1.,0.));
#112803=DIRECTION('ref_axis',(0.,0.,-1.));
#112804=DIRECTION('center_axis',(-1.22464679914735E-16,-4.71716788352797E-50,
1.));
#112805=DIRECTION('ref_axis',(1.,0.,1.22464679914735E-16));
#112806=DIRECTION('center_axis',(-3.85185988875507E-34,1.,0.));
#112807=DIRECTION('ref_axis',(0.,0.,1.));
#112808=DIRECTION('center_axis',(-3.85185988875507E-34,1.,0.));
#112809=DIRECTION('ref_axis',(0.,0.,1.));
#112810=DIRECTION('center_axis',(3.85185988875507E-34,-1.,0.));
#112811=DIRECTION('ref_axis',(-1.,0.,0.));
#112812=DIRECTION('center_axis',(3.85185988875507E-34,-1.,0.));
#112813=DIRECTION('ref_axis',(0.,0.,-1.));
#112814=DIRECTION('center_axis',(-1.22464679914735E-16,-4.71716788352797E-50,
1.));
#112815=DIRECTION('ref_axis',(1.,0.,1.22464679914735E-16));
#112816=DIRECTION('center_axis',(-3.85185988875507E-34,1.,0.));
#112817=DIRECTION('ref_axis',(0.,0.,1.));
#112818=DIRECTION('center_axis',(-3.85185988875507E-34,1.,0.));
#112819=DIRECTION('ref_axis',(0.,0.,1.));
#112820=DIRECTION('center_axis',(3.85185988875507E-34,-1.,0.));
#112821=DIRECTION('ref_axis',(-1.,-3.85185988875507E-34,0.));
#112822=DIRECTION('center_axis',(3.85185988875507E-34,-1.,0.));
#112823=DIRECTION('ref_axis',(0.,0.,-1.));
#112824=DIRECTION('',(3.85185988875507E-34,-1.,0.));
#112825=DIRECTION('center_axis',(-3.85185988875507E-34,1.,0.));
#112826=DIRECTION('ref_axis',(0.,0.,-1.));
#112827=DIRECTION('',(3.85185988875507E-34,-1.,0.));
#112828=DIRECTION('center_axis',(3.85185988875507E-34,-1.,0.));
#112829=DIRECTION('ref_axis',(-1.,-3.85185988875507E-34,0.));
#112830=DIRECTION('center_axis',(3.85185988875507E-34,-1.,0.));
#112831=DIRECTION('ref_axis',(0.,0.,-1.));
#112832=DIRECTION('',(3.85185988875507E-34,-1.,0.));
#112833=DIRECTION('center_axis',(-3.85185988875507E-34,1.,0.));
#112834=DIRECTION('ref_axis',(0.,0.,-1.));
#112835=DIRECTION('',(3.85185988875507E-34,-1.,0.));
#112836=DIRECTION('center_axis',(3.85185988875507E-34,-1.,0.));
#112837=DIRECTION('ref_axis',(-1.,-3.85185988875507E-34,0.));
#112838=DIRECTION('center_axis',(3.85185988875507E-34,-1.,0.));
#112839=DIRECTION('ref_axis',(0.,0.,-1.));
#112840=DIRECTION('',(3.85185988875507E-34,-1.,0.));
#112841=DIRECTION('center_axis',(-3.85185988875507E-34,1.,0.));
#112842=DIRECTION('ref_axis',(1.,3.85185988875507E-34,0.));
#112843=DIRECTION('',(3.85185988875507E-34,-1.,0.));
#112844=DIRECTION('center_axis',(-3.85185988875507E-34,1.,0.));
#112845=DIRECTION('ref_axis',(1.,3.85185988875507E-34,0.));
#112846=DIRECTION('',(3.85185988875507E-34,-1.,0.));
#112847=DIRECTION('center_axis',(3.85185988875507E-34,-1.,0.));
#112848=DIRECTION('ref_axis',(-1.,-3.85185988875507E-34,0.));
#112849=DIRECTION('center_axis',(-3.85185988875507E-34,1.,0.));
#112850=DIRECTION('ref_axis',(0.,0.,-1.));
#112851=DIRECTION('',(-3.85185988875507E-34,1.,0.));
#112852=DIRECTION('center_axis',(-3.85185988875507E-34,1.,0.));
#112853=DIRECTION('ref_axis',(1.,3.85185988875507E-34,0.));
#112854=DIRECTION('center_axis',(-3.85185988875507E-34,1.,0.));
#112855=DIRECTION('ref_axis',(0.,0.,1.));
#112856=DIRECTION('',(-3.85185988875507E-34,1.,0.));
#112857=DIRECTION('center_axis',(-3.85185988875507E-34,1.,0.));
#112858=DIRECTION('ref_axis',(0.,0.,1.));
#112859=DIRECTION('',(-3.85185988875507E-34,1.,0.));
#112860=DIRECTION('center_axis',(-3.85185988875507E-34,1.,0.));
#112861=DIRECTION('ref_axis',(1.,3.85185988875507E-34,0.));
#112862=DIRECTION('center_axis',(-3.85185988875507E-34,1.,0.));
#112863=DIRECTION('ref_axis',(0.,0.,1.));
#112864=DIRECTION('',(-3.85185988875507E-34,1.,0.));
#112865=DIRECTION('center_axis',(-3.85185988875507E-34,1.,0.));
#112866=DIRECTION('ref_axis',(0.,0.,1.));
#112867=DIRECTION('',(-3.85185988875507E-34,1.,0.));
#112868=DIRECTION('center_axis',(-3.85185988875507E-34,1.,0.));
#112869=DIRECTION('ref_axis',(1.,3.85185988875507E-34,0.));
#112870=DIRECTION('center_axis',(-3.85185988875507E-34,1.,0.));
#112871=DIRECTION('ref_axis',(0.,0.,1.));
#112872=DIRECTION('',(-3.85185988875507E-34,1.,0.));
#112873=DIRECTION('center_axis',(3.85185988875507E-34,-1.,0.));
#112874=DIRECTION('ref_axis',(0.,0.,1.));
#112875=DIRECTION('',(3.85185988875507E-34,-1.,0.));
#112876=DIRECTION('center_axis',(-3.85185988875507E-34,1.,0.));
#112877=DIRECTION('ref_axis',(1.,3.85185988875507E-34,0.));
#112878=DIRECTION('center_axis',(-3.85185988875507E-34,1.,0.));
#112879=DIRECTION('ref_axis',(0.,0.,1.));
#112880=DIRECTION('',(-3.85185988875507E-34,1.,0.));
#112881=DIRECTION('center_axis',(3.85185988875507E-34,-1.,0.));
#112882=DIRECTION('ref_axis',(0.,0.,1.));
#112883=DIRECTION('',(3.85185988875507E-34,-1.,0.));
#112884=DIRECTION('center_axis',(-3.85185988875507E-34,1.,0.));
#112885=DIRECTION('ref_axis',(1.,3.85185988875507E-34,0.));
#112886=DIRECTION('',(-3.85185988875507E-34,1.,0.));
#112887=DIRECTION('center_axis',(-3.85185988875507E-34,1.,0.));
#112888=DIRECTION('ref_axis',(1.,3.85185988875507E-34,0.));
#112889=DIRECTION('center_axis',(-3.85185988875507E-34,1.,0.));
#112890=DIRECTION('ref_axis',(0.,0.,1.));
#112891=DIRECTION('center_axis',(-3.85185988875507E-34,1.,0.));
#112892=DIRECTION('ref_axis',(0.,0.,1.));
#112893=DIRECTION('center_axis',(-3.85185988875507E-34,1.,0.));
#112894=DIRECTION('ref_axis',(0.,0.,1.));
#112895=DIRECTION('center_axis',(-3.85185988875507E-34,1.,0.));
#112896=DIRECTION('ref_axis',(0.,0.,1.));
#112897=DIRECTION('center_axis',(-3.85185988875507E-34,1.,0.));
#112898=DIRECTION('ref_axis',(0.,0.,1.));
#112899=DIRECTION('center_axis',(-3.85185988875507E-34,1.,0.));
#112900=DIRECTION('ref_axis',(0.,0.,1.));
#112901=DIRECTION('center_axis',(-3.85185988875507E-34,1.,0.));
#112902=DIRECTION('ref_axis',(0.,0.,1.));
#112903=DIRECTION('center_axis',(-3.85185988875507E-34,1.,0.));
#112904=DIRECTION('ref_axis',(0.,0.,1.));
#112905=DIRECTION('center_axis',(-3.85185988875507E-34,1.,0.));
#112906=DIRECTION('ref_axis',(0.,0.,1.));
#112907=DIRECTION('center_axis',(-3.85185988875507E-34,1.,0.));
#112908=DIRECTION('ref_axis',(0.,0.,1.));
#112909=DIRECTION('center_axis',(-3.85185988875507E-34,1.,0.));
#112910=DIRECTION('ref_axis',(0.,0.,1.));
#112911=DIRECTION('center_axis',(-3.85185988875507E-34,1.,0.));
#112912=DIRECTION('ref_axis',(0.,0.,1.));
#112913=DIRECTION('center_axis',(-3.85185988875507E-34,1.,0.));
#112914=DIRECTION('ref_axis',(0.,0.,1.));
#112915=DIRECTION('center_axis',(-3.85185988875507E-34,1.,0.));
#112916=DIRECTION('ref_axis',(0.,0.,1.));
#112917=DIRECTION('center_axis',(-3.85185988875507E-34,1.,0.));
#112918=DIRECTION('ref_axis',(0.,0.,1.));
#112919=DIRECTION('center_axis',(-3.85185988875507E-34,1.,0.));
#112920=DIRECTION('ref_axis',(0.,0.,1.));
#112921=DIRECTION('center_axis',(-3.85185988875507E-34,1.,0.));
#112922=DIRECTION('ref_axis',(0.,0.,1.));
#112923=DIRECTION('center_axis',(-3.85185988875507E-34,1.,0.));
#112924=DIRECTION('ref_axis',(0.,0.,1.));
#112925=DIRECTION('center_axis',(-3.85185988875507E-34,1.,0.));
#112926=DIRECTION('ref_axis',(0.,0.,1.));
#112927=DIRECTION('center_axis',(-3.85185988875507E-34,1.,0.));
#112928=DIRECTION('ref_axis',(0.,0.,1.));
#112929=DIRECTION('center_axis',(-3.85185988875507E-34,1.,0.));
#112930=DIRECTION('ref_axis',(0.,0.,1.));
#112931=DIRECTION('center_axis',(-3.85185988875507E-34,1.,0.));
#112932=DIRECTION('ref_axis',(0.,0.,1.));
#112933=DIRECTION('center_axis',(-3.85185988875507E-34,1.,0.));
#112934=DIRECTION('ref_axis',(0.,0.,1.));
#112935=DIRECTION('center_axis',(-3.85185988875507E-34,1.,0.));
#112936=DIRECTION('ref_axis',(0.,0.,1.));
#112937=DIRECTION('center_axis',(-3.85185988875507E-34,1.,0.));
#112938=DIRECTION('ref_axis',(0.,0.,1.));
#112939=DIRECTION('center_axis',(-3.85185988875507E-34,1.,0.));
#112940=DIRECTION('ref_axis',(0.,0.,1.));
#112941=DIRECTION('center_axis',(-3.85185988875507E-34,1.,0.));
#112942=DIRECTION('ref_axis',(0.,0.,1.));
#112943=DIRECTION('center_axis',(-3.85185988875507E-34,1.,0.));
#112944=DIRECTION('ref_axis',(0.,0.,1.));
#112945=DIRECTION('center_axis',(-3.85185988875507E-34,1.,0.));
#112946=DIRECTION('ref_axis',(0.,0.,1.));
#112947=DIRECTION('center_axis',(-3.85185988875507E-34,1.,0.));
#112948=DIRECTION('ref_axis',(0.,0.,1.));
#112949=DIRECTION('center_axis',(-3.85185988875507E-34,1.,0.));
#112950=DIRECTION('ref_axis',(0.,0.,1.));
#112951=DIRECTION('center_axis',(-3.85185988875507E-34,1.,0.));
#112952=DIRECTION('ref_axis',(0.,0.,1.));
#112953=DIRECTION('center_axis',(-3.85185988875507E-34,1.,0.));
#112954=DIRECTION('ref_axis',(0.,0.,1.));
#112955=DIRECTION('center_axis',(-3.85185988875507E-34,1.,0.));
#112956=DIRECTION('ref_axis',(0.,0.,1.));
#112957=DIRECTION('center_axis',(-3.85185988875507E-34,1.,0.));
#112958=DIRECTION('ref_axis',(0.,0.,1.));
#112959=DIRECTION('center_axis',(-3.85185988875507E-34,1.,0.));
#112960=DIRECTION('ref_axis',(0.,0.,1.));
#112961=DIRECTION('center_axis',(-3.85185988875507E-34,1.,0.));
#112962=DIRECTION('ref_axis',(0.,0.,1.));
#112963=DIRECTION('center_axis',(-3.85185988875507E-34,1.,0.));
#112964=DIRECTION('ref_axis',(0.,0.,1.));
#112965=DIRECTION('center_axis',(-3.85185988875507E-34,1.,0.));
#112966=DIRECTION('ref_axis',(0.,0.,1.));
#112967=DIRECTION('center_axis',(-3.85185988875507E-34,1.,0.));
#112968=DIRECTION('ref_axis',(0.,0.,1.));
#112969=DIRECTION('center_axis',(-3.85185988875507E-34,1.,0.));
#112970=DIRECTION('ref_axis',(0.,0.,1.));
#112971=DIRECTION('center_axis',(-3.85185988875507E-34,1.,0.));
#112972=DIRECTION('ref_axis',(0.,0.,1.));
#112973=DIRECTION('center_axis',(-3.85185988875507E-34,1.,0.));
#112974=DIRECTION('ref_axis',(0.,0.,1.));
#112975=DIRECTION('center_axis',(-3.85185988875507E-34,1.,0.));
#112976=DIRECTION('ref_axis',(0.,0.,1.));
#112977=DIRECTION('center_axis',(-3.85185988875507E-34,1.,0.));
#112978=DIRECTION('ref_axis',(0.,0.,1.));
#112979=DIRECTION('center_axis',(-3.85185988875507E-34,1.,0.));
#112980=DIRECTION('ref_axis',(0.,0.,1.));
#112981=DIRECTION('center_axis',(-3.85185988875507E-34,1.,0.));
#112982=DIRECTION('ref_axis',(0.,0.,1.));
#112983=DIRECTION('center_axis',(-3.85185988875507E-34,1.,0.));
#112984=DIRECTION('ref_axis',(0.,0.,1.));
#112985=DIRECTION('center_axis',(-3.85185988875507E-34,1.,0.));
#112986=DIRECTION('ref_axis',(0.,0.,1.));
#112987=DIRECTION('center_axis',(-3.85185988875507E-34,1.,0.));
#112988=DIRECTION('ref_axis',(0.,0.,1.));
#112989=DIRECTION('center_axis',(-3.85185988875507E-34,1.,0.));
#112990=DIRECTION('ref_axis',(0.,0.,1.));
#112991=DIRECTION('center_axis',(-3.85185988875507E-34,1.,0.));
#112992=DIRECTION('ref_axis',(0.,0.,1.));
#112993=DIRECTION('center_axis',(-3.85185988875507E-34,1.,0.));
#112994=DIRECTION('ref_axis',(0.,0.,1.));
#112995=DIRECTION('center_axis',(-3.85185988875507E-34,1.,0.));
#112996=DIRECTION('ref_axis',(0.,0.,1.));
#112997=DIRECTION('center_axis',(-3.85185988875507E-34,1.,0.));
#112998=DIRECTION('ref_axis',(0.,0.,1.));
#112999=DIRECTION('center_axis',(-3.85185988875507E-34,1.,0.));
#113000=DIRECTION('ref_axis',(0.,0.,1.));
#113001=DIRECTION('center_axis',(-3.85185988875507E-34,1.,0.));
#113002=DIRECTION('ref_axis',(0.,0.,1.));
#113003=DIRECTION('center_axis',(-3.85185988875507E-34,1.,0.));
#113004=DIRECTION('ref_axis',(0.,0.,1.));
#113005=DIRECTION('center_axis',(-3.85185988875507E-34,1.,0.));
#113006=DIRECTION('ref_axis',(0.,0.,1.));
#113007=DIRECTION('center_axis',(-3.85185988875507E-34,1.,0.));
#113008=DIRECTION('ref_axis',(0.,0.,1.));
#113009=DIRECTION('center_axis',(-3.85185988875507E-34,1.,0.));
#113010=DIRECTION('ref_axis',(0.,0.,1.));
#113011=DIRECTION('center_axis',(-3.85185988875507E-34,1.,0.));
#113012=DIRECTION('ref_axis',(0.,0.,1.));
#113013=DIRECTION('center_axis',(-3.85185988875507E-34,1.,0.));
#113014=DIRECTION('ref_axis',(0.,0.,1.));
#113015=DIRECTION('center_axis',(-3.85185988875507E-34,1.,0.));
#113016=DIRECTION('ref_axis',(0.,0.,1.));
#113017=DIRECTION('center_axis',(-3.85185988875507E-34,1.,0.));
#113018=DIRECTION('ref_axis',(0.,0.,1.));
#113019=DIRECTION('center_axis',(-3.85185988875507E-34,1.,0.));
#113020=DIRECTION('ref_axis',(0.,0.,1.));
#113021=DIRECTION('center_axis',(-3.85185988875507E-34,1.,0.));
#113022=DIRECTION('ref_axis',(0.,0.,1.));
#113023=DIRECTION('center_axis',(-3.85185988875507E-34,1.,0.));
#113024=DIRECTION('ref_axis',(0.,0.,1.));
#113025=DIRECTION('center_axis',(-3.85185988875507E-34,1.,0.));
#113026=DIRECTION('ref_axis',(0.,0.,1.));
#113027=DIRECTION('center_axis',(-3.85185988875507E-34,1.,0.));
#113028=DIRECTION('ref_axis',(0.,0.,1.));
#113029=DIRECTION('center_axis',(-3.85185988875507E-34,1.,0.));
#113030=DIRECTION('ref_axis',(0.,0.,1.));
#113031=DIRECTION('center_axis',(-3.85185988875507E-34,1.,0.));
#113032=DIRECTION('ref_axis',(0.,0.,1.));
#113033=DIRECTION('center_axis',(-3.85185988875507E-34,1.,0.));
#113034=DIRECTION('ref_axis',(0.,0.,1.));
#113035=DIRECTION('center_axis',(-3.85185988875507E-34,1.,0.));
#113036=DIRECTION('ref_axis',(0.,0.,1.));
#113037=DIRECTION('center_axis',(-3.85185988875507E-34,1.,0.));
#113038=DIRECTION('ref_axis',(0.,0.,1.));
#113039=DIRECTION('center_axis',(-3.85185988875507E-34,1.,0.));
#113040=DIRECTION('ref_axis',(0.,0.,1.));
#113041=DIRECTION('center_axis',(-3.85185988875507E-34,1.,0.));
#113042=DIRECTION('ref_axis',(0.,0.,1.));
#113043=DIRECTION('center_axis',(-3.85185988875507E-34,1.,0.));
#113044=DIRECTION('ref_axis',(0.,0.,1.));
#113045=DIRECTION('center_axis',(-3.85185988875507E-34,1.,0.));
#113046=DIRECTION('ref_axis',(0.,0.,1.));
#113047=DIRECTION('center_axis',(-3.85185988875507E-34,1.,0.));
#113048=DIRECTION('ref_axis',(0.,0.,1.));
#113049=DIRECTION('center_axis',(-3.85185988875507E-34,1.,0.));
#113050=DIRECTION('ref_axis',(0.,0.,1.));
#113051=DIRECTION('center_axis',(-3.85185988875507E-34,1.,0.));
#113052=DIRECTION('ref_axis',(0.,0.,1.));
#113053=DIRECTION('center_axis',(-3.85185988875507E-34,1.,0.));
#113054=DIRECTION('ref_axis',(0.,0.,1.));
#113055=DIRECTION('center_axis',(-3.85185988875507E-34,1.,0.));
#113056=DIRECTION('ref_axis',(0.,0.,1.));
#113057=DIRECTION('center_axis',(-3.85185988875507E-34,1.,0.));
#113058=DIRECTION('ref_axis',(0.,0.,1.));
#113059=DIRECTION('center_axis',(-3.85185988875507E-34,1.,0.));
#113060=DIRECTION('ref_axis',(0.,0.,1.));
#113061=DIRECTION('center_axis',(-3.85185988875507E-34,1.,0.));
#113062=DIRECTION('ref_axis',(0.,0.,1.));
#113063=DIRECTION('center_axis',(-3.85185988875507E-34,1.,0.));
#113064=DIRECTION('ref_axis',(0.,0.,1.));
#113065=DIRECTION('center_axis',(-3.85185988875507E-34,1.,0.));
#113066=DIRECTION('ref_axis',(0.,0.,1.));
#113067=DIRECTION('center_axis',(-3.85185988875507E-34,1.,0.));
#113068=DIRECTION('ref_axis',(0.,0.,1.));
#113069=DIRECTION('center_axis',(-3.85185988875507E-34,1.,0.));
#113070=DIRECTION('ref_axis',(0.,0.,1.));
#113071=DIRECTION('center_axis',(-3.85185988875507E-34,1.,0.));
#113072=DIRECTION('ref_axis',(0.,0.,1.));
#113073=DIRECTION('center_axis',(-3.85185988875507E-34,1.,0.));
#113074=DIRECTION('ref_axis',(0.,0.,1.));
#113075=DIRECTION('center_axis',(-3.85185988875507E-34,1.,0.));
#113076=DIRECTION('ref_axis',(0.,0.,1.));
#113077=DIRECTION('center_axis',(-3.85185988875507E-34,1.,0.));
#113078=DIRECTION('ref_axis',(0.,0.,1.));
#113079=DIRECTION('center_axis',(-3.85185988875507E-34,1.,0.));
#113080=DIRECTION('ref_axis',(0.,0.,1.));
#113081=DIRECTION('center_axis',(-3.85185988875507E-34,1.,0.));
#113082=DIRECTION('ref_axis',(0.,0.,1.));
#113083=DIRECTION('center_axis',(-3.85185988875507E-34,1.,0.));
#113084=DIRECTION('ref_axis',(0.,0.,1.));
#113085=DIRECTION('center_axis',(-3.85185988875507E-34,1.,0.));
#113086=DIRECTION('ref_axis',(0.,0.,1.));
#113087=DIRECTION('center_axis',(-3.85185988875507E-34,1.,0.));
#113088=DIRECTION('ref_axis',(0.,0.,1.));
#113089=DIRECTION('center_axis',(-3.85185988875507E-34,1.,0.));
#113090=DIRECTION('ref_axis',(0.,0.,1.));
#113091=DIRECTION('center_axis',(-3.85185988875507E-34,1.,0.));
#113092=DIRECTION('ref_axis',(0.,0.,1.));
#113093=DIRECTION('center_axis',(-3.85185988875507E-34,1.,0.));
#113094=DIRECTION('ref_axis',(0.,0.,1.));
#113095=DIRECTION('center_axis',(-3.85185988875507E-34,1.,0.));
#113096=DIRECTION('ref_axis',(0.,0.,1.));
#113097=DIRECTION('center_axis',(-3.85185988875507E-34,1.,0.));
#113098=DIRECTION('ref_axis',(0.,0.,1.));
#113099=DIRECTION('center_axis',(-3.85185988875507E-34,1.,0.));
#113100=DIRECTION('ref_axis',(0.,0.,1.));
#113101=DIRECTION('center_axis',(-3.85185988875507E-34,1.,0.));
#113102=DIRECTION('ref_axis',(0.,0.,1.));
#113103=DIRECTION('center_axis',(-3.85185988875507E-34,1.,0.));
#113104=DIRECTION('ref_axis',(0.,0.,1.));
#113105=DIRECTION('center_axis',(-3.85185988875507E-34,1.,0.));
#113106=DIRECTION('ref_axis',(0.,0.,1.));
#113107=DIRECTION('center_axis',(-3.85185988875507E-34,1.,0.));
#113108=DIRECTION('ref_axis',(0.,0.,1.));
#113109=DIRECTION('center_axis',(-3.85185988875507E-34,1.,0.));
#113110=DIRECTION('ref_axis',(0.,0.,1.));
#113111=DIRECTION('center_axis',(-3.85185988875507E-34,1.,0.));
#113112=DIRECTION('ref_axis',(0.,0.,1.));
#113113=DIRECTION('center_axis',(-3.85185988875507E-34,1.,0.));
#113114=DIRECTION('ref_axis',(0.,0.,1.));
#113115=DIRECTION('center_axis',(-3.85185988875507E-34,1.,0.));
#113116=DIRECTION('ref_axis',(0.,0.,1.));
#113117=DIRECTION('center_axis',(-3.85185988875507E-34,1.,0.));
#113118=DIRECTION('ref_axis',(0.,0.,1.));
#113119=DIRECTION('center_axis',(-3.85185988875507E-34,1.,0.));
#113120=DIRECTION('ref_axis',(0.,0.,1.));
#113121=DIRECTION('center_axis',(-3.85185988875507E-34,1.,0.));
#113122=DIRECTION('ref_axis',(0.,0.,1.));
#113123=DIRECTION('center_axis',(-3.85185988875507E-34,1.,0.));
#113124=DIRECTION('ref_axis',(0.,0.,1.));
#113125=DIRECTION('center_axis',(-3.85185988875507E-34,1.,0.));
#113126=DIRECTION('ref_axis',(0.,0.,1.));
#113127=DIRECTION('center_axis',(-3.85185988875507E-34,1.,0.));
#113128=DIRECTION('ref_axis',(0.,0.,1.));
#113129=DIRECTION('center_axis',(-3.85185988875507E-34,1.,0.));
#113130=DIRECTION('ref_axis',(0.,0.,1.));
#113131=DIRECTION('center_axis',(-3.85185988875507E-34,1.,0.));
#113132=DIRECTION('ref_axis',(0.,0.,1.));
#113133=DIRECTION('center_axis',(-3.85185988875507E-34,1.,0.));
#113134=DIRECTION('ref_axis',(0.,0.,1.));
#113135=DIRECTION('center_axis',(-3.85185988875507E-34,1.,0.));
#113136=DIRECTION('ref_axis',(0.,0.,1.));
#113137=DIRECTION('center_axis',(-3.85185988875507E-34,1.,0.));
#113138=DIRECTION('ref_axis',(0.,0.,1.));
#113139=DIRECTION('center_axis',(-3.85185988875507E-34,1.,0.));
#113140=DIRECTION('ref_axis',(0.,0.,1.));
#113141=DIRECTION('center_axis',(-3.85185988875507E-34,1.,0.));
#113142=DIRECTION('ref_axis',(0.,0.,1.));
#113143=DIRECTION('center_axis',(-3.85185988875507E-34,1.,0.));
#113144=DIRECTION('ref_axis',(0.,0.,1.));
#113145=DIRECTION('center_axis',(-3.85185988875507E-34,1.,0.));
#113146=DIRECTION('ref_axis',(0.,0.,1.));
#113147=DIRECTION('center_axis',(-3.85185988875507E-34,1.,0.));
#113148=DIRECTION('ref_axis',(0.,0.,1.));
#113149=DIRECTION('center_axis',(-3.85185988875507E-34,1.,0.));
#113150=DIRECTION('ref_axis',(0.,0.,1.));
#113151=DIRECTION('center_axis',(-3.85185988875507E-34,1.,0.));
#113152=DIRECTION('ref_axis',(0.,0.,1.));
#113153=DIRECTION('center_axis',(-3.85185988875507E-34,1.,0.));
#113154=DIRECTION('ref_axis',(0.,0.,1.));
#113155=DIRECTION('center_axis',(-3.85185988875507E-34,1.,0.));
#113156=DIRECTION('ref_axis',(0.,0.,1.));
#113157=DIRECTION('center_axis',(-3.85185988875507E-34,1.,0.));
#113158=DIRECTION('ref_axis',(0.,0.,1.));
#113159=DIRECTION('center_axis',(-3.85185988875507E-34,1.,0.));
#113160=DIRECTION('ref_axis',(0.,0.,1.));
#113161=DIRECTION('center_axis',(-3.85185988875507E-34,1.,0.));
#113162=DIRECTION('ref_axis',(0.,0.,1.));
#113163=DIRECTION('center_axis',(-3.85185988875507E-34,1.,0.));
#113164=DIRECTION('ref_axis',(0.,0.,1.));
#113165=DIRECTION('center_axis',(-3.85185988875507E-34,1.,0.));
#113166=DIRECTION('ref_axis',(0.,0.,1.));
#113167=DIRECTION('center_axis',(-3.85185988875507E-34,1.,0.));
#113168=DIRECTION('ref_axis',(0.,0.,1.));
#113169=DIRECTION('center_axis',(-3.85185988875507E-34,1.,0.));
#113170=DIRECTION('ref_axis',(0.,0.,1.));
#113171=DIRECTION('center_axis',(-3.85185988875507E-34,1.,0.));
#113172=DIRECTION('ref_axis',(0.,0.,1.));
#113173=DIRECTION('center_axis',(-3.85185988875507E-34,1.,0.));
#113174=DIRECTION('ref_axis',(0.,0.,1.));
#113175=DIRECTION('center_axis',(-3.85185988875507E-34,1.,0.));
#113176=DIRECTION('ref_axis',(0.,0.,1.));
#113177=DIRECTION('center_axis',(3.85185988875507E-34,-1.,0.));
#113178=DIRECTION('ref_axis',(0.,0.,1.));
#113179=DIRECTION('center_axis',(-3.85185988875507E-34,1.,0.));
#113180=DIRECTION('ref_axis',(0.,0.,1.));
#113181=DIRECTION('',(0.942809041733257,3.63156833060794E-34,-0.333333332905692));
#113182=DIRECTION('center_axis',(-3.85185988875507E-34,1.,0.));
#113183=DIRECTION('ref_axis',(0.,0.,1.));
#113184=DIRECTION('center_axis',(-3.85185988875507E-34,1.,0.));
#113185=DIRECTION('ref_axis',(0.,0.,1.));
#113186=DIRECTION('',(0.942809041733257,3.63156833060794E-34,0.333333332905692));
#113187=DIRECTION('center_axis',(-3.85185988875507E-34,1.,0.));
#113188=DIRECTION('ref_axis',(0.,0.,1.));
#113189=DIRECTION('',(-0.942809041733257,-3.63156833060794E-34,0.333333332905692));
#113190=DIRECTION('center_axis',(-3.85185988875507E-34,1.,0.));
#113191=DIRECTION('ref_axis',(0.,0.,1.));
#113192=DIRECTION('center_axis',(-3.85185988875507E-34,1.,0.));
#113193=DIRECTION('ref_axis',(0.,0.,1.));
#113194=DIRECTION('',(-0.942809041733257,-3.63156833060794E-34,-0.333333332905692));
#113195=DIRECTION('center_axis',(-3.85185988875507E-34,1.,0.));
#113196=DIRECTION('ref_axis',(0.,0.,1.));
#113197=DIRECTION('center_axis',(3.85185988875507E-34,-1.,0.));
#113198=DIRECTION('ref_axis',(0.,0.,1.));
#113199=DIRECTION('center_axis',(-3.85185988875507E-34,1.,0.));
#113200=DIRECTION('ref_axis',(0.,0.,1.));
#113201=DIRECTION('center_axis',(-3.85185988875507E-34,1.,0.));
#113202=DIRECTION('ref_axis',(1.,3.85185988875507E-34,0.));
#113203=DIRECTION('',(-3.85185988875507E-34,1.,0.));
#113204=DIRECTION('',(3.85185988875507E-34,-1.,0.));
#113205=DIRECTION('center_axis',(-3.85185988875507E-34,1.,0.));
#113206=DIRECTION('ref_axis',(0.,0.,1.));
#113207=DIRECTION('center_axis',(-3.85185988875507E-34,1.,0.));
#113208=DIRECTION('ref_axis',(1.,3.85185988875507E-34,0.));
#113209=DIRECTION('',(3.85185988875507E-34,-1.,0.));
#113210=DIRECTION('center_axis',(-3.85185988875507E-34,1.,0.));
#113211=DIRECTION('ref_axis',(0.,0.,1.));
#113212=DIRECTION('',(-3.85185988875507E-34,1.,0.));
#113213=DIRECTION('center_axis',(-3.85185988875507E-34,1.,0.));
#113214=DIRECTION('ref_axis',(1.,3.85185988875507E-34,0.));
#113215=DIRECTION('',(-3.85185988875507E-34,1.,0.));
#113216=DIRECTION('',(3.85185988875507E-34,-1.,0.));
#113217=DIRECTION('center_axis',(-3.85185988875507E-34,1.,0.));
#113218=DIRECTION('ref_axis',(0.,0.,1.));
#113219=DIRECTION('center_axis',(-3.85185988875507E-34,1.,0.));
#113220=DIRECTION('ref_axis',(1.,3.85185988875507E-34,0.));
#113221=DIRECTION('',(-3.85185988875507E-34,1.,0.));
#113222=DIRECTION('',(3.85185988875507E-34,-1.,0.));
#113223=DIRECTION('center_axis',(-3.85185988875507E-34,1.,0.));
#113224=DIRECTION('ref_axis',(0.,0.,1.));
#113225=DIRECTION('center_axis',(-3.85185988875507E-34,1.,0.));
#113226=DIRECTION('ref_axis',(1.,3.85185988875507E-34,0.));
#113227=DIRECTION('',(-3.85185988875507E-34,1.,0.));
#113228=DIRECTION('',(3.85185988875507E-34,-1.,0.));
#113229=DIRECTION('center_axis',(-3.85185988875507E-34,1.,0.));
#113230=DIRECTION('ref_axis',(0.,0.,1.));
#113231=DIRECTION('center_axis',(-3.85185988875507E-34,1.,0.));
#113232=DIRECTION('ref_axis',(1.,3.85185988875507E-34,0.));
#113233=DIRECTION('',(3.85185988875507E-34,-1.,0.));
#113234=DIRECTION('center_axis',(-3.85185988875507E-34,1.,0.));
#113235=DIRECTION('ref_axis',(0.,0.,1.));
#113236=DIRECTION('center_axis',(-3.85185988875507E-34,1.,0.));
#113237=DIRECTION('ref_axis',(1.,3.85185988875507E-34,0.));
#113238=DIRECTION('',(3.85185988875507E-34,-1.,0.));
#113239=DIRECTION('center_axis',(-3.85185988875507E-34,1.,0.));
#113240=DIRECTION('ref_axis',(0.,0.,1.));
#113241=DIRECTION('center_axis',(-3.85185988875507E-34,1.,0.));
#113242=DIRECTION('ref_axis',(1.,3.85185988875507E-34,0.));
#113243=DIRECTION('',(3.85185988875507E-34,-1.,0.));
#113244=DIRECTION('center_axis',(-3.85185988875507E-34,1.,0.));
#113245=DIRECTION('ref_axis',(0.,0.,1.));
#113246=DIRECTION('',(-3.85185988875507E-34,1.,0.));
#113247=DIRECTION('center_axis',(-3.85185988875507E-34,1.,0.));
#113248=DIRECTION('ref_axis',(1.,3.85185988875507E-34,0.));
#113249=DIRECTION('',(-3.85185988875507E-34,1.,0.));
#113250=DIRECTION('',(3.85185988875507E-34,-1.,0.));
#113251=DIRECTION('center_axis',(-3.85185988875507E-34,1.,0.));
#113252=DIRECTION('ref_axis',(0.,0.,1.));
#113253=DIRECTION('center_axis',(-3.85185988875507E-34,1.,0.));
#113254=DIRECTION('ref_axis',(1.,3.85185988875507E-34,0.));
#113255=DIRECTION('',(-3.85185988875507E-34,1.,0.));
#113256=DIRECTION('',(3.85185988875507E-34,-1.,0.));
#113257=DIRECTION('center_axis',(-3.85185988875507E-34,1.,0.));
#113258=DIRECTION('ref_axis',(0.,0.,1.));
#113259=DIRECTION('center_axis',(-3.85185988875507E-34,1.,0.));
#113260=DIRECTION('ref_axis',(1.,3.85185988875507E-34,0.));
#113261=DIRECTION('',(3.85185988875507E-34,-1.,0.));
#113262=DIRECTION('center_axis',(-3.85185988875507E-34,1.,0.));
#113263=DIRECTION('ref_axis',(0.,0.,1.));
#113264=DIRECTION('',(-3.85185988875507E-34,1.,0.));
#113265=DIRECTION('center_axis',(-3.85185988875507E-34,1.,0.));
#113266=DIRECTION('ref_axis',(1.,3.85185988875507E-34,0.));
#113267=DIRECTION('',(-3.85185988875507E-34,1.,0.));
#113268=DIRECTION('',(3.85185988875507E-34,-1.,0.));
#113269=DIRECTION('center_axis',(-3.85185988875507E-34,1.,0.));
#113270=DIRECTION('ref_axis',(0.,0.,1.));
#113271=DIRECTION('center_axis',(-3.85185988875507E-34,1.,0.));
#113272=DIRECTION('ref_axis',(1.,3.85185988875507E-34,0.));
#113273=DIRECTION('center_axis',(-3.85185988875507E-34,1.,0.));
#113274=DIRECTION('ref_axis',(0.,0.,1.));
#113275=DIRECTION('',(-3.85185988875507E-34,1.,0.));
#113276=DIRECTION('center_axis',(-3.85185988875507E-34,1.,0.));
#113277=DIRECTION('ref_axis',(1.,3.85185988875507E-34,0.));
#113278=DIRECTION('center_axis',(-3.85185988875507E-34,1.,0.));
#113279=DIRECTION('ref_axis',(0.,0.,1.));
#113280=DIRECTION('',(-3.85185988875507E-34,1.,0.));
#113281=DIRECTION('center_axis',(-3.85185988875507E-34,1.,0.));
#113282=DIRECTION('ref_axis',(1.,3.85185988875507E-34,0.));
#113283=DIRECTION('',(3.85185988875507E-34,-1.,0.));
#113284=DIRECTION('center_axis',(-3.85185988875507E-34,1.,0.));
#113285=DIRECTION('ref_axis',(0.,0.,1.));
#113286=DIRECTION('',(-3.85185988875507E-34,1.,0.));
#113287=DIRECTION('center_axis',(-3.85185988875507E-34,1.,0.));
#113288=DIRECTION('ref_axis',(1.,3.85185988875507E-34,0.));
#113289=DIRECTION('',(-3.85185988875507E-34,1.,0.));
#113290=DIRECTION('',(3.85185988875507E-34,-1.,0.));
#113291=DIRECTION('center_axis',(-3.85185988875507E-34,1.,0.));
#113292=DIRECTION('ref_axis',(0.,0.,1.));
#113293=DIRECTION('center_axis',(-3.85185988875507E-34,1.,0.));
#113294=DIRECTION('ref_axis',(1.,3.85185988875507E-34,0.));
#113295=DIRECTION('',(3.85185988875507E-34,-1.,0.));
#113296=DIRECTION('center_axis',(-3.85185988875507E-34,1.,0.));
#113297=DIRECTION('ref_axis',(0.,0.,1.));
#113298=DIRECTION('',(-3.85185988875507E-34,1.,0.));
#113299=DIRECTION('center_axis',(-3.85185988875507E-34,1.,0.));
#113300=DIRECTION('ref_axis',(1.,3.85185988875507E-34,0.));
#113301=DIRECTION('',(-3.85185988875507E-34,1.,0.));
#113302=DIRECTION('',(3.85185988875507E-34,-1.,0.));
#113303=DIRECTION('center_axis',(-3.85185988875507E-34,1.,0.));
#113304=DIRECTION('ref_axis',(0.,0.,1.));
#113305=DIRECTION('center_axis',(-3.85185988875507E-34,1.,0.));
#113306=DIRECTION('ref_axis',(1.,3.85185988875507E-34,0.));
#113307=DIRECTION('',(-3.85185988875507E-34,1.,0.));
#113308=DIRECTION('',(3.85185988875507E-34,-1.,0.));
#113309=DIRECTION('center_axis',(-3.85185988875507E-34,1.,0.));
#113310=DIRECTION('ref_axis',(0.,0.,1.));
#113311=DIRECTION('center_axis',(-3.85185988875507E-34,1.,0.));
#113312=DIRECTION('ref_axis',(1.,3.85185988875507E-34,0.));
#113313=DIRECTION('',(3.85185988875507E-34,-1.,0.));
#113314=DIRECTION('center_axis',(-3.85185988875507E-34,1.,0.));
#113315=DIRECTION('ref_axis',(0.,0.,1.));
#113316=DIRECTION('',(-3.85185988875507E-34,1.,0.));
#113317=DIRECTION('center_axis',(-3.85185988875507E-34,1.,0.));
#113318=DIRECTION('ref_axis',(1.,3.85185988875507E-34,0.));
#113319=DIRECTION('',(-3.85185988875507E-34,1.,0.));
#113320=DIRECTION('',(3.85185988875507E-34,-1.,0.));
#113321=DIRECTION('center_axis',(-3.85185988875507E-34,1.,0.));
#113322=DIRECTION('ref_axis',(0.,0.,1.));
#113323=DIRECTION('center_axis',(-3.85185988875507E-34,1.,0.));
#113324=DIRECTION('ref_axis',(1.,3.85185988875507E-34,0.));
#113325=DIRECTION('',(3.85185988875507E-34,-1.,0.));
#113326=DIRECTION('center_axis',(-3.85185988875507E-34,1.,0.));
#113327=DIRECTION('ref_axis',(0.,0.,1.));
#113328=DIRECTION('',(-3.85185988875507E-34,1.,0.));
#113329=DIRECTION('center_axis',(-3.85185988875507E-34,1.,0.));
#113330=DIRECTION('ref_axis',(1.,3.85185988875507E-34,0.));
#113331=DIRECTION('',(3.85185988875507E-34,-1.,0.));
#113332=DIRECTION('center_axis',(-3.85185988875507E-34,1.,0.));
#113333=DIRECTION('ref_axis',(0.,0.,1.));
#113334=DIRECTION('',(-3.85185988875507E-34,1.,0.));
#113335=DIRECTION('center_axis',(-3.85185988875507E-34,1.,0.));
#113336=DIRECTION('ref_axis',(1.,3.85185988875507E-34,0.));
#113337=DIRECTION('',(3.85185988875507E-34,-1.,0.));
#113338=DIRECTION('center_axis',(-3.85185988875507E-34,1.,0.));
#113339=DIRECTION('ref_axis',(0.,0.,1.));
#113340=DIRECTION('',(-3.85185988875507E-34,1.,0.));
#113341=DIRECTION('center_axis',(-3.85185988875507E-34,1.,0.));
#113342=DIRECTION('ref_axis',(1.,3.85185988875507E-34,0.));
#113343=DIRECTION('',(-3.85185988875507E-34,1.,0.));
#113344=DIRECTION('',(3.85185988875507E-34,-1.,0.));
#113345=DIRECTION('center_axis',(-3.85185988875507E-34,1.,0.));
#113346=DIRECTION('ref_axis',(0.,0.,1.));
#113347=DIRECTION('center_axis',(-3.85185988875507E-34,1.,0.));
#113348=DIRECTION('ref_axis',(1.,3.85185988875507E-34,0.));
#113349=DIRECTION('',(3.85185988875507E-34,-1.,0.));
#113350=DIRECTION('center_axis',(-3.85185988875507E-34,1.,0.));
#113351=DIRECTION('ref_axis',(0.,0.,1.));
#113352=DIRECTION('',(-3.85185988875507E-34,1.,0.));
#113353=DIRECTION('center_axis',(-3.85185988875507E-34,1.,0.));
#113354=DIRECTION('ref_axis',(1.,3.85185988875507E-34,0.));
#113355=DIRECTION('',(-3.85185988875507E-34,1.,0.));
#113356=DIRECTION('',(3.85185988875507E-34,-1.,0.));
#113357=DIRECTION('center_axis',(-3.85185988875507E-34,1.,0.));
#113358=DIRECTION('ref_axis',(0.,0.,1.));
#113359=DIRECTION('center_axis',(-3.85185988875507E-34,1.,0.));
#113360=DIRECTION('ref_axis',(1.,3.85185988875507E-34,0.));
#113361=DIRECTION('',(-3.85185988875507E-34,1.,0.));
#113362=DIRECTION('',(3.85185988875507E-34,-1.,0.));
#113363=DIRECTION('center_axis',(-3.85185988875507E-34,1.,0.));
#113364=DIRECTION('ref_axis',(0.,0.,1.));
#113365=DIRECTION('center_axis',(-3.85185988875507E-34,1.,0.));
#113366=DIRECTION('ref_axis',(1.,3.85185988875507E-34,0.));
#113367=DIRECTION('',(3.85185988875507E-34,-1.,0.));
#113368=DIRECTION('center_axis',(-3.85185988875507E-34,1.,0.));
#113369=DIRECTION('ref_axis',(0.,0.,1.));
#113370=DIRECTION('',(-3.85185988875507E-34,1.,0.));
#113371=DIRECTION('center_axis',(-3.85185988875507E-34,1.,0.));
#113372=DIRECTION('ref_axis',(1.,3.85185988875507E-34,0.));
#113373=DIRECTION('',(-3.85185988875507E-34,1.,0.));
#113374=DIRECTION('',(3.85185988875507E-34,-1.,0.));
#113375=DIRECTION('center_axis',(-3.85185988875507E-34,1.,0.));
#113376=DIRECTION('ref_axis',(0.,0.,1.));
#113377=DIRECTION('center_axis',(-3.85185988875507E-34,1.,0.));
#113378=DIRECTION('ref_axis',(1.,3.85185988875507E-34,0.));
#113379=DIRECTION('',(3.85185988875507E-34,-1.,0.));
#113380=DIRECTION('center_axis',(-3.85185988875507E-34,1.,0.));
#113381=DIRECTION('ref_axis',(0.,0.,1.));
#113382=DIRECTION('',(-3.85185988875507E-34,1.,0.));
#113383=DIRECTION('center_axis',(-3.85185988875507E-34,1.,0.));
#113384=DIRECTION('ref_axis',(1.,3.85185988875507E-34,0.));
#113385=DIRECTION('',(3.85185988875507E-34,-1.,0.));
#113386=DIRECTION('center_axis',(-3.85185988875507E-34,1.,0.));
#113387=DIRECTION('ref_axis',(0.,0.,1.));
#113388=DIRECTION('',(-3.85185988875507E-34,1.,0.));
#113389=DIRECTION('center_axis',(-3.85185988875507E-34,1.,0.));
#113390=DIRECTION('ref_axis',(1.,3.85185988875507E-34,0.));
#113391=DIRECTION('',(3.85185988875507E-34,-1.,0.));
#113392=DIRECTION('center_axis',(-3.85185988875507E-34,1.,0.));
#113393=DIRECTION('ref_axis',(0.,0.,1.));
#113394=DIRECTION('',(-3.85185988875507E-34,1.,0.));
#113395=DIRECTION('center_axis',(-3.85185988875507E-34,1.,0.));
#113396=DIRECTION('ref_axis',(1.,3.85185988875507E-34,0.));
#113397=DIRECTION('',(-3.85185988875507E-34,1.,0.));
#113398=DIRECTION('',(3.85185988875507E-34,-1.,0.));
#113399=DIRECTION('center_axis',(-3.85185988875507E-34,1.,0.));
#113400=DIRECTION('ref_axis',(0.,0.,1.));
#113401=DIRECTION('center_axis',(-3.85185988875507E-34,1.,0.));
#113402=DIRECTION('ref_axis',(1.,3.85185988875507E-34,0.));
#113403=DIRECTION('',(-3.85185988875507E-34,1.,0.));
#113404=DIRECTION('',(3.85185988875507E-34,-1.,0.));
#113405=DIRECTION('center_axis',(-3.85185988875507E-34,1.,0.));
#113406=DIRECTION('ref_axis',(0.,0.,1.));
#113407=DIRECTION('center_axis',(-3.85185988875507E-34,1.,0.));
#113408=DIRECTION('ref_axis',(1.,3.85185988875507E-34,0.));
#113409=DIRECTION('',(-3.85185988875507E-34,1.,0.));
#113410=DIRECTION('',(3.85185988875507E-34,-1.,0.));
#113411=DIRECTION('center_axis',(-3.85185988875507E-34,1.,0.));
#113412=DIRECTION('ref_axis',(0.,0.,1.));
#113413=DIRECTION('center_axis',(3.85185988875507E-34,-1.,0.));
#113414=DIRECTION('ref_axis',(-1.,-3.85185988875507E-34,0.));
#113415=DIRECTION('center_axis',(-3.85185988875507E-34,1.,0.));
#113416=DIRECTION('ref_axis',(0.,0.,1.));
#113417=DIRECTION('center_axis',(3.85185988875507E-34,-1.,0.));
#113418=DIRECTION('ref_axis',(0.,0.,1.));
#113419=DIRECTION('center_axis',(-3.85185988875507E-34,1.,0.));
#113420=DIRECTION('ref_axis',(0.,0.,1.));
#113421=DIRECTION('center_axis',(-3.85185988875507E-34,1.,0.));
#113422=DIRECTION('ref_axis',(0.,0.,1.));
#113423=DIRECTION('center_axis',(3.85185988875507E-34,-1.,0.));
#113424=DIRECTION('ref_axis',(0.,0.,1.));
#113425=DIRECTION('center_axis',(-3.85185988875507E-34,1.,0.));
#113426=DIRECTION('ref_axis',(0.,0.,1.));
#113427=DIRECTION('center_axis',(-3.85185988875507E-34,1.,0.));
#113428=DIRECTION('ref_axis',(0.,0.,1.));
#113429=DIRECTION('center_axis',(3.85185988875507E-34,-1.,0.));
#113430=DIRECTION('ref_axis',(0.,0.,1.));
#113431=DIRECTION('center_axis',(-3.85185988875507E-34,1.,0.));
#113432=DIRECTION('ref_axis',(0.,0.,1.));
#113433=DIRECTION('center_axis',(-3.85185988875507E-34,1.,0.));
#113434=DIRECTION('ref_axis',(0.,0.,1.));
#113435=DIRECTION('center_axis',(3.85185988875507E-34,-1.,0.));
#113436=DIRECTION('ref_axis',(0.,0.,1.));
#113437=DIRECTION('center_axis',(-3.85185988875507E-34,1.,0.));
#113438=DIRECTION('ref_axis',(0.,0.,1.));
#113439=DIRECTION('center_axis',(-3.85185988875507E-34,1.,0.));
#113440=DIRECTION('ref_axis',(0.,0.,1.));
#113441=DIRECTION('center_axis',(3.85185988875507E-34,-1.,0.));
#113442=DIRECTION('ref_axis',(0.,0.,1.));
#113443=DIRECTION('center_axis',(-3.85185988875507E-34,1.,0.));
#113444=DIRECTION('ref_axis',(0.,0.,1.));
#113445=DIRECTION('center_axis',(-3.85185988875507E-34,1.,0.));
#113446=DIRECTION('ref_axis',(0.,0.,1.));
#113447=DIRECTION('center_axis',(3.85185988875507E-34,-1.,0.));
#113448=DIRECTION('ref_axis',(0.,0.,1.));
#113449=DIRECTION('center_axis',(-3.85185988875507E-34,1.,0.));
#113450=DIRECTION('ref_axis',(0.,0.,1.));
#113451=DIRECTION('center_axis',(3.85185988875507E-34,-1.,0.));
#113452=DIRECTION('ref_axis',(0.,0.,1.));
#113453=DIRECTION('center_axis',(-3.85185988875507E-34,1.,0.));
#113454=DIRECTION('ref_axis',(0.,0.,1.));
#113455=DIRECTION('center_axis',(3.85185988875507E-34,-1.,0.));
#113456=DIRECTION('ref_axis',(0.,0.,1.));
#113457=DIRECTION('center_axis',(-3.85185988875507E-34,1.,0.));
#113458=DIRECTION('ref_axis',(0.,0.,1.));
#113459=DIRECTION('center_axis',(-3.85185988875507E-34,1.,0.));
#113460=DIRECTION('ref_axis',(0.,0.,1.));
#113461=DIRECTION('center_axis',(-3.85185988875507E-34,1.,0.));
#113462=DIRECTION('ref_axis',(0.,0.,1.));
#113463=DIRECTION('center_axis',(3.85185988875507E-34,-1.,0.));
#113464=DIRECTION('ref_axis',(0.,0.,1.));
#113465=DIRECTION('center_axis',(-3.85185988875507E-34,1.,0.));
#113466=DIRECTION('ref_axis',(0.,0.,1.));
#113467=DIRECTION('center_axis',(-3.85185988875507E-34,1.,0.));
#113468=DIRECTION('ref_axis',(0.,0.,1.));
#113469=DIRECTION('center_axis',(3.85185988875507E-34,-1.,0.));
#113470=DIRECTION('ref_axis',(0.,0.,1.));
#113471=DIRECTION('center_axis',(-3.85185988875507E-34,1.,0.));
#113472=DIRECTION('ref_axis',(0.,0.,1.));
#113473=DIRECTION('center_axis',(-3.85185988875507E-34,1.,0.));
#113474=DIRECTION('ref_axis',(0.,0.,1.));
#113475=DIRECTION('center_axis',(3.85185988875507E-34,-1.,0.));
#113476=DIRECTION('ref_axis',(0.,0.,1.));
#113477=DIRECTION('center_axis',(-3.85185988875507E-34,1.,0.));
#113478=DIRECTION('ref_axis',(0.,0.,1.));
#113479=DIRECTION('center_axis',(-3.85185988875507E-34,1.,0.));
#113480=DIRECTION('ref_axis',(0.,0.,1.));
#113481=DIRECTION('center_axis',(3.85185988875507E-34,-1.,0.));
#113482=DIRECTION('ref_axis',(0.,0.,1.));
#113483=DIRECTION('center_axis',(-3.85185988875507E-34,1.,0.));
#113484=DIRECTION('ref_axis',(0.,0.,1.));
#113485=DIRECTION('center_axis',(-3.85185988875507E-34,1.,0.));
#113486=DIRECTION('ref_axis',(0.,0.,1.));
#113487=DIRECTION('center_axis',(3.85185988875507E-34,-1.,0.));
#113488=DIRECTION('ref_axis',(0.,0.,1.));
#113489=DIRECTION('center_axis',(-3.85185988875507E-34,1.,0.));
#113490=DIRECTION('ref_axis',(0.,0.,1.));
#113491=DIRECTION('center_axis',(-3.85185988875507E-34,1.,0.));
#113492=DIRECTION('ref_axis',(0.,0.,1.));
#113493=DIRECTION('center_axis',(3.85185988875507E-34,-1.,0.));
#113494=DIRECTION('ref_axis',(0.,0.,1.));
#113495=DIRECTION('center_axis',(-3.85185988875507E-34,1.,0.));
#113496=DIRECTION('ref_axis',(0.,0.,1.));
#113497=DIRECTION('center_axis',(-3.85185988875507E-34,1.,0.));
#113498=DIRECTION('ref_axis',(0.,0.,1.));
#113499=DIRECTION('center_axis',(3.85185988875507E-34,-1.,0.));
#113500=DIRECTION('ref_axis',(0.,0.,1.));
#113501=DIRECTION('center_axis',(-3.85185988875507E-34,1.,0.));
#113502=DIRECTION('ref_axis',(0.,0.,1.));
#113503=DIRECTION('center_axis',(-3.85185988875507E-34,1.,0.));
#113504=DIRECTION('ref_axis',(0.,0.,1.));
#113505=DIRECTION('center_axis',(3.85185988875507E-34,-1.,0.));
#113506=DIRECTION('ref_axis',(0.,0.,1.));
#113507=DIRECTION('center_axis',(-3.85185988875507E-34,1.,0.));
#113508=DIRECTION('ref_axis',(0.,0.,1.));
#113509=DIRECTION('center_axis',(-3.85185988875507E-34,1.,0.));
#113510=DIRECTION('ref_axis',(0.,0.,1.));
#113511=DIRECTION('center_axis',(3.85185988875507E-34,-1.,0.));
#113512=DIRECTION('ref_axis',(0.,0.,1.));
#113513=DIRECTION('center_axis',(-3.85185988875507E-34,1.,0.));
#113514=DIRECTION('ref_axis',(0.,0.,1.));
#113515=DIRECTION('center_axis',(-3.85185988875507E-34,1.,0.));
#113516=DIRECTION('ref_axis',(0.,0.,1.));
#113517=DIRECTION('center_axis',(3.85185988875507E-34,-1.,0.));
#113518=DIRECTION('ref_axis',(0.,0.,1.));
#113519=DIRECTION('center_axis',(-3.85185988875507E-34,1.,0.));
#113520=DIRECTION('ref_axis',(0.,0.,1.));
#113521=DIRECTION('center_axis',(-3.85185988875507E-34,1.,0.));
#113522=DIRECTION('ref_axis',(0.,0.,1.));
#113523=DIRECTION('center_axis',(3.85185988875507E-34,-1.,0.));
#113524=DIRECTION('ref_axis',(0.,0.,1.));
#113525=DIRECTION('center_axis',(-3.85185988875507E-34,1.,0.));
#113526=DIRECTION('ref_axis',(0.,0.,1.));
#113527=DIRECTION('center_axis',(-3.85185988875507E-34,1.,0.));
#113528=DIRECTION('ref_axis',(0.,0.,1.));
#113529=DIRECTION('center_axis',(3.85185988875507E-34,-1.,0.));
#113530=DIRECTION('ref_axis',(0.,0.,1.));
#113531=DIRECTION('center_axis',(-3.85185988875507E-34,1.,0.));
#113532=DIRECTION('ref_axis',(0.,0.,1.));
#113533=DIRECTION('center_axis',(-3.85185988875507E-34,1.,0.));
#113534=DIRECTION('ref_axis',(0.,0.,1.));
#113535=DIRECTION('center_axis',(3.85185988875507E-34,-1.,0.));
#113536=DIRECTION('ref_axis',(0.,0.,1.));
#113537=DIRECTION('center_axis',(-3.85185988875507E-34,1.,0.));
#113538=DIRECTION('ref_axis',(0.,0.,1.));
#113539=DIRECTION('center_axis',(-3.85185988875507E-34,1.,0.));
#113540=DIRECTION('ref_axis',(0.,0.,1.));
#113541=DIRECTION('center_axis',(3.85185988875507E-34,-1.,0.));
#113542=DIRECTION('ref_axis',(0.,0.,1.));
#113543=DIRECTION('center_axis',(-3.85185988875507E-34,1.,0.));
#113544=DIRECTION('ref_axis',(0.,0.,1.));
#113545=DIRECTION('center_axis',(-3.85185988875507E-34,1.,0.));
#113546=DIRECTION('ref_axis',(0.,0.,1.));
#113547=DIRECTION('center_axis',(3.85185988875507E-34,-1.,0.));
#113548=DIRECTION('ref_axis',(0.,0.,1.));
#113549=DIRECTION('center_axis',(-3.85185988875507E-34,1.,0.));
#113550=DIRECTION('ref_axis',(0.,0.,1.));
#113551=DIRECTION('center_axis',(-3.85185988875507E-34,1.,0.));
#113552=DIRECTION('ref_axis',(0.,0.,1.));
#113553=DIRECTION('center_axis',(3.85185988875507E-34,-1.,0.));
#113554=DIRECTION('ref_axis',(0.,0.,1.));
#113555=DIRECTION('center_axis',(-3.85185988875507E-34,1.,0.));
#113556=DIRECTION('ref_axis',(0.,0.,1.));
#113557=DIRECTION('center_axis',(-3.85185988875507E-34,1.,0.));
#113558=DIRECTION('ref_axis',(0.,0.,1.));
#113559=DIRECTION('center_axis',(3.85185988875507E-34,-1.,0.));
#113560=DIRECTION('ref_axis',(0.,0.,1.));
#113561=DIRECTION('center_axis',(-3.85185988875507E-34,1.,0.));
#113562=DIRECTION('ref_axis',(0.,0.,1.));
#113563=DIRECTION('center_axis',(-3.85185988875507E-34,1.,0.));
#113564=DIRECTION('ref_axis',(0.,0.,1.));
#113565=DIRECTION('center_axis',(3.85185988875507E-34,-1.,0.));
#113566=DIRECTION('ref_axis',(0.,0.,1.));
#113567=DIRECTION('center_axis',(-3.85185988875507E-34,1.,0.));
#113568=DIRECTION('ref_axis',(0.,0.,1.));
#113569=DIRECTION('center_axis',(-3.85185988875507E-34,1.,0.));
#113570=DIRECTION('ref_axis',(0.,0.,1.));
#113571=DIRECTION('center_axis',(3.85185988875507E-34,-1.,0.));
#113572=DIRECTION('ref_axis',(0.,0.,1.));
#113573=DIRECTION('center_axis',(-3.85185988875507E-34,1.,0.));
#113574=DIRECTION('ref_axis',(0.,0.,1.));
#113575=DIRECTION('center_axis',(-3.85185988875507E-34,1.,0.));
#113576=DIRECTION('ref_axis',(0.,0.,1.));
#113577=DIRECTION('center_axis',(3.85185988875507E-34,-1.,0.));
#113578=DIRECTION('ref_axis',(0.,0.,1.));
#113579=DIRECTION('center_axis',(-3.85185988875507E-34,1.,0.));
#113580=DIRECTION('ref_axis',(0.,0.,1.));
#113581=DIRECTION('center_axis',(-3.85185988875507E-34,1.,0.));
#113582=DIRECTION('ref_axis',(0.,0.,1.));
#113583=DIRECTION('center_axis',(-3.85185988875507E-34,1.,0.));
#113584=DIRECTION('ref_axis',(0.,0.,1.));
#113585=DIRECTION('center_axis',(-3.85185988875507E-34,1.,0.));
#113586=DIRECTION('ref_axis',(0.,0.,1.));
#113587=DIRECTION('center_axis',(-3.85185988875507E-34,1.,0.));
#113588=DIRECTION('ref_axis',(0.,0.,1.));
#113589=DIRECTION('center_axis',(-3.85185988875507E-34,1.,0.));
#113590=DIRECTION('ref_axis',(0.,0.,1.));
#113591=DIRECTION('center_axis',(3.85185988875507E-34,-1.,0.));
#113592=DIRECTION('ref_axis',(0.,0.,1.));
#113593=DIRECTION('center_axis',(-3.85185988875507E-34,1.,0.));
#113594=DIRECTION('ref_axis',(0.,0.,1.));
#113595=DIRECTION('center_axis',(-3.85185988875507E-34,1.,0.));
#113596=DIRECTION('ref_axis',(0.,0.,1.));
#113597=DIRECTION('center_axis',(3.85185988875507E-34,-1.,0.));
#113598=DIRECTION('ref_axis',(0.,0.,1.));
#113599=DIRECTION('center_axis',(-3.85185988875507E-34,1.,0.));
#113600=DIRECTION('ref_axis',(0.,0.,1.));
#113601=DIRECTION('center_axis',(-3.85185988875507E-34,1.,0.));
#113602=DIRECTION('ref_axis',(0.,0.,1.));
#113603=DIRECTION('center_axis',(3.85185988875507E-34,-1.,0.));
#113604=DIRECTION('ref_axis',(0.,0.,1.));
#113605=DIRECTION('center_axis',(-3.85185988875507E-34,1.,0.));
#113606=DIRECTION('ref_axis',(0.,0.,1.));
#113607=DIRECTION('center_axis',(-3.85185988875507E-34,1.,0.));
#113608=DIRECTION('ref_axis',(0.,0.,1.));
#113609=DIRECTION('center_axis',(3.85185988875507E-34,-1.,0.));
#113610=DIRECTION('ref_axis',(0.,0.,1.));
#113611=DIRECTION('center_axis',(-3.85185988875507E-34,1.,0.));
#113612=DIRECTION('ref_axis',(0.,0.,1.));
#113613=DIRECTION('center_axis',(-3.85185988875507E-34,1.,0.));
#113614=DIRECTION('ref_axis',(0.,0.,1.));
#113615=DIRECTION('center_axis',(3.85185988875507E-34,-1.,0.));
#113616=DIRECTION('ref_axis',(0.,0.,1.));
#113617=DIRECTION('center_axis',(-3.85185988875507E-34,1.,0.));
#113618=DIRECTION('ref_axis',(0.,0.,1.));
#113619=DIRECTION('center_axis',(-3.85185988875507E-34,1.,0.));
#113620=DIRECTION('ref_axis',(0.,0.,1.));
#113621=DIRECTION('center_axis',(3.85185988875507E-34,-1.,0.));
#113622=DIRECTION('ref_axis',(0.,0.,1.));
#113623=DIRECTION('center_axis',(-3.85185988875507E-34,1.,0.));
#113624=DIRECTION('ref_axis',(0.,0.,1.));
#113625=DIRECTION('center_axis',(-3.85185988875507E-34,1.,0.));
#113626=DIRECTION('ref_axis',(0.,0.,1.));
#113627=DIRECTION('center_axis',(3.85185988875507E-34,-1.,0.));
#113628=DIRECTION('ref_axis',(0.,0.,1.));
#113629=DIRECTION('center_axis',(-3.85185988875507E-34,1.,0.));
#113630=DIRECTION('ref_axis',(0.,0.,1.));
#113631=DIRECTION('center_axis',(-3.85185988875507E-34,1.,0.));
#113632=DIRECTION('ref_axis',(1.,3.85185988875507E-34,0.));
#113633=DIRECTION('',(-3.85185988875507E-34,1.,0.));
#113634=DIRECTION('',(3.85185988875507E-34,-1.,0.));
#113635=DIRECTION('center_axis',(-3.85185988875507E-34,1.,0.));
#113636=DIRECTION('ref_axis',(1.,3.85185988875507E-34,0.));
#113637=DIRECTION('',(-3.85185988875507E-34,1.,0.));
#113638=DIRECTION('center_axis',(-3.85185988875507E-34,1.,0.));
#113639=DIRECTION('ref_axis',(1.,3.85185988875507E-34,0.));
#113640=DIRECTION('',(-3.85185988875507E-34,1.,0.));
#113641=DIRECTION('center_axis',(-3.85185988875507E-34,1.,0.));
#113642=DIRECTION('ref_axis',(1.,3.85185988875507E-34,0.));
#113643=DIRECTION('center_axis',(-3.85185988875507E-34,1.,0.));
#113644=DIRECTION('ref_axis',(1.,3.85185988875507E-34,0.));
#113645=DIRECTION('',(-3.85185988875507E-34,1.,0.));
#113646=DIRECTION('center_axis',(-3.85185988875507E-34,1.,0.));
#113647=DIRECTION('ref_axis',(1.,3.85185988875507E-34,0.));
#113648=DIRECTION('',(-3.85185988875507E-34,1.,0.));
#113649=DIRECTION('center_axis',(-3.85185988875507E-34,1.,0.));
#113650=DIRECTION('ref_axis',(1.,3.85185988875507E-34,0.));
#113651=DIRECTION('center_axis',(-3.85185988875507E-34,1.,0.));
#113652=DIRECTION('ref_axis',(1.,3.85185988875507E-34,0.));
#113653=DIRECTION('',(-3.85185988875507E-34,1.,0.));
#113654=DIRECTION('center_axis',(-3.85185988875507E-34,1.,0.));
#113655=DIRECTION('ref_axis',(1.,3.85185988875507E-34,0.));
#113656=DIRECTION('',(-3.85185988875507E-34,1.,0.));
#113657=DIRECTION('center_axis',(-3.85185988875507E-34,1.,0.));
#113658=DIRECTION('ref_axis',(1.,3.85185988875507E-34,0.));
#113659=DIRECTION('center_axis',(-3.85185988875507E-34,1.,0.));
#113660=DIRECTION('ref_axis',(1.,3.85185988875507E-34,0.));
#113661=DIRECTION('',(-3.85185988875507E-34,1.,0.));
#113662=DIRECTION('center_axis',(-3.85185988875507E-34,1.,0.));
#113663=DIRECTION('ref_axis',(1.,3.85185988875507E-34,0.));
#113664=DIRECTION('',(-3.85185988875507E-34,1.,0.));
#113665=DIRECTION('center_axis',(-3.85185988875507E-34,1.,0.));
#113666=DIRECTION('ref_axis',(1.,3.85185988875507E-34,0.));
#113667=DIRECTION('center_axis',(-3.85185988875507E-34,1.,0.));
#113668=DIRECTION('ref_axis',(1.,3.85185988875507E-34,0.));
#113669=DIRECTION('',(-3.85185988875507E-34,1.,0.));
#113670=DIRECTION('center_axis',(-3.85185988875507E-34,1.,0.));
#113671=DIRECTION('ref_axis',(1.,3.85185988875507E-34,0.));
#113672=DIRECTION('',(-3.85185988875507E-34,1.,0.));
#113673=DIRECTION('center_axis',(-3.85185988875507E-34,1.,0.));
#113674=DIRECTION('ref_axis',(1.,3.85185988875507E-34,0.));
#113675=DIRECTION('center_axis',(-3.85185988875507E-34,1.,0.));
#113676=DIRECTION('ref_axis',(1.,3.85185988875507E-34,0.));
#113677=DIRECTION('',(-3.85185988875507E-34,1.,0.));
#113678=DIRECTION('center_axis',(-3.85185988875507E-34,1.,0.));
#113679=DIRECTION('ref_axis',(1.,3.85185988875507E-34,0.));
#113680=DIRECTION('',(-3.85185988875507E-34,1.,0.));
#113681=DIRECTION('center_axis',(-3.85185988875507E-34,1.,0.));
#113682=DIRECTION('ref_axis',(1.,3.85185988875507E-34,0.));
#113683=DIRECTION('center_axis',(-3.85185988875507E-34,1.,0.));
#113684=DIRECTION('ref_axis',(1.,3.85185988875507E-34,0.));
#113685=DIRECTION('',(-3.85185988875507E-34,1.,0.));
#113686=DIRECTION('center_axis',(-3.85185988875507E-34,1.,0.));
#113687=DIRECTION('ref_axis',(1.,3.85185988875507E-34,0.));
#113688=DIRECTION('',(-3.85185988875507E-34,1.,0.));
#113689=DIRECTION('center_axis',(-3.85185988875507E-34,1.,0.));
#113690=DIRECTION('ref_axis',(1.,3.85185988875507E-34,0.));
#113691=DIRECTION('center_axis',(-3.85185988875507E-34,1.,0.));
#113692=DIRECTION('ref_axis',(1.,3.85185988875507E-34,0.));
#113693=DIRECTION('',(-3.85185988875507E-34,1.,0.));
#113694=DIRECTION('center_axis',(-3.85185988875507E-34,1.,0.));
#113695=DIRECTION('ref_axis',(-0.998948206426938,-3.84780852727974E-34,
-0.0458528175405152));
#113696=DIRECTION('',(-3.85185988875507E-34,1.,0.));
#113697=DIRECTION('center_axis',(-3.85185988875507E-34,1.,0.));
#113698=DIRECTION('ref_axis',(1.,3.85185988875507E-34,0.));
#113699=DIRECTION('center_axis',(-3.85185988875507E-34,1.,0.));
#113700=DIRECTION('ref_axis',(1.,3.85185988875507E-34,0.));
#113701=DIRECTION('',(-3.85185988875507E-34,1.,0.));
#113702=DIRECTION('center_axis',(-3.85185988875507E-34,1.,0.));
#113703=DIRECTION('ref_axis',(-0.992328409627066,-3.8223099975146E-34,0.123629799995869));
#113704=DIRECTION('',(-3.85185988875507E-34,1.,0.));
#113705=DIRECTION('center_axis',(-3.85185988875507E-34,1.,0.));
#113706=DIRECTION('ref_axis',(1.,3.85185988875507E-34,0.));
#113707=DIRECTION('center_axis',(-3.85185988875507E-34,1.,0.));
#113708=DIRECTION('ref_axis',(1.,3.85185988875507E-34,0.));
#113709=DIRECTION('',(-3.85185988875507E-34,1.,0.));
#113710=DIRECTION('center_axis',(-3.85185988875507E-34,1.,0.));
#113711=DIRECTION('ref_axis',(1.,3.85185988875507E-34,0.));
#113712=DIRECTION('',(-3.85185988875507E-34,1.,0.));
#113713=DIRECTION('center_axis',(-3.85185988875507E-34,1.,0.));
#113714=DIRECTION('ref_axis',(1.,3.85185988875507E-34,0.));
#113715=DIRECTION('center_axis',(-3.85185988875507E-34,1.,0.));
#113716=DIRECTION('ref_axis',(1.,3.85185988875507E-34,0.));
#113717=DIRECTION('',(-3.85185988875507E-34,1.,0.));
#113718=DIRECTION('center_axis',(-3.85185988875507E-34,1.,0.));
#113719=DIRECTION('ref_axis',(1.,3.85185988875507E-34,0.));
#113720=DIRECTION('',(-3.85185988875507E-34,1.,0.));
#113721=DIRECTION('center_axis',(-3.85185988875507E-34,1.,0.));
#113722=DIRECTION('ref_axis',(1.,3.85185988875507E-34,0.));
#113723=DIRECTION('center_axis',(-3.85185988875507E-34,1.,0.));
#113724=DIRECTION('ref_axis',(1.,3.85185988875507E-34,0.));
#113725=DIRECTION('',(-3.85185988875507E-34,1.,0.));
#113726=DIRECTION('center_axis',(-3.85185988875507E-34,1.,0.));
#113727=DIRECTION('ref_axis',(1.,3.85185988875507E-34,0.));
#113728=DIRECTION('',(-3.85185988875507E-34,1.,0.));
#113729=DIRECTION('center_axis',(-3.85185988875507E-34,1.,0.));
#113730=DIRECTION('ref_axis',(1.,3.85185988875507E-34,0.));
#113731=DIRECTION('center_axis',(-3.85185988875507E-34,1.,0.));
#113732=DIRECTION('ref_axis',(-0.991460893518391,-3.81896844701275E-34,
0.130404358146931));
#113733=DIRECTION('',(-3.85185988875507E-34,1.,0.));
#113734=DIRECTION('center_axis',(-3.85185988875507E-34,1.,0.));
#113735=DIRECTION('ref_axis',(1.,3.85185988875507E-34,0.));
#113736=DIRECTION('',(-3.85185988875507E-34,1.,0.));
#113737=DIRECTION('center_axis',(-3.85185988875507E-34,1.,0.));
#113738=DIRECTION('ref_axis',(1.,3.85185988875507E-34,0.));
#113739=DIRECTION('center_axis',(-3.85185988875507E-34,1.,0.));
#113740=DIRECTION('ref_axis',(1.,3.85185988875507E-34,0.));
#113741=DIRECTION('',(-3.85185988875507E-34,1.,0.));
#113742=DIRECTION('center_axis',(-3.85185988875507E-34,1.,0.));
#113743=DIRECTION('ref_axis',(1.,3.85185988875507E-34,0.));
#113744=DIRECTION('',(-3.85185988875507E-34,1.,0.));
#113745=DIRECTION('center_axis',(-3.85185988875507E-34,1.,0.));
#113746=DIRECTION('ref_axis',(1.,3.85185988875507E-34,0.));
#113747=DIRECTION('center_axis',(-3.85185988875507E-34,1.,0.));
#113748=DIRECTION('ref_axis',(-0.999238074648388,-3.84892505905497E-34,
-0.0390290939298224));
#113749=DIRECTION('',(-3.85185988875507E-34,1.,0.));
#113750=DIRECTION('center_axis',(-3.85185988875507E-34,1.,0.));
#113751=DIRECTION('ref_axis',(1.,3.85185988875507E-34,0.));
#113752=DIRECTION('',(-3.85185988875507E-34,1.,0.));
#113753=DIRECTION('center_axis',(-3.85185988875507E-34,1.,0.));
#113754=DIRECTION('ref_axis',(1.,3.85185988875507E-34,0.));
#113755=DIRECTION('center_axis',(-3.85185988875507E-34,1.,0.));
#113756=DIRECTION('ref_axis',(1.,3.85185988875507E-34,0.));
#113757=DIRECTION('',(-3.85185988875507E-34,1.,0.));
#113758=DIRECTION('center_axis',(-3.85185988875507E-34,1.,0.));
#113759=DIRECTION('ref_axis',(1.,3.85185988875507E-34,0.));
#113760=DIRECTION('',(-3.85185988875507E-34,1.,0.));
#113761=DIRECTION('center_axis',(-3.85185988875507E-34,1.,0.));
#113762=DIRECTION('ref_axis',(1.,3.85185988875507E-34,0.));
#113763=DIRECTION('center_axis',(-3.85185988875507E-34,1.,0.));
#113764=DIRECTION('ref_axis',(1.,3.85185988875507E-34,0.));
#113765=DIRECTION('',(-3.85185988875507E-34,1.,0.));
#113766=DIRECTION('center_axis',(-3.85185988875507E-34,1.,0.));
#113767=DIRECTION('ref_axis',(1.,3.85185988875507E-34,0.));
#113768=DIRECTION('',(-3.85185988875507E-34,1.,0.));
#113769=DIRECTION('center_axis',(-3.85185988875507E-34,1.,0.));
#113770=DIRECTION('ref_axis',(1.,3.85185988875507E-34,0.));
#113771=DIRECTION('center_axis',(-3.85185988875507E-34,1.,0.));
#113772=DIRECTION('ref_axis',(1.,3.85185988875507E-34,0.));
#113773=DIRECTION('',(-3.85185988875507E-34,1.,0.));
#113774=DIRECTION('center_axis',(-3.85185988875507E-34,1.,0.));
#113775=DIRECTION('ref_axis',(1.,3.85185988875507E-34,0.));
#113776=DIRECTION('',(-3.85185988875507E-34,1.,0.));
#113777=DIRECTION('center_axis',(-3.85185988875507E-34,1.,0.));
#113778=DIRECTION('ref_axis',(1.,3.85185988875507E-34,0.));
#113779=DIRECTION('center_axis',(-3.85185988875507E-34,1.,0.));
#113780=DIRECTION('ref_axis',(1.,3.85185988875507E-34,0.));
#113781=DIRECTION('',(-3.85185988875507E-34,1.,0.));
#113782=DIRECTION('center_axis',(-3.85185988875507E-34,1.,0.));
#113783=DIRECTION('ref_axis',(1.,3.85185988875507E-34,0.));
#113784=DIRECTION('',(-3.85185988875507E-34,1.,0.));
#113785=DIRECTION('center_axis',(-3.85185988875507E-34,1.,0.));
#113786=DIRECTION('ref_axis',(1.,3.85185988875507E-34,0.));
#113787=DIRECTION('center_axis',(-3.85185988875507E-34,1.,0.));
#113788=DIRECTION('ref_axis',(1.,3.85185988875507E-34,0.));
#113789=DIRECTION('',(-3.85185988875507E-34,1.,0.));
#113790=DIRECTION('center_axis',(-3.85185988875507E-34,1.,0.));
#113791=DIRECTION('ref_axis',(1.,3.85185988875507E-34,0.));
#113792=DIRECTION('',(-3.85185988875507E-34,1.,0.));
#113793=DIRECTION('center_axis',(-3.85185988875507E-34,1.,0.));
#113794=DIRECTION('ref_axis',(1.,3.85185988875507E-34,0.));
#113795=DIRECTION('center_axis',(-3.85185988875507E-34,1.,0.));
#113796=DIRECTION('ref_axis',(1.,3.85185988875507E-34,0.));
#113797=DIRECTION('',(-3.85185988875507E-34,1.,0.));
#113798=DIRECTION('center_axis',(-3.85185988875507E-34,1.,0.));
#113799=DIRECTION('ref_axis',(1.,3.85185988875507E-34,0.));
#113800=DIRECTION('',(-3.85185988875507E-34,1.,0.));
#113801=DIRECTION('center_axis',(-3.85185988875507E-34,1.,0.));
#113802=DIRECTION('ref_axis',(1.,3.85185988875507E-34,0.));
#113803=DIRECTION('center_axis',(-3.85185988875507E-34,1.,0.));
#113804=DIRECTION('ref_axis',(1.,3.85185988875507E-34,0.));
#113805=DIRECTION('',(-3.85185988875507E-34,1.,0.));
#113806=DIRECTION('center_axis',(-3.85185988875507E-34,1.,0.));
#113807=DIRECTION('ref_axis',(1.,3.85185988875507E-34,0.));
#113808=DIRECTION('',(-3.85185988875507E-34,1.,0.));
#113809=DIRECTION('center_axis',(-3.85185988875507E-34,1.,0.));
#113810=DIRECTION('ref_axis',(1.,3.85185988875507E-34,0.));
#113811=DIRECTION('center_axis',(-3.85185988875507E-34,1.,0.));
#113812=DIRECTION('ref_axis',(1.,3.85185988875507E-34,0.));
#113813=DIRECTION('',(-3.85185988875507E-34,1.,0.));
#113814=DIRECTION('center_axis',(-3.85185988875507E-34,1.,0.));
#113815=DIRECTION('ref_axis',(1.,3.85185988875507E-34,0.));
#113816=DIRECTION('',(-3.85185988875507E-34,1.,0.));
#113817=DIRECTION('center_axis',(-3.85185988875507E-34,1.,0.));
#113818=DIRECTION('ref_axis',(1.,3.85185988875507E-34,0.));
#113819=DIRECTION('center_axis',(-3.85185988875507E-34,1.,0.));
#113820=DIRECTION('ref_axis',(1.,3.85185988875507E-34,0.));
#113821=DIRECTION('',(-3.85185988875507E-34,1.,0.));
#113822=DIRECTION('center_axis',(-3.85185988875507E-34,1.,0.));
#113823=DIRECTION('ref_axis',(1.,3.85185988875507E-34,0.));
#113824=DIRECTION('',(-3.85185988875507E-34,1.,0.));
#113825=DIRECTION('center_axis',(-3.85185988875507E-34,1.,0.));
#113826=DIRECTION('ref_axis',(1.,3.85185988875507E-34,0.));
#113827=DIRECTION('center_axis',(-3.85185988875507E-34,1.,0.));
#113828=DIRECTION('ref_axis',(1.,3.85185988875507E-34,0.));
#113829=DIRECTION('',(-3.85185988875507E-34,1.,0.));
#113830=DIRECTION('center_axis',(-3.85185988875507E-34,1.,0.));
#113831=DIRECTION('ref_axis',(1.,3.85185988875507E-34,0.));
#113832=DIRECTION('',(-3.85185988875507E-34,1.,0.));
#113833=DIRECTION('center_axis',(-3.85185988875507E-34,1.,0.));
#113834=DIRECTION('ref_axis',(1.,3.85185988875507E-34,0.));
#113835=DIRECTION('center_axis',(-3.85185988875507E-34,1.,0.));
#113836=DIRECTION('ref_axis',(1.,3.85185988875507E-34,0.));
#113837=DIRECTION('',(-3.85185988875507E-34,1.,0.));
#113838=DIRECTION('center_axis',(-3.85185988875507E-34,1.,0.));
#113839=DIRECTION('ref_axis',(1.,3.85185988875507E-34,0.));
#113840=DIRECTION('center_axis',(-3.85185988875507E-34,1.,0.));
#113841=DIRECTION('ref_axis',(1.,3.85185988875507E-34,0.));
#113842=DIRECTION('',(-3.85185988875507E-34,1.,0.));
#113843=DIRECTION('center_axis',(-3.85185988875507E-34,1.,0.));
#113844=DIRECTION('ref_axis',(1.,3.85185988875507E-34,0.));
#113845=DIRECTION('center_axis',(-3.85185988875507E-34,1.,0.));
#113846=DIRECTION('ref_axis',(1.,3.85185988875507E-34,0.));
#113847=DIRECTION('',(-3.85185988875507E-34,1.,0.));
#113848=DIRECTION('center_axis',(-3.85185988875507E-34,1.,0.));
#113849=DIRECTION('ref_axis',(1.,3.85185988875507E-34,0.));
#113850=DIRECTION('',(-3.85185988875507E-34,1.,0.));
#113851=DIRECTION('center_axis',(-3.85185988875507E-34,1.,0.));
#113852=DIRECTION('ref_axis',(1.,3.85185988875507E-34,0.));
#113853=DIRECTION('center_axis',(-3.85185988875507E-34,1.,0.));
#113854=DIRECTION('ref_axis',(1.,3.85185988875507E-34,0.));
#113855=DIRECTION('',(-3.85185988875507E-34,1.,0.));
#113856=DIRECTION('center_axis',(-3.85185988875507E-34,1.,0.));
#113857=DIRECTION('ref_axis',(1.,3.85185988875507E-34,0.));
#113858=DIRECTION('',(-3.85185988875507E-34,1.,0.));
#113859=DIRECTION('center_axis',(-3.85185988875507E-34,1.,0.));
#113860=DIRECTION('ref_axis',(1.,3.85185988875507E-34,0.));
#113861=DIRECTION('center_axis',(-3.85185988875507E-34,1.,0.));
#113862=DIRECTION('ref_axis',(1.,3.85185988875507E-34,0.));
#113863=DIRECTION('',(-3.85185988875507E-34,1.,0.));
#113864=DIRECTION('center_axis',(-3.85185988875507E-34,1.,0.));
#113865=DIRECTION('ref_axis',(1.,3.85185988875507E-34,0.));
#113866=DIRECTION('',(-3.85185988875507E-34,1.,0.));
#113867=DIRECTION('center_axis',(-3.85185988875507E-34,1.,0.));
#113868=DIRECTION('ref_axis',(1.,3.85185988875507E-34,0.));
#113869=DIRECTION('center_axis',(-3.85185988875507E-34,1.,0.));
#113870=DIRECTION('ref_axis',(1.,3.85185988875507E-34,0.));
#113871=DIRECTION('',(-3.85185988875507E-34,1.,0.));
#113872=DIRECTION('center_axis',(-3.85185988875507E-34,1.,0.));
#113873=DIRECTION('ref_axis',(1.,3.85185988875507E-34,0.));
#113874=DIRECTION('',(-3.85185988875507E-34,1.,0.));
#113875=DIRECTION('center_axis',(-3.85185988875507E-34,1.,0.));
#113876=DIRECTION('ref_axis',(1.,3.85185988875507E-34,0.));
#113877=DIRECTION('center_axis',(-3.85185988875507E-34,1.,0.));
#113878=DIRECTION('ref_axis',(1.,3.85185988875507E-34,0.));
#113879=DIRECTION('',(-3.85185988875507E-34,1.,0.));
#113880=DIRECTION('center_axis',(-3.85185988875507E-34,1.,0.));
#113881=DIRECTION('ref_axis',(1.,3.85185988875507E-34,0.));
#113882=DIRECTION('center_axis',(-3.85185988875507E-34,1.,0.));
#113883=DIRECTION('ref_axis',(1.,3.85185988875507E-34,0.));
#113884=DIRECTION('',(-3.85185988875507E-34,1.,0.));
#113885=DIRECTION('center_axis',(-3.85185988875507E-34,1.,0.));
#113886=DIRECTION('ref_axis',(1.,3.85185988875507E-34,0.));
#113887=DIRECTION('center_axis',(-3.85185988875507E-34,1.,0.));
#113888=DIRECTION('ref_axis',(1.,3.85185988875507E-34,0.));
#113889=DIRECTION('',(-3.85185988875507E-34,1.,0.));
#113890=DIRECTION('center_axis',(-3.85185988875507E-34,1.,0.));
#113891=DIRECTION('ref_axis',(1.,3.85185988875507E-34,0.));
#113892=DIRECTION('',(-3.85185988875507E-34,1.,0.));
#113893=DIRECTION('center_axis',(-3.85185988875507E-34,1.,0.));
#113894=DIRECTION('ref_axis',(1.,3.85185988875507E-34,0.));
#113895=DIRECTION('center_axis',(-3.85185988875507E-34,1.,0.));
#113896=DIRECTION('ref_axis',(1.,3.85185988875507E-34,0.));
#113897=DIRECTION('',(-3.85185988875507E-34,1.,0.));
#113898=DIRECTION('center_axis',(-3.85185988875507E-34,1.,0.));
#113899=DIRECTION('ref_axis',(1.,3.85185988875507E-34,0.));
#113900=DIRECTION('',(-3.85185988875507E-34,1.,0.));
#113901=DIRECTION('center_axis',(-3.85185988875507E-34,1.,0.));
#113902=DIRECTION('ref_axis',(1.,3.85185988875507E-34,0.));
#113903=DIRECTION('center_axis',(-3.85185988875507E-34,1.,0.));
#113904=DIRECTION('ref_axis',(1.,3.85185988875507E-34,0.));
#113905=DIRECTION('',(-3.85185988875507E-34,1.,0.));
#113906=DIRECTION('center_axis',(-3.85185988875507E-34,1.,0.));
#113907=DIRECTION('ref_axis',(1.,3.85185988875507E-34,0.));
#113908=DIRECTION('',(-3.85185988875507E-34,1.,0.));
#113909=DIRECTION('center_axis',(-3.85185988875507E-34,1.,0.));
#113910=DIRECTION('ref_axis',(1.,3.85185988875507E-34,0.));
#113911=DIRECTION('center_axis',(-3.85185988875507E-34,1.,0.));
#113912=DIRECTION('ref_axis',(1.,3.85185988875507E-34,0.));
#113913=DIRECTION('',(-3.85185988875507E-34,1.,0.));
#113914=DIRECTION('center_axis',(-3.85185988875507E-34,1.,0.));
#113915=DIRECTION('ref_axis',(1.,3.85185988875507E-34,0.));
#113916=DIRECTION('',(-3.85185988875507E-34,1.,0.));
#113917=DIRECTION('center_axis',(-3.85185988875507E-34,1.,0.));
#113918=DIRECTION('ref_axis',(1.,3.85185988875507E-34,0.));
#113919=DIRECTION('center_axis',(-3.85185988875507E-34,1.,0.));
#113920=DIRECTION('ref_axis',(1.,3.85185988875507E-34,0.));
#113921=DIRECTION('center_axis',(3.85185988875507E-34,-1.,0.));
#113922=DIRECTION('ref_axis',(-1.,-3.85185988875507E-34,0.));
#113923=DIRECTION('center_axis',(3.85185988875507E-34,-1.,0.));
#113924=DIRECTION('ref_axis',(-1.,-3.85185988875507E-34,0.));
#113925=DIRECTION('center_axis',(3.85185988875507E-34,-1.,0.));
#113926=DIRECTION('ref_axis',(-1.,-3.85185988875507E-34,0.));
#113927=DIRECTION('center_axis',(0.333333332905692,1.28395329460448E-34,
-0.942809041733257));
#113928=DIRECTION('ref_axis',(-0.942809041733257,-3.63156833060794E-34,
-0.333333332905692));
#113929=DIRECTION('',(3.85185988875507E-34,-1.,0.));
#113930=DIRECTION('',(-0.942809041733257,-3.63156833060794E-34,-0.333333332905692));
#113931=DIRECTION('',(0.942809041733257,3.63156833060794E-34,0.333333332905692));
#113932=DIRECTION('center_axis',(3.85185988875507E-34,-1.,0.));
#113933=DIRECTION('ref_axis',(-1.,-3.85185988875507E-34,0.));
#113934=DIRECTION('',(3.85185988875507E-34,-1.,0.));
#113935=DIRECTION('center_axis',(3.85185988875507E-34,-1.,0.));
#113936=DIRECTION('ref_axis',(0.,0.,-1.));
#113937=DIRECTION('center_axis',(-3.85185988875507E-34,1.,0.));
#113938=DIRECTION('ref_axis',(0.,0.,-1.));
#113939=DIRECTION('center_axis',(3.85185988875507E-34,-1.,0.));
#113940=DIRECTION('ref_axis',(-1.,-3.85185988875507E-34,0.));
#113941=DIRECTION('',(3.85185988875507E-34,-1.,0.));
#113942=DIRECTION('center_axis',(-3.85185988875507E-34,1.,0.));
#113943=DIRECTION('ref_axis',(0.,0.,-1.));
#113944=DIRECTION('center_axis',(3.85185988875507E-34,-1.,0.));
#113945=DIRECTION('ref_axis',(0.,0.,-1.));
#113946=DIRECTION('center_axis',(3.85185988875507E-34,-1.,0.));
#113947=DIRECTION('ref_axis',(-1.,-3.85185988875507E-34,0.));
#113948=DIRECTION('',(3.85185988875507E-34,-1.,0.));
#113949=DIRECTION('center_axis',(3.85185988875507E-34,-1.,0.));
#113950=DIRECTION('ref_axis',(0.,0.,-1.));
#113951=DIRECTION('center_axis',(-3.85185988875507E-34,1.,0.));
#113952=DIRECTION('ref_axis',(0.,0.,-1.));
#113953=DIRECTION('center_axis',(-0.333333332905692,-1.28395329460448E-34,
-0.942809041733257));
#113954=DIRECTION('ref_axis',(-0.942809041733257,-3.63156833060794E-34,
0.333333332905692));
#113955=DIRECTION('',(3.85185988875507E-34,-1.,0.));
#113956=DIRECTION('',(-0.942809041733257,-3.63156833060794E-34,0.333333332905692));
#113957=DIRECTION('',(0.942809041733257,3.63156833060794E-34,-0.333333332905692));
#113958=DIRECTION('center_axis',(3.85185988875507E-34,-1.,0.));
#113959=DIRECTION('ref_axis',(0.91465912113048,3.52313878056646E-34,0.404226040889028));
#113960=DIRECTION('',(3.85185988875507E-34,-1.,0.));
#113961=DIRECTION('center_axis',(-3.85185988875507E-34,1.,0.));
#113962=DIRECTION('ref_axis',(0.,0.,-1.));
#113963=DIRECTION('center_axis',(3.85185988875507E-34,-1.,0.));
#113964=DIRECTION('ref_axis',(-1.,-3.85185988875507E-34,0.));
#113965=DIRECTION('center_axis',(3.85185988875507E-34,-1.,0.));
#113966=DIRECTION('ref_axis',(0.,0.,-1.));
#113967=DIRECTION('center_axis',(-3.85185988875507E-34,1.,0.));
#113968=DIRECTION('ref_axis',(0.,0.,-1.));
#113969=DIRECTION('center_axis',(-3.85185988875507E-34,1.,0.));
#113970=DIRECTION('ref_axis',(1.,3.85185988875507E-34,0.));
#113971=DIRECTION('center_axis',(3.85185988875507E-34,-1.,0.));
#113972=DIRECTION('ref_axis',(-1.,-3.85185988875507E-34,0.));
#113973=DIRECTION('',(3.85185988875507E-34,-1.,0.));
#113974=DIRECTION('center_axis',(3.85185988875507E-34,-1.,0.));
#113975=DIRECTION('ref_axis',(0.,0.,-1.));
#113976=DIRECTION('',(3.85185988875507E-34,-1.,0.));
#113977=DIRECTION('center_axis',(-3.85185988875507E-34,1.,0.));
#113978=DIRECTION('ref_axis',(0.,0.,-1.));
#113979=DIRECTION('center_axis',(0.333333332905692,1.28395329460448E-34,
0.942809041733257));
#113980=DIRECTION('ref_axis',(0.942809041733257,3.63156833060794E-34,-0.333333332905692));
#113981=DIRECTION('',(0.942809041733257,3.63156833060794E-34,-0.333333332905692));
#113982=DIRECTION('',(-0.942809041733257,-3.63156833060794E-34,0.333333332905692));
#113983=DIRECTION('center_axis',(3.85185988875507E-34,-1.,0.));
#113984=DIRECTION('ref_axis',(-1.,-3.85185988875507E-34,0.));
#113985=DIRECTION('',(3.85185988875507E-34,-1.,0.));
#113986=DIRECTION('center_axis',(3.85185988875507E-34,-1.,0.));
#113987=DIRECTION('ref_axis',(0.,0.,-1.));
#113988=DIRECTION('center_axis',(-3.85185988875507E-34,1.,0.));
#113989=DIRECTION('ref_axis',(0.,0.,-1.));
#113990=DIRECTION('center_axis',(3.85185988875507E-34,-1.,0.));
#113991=DIRECTION('ref_axis',(0.914659120962055,3.52313877991771E-34,-0.40422604127013));
#113992=DIRECTION('',(3.85185988875507E-34,-1.,0.));
#113993=DIRECTION('center_axis',(-3.85185988875507E-34,1.,0.));
#113994=DIRECTION('ref_axis',(0.,0.,-1.));
#113995=DIRECTION('center_axis',(-0.333333332905692,-1.28395329460448E-34,
0.942809041733257));
#113996=DIRECTION('ref_axis',(0.942809041733257,3.63156833060794E-34,0.333333332905692));
#113997=DIRECTION('',(3.85185988875507E-34,-1.,0.));
#113998=DIRECTION('',(0.942809041733257,3.63156833060794E-34,0.333333332905692));
#113999=DIRECTION('',(-0.942809041733257,-3.63156833060794E-34,-0.333333332905692));
#114000=DIRECTION('center_axis',(3.85185988875507E-34,-1.,0.));
#114001=DIRECTION('ref_axis',(-1.,-3.85185988875507E-34,0.));
#114002=DIRECTION('',(3.85185988875507E-34,-1.,0.));
#114003=DIRECTION('center_axis',(3.85185988875507E-34,-1.,0.));
#114004=DIRECTION('ref_axis',(0.,0.,-1.));
#114005=DIRECTION('center_axis',(-3.85185988875507E-34,1.,0.));
#114006=DIRECTION('ref_axis',(0.,0.,-1.));
#114007=DIRECTION('center_axis',(3.85185988875507E-34,-1.,0.));
#114008=DIRECTION('ref_axis',(-1.,-3.85185988875507E-34,0.));
#114009=DIRECTION('center_axis',(-3.85185988875507E-34,1.,0.));
#114010=DIRECTION('ref_axis',(0.,0.,-1.));
#114011=DIRECTION('center_axis',(3.85185988875507E-34,-1.,0.));
#114012=DIRECTION('ref_axis',(0.,0.,-1.));
#114013=DIRECTION('center_axis',(3.85185988875507E-34,-1.,0.));
#114014=DIRECTION('ref_axis',(-1.,-3.85185988875507E-34,0.));
#114015=DIRECTION('center_axis',(-3.85185988875507E-34,1.,0.));
#114016=DIRECTION('ref_axis',(-0.914659120976061,0.,0.404226041238437));
#114017=DIRECTION('center_axis',(0.388215488117679,1.49535166687396E-34,
-0.921568627279354));
#114018=DIRECTION('ref_axis',(-0.921568627279354,-3.54975323015241E-34,
-0.388215488117679));
#114019=DIRECTION('center_axis',(0.942809041733257,3.63156833060794E-34,
0.333333332905692));
#114020=DIRECTION('ref_axis',(-0.333333332905692,-1.28395329460448E-34,
0.942809041733257));
#114021=DIRECTION('center_axis',(-0.942809041733257,-3.63156833060794E-34,
-0.333333332905692));
#114022=DIRECTION('ref_axis',(0.235702261544926,-0.707106776831155,-0.666666670879881));
#114023=DIRECTION('center_axis',(0.942809041733257,3.63156833060794E-34,
0.333333332905692));
#114024=DIRECTION('ref_axis',(-0.333333332905692,-1.28395329460448E-34,
0.942809041733257));
#114025=DIRECTION('center_axis',(-3.85185988875507E-34,1.,0.));
#114026=DIRECTION('ref_axis',(1.,0.,0.));
#114027=DIRECTION('center_axis',(-3.85185988875507E-34,1.,0.));
#114028=DIRECTION('ref_axis',(1.,0.,0.));
#114029=DIRECTION('center_axis',(0.402255287051866,1.54943100523474E-34,
-0.915527544118046));
#114030=DIRECTION('ref_axis',(-0.915527544118046,-3.52648382423874E-34,
-0.402255287051866));
#114031=DIRECTION('center_axis',(-3.85185988875507E-34,1.,0.));
#114032=DIRECTION('ref_axis',(1.,0.,0.));
#114033=DIRECTION('center_axis',(0.402255287051866,1.54943100523474E-34,
0.915527544118046));
#114034=DIRECTION('ref_axis',(-0.915527544118046,-3.52648382423874E-34,
0.402255287051866));
#114035=DIRECTION('center_axis',(-0.942809041733257,-3.63156833060794E-34,
0.333333332905692));
#114036=DIRECTION('ref_axis',(0.333333332905692,1.28395329460448E-34,0.942809041733257));
#114037=DIRECTION('center_axis',(-0.942809041307877,-3.63156832896943E-34,
0.333333334108851));
#114038=DIRECTION('ref_axis',(0.333333334108851,1.28395329923887E-34,0.942809041307877));
#114039=DIRECTION('center_axis',(-3.85185988875507E-34,1.,0.));
#114040=DIRECTION('ref_axis',(1.,0.,0.));
#114041=DIRECTION('center_axis',(-3.85185988875507E-34,1.,0.));
#114042=DIRECTION('ref_axis',(1.,0.,0.));
#114043=DIRECTION('center_axis',(0.942809041733257,3.63156833060794E-34,
0.333333332905692));
#114044=DIRECTION('ref_axis',(0.333333332905692,1.28395329460448E-34,-0.942809041733257));
#114045=DIRECTION('center_axis',(-0.402255287051866,-1.54943100523474E-34,
0.915527544118046));
#114046=DIRECTION('ref_axis',(0.915527544118046,3.52648382423874E-34,0.402255287051866));
#114047=DIRECTION('center_axis',(-3.85185988875507E-34,1.,0.));
#114048=DIRECTION('ref_axis',(1.,0.,0.));
#114049=DIRECTION('center_axis',(-0.402255287051866,-1.54943100523474E-34,
-0.915527544118046));
#114050=DIRECTION('ref_axis',(0.915527544118046,3.52648382423874E-34,-0.402255287051866));
#114051=DIRECTION('center_axis',(0.942809041733257,3.63156833060794E-34,
0.333333332905692));
#114052=DIRECTION('ref_axis',(0.333333332905692,1.28395329460448E-34,-0.942809041733257));
#114053=DIRECTION('center_axis',(-3.85185988875507E-34,1.,0.));
#114054=DIRECTION('ref_axis',(1.,0.,0.));
#114055=DIRECTION('center_axis',(-0.942809041733257,-3.63156833060794E-34,
0.333333332905692));
#114056=DIRECTION('ref_axis',(-0.333333332905692,-1.28395329460448E-34,
-0.942809041733257));
#114057=DIRECTION('center_axis',(0.942809041733257,3.63156833060794E-34,
-0.333333332905692));
#114058=DIRECTION('ref_axis',(-0.333333332905692,-1.28395329460448E-34,
-0.942809041733257));
#114059=DIRECTION('center_axis',(-0.942809041733257,-3.63156833060794E-34,
0.333333332905692));
#114060=DIRECTION('ref_axis',(-0.333333332905692,-1.28395329460448E-34,
-0.942809041733257));
#114061=DIRECTION('center_axis',(-3.85185988875507E-34,1.,0.));
#114062=DIRECTION('ref_axis',(1.,0.,0.));
#114063=DIRECTION('center_axis',(-0.388215488966968,-1.4953516701453E-34,
-0.921568626921586));
#114064=DIRECTION('ref_axis',(-0.921568626921586,-3.54975322877434E-34,
0.388215488966968));
#114065=DIRECTION('center_axis',(-3.85185988875507E-34,1.,0.));
#114066=DIRECTION('ref_axis',(-0.914659121133649,0.,-0.404226040881857));
#114067=DIRECTION('center_axis',(-3.85185988875507E-34,1.,0.));
#114068=DIRECTION('ref_axis',(1.,3.85185988875507E-34,0.));
#114069=DIRECTION('center_axis',(-3.85185988875507E-34,1.,0.));
#114070=DIRECTION('ref_axis',(1.,3.85185988875507E-34,0.));
#114071=DIRECTION('axis',(0.,0.,1.));
#114072=DIRECTION('refdir',(1.,0.,0.));
#114073=DIRECTION('center_axis',(5.13675726285535E-34,-1.,-1.22464674570954E-16));
#114074=DIRECTION('ref_axis',(0.0618200639786049,1.22230437692711E-16,-0.998087310654575));
#114075=DIRECTION('center_axis',(5.13675726285535E-34,-1.,-1.22464674570954E-16));
#114076=DIRECTION('ref_axis',(-0.93969262091562,4.18853855054451E-17,-0.342020142969288));
#114077=DIRECTION('',(5.13675726285535E-34,-1.,-1.22464674570954E-16));
#114078=DIRECTION('center_axis',(5.13675726285535E-34,-1.,-1.22464674570954E-16));
#114079=DIRECTION('ref_axis',(-0.93969262091562,4.18853855054451E-17,-0.342020142969288));
#114080=DIRECTION('',(5.13675726285535E-34,-1.,-1.22464674570954E-16));
#114081=DIRECTION('',(5.13675726285535E-34,-1.,-1.22464674570954E-16));
#114082=DIRECTION('',(-5.13675726285535E-34,1.,1.22464674570954E-16));
#114083=DIRECTION('center_axis',(5.13675726285535E-34,-1.,-1.22464674570954E-16));
#114084=DIRECTION('ref_axis',(0.0784590959774507,1.22087156847365E-16,-0.996917333713484));
#114085=DIRECTION('',(5.13675726285535E-34,-1.,-1.22464674570954E-16));
#114086=DIRECTION('center_axis',(5.13675726285535E-34,-1.,-1.22464674570954E-16));
#114087=DIRECTION('ref_axis',(-0.93969262091562,4.18853855054451E-17,-0.342020142969288));
#114088=DIRECTION('center_axis',(5.13675726285535E-34,-1.,-1.22464674570954E-16));
#114089=DIRECTION('ref_axis',(-0.93969262091562,4.18853855054451E-17,-0.342020142969288));
#114090=DIRECTION('center_axis',(5.13675726285535E-34,-1.,-1.22464674570954E-16));
#114091=DIRECTION('ref_axis',(0.203233458912656,1.1990887460271E-16,-0.979130308579199));
#114092=DIRECTION('center_axis',(5.13675726285535E-34,-1.,-1.22464674570954E-16));
#114093=DIRECTION('ref_axis',(-0.93969262091562,4.18853855054451E-17,-0.342020142969288));
#114094=DIRECTION('',(5.13675726285535E-34,-1.,-1.22464674570954E-16));
#114095=DIRECTION('center_axis',(5.13675726285535E-34,-1.,-1.22464674570954E-16));
#114096=DIRECTION('ref_axis',(-0.93969262091562,4.18853855054451E-17,-0.342020142969288));
#114097=DIRECTION('',(5.13675726285535E-34,-1.,-1.22464674570954E-16));
#114098=DIRECTION('',(-5.13675726285535E-34,1.,1.22464674570954E-16));
#114099=DIRECTION('center_axis',(5.13675726285535E-34,-1.,-1.22464674570954E-16));
#114100=DIRECTION('ref_axis',(0.0784590959774507,1.22087156847365E-16,-0.996917333713484));
#114101=DIRECTION('',(5.13675726285535E-34,-1.,-1.22464674570954E-16));
#114102=DIRECTION('center_axis',(5.13675726285535E-34,-1.,-1.22464674570954E-16));
#114103=DIRECTION('ref_axis',(-0.93969262091562,4.18853855054451E-17,-0.342020142969288));
#114104=DIRECTION('center_axis',(5.13675726285535E-34,-1.,-1.22464674570954E-16));
#114105=DIRECTION('ref_axis',(-0.93969262091562,4.18853855054451E-17,-0.342020142969288));
#114106=DIRECTION('center_axis',(5.13675726285535E-34,-1.,-1.22464674570954E-16));
#114107=DIRECTION('ref_axis',(0.340509606979888,1.1514631260766E-16,-0.940241036944465));
#114108=DIRECTION('center_axis',(5.13675726285535E-34,-1.,-1.22464674570954E-16));
#114109=DIRECTION('ref_axis',(-0.93969262091562,4.18853855054451E-17,-0.342020142969288));
#114110=DIRECTION('',(5.13675726285535E-34,-1.,-1.22464674570954E-16));
#114111=DIRECTION('center_axis',(5.13675726285535E-34,-1.,-1.22464674570954E-16));
#114112=DIRECTION('ref_axis',(-0.93969262091562,4.18853855054451E-17,-0.342020142969288));
#114113=DIRECTION('',(5.13675726285535E-34,-1.,-1.22464674570954E-16));
#114114=DIRECTION('',(-5.13675726285535E-34,1.,1.22464674570954E-16));
#114115=DIRECTION('center_axis',(5.13675726285535E-34,-1.,-1.22464674570954E-16));
#114116=DIRECTION('ref_axis',(0.0784590959774507,1.22087156847365E-16,-0.996917333713484));
#114117=DIRECTION('',(5.13675726285535E-34,-1.,-1.22464674570954E-16));
#114118=DIRECTION('center_axis',(5.13675726285535E-34,-1.,-1.22464674570954E-16));
#114119=DIRECTION('ref_axis',(-0.93969262091562,4.18853855054451E-17,-0.342020142969288));
#114120=DIRECTION('center_axis',(5.13675726285535E-34,-1.,-1.22464674570954E-16));
#114121=DIRECTION('ref_axis',(-0.93969262091562,4.18853855054451E-17,-0.342020142969288));
#114122=DIRECTION('center_axis',(5.13675726285535E-34,-1.,-1.22464674570954E-16));
#114123=DIRECTION('ref_axis',(0.470853961165332,1.08039703752382E-16,-0.882211169309773));
#114124=DIRECTION('center_axis',(5.13675726285535E-34,-1.,-1.22464674570954E-16));
#114125=DIRECTION('ref_axis',(-0.93969262091562,4.18853855054451E-17,-0.342020142969288));
#114126=DIRECTION('',(5.13675726285535E-34,-1.,-1.22464674570954E-16));
#114127=DIRECTION('center_axis',(5.13675726285535E-34,-1.,-1.22464674570954E-16));
#114128=DIRECTION('ref_axis',(-0.93969262091562,4.18853855054451E-17,-0.342020142969288));
#114129=DIRECTION('',(5.13675726285535E-34,-1.,-1.22464674570954E-16));
#114130=DIRECTION('',(-5.13675726285535E-34,1.,1.22464674570954E-16));
#114131=DIRECTION('center_axis',(5.13675726285535E-34,-1.,-1.22464674570954E-16));
#114132=DIRECTION('ref_axis',(0.0784590959774507,1.22087156847365E-16,-0.996917333713484));
#114133=DIRECTION('',(5.13675726285535E-34,-1.,-1.22464674570954E-16));
#114134=DIRECTION('center_axis',(5.13675726285535E-34,-1.,-1.22464674570954E-16));
#114135=DIRECTION('ref_axis',(-0.93969262091562,4.18853855054451E-17,-0.342020142969288));
#114136=DIRECTION('center_axis',(5.13675726285535E-34,-1.,-1.22464674570954E-16));
#114137=DIRECTION('ref_axis',(-0.93969262091562,4.18853855054451E-17,-0.342020142969288));
#114138=DIRECTION('center_axis',(5.13675726285535E-34,-1.,-1.22464674570954E-16));
#114139=DIRECTION('ref_axis',(0.591613087024489,9.87337180501123E-17,-0.806222026033372));
#114140=DIRECTION('center_axis',(5.13675726285535E-34,-1.,-1.22464674570954E-16));
#114141=DIRECTION('ref_axis',(-0.93969262091562,4.18853855054451E-17,-0.342020142969288));
#114142=DIRECTION('',(5.13675726285535E-34,-1.,-1.22464674570954E-16));
#114143=DIRECTION('center_axis',(5.13675726285535E-34,-1.,-1.22464674570954E-16));
#114144=DIRECTION('ref_axis',(-0.93969262091562,4.18853855054451E-17,-0.342020142969288));
#114145=DIRECTION('',(5.13675726285535E-34,-1.,-1.22464674570954E-16));
#114146=DIRECTION('',(-5.13675726285535E-34,1.,1.22464674570954E-16));
#114147=DIRECTION('center_axis',(5.13675726285535E-34,-1.,-1.22464674570954E-16));
#114148=DIRECTION('ref_axis',(0.0784590959774507,1.22087156847365E-16,-0.996917333713484));
#114149=DIRECTION('',(5.13675726285535E-34,-1.,-1.22464674570954E-16));
#114150=DIRECTION('center_axis',(5.13675726285535E-34,-1.,-1.22464674570954E-16));
#114151=DIRECTION('ref_axis',(-0.93969262091562,4.18853855054451E-17,-0.342020142969288));
#114152=DIRECTION('center_axis',(5.13675726285535E-34,-1.,-1.22464674570954E-16));
#114153=DIRECTION('ref_axis',(-0.93969262091562,4.18853855054451E-17,-0.342020142969288));
#114154=DIRECTION('center_axis',(5.13675726285535E-34,-1.,-1.22464674570954E-16));
#114155=DIRECTION('ref_axis',(0.700328675782159,8.74177986363949E-17,-0.713820527777962));
#114156=DIRECTION('center_axis',(5.13675726285535E-34,-1.,-1.22464674570954E-16));
#114157=DIRECTION('ref_axis',(-0.93969262091562,4.18853855054451E-17,-0.342020142969288));
#114158=DIRECTION('',(5.13675726285535E-34,-1.,-1.22464674570954E-16));
#114159=DIRECTION('center_axis',(5.13675726285535E-34,-1.,-1.22464674570954E-16));
#114160=DIRECTION('ref_axis',(-0.93969262091562,4.18853855054451E-17,-0.342020142969288));
#114161=DIRECTION('',(5.13675726285535E-34,-1.,-1.22464674570954E-16));
#114162=DIRECTION('',(-5.13675726285535E-34,1.,1.22464674570954E-16));
#114163=DIRECTION('center_axis',(5.13675726285535E-34,-1.,-1.22464674570954E-16));
#114164=DIRECTION('ref_axis',(0.0784590959774507,1.22087156847365E-16,-0.996917333713484));
#114165=DIRECTION('',(5.13675726285535E-34,-1.,-1.22464674570954E-16));
#114166=DIRECTION('center_axis',(5.13675726285535E-34,-1.,-1.22464674570954E-16));
#114167=DIRECTION('ref_axis',(-0.93969262091562,4.18853855054451E-17,-0.342020142969288));
#114168=DIRECTION('center_axis',(5.13675726285535E-34,-1.,-1.22464674570954E-16));
#114169=DIRECTION('ref_axis',(-0.93969262091562,4.18853855054451E-17,-0.342020142969288));
#114170=DIRECTION('center_axis',(5.13675726285535E-34,-1.,-1.22464674570954E-16));
#114171=DIRECTION('ref_axis',(0.794787592671922,7.4322304895865E-17,-0.606887701749485));
#114172=DIRECTION('center_axis',(5.13675726285535E-34,-1.,-1.22464674570954E-16));
#114173=DIRECTION('ref_axis',(-0.93969262091562,4.18853855054451E-17,-0.342020142969288));
#114174=DIRECTION('',(5.13675726285535E-34,-1.,-1.22464674570954E-16));
#114175=DIRECTION('center_axis',(5.13675726285535E-34,-1.,-1.22464674570954E-16));
#114176=DIRECTION('ref_axis',(-0.93969262091562,4.18853855054451E-17,-0.342020142969288));
#114177=DIRECTION('',(5.13675726285535E-34,-1.,-1.22464674570954E-16));
#114178=DIRECTION('',(-5.13675726285535E-34,1.,1.22464674570954E-16));
#114179=DIRECTION('center_axis',(5.13675726285535E-34,-1.,-1.22464674570954E-16));
#114180=DIRECTION('ref_axis',(0.0784590959774507,1.22087156847365E-16,-0.996917333713484));
#114181=DIRECTION('',(5.13675726285535E-34,-1.,-1.22464674570954E-16));
#114182=DIRECTION('center_axis',(5.13675726285535E-34,-1.,-1.22464674570954E-16));
#114183=DIRECTION('ref_axis',(-0.93969262091562,4.18853855054451E-17,-0.342020142969288));
#114184=DIRECTION('center_axis',(5.13675726285535E-34,-1.,-1.22464674570954E-16));
#114185=DIRECTION('ref_axis',(-0.93969262091562,4.18853855054451E-17,-0.342020142969288));
#114186=DIRECTION('center_axis',(5.13675726285535E-34,-1.,-1.22464674570954E-16));
#114187=DIRECTION('ref_axis',(0.87306692619485,5.97138233402766E-17,-0.487600392108822));
#114188=DIRECTION('center_axis',(5.13675726285535E-34,-1.,-1.22464674570954E-16));
#114189=DIRECTION('ref_axis',(-0.93969262091562,4.18853855054451E-17,-0.342020142969288));
#114190=DIRECTION('',(5.13675726285535E-34,-1.,-1.22464674570954E-16));
#114191=DIRECTION('center_axis',(5.13675726285535E-34,-1.,-1.22464674570954E-16));
#114192=DIRECTION('ref_axis',(-0.93969262091562,4.18853855054451E-17,-0.342020142969288));
#114193=DIRECTION('',(5.13675726285535E-34,-1.,-1.22464674570954E-16));
#114194=DIRECTION('',(-5.13675726285535E-34,1.,1.22464674570954E-16));
#114195=DIRECTION('center_axis',(5.13675726285535E-34,-1.,-1.22464674570954E-16));
#114196=DIRECTION('ref_axis',(0.0784590959774507,1.22087156847365E-16,-0.996917333713484));
#114197=DIRECTION('',(5.13675726285535E-34,-1.,-1.22464674570954E-16));
#114198=DIRECTION('center_axis',(5.13675726285535E-34,-1.,-1.22464674570954E-16));
#114199=DIRECTION('ref_axis',(-0.93969262091562,4.18853855054451E-17,-0.342020142969288));
#114200=DIRECTION('center_axis',(5.13675726285535E-34,-1.,-1.22464674570954E-16));
#114201=DIRECTION('ref_axis',(-0.93969262091562,4.18853855054451E-17,-0.342020142969288));
#114202=DIRECTION('center_axis',(5.13675726285535E-34,-1.,-1.22464674570954E-16));
#114203=DIRECTION('ref_axis',(0.933573134654503,4.38897405736607E-17,-0.358386944867368));
#114204=DIRECTION('center_axis',(5.13675726285535E-34,-1.,-1.22464674570954E-16));
#114205=DIRECTION('ref_axis',(-0.93969262091562,4.18853855054451E-17,-0.342020142969288));
#114206=DIRECTION('',(5.13675726285535E-34,-1.,-1.22464674570954E-16));
#114207=DIRECTION('center_axis',(5.13675726285535E-34,-1.,-1.22464674570954E-16));
#114208=DIRECTION('ref_axis',(-0.93969262091562,4.18853855054451E-17,-0.342020142969288));
#114209=DIRECTION('',(5.13675726285535E-34,-1.,-1.22464674570954E-16));
#114210=DIRECTION('',(-5.13675726285535E-34,1.,1.22464674570954E-16));
#114211=DIRECTION('center_axis',(5.13675726285535E-34,-1.,-1.22464674570954E-16));
#114212=DIRECTION('ref_axis',(0.0784590959774507,1.22087156847365E-16,-0.996917333713484));
#114213=DIRECTION('',(5.13675726285535E-34,-1.,-1.22464674570954E-16));
#114214=DIRECTION('center_axis',(5.13675726285535E-34,-1.,-1.22464674570954E-16));
#114215=DIRECTION('ref_axis',(-0.93969262091562,4.18853855054451E-17,-0.342020142969288));
#114216=DIRECTION('center_axis',(5.13675726285535E-34,-1.,-1.22464674570954E-16));
#114217=DIRECTION('ref_axis',(-0.93969262091562,4.18853855054451E-17,-0.342020142969288));
#114218=DIRECTION('center_axis',(5.13675726285535E-34,-1.,-1.22464674570954E-16));
#114219=DIRECTION('ref_axis',(0.975074486292716,2.71721892731301E-17,-0.221877773066607));
#114220=DIRECTION('center_axis',(5.13675726285535E-34,-1.,-1.22464674570954E-16));
#114221=DIRECTION('ref_axis',(-0.93969262091562,4.18853855054451E-17,-0.342020142969288));
#114222=DIRECTION('',(5.13675726285535E-34,-1.,-1.22464674570954E-16));
#114223=DIRECTION('center_axis',(5.13675726285535E-34,-1.,-1.22464674570954E-16));
#114224=DIRECTION('ref_axis',(-0.93969262091562,4.18853855054451E-17,-0.342020142969288));
#114225=DIRECTION('',(5.13675726285535E-34,-1.,-1.22464674570954E-16));
#114226=DIRECTION('',(-5.13675726285535E-34,1.,1.22464674570954E-16));
#114227=DIRECTION('center_axis',(5.13675726285535E-34,-1.,-1.22464674570954E-16));
#114228=DIRECTION('ref_axis',(0.0784590959774507,1.22087156847365E-16,-0.996917333713484));
#114229=DIRECTION('',(5.13675726285535E-34,-1.,-1.22464674570954E-16));
#114230=DIRECTION('center_axis',(5.13675726285535E-34,-1.,-1.22464674570954E-16));
#114231=DIRECTION('ref_axis',(-0.93969262091562,4.18853855054451E-17,-0.342020142969288));
#114232=DIRECTION('center_axis',(5.13675726285535E-34,-1.,-1.22464674570954E-16));
#114233=DIRECTION('ref_axis',(-0.93969262091562,4.18853855054451E-17,-0.342020142969288));
#114234=DIRECTION('center_axis',(5.13675726285535E-34,-1.,-1.22464674570954E-16));
#114235=DIRECTION('ref_axis',(0.996726133306289,9.9014906031653E-18,-0.0808518100248454));
#114236=DIRECTION('center_axis',(5.13675726285535E-34,-1.,-1.22464674570954E-16));
#114237=DIRECTION('ref_axis',(-0.93969262091562,4.18853855054451E-17,-0.342020142969288));
#114238=DIRECTION('',(5.13675726285535E-34,-1.,-1.22464674570954E-16));
#114239=DIRECTION('center_axis',(5.13675726285535E-34,-1.,-1.22464674570954E-16));
#114240=DIRECTION('ref_axis',(-0.93969262091562,4.18853855054451E-17,-0.342020142969288));
#114241=DIRECTION('',(5.13675726285535E-34,-1.,-1.22464674570954E-16));
#114242=DIRECTION('',(-5.13675726285535E-34,1.,1.22464674570954E-16));
#114243=DIRECTION('center_axis',(5.13675726285535E-34,-1.,-1.22464674570954E-16));
#114244=DIRECTION('ref_axis',(0.0784590959774507,1.22087156847365E-16,-0.996917333713484));
#114245=DIRECTION('',(5.13675726285535E-34,-1.,-1.22464674570954E-16));
#114246=DIRECTION('center_axis',(5.13675726285535E-34,-1.,-1.22464674570954E-16));
#114247=DIRECTION('ref_axis',(-0.93969262091562,4.18853855054451E-17,-0.342020142969288));
#114248=DIRECTION('center_axis',(5.13675726285535E-34,-1.,-1.22464674570954E-16));
#114249=DIRECTION('ref_axis',(-0.93969262091562,4.18853855054451E-17,-0.342020142969288));
#114250=DIRECTION('center_axis',(5.13675726285535E-34,-1.,-1.22464674570954E-16));
#114251=DIRECTION('ref_axis',(0.998087310654575,-7.57077401709542E-18,0.0618200639786049));
#114252=DIRECTION('center_axis',(5.13675726285535E-34,-1.,-1.22464674570954E-16));
#114253=DIRECTION('ref_axis',(-0.93969262091562,4.18853855054451E-17,-0.342020142969288));
#114254=DIRECTION('',(5.13675726285535E-34,-1.,-1.22464674570954E-16));
#114255=DIRECTION('center_axis',(5.13675726285535E-34,-1.,-1.22464674570954E-16));
#114256=DIRECTION('ref_axis',(-0.93969262091562,4.18853855054451E-17,-0.342020142969288));
#114257=DIRECTION('',(5.13675726285535E-34,-1.,-1.22464674570954E-16));
#114258=DIRECTION('',(-5.13675726285535E-34,1.,1.22464674570954E-16));
#114259=DIRECTION('center_axis',(5.13675726285535E-34,-1.,-1.22464674570954E-16));
#114260=DIRECTION('ref_axis',(0.0784590959774507,1.22087156847365E-16,-0.996917333713484));
#114261=DIRECTION('',(5.13675726285535E-34,-1.,-1.22464674570954E-16));
#114262=DIRECTION('center_axis',(5.13675726285535E-34,-1.,-1.22464674570954E-16));
#114263=DIRECTION('ref_axis',(-0.93969262091562,4.18853855054451E-17,-0.342020142969288));
#114264=DIRECTION('center_axis',(5.13675726285535E-34,-1.,-1.22464674570954E-16));
#114265=DIRECTION('ref_axis',(-0.93969262091562,4.18853855054451E-17,-0.342020142969288));
#114266=DIRECTION('center_axis',(5.13675726285535E-34,-1.,-1.22464674570954E-16));
#114267=DIRECTION('ref_axis',(0.979130308579199,-2.48889194076679E-17,0.203233458912656));
#114268=DIRECTION('center_axis',(5.13675726285535E-34,-1.,-1.22464674570954E-16));
#114269=DIRECTION('ref_axis',(-0.93969262091562,4.18853855054451E-17,-0.342020142969288));
#114270=DIRECTION('',(5.13675726285535E-34,-1.,-1.22464674570954E-16));
#114271=DIRECTION('center_axis',(5.13675726285535E-34,-1.,-1.22464674570954E-16));
#114272=DIRECTION('ref_axis',(-0.93969262091562,4.18853855054451E-17,-0.342020142969288));
#114273=DIRECTION('',(5.13675726285535E-34,-1.,-1.22464674570954E-16));
#114274=DIRECTION('',(-5.13675726285535E-34,1.,1.22464674570954E-16));
#114275=DIRECTION('center_axis',(5.13675726285535E-34,-1.,-1.22464674570954E-16));
#114276=DIRECTION('ref_axis',(0.0784590959774507,1.22087156847365E-16,-0.996917333713484));
#114277=DIRECTION('',(5.13675726285535E-34,-1.,-1.22464674570954E-16));
#114278=DIRECTION('center_axis',(5.13675726285535E-34,-1.,-1.22464674570954E-16));
#114279=DIRECTION('ref_axis',(-0.93969262091562,4.18853855054451E-17,-0.342020142969288));
#114280=DIRECTION('center_axis',(5.13675726285535E-34,-1.,-1.22464674570954E-16));
#114281=DIRECTION('ref_axis',(-0.93969262091562,4.18853855054451E-17,-0.342020142969288));
#114282=DIRECTION('center_axis',(5.13675726285535E-34,-1.,-1.22464674570954E-16));
#114283=DIRECTION('ref_axis',(0.940241036944465,-4.17003982070755E-17,0.340509606979888));
#114284=DIRECTION('center_axis',(5.13675726285535E-34,-1.,-1.22464674570954E-16));
#114285=DIRECTION('ref_axis',(-0.93969262091562,4.18853855054451E-17,-0.342020142969288));
#114286=DIRECTION('',(5.13675726285535E-34,-1.,-1.22464674570954E-16));
#114287=DIRECTION('center_axis',(5.13675726285535E-34,-1.,-1.22464674570954E-16));
#114288=DIRECTION('ref_axis',(-0.93969262091562,4.18853855054451E-17,-0.342020142969288));
#114289=DIRECTION('',(5.13675726285535E-34,-1.,-1.22464674570954E-16));
#114290=DIRECTION('',(-5.13675726285535E-34,1.,1.22464674570954E-16));
#114291=DIRECTION('center_axis',(5.13675726285535E-34,-1.,-1.22464674570954E-16));
#114292=DIRECTION('ref_axis',(0.0784590959774507,1.22087156847365E-16,-0.996917333713484));
#114293=DIRECTION('',(5.13675726285535E-34,-1.,-1.22464674570954E-16));
#114294=DIRECTION('center_axis',(5.13675726285535E-34,-1.,-1.22464674570954E-16));
#114295=DIRECTION('ref_axis',(-0.93969262091562,4.18853855054451E-17,-0.342020142969288));
#114296=DIRECTION('center_axis',(5.13675726285535E-34,-1.,-1.22464674570954E-16));
#114297=DIRECTION('ref_axis',(-0.93969262091562,4.18853855054451E-17,-0.342020142969288));
#114298=DIRECTION('center_axis',(5.13675726285535E-34,-1.,-1.22464674570954E-16));
#114299=DIRECTION('ref_axis',(0.882211169309773,-5.76629771245571E-17,0.470853961165332));
#114300=DIRECTION('center_axis',(5.13675726285535E-34,-1.,-1.22464674570954E-16));
#114301=DIRECTION('ref_axis',(-0.93969262091562,4.18853855054451E-17,-0.342020142969288));
#114302=DIRECTION('',(5.13675726285535E-34,-1.,-1.22464674570954E-16));
#114303=DIRECTION('center_axis',(5.13675726285535E-34,-1.,-1.22464674570954E-16));
#114304=DIRECTION('ref_axis',(-0.93969262091562,4.18853855054451E-17,-0.342020142969288));
#114305=DIRECTION('',(5.13675726285535E-34,-1.,-1.22464674570954E-16));
#114306=DIRECTION('',(-5.13675726285535E-34,1.,1.22464674570954E-16));
#114307=DIRECTION('center_axis',(5.13675726285535E-34,-1.,-1.22464674570954E-16));
#114308=DIRECTION('ref_axis',(0.0784590959774507,1.22087156847365E-16,-0.996917333713484));
#114309=DIRECTION('',(5.13675726285535E-34,-1.,-1.22464674570954E-16));
#114310=DIRECTION('center_axis',(5.13675726285535E-34,-1.,-1.22464674570954E-16));
#114311=DIRECTION('ref_axis',(-0.93969262091562,4.18853855054451E-17,-0.342020142969288));
#114312=DIRECTION('center_axis',(5.13675726285535E-34,-1.,-1.22464674570954E-16));
#114313=DIRECTION('ref_axis',(-0.93969262091562,4.18853855054451E-17,-0.342020142969288));
#114314=DIRECTION('center_axis',(5.13675726285535E-34,-1.,-1.22464674570954E-16));
#114315=DIRECTION('ref_axis',(0.806222026033372,-7.24517041743716E-17,0.591613087024489));
#114316=DIRECTION('center_axis',(5.13675726285535E-34,-1.,-1.22464674570954E-16));
#114317=DIRECTION('ref_axis',(-0.93969262091562,4.18853855054451E-17,-0.342020142969288));
#114318=DIRECTION('',(5.13675726285535E-34,-1.,-1.22464674570954E-16));
#114319=DIRECTION('center_axis',(5.13675726285535E-34,-1.,-1.22464674570954E-16));
#114320=DIRECTION('ref_axis',(-0.93969262091562,4.18853855054451E-17,-0.342020142969288));
#114321=DIRECTION('',(5.13675726285535E-34,-1.,-1.22464674570954E-16));
#114322=DIRECTION('',(-5.13675726285535E-34,1.,1.22464674570954E-16));
#114323=DIRECTION('center_axis',(5.13675726285535E-34,-1.,-1.22464674570954E-16));
#114324=DIRECTION('ref_axis',(0.0784590959774507,1.22087156847365E-16,-0.996917333713484));
#114325=DIRECTION('',(5.13675726285535E-34,-1.,-1.22464674570954E-16));
#114326=DIRECTION('center_axis',(5.13675726285535E-34,-1.,-1.22464674570954E-16));
#114327=DIRECTION('ref_axis',(-0.93969262091562,4.18853855054451E-17,-0.342020142969288));
#114328=DIRECTION('center_axis',(5.13675726285535E-34,-1.,-1.22464674570954E-16));
#114329=DIRECTION('ref_axis',(-0.93969262091562,4.18853855054451E-17,-0.342020142969288));
#114330=DIRECTION('center_axis',(5.13675726285535E-34,-1.,-1.22464674570954E-16));
#114331=DIRECTION('ref_axis',(0.713820527777962,-8.57655233723694E-17,0.700328675782159));
#114332=DIRECTION('center_axis',(5.13675726285535E-34,-1.,-1.22464674570954E-16));
#114333=DIRECTION('ref_axis',(-0.93969262091562,4.18853855054451E-17,-0.342020142969288));
#114334=DIRECTION('',(5.13675726285535E-34,-1.,-1.22464674570954E-16));
#114335=DIRECTION('center_axis',(5.13675726285535E-34,-1.,-1.22464674570954E-16));
#114336=DIRECTION('ref_axis',(-0.93969262091562,4.18853855054451E-17,-0.342020142969288));
#114337=DIRECTION('',(5.13675726285535E-34,-1.,-1.22464674570954E-16));
#114338=DIRECTION('',(-5.13675726285535E-34,1.,1.22464674570954E-16));
#114339=DIRECTION('center_axis',(5.13675726285535E-34,-1.,-1.22464674570954E-16));
#114340=DIRECTION('ref_axis',(0.0784590959774507,1.22087156847365E-16,-0.996917333713484));
#114341=DIRECTION('',(5.13675726285535E-34,-1.,-1.22464674570954E-16));
#114342=DIRECTION('center_axis',(5.13675726285535E-34,-1.,-1.22464674570954E-16));
#114343=DIRECTION('ref_axis',(-0.93969262091562,4.18853855054451E-17,-0.342020142969288));
#114344=DIRECTION('center_axis',(5.13675726285535E-34,-1.,-1.22464674570954E-16));
#114345=DIRECTION('ref_axis',(-0.93969262091562,4.18853855054451E-17,-0.342020142969288));
#114346=DIRECTION('center_axis',(5.13675726285535E-34,-1.,-1.22464674570954E-16));
#114347=DIRECTION('ref_axis',(0.606887701749485,-9.73334038895991E-17,0.794787592671922));
#114348=DIRECTION('center_axis',(5.13675726285535E-34,-1.,-1.22464674570954E-16));
#114349=DIRECTION('ref_axis',(-0.93969262091562,4.18853855054451E-17,-0.342020142969288));
#114350=DIRECTION('',(5.13675726285535E-34,-1.,-1.22464674570954E-16));
#114351=DIRECTION('center_axis',(5.13675726285535E-34,-1.,-1.22464674570954E-16));
#114352=DIRECTION('ref_axis',(-0.93969262091562,4.18853855054451E-17,-0.342020142969288));
#114353=DIRECTION('',(5.13675726285535E-34,-1.,-1.22464674570954E-16));
#114354=DIRECTION('',(-5.13675726285535E-34,1.,1.22464674570954E-16));
#114355=DIRECTION('center_axis',(5.13675726285535E-34,-1.,-1.22464674570954E-16));
#114356=DIRECTION('ref_axis',(0.0784590959774507,1.22087156847365E-16,-0.996917333713484));
#114357=DIRECTION('',(5.13675726285535E-34,-1.,-1.22464674570954E-16));
#114358=DIRECTION('center_axis',(5.13675726285535E-34,-1.,-1.22464674570954E-16));
#114359=DIRECTION('ref_axis',(-0.93969262091562,4.18853855054451E-17,-0.342020142969288));
#114360=DIRECTION('center_axis',(5.13675726285535E-34,-1.,-1.22464674570954E-16));
#114361=DIRECTION('ref_axis',(-0.93969262091562,4.18853855054451E-17,-0.342020142969288));
#114362=DIRECTION('center_axis',(5.13675726285535E-34,-1.,-1.22464674570954E-16));
#114363=DIRECTION('ref_axis',(0.487600392108822,-1.06919856995116E-16,0.87306692619485));
#114364=DIRECTION('center_axis',(5.13675726285535E-34,-1.,-1.22464674570954E-16));
#114365=DIRECTION('ref_axis',(-0.93969262091562,4.18853855054451E-17,-0.342020142969288));
#114366=DIRECTION('',(5.13675726285535E-34,-1.,-1.22464674570954E-16));
#114367=DIRECTION('center_axis',(5.13675726285535E-34,-1.,-1.22464674570954E-16));
#114368=DIRECTION('ref_axis',(-0.93969262091562,4.18853855054451E-17,-0.342020142969288));
#114369=DIRECTION('',(5.13675726285535E-34,-1.,-1.22464674570954E-16));
#114370=DIRECTION('',(-5.13675726285535E-34,1.,1.22464674570954E-16));
#114371=DIRECTION('center_axis',(5.13675726285535E-34,-1.,-1.22464674570954E-16));
#114372=DIRECTION('ref_axis',(0.0784590959774507,1.22087156847365E-16,-0.996917333713484));
#114373=DIRECTION('',(5.13675726285535E-34,-1.,-1.22464674570954E-16));
#114374=DIRECTION('center_axis',(5.13675726285535E-34,-1.,-1.22464674570954E-16));
#114375=DIRECTION('ref_axis',(-0.93969262091562,4.18853855054451E-17,-0.342020142969288));
#114376=DIRECTION('center_axis',(5.13675726285535E-34,-1.,-1.22464674570954E-16));
#114377=DIRECTION('ref_axis',(-0.93969262091562,4.18853855054451E-17,-0.342020142969288));
#114378=DIRECTION('center_axis',(5.13675726285535E-34,-1.,-1.22464674570954E-16));
#114379=DIRECTION('ref_axis',(0.358386944867368,-1.14329730123649E-16,0.933573134654503));
#114380=DIRECTION('center_axis',(5.13675726285535E-34,-1.,-1.22464674570954E-16));
#114381=DIRECTION('ref_axis',(-0.93969262091562,4.18853855054451E-17,-0.342020142969288));
#114382=DIRECTION('',(5.13675726285535E-34,-1.,-1.22464674570954E-16));
#114383=DIRECTION('center_axis',(5.13675726285535E-34,-1.,-1.22464674570954E-16));
#114384=DIRECTION('ref_axis',(-0.93969262091562,4.18853855054451E-17,-0.342020142969288));
#114385=DIRECTION('',(5.13675726285535E-34,-1.,-1.22464674570954E-16));
#114386=DIRECTION('',(-5.13675726285535E-34,1.,1.22464674570954E-16));
#114387=DIRECTION('center_axis',(5.13675726285535E-34,-1.,-1.22464674570954E-16));
#114388=DIRECTION('ref_axis',(0.0784590959774507,1.22087156847365E-16,-0.996917333713484));
#114389=DIRECTION('',(5.13675726285535E-34,-1.,-1.22464674570954E-16));
#114390=DIRECTION('center_axis',(5.13675726285535E-34,-1.,-1.22464674570954E-16));
#114391=DIRECTION('ref_axis',(-0.93969262091562,4.18853855054451E-17,-0.342020142969288));
#114392=DIRECTION('center_axis',(5.13675726285535E-34,-1.,-1.22464674570954E-16));
#114393=DIRECTION('ref_axis',(-0.93969262091562,4.18853855054451E-17,-0.342020142969288));
#114394=DIRECTION('center_axis',(5.13675726285535E-34,-1.,-1.22464674570954E-16));
#114395=DIRECTION('ref_axis',(0.221877773066607,-1.19412179646278E-16,0.975074486292716));
#114396=DIRECTION('center_axis',(5.13675726285535E-34,-1.,-1.22464674570954E-16));
#114397=DIRECTION('ref_axis',(-0.93969262091562,4.18853855054451E-17,-0.342020142969288));
#114398=DIRECTION('',(5.13675726285535E-34,-1.,-1.22464674570954E-16));
#114399=DIRECTION('center_axis',(5.13675726285535E-34,-1.,-1.22464674570954E-16));
#114400=DIRECTION('ref_axis',(-0.93969262091562,4.18853855054451E-17,-0.342020142969288));
#114401=DIRECTION('',(5.13675726285535E-34,-1.,-1.22464674570954E-16));
#114402=DIRECTION('',(-5.13675726285535E-34,1.,1.22464674570954E-16));
#114403=DIRECTION('center_axis',(5.13675726285535E-34,-1.,-1.22464674570954E-16));
#114404=DIRECTION('ref_axis',(0.0784590959774507,1.22087156847365E-16,-0.996917333713484));
#114405=DIRECTION('',(5.13675726285535E-34,-1.,-1.22464674570954E-16));
#114406=DIRECTION('center_axis',(5.13675726285535E-34,-1.,-1.22464674570954E-16));
#114407=DIRECTION('ref_axis',(-0.93969262091562,4.18853855054451E-17,-0.342020142969288));
#114408=DIRECTION('center_axis',(5.13675726285535E-34,-1.,-1.22464674570954E-16));
#114409=DIRECTION('ref_axis',(-0.93969262091562,4.18853855054451E-17,-0.342020142969288));
#114410=DIRECTION('center_axis',(5.13675726285535E-34,-1.,-1.22464674570954E-16));
#114411=DIRECTION('ref_axis',(0.0808518100248454,-1.2206374155172E-16,0.996726133306289));
#114412=DIRECTION('center_axis',(5.13675726285535E-34,-1.,-1.22464674570954E-16));
#114413=DIRECTION('ref_axis',(-0.93969262091562,4.18853855054451E-17,-0.342020142969288));
#114414=DIRECTION('',(5.13675726285535E-34,-1.,-1.22464674570954E-16));
#114415=DIRECTION('center_axis',(5.13675726285535E-34,-1.,-1.22464674570954E-16));
#114416=DIRECTION('ref_axis',(-0.93969262091562,4.18853855054451E-17,-0.342020142969288));
#114417=DIRECTION('',(5.13675726285535E-34,-1.,-1.22464674570954E-16));
#114418=DIRECTION('',(-5.13675726285535E-34,1.,1.22464674570954E-16));
#114419=DIRECTION('center_axis',(5.13675726285535E-34,-1.,-1.22464674570954E-16));
#114420=DIRECTION('ref_axis',(0.0784590959774507,1.22087156847365E-16,-0.996917333713484));
#114421=DIRECTION('',(5.13675726285535E-34,-1.,-1.22464674570954E-16));
#114422=DIRECTION('center_axis',(5.13675726285535E-34,-1.,-1.22464674570954E-16));
#114423=DIRECTION('ref_axis',(-0.93969262091562,4.18853855054451E-17,-0.342020142969288));
#114424=DIRECTION('center_axis',(5.13675726285535E-34,-1.,-1.22464674570954E-16));
#114425=DIRECTION('ref_axis',(-0.93969262091562,4.18853855054451E-17,-0.342020142969288));
#114426=DIRECTION('center_axis',(5.13675726285535E-34,-1.,-1.22464674570954E-16));
#114427=DIRECTION('ref_axis',(-0.0618200639786049,-1.22230437692711E-16,
0.998087310654575));
#114428=DIRECTION('center_axis',(5.13675726285535E-34,-1.,-1.22464674570954E-16));
#114429=DIRECTION('ref_axis',(-0.93969262091562,4.18853855054451E-17,-0.342020142969288));
#114430=DIRECTION('',(5.13675726285535E-34,-1.,-1.22464674570954E-16));
#114431=DIRECTION('center_axis',(5.13675726285535E-34,-1.,-1.22464674570954E-16));
#114432=DIRECTION('ref_axis',(-0.93969262091562,4.18853855054451E-17,-0.342020142969288));
#114433=DIRECTION('',(5.13675726285535E-34,-1.,-1.22464674570954E-16));
#114434=DIRECTION('',(-5.13675726285535E-34,1.,1.22464674570954E-16));
#114435=DIRECTION('center_axis',(5.13675726285535E-34,-1.,-1.22464674570954E-16));
#114436=DIRECTION('ref_axis',(0.0784590959774507,1.22087156847365E-16,-0.996917333713484));
#114437=DIRECTION('',(5.13675726285535E-34,-1.,-1.22464674570954E-16));
#114438=DIRECTION('center_axis',(5.13675726285535E-34,-1.,-1.22464674570954E-16));
#114439=DIRECTION('ref_axis',(-0.93969262091562,4.18853855054451E-17,-0.342020142969288));
#114440=DIRECTION('center_axis',(5.13675726285535E-34,-1.,-1.22464674570954E-16));
#114441=DIRECTION('ref_axis',(-0.93969262091562,4.18853855054451E-17,-0.342020142969288));
#114442=DIRECTION('center_axis',(5.13675726285535E-34,-1.,-1.22464674570954E-16));
#114443=DIRECTION('ref_axis',(-0.203233458912656,-1.1990887460271E-16,0.979130308579199));
#114444=DIRECTION('center_axis',(5.13675726285535E-34,-1.,-1.22464674570954E-16));
#114445=DIRECTION('ref_axis',(-0.93969262091562,4.18853855054451E-17,-0.342020142969288));
#114446=DIRECTION('',(5.13675726285535E-34,-1.,-1.22464674570954E-16));
#114447=DIRECTION('center_axis',(5.13675726285535E-34,-1.,-1.22464674570954E-16));
#114448=DIRECTION('ref_axis',(-0.93969262091562,4.18853855054451E-17,-0.342020142969288));
#114449=DIRECTION('',(5.13675726285535E-34,-1.,-1.22464674570954E-16));
#114450=DIRECTION('',(-5.13675726285535E-34,1.,1.22464674570954E-16));
#114451=DIRECTION('center_axis',(5.13675726285535E-34,-1.,-1.22464674570954E-16));
#114452=DIRECTION('ref_axis',(0.0784590959774507,1.22087156847365E-16,-0.996917333713484));
#114453=DIRECTION('',(5.13675726285535E-34,-1.,-1.22464674570954E-16));
#114454=DIRECTION('center_axis',(5.13675726285535E-34,-1.,-1.22464674570954E-16));
#114455=DIRECTION('ref_axis',(-0.93969262091562,4.18853855054451E-17,-0.342020142969288));
#114456=DIRECTION('center_axis',(5.13675726285535E-34,-1.,-1.22464674570954E-16));
#114457=DIRECTION('ref_axis',(-0.93969262091562,4.18853855054451E-17,-0.342020142969288));
#114458=DIRECTION('center_axis',(5.13675726285535E-34,-1.,-1.22464674570954E-16));
#114459=DIRECTION('ref_axis',(-0.340509606979888,-1.1514631260766E-16,0.940241036944465));
#114460=DIRECTION('center_axis',(5.13675726285535E-34,-1.,-1.22464674570954E-16));
#114461=DIRECTION('ref_axis',(-0.93969262091562,4.18853855054451E-17,-0.342020142969288));
#114462=DIRECTION('',(5.13675726285535E-34,-1.,-1.22464674570954E-16));
#114463=DIRECTION('center_axis',(5.13675726285535E-34,-1.,-1.22464674570954E-16));
#114464=DIRECTION('ref_axis',(-0.93969262091562,4.18853855054451E-17,-0.342020142969288));
#114465=DIRECTION('',(5.13675726285535E-34,-1.,-1.22464674570954E-16));
#114466=DIRECTION('',(-5.13675726285535E-34,1.,1.22464674570954E-16));
#114467=DIRECTION('center_axis',(5.13675726285535E-34,-1.,-1.22464674570954E-16));
#114468=DIRECTION('ref_axis',(0.0784590959774507,1.22087156847365E-16,-0.996917333713484));
#114469=DIRECTION('',(5.13675726285535E-34,-1.,-1.22464674570954E-16));
#114470=DIRECTION('center_axis',(5.13675726285535E-34,-1.,-1.22464674570954E-16));
#114471=DIRECTION('ref_axis',(-0.93969262091562,4.18853855054451E-17,-0.342020142969288));
#114472=DIRECTION('center_axis',(5.13675726285535E-34,-1.,-1.22464674570954E-16));
#114473=DIRECTION('ref_axis',(-0.93969262091562,4.18853855054451E-17,-0.342020142969288));
#114474=DIRECTION('center_axis',(5.13675726285535E-34,-1.,-1.22464674570954E-16));
#114475=DIRECTION('ref_axis',(-0.470853961165332,-1.08039703752382E-16,
0.882211169309773));
#114476=DIRECTION('center_axis',(5.13675726285535E-34,-1.,-1.22464674570954E-16));
#114477=DIRECTION('ref_axis',(-0.93969262091562,4.18853855054451E-17,-0.342020142969288));
#114478=DIRECTION('',(5.13675726285535E-34,-1.,-1.22464674570954E-16));
#114479=DIRECTION('center_axis',(5.13675726285535E-34,-1.,-1.22464674570954E-16));
#114480=DIRECTION('ref_axis',(-0.93969262091562,4.18853855054451E-17,-0.342020142969288));
#114481=DIRECTION('',(5.13675726285535E-34,-1.,-1.22464674570954E-16));
#114482=DIRECTION('',(-5.13675726285535E-34,1.,1.22464674570954E-16));
#114483=DIRECTION('center_axis',(5.13675726285535E-34,-1.,-1.22464674570954E-16));
#114484=DIRECTION('ref_axis',(0.0784590959774507,1.22087156847365E-16,-0.996917333713484));
#114485=DIRECTION('',(5.13675726285535E-34,-1.,-1.22464674570954E-16));
#114486=DIRECTION('center_axis',(5.13675726285535E-34,-1.,-1.22464674570954E-16));
#114487=DIRECTION('ref_axis',(-0.93969262091562,4.18853855054451E-17,-0.342020142969288));
#114488=DIRECTION('center_axis',(5.13675726285535E-34,-1.,-1.22464674570954E-16));
#114489=DIRECTION('ref_axis',(-0.93969262091562,4.18853855054451E-17,-0.342020142969288));
#114490=DIRECTION('center_axis',(5.13675726285535E-34,-1.,-1.22464674570954E-16));
#114491=DIRECTION('ref_axis',(-0.591613087024489,-9.87337180501123E-17,
0.806222026033372));
#114492=DIRECTION('center_axis',(5.13675726285535E-34,-1.,-1.22464674570954E-16));
#114493=DIRECTION('ref_axis',(-0.93969262091562,4.18853855054451E-17,-0.342020142969288));
#114494=DIRECTION('',(5.13675726285535E-34,-1.,-1.22464674570954E-16));
#114495=DIRECTION('center_axis',(5.13675726285535E-34,-1.,-1.22464674570954E-16));
#114496=DIRECTION('ref_axis',(-0.93969262091562,4.18853855054451E-17,-0.342020142969288));
#114497=DIRECTION('',(5.13675726285535E-34,-1.,-1.22464674570954E-16));
#114498=DIRECTION('',(-5.13675726285535E-34,1.,1.22464674570954E-16));
#114499=DIRECTION('center_axis',(5.13675726285535E-34,-1.,-1.22464674570954E-16));
#114500=DIRECTION('ref_axis',(0.0784590959774507,1.22087156847365E-16,-0.996917333713484));
#114501=DIRECTION('',(5.13675726285535E-34,-1.,-1.22464674570954E-16));
#114502=DIRECTION('center_axis',(5.13675726285535E-34,-1.,-1.22464674570954E-16));
#114503=DIRECTION('ref_axis',(-0.93969262091562,4.18853855054451E-17,-0.342020142969288));
#114504=DIRECTION('center_axis',(5.13675726285535E-34,-1.,-1.22464674570954E-16));
#114505=DIRECTION('ref_axis',(-0.93969262091562,4.18853855054451E-17,-0.342020142969288));
#114506=DIRECTION('center_axis',(5.13675726285535E-34,-1.,-1.22464674570954E-16));
#114507=DIRECTION('ref_axis',(-0.700328675782159,-8.74177986363949E-17,
0.713820527777962));
#114508=DIRECTION('center_axis',(5.13675726285535E-34,-1.,-1.22464674570954E-16));
#114509=DIRECTION('ref_axis',(-0.93969262091562,4.18853855054451E-17,-0.342020142969288));
#114510=DIRECTION('',(5.13675726285535E-34,-1.,-1.22464674570954E-16));
#114511=DIRECTION('center_axis',(5.13675726285535E-34,-1.,-1.22464674570954E-16));
#114512=DIRECTION('ref_axis',(-0.93969262091562,4.18853855054451E-17,-0.342020142969288));
#114513=DIRECTION('',(5.13675726285535E-34,-1.,-1.22464674570954E-16));
#114514=DIRECTION('',(-5.13675726285535E-34,1.,1.22464674570954E-16));
#114515=DIRECTION('center_axis',(5.13675726285535E-34,-1.,-1.22464674570954E-16));
#114516=DIRECTION('ref_axis',(0.0784590959774507,1.22087156847365E-16,-0.996917333713484));
#114517=DIRECTION('',(5.13675726285535E-34,-1.,-1.22464674570954E-16));
#114518=DIRECTION('center_axis',(5.13675726285535E-34,-1.,-1.22464674570954E-16));
#114519=DIRECTION('ref_axis',(-0.93969262091562,4.18853855054451E-17,-0.342020142969288));
#114520=DIRECTION('center_axis',(5.13675726285535E-34,-1.,-1.22464674570954E-16));
#114521=DIRECTION('ref_axis',(-0.93969262091562,4.18853855054451E-17,-0.342020142969288));
#114522=DIRECTION('center_axis',(5.13675726285535E-34,-1.,-1.22464674570954E-16));
#114523=DIRECTION('ref_axis',(-0.794787592671922,-7.4322304895865E-17,0.606887701749485));
#114524=DIRECTION('center_axis',(5.13675726285535E-34,-1.,-1.22464674570954E-16));
#114525=DIRECTION('ref_axis',(-0.93969262091562,4.18853855054451E-17,-0.342020142969288));
#114526=DIRECTION('',(5.13675726285535E-34,-1.,-1.22464674570954E-16));
#114527=DIRECTION('center_axis',(5.13675726285535E-34,-1.,-1.22464674570954E-16));
#114528=DIRECTION('ref_axis',(-0.93969262091562,4.18853855054451E-17,-0.342020142969288));
#114529=DIRECTION('',(5.13675726285535E-34,-1.,-1.22464674570954E-16));
#114530=DIRECTION('',(-5.13675726285535E-34,1.,1.22464674570954E-16));
#114531=DIRECTION('center_axis',(5.13675726285535E-34,-1.,-1.22464674570954E-16));
#114532=DIRECTION('ref_axis',(0.0784590959774507,1.22087156847365E-16,-0.996917333713484));
#114533=DIRECTION('',(5.13675726285535E-34,-1.,-1.22464674570954E-16));
#114534=DIRECTION('center_axis',(5.13675726285535E-34,-1.,-1.22464674570954E-16));
#114535=DIRECTION('ref_axis',(-0.93969262091562,4.18853855054451E-17,-0.342020142969288));
#114536=DIRECTION('center_axis',(5.13675726285535E-34,-1.,-1.22464674570954E-16));
#114537=DIRECTION('ref_axis',(-0.93969262091562,4.18853855054451E-17,-0.342020142969288));
#114538=DIRECTION('center_axis',(5.13675726285535E-34,-1.,-1.22464674570954E-16));
#114539=DIRECTION('ref_axis',(-0.87306692619485,-5.97138233402766E-17,0.487600392108822));
#114540=DIRECTION('center_axis',(5.13675726285535E-34,-1.,-1.22464674570954E-16));
#114541=DIRECTION('ref_axis',(-0.93969262091562,4.18853855054451E-17,-0.342020142969288));
#114542=DIRECTION('',(5.13675726285535E-34,-1.,-1.22464674570954E-16));
#114543=DIRECTION('center_axis',(5.13675726285535E-34,-1.,-1.22464674570954E-16));
#114544=DIRECTION('ref_axis',(-0.93969262091562,4.18853855054451E-17,-0.342020142969288));
#114545=DIRECTION('',(5.13675726285535E-34,-1.,-1.22464674570954E-16));
#114546=DIRECTION('',(-5.13675726285535E-34,1.,1.22464674570954E-16));
#114547=DIRECTION('center_axis',(5.13675726285535E-34,-1.,-1.22464674570954E-16));
#114548=DIRECTION('ref_axis',(0.0784590959774507,1.22087156847365E-16,-0.996917333713484));
#114549=DIRECTION('',(5.13675726285535E-34,-1.,-1.22464674570954E-16));
#114550=DIRECTION('center_axis',(5.13675726285535E-34,-1.,-1.22464674570954E-16));
#114551=DIRECTION('ref_axis',(-0.93969262091562,4.18853855054451E-17,-0.342020142969288));
#114552=DIRECTION('center_axis',(5.13675726285535E-34,-1.,-1.22464674570954E-16));
#114553=DIRECTION('ref_axis',(-0.93969262091562,4.18853855054451E-17,-0.342020142969288));
#114554=DIRECTION('center_axis',(5.13675726285535E-34,-1.,-1.22464674570954E-16));
#114555=DIRECTION('ref_axis',(-0.933573134654503,-4.38897405736607E-17,
0.358386944867368));
#114556=DIRECTION('center_axis',(5.13675726285535E-34,-1.,-1.22464674570954E-16));
#114557=DIRECTION('ref_axis',(-0.93969262091562,4.18853855054451E-17,-0.342020142969288));
#114558=DIRECTION('',(5.13675726285535E-34,-1.,-1.22464674570954E-16));
#114559=DIRECTION('center_axis',(5.13675726285535E-34,-1.,-1.22464674570954E-16));
#114560=DIRECTION('ref_axis',(-0.93969262091562,4.18853855054451E-17,-0.342020142969288));
#114561=DIRECTION('',(5.13675726285535E-34,-1.,-1.22464674570954E-16));
#114562=DIRECTION('',(-5.13675726285535E-34,1.,1.22464674570954E-16));
#114563=DIRECTION('center_axis',(5.13675726285535E-34,-1.,-1.22464674570954E-16));
#114564=DIRECTION('ref_axis',(0.0784590959774507,1.22087156847365E-16,-0.996917333713484));
#114565=DIRECTION('',(5.13675726285535E-34,-1.,-1.22464674570954E-16));
#114566=DIRECTION('center_axis',(5.13675726285535E-34,-1.,-1.22464674570954E-16));
#114567=DIRECTION('ref_axis',(-0.93969262091562,4.18853855054451E-17,-0.342020142969288));
#114568=DIRECTION('center_axis',(5.13675726285535E-34,-1.,-1.22464674570954E-16));
#114569=DIRECTION('ref_axis',(-0.93969262091562,4.18853855054451E-17,-0.342020142969288));
#114570=DIRECTION('center_axis',(5.13675726285535E-34,-1.,-1.22464674570954E-16));
#114571=DIRECTION('ref_axis',(-0.975074486292716,-2.71721892731301E-17,
0.221877773066607));
#114572=DIRECTION('center_axis',(5.13675726285535E-34,-1.,-1.22464674570954E-16));
#114573=DIRECTION('ref_axis',(-0.93969262091562,4.18853855054451E-17,-0.342020142969288));
#114574=DIRECTION('',(5.13675726285535E-34,-1.,-1.22464674570954E-16));
#114575=DIRECTION('center_axis',(5.13675726285535E-34,-1.,-1.22464674570954E-16));
#114576=DIRECTION('ref_axis',(-0.93969262091562,4.18853855054451E-17,-0.342020142969288));
#114577=DIRECTION('',(5.13675726285535E-34,-1.,-1.22464674570954E-16));
#114578=DIRECTION('',(-5.13675726285535E-34,1.,1.22464674570954E-16));
#114579=DIRECTION('center_axis',(5.13675726285535E-34,-1.,-1.22464674570954E-16));
#114580=DIRECTION('ref_axis',(0.0784590959774507,1.22087156847365E-16,-0.996917333713484));
#114581=DIRECTION('',(5.13675726285535E-34,-1.,-1.22464674570954E-16));
#114582=DIRECTION('center_axis',(5.13675726285535E-34,-1.,-1.22464674570954E-16));
#114583=DIRECTION('ref_axis',(-0.93969262091562,4.18853855054451E-17,-0.342020142969288));
#114584=DIRECTION('center_axis',(5.13675726285535E-34,-1.,-1.22464674570954E-16));
#114585=DIRECTION('ref_axis',(-0.93969262091562,4.18853855054451E-17,-0.342020142969288));
#114586=DIRECTION('center_axis',(5.13675726285535E-34,-1.,-1.22464674570954E-16));
#114587=DIRECTION('ref_axis',(-0.996726133306289,-9.9014906031653E-18,0.0808518100248454));
#114588=DIRECTION('center_axis',(5.13675726285535E-34,-1.,-1.22464674570954E-16));
#114589=DIRECTION('ref_axis',(-0.93969262091562,4.18853855054451E-17,-0.342020142969288));
#114590=DIRECTION('',(5.13675726285535E-34,-1.,-1.22464674570954E-16));
#114591=DIRECTION('center_axis',(5.13675726285535E-34,-1.,-1.22464674570954E-16));
#114592=DIRECTION('ref_axis',(-0.93969262091562,4.18853855054451E-17,-0.342020142969288));
#114593=DIRECTION('',(5.13675726285535E-34,-1.,-1.22464674570954E-16));
#114594=DIRECTION('',(-5.13675726285535E-34,1.,1.22464674570954E-16));
#114595=DIRECTION('center_axis',(5.13675726285535E-34,-1.,-1.22464674570954E-16));
#114596=DIRECTION('ref_axis',(0.0784590959774507,1.22087156847365E-16,-0.996917333713484));
#114597=DIRECTION('',(5.13675726285535E-34,-1.,-1.22464674570954E-16));
#114598=DIRECTION('center_axis',(5.13675726285535E-34,-1.,-1.22464674570954E-16));
#114599=DIRECTION('ref_axis',(-0.93969262091562,4.18853855054451E-17,-0.342020142969288));
#114600=DIRECTION('center_axis',(5.13675726285535E-34,-1.,-1.22464674570954E-16));
#114601=DIRECTION('ref_axis',(-0.93969262091562,4.18853855054451E-17,-0.342020142969288));
#114602=DIRECTION('center_axis',(5.13675726285535E-34,-1.,-1.22464674570954E-16));
#114603=DIRECTION('ref_axis',(-0.998087310654575,7.57077401709542E-18,-0.0618200639786049));
#114604=DIRECTION('center_axis',(5.13675726285535E-34,-1.,-1.22464674570954E-16));
#114605=DIRECTION('ref_axis',(-0.93969262091562,4.18853855054451E-17,-0.342020142969288));
#114606=DIRECTION('',(5.13675726285535E-34,-1.,-1.22464674570954E-16));
#114607=DIRECTION('center_axis',(5.13675726285535E-34,-1.,-1.22464674570954E-16));
#114608=DIRECTION('ref_axis',(-0.93969262091562,4.18853855054451E-17,-0.342020142969288));
#114609=DIRECTION('',(5.13675726285535E-34,-1.,-1.22464674570954E-16));
#114610=DIRECTION('',(-5.13675726285535E-34,1.,1.22464674570954E-16));
#114611=DIRECTION('center_axis',(5.13675726285535E-34,-1.,-1.22464674570954E-16));
#114612=DIRECTION('ref_axis',(0.0784590959774507,1.22087156847365E-16,-0.996917333713484));
#114613=DIRECTION('',(5.13675726285535E-34,-1.,-1.22464674570954E-16));
#114614=DIRECTION('center_axis',(5.13675726285535E-34,-1.,-1.22464674570954E-16));
#114615=DIRECTION('ref_axis',(-0.93969262091562,4.18853855054451E-17,-0.342020142969288));
#114616=DIRECTION('center_axis',(5.13675726285535E-34,-1.,-1.22464674570954E-16));
#114617=DIRECTION('ref_axis',(-0.93969262091562,4.18853855054451E-17,-0.342020142969288));
#114618=DIRECTION('center_axis',(5.13675726285535E-34,-1.,-1.22464674570954E-16));
#114619=DIRECTION('ref_axis',(-0.979130308579199,2.48889194076679E-17,-0.203233458912656));
#114620=DIRECTION('center_axis',(5.13675726285535E-34,-1.,-1.22464674570954E-16));
#114621=DIRECTION('ref_axis',(-0.93969262091562,4.18853855054451E-17,-0.342020142969288));
#114622=DIRECTION('',(5.13675726285535E-34,-1.,-1.22464674570954E-16));
#114623=DIRECTION('center_axis',(5.13675726285535E-34,-1.,-1.22464674570954E-16));
#114624=DIRECTION('ref_axis',(-0.93969262091562,4.18853855054451E-17,-0.342020142969288));
#114625=DIRECTION('',(5.13675726285535E-34,-1.,-1.22464674570954E-16));
#114626=DIRECTION('',(-5.13675726285535E-34,1.,1.22464674570954E-16));
#114627=DIRECTION('center_axis',(5.13675726285535E-34,-1.,-1.22464674570954E-16));
#114628=DIRECTION('ref_axis',(0.0784590959774507,1.22087156847365E-16,-0.996917333713484));
#114629=DIRECTION('',(5.13675726285535E-34,-1.,-1.22464674570954E-16));
#114630=DIRECTION('center_axis',(5.13675726285535E-34,-1.,-1.22464674570954E-16));
#114631=DIRECTION('ref_axis',(-0.93969262091562,4.18853855054451E-17,-0.342020142969288));
#114632=DIRECTION('center_axis',(5.13675726285535E-34,-1.,-1.22464674570954E-16));
#114633=DIRECTION('ref_axis',(-0.93969262091562,4.18853855054451E-17,-0.342020142969288));
#114634=DIRECTION('center_axis',(5.13675726285535E-34,-1.,-1.22464674570954E-16));
#114635=DIRECTION('ref_axis',(-0.940241036944465,4.17003982070755E-17,-0.340509606979888));
#114636=DIRECTION('center_axis',(5.13675726285535E-34,-1.,-1.22464674570954E-16));
#114637=DIRECTION('ref_axis',(-0.93969262091562,4.18853855054451E-17,-0.342020142969288));
#114638=DIRECTION('',(5.13675726285535E-34,-1.,-1.22464674570954E-16));
#114639=DIRECTION('center_axis',(5.13675726285535E-34,-1.,-1.22464674570954E-16));
#114640=DIRECTION('ref_axis',(-0.93969262091562,4.18853855054451E-17,-0.342020142969288));
#114641=DIRECTION('',(5.13675726285535E-34,-1.,-1.22464674570954E-16));
#114642=DIRECTION('',(-5.13675726285535E-34,1.,1.22464674570954E-16));
#114643=DIRECTION('center_axis',(5.13675726285535E-34,-1.,-1.22464674570954E-16));
#114644=DIRECTION('ref_axis',(0.0784590959774507,1.22087156847365E-16,-0.996917333713484));
#114645=DIRECTION('',(5.13675726285535E-34,-1.,-1.22464674570954E-16));
#114646=DIRECTION('center_axis',(5.13675726285535E-34,-1.,-1.22464674570954E-16));
#114647=DIRECTION('ref_axis',(-0.93969262091562,4.18853855054451E-17,-0.342020142969288));
#114648=DIRECTION('center_axis',(5.13675726285535E-34,-1.,-1.22464674570954E-16));
#114649=DIRECTION('ref_axis',(-0.93969262091562,4.18853855054451E-17,-0.342020142969288));
#114650=DIRECTION('center_axis',(5.13675726285535E-34,-1.,-1.22464674570954E-16));
#114651=DIRECTION('ref_axis',(-0.882211169309773,5.76629771245571E-17,-0.470853961165332));
#114652=DIRECTION('center_axis',(5.13675726285535E-34,-1.,-1.22464674570954E-16));
#114653=DIRECTION('ref_axis',(-0.93969262091562,4.18853855054451E-17,-0.342020142969288));
#114654=DIRECTION('',(5.13675726285535E-34,-1.,-1.22464674570954E-16));
#114655=DIRECTION('center_axis',(5.13675726285535E-34,-1.,-1.22464674570954E-16));
#114656=DIRECTION('ref_axis',(-0.93969262091562,4.18853855054451E-17,-0.342020142969288));
#114657=DIRECTION('',(5.13675726285535E-34,-1.,-1.22464674570954E-16));
#114658=DIRECTION('',(-5.13675726285535E-34,1.,1.22464674570954E-16));
#114659=DIRECTION('center_axis',(5.13675726285535E-34,-1.,-1.22464674570954E-16));
#114660=DIRECTION('ref_axis',(0.0784590959774507,1.22087156847365E-16,-0.996917333713484));
#114661=DIRECTION('',(5.13675726285535E-34,-1.,-1.22464674570954E-16));
#114662=DIRECTION('center_axis',(5.13675726285535E-34,-1.,-1.22464674570954E-16));
#114663=DIRECTION('ref_axis',(-0.93969262091562,4.18853855054451E-17,-0.342020142969288));
#114664=DIRECTION('center_axis',(5.13675726285535E-34,-1.,-1.22464674570954E-16));
#114665=DIRECTION('ref_axis',(-0.93969262091562,4.18853855054451E-17,-0.342020142969288));
#114666=DIRECTION('center_axis',(5.13675726285535E-34,-1.,-1.22464674570954E-16));
#114667=DIRECTION('ref_axis',(-0.806222026033372,7.24517041743716E-17,-0.591613087024489));
#114668=DIRECTION('center_axis',(5.13675726285535E-34,-1.,-1.22464674570954E-16));
#114669=DIRECTION('ref_axis',(-0.93969262091562,4.18853855054451E-17,-0.342020142969288));
#114670=DIRECTION('',(5.13675726285535E-34,-1.,-1.22464674570954E-16));
#114671=DIRECTION('center_axis',(5.13675726285535E-34,-1.,-1.22464674570954E-16));
#114672=DIRECTION('ref_axis',(-0.93969262091562,4.18853855054451E-17,-0.342020142969288));
#114673=DIRECTION('',(5.13675726285535E-34,-1.,-1.22464674570954E-16));
#114674=DIRECTION('',(-5.13675726285535E-34,1.,1.22464674570954E-16));
#114675=DIRECTION('center_axis',(5.13675726285535E-34,-1.,-1.22464674570954E-16));
#114676=DIRECTION('ref_axis',(0.0784590959774507,1.22087156847365E-16,-0.996917333713484));
#114677=DIRECTION('',(5.13675726285535E-34,-1.,-1.22464674570954E-16));
#114678=DIRECTION('center_axis',(5.13675726285535E-34,-1.,-1.22464674570954E-16));
#114679=DIRECTION('ref_axis',(-0.93969262091562,4.18853855054451E-17,-0.342020142969288));
#114680=DIRECTION('center_axis',(5.13675726285535E-34,-1.,-1.22464674570954E-16));
#114681=DIRECTION('ref_axis',(-0.93969262091562,4.18853855054451E-17,-0.342020142969288));
#114682=DIRECTION('center_axis',(5.13675726285535E-34,-1.,-1.22464674570954E-16));
#114683=DIRECTION('ref_axis',(-0.713820527777962,8.57655233723694E-17,-0.700328675782159));
#114684=DIRECTION('center_axis',(5.13675726285535E-34,-1.,-1.22464674570954E-16));
#114685=DIRECTION('ref_axis',(-0.93969262091562,4.18853855054451E-17,-0.342020142969288));
#114686=DIRECTION('',(5.13675726285535E-34,-1.,-1.22464674570954E-16));
#114687=DIRECTION('center_axis',(5.13675726285535E-34,-1.,-1.22464674570954E-16));
#114688=DIRECTION('ref_axis',(-0.93969262091562,4.18853855054451E-17,-0.342020142969288));
#114689=DIRECTION('',(5.13675726285535E-34,-1.,-1.22464674570954E-16));
#114690=DIRECTION('',(-5.13675726285535E-34,1.,1.22464674570954E-16));
#114691=DIRECTION('center_axis',(5.13675726285535E-34,-1.,-1.22464674570954E-16));
#114692=DIRECTION('ref_axis',(0.0784590959774507,1.22087156847365E-16,-0.996917333713484));
#114693=DIRECTION('',(5.13675726285535E-34,-1.,-1.22464674570954E-16));
#114694=DIRECTION('center_axis',(5.13675726285535E-34,-1.,-1.22464674570954E-16));
#114695=DIRECTION('ref_axis',(-0.93969262091562,4.18853855054451E-17,-0.342020142969288));
#114696=DIRECTION('center_axis',(5.13675726285535E-34,-1.,-1.22464674570954E-16));
#114697=DIRECTION('ref_axis',(-0.93969262091562,4.18853855054451E-17,-0.342020142969288));
#114698=DIRECTION('center_axis',(5.13675726285535E-34,-1.,-1.22464674570954E-16));
#114699=DIRECTION('ref_axis',(-0.606887701749485,9.73334038895991E-17,-0.794787592671922));
#114700=DIRECTION('center_axis',(5.13675726285535E-34,-1.,-1.22464674570954E-16));
#114701=DIRECTION('ref_axis',(-0.93969262091562,4.18853855054451E-17,-0.342020142969288));
#114702=DIRECTION('',(5.13675726285535E-34,-1.,-1.22464674570954E-16));
#114703=DIRECTION('center_axis',(5.13675726285535E-34,-1.,-1.22464674570954E-16));
#114704=DIRECTION('ref_axis',(-0.93969262091562,4.18853855054451E-17,-0.342020142969288));
#114705=DIRECTION('',(5.13675726285535E-34,-1.,-1.22464674570954E-16));
#114706=DIRECTION('',(-5.13675726285535E-34,1.,1.22464674570954E-16));
#114707=DIRECTION('center_axis',(5.13675726285535E-34,-1.,-1.22464674570954E-16));
#114708=DIRECTION('ref_axis',(0.0784590959774507,1.22087156847365E-16,-0.996917333713484));
#114709=DIRECTION('',(5.13675726285535E-34,-1.,-1.22464674570954E-16));
#114710=DIRECTION('center_axis',(5.13675726285535E-34,-1.,-1.22464674570954E-16));
#114711=DIRECTION('ref_axis',(-0.93969262091562,4.18853855054451E-17,-0.342020142969288));
#114712=DIRECTION('center_axis',(5.13675726285535E-34,-1.,-1.22464674570954E-16));
#114713=DIRECTION('ref_axis',(-0.93969262091562,4.18853855054451E-17,-0.342020142969288));
#114714=DIRECTION('center_axis',(5.13675726285535E-34,-1.,-1.22464674570954E-16));
#114715=DIRECTION('ref_axis',(-0.487600392108822,1.06919856995116E-16,-0.87306692619485));
#114716=DIRECTION('center_axis',(5.13675726285535E-34,-1.,-1.22464674570954E-16));
#114717=DIRECTION('ref_axis',(-0.93969262091562,4.18853855054451E-17,-0.342020142969288));
#114718=DIRECTION('',(5.13675726285535E-34,-1.,-1.22464674570954E-16));
#114719=DIRECTION('center_axis',(5.13675726285535E-34,-1.,-1.22464674570954E-16));
#114720=DIRECTION('ref_axis',(-0.93969262091562,4.18853855054451E-17,-0.342020142969288));
#114721=DIRECTION('',(5.13675726285535E-34,-1.,-1.22464674570954E-16));
#114722=DIRECTION('',(-5.13675726285535E-34,1.,1.22464674570954E-16));
#114723=DIRECTION('center_axis',(5.13675726285535E-34,-1.,-1.22464674570954E-16));
#114724=DIRECTION('ref_axis',(0.0784590959774507,1.22087156847365E-16,-0.996917333713484));
#114725=DIRECTION('',(5.13675726285535E-34,-1.,-1.22464674570954E-16));
#114726=DIRECTION('center_axis',(5.13675726285535E-34,-1.,-1.22464674570954E-16));
#114727=DIRECTION('ref_axis',(-0.93969262091562,4.18853855054451E-17,-0.342020142969288));
#114728=DIRECTION('center_axis',(5.13675726285535E-34,-1.,-1.22464674570954E-16));
#114729=DIRECTION('ref_axis',(-0.93969262091562,4.18853855054451E-17,-0.342020142969288));
#114730=DIRECTION('center_axis',(5.13675726285535E-34,-1.,-1.22464674570954E-16));
#114731=DIRECTION('ref_axis',(-0.358386944867368,1.14329730123649E-16,-0.933573134654503));
#114732=DIRECTION('center_axis',(5.13675726285535E-34,-1.,-1.22464674570954E-16));
#114733=DIRECTION('ref_axis',(-0.93969262091562,4.18853855054451E-17,-0.342020142969288));
#114734=DIRECTION('',(5.13675726285535E-34,-1.,-1.22464674570954E-16));
#114735=DIRECTION('center_axis',(5.13675726285535E-34,-1.,-1.22464674570954E-16));
#114736=DIRECTION('ref_axis',(-0.93969262091562,4.18853855054451E-17,-0.342020142969288));
#114737=DIRECTION('',(5.13675726285535E-34,-1.,-1.22464674570954E-16));
#114738=DIRECTION('',(-5.13675726285535E-34,1.,1.22464674570954E-16));
#114739=DIRECTION('center_axis',(5.13675726285535E-34,-1.,-1.22464674570954E-16));
#114740=DIRECTION('ref_axis',(0.0784590959774507,1.22087156847365E-16,-0.996917333713484));
#114741=DIRECTION('',(5.13675726285535E-34,-1.,-1.22464674570954E-16));
#114742=DIRECTION('center_axis',(5.13675726285535E-34,-1.,-1.22464674570954E-16));
#114743=DIRECTION('ref_axis',(-0.93969262091562,4.18853855054451E-17,-0.342020142969288));
#114744=DIRECTION('center_axis',(5.13675726285535E-34,-1.,-1.22464674570954E-16));
#114745=DIRECTION('ref_axis',(-0.93969262091562,4.18853855054451E-17,-0.342020142969288));
#114746=DIRECTION('center_axis',(5.13675726285535E-34,-1.,-1.22464674570954E-16));
#114747=DIRECTION('ref_axis',(-0.221877773066607,1.19412179646278E-16,-0.975074486292716));
#114748=DIRECTION('center_axis',(5.13675726285535E-34,-1.,-1.22464674570954E-16));
#114749=DIRECTION('ref_axis',(-0.93969262091562,4.18853855054451E-17,-0.342020142969288));
#114750=DIRECTION('',(5.13675726285535E-34,-1.,-1.22464674570954E-16));
#114751=DIRECTION('center_axis',(5.13675726285535E-34,-1.,-1.22464674570954E-16));
#114752=DIRECTION('ref_axis',(-0.93969262091562,4.18853855054451E-17,-0.342020142969288));
#114753=DIRECTION('',(5.13675726285535E-34,-1.,-1.22464674570954E-16));
#114754=DIRECTION('',(-5.13675726285535E-34,1.,1.22464674570954E-16));
#114755=DIRECTION('center_axis',(5.13675726285535E-34,-1.,-1.22464674570954E-16));
#114756=DIRECTION('ref_axis',(0.0784590959774507,1.22087156847365E-16,-0.996917333713484));
#114757=DIRECTION('center_axis',(5.13675726285535E-34,-1.,-1.22464674570954E-16));
#114758=DIRECTION('ref_axis',(-0.93969262091562,4.18853855054451E-17,-0.342020142969288));
#114759=DIRECTION('center_axis',(5.13675726285535E-34,-1.,-1.22464674570954E-16));
#114760=DIRECTION('ref_axis',(-0.93969262091562,4.18853855054451E-17,-0.342020142969288));
#114761=DIRECTION('center_axis',(5.13675726285535E-34,-1.,-1.22464674570954E-16));
#114762=DIRECTION('ref_axis',(-0.93969262091562,4.18853855054451E-17,-0.342020142969288));
#114763=DIRECTION('center_axis',(5.13675726285535E-34,-1.,-1.22464674570954E-16));
#114764=DIRECTION('ref_axis',(0.93969262091562,-4.18853855054451E-17,0.342020142969288));
#114765=DIRECTION('center_axis',(5.13675726285535E-34,-1.,-1.22464674570954E-16));
#114766=DIRECTION('ref_axis',(0.0784590959774507,1.22087156847365E-16,-0.996917333713484));
#114767=DIRECTION('',(-5.13675726285535E-34,1.,1.22464674570954E-16));
#114768=DIRECTION('center_axis',(5.13675726285535E-34,-1.,-1.22464674570954E-16));
#114769=DIRECTION('ref_axis',(-0.93969262091562,4.18853855054451E-17,-0.342020142969288));
#114770=DIRECTION('center_axis',(5.13675726285535E-34,-1.,-1.22464674570954E-16));
#114771=DIRECTION('ref_axis',(0.0784590959774507,1.22087156847365E-16,-0.996917333713484));
#114772=DIRECTION('',(5.13675726285535E-34,-1.,-1.22464674570954E-16));
#114773=DIRECTION('center_axis',(5.13675726285535E-34,-1.,-1.22464674570954E-16));
#114774=DIRECTION('ref_axis',(-0.93969262091562,4.18853855054451E-17,-0.342020142969288));
#114775=DIRECTION('center_axis',(5.13675726285535E-34,-1.,-1.22464674570954E-16));
#114776=DIRECTION('ref_axis',(-0.0808518100248454,1.2206374155172E-16,-0.996726133306289));
#114777=DIRECTION('',(5.13675726285535E-34,-1.,-1.22464674570954E-16));
#114778=DIRECTION('center_axis',(5.13675726285535E-34,-1.,-1.22464674570954E-16));
#114779=DIRECTION('ref_axis',(-0.93969262091562,4.18853855054451E-17,-0.342020142969288));
#114780=DIRECTION('',(5.13675726285535E-34,-1.,-1.22464674570954E-16));
#114781=DIRECTION('center_axis',(5.13675726285535E-34,-1.,-1.22464674570954E-16));
#114782=DIRECTION('ref_axis',(0.93969262091562,-4.18853855054451E-17,0.342020142969288));
#114783=DIRECTION('',(5.13675726285535E-34,-1.,-1.22464674570954E-16));
#114784=DIRECTION('center_axis',(5.13675726285535E-34,-1.,-1.22464674570954E-16));
#114785=DIRECTION('ref_axis',(0.93969262091562,-4.18853855054451E-17,0.342020142969288));
#114786=DIRECTION('center_axis',(5.13675726285535E-34,-1.,-1.22464674570954E-16));
#114787=DIRECTION('ref_axis',(-1.5735453877384E-50,1.22464674570954E-16,
-1.));
#114788=DIRECTION('center_axis',(4.44089209850063E-16,1.,1.22464674570954E-16));
#114789=DIRECTION('ref_axis',(-1.,4.44089209850063E-16,-2.07165259840883E-30));
#114790=DIRECTION('center_axis',(5.55111512312577E-16,1.,1.22464679914736E-16));
#114791=DIRECTION('ref_axis',(-1.,5.55111512312577E-16,-2.05805628826764E-30));
#114792=DIRECTION('',(-4.44089209850063E-16,-1.,-1.22464674570954E-16));
#114793=DIRECTION('center_axis',(-1.56641358065672E-32,-1.,-1.22464674570954E-16));
#114794=DIRECTION('ref_axis',(-0.0784590959774507,-1.22087156847365E-16,
0.996917333713484));
#114795=DIRECTION('center_axis',(4.44089209850063E-16,1.,1.22464674570954E-16));
#114796=DIRECTION('ref_axis',(-1.,4.44089209850063E-16,-2.07165259840883E-30));
#114797=DIRECTION('center_axis',(-1.56641358065672E-32,-1.,-1.22464674570954E-16));
#114798=DIRECTION('ref_axis',(-1.,4.44089209850063E-16,-2.07165259840883E-30));
#114799=DIRECTION('',(-4.44089209850063E-16,-1.,-1.22464674570954E-16));
#114800=DIRECTION('center_axis',(-5.55111512312577E-16,-1.,-1.22464679914736E-16));
#114801=DIRECTION('ref_axis',(-1.,5.55111512312577E-16,-2.05805628826764E-30));
#114802=DIRECTION('center_axis',(5.55111512312577E-16,1.,1.22464679914736E-16));
#114803=DIRECTION('ref_axis',(-1.,5.55111512312577E-16,-2.05805628826764E-30));
#114804=DIRECTION('center_axis',(5.55111512312577E-16,1.,1.22464679914736E-16));
#114805=DIRECTION('ref_axis',(-1.,5.55111512312577E-16,-2.05805628826764E-30));
#114806=DIRECTION('center_axis',(1.56641358065672E-32,1.,1.22464674570954E-16));
#114807=DIRECTION('ref_axis',(0.0784590959774507,1.22087156847365E-16,-0.996917333713484));
#114808=DIRECTION('',(-0.334274317935853,-1.15419995177468E-16,0.942475824819141));
#114809=DIRECTION('center_axis',(1.56641358065672E-32,1.,1.22464674570954E-16));
#114810=DIRECTION('ref_axis',(-0.93969262091562,4.18853855054452E-17,-0.342020142969288));
#114811=DIRECTION('',(0.184775606034611,1.20355923031387E-16,-0.98278073618409));
#114812=DIRECTION('center_axis',(1.56641358065672E-32,1.,1.22464674570954E-16));
#114813=DIRECTION('ref_axis',(-0.93969262091562,4.18853855054451E-17,-0.342020142969288));
#114814=DIRECTION('',(0.0287600210011737,-1.2241401645099E-16,0.999586345040793));
#114815=DIRECTION('center_axis',(1.56641358065672E-32,1.,1.22464674570954E-16));
#114816=DIRECTION('ref_axis',(-0.93969262091562,4.18853855054452E-17,-0.342020142969288));
#114817=DIRECTION('',(-0.182723229956296,1.20402907287232E-16,-0.983164391764845));
#114818=DIRECTION('center_axis',(1.56641358065672E-32,1.,1.22464674570954E-16));
#114819=DIRECTION('ref_axis',(-0.93969262091562,4.18853855054451E-17,-0.342020142969288));
#114820=DIRECTION('',(0.387910159064799,-1.12875346322704E-16,0.921697189153966));
#114821=DIRECTION('center_axis',(1.56641358065672E-32,1.,1.22464674570954E-16));
#114822=DIRECTION('ref_axis',(-0.93969262091562,4.18853855054452E-17,-0.342020142969288));
#114823=DIRECTION('',(-0.525544280992694,1.04188811695823E-16,-0.850766247988172));
#114824=DIRECTION('center_axis',(1.56641358065672E-32,1.,1.22464674570954E-16));
#114825=DIRECTION('ref_axis',(-0.93969262091562,4.18853855054451E-17,-0.342020142969288));
#114826=DIRECTION('',(0.694670879902617,-8.80922351273172E-17,0.71932771989916));
#114827=DIRECTION('center_axis',(1.56641358065672E-32,1.,1.22464674570954E-16));
#114828=DIRECTION('ref_axis',(-0.93969262091562,4.18853855054452E-17,-0.342020142969288));
#114829=DIRECTION('',(-0.797387662985364,7.39034399784702E-17,-0.603467409988924));
#114830=DIRECTION('center_axis',(1.56641358065672E-32,1.,1.22464674570954E-16));
#114831=DIRECTION('ref_axis',(-0.93969262091562,4.18853855054451E-17,-0.342020142969288));
#114832=DIRECTION('',(0.907612447952903,-5.14117795447764E-17,0.419809056978216));
#114833=DIRECTION('center_axis',(1.56641358065672E-32,1.,1.22464674570954E-16));
#114834=DIRECTION('ref_axis',(-0.93969262091562,4.18853855054452E-17,-0.342020142969288));
#114835=DIRECTION('',(-0.961539424227938,3.36369991449791E-17,-0.274666954065111));
#114836=DIRECTION('center_axis',(1.56641358065672E-32,1.,1.22464674570954E-16));
#114837=DIRECTION('ref_axis',(-0.93969262091562,4.18853855054451E-17,-0.342020142969288));
#114838=DIRECTION('',(0.997975925895315,-7.78787841426065E-18,0.0635928559933293));
#114839=DIRECTION('center_axis',(1.56641358065672E-32,1.,1.22464674570954E-16));
#114840=DIRECTION('ref_axis',(-0.93969262091562,4.18853855054452E-17,-0.342020142969288));
#114841=DIRECTION('',(-0.995829958489319,-1.11723051865237E-17,0.0912287990448269));
#114842=DIRECTION('center_axis',(1.56641358065672E-32,1.,1.22464674570954E-16));
#114843=DIRECTION('ref_axis',(-0.93969262091562,4.18853855054451E-17,-0.342020142969288));
#114844=DIRECTION('',(0.953557225147758,3.68878192755495E-17,-0.301211916046674));
#114845=DIRECTION('center_axis',(1.56641358065672E-32,1.,1.22464674570954E-16));
#114846=DIRECTION('ref_axis',(-0.93969262091562,4.18853855054452E-17,-0.342020142969288));
#114847=DIRECTION('',(-0.895628138133327,-5.44727275177746E-17,0.444803595066215));
#114848=DIRECTION('center_axis',(1.56641358065672E-32,1.,1.22464674570954E-16));
#114849=DIRECTION('ref_axis',(-0.93969262091562,4.18853855054451E-17,-0.342020142969288));
#114850=DIRECTION('',(0.780355338322394,7.65816121419183E-17,-0.62533634625835));
#114851=DIRECTION('center_axis',(1.56641358065672E-32,1.,1.22464674570954E-16));
#114852=DIRECTION('ref_axis',(-0.93969262091562,4.18853855054452E-17,-0.342020142969288));
#114853=DIRECTION('',(-0.674466775907303,-9.04163060396167E-17,0.738305199898529));
#114854=DIRECTION('center_axis',(1.56641358065672E-32,1.,1.22464674570954E-16));
#114855=DIRECTION('ref_axis',(-0.93969262091562,4.18853855054451E-17,-0.342020142969288));
#114856=DIRECTION('',(0.501762135978649,1.05932634322597E-16,-0.865005640963193));
#114857=DIRECTION('center_axis',(1.56641358065672E-32,1.,1.22464674570954E-16));
#114858=DIRECTION('ref_axis',(-0.93969262091562,4.18853855054452E-17,-0.342020142969288));
#114859=DIRECTION('',(-0.362214936962566,-1.14148661601617E-16,0.93209459790367));
#114860=DIRECTION('center_axis',(1.56641358065672E-32,1.,1.22464674570954E-16));
#114861=DIRECTION('ref_axis',(-0.93969262091562,4.18853855054451E-17,-0.342020142969288));
#114862=DIRECTION('',(0.15540318800344,1.20976866795283E-16,-0.987851127021864));
#114863=DIRECTION('center_axis',(1.56641358065672E-32,1.,1.22464674570954E-16));
#114864=DIRECTION('ref_axis',(-0.93969262091562,4.18853855054452E-17,-0.342020142969288));
#114865=DIRECTION('',(-0.00104396100007576,-1.22464607836593E-16,0.999999455072567));
#114866=DIRECTION('center_axis',(1.56641358065672E-32,1.,1.22464674570954E-16));
#114867=DIRECTION('ref_axis',(-0.93969262091562,4.18853855054451E-17,-0.342020142969288));
#114868=DIRECTION('',(-0.211943832922472,1.19682503558106E-16,-0.977281848642515));
#114869=DIRECTION('center_axis',(1.56641358065672E-32,1.,1.22464674570954E-16));
#114870=DIRECTION('ref_axis',(-0.93969262091562,4.18853855054452E-17,-0.342020142969288));
#114871=DIRECTION('',(0.360268003917448,-1.14241030078174E-16,0.932848843786247));
#114872=DIRECTION('center_axis',(1.56641358065672E-32,1.,1.22464674570954E-16));
#114873=DIRECTION('ref_axis',(-0.93969262091562,4.18853855054451E-17,-0.342020142969288));
#114874=DIRECTION('',(-0.550666659981411,1.0222435511424E-16,-0.834725241971822));
#114875=DIRECTION('center_axis',(1.56641358065672E-32,1.,1.22464674570954E-16));
#114876=DIRECTION('ref_axis',(-0.93969262091562,4.18853855054452E-17,-0.342020142969288));
#114877=DIRECTION('',(0.672923776631946,-9.05885684876879E-17,0.739711829595417));
#114878=DIRECTION('center_axis',(1.56641358065672E-32,1.,1.22464674570954E-16));
#114879=DIRECTION('ref_axis',(-0.93969262091562,4.18853855054451E-17,-0.342020142969288));
#114880=DIRECTION('',(-0.815018905804237,7.09602409279082E-17,-0.579434364860823));
#114881=DIRECTION('center_axis',(1.56641358065672E-32,1.,1.22464674570954E-16));
#114882=DIRECTION('ref_axis',(-0.93969262091562,4.18853855054452E-17,-0.342020142969288));
#114883=DIRECTION('',(0.894697468857086,-5.47016183864292E-17,0.446672630928651));
#114884=DIRECTION('center_axis',(1.56641358065672E-32,1.,1.22464674570954E-16));
#114885=DIRECTION('ref_axis',(-0.93969262091562,4.18853855054451E-17,-0.342020142969288));
#114886=DIRECTION('',(-0.969298331894766,3.01125528719676E-17,-0.245887664973305));
#114887=DIRECTION('center_axis',(1.56641358065672E-32,1.,1.22464674570954E-16));
#114888=DIRECTION('ref_axis',(-0.93969262091562,4.18853855054452E-17,-0.342020142969288));
#114889=DIRECTION('',(0.995637308827798,-1.14269118092488E-17,0.0933078199838617));
#114890=DIRECTION('center_axis',(1.56641358065672E-32,1.,1.22464674570954E-16));
#114891=DIRECTION('ref_axis',(-0.93969262091562,4.18853855054451E-17,-0.342020142969288));
#114892=DIRECTION('',(-0.992668646322072,-1.48020021201242E-17,0.120867525039216));
#114893=DIRECTION('center_axis',(1.56641358065672E-32,1.,1.22464674570954E-16));
#114894=DIRECTION('ref_axis',(-0.93969262091562,4.18853855054452E-17,-0.342020142969288));
#114895=DIRECTION('',(0.96211081236153,3.3391063018321E-17,-0.272658733102456));
#114896=DIRECTION('center_axis',(1.56641358065672E-32,1.,1.22464674570954E-16));
#114897=DIRECTION('ref_axis',(-0.93969262091562,4.18853855054451E-17,-0.342020142969288));
#114898=DIRECTION('',(-0.881973559148804,-5.77174648318459E-17,0.471298887079516));
#114899=DIRECTION('center_axis',(1.56641358065672E-32,1.,1.22464674570954E-16));
#114900=DIRECTION('ref_axis',(-0.93969262091562,4.18853855054452E-17,-0.342020142969288));
#114901=DIRECTION('',(0.798645919725862,7.36993891912942E-17,-0.601801208793429));
#114902=DIRECTION('center_axis',(1.56641358065672E-32,1.,1.22464674570954E-16));
#114903=DIRECTION('ref_axis',(-0.93969262091562,4.18853855054451E-17,-0.342020142969288));
#114904=DIRECTION('',(-0.652163056951551,-9.28378638595332E-17,0.758078720943682));
#114905=DIRECTION('center_axis',(1.56641358065672E-32,1.,1.22464674570954E-16));
#114906=DIRECTION('ref_axis',(-0.93969262091562,4.18853855054452E-17,-0.342020142969288));
#114907=DIRECTION('',(0.527319471663896,1.0405420446143E-16,-0.849667096458437));
#114908=DIRECTION('center_axis',(1.56641358065672E-32,1.,1.22464674570954E-16));
#114909=DIRECTION('ref_axis',(-0.93969262091562,4.18853855054451E-17,-0.342020142969288));
#114910=DIRECTION('center_axis',(-1.56641358065672E-32,-1.,-1.22464674570954E-16));
#114911=DIRECTION('ref_axis',(0.93969262091562,-4.18853855054452E-17,0.342020142969288));
#114912=DIRECTION('center_axis',(-1.56641358065672E-32,-1.,-1.22464674570954E-16));
#114913=DIRECTION('ref_axis',(-0.0784590959774507,-1.22087156847365E-16,
0.996917333713484));
#114914=DIRECTION('center_axis',(1.56641358065672E-32,1.,1.22464674570954E-16));
#114915=DIRECTION('ref_axis',(-0.0784590959774507,-1.22087156847365E-16,
0.996917333713484));
#114916=DIRECTION('',(1.56641358065672E-32,1.,1.22464674570954E-16));
#114917=DIRECTION('center_axis',(1.56641358065672E-32,1.,1.22464674570954E-16));
#114918=DIRECTION('ref_axis',(-0.0784590959774507,-1.22087156847365E-16,
0.996917333713484));
#114919=DIRECTION('center_axis',(-1.56641358065672E-32,-1.,-1.22464674570954E-16));
#114920=DIRECTION('ref_axis',(-0.0784590959774507,-1.22087156847365E-16,
0.996917333713484));
#114921=DIRECTION('center_axis',(-1.56641358065672E-32,-1.,-1.22464674570954E-16));
#114922=DIRECTION('ref_axis',(-0.225894875006821,-1.19299169089874E-16,
0.974151685029417));
#114923=DIRECTION('',(-1.56641358065672E-32,-1.,-1.22464674570954E-16));
#114924=DIRECTION('center_axis',(-1.56641358065672E-32,-1.,-1.22464674570954E-16));
#114925=DIRECTION('ref_axis',(-0.225894875006821,-1.19299169089874E-16,
0.974151685029417));
#114926=DIRECTION('',(-1.56641358065672E-32,-1.,-1.22464674570954E-16));
#114927=DIRECTION('',(-1.56641358065672E-32,-1.,-1.22464674570954E-16));
#114928=DIRECTION('center_axis',(-0.932094434249406,4.4358585953941E-17,
-0.36221535809692));
#114929=DIRECTION('ref_axis',(0.36221535809692,1.14148641559751E-16,-0.932094434249406));
#114930=DIRECTION('',(1.56641358065672E-32,1.,1.22464674570954E-16));
#114931=DIRECTION('',(0.36221535809692,1.14148641559751E-16,-0.932094434249406));
#114932=DIRECTION('center_axis',(-1.56641358065672E-32,-1.,-1.22464674570954E-16));
#114933=DIRECTION('ref_axis',(0.0784590959774507,1.22087156847365E-16,-0.996917333713484));
#114934=DIRECTION('',(-1.56641358065672E-32,-1.,-1.22464674570954E-16));
#114935=DIRECTION('center_axis',(-1.56641358065672E-32,-1.,-1.22464674570954E-16));
#114936=DIRECTION('ref_axis',(0.0784590959774507,1.22087156847365E-16,-0.996917333713484));
#114937=DIRECTION('center_axis',(0.865005821949093,-6.14480984846721E-17,
0.501761823970471));
#114938=DIRECTION('ref_axis',(-0.501761823970471,-1.05932656486976E-16,
0.865005821949093));
#114939=DIRECTION('',(-1.56641358065672E-32,-1.,-1.22464674570954E-16));
#114940=DIRECTION('',(-0.501761823970471,-1.05932656486976E-16,0.865005821949093));
#114941=DIRECTION('',(-1.56641358065672E-32,-1.,-1.22464674570954E-16));
#114942=DIRECTION('center_axis',(-1.56641358065672E-32,-1.,-1.22464674570954E-16));
#114943=DIRECTION('ref_axis',(-0.562544874928296,-1.01249721339324E-16,
0.826766752894617));
#114944=DIRECTION('',(-1.56641358065672E-32,-1.,-1.22464674570954E-16));
#114945=DIRECTION('center_axis',(-1.56641358065672E-32,-1.,-1.22464674570954E-16));
#114946=DIRECTION('ref_axis',(-0.562544874928296,-1.01249721339324E-16,
0.826766752894617));
#114947=DIRECTION('',(-1.56641358065672E-32,-1.,-1.22464674570954E-16));
#114948=DIRECTION('center_axis',(-0.738304895785748,8.25983949885278E-17,
-0.674467108804273));
#114949=DIRECTION('ref_axis',(0.674467108804273,9.04162687965439E-17,-0.738304895785748));
#114950=DIRECTION('',(1.56641358065672E-32,1.,1.22464674570954E-16));
#114951=DIRECTION('',(0.674467108804273,9.04162687965439E-17,-0.738304895785748));
#114952=DIRECTION('center_axis',(-1.56641358065672E-32,-1.,-1.22464674570954E-16));
#114953=DIRECTION('ref_axis',(0.0784590959774507,1.22087156847365E-16,-0.996917333713484));
#114954=DIRECTION('',(-1.56641358065672E-32,-1.,-1.22464674570954E-16));
#114955=DIRECTION('center_axis',(-1.56641358065672E-32,-1.,-1.22464674570954E-16));
#114956=DIRECTION('ref_axis',(0.0784590959774507,1.22087156847365E-16,-0.996917333713484));
#114957=DIRECTION('center_axis',(0.625336629973868,-9.55659347144022E-17,
0.780355110967389));
#114958=DIRECTION('ref_axis',(-0.780355110967389,-7.65816468870469E-17,
0.625336629973867));
#114959=DIRECTION('',(-1.56641358065672E-32,-1.,-1.22464674570954E-16));
#114960=DIRECTION('',(-0.780355110967389,-7.65816468870469E-17,0.625336629973867));
#114961=DIRECTION('',(-1.56641358065672E-32,-1.,-1.22464674570954E-16));
#114962=DIRECTION('center_axis',(-1.56641358065672E-32,-1.,-1.22464674570954E-16));
#114963=DIRECTION('ref_axis',(-0.823220073969957,-6.95259374905277E-17,
0.567722387979282));
#114964=DIRECTION('',(-1.56641358065672E-32,-1.,-1.22464674570954E-16));
#114965=DIRECTION('center_axis',(-1.56641358065672E-32,-1.,-1.22464674570954E-16));
#114966=DIRECTION('ref_axis',(-0.823220073969957,-6.95259374905277E-17,
0.567722387979282));
#114967=DIRECTION('',(-1.56641358065672E-32,-1.,-1.22464674570954E-16));
#114968=DIRECTION('center_axis',(-0.444803189723036,1.09682833126328E-16,
-0.895628339442323));
#114969=DIRECTION('ref_axis',(0.895628339442323,5.4472677877554E-17,-0.444803189723036));
#114970=DIRECTION('',(1.56641358065672E-32,1.,1.22464674570954E-16));
#114971=DIRECTION('',(0.895628339442323,5.4472677877554E-17,-0.444803189723036));
#114972=DIRECTION('center_axis',(-1.56641358065672E-32,-1.,-1.22464674570954E-16));
#114973=DIRECTION('ref_axis',(0.0784590959774507,1.22087156847365E-16,-0.996917333713484));
#114974=DIRECTION('',(-1.56641358065672E-32,-1.,-1.22464674570954E-16));
#114975=DIRECTION('center_axis',(-1.56641358065672E-32,-1.,-1.22464674570954E-16));
#114976=DIRECTION('ref_axis',(0.0784590959774507,1.22087156847365E-16,-0.996917333713484));
#114977=DIRECTION('center_axis',(0.301212261052566,-1.16777061916137E-16,
0.95355711616641));
#114978=DIRECTION('ref_axis',(-0.95355711616641,-3.68878615265838E-17,0.301212261052566));
#114979=DIRECTION('',(-1.56641358065672E-32,-1.,-1.22464674570954E-16));
#114980=DIRECTION('',(-0.95355711616641,-3.68878615265838E-17,0.301212261052566));
#114981=DIRECTION('',(-1.56641358065672E-32,-1.,-1.22464674570954E-16));
#114982=DIRECTION('center_axis',(-1.56641358065672E-32,-1.,-1.22464674570954E-16));
#114983=DIRECTION('ref_axis',(-0.972714838948175,-2.84122906837056E-17,
0.232003969987639));
#114984=DIRECTION('',(-1.56641358065672E-32,-1.,-1.22464674570954E-16));
#114985=DIRECTION('center_axis',(-1.56641358065672E-32,-1.,-1.22464674570954E-16));
#114986=DIRECTION('ref_axis',(-0.972714838948175,-2.84122906837056E-17,
0.232003969987639));
#114987=DIRECTION('',(-1.56641358065672E-32,-1.,-1.22464674570954E-16));
#114988=DIRECTION('center_axis',(-0.0912283479827209,1.21953996854895E-16,
-0.995829999811385));
#114989=DIRECTION('ref_axis',(0.995829999811385,1.11722499473497E-17,-0.091228347982721));
#114990=DIRECTION('',(1.56641358065672E-32,1.,1.22464674570954E-16));
#114991=DIRECTION('',(0.995829999811385,1.11722499473497E-17,-0.0912283479827209));
#114992=DIRECTION('center_axis',(-1.56641358065672E-32,-1.,-1.22464674570954E-16));
#114993=DIRECTION('ref_axis',(0.0784590959774507,1.22087156847365E-16,-0.996917333713484));
#114994=DIRECTION('',(-1.56641358065672E-32,-1.,-1.22464674570954E-16));
#114995=DIRECTION('center_axis',(-1.56641358065672E-32,-1.,-1.22464674570954E-16));
#114996=DIRECTION('ref_axis',(0.0784590959774507,1.22087156847365E-16,-0.996917333713484));
#114997=DIRECTION('center_axis',(-0.0635924930016405,-1.22216799827077E-16,
0.997975949025745));
#114998=DIRECTION('ref_axis',(-0.997975949025745,7.78783396060161E-18,-0.0635924930016405));
#114999=DIRECTION('',(-1.56641358065672E-32,-1.,-1.22464674570954E-16));
#115000=DIRECTION('',(-0.997975949025745,7.78783396060161E-18,-0.0635924930016405));
#115001=DIRECTION('',(-1.56641358065672E-32,-1.,-1.22464674570954E-16));
#115002=DIRECTION('center_axis',(-1.56641358065672E-32,-1.,-1.22464674570954E-16));
#115003=DIRECTION('ref_axis',(-0.990839075129605,1.65385934532139E-17,-0.135047870017665));
#115004=DIRECTION('',(-1.56641358065672E-32,-1.,-1.22464674570954E-16));
#115005=DIRECTION('center_axis',(-1.56641358065672E-32,-1.,-1.22464674570954E-16));
#115006=DIRECTION('ref_axis',(-0.990839075129605,1.65385934532139E-17,-0.135047870017665));
#115007=DIRECTION('',(-1.56641358065672E-32,-1.,-1.22464674570954E-16));
#115008=DIRECTION('center_axis',(0.274667386883407,1.17754597534162E-16,
-0.961539300591838));
#115009=DIRECTION('ref_axis',(0.961539300591838,-3.36370521499308E-17,0.274667386883407));
#115010=DIRECTION('',(1.56641358065672E-32,1.,1.22464674570954E-16));
#115011=DIRECTION('',(0.961539300591838,-3.36370521499308E-17,0.274667386883407));
#115012=DIRECTION('center_axis',(-1.56641358065672E-32,-1.,-1.22464674570954E-16));
#115013=DIRECTION('ref_axis',(0.0784590959774507,1.22087156847365E-16,-0.996917333713484));
#115014=DIRECTION('',(-1.56641358065672E-32,-1.,-1.22464674570954E-16));
#115015=DIRECTION('center_axis',(-1.56641358065672E-32,-1.,-1.22464674570954E-16));
#115016=DIRECTION('ref_axis',(0.0784590959774507,1.22087156847365E-16,-0.996917333713484));
#115017=DIRECTION('center_axis',(-0.419808728869155,-1.11150481660855E-16,
0.907612599717117));
#115018=DIRECTION('ref_axis',(-0.907612599717117,5.1411739363007E-17,-0.419808728869155));
#115019=DIRECTION('',(-1.56641358065672E-32,-1.,-1.22464674570954E-16));
#115020=DIRECTION('',(-0.907612599717117,5.1411739363007E-17,-0.419808728869155));
#115021=DIRECTION('',(-1.56641358065672E-32,-1.,-1.22464674570954E-16));
#115022=DIRECTION('center_axis',(-1.56641358065672E-32,-1.,-1.22464674570954E-16));
#115023=DIRECTION('ref_axis',(-0.875145004198729,5.92558488100051E-17,-0.483860746109876));
#115024=DIRECTION('',(-1.56641358065672E-32,-1.,-1.22464674570954E-16));
#115025=DIRECTION('center_axis',(-1.56641358065672E-32,-1.,-1.22464674570954E-16));
#115026=DIRECTION('ref_axis',(-0.875145004198729,5.92558488100051E-17,-0.483860746109876));
#115027=DIRECTION('',(-1.56641358065672E-32,-1.,-1.22464674570954E-16));
#115028=DIRECTION('center_axis',(0.603467769136497,9.76517873678849E-17,
-0.797387391180359));
#115029=DIRECTION('ref_axis',(0.79738739118036,-7.39034839613609E-17,0.603467769136497));
#115030=DIRECTION('',(1.56641358065672E-32,1.,1.22464674570954E-16));
#115031=DIRECTION('',(0.797387391180359,-7.39034839613609E-17,0.603467769136497));
#115032=DIRECTION('center_axis',(-1.56641358065672E-32,-1.,-1.22464674570954E-16));
#115033=DIRECTION('ref_axis',(0.0784590959774507,1.22087156847365E-16,-0.996917333713484));
#115034=DIRECTION('',(-1.56641358065672E-32,-1.,-1.22464674570954E-16));
#115035=DIRECTION('center_axis',(-1.56641358065672E-32,-1.,-1.22464674570954E-16));
#115036=DIRECTION('ref_axis',(0.0784590959774507,1.22087156847365E-16,-0.996917333713484));
#115037=DIRECTION('center_axis',(-0.719327468371104,-8.50726751378232E-17,
0.694671140358384));
#115038=DIRECTION('ref_axis',(-0.694671140358384,8.80922043240157E-17,-0.719327468371104));
#115039=DIRECTION('',(-1.56641358065672E-32,-1.,-1.22464674570954E-16));
#115040=DIRECTION('',(-0.694671140358384,8.80922043240157E-17,-0.719327468371104));
#115041=DIRECTION('',(-1.56641358065672E-32,-1.,-1.22464674570954E-16));
#115042=DIRECTION('center_axis',(-1.56641358065672E-32,-1.,-1.22464674570954E-16));
#115043=DIRECTION('ref_axis',(-0.641257749973319,9.3970273644354E-17,-0.767325548968074));
#115044=DIRECTION('',(-1.56641358065672E-32,-1.,-1.22464674570954E-16));
#115045=DIRECTION('center_axis',(-1.56641358065672E-32,-1.,-1.22464674570954E-16));
#115046=DIRECTION('ref_axis',(-0.641257749973319,9.3970273644354E-17,-0.767325548968074));
#115047=DIRECTION('',(-1.56641358065672E-32,-1.,-1.22464674570954E-16));
#115048=DIRECTION('center_axis',(0.850766486309441,6.4360562097336E-17,
-0.525543895191151));
#115049=DIRECTION('ref_axis',(0.525543895191151,-1.0418884088176E-16,0.850766486309441));
#115050=DIRECTION('',(1.56641358065672E-32,1.,1.22464674570954E-16));
#115051=DIRECTION('',(0.525543895191151,-1.0418884088176E-16,0.850766486309441));
#115052=DIRECTION('center_axis',(-1.56641358065672E-32,-1.,-1.22464674570954E-16));
#115053=DIRECTION('ref_axis',(0.0784590959774507,1.22087156847365E-16,-0.996917333713484));
#115054=DIRECTION('',(-1.56641358065672E-32,-1.,-1.22464674570954E-16));
#115055=DIRECTION('center_axis',(-1.56641358065672E-32,-1.,-1.22464674570954E-16));
#115056=DIRECTION('ref_axis',(0.0784590959774507,1.22087156847365E-16,-0.996917333713484));
#115057=DIRECTION('center_axis',(-0.92169704816257,-4.75053324187471E-17,
0.38791049406842));
#115058=DIRECTION('ref_axis',(-0.38791049406842,1.12875329056238E-16,-0.92169704816257));
#115059=DIRECTION('',(-1.56641358065672E-32,-1.,-1.22464674570954E-16));
#115060=DIRECTION('',(-0.38791049406842,1.12875329056238E-16,-0.92169704816257));
#115061=DIRECTION('',(-1.56641358065672E-32,-1.,-1.22464674570954E-16));
#115062=DIRECTION('center_axis',(-1.56641358065672E-32,-1.,-1.22464674570954E-16));
#115063=DIRECTION('ref_axis',(-0.320765085004956,1.15993492128908E-16,-0.947158783014634));
#115064=DIRECTION('',(-1.56641358065672E-32,-1.,-1.22464674570954E-16));
#115065=DIRECTION('center_axis',(-1.56641358065672E-32,-1.,-1.22464674570954E-16));
#115066=DIRECTION('ref_axis',(-0.320765085004956,1.15993492128908E-16,-0.947158783014634));
#115067=DIRECTION('',(-1.56641358065672E-32,-1.,-1.22464674570954E-16));
#115068=DIRECTION('center_axis',(0.983164474478833,2.23770863898615E-17,
-0.18272278490314));
#115069=DIRECTION('ref_axis',(0.18272278490314,-1.20402917416774E-16,0.983164474478834));
#115070=DIRECTION('',(1.56641358065672E-32,1.,1.22464674570954E-16));
#115071=DIRECTION('',(0.18272278490314,-1.20402917416774E-16,0.983164474478833));
#115072=DIRECTION('center_axis',(-1.56641358065672E-32,-1.,-1.22464674570954E-16));
#115073=DIRECTION('ref_axis',(0.0784590959774507,1.22087156847365E-16,-0.996917333713484));
#115074=DIRECTION('',(-1.56641358065672E-32,-1.,-1.22464674570954E-16));
#115075=DIRECTION('center_axis',(-1.56641358065672E-32,-1.,-1.22464674570954E-16));
#115076=DIRECTION('ref_axis',(0.0784590959774507,1.22087156847365E-16,-0.996917333713484));
#115077=DIRECTION('center_axis',(-0.999586334568139,-3.52213118803864E-18,
0.0287603849875744));
#115078=DIRECTION('ref_axis',(-0.0287603849875744,1.2241401516846E-16,-0.999586334568139));
#115079=DIRECTION('',(-1.56641358065672E-32,-1.,-1.22464674570954E-16));
#115080=DIRECTION('',(-0.0287603849875744,1.2241401516846E-16,-0.999586334568139));
#115081=DIRECTION('',(-1.56641358065672E-32,-1.,-1.22464674570954E-16));
#115082=DIRECTION('center_axis',(-1.56641358065672E-32,-1.,-1.22464674570954E-16));
#115083=DIRECTION('ref_axis',(0.0430486839877822,1.2235114684375E-16,-0.999072975716449));
#115084=DIRECTION('',(-1.56641358065672E-32,-1.,-1.22464674570954E-16));
#115085=DIRECTION('center_axis',(-1.56641358065672E-32,-1.,-1.22464674570954E-16));
#115086=DIRECTION('ref_axis',(0.0430486839877822,1.2235114684375E-16,-0.999072975716449));
#115087=DIRECTION('',(-1.56641358065672E-32,-1.,-1.22464674570954E-16));
#115088=DIRECTION('center_axis',(0.982780652540913,-2.26285389436506E-17,
0.184776050913685));
#115089=DIRECTION('ref_axis',(-0.184776050913685,-1.20355912788053E-16,
0.982780652540913));
#115090=DIRECTION('',(1.56641358065672E-32,1.,1.22464674570954E-16));
#115091=DIRECTION('',(-0.184776050913685,-1.20355912788053E-16,0.982780652540913));
#115092=DIRECTION('center_axis',(-1.56641358065672E-32,-1.,-1.22464674570954E-16));
#115093=DIRECTION('ref_axis',(0.0784590959774507,1.22087156847365E-16,-0.996917333713484));
#115094=DIRECTION('center_axis',(-1.56641358065672E-32,-1.,-1.22464674570954E-16));
#115095=DIRECTION('ref_axis',(0.0784590959774507,1.22087156847365E-16,-0.996917333713484));
#115096=DIRECTION('',(0.33427397305035,1.15420010157692E-16,-0.94247594714196));
#115097=DIRECTION('center_axis',(-1.56641358065672E-32,-1.,-1.22464674570954E-16));
#115098=DIRECTION('ref_axis',(0.401048487995911,1.12184601205912E-16,-0.916056826990659));
#115099=DIRECTION('',(-0.52731985596956,-1.04054175252689E-16,0.849666857950952));
#115100=DIRECTION('center_axis',(-1.56641358065672E-32,-1.,-1.22464674570954E-16));
#115101=DIRECTION('ref_axis',(0.0784590959774507,1.22087156847365E-16,-0.996917333713484));
#115102=DIRECTION('',(0.652162777961028,9.28378932524043E-17,-0.758078960954699));
#115103=DIRECTION('center_axis',(-1.56641358065672E-32,-1.,-1.22464674570954E-16));
#115104=DIRECTION('ref_axis',(0.704884471951656,8.68669035655391E-17,-0.709322127951352));
#115105=DIRECTION('',(-0.798646193064008,-7.36993447678216E-17,0.601800846048232));
#115106=DIRECTION('center_axis',(-1.56641358065672E-32,-1.,-1.22464674570954E-16));
#115107=DIRECTION('ref_axis',(0.0784590959774507,1.22087156847365E-16,-0.996917333713484));
#115108=DIRECTION('',(0.881973386681221,5.77175043573365E-17,-0.471299209829655));
#115109=DIRECTION('center_axis',(-1.56641358065672E-32,-1.,-1.22464674570954E-16));
#115110=DIRECTION('ref_axis',(0.913521902831698,4.98173491156488E-17,-0.406789543925055));
#115111=DIRECTION('',(-0.962110936816233,-3.33910092374037E-17,0.272658293947921));
#115112=DIRECTION('center_axis',(-1.56641358065672E-32,-1.,-1.22464674570954E-16));
#115113=DIRECTION('ref_axis',(0.0784590959774507,1.22087156847365E-16,-0.996917333713484));
#115114=DIRECTION('',(0.992668602005981,1.48020466925524E-17,-0.120867889000728));
#115115=DIRECTION('center_axis',(-1.56641358065672E-32,-1.,-1.22464674570954E-16));
#115116=DIRECTION('ref_axis',(0.998783137960738,6.03968575555981E-18,-0.0493177789980613));
#115117=DIRECTION('',(-0.995637266656693,1.14269669163886E-17,-0.0933082699678263));
#115118=DIRECTION('center_axis',(-1.56641358065672E-32,-1.,-1.22464674570954E-16));
#115119=DIRECTION('ref_axis',(0.0784590959774507,1.22087156847365E-16,-0.996917333713484));
#115120=DIRECTION('',(0.969298422184675,-3.01125092835498E-17,0.245887309046847));
#115121=DIRECTION('center_axis',(-1.56641358065672E-32,-1.,-1.22464674570954E-16));
#115122=DIRECTION('ref_axis',(0.949153176178072,-3.85536706080351E-17,0.314814625059063));
#115123=DIRECTION('',(-0.894697266701741,5.47016679751246E-17,-0.446673035851096));
#115124=DIRECTION('center_axis',(-1.56641358065672E-32,-1.,-1.22464674570954E-16));
#115125=DIRECTION('ref_axis',(0.0784590959774507,1.22087156847365E-16,-0.996917333713484));
#115126=DIRECTION('',(0.815019118992681,-7.09602042049129E-17,0.579434064994797));
#115127=DIRECTION('center_axis',(-1.56641358065672E-32,-1.,-1.22464674570954E-16));
#115128=DIRECTION('ref_axis',(0.771334818374299,-7.79401402152037E-17,0.636429570308834));
#115129=DIRECTION('',(-0.67292344359886,9.05886055900302E-17,-0.739712132559046));
#115130=DIRECTION('center_axis',(-1.56641358065672E-32,-1.,-1.22464674570954E-16));
#115131=DIRECTION('ref_axis',(0.0784590959774507,1.22087156847365E-16,-0.996917333713484));
#115132=DIRECTION('',(0.550666967895411,-1.02224330237946E-16,0.834725038841459));
#115133=DIRECTION('center_axis',(-1.56641358065672E-32,-1.,-1.22464674570954E-16));
#115134=DIRECTION('ref_axis',(0.489343419188033,-1.06800361983615E-16,0.872091175335105));
#115135=DIRECTION('',(-0.360267580169336,1.14241050119789E-16,-0.932849007438466));
#115136=DIRECTION('center_axis',(-1.56641358065672E-32,-1.,-1.22464674570954E-16));
#115137=DIRECTION('ref_axis',(0.0784590959774507,1.22087156847365E-16,-0.996917333713484));
#115138=DIRECTION('',(0.211944190997081,-1.19682494047993E-16,0.977281770986542));
#115139=DIRECTION('center_axis',(-1.56641358065672E-32,-1.,-1.22464674570954E-16));
#115140=DIRECTION('ref_axis',(0.141263479938992,-1.21236603048261E-16,0.989972034572455));
#115141=DIRECTION('',(0.00104441599957958,1.2246460777841E-16,-0.999999454597461));
#115142=DIRECTION('center_axis',(-1.56641358065672E-32,-1.,-1.22464674570954E-16));
#115143=DIRECTION('ref_axis',(-0.0784590959774507,-1.22087156847365E-16,
0.996917333713484));
#115144=DIRECTION('',(-0.155402821938502,-1.20976873847682E-16,0.987851184609074));
#115145=DIRECTION('center_axis',(0.987851184609074,-1.90313560161066E-17,
0.155402821938502));
#115146=DIRECTION('ref_axis',(-0.155402821938502,-1.20976873847682E-16,
0.987851184609074));
#115147=DIRECTION('',(-1.56641358065672E-32,-1.,-1.22464674570954E-16));
#115148=DIRECTION('',(-1.56641358065672E-32,-1.,-1.22464674570954E-16));
#115149=DIRECTION('center_axis',(-1.56641358065672E-32,-1.,-1.22464674570954E-16));
#115150=DIRECTION('ref_axis',(-0.0784590959774507,-1.22087156847365E-16,
0.996917333713484));
#115151=DIRECTION('',(1.56641358065672E-32,1.,1.22464674570954E-16));
#115152=DIRECTION('center_axis',(-0.999999454597461,1.27904065505227E-19,
-0.00104441599957958));
#115153=DIRECTION('ref_axis',(0.00104441599957958,1.2246460777841E-16,-0.999999454597461));
#115154=DIRECTION('',(-1.56641358065672E-32,-1.,-1.22464674570954E-16));
#115155=DIRECTION('',(-1.56641358065672E-32,-1.,-1.22464674570954E-16));
#115156=DIRECTION('center_axis',(-1.56641358065672E-32,-1.,-1.22464674570954E-16));
#115157=DIRECTION('ref_axis',(0.141263479938992,-1.21236603048261E-16,0.989972034572455));
#115158=DIRECTION('',(-1.56641358065672E-32,-1.,-1.22464674570954E-16));
#115159=DIRECTION('',(-1.56641358065672E-32,-1.,-1.22464674570954E-16));
#115160=DIRECTION('center_axis',(0.977281770986542,2.59556763776617E-17,
-0.211944190997081));
#115161=DIRECTION('ref_axis',(0.211944190997081,-1.19682494047993E-16,0.977281770986542));
#115162=DIRECTION('',(-1.56641358065672E-32,-1.,-1.22464674570954E-16));
#115163=DIRECTION('center_axis',(-1.56641358065672E-32,-1.,-1.22464674570954E-16));
#115164=DIRECTION('ref_axis',(0.0784590959774507,1.22087156847365E-16,-0.996917333713484));
#115165=DIRECTION('',(1.56641358065672E-32,1.,1.22464674570954E-16));
#115166=DIRECTION('center_axis',(0.834725038841459,6.74372510202856E-17,
-0.550666967895411));
#115167=DIRECTION('ref_axis',(0.550666967895411,-1.02224330237946E-16,0.834725038841459));
#115168=DIRECTION('',(-1.56641358065672E-32,-1.,-1.22464674570954E-16));
#115169=DIRECTION('',(-1.56641358065672E-32,-1.,-1.22464674570954E-16));
#115170=DIRECTION('center_axis',(-0.932849007438466,-4.41200519639029E-17,
0.360267580169336));
#115171=DIRECTION('ref_axis',(-0.360267580169336,1.14241050119789E-16,-0.932849007438466));
#115172=DIRECTION('',(-1.56641358065672E-32,-1.,-1.22464674570954E-16));
#115173=DIRECTION('',(-1.56641358065672E-32,-1.,-1.22464674570954E-16));
#115174=DIRECTION('center_axis',(-1.56641358065672E-32,-1.,-1.22464674570954E-16));
#115175=DIRECTION('ref_axis',(0.489343419188033,-1.06800361983615E-16,0.872091175335105));
#115176=DIRECTION('',(-1.56641358065672E-32,-1.,-1.22464674570954E-16));
#115177=DIRECTION('center_axis',(-0.739712132559046,-8.24093505315003E-17,
0.67292344359886));
#115178=DIRECTION('ref_axis',(-0.67292344359886,9.05886055900302E-17,-0.739712132559046));
#115179=DIRECTION('',(1.56641358065672E-32,1.,1.22464674570954E-16));
#115180=DIRECTION('',(-1.56641358065672E-32,-1.,-1.22464674570954E-16));
#115181=DIRECTION('center_axis',(0.579434064994797,9.98110511765445E-17,
-0.815019118992681));
#115182=DIRECTION('ref_axis',(0.815019118992681,-7.09602042049129E-17,0.579434064994797));
#115183=DIRECTION('',(-1.56641358065672E-32,-1.,-1.22464674570954E-16));
#115184=DIRECTION('',(-1.56641358065672E-32,-1.,-1.22464674570954E-16));
#115185=DIRECTION('',(-1.56641358065672E-32,-1.,-1.22464674570954E-16));
#115186=DIRECTION('center_axis',(-1.56641358065672E-32,-1.,-1.22464674570954E-16));
#115187=DIRECTION('ref_axis',(0.771334818374299,-7.79401402152037E-17,0.636429570308834));
#115188=DIRECTION('',(-1.56641358065672E-32,-1.,-1.22464674570954E-16));
#115189=DIRECTION('center_axis',(-1.56641358065672E-32,-1.,-1.22464674570954E-16));
#115190=DIRECTION('ref_axis',(0.0784590959774507,1.22087156847365E-16,-0.996917333713484));
#115191=DIRECTION('',(1.56641358065672E-32,1.,1.22464674570954E-16));
#115192=DIRECTION('center_axis',(-0.446673035851096,-1.09568809606151E-16,
0.894697266701741));
#115193=DIRECTION('ref_axis',(-0.894697266701741,5.47016679751246E-17,-0.446673035851096));
#115194=DIRECTION('',(-1.56641358065672E-32,-1.,-1.22464674570954E-16));
#115195=DIRECTION('',(-1.56641358065672E-32,-1.,-1.22464674570954E-16));
#115196=DIRECTION('center_axis',(-1.56641358065672E-32,-1.,-1.22464674570954E-16));
#115197=DIRECTION('ref_axis',(0.949153176178072,-3.85536706080351E-17,0.314814625059063));
#115198=DIRECTION('',(-1.56641358065672E-32,-1.,-1.22464674570954E-16));
#115199=DIRECTION('',(-1.56641358065672E-32,-1.,-1.22464674570954E-16));
#115200=DIRECTION('center_axis',(0.245887309046847,1.18704815834986E-16,
-0.969298422184675));
#115201=DIRECTION('ref_axis',(0.969298422184675,-3.01125092835499E-17,0.245887309046847));
#115202=DIRECTION('',(-1.56641358065672E-32,-1.,-1.22464674570954E-16));
#115203=DIRECTION('center_axis',(-1.56641358065672E-32,-1.,-1.22464674570954E-16));
#115204=DIRECTION('ref_axis',(0.0784590959774507,1.22087156847365E-16,-0.996917333713484));
#115205=DIRECTION('center_axis',(-1.56641358065672E-32,-1.,-1.22464674570954E-16));
#115206=DIRECTION('ref_axis',(0.0784590959774507,1.22087156847365E-16,-0.996917333713484));
#115207=DIRECTION('',(1.56641358065672E-32,1.,1.22464674570954E-16));
#115208=DIRECTION('center_axis',(-0.120867889000728,1.21566837301467E-16,
-0.992668602005981));
#115209=DIRECTION('ref_axis',(0.992668602005981,1.48020466925524E-17,-0.120867889000728));
#115210=DIRECTION('',(-1.56641358065672E-32,-1.,-1.22464674570954E-16));
#115211=DIRECTION('',(-1.56641358065672E-32,-1.,-1.22464674570954E-16));
#115212=DIRECTION('center_axis',(-0.0933082699678263,-1.21930393851826E-16,
0.995637266656693));
#115213=DIRECTION('ref_axis',(-0.995637266656693,1.14269669163886E-17,-0.0933082699678263));
#115214=DIRECTION('',(-1.56641358065672E-32,-1.,-1.22464674570954E-16));
#115215=DIRECTION('',(-1.56641358065672E-32,-1.,-1.22464674570954E-16));
#115216=DIRECTION('center_axis',(-1.56641358065672E-32,-1.,-1.22464674570954E-16));
#115217=DIRECTION('ref_axis',(0.998783137960738,6.03968575555981E-18,-0.0493177789980613));
#115218=DIRECTION('',(-1.56641358065672E-32,-1.,-1.22464674570954E-16));
#115219=DIRECTION('center_axis',(0.272658293947921,-1.17824602778356E-16,
0.962110936816233));
#115220=DIRECTION('ref_axis',(-0.962110936816233,-3.33910092374037E-17,
0.272658293947921));
#115221=DIRECTION('',(1.56641358065672E-32,1.,1.22464674570954E-16));
#115222=DIRECTION('',(-1.56641358065672E-32,-1.,-1.22464674570954E-16));
#115223=DIRECTION('center_axis',(-0.471299209829655,1.08010583780158E-16,
-0.881973386681221));
#115224=DIRECTION('ref_axis',(0.881973386681221,5.77175043573365E-17,-0.471299209829655));
#115225=DIRECTION('',(-1.56641358065672E-32,-1.,-1.22464674570954E-16));
#115226=DIRECTION('',(-1.56641358065672E-32,-1.,-1.22464674570954E-16));
#115227=DIRECTION('',(-1.56641358065672E-32,-1.,-1.22464674570954E-16));
#115228=DIRECTION('center_axis',(-1.56641358065672E-32,-1.,-1.22464674570954E-16));
#115229=DIRECTION('ref_axis',(0.913521902831698,4.98173491156488E-17,-0.406789543925055));
#115230=DIRECTION('',(-1.56641358065672E-32,-1.,-1.22464674570954E-16));
#115231=DIRECTION('center_axis',(-1.56641358065672E-32,-1.,-1.22464674570954E-16));
#115232=DIRECTION('ref_axis',(0.0784590959774507,1.22087156847365E-16,-0.996917333713484));
#115233=DIRECTION('',(1.56641358065672E-32,1.,1.22464674570954E-16));
#115234=DIRECTION('center_axis',(0.601800846048232,-9.78059461309152E-17,
0.798646193064008));
#115235=DIRECTION('ref_axis',(-0.798646193064008,-7.36993447678216E-17,
0.601800846048232));
#115236=DIRECTION('',(-1.56641358065672E-32,-1.,-1.22464674570954E-16));
#115237=DIRECTION('',(-1.56641358065672E-32,-1.,-1.22464674570954E-16));
#115238=DIRECTION('center_axis',(-1.56641358065672E-32,-1.,-1.22464674570954E-16));
#115239=DIRECTION('ref_axis',(0.704884471951656,8.68669035655391E-17,-0.709322127951352));
#115240=DIRECTION('',(-1.56641358065672E-32,-1.,-1.22464674570954E-16));
#115241=DIRECTION('',(-1.56641358065672E-32,-1.,-1.22464674570954E-16));
#115242=DIRECTION('center_axis',(-0.758078960954699,7.98669023702868E-17,
-0.652162777961028));
#115243=DIRECTION('ref_axis',(0.652162777961028,9.28378932524043E-17,-0.758078960954699));
#115244=DIRECTION('',(-1.56641358065672E-32,-1.,-1.22464674570954E-16));
#115245=DIRECTION('center_axis',(-1.56641358065672E-32,-1.,-1.22464674570954E-16));
#115246=DIRECTION('ref_axis',(0.0784590959774507,1.22087156847365E-16,-0.996917333713484));
#115247=DIRECTION('center_axis',(-1.56641358065672E-32,-1.,-1.22464674570954E-16));
#115248=DIRECTION('ref_axis',(0.0784590959774507,1.22087156847365E-16,-0.996917333713484));
#115249=DIRECTION('',(1.56641358065672E-32,1.,1.22464674570954E-16));
#115250=DIRECTION('center_axis',(-0.94247594714196,4.0936753327151E-17,
-0.33427397305035));
#115251=DIRECTION('ref_axis',(0.33427397305035,1.15420010157692E-16,-0.94247594714196));
#115252=DIRECTION('',(-1.56641358065672E-32,-1.,-1.22464674570954E-16));
#115253=DIRECTION('',(-1.56641358065672E-32,-1.,-1.22464674570954E-16));
#115254=DIRECTION('center_axis',(0.849666857950952,-6.45780545561146E-17,
0.52731985596956));
#115255=DIRECTION('ref_axis',(-0.52731985596956,-1.04054175252689E-16,0.849666857950952));
#115256=DIRECTION('',(-1.56641358065672E-32,-1.,-1.22464674570954E-16));
#115257=DIRECTION('',(-1.56641358065672E-32,-1.,-1.22464674570954E-16));
#115258=DIRECTION('center_axis',(-1.56641358065672E-32,-1.,-1.22464674570954E-16));
#115259=DIRECTION('ref_axis',(0.401048487995911,1.12184601205912E-16,-0.916056826990659));
#115260=DIRECTION('',(-1.56641358065672E-32,-1.,-1.22464674570954E-16));
#115261=DIRECTION('center_axis',(-1.56641358065672E-32,-1.,-1.22464674570954E-16));
#115262=DIRECTION('ref_axis',(0.0784590959774507,1.22087156847365E-16,-0.996917333713484));
#115263=DIRECTION('center_axis',(-1.56641358065672E-32,-1.,-1.22464674570954E-16));
#115264=DIRECTION('ref_axis',(0.93969262091562,-4.18853855054452E-17,0.342020142969288));
#115265=DIRECTION('',(1.56641358065672E-32,1.,1.22464674570954E-16));
#115266=DIRECTION('center_axis',(1.56641358065672E-32,1.,1.22464674570954E-16));
#115267=DIRECTION('ref_axis',(0.93969262091562,-4.18853855054452E-17,0.342020142969288));
#115268=DIRECTION('center_axis',(1.56641358065672E-32,1.,1.22464674570954E-16));
#115269=DIRECTION('ref_axis',(0.0784590959774507,1.22087156847365E-16,-0.996917333713484));
#115270=DIRECTION('axis',(0.,0.,1.));
#115271=DIRECTION('refdir',(1.,0.,0.));
#115272=DIRECTION('center_axis',(0.,0.,1.));
#115273=DIRECTION('ref_axis',(1.,0.,0.));
#115274=DIRECTION('center_axis',(0.,0.,-1.));
#115275=DIRECTION('ref_axis',(1.,0.,0.));
#115276=DIRECTION('center_axis',(1.22464679914735E-16,-1.,0.));
#115277=DIRECTION('ref_axis',(-1.,-1.22464679914735E-16,0.));
#115278=DIRECTION('center_axis',(0.,0.,1.));
#115279=DIRECTION('ref_axis',(1.,0.,0.));
#115280=DIRECTION('center_axis',(0.,0.,1.));
#115281=DIRECTION('ref_axis',(1.,0.,0.));
#115282=DIRECTION('center_axis',(0.,0.,1.));
#115283=DIRECTION('ref_axis',(1.,0.,0.));
#115284=DIRECTION('center_axis',(0.,0.,1.));
#115285=DIRECTION('ref_axis',(1.,0.,0.));
#115286=DIRECTION('',(0.,0.,1.));
#115287=DIRECTION('center_axis',(0.,0.,1.));
#115288=DIRECTION('ref_axis',(1.,0.,0.));
#115289=DIRECTION('',(0.,0.,1.));
#115290=DIRECTION('center_axis',(0.,0.,-1.));
#115291=DIRECTION('ref_axis',(1.,0.,0.));
#115292=DIRECTION('',(0.,0.,1.));
#115293=DIRECTION('center_axis',(0.,0.,-1.));
#115294=DIRECTION('ref_axis',(1.,0.,0.));
#115295=DIRECTION('center_axis',(0.,0.,-1.));
#115296=DIRECTION('ref_axis',(1.,0.,0.));
#115297=DIRECTION('center_axis',(0.,0.,-1.));
#115298=DIRECTION('ref_axis',(1.,0.,0.));
#115299=DIRECTION('',(0.,0.,-1.));
#115300=DIRECTION('center_axis',(0.,0.,1.));
#115301=DIRECTION('ref_axis',(1.,0.,0.));
#115302=DIRECTION('center_axis',(0.,0.,1.));
#115303=DIRECTION('ref_axis',(1.,0.,0.));
#115304=DIRECTION('',(0.,0.,1.));
#115305=DIRECTION('center_axis',(0.,0.,-1.));
#115306=DIRECTION('ref_axis',(1.,0.,0.));
#115307=DIRECTION('',(0.,0.,-1.));
#115308=DIRECTION('center_axis',(0.,0.,1.));
#115309=DIRECTION('ref_axis',(1.,0.,0.));
#115310=DIRECTION('',(0.,0.,1.));
#115311=DIRECTION('center_axis',(0.,0.,-1.));
#115312=DIRECTION('ref_axis',(1.,0.,0.));
#115313=DIRECTION('',(0.,0.,-1.));
#115314=DIRECTION('center_axis',(0.,0.,1.));
#115315=DIRECTION('ref_axis',(1.,0.,0.));
#115316=DIRECTION('',(0.,0.,1.));
#115317=DIRECTION('center_axis',(0.,0.,-1.));
#115318=DIRECTION('ref_axis',(1.,0.,0.));
#115319=DIRECTION('',(0.,0.,-1.));
#115320=DIRECTION('center_axis',(0.,0.,1.));
#115321=DIRECTION('ref_axis',(1.,0.,0.));
#115322=DIRECTION('',(0.,0.,1.));
#115323=DIRECTION('center_axis',(0.,0.,-1.));
#115324=DIRECTION('ref_axis',(1.,0.,0.));
#115325=DIRECTION('',(0.,0.,-1.));
#115326=DIRECTION('center_axis',(0.,0.,1.));
#115327=DIRECTION('ref_axis',(1.,0.,0.));
#115328=DIRECTION('',(0.,0.,1.));
#115329=DIRECTION('center_axis',(0.,0.,-1.));
#115330=DIRECTION('ref_axis',(1.,0.,0.));
#115331=DIRECTION('',(0.,0.,-1.));
#115332=DIRECTION('center_axis',(0.,0.,1.));
#115333=DIRECTION('ref_axis',(1.,0.,0.));
#115334=DIRECTION('',(0.,0.,1.));
#115335=DIRECTION('center_axis',(0.,0.,-1.));
#115336=DIRECTION('ref_axis',(1.,0.,0.));
#115337=DIRECTION('',(0.,0.,-1.));
#115338=DIRECTION('center_axis',(0.,0.,1.));
#115339=DIRECTION('ref_axis',(1.,0.,0.));
#115340=DIRECTION('',(0.,0.,1.));
#115341=DIRECTION('center_axis',(0.,0.,-1.));
#115342=DIRECTION('ref_axis',(1.,0.,0.));
#115343=DIRECTION('',(0.,0.,-1.));
#115344=DIRECTION('center_axis',(0.,0.,-1.));
#115345=DIRECTION('ref_axis',(-1.,0.,0.));
#115346=DIRECTION('center_axis',(-1.22464679914735E-16,-1.,0.));
#115347=DIRECTION('ref_axis',(1.,-1.22464679914735E-16,0.));
#115348=DIRECTION('center_axis',(0.,0.,-1.));
#115349=DIRECTION('ref_axis',(1.,0.,0.));
#115350=DIRECTION('center_axis',(0.,0.,-1.));
#115351=DIRECTION('ref_axis',(1.,0.,0.));
#115352=DIRECTION('center_axis',(0.,0.,1.));
#115353=DIRECTION('ref_axis',(1.,0.,0.));
#115354=DIRECTION('center_axis',(0.,0.,1.));
#115355=DIRECTION('ref_axis',(1.,0.,0.));
#115356=DIRECTION('',(0.,0.,-1.));
#115357=DIRECTION('center_axis',(0.,0.,1.));
#115358=DIRECTION('ref_axis',(1.,0.,0.));
#115359=DIRECTION('',(0.,0.,-1.));
#115360=DIRECTION('center_axis',(0.,0.,-1.));
#115361=DIRECTION('ref_axis',(1.,0.,0.));
#115362=DIRECTION('',(0.,0.,-1.));
#115363=DIRECTION('center_axis',(0.,0.,-1.));
#115364=DIRECTION('ref_axis',(1.,0.,0.));
#115365=DIRECTION('',(0.,0.,1.));
#115366=DIRECTION('center_axis',(0.,0.,1.));
#115367=DIRECTION('ref_axis',(1.,0.,0.));
#115368=DIRECTION('center_axis',(0.,0.,-1.));
#115369=DIRECTION('ref_axis',(1.,0.,0.));
#115370=DIRECTION('',(0.,0.,1.));
#115371=DIRECTION('center_axis',(0.,0.,1.));
#115372=DIRECTION('ref_axis',(1.,0.,0.));
#115373=DIRECTION('',(0.,0.,-1.));
#115374=DIRECTION('center_axis',(0.,0.,-1.));
#115375=DIRECTION('ref_axis',(1.,0.,0.));
#115376=DIRECTION('',(0.,0.,1.));
#115377=DIRECTION('center_axis',(0.,0.,1.));
#115378=DIRECTION('ref_axis',(1.,0.,0.));
#115379=DIRECTION('',(0.,0.,-1.));
#115380=DIRECTION('center_axis',(0.,0.,-1.));
#115381=DIRECTION('ref_axis',(1.,0.,0.));
#115382=DIRECTION('',(0.,0.,1.));
#115383=DIRECTION('center_axis',(0.,0.,1.));
#115384=DIRECTION('ref_axis',(1.,0.,0.));
#115385=DIRECTION('',(0.,0.,-1.));
#115386=DIRECTION('center_axis',(0.,0.,-1.));
#115387=DIRECTION('ref_axis',(1.,0.,0.));
#115388=DIRECTION('',(0.,0.,1.));
#115389=DIRECTION('center_axis',(0.,0.,1.));
#115390=DIRECTION('ref_axis',(1.,0.,0.));
#115391=DIRECTION('',(0.,0.,-1.));
#115392=DIRECTION('center_axis',(0.,0.,-1.));
#115393=DIRECTION('ref_axis',(1.,0.,0.));
#115394=DIRECTION('',(0.,0.,1.));
#115395=DIRECTION('center_axis',(0.,0.,1.));
#115396=DIRECTION('ref_axis',(1.,0.,0.));
#115397=DIRECTION('',(0.,0.,-1.));
#115398=DIRECTION('center_axis',(0.,0.,-1.));
#115399=DIRECTION('ref_axis',(1.,0.,0.));
#115400=DIRECTION('',(0.,0.,1.));
#115401=DIRECTION('center_axis',(0.,0.,1.));
#115402=DIRECTION('ref_axis',(1.,0.,0.));
#115403=DIRECTION('',(0.,0.,-1.));
#115404=DIRECTION('center_axis',(0.,0.,-1.));
#115405=DIRECTION('ref_axis',(1.,0.,0.));
#115406=DIRECTION('',(0.,0.,1.));
#115407=DIRECTION('center_axis',(0.,0.,1.));
#115408=DIRECTION('ref_axis',(1.,0.,0.));
#115409=DIRECTION('',(0.,0.,-1.));
#115410=DIRECTION('center_axis',(0.,0.,1.));
#115411=DIRECTION('ref_axis',(1.,0.,0.));
#115412=DIRECTION('center_axis',(0.,0.,-1.));
#115413=DIRECTION('ref_axis',(1.,0.,0.));
#115414=DIRECTION('center_axis',(1.22464679914735E-16,-1.,0.));
#115415=DIRECTION('ref_axis',(-1.,-1.22464679914735E-16,0.));
#115416=DIRECTION('center_axis',(0.,0.,1.));
#115417=DIRECTION('ref_axis',(1.,0.,0.));
#115418=DIRECTION('center_axis',(0.,0.,1.));
#115419=DIRECTION('ref_axis',(1.,0.,0.));
#115420=DIRECTION('center_axis',(0.,0.,-1.));
#115421=DIRECTION('ref_axis',(-1.,0.,0.));
#115422=DIRECTION('center_axis',(-1.22464679914735E-16,-1.,0.));
#115423=DIRECTION('ref_axis',(1.,-1.22464679914735E-16,0.));
#115424=DIRECTION('center_axis',(0.,0.,1.));
#115425=DIRECTION('ref_axis',(0.707106781186547,-0.707106781186548,0.));
#115426=DIRECTION('center_axis',(0.,0.,1.));
#115427=DIRECTION('ref_axis',(0.707106781186547,-0.707106781186548,0.));
#115428=DIRECTION('center_axis',(0.,0.,1.));
#115429=DIRECTION('ref_axis',(0.707106781186547,-0.707106781186548,0.));
#115430=DIRECTION('center_axis',(0.,0.,1.));
#115431=DIRECTION('ref_axis',(0.707106781186547,-0.707106781186548,0.));
#115432=DIRECTION('center_axis',(0.,0.,-1.));
#115433=DIRECTION('ref_axis',(0.707106781186547,-0.707106781186548,0.));
#115434=DIRECTION('center_axis',(0.,0.,1.));
#115435=DIRECTION('ref_axis',(0.707106781186547,-0.707106781186548,0.));
#115436=DIRECTION('center_axis',(0.,0.,-1.));
#115437=DIRECTION('ref_axis',(0.707106781186547,-0.707106781186548,0.));
#115438=DIRECTION('center_axis',(0.,0.,1.));
#115439=DIRECTION('ref_axis',(0.707106781186547,-0.707106781186548,0.));
#115440=DIRECTION('center_axis',(0.,0.,1.));
#115441=DIRECTION('ref_axis',(-1.83697019872103E-16,-1.,0.));
#115442=DIRECTION('center_axis',(0.,0.,1.));
#115443=DIRECTION('ref_axis',(-1.83697019872103E-16,-1.,0.));
#115444=DIRECTION('center_axis',(0.,0.,1.));
#115445=DIRECTION('ref_axis',(-1.83697019872103E-16,-1.,0.));
#115446=DIRECTION('center_axis',(0.,0.,1.));
#115447=DIRECTION('ref_axis',(-1.83697019872103E-16,-1.,0.));
#115448=DIRECTION('center_axis',(0.,0.,-1.));
#115449=DIRECTION('ref_axis',(-1.83697019872103E-16,-1.,0.));
#115450=DIRECTION('center_axis',(0.,0.,1.));
#115451=DIRECTION('ref_axis',(-1.83697019872103E-16,-1.,0.));
#115452=DIRECTION('center_axis',(0.,0.,-1.));
#115453=DIRECTION('ref_axis',(-1.83697019872103E-16,-1.,0.));
#115454=DIRECTION('center_axis',(0.,0.,1.));
#115455=DIRECTION('ref_axis',(-1.83697019872103E-16,-1.,0.));
#115456=DIRECTION('center_axis',(0.,0.,1.));
#115457=DIRECTION('ref_axis',(-0.707106781186548,-0.707106781186547,0.));
#115458=DIRECTION('center_axis',(0.,0.,1.));
#115459=DIRECTION('ref_axis',(-0.707106781186548,-0.707106781186548,0.));
#115460=DIRECTION('center_axis',(0.,0.,1.));
#115461=DIRECTION('ref_axis',(-0.707106781186548,-0.707106781186548,0.));
#115462=DIRECTION('center_axis',(0.,0.,1.));
#115463=DIRECTION('ref_axis',(-0.707106781186548,-0.707106781186548,0.));
#115464=DIRECTION('center_axis',(0.,0.,-1.));
#115465=DIRECTION('ref_axis',(-0.707106781186548,-0.707106781186548,0.));
#115466=DIRECTION('center_axis',(0.,0.,1.));
#115467=DIRECTION('ref_axis',(-0.707106781186548,-0.707106781186547,0.));
#115468=DIRECTION('center_axis',(0.,0.,-1.));
#115469=DIRECTION('ref_axis',(-0.707106781186548,-0.707106781186548,0.));
#115470=DIRECTION('center_axis',(0.,0.,1.));
#115471=DIRECTION('ref_axis',(-0.707106781186548,-0.707106781186548,0.));
#115472=DIRECTION('center_axis',(0.,0.,1.));
#115473=DIRECTION('ref_axis',(-1.,1.22464679914735E-16,0.));
#115474=DIRECTION('center_axis',(0.,0.,1.));
#115475=DIRECTION('ref_axis',(-1.,1.22464679914735E-16,0.));
#115476=DIRECTION('center_axis',(0.,0.,1.));
#115477=DIRECTION('ref_axis',(-1.,1.22464679914735E-16,0.));
#115478=DIRECTION('center_axis',(0.,0.,1.));
#115479=DIRECTION('ref_axis',(-1.,1.22464679914735E-16,0.));
#115480=DIRECTION('center_axis',(0.,0.,-1.));
#115481=DIRECTION('ref_axis',(-1.,1.22464679914735E-16,0.));
#115482=DIRECTION('center_axis',(0.,0.,1.));
#115483=DIRECTION('ref_axis',(-1.,1.22464679914735E-16,0.));
#115484=DIRECTION('center_axis',(0.,0.,-1.));
#115485=DIRECTION('ref_axis',(-1.,1.22464679914735E-16,0.));
#115486=DIRECTION('center_axis',(0.,0.,1.));
#115487=DIRECTION('ref_axis',(-1.,1.22464679914735E-16,0.));
#115488=DIRECTION('center_axis',(0.,0.,1.));
#115489=DIRECTION('ref_axis',(-0.707106781186547,0.707106781186548,0.));
#115490=DIRECTION('center_axis',(0.,0.,1.));
#115491=DIRECTION('ref_axis',(-0.707106781186548,0.707106781186548,0.));
#115492=DIRECTION('center_axis',(0.,0.,1.));
#115493=DIRECTION('ref_axis',(-0.707106781186548,0.707106781186548,0.));
#115494=DIRECTION('center_axis',(0.,0.,1.));
#115495=DIRECTION('ref_axis',(-0.707106781186548,0.707106781186548,0.));
#115496=DIRECTION('center_axis',(0.,0.,-1.));
#115497=DIRECTION('ref_axis',(-0.707106781186548,0.707106781186548,0.));
#115498=DIRECTION('center_axis',(0.,0.,1.));
#115499=DIRECTION('ref_axis',(-0.707106781186547,0.707106781186548,0.));
#115500=DIRECTION('center_axis',(0.,0.,-1.));
#115501=DIRECTION('ref_axis',(-0.707106781186548,0.707106781186548,0.));
#115502=DIRECTION('center_axis',(0.,0.,1.));
#115503=DIRECTION('ref_axis',(-0.707106781186548,0.707106781186548,0.));
#115504=DIRECTION('center_axis',(0.,0.,1.));
#115505=DIRECTION('ref_axis',(6.12323399573677E-17,1.,0.));
#115506=DIRECTION('center_axis',(0.,0.,1.));
#115507=DIRECTION('ref_axis',(6.12323399573677E-17,1.,0.));
#115508=DIRECTION('center_axis',(0.,0.,1.));
#115509=DIRECTION('ref_axis',(6.12323399573677E-17,1.,0.));
#115510=DIRECTION('center_axis',(0.,0.,1.));
#115511=DIRECTION('ref_axis',(6.12323399573677E-17,1.,0.));
#115512=DIRECTION('center_axis',(0.,0.,-1.));
#115513=DIRECTION('ref_axis',(6.12323399573677E-17,1.,0.));
#115514=DIRECTION('center_axis',(0.,0.,1.));
#115515=DIRECTION('ref_axis',(6.12323399573677E-17,1.,0.));
#115516=DIRECTION('center_axis',(0.,0.,-1.));
#115517=DIRECTION('ref_axis',(6.12323399573677E-17,1.,0.));
#115518=DIRECTION('center_axis',(0.,0.,1.));
#115519=DIRECTION('ref_axis',(6.12323399573677E-17,1.,0.));
#115520=DIRECTION('center_axis',(0.,0.,1.));
#115521=DIRECTION('ref_axis',(0.707106781186548,0.707106781186548,0.));
#115522=DIRECTION('center_axis',(0.,0.,1.));
#115523=DIRECTION('ref_axis',(0.707106781186548,0.707106781186548,0.));
#115524=DIRECTION('center_axis',(0.,0.,1.));
#115525=DIRECTION('ref_axis',(0.707106781186548,0.707106781186548,0.));
#115526=DIRECTION('center_axis',(0.,0.,1.));
#115527=DIRECTION('ref_axis',(0.707106781186548,0.707106781186548,0.));
#115528=DIRECTION('center_axis',(0.,0.,-1.));
#115529=DIRECTION('ref_axis',(0.707106781186548,0.707106781186548,0.));
#115530=DIRECTION('center_axis',(0.,0.,1.));
#115531=DIRECTION('ref_axis',(0.707106781186548,0.707106781186548,0.));
#115532=DIRECTION('center_axis',(0.,0.,-1.));
#115533=DIRECTION('ref_axis',(0.707106781186548,0.707106781186548,0.));
#115534=DIRECTION('center_axis',(0.,0.,1.));
#115535=DIRECTION('ref_axis',(0.707106781186548,0.707106781186548,0.));
#115536=DIRECTION('center_axis',(0.,0.,1.));
#115537=DIRECTION('ref_axis',(1.,0.,0.));
#115538=DIRECTION('center_axis',(0.,0.,1.));
#115539=DIRECTION('ref_axis',(1.,0.,0.));
#115540=DIRECTION('center_axis',(0.,0.,1.));
#115541=DIRECTION('ref_axis',(1.,0.,0.));
#115542=DIRECTION('center_axis',(0.,0.,1.));
#115543=DIRECTION('ref_axis',(1.,0.,0.));
#115544=DIRECTION('center_axis',(0.,0.,-1.));
#115545=DIRECTION('ref_axis',(1.,0.,0.));
#115546=DIRECTION('center_axis',(0.,0.,1.));
#115547=DIRECTION('ref_axis',(1.,0.,0.));
#115548=DIRECTION('center_axis',(0.,0.,-1.));
#115549=DIRECTION('ref_axis',(1.,0.,0.));
#115550=DIRECTION('center_axis',(0.,0.,1.));
#115551=DIRECTION('ref_axis',(1.,0.,0.));
#115552=DIRECTION('center_axis',(0.,0.,1.));
#115553=DIRECTION('ref_axis',(1.,0.,0.));
#115554=DIRECTION('center_axis',(0.,0.,-1.));
#115555=DIRECTION('ref_axis',(1.,0.,0.));
#115556=DIRECTION('',(0.707106781186547,8.65956056235493E-17,-0.707106781186548));
#115557=DIRECTION('center_axis',(0.,0.,1.));
#115558=DIRECTION('ref_axis',(1.,0.,0.));
#115559=DIRECTION('center_axis',(0.,0.,1.));
#115560=DIRECTION('ref_axis',(1.,0.,0.));
#115561=DIRECTION('center_axis',(0.,0.,1.));
#115562=DIRECTION('ref_axis',(1.,0.,0.));
#115563=DIRECTION('',(0.,0.,-1.));
#115564=DIRECTION('center_axis',(0.,0.,1.));
#115565=DIRECTION('ref_axis',(1.,0.,0.));
#115566=DIRECTION('center_axis',(0.,0.,-1.));
#115567=DIRECTION('ref_axis',(1.,0.,0.));
#115568=DIRECTION('',(0.707106781186547,-8.65956056235493E-17,0.707106781186548));
#115569=DIRECTION('center_axis',(0.,0.,-1.));
#115570=DIRECTION('ref_axis',(1.,0.,0.));
#115571=DIRECTION('center_axis',(0.,0.,1.));
#115572=DIRECTION('ref_axis',(1.,0.,0.));
#115573=DIRECTION('center_axis',(0.,0.,1.));
#115574=DIRECTION('ref_axis',(0.707106781186548,0.707106781186548,0.));
#115575=DIRECTION('center_axis',(0.,0.,-1.));
#115576=DIRECTION('ref_axis',(0.707106781186548,0.707106781186548,0.));
#115577=DIRECTION('',(0.500000000000022,0.500000000000022,-0.707106781186517));
#115578=DIRECTION('center_axis',(0.,0.,1.));
#115579=DIRECTION('ref_axis',(0.707106781186548,0.707106781186548,0.));
#115580=DIRECTION('center_axis',(0.,0.,1.));
#115581=DIRECTION('ref_axis',(0.707106781186548,0.707106781186548,0.));
#115582=DIRECTION('center_axis',(0.,0.,1.));
#115583=DIRECTION('ref_axis',(0.707106781186548,0.707106781186548,0.));
#115584=DIRECTION('',(0.,0.,-1.));
#115585=DIRECTION('center_axis',(0.,0.,1.));
#115586=DIRECTION('ref_axis',(0.707106781186548,0.707106781186548,0.));
#115587=DIRECTION('center_axis',(0.,0.,-1.));
#115588=DIRECTION('ref_axis',(0.707106781186548,0.707106781186548,0.));
#115589=DIRECTION('',(0.500000000000022,0.500000000000022,0.707106781186517));
#115590=DIRECTION('center_axis',(0.,0.,-1.));
#115591=DIRECTION('ref_axis',(0.707106781186548,0.707106781186548,0.));
#115592=DIRECTION('center_axis',(0.,0.,1.));
#115593=DIRECTION('ref_axis',(0.707106781186548,0.707106781186548,0.));
#115594=DIRECTION('center_axis',(0.,0.,1.));
#115595=DIRECTION('ref_axis',(6.12323399573677E-17,1.,0.));
#115596=DIRECTION('center_axis',(0.,0.,-1.));
#115597=DIRECTION('ref_axis',(6.12323399573677E-17,1.,0.));
#115598=DIRECTION('',(-4.32978028117746E-17,0.707106781186547,-0.707106781186548));
#115599=DIRECTION('center_axis',(0.,0.,1.));
#115600=DIRECTION('ref_axis',(6.12323399573677E-17,1.,0.));
#115601=DIRECTION('center_axis',(0.,0.,1.));
#115602=DIRECTION('ref_axis',(6.12323399573677E-17,1.,0.));
#115603=DIRECTION('center_axis',(0.,0.,1.));
#115604=DIRECTION('ref_axis',(6.12323399573677E-17,1.,0.));
#115605=DIRECTION('',(0.,0.,-1.));
#115606=DIRECTION('center_axis',(0.,0.,1.));
#115607=DIRECTION('ref_axis',(6.12323399573677E-17,1.,0.));
#115608=DIRECTION('center_axis',(0.,0.,-1.));
#115609=DIRECTION('ref_axis',(6.12323399573677E-17,1.,0.));
#115610=DIRECTION('',(1.29893408435324E-16,0.707106781186547,0.707106781186548));
#115611=DIRECTION('center_axis',(0.,0.,-1.));
#115612=DIRECTION('ref_axis',(6.12323399573677E-17,1.,0.));
#115613=DIRECTION('center_axis',(0.,0.,1.));
#115614=DIRECTION('ref_axis',(6.12323399573677E-17,1.,0.));
#115615=DIRECTION('center_axis',(0.,0.,1.));
#115616=DIRECTION('ref_axis',(-0.707106781186547,0.707106781186548,0.));
#115617=DIRECTION('center_axis',(0.,0.,-1.));
#115618=DIRECTION('ref_axis',(-0.707106781186547,0.707106781186548,0.));
#115619=DIRECTION('',(-0.500000000000001,0.500000000000001,-0.707106781186546));
#115620=DIRECTION('center_axis',(0.,0.,1.));
#115621=DIRECTION('ref_axis',(-0.707106781186547,0.707106781186548,0.));
#115622=DIRECTION('center_axis',(0.,0.,1.));
#115623=DIRECTION('ref_axis',(-0.707106781186547,0.707106781186548,0.));
#115624=DIRECTION('center_axis',(0.,0.,1.));
#115625=DIRECTION('ref_axis',(-0.707106781186547,0.707106781186548,0.));
#115626=DIRECTION('',(0.,0.,-1.));
#115627=DIRECTION('center_axis',(0.,0.,1.));
#115628=DIRECTION('ref_axis',(-0.707106781186547,0.707106781186548,0.));
#115629=DIRECTION('center_axis',(0.,0.,-1.));
#115630=DIRECTION('ref_axis',(-0.707106781186547,0.707106781186548,0.));
#115631=DIRECTION('',(-0.5,0.500000000000001,0.707106781186546));
#115632=DIRECTION('center_axis',(0.,0.,-1.));
#115633=DIRECTION('ref_axis',(-0.707106781186547,0.707106781186548,0.));
#115634=DIRECTION('center_axis',(0.,0.,1.));
#115635=DIRECTION('ref_axis',(-0.707106781186547,0.707106781186548,0.));
#115636=DIRECTION('center_axis',(0.,0.,1.));
#115637=DIRECTION('ref_axis',(-1.,1.22464679914735E-16,0.));
#115638=DIRECTION('center_axis',(0.,0.,-1.));
#115639=DIRECTION('ref_axis',(-1.,1.22464679914735E-16,0.));
#115640=DIRECTION('',(-0.707106781186547,-2.34655184402833E-31,-0.707106781186548));
#115641=DIRECTION('center_axis',(0.,0.,1.));
#115642=DIRECTION('ref_axis',(-1.,1.22464679914735E-16,0.));
#115643=DIRECTION('center_axis',(0.,0.,1.));
#115644=DIRECTION('ref_axis',(-1.,1.22464679914735E-16,0.));
#115645=DIRECTION('center_axis',(0.,0.,1.));
#115646=DIRECTION('ref_axis',(-1.,1.22464679914735E-16,0.));
#115647=DIRECTION('',(0.,0.,-1.));
#115648=DIRECTION('center_axis',(0.,0.,1.));
#115649=DIRECTION('ref_axis',(-1.,1.22464679914735E-16,0.));
#115650=DIRECTION('center_axis',(0.,0.,-1.));
#115651=DIRECTION('ref_axis',(-1.,1.22464679914735E-16,0.));
#115652=DIRECTION('',(-0.707106781186547,1.73191211247098E-16,0.707106781186548));
#115653=DIRECTION('center_axis',(0.,0.,-1.));
#115654=DIRECTION('ref_axis',(-1.,1.22464679914735E-16,0.));
#115655=DIRECTION('center_axis',(0.,0.,1.));
#115656=DIRECTION('ref_axis',(-1.,1.22464679914735E-16,0.));
#115657=DIRECTION('center_axis',(0.,0.,1.));
#115658=DIRECTION('ref_axis',(-0.707106781186548,-0.707106781186547,0.));
#115659=DIRECTION('center_axis',(0.,0.,-1.));
#115660=DIRECTION('ref_axis',(-0.707106781186548,-0.707106781186547,0.));
#115661=DIRECTION('',(-0.500000000000001,-0.500000000000001,-0.707106781186546));
#115662=DIRECTION('center_axis',(0.,0.,1.));
#115663=DIRECTION('ref_axis',(-0.707106781186548,-0.707106781186547,0.));
#115664=DIRECTION('center_axis',(0.,0.,1.));
#115665=DIRECTION('ref_axis',(-0.707106781186548,-0.707106781186547,0.));
#115666=DIRECTION('center_axis',(0.,0.,1.));
#115667=DIRECTION('ref_axis',(-0.707106781186548,-0.707106781186547,0.));
#115668=DIRECTION('',(0.,0.,-1.));
#115669=DIRECTION('center_axis',(0.,0.,1.));
#115670=DIRECTION('ref_axis',(-0.707106781186548,-0.707106781186547,0.));
#115671=DIRECTION('center_axis',(0.,0.,-1.));
#115672=DIRECTION('ref_axis',(-0.707106781186548,-0.707106781186547,0.));
#115673=DIRECTION('',(-0.500000000000001,-0.5,0.707106781186546));
#115674=DIRECTION('center_axis',(0.,0.,-1.));
#115675=DIRECTION('ref_axis',(-0.707106781186548,-0.707106781186547,0.));
#115676=DIRECTION('center_axis',(0.,0.,1.));
#115677=DIRECTION('ref_axis',(-0.707106781186548,-0.707106781186547,0.));
#115678=DIRECTION('center_axis',(0.,0.,1.));
#115679=DIRECTION('ref_axis',(-1.83697019872103E-16,-1.,0.));
#115680=DIRECTION('center_axis',(0.,0.,-1.));
#115681=DIRECTION('ref_axis',(-1.83697019872103E-16,-1.,0.));
#115682=DIRECTION('',(-4.32978028117747E-17,-0.707106781186547,-0.707106781186548));
#115683=DIRECTION('center_axis',(0.,0.,1.));
#115684=DIRECTION('ref_axis',(-1.83697019872103E-16,-1.,0.));
#115685=DIRECTION('center_axis',(0.,0.,1.));
#115686=DIRECTION('ref_axis',(-1.83697019872103E-16,-1.,0.));
#115687=DIRECTION('center_axis',(0.,0.,1.));
#115688=DIRECTION('ref_axis',(-1.83697019872103E-16,-1.,0.));
#115689=DIRECTION('',(0.,0.,-1.));
#115690=DIRECTION('center_axis',(0.,0.,1.));
#115691=DIRECTION('ref_axis',(-1.83697019872103E-16,-1.,0.));
#115692=DIRECTION('center_axis',(0.,0.,-1.));
#115693=DIRECTION('ref_axis',(-1.83697019872103E-16,-1.,0.));
#115694=DIRECTION('',(-2.16489014058873E-16,-0.707106781186547,0.707106781186548));
#115695=DIRECTION('center_axis',(0.,0.,-1.));
#115696=DIRECTION('ref_axis',(-1.83697019872103E-16,-1.,0.));
#115697=DIRECTION('center_axis',(0.,0.,1.));
#115698=DIRECTION('ref_axis',(-1.83697019872103E-16,-1.,0.));
#115699=DIRECTION('center_axis',(0.,0.,1.));
#115700=DIRECTION('ref_axis',(0.707106781186547,-0.707106781186548,0.));
#115701=DIRECTION('center_axis',(0.,0.,-1.));
#115702=DIRECTION('ref_axis',(0.707106781186547,-0.707106781186548,0.));
#115703=DIRECTION('',(0.500000000000001,-0.500000000000001,-0.707106781186546));
#115704=DIRECTION('center_axis',(0.,0.,1.));
#115705=DIRECTION('ref_axis',(0.707106781186547,-0.707106781186548,0.));
#115706=DIRECTION('center_axis',(0.,0.,1.));
#115707=DIRECTION('ref_axis',(0.707106781186547,-0.707106781186548,0.));
#115708=DIRECTION('center_axis',(0.,0.,1.));
#115709=DIRECTION('ref_axis',(0.707106781186547,-0.707106781186548,0.));
#115710=DIRECTION('',(0.,0.,-1.));
#115711=DIRECTION('center_axis',(0.,0.,1.));
#115712=DIRECTION('ref_axis',(0.707106781186547,-0.707106781186548,0.));
#115713=DIRECTION('center_axis',(0.,0.,-1.));
#115714=DIRECTION('ref_axis',(0.707106781186547,-0.707106781186548,0.));
#115715=DIRECTION('',(0.5,-0.500000000000001,0.707106781186546));
#115716=DIRECTION('center_axis',(0.,0.,-1.));
#115717=DIRECTION('ref_axis',(0.707106781186547,-0.707106781186548,0.));
#115718=DIRECTION('center_axis',(0.,0.,1.));
#115719=DIRECTION('ref_axis',(0.707106781186547,-0.707106781186548,0.));
#115720=DIRECTION('axis',(0.,0.,1.));
#115721=DIRECTION('refdir',(1.,0.,0.));
#115722=DIRECTION('axis',(0.,0.,1.));
#115723=DIRECTION('refdir',(1.,0.,0.));
#115724=DIRECTION('center_axis',(-3.15057456128877E-15,3.72034542862913E-31,
-1.));
#115725=DIRECTION('ref_axis',(1.18084665392185E-16,1.,0.));
#115726=DIRECTION('',(3.15057456128877E-15,-3.72034542862913E-31,1.));
#115727=DIRECTION('center_axis',(0.,0.,-1.));
#115728=DIRECTION('ref_axis',(-0.700629269222024,-0.713525491562434,0.));
#115729=DIRECTION('center_axis',(-3.15057456128877E-15,3.72034542862913E-31,
-1.));
#115730=DIRECTION('ref_axis',(1.18084665392185E-16,1.,0.));
#115731=DIRECTION('',(3.15057456128877E-15,-3.72034542862913E-31,1.));
#115732=DIRECTION('center_axis',(-3.15057456128877E-15,3.72034542862913E-31,
-1.));
#115733=DIRECTION('ref_axis',(1.18084665392185E-16,1.,0.));
#115734=DIRECTION('',(3.15057456128877E-15,-3.72034542862913E-31,1.));
#115735=DIRECTION('center_axis',(-3.15057456128877E-15,3.72034542862913E-31,
-1.));
#115736=DIRECTION('ref_axis',(1.18084665392185E-16,1.,0.));
#115737=DIRECTION('',(3.15057456128877E-15,-3.72034542862913E-31,1.));
#115738=DIRECTION('center_axis',(-3.15057456128877E-15,3.72034542862913E-31,
-1.));
#115739=DIRECTION('ref_axis',(1.18084665392185E-16,1.,0.));
#115740=DIRECTION('',(3.15057456128877E-15,-3.72034542862913E-31,1.));
#115741=DIRECTION('center_axis',(-3.15057456128877E-15,3.72034542862913E-31,
-1.));
#115742=DIRECTION('ref_axis',(1.18084665392185E-16,1.,0.));
#115743=DIRECTION('',(3.15057456128877E-15,-3.72034542862913E-31,1.));
#115744=DIRECTION('center_axis',(-3.15057456128877E-15,3.72034542862913E-31,
-1.));
#115745=DIRECTION('ref_axis',(1.18084665392185E-16,1.,0.));
#115746=DIRECTION('',(3.15057456128877E-15,-3.72034542862913E-31,1.));
#115747=DIRECTION('center_axis',(-3.15057456128877E-15,3.72034542862913E-31,
-1.));
#115748=DIRECTION('ref_axis',(1.18084665392185E-16,1.,0.));
#115749=DIRECTION('',(3.15057456128877E-15,-3.72034542862913E-31,1.));
#115750=DIRECTION('center_axis',(-3.15057456128877E-15,3.72034542862913E-31,
-1.));
#115751=DIRECTION('ref_axis',(1.18084665392185E-16,1.,0.));
#115752=DIRECTION('',(3.15057456128877E-15,-3.72034542862913E-31,1.));
#115753=DIRECTION('center_axis',(-3.15057456128877E-15,3.72034542862913E-31,
-1.));
#115754=DIRECTION('ref_axis',(1.18084665392185E-16,1.,0.));
#115755=DIRECTION('',(3.15057456128877E-15,-3.72034542862913E-31,1.));
#115756=DIRECTION('center_axis',(-3.15057456128877E-15,3.72034542862913E-31,
-1.));
#115757=DIRECTION('ref_axis',(1.18084665392185E-16,1.,0.));
#115758=DIRECTION('',(3.15057456128877E-15,-3.72034542862913E-31,1.));
#115759=DIRECTION('center_axis',(-3.15057456128877E-15,3.72034542862913E-31,
-1.));
#115760=DIRECTION('ref_axis',(1.18084665392185E-16,1.,0.));
#115761=DIRECTION('',(3.15057456128877E-15,-3.72034542862913E-31,1.));
#115762=DIRECTION('center_axis',(-3.15057456128877E-15,3.72034542862913E-31,
-1.));
#115763=DIRECTION('ref_axis',(1.18084665392185E-16,1.,0.));
#115764=DIRECTION('',(3.15057456128877E-15,-3.72034542862913E-31,1.));
#115765=DIRECTION('center_axis',(-3.15057456128877E-15,3.72034542862913E-31,
-1.));
#115766=DIRECTION('ref_axis',(1.18084665392185E-16,1.,0.));
#115767=DIRECTION('',(3.15057456128877E-15,-3.72034542862913E-31,1.));
#115768=DIRECTION('center_axis',(-3.15057456128877E-15,3.72034542862913E-31,
-1.));
#115769=DIRECTION('ref_axis',(1.18084665392185E-16,1.,0.));
#115770=DIRECTION('',(3.15057456128877E-15,-3.72034542862913E-31,1.));
#115771=DIRECTION('center_axis',(-3.15057456128877E-15,3.72034542862913E-31,
-1.));
#115772=DIRECTION('ref_axis',(1.18084665392185E-16,1.,0.));
#115773=DIRECTION('',(3.15057456128877E-15,-3.72034542862913E-31,1.));
#115774=DIRECTION('center_axis',(-3.15057456128877E-15,3.72034542862913E-31,
-1.));
#115775=DIRECTION('ref_axis',(1.18084665392185E-16,1.,0.));
#115776=DIRECTION('',(3.15057456128877E-15,-3.72034542862913E-31,1.));
#115777=DIRECTION('center_axis',(-3.15057456128877E-15,3.72034542862913E-31,
-1.));
#115778=DIRECTION('ref_axis',(1.18084665392185E-16,1.,0.));
#115779=DIRECTION('',(3.15057456128877E-15,-3.72034542862913E-31,1.));
#115780=DIRECTION('center_axis',(-3.15057456128877E-15,3.72034542862913E-31,
-1.));
#115781=DIRECTION('ref_axis',(1.18084665392185E-16,1.,0.));
#115782=DIRECTION('',(3.15057456128877E-15,-3.72034542862913E-31,1.));
#115783=DIRECTION('center_axis',(-3.15057456128877E-15,3.72034542862913E-31,
-1.));
#115784=DIRECTION('ref_axis',(1.18084665392185E-16,1.,0.));
#115785=DIRECTION('',(3.15057456128877E-15,-3.72034542862913E-31,1.));
#115786=DIRECTION('center_axis',(-3.15057456128877E-15,3.72034542862913E-31,
-1.));
#115787=DIRECTION('ref_axis',(1.18084665392185E-16,1.,0.));
#115788=DIRECTION('',(3.15057456128877E-15,-3.72034542862913E-31,1.));
#115789=DIRECTION('center_axis',(-3.15057456128877E-15,3.72034542862913E-31,
-1.));
#115790=DIRECTION('ref_axis',(1.18084665392185E-16,1.,0.));
#115791=DIRECTION('',(3.15057456128877E-15,-3.72034542862913E-31,1.));
#115792=DIRECTION('center_axis',(-3.15057456128877E-15,3.72034542862913E-31,
-1.));
#115793=DIRECTION('ref_axis',(1.18084665392185E-16,1.,0.));
#115794=DIRECTION('',(3.15057456128877E-15,-3.72034542862913E-31,1.));
#115795=DIRECTION('center_axis',(-3.15057456128877E-15,3.72034542862913E-31,
-1.));
#115796=DIRECTION('ref_axis',(1.18084665392185E-16,1.,0.));
#115797=DIRECTION('',(3.15057456128877E-15,-3.72034542862913E-31,1.));
#115798=DIRECTION('center_axis',(-3.15057456128877E-15,3.72034542862913E-31,
-1.));
#115799=DIRECTION('ref_axis',(1.18084665392185E-16,1.,0.));
#115800=DIRECTION('',(3.15057456128877E-15,-3.72034542862913E-31,1.));
#115801=DIRECTION('center_axis',(-3.15057456128877E-15,3.72034542862913E-31,
-1.));
#115802=DIRECTION('ref_axis',(1.18084665392185E-16,1.,0.));
#115803=DIRECTION('',(3.15057456128877E-15,-3.72034542862913E-31,1.));
#115804=DIRECTION('center_axis',(-3.15057456128877E-15,3.72034542862913E-31,
-1.));
#115805=DIRECTION('ref_axis',(1.18084665392185E-16,1.,0.));
#115806=DIRECTION('',(3.15057456128877E-15,-3.72034542862913E-31,1.));
#115807=DIRECTION('center_axis',(-3.15057456128877E-15,3.72034542862913E-31,
-1.));
#115808=DIRECTION('ref_axis',(1.18084665392185E-16,1.,0.));
#115809=DIRECTION('',(3.15057456128877E-15,-3.72034542862913E-31,1.));
#115810=DIRECTION('center_axis',(-3.15057456128877E-15,3.72034542862913E-31,
-1.));
#115811=DIRECTION('ref_axis',(1.18084665392185E-16,1.,0.));
#115812=DIRECTION('',(3.15057456128877E-15,-3.72034542862913E-31,1.));
#115813=DIRECTION('center_axis',(-3.15057456128877E-15,3.72034542862913E-31,
-1.));
#115814=DIRECTION('ref_axis',(1.18084665392185E-16,1.,0.));
#115815=DIRECTION('',(3.15057456128877E-15,-3.72034542862913E-31,1.));
#115816=DIRECTION('center_axis',(-3.15057456128877E-15,3.72034542862913E-31,
-1.));
#115817=DIRECTION('ref_axis',(1.18084665392185E-16,1.,0.));
#115818=DIRECTION('',(3.15057456128877E-15,-3.72034542862913E-31,1.));
#115819=DIRECTION('center_axis',(-3.15057456128877E-15,3.72034542862913E-31,
-1.));
#115820=DIRECTION('ref_axis',(1.18084665392185E-16,1.,0.));
#115821=DIRECTION('',(3.15057456128877E-15,-3.72034542862913E-31,1.));
#115822=DIRECTION('center_axis',(1.38133616053571E-12,-4.24340571905306E-12,
-1.));
#115823=DIRECTION('ref_axis',(-1.35431357084844E-12,-1.,4.2434905355515E-12));
#115824=DIRECTION('center_axis',(0.,8.13151629364128E-17,-1.));
#115825=DIRECTION('ref_axis',(0.,1.,8.13151629364128E-17));
#115826=DIRECTION('',(0.,-8.13151629364128E-17,1.));
#115827=DIRECTION('center_axis',(0.,0.,-1.));
#115828=DIRECTION('ref_axis',(1.,0.,0.));
#115829=DIRECTION('center_axis',(0.,8.13151629364128E-17,-1.));
#115830=DIRECTION('ref_axis',(0.,1.,8.13151629364128E-17));
#115831=DIRECTION('',(0.,-8.13151629364128E-17,1.));
#115832=DIRECTION('center_axis',(0.,8.13151629364128E-17,-1.));
#115833=DIRECTION('ref_axis',(0.,1.,8.13151629364128E-17));
#115834=DIRECTION('',(0.,-8.13151629364128E-17,1.));
#115835=DIRECTION('center_axis',(0.,8.13151629364128E-17,-1.));
#115836=DIRECTION('ref_axis',(0.,1.,8.13151629364128E-17));
#115837=DIRECTION('',(0.,-8.13151629364128E-17,1.));
#115838=DIRECTION('center_axis',(0.,8.13151629364128E-17,-1.));
#115839=DIRECTION('ref_axis',(0.,1.,8.13151629364128E-17));
#115840=DIRECTION('',(0.,-8.13151629364128E-17,1.));
#115841=DIRECTION('center_axis',(0.,8.13151629364128E-17,-1.));
#115842=DIRECTION('ref_axis',(0.,1.,8.13151629364128E-17));
#115843=DIRECTION('',(0.,-8.13151629364128E-17,1.));
#115844=DIRECTION('center_axis',(0.,8.13151629364128E-17,-1.));
#115845=DIRECTION('ref_axis',(0.,1.,8.13151629364128E-17));
#115846=DIRECTION('',(0.,-8.13151629364128E-17,1.));
#115847=DIRECTION('center_axis',(0.,8.13151629364128E-17,-1.));
#115848=DIRECTION('ref_axis',(0.,1.,8.13151629364128E-17));
#115849=DIRECTION('',(0.,-8.13151629364128E-17,1.));
#115850=DIRECTION('center_axis',(0.,8.13151629364128E-17,-1.));
#115851=DIRECTION('ref_axis',(0.,1.,8.13151629364128E-17));
#115852=DIRECTION('',(0.,-8.13151629364128E-17,1.));
#115853=DIRECTION('center_axis',(0.,8.13151629364128E-17,-1.));
#115854=DIRECTION('ref_axis',(0.,1.,8.13151629364128E-17));
#115855=DIRECTION('',(0.,-8.13151629364128E-17,1.));
#115856=DIRECTION('center_axis',(0.,8.13151629364128E-17,-1.));
#115857=DIRECTION('ref_axis',(0.,1.,8.13151629364128E-17));
#115858=DIRECTION('',(0.,-8.13151629364128E-17,1.));
#115859=DIRECTION('center_axis',(0.,8.13151629364128E-17,-1.));
#115860=DIRECTION('ref_axis',(0.,1.,8.13151629364128E-17));
#115861=DIRECTION('',(0.,-8.13151629364128E-17,1.));
#115862=DIRECTION('center_axis',(0.,8.13151629364128E-17,-1.));
#115863=DIRECTION('ref_axis',(0.,1.,8.13151629364128E-17));
#115864=DIRECTION('',(0.,-8.13151629364128E-17,1.));
#115865=DIRECTION('center_axis',(0.,8.13151629364128E-17,-1.));
#115866=DIRECTION('ref_axis',(0.,1.,8.13151629364128E-17));
#115867=DIRECTION('',(0.,-8.13151629364128E-17,1.));
#115868=DIRECTION('center_axis',(0.,8.13151629364128E-17,-1.));
#115869=DIRECTION('ref_axis',(0.,1.,8.13151629364128E-17));
#115870=DIRECTION('',(0.,-8.13151629364128E-17,1.));
#115871=DIRECTION('center_axis',(0.,8.13151629364128E-17,-1.));
#115872=DIRECTION('ref_axis',(0.,1.,8.13151629364128E-17));
#115873=DIRECTION('',(0.,-8.13151629364128E-17,1.));
#115874=DIRECTION('center_axis',(0.,8.13151629364128E-17,-1.));
#115875=DIRECTION('ref_axis',(0.,1.,8.13151629364128E-17));
#115876=DIRECTION('',(0.,-8.13151629364128E-17,1.));
#115877=DIRECTION('center_axis',(0.,8.13151629364128E-17,-1.));
#115878=DIRECTION('ref_axis',(0.,1.,8.13151629364128E-17));
#115879=DIRECTION('',(0.,-8.13151629364128E-17,1.));
#115880=DIRECTION('center_axis',(0.,8.13151629364128E-17,-1.));
#115881=DIRECTION('ref_axis',(0.,1.,8.13151629364128E-17));
#115882=DIRECTION('',(0.,-8.13151629364128E-17,1.));
#115883=DIRECTION('center_axis',(0.,8.13151629364128E-17,-1.));
#115884=DIRECTION('ref_axis',(0.,1.,8.13151629364128E-17));
#115885=DIRECTION('',(0.,-8.13151629364128E-17,1.));
#115886=DIRECTION('center_axis',(0.,8.13151629364128E-17,-1.));
#115887=DIRECTION('ref_axis',(0.,1.,8.13151629364128E-17));
#115888=DIRECTION('',(0.,-8.13151629364128E-17,1.));
#115889=DIRECTION('center_axis',(0.,8.13151629364128E-17,-1.));
#115890=DIRECTION('ref_axis',(0.,1.,8.13151629364128E-17));
#115891=DIRECTION('',(0.,-8.13151629364128E-17,1.));
#115892=DIRECTION('center_axis',(0.,8.13151629364128E-17,-1.));
#115893=DIRECTION('ref_axis',(0.,1.,8.13151629364128E-17));
#115894=DIRECTION('',(0.,-8.13151629364128E-17,1.));
#115895=DIRECTION('center_axis',(0.,8.13151629364128E-17,-1.));
#115896=DIRECTION('ref_axis',(0.,1.,8.13151629364128E-17));
#115897=DIRECTION('',(0.,-8.13151629364128E-17,1.));
#115898=DIRECTION('center_axis',(0.,8.13151629364128E-17,-1.));
#115899=DIRECTION('ref_axis',(0.,1.,8.13151629364128E-17));
#115900=DIRECTION('',(0.,-8.13151629364128E-17,1.));
#115901=DIRECTION('center_axis',(0.,8.13151629364128E-17,-1.));
#115902=DIRECTION('ref_axis',(0.,1.,8.13151629364128E-17));
#115903=DIRECTION('',(0.,-8.13151629364128E-17,1.));
#115904=DIRECTION('center_axis',(0.,8.13151629364128E-17,-1.));
#115905=DIRECTION('ref_axis',(0.,1.,8.13151629364128E-17));
#115906=DIRECTION('',(0.,-8.13151629364128E-17,1.));
#115907=DIRECTION('center_axis',(0.,8.13151629364128E-17,-1.));
#115908=DIRECTION('ref_axis',(0.,1.,8.13151629364128E-17));
#115909=DIRECTION('',(0.,-8.13151629364128E-17,1.));
#115910=DIRECTION('center_axis',(0.,8.13151629364128E-17,-1.));
#115911=DIRECTION('ref_axis',(0.,1.,8.13151629364128E-17));
#115912=DIRECTION('',(0.,-8.13151629364128E-17,1.));
#115913=DIRECTION('center_axis',(0.,8.13151629364128E-17,-1.));
#115914=DIRECTION('ref_axis',(0.,1.,8.13151629364128E-17));
#115915=DIRECTION('',(0.,-8.13151629364128E-17,1.));
#115916=DIRECTION('center_axis',(0.,8.13151629364128E-17,-1.));
#115917=DIRECTION('ref_axis',(0.,1.,8.13151629364128E-17));
#115918=DIRECTION('',(0.,-8.13151629364128E-17,1.));
#115919=DIRECTION('center_axis',(0.,0.,1.));
#115920=DIRECTION('ref_axis',(1.,0.,0.));
#115921=DIRECTION('center_axis',(0.,0.,1.));
#115922=DIRECTION('ref_axis',(1.,0.,0.));
#115923=DIRECTION('center_axis',(1.,6.9217303377289E-15,0.));
#115924=DIRECTION('ref_axis',(6.98296267768627E-15,-1.,0.));
#115925=DIRECTION('center_axis',(0.,0.,-1.));
#115926=DIRECTION('ref_axis',(-1.,0.,0.));
#115927=DIRECTION('center_axis',(0.,0.,1.));
#115928=DIRECTION('ref_axis',(1.,0.,0.));
#115929=DIRECTION('center_axis',(0.,0.,-1.));
#115930=DIRECTION('ref_axis',(-1.,0.,0.));
#115931=DIRECTION('center_axis',(0.,0.,-1.));
#115932=DIRECTION('ref_axis',(-1.,0.,0.));
#115933=DIRECTION('',(0.,0.,1.));
#115934=DIRECTION('center_axis',(0.,0.,-1.));
#115935=DIRECTION('ref_axis',(-1.,0.,0.));
#115936=DIRECTION('center_axis',(0.,-8.13151629364128E-17,1.));
#115937=DIRECTION('ref_axis',(0.,-1.,-8.13151629364128E-17));
#115938=DIRECTION('center_axis',(1.38133616053571E-12,-4.24340571905306E-12,
-1.));
#115939=DIRECTION('ref_axis',(-1.35431357084844E-12,-1.,4.2434905355515E-12));
#115940=DIRECTION('center_axis',(0.,-8.13151629364128E-17,1.));
#115941=DIRECTION('ref_axis',(0.,1.,8.13151629364128E-17));
#115942=DIRECTION('',(8.65956056235493E-17,-0.707106781186547,-0.707106781186548));
#115943=DIRECTION('center_axis',(0.,8.13151629364128E-17,-1.));
#115944=DIRECTION('ref_axis',(0.,1.,8.13151629364128E-17));
#115945=DIRECTION('center_axis',(0.,8.13151629364128E-17,-1.));
#115946=DIRECTION('ref_axis',(0.,1.,8.13151629364128E-17));
#115947=DIRECTION('center_axis',(0.,8.13151629364128E-17,-1.));
#115948=DIRECTION('ref_axis',(0.,1.,8.13151629364128E-17));
#115949=DIRECTION('center_axis',(0.,0.,1.));
#115950=DIRECTION('ref_axis',(1.,0.,0.));
#115951=DIRECTION('center_axis',(0.,0.,-1.));
#115952=DIRECTION('ref_axis',(-1.,0.,0.));
#115953=DIRECTION('center_axis',(0.,0.,-1.));
#115954=DIRECTION('ref_axis',(-1.,0.,0.));
#115955=DIRECTION('center_axis',(0.,0.,1.));
#115956=DIRECTION('ref_axis',(1.,0.,0.));
#115957=DIRECTION('center_axis',(0.,0.,1.));
#115958=DIRECTION('ref_axis',(1.,0.,0.));
#115959=DIRECTION('center_axis',(0.,0.,1.));
#115960=DIRECTION('ref_axis',(1.,0.,0.));
#115961=DIRECTION('center_axis',(0.,0.,1.));
#115962=DIRECTION('ref_axis',(1.,0.,0.));
#115963=DIRECTION('center_axis',(0.,0.,1.));
#115964=DIRECTION('ref_axis',(1.,0.,0.));
#115965=DIRECTION('center_axis',(0.,0.,1.));
#115966=DIRECTION('ref_axis',(1.,0.,0.));
#115967=DIRECTION('center_axis',(0.,0.,1.));
#115968=DIRECTION('ref_axis',(1.,0.,0.));
#115969=DIRECTION('center_axis',(0.,0.,1.));
#115970=DIRECTION('ref_axis',(-1.,-3.21624529935327E-16,0.));
#115971=DIRECTION('center_axis',(0.,0.,1.));
#115972=DIRECTION('ref_axis',(1.,0.,0.));
#115973=DIRECTION('center_axis',(0.,0.,1.));
#115974=DIRECTION('ref_axis',(1.,0.,0.));
#115975=DIRECTION('center_axis',(0.,0.,1.));
#115976=DIRECTION('ref_axis',(1.,0.,0.));
#115977=DIRECTION('',(0.866025403784438,0.5,0.));
#115978=DIRECTION('',(0.,1.,0.));
#115979=DIRECTION('',(-0.866025403784439,0.5,0.));
#115980=DIRECTION('',(-0.866025403784438,-0.5,0.));
#115981=DIRECTION('',(1.87789324842145E-16,-1.,0.));
#115982=DIRECTION('',(0.866025403784438,-0.5,0.));
#115983=DIRECTION('center_axis',(1.,0.,0.));
#115984=DIRECTION('ref_axis',(0.,0.,-1.));
#115985=DIRECTION('',(0.,0.,1.));
#115986=DIRECTION('',(0.,0.,1.));
#115987=DIRECTION('center_axis',(0.5,0.866025403784439,0.));
#115988=DIRECTION('ref_axis',(-0.866025403784439,0.5,0.));
#115989=DIRECTION('',(0.,0.,1.));
#115990=DIRECTION('center_axis',(-0.5,0.866025403784439,0.));
#115991=DIRECTION('ref_axis',(-0.866025403784439,-0.5,0.));
#115992=DIRECTION('',(0.,0.,1.));
#115993=DIRECTION('center_axis',(-1.,-1.87789324842145E-16,0.));
#115994=DIRECTION('ref_axis',(1.87789324842145E-16,-1.,0.));
#115995=DIRECTION('',(0.,0.,1.));
#115996=DIRECTION('center_axis',(-0.5,-0.866025403784439,0.));
#115997=DIRECTION('ref_axis',(0.866025403784439,-0.5,0.));
#115998=DIRECTION('',(0.,0.,1.));
#115999=DIRECTION('center_axis',(0.5,-0.866025403784438,0.));
#116000=DIRECTION('ref_axis',(0.866025403784438,0.5,0.));
#116001=DIRECTION('center_axis',(-3.15057456128877E-15,3.72034542862913E-31,
-1.));
#116002=DIRECTION('ref_axis',(1.18084665392185E-16,1.,0.));
#116003=DIRECTION('axis',(0.,0.,1.));
#116004=DIRECTION('refdir',(1.,0.,0.));
#116005=DIRECTION('center_axis',(1.90014037850669E-13,0.994089659369792,
0.108562190167897));
#116006=DIRECTION('ref_axis',(0.999999999984429,-6.05836258509456E-7,5.54756097781441E-6));
#116007=DIRECTION('center_axis',(-1.04862710274864E-14,-0.997667534637082,
-0.0682604595001084));
#116008=DIRECTION('ref_axis',(0.99999999997237,-5.07429128929804E-7,7.41638074638744E-6));
#116009=DIRECTION('center_axis',(1.90014037850669E-13,0.994089659369792,
0.108562190167897));
#116010=DIRECTION('ref_axis',(0.999999999984429,-6.05836258509456E-7,5.54756097781441E-6));
#116011=DIRECTION('center_axis',(4.15449470707835E-15,-0.994089659369792,
-0.108562190167898));
#116012=DIRECTION('ref_axis',(0.999999999999024,-1.5165736758839E-7,1.38870655435557E-6));
#116013=DIRECTION('center_axis',(4.15449470707835E-15,-0.994089659369792,
-0.108562190167898));
#116014=DIRECTION('ref_axis',(0.999999999999024,-1.5165736758839E-7,1.38870655435557E-6));
#116015=DIRECTION('center_axis',(0.,1.,0.));
#116016=DIRECTION('ref_axis',(1.,0.,0.));
#116017=DIRECTION('center_axis',(0.,1.,0.));
#116018=DIRECTION('ref_axis',(1.,0.,0.));
#116019=DIRECTION('center_axis',(4.15449470707834E-15,-0.994089659369792,
-0.108562190167898));
#116020=DIRECTION('ref_axis',(0.999999999999024,-1.51657367553393E-7,1.3887065540351E-6));
#116021=DIRECTION('center_axis',(4.15449470707834E-15,-0.994089659369792,
-0.108562190167898));
#116022=DIRECTION('ref_axis',(0.999999999999024,-1.51657367553393E-7,1.3887065540351E-6));
#116023=DIRECTION('center_axis',(0.,1.,0.));
#116024=DIRECTION('ref_axis',(0.,0.,1.));
#116025=DIRECTION('center_axis',(-1.41956054810603E-13,0.994089659369792,
0.108562190167897));
#116026=DIRECTION('ref_axis',(0.999999999984429,-6.05835921327016E-7,5.54756094815878E-6));
#116027=DIRECTION('center_axis',(-1.41956054810603E-13,0.994089659369792,
0.108562190167897));
#116028=DIRECTION('ref_axis',(0.999999999984429,-6.05835921327016E-7,5.54756094815878E-6));
#116029=DIRECTION('center_axis',(-1.05710970162048E-14,-0.997667534637082,
-0.0682604595001086));
#116030=DIRECTION('ref_axis',(0.,0.0682604595001086,-0.997667534637082));
#116031=DIRECTION('center_axis',(-1.06920965951746E-14,-0.997667534637082,
-0.0682604595001082));
#116032=DIRECTION('ref_axis',(0.99999999997237,-5.07429130466677E-7,7.41638076583464E-6));
#116033=DIRECTION('',(-1.11697817138104E-15,1.,-1.70169575503835E-16));
#116034=DIRECTION('',(0.999999999999997,1.39453392450933E-15,-1.09634523681735E-15));
#116035=DIRECTION('',(1.07577848882655E-15,-1.,-1.044288650618E-17));
#116036=DIRECTION('',(0.999999999999999,1.29782309072364E-15,-9.67991738112865E-16));
#116037=DIRECTION('axis',(0.,0.,1.));
#116038=DIRECTION('refdir',(1.,0.,0.));
#116039=DIRECTION('center_axis',(0.,0.,1.));
#116040=DIRECTION('ref_axis',(1.,0.,0.));
#116041=DIRECTION('center_axis',(0.,0.,1.));
#116042=DIRECTION('ref_axis',(1.,0.,0.));
#116043=DIRECTION('',(0.,0.,1.));
#116044=DIRECTION('center_axis',(0.,0.,1.));
#116045=DIRECTION('ref_axis',(1.,0.,0.));
#116046=DIRECTION('center_axis',(0.,0.,1.));
#116047=DIRECTION('ref_axis',(1.,0.,0.));
#116048=DIRECTION('center_axis',(0.,0.,1.));
#116049=DIRECTION('ref_axis',(1.,0.,0.));
#116050=DIRECTION('center_axis',(-1.22464679914735E-16,1.,0.));
#116051=DIRECTION('ref_axis',(-1.,-1.22464679914735E-16,0.));
#116052=DIRECTION('center_axis',(0.,0.,1.));
#116053=DIRECTION('ref_axis',(1.,0.,0.));
#116054=DIRECTION('center_axis',(0.,0.,1.));
#116055=DIRECTION('ref_axis',(1.,0.,0.));
#116056=DIRECTION('',(0.,0.,1.));
#116057=DIRECTION('center_axis',(0.,0.,1.));
#116058=DIRECTION('ref_axis',(1.,0.,0.));
#116059=DIRECTION('center_axis',(0.,0.,1.));
#116060=DIRECTION('ref_axis',(1.,0.,0.));
#116061=DIRECTION('',(0.707106781186549,8.65956056235495E-17,-0.707106781186546));
#116062=DIRECTION('center_axis',(0.,0.,1.));
#116063=DIRECTION('ref_axis',(1.,0.,0.));
#116064=DIRECTION('center_axis',(0.,0.,1.));
#116065=DIRECTION('ref_axis',(1.,0.,0.));
#116066=DIRECTION('center_axis',(0.,0.,1.));
#116067=DIRECTION('ref_axis',(1.,0.,0.));
#116068=DIRECTION('center_axis',(0.,0.,1.));
#116069=DIRECTION('ref_axis',(1.,0.,0.));
#116070=DIRECTION('',(0.,0.,-1.));
#116071=DIRECTION('center_axis',(0.,0.,-1.));
#116072=DIRECTION('ref_axis',(-1.,0.,0.));
#116073=DIRECTION('',(-0.707106781186548,8.65956056235494E-17,0.707106781186547));
#116074=DIRECTION('center_axis',(0.,0.,1.));
#116075=DIRECTION('ref_axis',(1.,0.,0.));
#116076=DIRECTION('center_axis',(0.,0.,1.));
#116077=DIRECTION('ref_axis',(1.,0.,0.));
#116078=DIRECTION('center_axis',(0.,0.,-1.));
#116079=DIRECTION('ref_axis',(-1.,0.,0.));
#116080=DIRECTION('center_axis',(0.,0.,1.));
#116081=DIRECTION('ref_axis',(1.,0.,0.));
#116082=DIRECTION('center_axis',(0.,0.,1.));
#116083=DIRECTION('ref_axis',(1.,0.,0.));
#116084=DIRECTION('center_axis',(-1.22464679914735E-16,1.,0.));
#116085=DIRECTION('ref_axis',(-1.,-1.22464679914735E-16,0.));
#116086=DIRECTION('center_axis',(0.,0.,1.));
#116087=DIRECTION('ref_axis',(1.,0.,0.));
#116088=DIRECTION('center_axis',(0.,0.,1.));
#116089=DIRECTION('ref_axis',(1.,0.,0.));
#116090=DIRECTION('center_axis',(0.,0.,1.));
#116091=DIRECTION('ref_axis',(1.,0.,0.));
#116092=DIRECTION('',(-0.707106781186547,-8.65956056235493E-17,0.707106781186548));
#116093=DIRECTION('center_axis',(0.,0.,1.));
#116094=DIRECTION('ref_axis',(1.,0.,0.));
#116095=DIRECTION('center_axis',(0.,0.,1.));
#116096=DIRECTION('ref_axis',(1.,0.,0.));
#116097=DIRECTION('center_axis',(0.,0.,1.));
#116098=DIRECTION('ref_axis',(1.,0.,0.));
#116099=DIRECTION('center_axis',(0.,0.,1.));
#116100=DIRECTION('ref_axis',(1.,0.,0.));
#116101=DIRECTION('',(0.,0.,1.));
#116102=DIRECTION('center_axis',(0.,0.,-1.));
#116103=DIRECTION('ref_axis',(-1.,0.,0.));
#116104=DIRECTION('',(0.707106781186548,-8.65956056235494E-17,-0.707106781186547));
#116105=DIRECTION('center_axis',(0.,0.,1.));
#116106=DIRECTION('ref_axis',(1.,0.,0.));
#116107=DIRECTION('center_axis',(0.,0.,1.));
#116108=DIRECTION('ref_axis',(1.,0.,0.));
#116109=DIRECTION('',(0.,0.,-1.));
#116110=DIRECTION('center_axis',(0.,0.,1.));
#116111=DIRECTION('ref_axis',(1.,0.,0.));
#116112=DIRECTION('center_axis',(0.,0.,1.));
#116113=DIRECTION('ref_axis',(1.,0.,0.));
#116114=DIRECTION('center_axis',(0.,0.,1.));
#116115=DIRECTION('ref_axis',(1.,0.,0.));
#116116=DIRECTION('',(0.,0.,-1.));
#116117=DIRECTION('center_axis',(0.,0.,-1.));
#116118=DIRECTION('ref_axis',(-1.,0.,0.));
#116119=DIRECTION('center_axis',(0.,0.,1.));
#116120=DIRECTION('ref_axis',(1.,0.,0.));
#116121=DIRECTION('center_axis',(-1.,0.,0.));
#116122=DIRECTION('ref_axis',(0.,1.,0.));
#116123=DIRECTION('center_axis',(0.,1.22464679914735E-16,1.));
#116124=DIRECTION('ref_axis',(0.,-1.,1.22464679914735E-16));
#116125=DIRECTION('center_axis',(-0.866025403784438,0.500000000000001,0.));
#116126=DIRECTION('ref_axis',(0.500000000000001,0.866025403784438,0.));
#116127=DIRECTION('center_axis',(6.12323399573678E-17,1.06057523872491E-16,
1.));
#116128=DIRECTION('ref_axis',(-0.500000000000001,-0.866025403784438,1.22464679914735E-16));
#116129=DIRECTION('center_axis',(-0.499999999999998,0.86602540378444,0.));
#116130=DIRECTION('ref_axis',(0.86602540378444,0.499999999999998,0.));
#116131=DIRECTION('center_axis',(1.06057523872491E-16,6.12323399573674E-17,
1.));
#116132=DIRECTION('ref_axis',(-0.86602540378444,-0.499999999999998,1.22464679914735E-16));
#116133=DIRECTION('center_axis',(3.85183893531728E-15,1.,0.));
#116134=DIRECTION('ref_axis',(1.,-3.49148133884313E-15,0.));
#116135=DIRECTION('center_axis',(1.22464679914735E-16,-4.27583144589696E-31,
1.));
#116136=DIRECTION('ref_axis',(-1.,3.49148133884314E-15,1.22464679914735E-16));
#116137=DIRECTION('center_axis',(0.500000000000004,0.866025403784436,0.));
#116138=DIRECTION('ref_axis',(0.866025403784436,-0.500000000000004,0.));
#116139=DIRECTION('center_axis',(1.0605752387249E-16,-6.12323399573682E-17,
1.));
#116140=DIRECTION('ref_axis',(-0.866025403784436,0.500000000000004,1.22464679914735E-16));
#116141=DIRECTION('center_axis',(0.866025403784442,0.499999999999995,0.));
#116142=DIRECTION('ref_axis',(0.499999999999995,-0.866025403784442,0.));
#116143=DIRECTION('center_axis',(6.1232339957367E-17,-1.06057523872491E-16,
1.));
#116144=DIRECTION('ref_axis',(-0.499999999999995,0.866025403784442,1.22464679914735E-16));
#116145=DIRECTION('center_axis',(1.,-6.9333100835711E-15,0.));
#116146=DIRECTION('ref_axis',(-6.98296267768627E-15,-1.,0.));
#116147=DIRECTION('center_axis',(-8.55166289179392E-31,-1.22464679914735E-16,
1.));
#116148=DIRECTION('ref_axis',(6.98296267768627E-15,1.,1.22464679914735E-16));
#116149=DIRECTION('center_axis',(0.866025403784434,-0.500000000000007,0.));
#116150=DIRECTION('ref_axis',(-0.500000000000008,-0.866025403784434,0.));
#116151=DIRECTION('center_axis',(-6.12323399573685E-17,-1.0605752387249E-16,
1.));
#116152=DIRECTION('ref_axis',(0.500000000000007,0.866025403784435,1.22464679914735E-16));
#116153=DIRECTION('center_axis',(0.499999999999992,-0.866025403784443,0.));
#116154=DIRECTION('ref_axis',(-0.866025403784443,-0.499999999999992,0.));
#116155=DIRECTION('center_axis',(-1.06057523872491E-16,-6.12323399573667E-17,
1.));
#116156=DIRECTION('ref_axis',(0.866025403784443,0.499999999999992,1.22464679914735E-16));
#116157=DIRECTION('center_axis',(-1.07851490188884E-14,-1.,0.));
#116158=DIRECTION('ref_axis',(-1.,1.04744440165294E-14,0.));
#116159=DIRECTION('center_axis',(-1.22464679914735E-16,1.28274943376909E-30,
1.));
#116160=DIRECTION('ref_axis',(1.,-1.04744440165294E-14,1.22464679914735E-16));
#116161=DIRECTION('center_axis',(-0.50000000000001,-0.866025403784433,0.));
#116162=DIRECTION('ref_axis',(-0.866025403784433,0.50000000000001,0.));
#116163=DIRECTION('center_axis',(-1.0605752387249E-16,6.12323399573689E-17,
1.));
#116164=DIRECTION('ref_axis',(0.866025403784433,-0.50000000000001,1.22464679914735E-16));
#116165=DIRECTION('center_axis',(-0.866025403784445,-0.499999999999989,
0.));
#116166=DIRECTION('ref_axis',(-0.499999999999989,0.866025403784445,0.));
#116167=DIRECTION('center_axis',(-6.12323399573663E-17,1.06057523872491E-16,
1.));
#116168=DIRECTION('ref_axis',(0.499999999999989,-0.866025403784445,1.22464679914735E-16));
#116169=DIRECTION('center_axis',(0.,0.,1.));
#116170=DIRECTION('ref_axis',(1.,0.,0.));
#116171=DIRECTION('center_axis',(0.,0.,1.));
#116172=DIRECTION('ref_axis',(1.,0.,0.));
#116173=DIRECTION('',(0.,0.,-1.));
#116174=DIRECTION('center_axis',(0.,0.,1.));
#116175=DIRECTION('ref_axis',(1.,0.,0.));
#116176=DIRECTION('center_axis',(0.,0.,1.));
#116177=DIRECTION('ref_axis',(1.,0.,0.));
#116178=DIRECTION('center_axis',(0.,0.,1.));
#116179=DIRECTION('ref_axis',(1.,0.,0.));
#116180=DIRECTION('',(0.,0.,1.));
#116181=DIRECTION('center_axis',(0.,0.,1.));
#116182=DIRECTION('ref_axis',(1.,0.,0.));
#116183=DIRECTION('center_axis',(0.,0.,-1.));
#116184=DIRECTION('ref_axis',(-1.,0.,0.));
#116185=DIRECTION('center_axis',(0.,0.,1.));
#116186=DIRECTION('ref_axis',(1.,0.,0.));
#116187=DIRECTION('center_axis',(0.,0.,1.));
#116188=DIRECTION('ref_axis',(1.,0.,0.));
#116189=DIRECTION('center_axis',(0.,0.,1.));
#116190=DIRECTION('ref_axis',(1.,0.,0.));
#116191=DIRECTION('',(0.,0.,-1.));
#116192=DIRECTION('center_axis',(0.,0.,1.));
#116193=DIRECTION('ref_axis',(1.,0.,0.));
#116194=DIRECTION('center_axis',(0.,0.,1.));
#116195=DIRECTION('ref_axis',(1.,0.,0.));
#116196=DIRECTION('center_axis',(0.,0.,1.));
#116197=DIRECTION('ref_axis',(1.,0.,0.));
#116198=DIRECTION('',(0.,0.,1.));
#116199=DIRECTION('center_axis',(0.,0.,1.));
#116200=DIRECTION('ref_axis',(1.,0.,0.));
#116201=DIRECTION('center_axis',(0.,0.,1.));
#116202=DIRECTION('ref_axis',(1.,0.,0.));
#116203=DIRECTION('center_axis',(0.,0.,-1.));
#116204=DIRECTION('ref_axis',(-1.,0.,0.));
#116205=DIRECTION('axis',(0.,0.,1.));
#116206=DIRECTION('refdir',(1.,0.,0.));
#116207=DIRECTION('center_axis',(0.,0.,1.));
#116208=DIRECTION('ref_axis',(0.,1.,0.));
#116209=DIRECTION('',(0.,0.,-1.));
#116210=DIRECTION('center_axis',(-1.94626492602832E-14,6.50402624464167E-14,
-1.));
#116211=DIRECTION('ref_axis',(1.5941429827944E-14,-1.,-6.51827352964822E-14));
#116212=DIRECTION('center_axis',(0.,0.,1.));
#116213=DIRECTION('ref_axis',(0.,1.,0.));
#116214=DIRECTION('',(0.,0.,-1.));
#116215=DIRECTION('center_axis',(-1.94626492602832E-14,6.50402624464167E-14,
-1.));
#116216=DIRECTION('ref_axis',(1.5941429827944E-14,-1.,-6.51827352964822E-14));
#116217=DIRECTION('center_axis',(0.,0.,1.));
#116218=DIRECTION('ref_axis',(0.,1.,0.));
#116219=DIRECTION('',(0.,0.,-1.));
#116220=DIRECTION('center_axis',(0.,0.,1.));
#116221=DIRECTION('ref_axis',(0.,1.,0.));
#116222=DIRECTION('',(0.,0.,-1.));
#116223=DIRECTION('center_axis',(0.,0.,1.));
#116224=DIRECTION('ref_axis',(0.,1.,0.));
#116225=DIRECTION('',(0.,0.,-1.));
#116226=DIRECTION('center_axis',(0.,0.,1.));
#116227=DIRECTION('ref_axis',(0.,1.,0.));
#116228=DIRECTION('',(0.,0.,-1.));
#116229=DIRECTION('center_axis',(0.,0.,1.));
#116230=DIRECTION('ref_axis',(0.,1.,0.));
#116231=DIRECTION('',(0.,0.,-1.));
#116232=DIRECTION('center_axis',(0.,0.,1.));
#116233=DIRECTION('ref_axis',(0.,1.,0.));
#116234=DIRECTION('',(0.,0.,-1.));
#116235=DIRECTION('center_axis',(0.,0.,1.));
#116236=DIRECTION('ref_axis',(0.,1.,0.));
#116237=DIRECTION('',(0.,0.,-1.));
#116238=DIRECTION('center_axis',(0.,0.,1.));
#116239=DIRECTION('ref_axis',(0.,1.,0.));
#116240=DIRECTION('',(0.,0.,-1.));
#116241=DIRECTION('center_axis',(0.,0.,1.));
#116242=DIRECTION('ref_axis',(0.,1.,0.));
#116243=DIRECTION('',(0.,0.,-1.));
#116244=DIRECTION('center_axis',(0.,0.,1.));
#116245=DIRECTION('ref_axis',(0.,1.,0.));
#116246=DIRECTION('',(0.,0.,-1.));
#116247=DIRECTION('center_axis',(0.,0.,1.));
#116248=DIRECTION('ref_axis',(0.,1.,0.));
#116249=DIRECTION('',(0.,0.,-1.));
#116250=DIRECTION('center_axis',(0.,0.,1.));
#116251=DIRECTION('ref_axis',(0.,1.,0.));
#116252=DIRECTION('',(0.,0.,-1.));
#116253=DIRECTION('center_axis',(0.,0.,1.));
#116254=DIRECTION('ref_axis',(0.,1.,0.));
#116255=DIRECTION('',(0.,0.,-1.));
#116256=DIRECTION('center_axis',(0.,0.,1.));
#116257=DIRECTION('ref_axis',(0.,1.,0.));
#116258=DIRECTION('',(0.,0.,-1.));
#116259=DIRECTION('center_axis',(0.,2.71050543121376E-17,-1.));
#116260=DIRECTION('ref_axis',(0.,1.,2.71050543121376E-17));
#116261=DIRECTION('',(0.,-2.71050543121376E-17,1.));
#116262=DIRECTION('center_axis',(0.,0.,-1.));
#116263=DIRECTION('ref_axis',(1.,-3.5527136788005E-15,0.));
#116264=DIRECTION('center_axis',(0.,2.71050543121376E-17,-1.));
#116265=DIRECTION('ref_axis',(0.,1.,2.71050543121376E-17));
#116266=DIRECTION('',(0.,-2.71050543121376E-17,1.));
#116267=DIRECTION('center_axis',(0.,2.71050543121376E-17,-1.));
#116268=DIRECTION('ref_axis',(0.,1.,2.71050543121376E-17));
#116269=DIRECTION('',(0.,-2.71050543121376E-17,1.));
#116270=DIRECTION('center_axis',(0.,2.71050543121376E-17,-1.));
#116271=DIRECTION('ref_axis',(0.,1.,2.71050543121376E-17));
#116272=DIRECTION('',(0.,-2.71050543121376E-17,1.));
#116273=DIRECTION('center_axis',(0.,2.71050543121376E-17,-1.));
#116274=DIRECTION('ref_axis',(0.,1.,2.71050543121376E-17));
#116275=DIRECTION('',(0.,-2.71050543121376E-17,1.));
#116276=DIRECTION('center_axis',(0.,2.71050543121376E-17,-1.));
#116277=DIRECTION('ref_axis',(0.,1.,2.71050543121376E-17));
#116278=DIRECTION('',(0.,-2.71050543121376E-17,1.));
#116279=DIRECTION('center_axis',(0.,2.71050543121376E-17,-1.));
#116280=DIRECTION('ref_axis',(0.,1.,2.71050543121376E-17));
#116281=DIRECTION('',(0.,-2.71050543121376E-17,1.));
#116282=DIRECTION('center_axis',(0.,2.71050543121376E-17,-1.));
#116283=DIRECTION('ref_axis',(0.,1.,2.71050543121376E-17));
#116284=DIRECTION('',(0.,-2.71050543121376E-17,1.));
#116285=DIRECTION('center_axis',(0.,2.71050543121376E-17,-1.));
#116286=DIRECTION('ref_axis',(0.,1.,2.71050543121376E-17));
#116287=DIRECTION('',(0.,-2.71050543121376E-17,1.));
#116288=DIRECTION('center_axis',(0.,2.71050543121376E-17,-1.));
#116289=DIRECTION('ref_axis',(0.,1.,2.71050543121376E-17));
#116290=DIRECTION('',(0.,-2.71050543121376E-17,1.));
#116291=DIRECTION('center_axis',(0.,2.71050543121376E-17,-1.));
#116292=DIRECTION('ref_axis',(0.,1.,2.71050543121376E-17));
#116293=DIRECTION('',(0.,-2.71050543121376E-17,1.));
#116294=DIRECTION('center_axis',(0.,2.71050543121376E-17,-1.));
#116295=DIRECTION('ref_axis',(0.,1.,2.71050543121376E-17));
#116296=DIRECTION('',(0.,-2.71050543121376E-17,1.));
#116297=DIRECTION('center_axis',(0.,2.71050543121376E-17,-1.));
#116298=DIRECTION('ref_axis',(0.,1.,2.71050543121376E-17));
#116299=DIRECTION('',(0.,-2.71050543121376E-17,1.));
#116300=DIRECTION('center_axis',(0.,2.71050543121376E-17,-1.));
#116301=DIRECTION('ref_axis',(0.,1.,2.71050543121376E-17));
#116302=DIRECTION('',(0.,-2.71050543121376E-17,1.));
#116303=DIRECTION('center_axis',(0.,2.71050543121376E-17,-1.));
#116304=DIRECTION('ref_axis',(0.,1.,2.71050543121376E-17));
#116305=DIRECTION('',(0.,-2.71050543121376E-17,1.));
#116306=DIRECTION('center_axis',(0.,0.,1.));
#116307=DIRECTION('ref_axis',(1.,0.,0.));
#116308=DIRECTION('center_axis',(0.,0.,1.));
#116309=DIRECTION('ref_axis',(1.,0.,0.));
#116310=DIRECTION('center_axis',(1.,6.9217303377289E-15,0.));
#116311=DIRECTION('ref_axis',(6.98296267768627E-15,-1.,0.));
#116312=DIRECTION('center_axis',(0.,0.,-1.));
#116313=DIRECTION('ref_axis',(-1.,0.,0.));
#116314=DIRECTION('center_axis',(0.,0.,1.));
#116315=DIRECTION('ref_axis',(1.,0.,0.));
#116316=DIRECTION('center_axis',(0.,0.,-1.));
#116317=DIRECTION('ref_axis',(-1.,0.,0.));
#116318=DIRECTION('center_axis',(0.,0.,-1.));
#116319=DIRECTION('ref_axis',(-1.,0.,0.));
#116320=DIRECTION('',(0.,0.,1.));
#116321=DIRECTION('center_axis',(0.,0.,-1.));
#116322=DIRECTION('ref_axis',(-1.,0.,0.));
#116323=DIRECTION('center_axis',(0.,-2.71050543121376E-17,1.));
#116324=DIRECTION('ref_axis',(0.,-1.,-2.71050543121376E-17));
#116325=DIRECTION('center_axis',(0.,-2.71050543121376E-17,1.));
#116326=DIRECTION('ref_axis',(1.77635683940025E-15,1.,2.71050543121376E-17));
#116327=DIRECTION('',(8.65956056235491E-17,-0.707106781186546,-0.707106781186549));
#116328=DIRECTION('center_axis',(0.,2.71050543121376E-17,-1.));
#116329=DIRECTION('ref_axis',(0.,1.,2.71050543121376E-17));
#116330=DIRECTION('center_axis',(0.,2.71050543121376E-17,-1.));
#116331=DIRECTION('ref_axis',(0.,1.,2.71050543121376E-17));
#116332=DIRECTION('center_axis',(0.,2.71050543121376E-17,-1.));
#116333=DIRECTION('ref_axis',(0.,1.,2.71050543121376E-17));
#116334=DIRECTION('center_axis',(0.,0.,1.));
#116335=DIRECTION('ref_axis',(1.,0.,0.));
#116336=DIRECTION('center_axis',(1.77885347431222E-15,2.70173479802082E-15,
-1.));
#116337=DIRECTION('ref_axis',(-0.700629269222034,-0.713525491562424,-3.07020130019678E-15));
#116338=DIRECTION('center_axis',(0.,0.,-1.));
#116339=DIRECTION('ref_axis',(-1.,0.,0.));
#116340=DIRECTION('center_axis',(0.,0.,-1.));
#116341=DIRECTION('ref_axis',(-1.,0.,0.));
#116342=DIRECTION('center_axis',(0.,0.,1.));
#116343=DIRECTION('ref_axis',(1.,0.,0.));
#116344=DIRECTION('center_axis',(0.,0.,1.));
#116345=DIRECTION('ref_axis',(1.,0.,0.));
#116346=DIRECTION('center_axis',(0.,0.,1.));
#116347=DIRECTION('ref_axis',(1.,0.,0.));
#116348=DIRECTION('center_axis',(0.,0.,1.));
#116349=DIRECTION('ref_axis',(1.,0.,0.));
#116350=DIRECTION('center_axis',(0.,0.,1.));
#116351=DIRECTION('ref_axis',(1.,0.,0.));
#116352=DIRECTION('center_axis',(0.,0.,1.));
#116353=DIRECTION('ref_axis',(1.,0.,0.));
#116354=DIRECTION('center_axis',(0.,0.,1.));
#116355=DIRECTION('ref_axis',(1.,0.,0.));
#116356=DIRECTION('center_axis',(0.,0.,1.));
#116357=DIRECTION('ref_axis',(-1.,-3.21624529935327E-16,0.));
#116358=DIRECTION('center_axis',(0.,0.,1.));
#116359=DIRECTION('ref_axis',(1.,0.,0.));
#116360=DIRECTION('center_axis',(0.,0.,1.));
#116361=DIRECTION('ref_axis',(1.,0.,0.));
#116362=DIRECTION('center_axis',(0.,0.,1.));
#116363=DIRECTION('ref_axis',(1.,0.,0.));
#116364=DIRECTION('',(0.866025403784438,0.5,0.));
#116365=DIRECTION('',(0.,1.,0.));
#116366=DIRECTION('',(-0.866025403784439,0.5,0.));
#116367=DIRECTION('',(-0.866025403784438,-0.5,0.));
#116368=DIRECTION('',(1.87789324842145E-16,-1.,0.));
#116369=DIRECTION('',(0.866025403784438,-0.5,0.));
#116370=DIRECTION('center_axis',(1.,0.,0.));
#116371=DIRECTION('ref_axis',(0.,0.,-1.));
#116372=DIRECTION('',(0.,0.,1.));
#116373=DIRECTION('',(0.,0.,1.));
#116374=DIRECTION('center_axis',(0.5,0.866025403784439,0.));
#116375=DIRECTION('ref_axis',(-0.866025403784439,0.5,0.));
#116376=DIRECTION('',(0.,0.,1.));
#116377=DIRECTION('center_axis',(-0.5,0.866025403784439,0.));
#116378=DIRECTION('ref_axis',(-0.866025403784439,-0.5,0.));
#116379=DIRECTION('',(0.,0.,1.));
#116380=DIRECTION('center_axis',(-1.,-1.87789324842145E-16,0.));
#116381=DIRECTION('ref_axis',(1.87789324842145E-16,-1.,0.));
#116382=DIRECTION('',(0.,0.,1.));
#116383=DIRECTION('center_axis',(-0.5,-0.866025403784439,0.));
#116384=DIRECTION('ref_axis',(0.866025403784439,-0.5,0.));
#116385=DIRECTION('',(0.,0.,1.));
#116386=DIRECTION('center_axis',(0.5,-0.866025403784438,0.));
#116387=DIRECTION('ref_axis',(0.866025403784438,0.5,0.));
#116388=DIRECTION('center_axis',(0.,0.,1.));
#116389=DIRECTION('ref_axis',(0.,1.,0.));
#116390=DIRECTION('axis',(0.,0.,1.));
#116391=DIRECTION('refdir',(1.,0.,0.));
#116392=DIRECTION('center_axis',(-1.02434006807916E-22,-1.4843197546388E-38,
-1.));
#116393=DIRECTION('ref_axis',(-1.4490497842403E-16,1.,0.));
#116394=DIRECTION('',(1.02434006807916E-22,1.4843197546388E-38,1.));
#116395=DIRECTION('center_axis',(0.,-6.8448976313476E-17,-1.));
#116396=DIRECTION('ref_axis',(-1.4490497842403E-16,1.,0.));
#116397=DIRECTION('center_axis',(-1.02434006807916E-22,-1.4843197546388E-38,
-1.));
#116398=DIRECTION('ref_axis',(-1.4490497842403E-16,1.,0.));
#116399=DIRECTION('',(1.02434006807916E-22,1.4843197546388E-38,1.));
#116400=DIRECTION('center_axis',(-1.02434006807916E-22,-1.4843197546388E-38,
-1.));
#116401=DIRECTION('ref_axis',(-1.4490497842403E-16,1.,0.));
#116402=DIRECTION('',(1.02434006807916E-22,1.4843197546388E-38,1.));
#116403=DIRECTION('center_axis',(-1.02434006807916E-22,-1.4843197546388E-38,
-1.));
#116404=DIRECTION('ref_axis',(-1.4490497842403E-16,1.,0.));
#116405=DIRECTION('',(1.02434006807916E-22,1.4843197546388E-38,1.));
#116406=DIRECTION('center_axis',(-1.02434006807916E-22,-1.4843197546388E-38,
-1.));
#116407=DIRECTION('ref_axis',(-1.4490497842403E-16,1.,0.));
#116408=DIRECTION('',(1.02434006807916E-22,1.4843197546388E-38,1.));
#116409=DIRECTION('center_axis',(-1.02434006807916E-22,-1.4843197546388E-38,
-1.));
#116410=DIRECTION('ref_axis',(-1.4490497842403E-16,1.,0.));
#116411=DIRECTION('',(1.02434006807916E-22,1.4843197546388E-38,1.));
#116412=DIRECTION('center_axis',(-1.02434006807916E-22,-1.4843197546388E-38,
-1.));
#116413=DIRECTION('ref_axis',(-1.4490497842403E-16,1.,0.));
#116414=DIRECTION('',(1.02434006807916E-22,1.4843197546388E-38,1.));
#116415=DIRECTION('center_axis',(-1.02434006807916E-22,-1.4843197546388E-38,
-1.));
#116416=DIRECTION('ref_axis',(-1.4490497842403E-16,1.,0.));
#116417=DIRECTION('',(1.02434006807916E-22,1.4843197546388E-38,1.));
#116418=DIRECTION('center_axis',(-1.02434006807916E-22,-1.4843197546388E-38,
-1.));
#116419=DIRECTION('ref_axis',(-1.4490497842403E-16,1.,0.));
#116420=DIRECTION('',(1.02434006807916E-22,1.4843197546388E-38,1.));
#116421=DIRECTION('center_axis',(-1.02434006807916E-22,-1.4843197546388E-38,
-1.));
#116422=DIRECTION('ref_axis',(-1.4490497842403E-16,1.,0.));
#116423=DIRECTION('',(1.02434006807916E-22,1.4843197546388E-38,1.));
#116424=DIRECTION('center_axis',(-1.02434006807916E-22,-1.4843197546388E-38,
-1.));
#116425=DIRECTION('ref_axis',(-1.4490497842403E-16,1.,0.));
#116426=DIRECTION('',(1.02434006807916E-22,1.4843197546388E-38,1.));
#116427=DIRECTION('center_axis',(-1.02434006807916E-22,-1.4843197546388E-38,
-1.));
#116428=DIRECTION('ref_axis',(-1.4490497842403E-16,1.,0.));
#116429=DIRECTION('',(1.02434006807916E-22,1.4843197546388E-38,1.));
#116430=DIRECTION('center_axis',(-1.02434006807916E-22,-1.4843197546388E-38,
-1.));
#116431=DIRECTION('ref_axis',(-1.4490497842403E-16,1.,0.));
#116432=DIRECTION('',(1.02434006807916E-22,1.4843197546388E-38,1.));
#116433=DIRECTION('center_axis',(-1.02434006807916E-22,-1.4843197546388E-38,
-1.));
#116434=DIRECTION('ref_axis',(-1.4490497842403E-16,1.,0.));
#116435=DIRECTION('',(1.02434006807916E-22,1.4843197546388E-38,1.));
#116436=DIRECTION('center_axis',(-1.02434006807916E-22,-1.4843197546388E-38,
-1.));
#116437=DIRECTION('ref_axis',(-1.4490497842403E-16,1.,0.));
#116438=DIRECTION('',(1.02434006807916E-22,1.4843197546388E-38,1.));
#116439=DIRECTION('center_axis',(-4.78053475807573E-13,1.83844196516503E-12,
-1.));
#116440=DIRECTION('ref_axis',(-1.50232827312377E-11,-1.,-1.83855436624071E-12));
#116441=DIRECTION('center_axis',(0.,1.47731603554264E-17,1.));
#116442=DIRECTION('ref_axis',(0.,-1.,1.47731603554264E-17));
#116443=DIRECTION('',(0.,-1.47731603554264E-17,-1.));
#116444=DIRECTION('center_axis',(0.,1.47731603554263E-17,1.));
#116445=DIRECTION('ref_axis',(0.,-1.,1.47731603554263E-17));
#116446=DIRECTION('center_axis',(0.,1.47731603554264E-17,1.));
#116447=DIRECTION('ref_axis',(0.,-1.,1.47731603554264E-17));
#116448=DIRECTION('',(0.,-1.47731603554264E-17,-1.));
#116449=DIRECTION('center_axis',(0.,1.47731603554264E-17,1.));
#116450=DIRECTION('ref_axis',(0.,-1.,1.47731603554264E-17));
#116451=DIRECTION('',(0.,-1.47731603554264E-17,-1.));
#116452=DIRECTION('center_axis',(0.,1.47731603554264E-17,1.));
#116453=DIRECTION('ref_axis',(0.,-1.,1.47731603554264E-17));
#116454=DIRECTION('',(0.,-1.47731603554264E-17,-1.));
#116455=DIRECTION('center_axis',(0.,1.47731603554264E-17,1.));
#116456=DIRECTION('ref_axis',(0.,-1.,1.47731603554264E-17));
#116457=DIRECTION('',(0.,-1.47731603554264E-17,-1.));
#116458=DIRECTION('center_axis',(0.,1.47731603554264E-17,1.));
#116459=DIRECTION('ref_axis',(0.,-1.,1.47731603554264E-17));
#116460=DIRECTION('',(0.,-1.47731603554264E-17,-1.));
#116461=DIRECTION('center_axis',(0.,1.47731603554264E-17,1.));
#116462=DIRECTION('ref_axis',(0.,-1.,1.47731603554264E-17));
#116463=DIRECTION('',(0.,-1.47731603554264E-17,-1.));
#116464=DIRECTION('center_axis',(0.,1.47731603554264E-17,1.));
#116465=DIRECTION('ref_axis',(0.,-1.,1.47731603554264E-17));
#116466=DIRECTION('',(0.,-1.47731603554264E-17,-1.));
#116467=DIRECTION('center_axis',(0.,1.47731603554264E-17,1.));
#116468=DIRECTION('ref_axis',(0.,-1.,1.47731603554264E-17));
#116469=DIRECTION('',(0.,-1.47731603554264E-17,-1.));
#116470=DIRECTION('center_axis',(0.,1.47731603554264E-17,1.));
#116471=DIRECTION('ref_axis',(0.,-1.,1.47731603554264E-17));
#116472=DIRECTION('',(0.,-1.47731603554264E-17,-1.));
#116473=DIRECTION('center_axis',(0.,1.47731603554264E-17,1.));
#116474=DIRECTION('ref_axis',(0.,-1.,1.47731603554264E-17));
#116475=DIRECTION('',(0.,-1.47731603554264E-17,-1.));
#116476=DIRECTION('center_axis',(0.,1.47731603554264E-17,1.));
#116477=DIRECTION('ref_axis',(0.,-1.,1.47731603554264E-17));
#116478=DIRECTION('',(0.,-1.47731603554264E-17,-1.));
#116479=DIRECTION('center_axis',(0.,1.47731603554264E-17,1.));
#116480=DIRECTION('ref_axis',(0.,-1.,1.47731603554264E-17));
#116481=DIRECTION('',(0.,-1.47731603554264E-17,-1.));
#116482=DIRECTION('center_axis',(0.,1.47731603554264E-17,1.));
#116483=DIRECTION('ref_axis',(0.,-1.,1.47731603554264E-17));
#116484=DIRECTION('',(0.,-1.47731603554264E-17,-1.));
#116485=DIRECTION('center_axis',(0.,1.47731603554263E-17,1.));
#116486=DIRECTION('ref_axis',(0.,-1.,1.47731603554263E-17));
#116487=DIRECTION('center_axis',(-4.78053475807573E-13,1.83844196516503E-12,
-1.));
#116488=DIRECTION('ref_axis',(-1.50232827312377E-11,-1.,-1.83855436624071E-12));
#116489=DIRECTION('',(8.65956056235495E-17,-0.707106781186549,-0.707106781186546));
#116490=DIRECTION('center_axis',(0.,-1.47731603554264E-17,-1.));
#116491=DIRECTION('ref_axis',(0.,-1.,1.47731603554264E-17));
#116492=DIRECTION('center_axis',(0.,1.47731603554264E-17,1.));
#116493=DIRECTION('ref_axis',(0.,-1.,1.47731603554264E-17));
#116494=DIRECTION('center_axis',(0.,6.8448976313476E-17,1.));
#116495=DIRECTION('ref_axis',(0.,-1.,6.8448976313476E-17));
#116496=DIRECTION('center_axis',(0.,0.,1.));
#116497=DIRECTION('ref_axis',(-1.,0.,0.));
#116498=DIRECTION('center_axis',(0.,0.,-1.));
#116499=DIRECTION('ref_axis',(-1.,0.,0.));
#116500=DIRECTION('center_axis',(0.,6.8448976313476E-17,1.));
#116501=DIRECTION('ref_axis',(0.,-1.,6.8448976313476E-17));
#116502=DIRECTION('center_axis',(0.,6.8448976313476E-17,1.));
#116503=DIRECTION('ref_axis',(0.,-1.,6.8448976313476E-17));
#116504=DIRECTION('',(0.,-6.8448976313476E-17,-1.));
#116505=DIRECTION('center_axis',(0.,6.8448976313476E-17,1.));
#116506=DIRECTION('ref_axis',(0.,-1.,6.8448976313476E-17));
#116507=DIRECTION('center_axis',(0.,6.8448976313476E-17,1.));
#116508=DIRECTION('ref_axis',(0.,-1.,6.8448976313476E-17));
#116509=DIRECTION('',(8.65956056235493E-17,-0.707106781186548,-0.707106781186548));
#116510=DIRECTION('center_axis',(0.,6.8448976313476E-17,1.));
#116511=DIRECTION('ref_axis',(0.,-1.,6.8448976313476E-17));
#116512=DIRECTION('center_axis',(0.,6.8448976313476E-17,1.));
#116513=DIRECTION('ref_axis',(0.,-1.,6.8448976313476E-17));
#116514=DIRECTION('center_axis',(0.,-6.8448976313476E-17,-1.));
#116515=DIRECTION('ref_axis',(0.,1.,-6.8448976313476E-17));
#116516=DIRECTION('center_axis',(0.,0.,-1.));
#116517=DIRECTION('ref_axis',(-1.,0.,0.));
#116518=DIRECTION('center_axis',(0.,0.,-1.));
#116519=DIRECTION('ref_axis',(-1.,0.,0.));
#116520=DIRECTION('center_axis',(0.,0.,-1.));
#116521=DIRECTION('ref_axis',(-1.,0.,0.));
#116522=DIRECTION('center_axis',(0.,0.,-1.));
#116523=DIRECTION('ref_axis',(-1.,0.,0.));
#116524=DIRECTION('center_axis',(0.,0.,-1.));
#116525=DIRECTION('ref_axis',(-1.,0.,0.));
#116526=DIRECTION('center_axis',(0.,-6.8448976313476E-17,-1.));
#116527=DIRECTION('ref_axis',(0.,1.,-6.8448976313476E-17));
#116528=DIRECTION('center_axis',(0.,0.,1.));
#116529=DIRECTION('ref_axis',(1.,-7.6571373978539E-16,0.));
#116530=DIRECTION('center_axis',(0.,0.,1.));
#116531=DIRECTION('ref_axis',(-1.,0.,0.));
#116532=DIRECTION('center_axis',(0.,0.,1.));
#116533=DIRECTION('ref_axis',(-1.,0.,0.));
#116534=DIRECTION('center_axis',(0.,0.,1.));
#116535=DIRECTION('ref_axis',(-1.,0.,0.));
#116536=DIRECTION('center_axis',(0.,0.,1.));
#116537=DIRECTION('ref_axis',(-1.,0.,0.));
#116538=DIRECTION('center_axis',(0.,0.,1.));
#116539=DIRECTION('ref_axis',(1.,0.,0.));
#116540=DIRECTION('',(0.866025403784438,0.5,0.));
#116541=DIRECTION('',(2.50385766456193E-16,1.,0.));
#116542=DIRECTION('',(-0.866025403784439,0.5,0.));
#116543=DIRECTION('',(-0.866025403784439,-0.5,0.));
#116544=DIRECTION('',(2.50385766456193E-16,-1.,0.));
#116545=DIRECTION('',(0.866025403784438,-0.5,0.));
#116546=DIRECTION('center_axis',(1.,-2.50385766456193E-16,0.));
#116547=DIRECTION('ref_axis',(2.50385766456193E-16,1.,0.));
#116548=DIRECTION('',(0.,0.,1.));
#116549=DIRECTION('',(0.,0.,1.));
#116550=DIRECTION('center_axis',(0.5,0.866025403784439,0.));
#116551=DIRECTION('ref_axis',(-0.866025403784439,0.5,0.));
#116552=DIRECTION('',(0.,0.,1.));
#116553=DIRECTION('center_axis',(-0.5,0.866025403784439,0.));
#116554=DIRECTION('ref_axis',(-0.866025403784439,-0.5,0.));
#116555=DIRECTION('',(0.,0.,1.));
#116556=DIRECTION('center_axis',(-1.,-2.50385766456193E-16,0.));
#116557=DIRECTION('ref_axis',(2.50385766456193E-16,-1.,0.));
#116558=DIRECTION('',(0.,0.,1.));
#116559=DIRECTION('center_axis',(-0.5,-0.866025403784439,0.));
#116560=DIRECTION('ref_axis',(0.866025403784439,-0.5,0.));
#116561=DIRECTION('',(0.,0.,1.));
#116562=DIRECTION('center_axis',(0.5,-0.866025403784439,0.));
#116563=DIRECTION('ref_axis',(0.866025403784439,0.5,0.));
#116564=DIRECTION('center_axis',(0.,1.47731603554264E-17,1.));
#116565=DIRECTION('ref_axis',(0.,-1.,1.47731603554264E-17));
#116566=DIRECTION('center_axis',(-1.02434006807916E-22,-1.4843197546388E-38,
-1.));
#116567=DIRECTION('ref_axis',(-1.4490497842403E-16,1.,0.));
#116568=DIRECTION('axis',(0.,0.,1.));
#116569=DIRECTION('refdir',(1.,0.,0.));
#116570=DIRECTION('center_axis',(0.,0.,1.));
#116571=DIRECTION('ref_axis',(-5.9042332696092E-17,1.,0.));
#116572=DIRECTION('',(0.,0.,-1.));
#116573=DIRECTION('center_axis',(0.,0.,1.));
#116574=DIRECTION('ref_axis',(1.,0.,0.));
#116575=DIRECTION('center_axis',(0.,0.,1.));
#116576=DIRECTION('ref_axis',(-5.9042332696092E-17,1.,0.));
#116577=DIRECTION('',(0.,0.,-1.));
#116578=DIRECTION('center_axis',(0.,0.,1.));
#116579=DIRECTION('ref_axis',(-5.9042332696092E-17,1.,0.));
#116580=DIRECTION('',(0.,0.,-1.));
#116581=DIRECTION('center_axis',(0.,0.,1.));
#116582=DIRECTION('ref_axis',(-5.9042332696092E-17,1.,0.));
#116583=DIRECTION('',(0.,0.,-1.));
#116584=DIRECTION('center_axis',(0.,0.,1.));
#116585=DIRECTION('ref_axis',(-5.9042332696092E-17,1.,0.));
#116586=DIRECTION('',(0.,0.,-1.));
#116587=DIRECTION('center_axis',(0.,0.,1.));
#116588=DIRECTION('ref_axis',(-5.9042332696092E-17,1.,0.));
#116589=DIRECTION('',(0.,0.,-1.));
#116590=DIRECTION('center_axis',(0.,0.,1.));
#116591=DIRECTION('ref_axis',(-5.9042332696092E-17,1.,0.));
#116592=DIRECTION('',(0.,0.,-1.));
#116593=DIRECTION('center_axis',(0.,0.,1.));
#116594=DIRECTION('ref_axis',(-5.9042332696092E-17,1.,0.));
#116595=DIRECTION('',(0.,0.,-1.));
#116596=DIRECTION('center_axis',(0.,0.,1.));
#116597=DIRECTION('ref_axis',(-5.9042332696092E-17,1.,0.));
#116598=DIRECTION('',(0.,0.,-1.));
#116599=DIRECTION('center_axis',(0.,0.,1.));
#116600=DIRECTION('ref_axis',(-5.9042332696092E-17,1.,0.));
#116601=DIRECTION('',(0.,0.,-1.));
#116602=DIRECTION('center_axis',(0.,0.,1.));
#116603=DIRECTION('ref_axis',(-5.9042332696092E-17,1.,0.));
#116604=DIRECTION('',(0.,0.,-1.));
#116605=DIRECTION('center_axis',(0.,0.,1.));
#116606=DIRECTION('ref_axis',(-5.9042332696092E-17,1.,0.));
#116607=DIRECTION('',(0.,0.,-1.));
#116608=DIRECTION('center_axis',(0.,0.,1.));
#116609=DIRECTION('ref_axis',(-5.9042332696092E-17,1.,0.));
#116610=DIRECTION('',(0.,0.,-1.));
#116611=DIRECTION('center_axis',(0.,0.,1.));
#116612=DIRECTION('ref_axis',(-5.9042332696092E-17,1.,0.));
#116613=DIRECTION('',(0.,0.,-1.));
#116614=DIRECTION('center_axis',(0.,0.,1.));
#116615=DIRECTION('ref_axis',(-5.9042332696092E-17,1.,0.));
#116616=DIRECTION('',(0.,0.,-1.));
#116617=DIRECTION('center_axis',(0.,0.,1.));
#116618=DIRECTION('ref_axis',(-5.9042332696092E-17,1.,0.));
#116619=DIRECTION('',(0.,0.,-1.));
#116620=DIRECTION('center_axis',(0.,0.,1.));
#116621=DIRECTION('ref_axis',(-5.9042332696092E-17,1.,0.));
#116622=DIRECTION('',(0.,0.,-1.));
#116623=DIRECTION('center_axis',(0.,0.,1.));
#116624=DIRECTION('ref_axis',(-5.9042332696092E-17,1.,0.));
#116625=DIRECTION('',(0.,0.,-1.));
#116626=DIRECTION('center_axis',(0.,0.,1.));
#116627=DIRECTION('ref_axis',(-5.9042332696092E-17,1.,0.));
#116628=DIRECTION('',(0.,0.,-1.));
#116629=DIRECTION('center_axis',(0.,0.,1.));
#116630=DIRECTION('ref_axis',(-5.9042332696092E-17,1.,0.));
#116631=DIRECTION('',(0.,0.,-1.));
#116632=DIRECTION('center_axis',(0.,0.,1.));
#116633=DIRECTION('ref_axis',(-5.9042332696092E-17,1.,0.));
#116634=DIRECTION('',(0.,0.,-1.));
#116635=DIRECTION('center_axis',(0.,0.,1.));
#116636=DIRECTION('ref_axis',(-5.9042332696092E-17,1.,0.));
#116637=DIRECTION('',(0.,0.,-1.));
#116638=DIRECTION('center_axis',(0.,0.,1.));
#116639=DIRECTION('ref_axis',(-5.9042332696092E-17,1.,0.));
#116640=DIRECTION('',(0.,0.,-1.));
#116641=DIRECTION('center_axis',(0.,0.,1.));
#116642=DIRECTION('ref_axis',(-5.9042332696092E-17,1.,0.));
#116643=DIRECTION('',(0.,0.,-1.));
#116644=DIRECTION('center_axis',(0.,0.,1.));
#116645=DIRECTION('ref_axis',(-5.9042332696092E-17,1.,0.));
#116646=DIRECTION('',(0.,0.,-1.));
#116647=DIRECTION('center_axis',(0.,0.,1.));
#116648=DIRECTION('ref_axis',(-5.9042332696092E-17,1.,0.));
#116649=DIRECTION('',(0.,0.,-1.));
#116650=DIRECTION('center_axis',(0.,0.,1.));
#116651=DIRECTION('ref_axis',(-5.9042332696092E-17,1.,0.));
#116652=DIRECTION('',(0.,0.,-1.));
#116653=DIRECTION('center_axis',(0.,0.,1.));
#116654=DIRECTION('ref_axis',(-5.9042332696092E-17,1.,0.));
#116655=DIRECTION('',(0.,0.,-1.));
#116656=DIRECTION('center_axis',(0.,0.,1.));
#116657=DIRECTION('ref_axis',(-5.9042332696092E-17,1.,0.));
#116658=DIRECTION('',(0.,0.,-1.));
#116659=DIRECTION('center_axis',(0.,1.19813586852189E-16,-1.));
#116660=DIRECTION('ref_axis',(0.,1.,1.19813586852189E-16));
#116661=DIRECTION('',(0.,-1.19813586852189E-16,1.));
#116662=DIRECTION('center_axis',(0.,1.19813586852189E-16,-1.));
#116663=DIRECTION('ref_axis',(0.,1.,1.19813586852189E-16));
#116664=DIRECTION('',(0.,-1.19813586852189E-16,1.));
#116665=DIRECTION('center_axis',(0.,1.19813586852189E-16,-1.));
#116666=DIRECTION('ref_axis',(0.,1.,1.19813586852189E-16));
#116667=DIRECTION('center_axis',(0.,1.19813586852189E-16,-1.));
#116668=DIRECTION('ref_axis',(0.,1.,1.19813586852189E-16));
#116669=DIRECTION('center_axis',(0.,1.19813586852189E-16,-1.));
#116670=DIRECTION('ref_axis',(0.,1.,1.19813586852189E-16));
#116671=DIRECTION('',(0.,-1.19813586852189E-16,1.));
#116672=DIRECTION('center_axis',(0.,1.19813586852189E-16,-1.));
#116673=DIRECTION('ref_axis',(0.,1.,1.19813586852189E-16));
#116674=DIRECTION('',(0.,-1.19813586852189E-16,1.));
#116675=DIRECTION('center_axis',(0.,1.19813586852189E-16,-1.));
#116676=DIRECTION('ref_axis',(0.,1.,1.19813586852189E-16));
#116677=DIRECTION('',(0.,-1.19813586852189E-16,1.));
#116678=DIRECTION('center_axis',(0.,1.19813586852189E-16,-1.));
#116679=DIRECTION('ref_axis',(0.,1.,1.19813586852189E-16));
#116680=DIRECTION('',(0.,-1.19813586852189E-16,1.));
#116681=DIRECTION('center_axis',(0.,1.19813586852189E-16,-1.));
#116682=DIRECTION('ref_axis',(0.,1.,1.19813586852189E-16));
#116683=DIRECTION('',(0.,-1.19813586852189E-16,1.));
#116684=DIRECTION('center_axis',(0.,1.19813586852189E-16,-1.));
#116685=DIRECTION('ref_axis',(0.,1.,1.19813586852189E-16));
#116686=DIRECTION('',(0.,-1.19813586852189E-16,1.));
#116687=DIRECTION('center_axis',(0.,1.19813586852189E-16,-1.));
#116688=DIRECTION('ref_axis',(0.,1.,1.19813586852189E-16));
#116689=DIRECTION('',(0.,-1.19813586852189E-16,1.));
#116690=DIRECTION('center_axis',(0.,1.19813586852189E-16,-1.));
#116691=DIRECTION('ref_axis',(0.,1.,1.19813586852189E-16));
#116692=DIRECTION('',(0.,-1.19813586852189E-16,1.));
#116693=DIRECTION('center_axis',(0.,1.19813586852189E-16,-1.));
#116694=DIRECTION('ref_axis',(0.,1.,1.19813586852189E-16));
#116695=DIRECTION('',(0.,-1.19813586852189E-16,1.));
#116696=DIRECTION('center_axis',(0.,1.19813586852189E-16,-1.));
#116697=DIRECTION('ref_axis',(0.,1.,1.19813586852189E-16));
#116698=DIRECTION('',(0.,-1.19813586852189E-16,1.));
#116699=DIRECTION('center_axis',(0.,1.19813586852189E-16,-1.));
#116700=DIRECTION('ref_axis',(0.,1.,1.19813586852189E-16));
#116701=DIRECTION('',(0.,-1.19813586852189E-16,1.));
#116702=DIRECTION('center_axis',(0.,1.19813586852189E-16,-1.));
#116703=DIRECTION('ref_axis',(0.,1.,1.19813586852189E-16));
#116704=DIRECTION('',(0.,-1.19813586852189E-16,1.));
#116705=DIRECTION('center_axis',(0.,1.19813586852189E-16,-1.));
#116706=DIRECTION('ref_axis',(0.,1.,1.19813586852189E-16));
#116707=DIRECTION('',(0.,-1.19813586852189E-16,1.));
#116708=DIRECTION('center_axis',(0.,1.19813586852189E-16,-1.));
#116709=DIRECTION('ref_axis',(0.,1.,1.19813586852189E-16));
#116710=DIRECTION('',(0.,-1.19813586852189E-16,1.));
#116711=DIRECTION('center_axis',(0.,1.19813586852189E-16,-1.));
#116712=DIRECTION('ref_axis',(0.,1.,1.19813586852189E-16));
#116713=DIRECTION('',(0.,-1.19813586852189E-16,1.));
#116714=DIRECTION('center_axis',(0.,1.19813586852189E-16,-1.));
#116715=DIRECTION('ref_axis',(0.,1.,1.19813586852189E-16));
#116716=DIRECTION('',(0.,-1.19813586852189E-16,1.));
#116717=DIRECTION('center_axis',(0.,1.19813586852189E-16,-1.));
#116718=DIRECTION('ref_axis',(0.,1.,1.19813586852189E-16));
#116719=DIRECTION('',(0.,-1.19813586852189E-16,1.));
#116720=DIRECTION('center_axis',(0.,1.19813586852189E-16,-1.));
#116721=DIRECTION('ref_axis',(0.,1.,1.19813586852189E-16));
#116722=DIRECTION('',(0.,-1.19813586852189E-16,1.));
#116723=DIRECTION('center_axis',(0.,1.19813586852189E-16,-1.));
#116724=DIRECTION('ref_axis',(0.,1.,1.19813586852189E-16));
#116725=DIRECTION('',(0.,-1.19813586852189E-16,1.));
#116726=DIRECTION('center_axis',(0.,1.19813586852189E-16,-1.));
#116727=DIRECTION('ref_axis',(0.,1.,1.19813586852189E-16));
#116728=DIRECTION('',(0.,-1.19813586852189E-16,1.));
#116729=DIRECTION('center_axis',(0.,1.19813586852189E-16,-1.));
#116730=DIRECTION('ref_axis',(0.,1.,1.19813586852189E-16));
#116731=DIRECTION('',(0.,-1.19813586852189E-16,1.));
#116732=DIRECTION('center_axis',(0.,1.19813586852189E-16,-1.));
#116733=DIRECTION('ref_axis',(0.,1.,1.19813586852189E-16));
#116734=DIRECTION('',(0.,-1.19813586852189E-16,1.));
#116735=DIRECTION('center_axis',(0.,1.19813586852189E-16,-1.));
#116736=DIRECTION('ref_axis',(0.,1.,1.19813586852189E-16));
#116737=DIRECTION('',(0.,-1.19813586852189E-16,1.));
#116738=DIRECTION('center_axis',(0.,1.19813586852189E-16,-1.));
#116739=DIRECTION('ref_axis',(0.,1.,1.19813586852189E-16));
#116740=DIRECTION('',(0.,-1.19813586852189E-16,1.));
#116741=DIRECTION('center_axis',(0.,1.19813586852189E-16,-1.));
#116742=DIRECTION('ref_axis',(0.,1.,1.19813586852189E-16));
#116743=DIRECTION('',(0.,-1.19813586852189E-16,1.));
#116744=DIRECTION('center_axis',(0.,1.19813586852189E-16,-1.));
#116745=DIRECTION('ref_axis',(0.,1.,1.19813586852189E-16));
#116746=DIRECTION('',(0.,-1.19813586852189E-16,1.));
#116747=DIRECTION('center_axis',(0.,1.19813586852189E-16,-1.));
#116748=DIRECTION('ref_axis',(0.,1.,1.19813586852189E-16));
#116749=DIRECTION('',(0.,-1.19813586852189E-16,1.));
#116750=DIRECTION('center_axis',(0.,-1.19813586852189E-16,1.));
#116751=DIRECTION('ref_axis',(0.,-1.,-1.19813586852189E-16));
#116752=DIRECTION('',(8.65956056235489E-17,-0.707106781186543,-0.707106781186552));
#116753=DIRECTION('center_axis',(0.,0.,-1.));
#116754=DIRECTION('ref_axis',(0.989119496180713,-0.147114317030034,0.));
#116755=DIRECTION('center_axis',(0.,0.,1.));
#116756=DIRECTION('ref_axis',(1.,0.,0.));
#116757=DIRECTION('',(0.707106781186551,8.65956056235497E-17,-0.707106781186544));
#116758=DIRECTION('center_axis',(0.,0.,1.));
#116759=DIRECTION('ref_axis',(1.,0.,0.));
#116760=DIRECTION('center_axis',(0.,0.,1.));
#116761=DIRECTION('ref_axis',(1.,0.,0.));
#116762=DIRECTION('center_axis',(0.,0.,1.));
#116763=DIRECTION('ref_axis',(1.,0.,0.));
#116764=DIRECTION('center_axis',(0.,0.,1.));
#116765=DIRECTION('ref_axis',(1.,0.,0.));
#116766=DIRECTION('center_axis',(0.,-1.19813586852189E-16,1.));
#116767=DIRECTION('ref_axis',(0.,-1.,-1.19813586852189E-16));
#116768=DIRECTION('center_axis',(0.,1.19813586852189E-16,-1.));
#116769=DIRECTION('ref_axis',(0.,1.,1.19813586852189E-16));
#116770=DIRECTION('center_axis',(0.,1.19813586852189E-16,-1.));
#116771=DIRECTION('ref_axis',(0.,1.,0.));
#116772=DIRECTION('center_axis',(1.,-1.22464679914735E-16,-1.46729325632897E-32));
#116773=DIRECTION('ref_axis',(-1.22464679914735E-16,-1.,0.));
#116774=DIRECTION('center_axis',(0.,1.19813586852189E-16,-1.));
#116775=DIRECTION('ref_axis',(0.,1.,1.19813586852189E-16));
#116776=DIRECTION('center_axis',(0.,0.,1.));
#116777=DIRECTION('ref_axis',(1.,0.,0.));
#116778=DIRECTION('',(-0.86602540378444,-1.06057523872491E-16,0.499999999999998));
#116779=DIRECTION('center_axis',(0.,0.,-1.));
#116780=DIRECTION('ref_axis',(-1.,0.,0.));
#116781=DIRECTION('center_axis',(0.,0.,-1.));
#116782=DIRECTION('ref_axis',(-1.,0.,0.));
#116783=DIRECTION('center_axis',(0.,0.,-1.));
#116784=DIRECTION('ref_axis',(-1.,0.,0.));
#116785=DIRECTION('center_axis',(0.,0.,1.));
#116786=DIRECTION('ref_axis',(1.,0.,0.));
#116787=DIRECTION('center_axis',(0.,0.,-1.));
#116788=DIRECTION('ref_axis',(-1.,0.,0.));
#116789=DIRECTION('center_axis',(0.,0.,-1.));
#116790=DIRECTION('ref_axis',(-1.,0.,0.));
#116791=DIRECTION('center_axis',(0.,0.,1.));
#116792=DIRECTION('ref_axis',(1.,0.,0.));
#116793=DIRECTION('center_axis',(0.,0.,1.));
#116794=DIRECTION('ref_axis',(1.,0.,0.));
#116795=DIRECTION('center_axis',(0.,0.,1.));
#116796=DIRECTION('ref_axis',(1.,0.,0.));
#116797=DIRECTION('center_axis',(0.,0.,1.));
#116798=DIRECTION('ref_axis',(1.,0.,0.));
#116799=DIRECTION('center_axis',(1.22464679914735E-16,-1.,0.));
#116800=DIRECTION('ref_axis',(-1.,-1.22464679914735E-16,0.));
#116801=DIRECTION('center_axis',(0.,0.,1.));
#116802=DIRECTION('ref_axis',(1.,0.,0.));
#116803=DIRECTION('center_axis',(0.,0.,1.));
#116804=DIRECTION('ref_axis',(1.,0.,0.));
#116805=DIRECTION('center_axis',(0.,0.,1.));
#116806=DIRECTION('ref_axis',(1.,0.,0.));
#116807=DIRECTION('',(0.707106781186541,8.65956056235485E-17,-0.707106781186554));
#116808=DIRECTION('center_axis',(0.,0.,1.));
#116809=DIRECTION('ref_axis',(1.,0.,0.));
#116810=DIRECTION('center_axis',(0.,0.,1.));
#116811=DIRECTION('ref_axis',(1.,0.,0.));
#116812=DIRECTION('center_axis',(1.22464679914735E-16,-1.,0.));
#116813=DIRECTION('ref_axis',(-1.,-1.22464679914735E-16,0.));
#116814=DIRECTION('center_axis',(0.,0.,-1.));
#116815=DIRECTION('ref_axis',(-1.,0.,0.));
#116816=DIRECTION('center_axis',(0.,0.,1.));
#116817=DIRECTION('ref_axis',(1.,0.,0.));
#116818=DIRECTION('center_axis',(0.708643409675333,0.0227248148575671,-0.705200752065259));
#116819=DIRECTION('ref_axis',(0.704838421157334,0.0226031142521084,0.709007686338126));
#116820=DIRECTION('center_axis',(0.,0.,1.));
#116821=DIRECTION('ref_axis',(1.,0.,0.));
#116822=DIRECTION('center_axis',(0.705731441901385,0.068081063433995,-0.705200752065317));
#116823=DIRECTION('ref_axis',(0.701942068525029,0.067715826424425,0.709007686338069));
#116824=DIRECTION('center_axis',(0.,0.,1.));
#116825=DIRECTION('ref_axis',(1.,0.,0.));
#116826=DIRECTION('center_axis',(0.699919472253828,0.113157552317439,-0.705200752065289));
#116827=DIRECTION('ref_axis',(0.696161285367033,0.112550279740303,0.709007686338096));
#116828=DIRECTION('center_axis',(0.,0.,1.));
#116829=DIRECTION('ref_axis',(1.,0.,0.));
#116830=DIRECTION('center_axis',(0.691231383362495,0.15776905254617,-0.705200752065293));
#116831=DIRECTION('ref_axis',(0.687519826161253,0.156922239815477,0.709007686338092));
#116832=DIRECTION('center_axis',(0.,0.,1.));
#116833=DIRECTION('ref_axis',(1.,0.,0.));
#116834=DIRECTION('center_axis',(0.679702876448271,0.201732245896655,-0.705200752065281));
#116835=DIRECTION('ref_axis',(0.676053200517231,0.200649372747332,0.709007686338104));
#116836=DIRECTION('center_axis',(0.,0.,1.));
#116837=DIRECTION('ref_axis',(1.,0.,0.));
#116838=DIRECTION('center_axis',(0.665381324618886,0.244866478177282,-0.705200752065305));
#116839=DIRECTION('ref_axis',(0.661808527259506,0.243551994366965,0.709007686338081));
#116840=DIRECTION('center_axis',(0.,0.,1.));
#116841=DIRECTION('ref_axis',(1.,0.,0.));
#116842=DIRECTION('center_axis',(0.648325578202831,0.286994501575423,-0.705200752065282));
#116843=DIRECTION('ref_axis',(0.64484434080553,0.28545380860057,0.709007686338103));
#116844=DIRECTION('center_axis',(0.,0.,1.));
#116845=DIRECTION('ref_axis',(1.,0.,0.));
#116846=DIRECTION('center_axis',(0.628605722920504,0.327943203006452,-0.705200752065297));
#116847=DIRECTION('ref_axis',(0.625230350636733,0.326182631904548,0.709007686338089));
#116848=DIRECTION('center_axis',(0.,0.,1.));
#116849=DIRECTION('ref_axis',(1.,0.,0.));
#116850=DIRECTION('center_axis',(0.606302791887208,0.367544315472732,-0.705200752065295));
#116851=DIRECTION('ref_axis',(0.603047154845681,0.365571100808089,0.70900768633809));
#116852=DIRECTION('center_axis',(0.,0.,1.));
#116853=DIRECTION('ref_axis',(1.,0.,0.));
#116854=DIRECTION('center_axis',(0.581508432630507,0.40563510950871,-0.705200752065302));
#116855=DIRECTION('ref_axis',(0.578385908942004,0.403457359643929,0.709007686338083));
#116856=DIRECTION('center_axis',(0.,0.,1.));
#116857=DIRECTION('ref_axis',(1.,0.,0.));
#116858=DIRECTION('center_axis',(0.55432453049096,0.442059061871265,-0.705200752065307));
#116859=DIRECTION('ref_axis',(0.551347951275109,0.439685725647609,0.709007686338079));
#116860=DIRECTION('center_axis',(0.,0.,1.));
#116861=DIRECTION('ref_axis',(1.,0.,0.));
#116862=DIRECTION('center_axis',(0.524862789953404,0.47666649872725,-0.705200752065278));
#116863=DIRECTION('ref_axis',(0.522044386613039,0.474107328691827,0.709007686338108));
#116864=DIRECTION('center_axis',(0.,0.,1.));
#116865=DIRECTION('ref_axis',(1.,0.,0.));
#116866=DIRECTION('center_axis',(0.49324427562918,0.509315210695285,-0.705200752065299));
#116867=DIRECTION('ref_axis',(0.490595629587655,0.506580723027443,0.709007686338087));
#116868=DIRECTION('center_axis',(0.,0.,1.));
#116869=DIRECTION('ref_axis',(1.,0.,0.));
#116870=DIRECTION('center_axis',(0.459598914775843,0.53987103721482,-0.705200752065298));
#116871=DIRECTION('ref_axis',(0.457130909888052,0.536972468510662,0.709007686338087));
#116872=DIRECTION('center_axis',(0.,0.,1.));
#116873=DIRECTION('ref_axis',(1.,0.,0.));
#116874=DIRECTION('center_axis',(0.424064963398038,0.568208417840459,-0.705200752065299));
#116875=DIRECTION('ref_axis',(0.421787741225521,0.565157678940477,0.709007686338086));
#116876=DIRECTION('center_axis',(0.,0.,1.));
#116877=DIRECTION('ref_axis',(1.,0.,0.));
#116878=DIRECTION('center_axis',(0.386788438123989,0.594210908196879,-0.705200752065287));
#116879=DIRECTION('ref_axis',(0.384711356260997,0.591020535241645,0.709007686338099));
#116880=DIRECTION('center_axis',(0.,0.,1.));
#116881=DIRECTION('ref_axis',(1.,0.,0.));
#116882=DIRECTION('center_axis',(0.347922516191844,0.617771658473695,-0.705200752065251));
#116883=DIRECTION('ref_axis',(0.346054109813753,0.614454761389687,0.709007686338133));
#116884=DIRECTION('center_axis',(0.,0.,1.));
#116885=DIRECTION('ref_axis',(1.,0.,0.));
#116886=DIRECTION('center_axis',(0.307626906011472,0.638793852494177,-0.705200752065294));
#116887=DIRECTION('ref_axis',(0.305974852800091,0.635364061123597,0.709007686338091));
#116888=DIRECTION('center_axis',(0.,0.,1.));
#116889=DIRECTION('ref_axis',(1.,0.,0.));
#116890=DIRECTION('center_axis',(0.266067190888551,0.657191105553966,-0.705200752065277));
#116891=DIRECTION('ref_axis',(0.264638279485051,0.653662513644981,0.709007686338108));
#116892=DIRECTION('center_axis',(0.,0.,1.));
#116893=DIRECTION('ref_axis',(1.,0.,0.));
#116894=DIRECTION('center_axis',(0.223414148607074,0.672887819393937,-0.705200752065289));
#116895=DIRECTION('ref_axis',(0.22221425071527,0.669274926687495,0.709007686338096));
#116896=DIRECTION('center_axis',(0.,0.,1.));
#116897=DIRECTION('ref_axis',(1.,0.,0.));
#116898=DIRECTION('center_axis',(0.17984304966674,0.685819492850107,-0.705200752065246));
#116899=DIRECTION('ref_axis',(0.17887709592441,0.682137145497215,0.709007686338139));
#116900=DIRECTION('center_axis',(0.,0.,1.));
#116901=DIRECTION('ref_axis',(1.,0.,0.));
#116902=DIRECTION('center_axis',(0.135532937059139,0.695932986902273,-0.705200752065257));
#116903=DIRECTION('ref_axis',(0.134804896777401,0.692196316458192,0.709007686338127));
#116904=DIRECTION('center_axis',(0.,0.,1.));
#116905=DIRECTION('ref_axis',(1.,0.,0.));
#116906=DIRECTION('center_axis',(0.0906658905414403,0.703186743034099,-0.705200752065271));
#116907=DIRECTION('ref_axis',(0.0901787553937343,0.699411104279244,0.709007686338114));
#116908=DIRECTION('center_axis',(0.,0.,1.));
#116909=DIRECTION('ref_axis',(1.,0.,0.));
#116910=DIRECTION('center_axis',(0.0454262784316856,0.70755095400576,-0.705200752065244));
#116911=DIRECTION('ref_axis',(0.0451820501609615,0.703751861849536,0.709007686338141));
#116912=DIRECTION('center_axis',(0.,0.,1.));
#116913=DIRECTION('ref_axis',(1.,0.,0.));
#116914=DIRECTION('center_axis',(0.,0.709007686338145,-0.705200752065276));
#116915=DIRECTION('ref_axis',(-3.17807183472368E-7,0.70520075206524,0.709007686338109));
#116916=DIRECTION('center_axis',(0.,0.,1.));
#116917=DIRECTION('ref_axis',(1.,0.,0.));
#116918=DIRECTION('center_axis',(-0.0454262784316862,0.707550954005719,
-0.705200752065285));
#116919=DIRECTION('ref_axis',(-0.0451826844694947,0.703751821125619,0.7090076863381));
#116920=DIRECTION('center_axis',(0.,0.,1.));
#116921=DIRECTION('ref_axis',(1.,0.,0.));
#116922=DIRECTION('center_axis',(-0.0906658905414509,0.70318674303409,-0.705200752065278));
#116923=DIRECTION('ref_axis',(-0.0901793857895431,0.699411022998713,0.709007686338107));
#116924=DIRECTION('center_axis',(0.,0.,1.));
#116925=DIRECTION('ref_axis',(1.,0.,0.));
#116926=DIRECTION('center_axis',(-0.135532937059151,0.695932986902274,-0.705200752065254));
#116927=DIRECTION('ref_axis',(-0.134805520670624,0.692196194954994,0.709007686338131));
#116928=DIRECTION('center_axis',(0.,0.,1.));
#116929=DIRECTION('ref_axis',(1.,0.,0.));
#116930=DIRECTION('center_axis',(-0.179843049666727,0.685819492850053,-0.705200752065302));
#116931=DIRECTION('ref_axis',(-0.178877710751454,0.682136984270636,0.709007686338083));
#116932=DIRECTION('center_axis',(0.,0.,1.));
#116933=DIRECTION('ref_axis',(1.,0.,0.));
#116934=DIRECTION('center_axis',(-0.223414148607083,0.672887819393958,-0.705200752065266));
#116935=DIRECTION('ref_axis',(-0.222214853948597,0.669274726400206,0.709007686338119));
#116936=DIRECTION('center_axis',(0.,0.,1.));
#116937=DIRECTION('ref_axis',(1.,0.,0.));
#116938=DIRECTION('center_axis',(-0.266067190888595,0.657191105553951,-0.705200752065274));
#116939=DIRECTION('ref_axis',(-0.264638868646668,0.653662275119875,0.709007686338111));
#116940=DIRECTION('center_axis',(0.,0.,1.));
#116941=DIRECTION('ref_axis',(1.,0.,0.));
#116942=DIRECTION('center_axis',(-0.307626906011484,0.638793852494172,-0.705200752065293));
#116943=DIRECTION('ref_axis',(-0.305975425468794,0.635363785340884,0.709007686338092));
#116944=DIRECTION('center_axis',(0.,0.,1.));
#116945=DIRECTION('ref_axis',(1.,0.,0.));
#116946=DIRECTION('center_axis',(-0.347922516191818,0.61777165847369,-0.705200752065269));
#116947=DIRECTION('ref_axis',(-0.346054663636128,0.614454449482756,0.709007686338117));
#116948=DIRECTION('center_axis',(0.,0.,1.));
#116949=DIRECTION('ref_axis',(1.,0.,0.));
#116950=DIRECTION('center_axis',(-0.386788438124013,0.594210908196864,-0.705200752065286));
#116951=DIRECTION('ref_axis',(-0.384711888962196,0.59102018849159,0.709007686338099));
#116952=DIRECTION('center_axis',(0.,0.,1.));
#116953=DIRECTION('ref_axis',(1.,0.,0.));
#116954=DIRECTION('center_axis',(-0.424064963398083,0.568208417840489,-0.705200752065248));
#116955=DIRECTION('ref_axis',(-0.421788250615727,0.565157298772622,0.709007686338137));
#116956=DIRECTION('center_axis',(0.,0.,1.));
#116957=DIRECTION('ref_axis',(1.,0.,0.));
#116958=DIRECTION('center_axis',(-0.459598914775863,0.539871037214812,-0.705200752065291));
#116959=DIRECTION('ref_axis',(-0.457131393874339,0.53697205648712,0.709007686338094));
#116960=DIRECTION('center_axis',(0.,0.,1.));
#116961=DIRECTION('ref_axis',(1.,0.,0.));
#116962=DIRECTION('center_axis',(-0.493244275629213,0.50931521069529,-0.705200752065272));
#116963=DIRECTION('ref_axis',(-0.490596086180789,0.506580280841613,0.709007686338113));
#116964=DIRECTION('center_axis',(0.,0.,1.));
#116965=DIRECTION('ref_axis',(1.,0.,0.));
#116966=DIRECTION('center_axis',(-0.524862789953399,0.476666498727232,-0.705200752065294));
#116967=DIRECTION('ref_axis',(-0.522044813936732,0.474106858160974,0.709007686338091));
#116968=DIRECTION('center_axis',(0.,0.,1.));
#116969=DIRECTION('ref_axis',(1.,0.,0.));
#116970=DIRECTION('center_axis',(-0.554324530490975,0.442059061871271,-0.705200752065291));
#116971=DIRECTION('ref_axis',(-0.551348347574532,0.439685228703826,0.709007686338094));
#116972=DIRECTION('center_axis',(0.,0.,1.));
#116973=DIRECTION('ref_axis',(1.,0.,0.));
#116974=DIRECTION('center_axis',(-0.581508432630519,0.405635109508721,-0.705200752065286));
#116975=DIRECTION('ref_axis',(0.578386272587459,-0.403456838330795,-0.709007686338099));
#116976=DIRECTION('center_axis',(0.,0.,1.));
#116977=DIRECTION('ref_axis',(1.,0.,0.));
#116978=DIRECTION('center_axis',(-0.606302791887217,0.367544315472719,-0.705200752065294));
#116979=DIRECTION('ref_axis',(0.603047484343626,-0.365570557266762,-0.709007686338091));
#116980=DIRECTION('center_axis',(0.,0.,1.));
#116981=DIRECTION('ref_axis',(1.,0.,0.));
#116982=DIRECTION('center_axis',(-0.628605722920505,0.32794320300644,-0.705200752065301));
#116983=DIRECTION('ref_axis',(0.625230644632876,-0.326182068368994,-0.709007686338084));
#116984=DIRECTION('center_axis',(0.,0.,1.));
#116985=DIRECTION('ref_axis',(1.,0.,0.));
#116986=DIRECTION('center_axis',(-0.648325578202841,0.286994501575399,-0.705200752065283));
#116987=DIRECTION('ref_axis',(0.644844598091737,-0.28545322738655,-0.709007686338102));
#116988=DIRECTION('center_axis',(0.,0.,1.));
#116989=DIRECTION('ref_axis',(1.,0.,0.));
#116990=DIRECTION('center_axis',(-0.665381324618884,0.244866478177285,-0.705200752065305));
#116991=DIRECTION('ref_axis',(0.661808746778622,-0.243551397862613,-0.70900768633808));
#116992=DIRECTION('center_axis',(0.,0.,1.));
#116993=DIRECTION('ref_axis',(1.,0.,0.));
#116994=DIRECTION('center_axis',(-0.679702876448276,0.201732245896628,-0.705200752065284));
#116995=DIRECTION('ref_axis',(0.676053381367121,-0.200648763404049,-0.709007686338101));
#116996=DIRECTION('center_axis',(0.,0.,1.));
#116997=DIRECTION('ref_axis',(1.,0.,0.));
#116998=DIRECTION('center_axis',(-0.69123138336253,0.157769052546159,-0.705200752065261));
#116999=DIRECTION('ref_axis',(0.687519967598698,-0.1569216201374,-0.709007686338124));
#117000=DIRECTION('center_axis',(0.,0.,1.));
#117001=DIRECTION('ref_axis',(1.,0.,0.));
#117002=DIRECTION('center_axis',(-0.699919472253854,0.113157552317423,-0.705200752065265));
#117003=DIRECTION('ref_axis',(0.696161386810957,-0.112549652273613,-0.70900768633812));
#117004=DIRECTION('center_axis',(0.,0.,1.));
#117005=DIRECTION('ref_axis',(1.,0.,0.));
#117006=DIRECTION('center_axis',(-0.705731441901413,0.0680810634339954,
-0.705200752065289));
#117007=DIRECTION('ref_axis',(0.701942129558611,-0.0677151937472035,-0.709007686338097));
#117008=DIRECTION('center_axis',(0.,0.,1.));
#117009=DIRECTION('ref_axis',(1.,0.,0.));
#117010=DIRECTION('center_axis',(-0.708643409675306,0.0227248148575655,
-0.705200752065287));
#117011=DIRECTION('ref_axis',(0.704838441529815,-0.0226024789640054,-0.709007686338098));
#117012=DIRECTION('center_axis',(0.,0.,1.));
#117013=DIRECTION('ref_axis',(1.,0.,0.));
#117014=DIRECTION('',(-0.707106781186552,8.659560562355E-17,0.707106781186543));
#117015=DIRECTION('center_axis',(0.,0.,1.));
#117016=DIRECTION('ref_axis',(1.,0.,0.));
#117017=DIRECTION('center_axis',(0.,0.,1.));
#117018=DIRECTION('ref_axis',(1.,0.,0.));
#117019=DIRECTION('center_axis',(0.,0.,1.));
#117020=DIRECTION('ref_axis',(1.,0.,0.));
#117021=DIRECTION('center_axis',(-0.708643409675315,-0.0227248148575665,
-0.705200752065277));
#117022=DIRECTION('ref_axis',(0.70483842115735,0.0226031142522111,-0.709007686338108));
#117023=DIRECTION('center_axis',(0.,0.,1.));
#117024=DIRECTION('ref_axis',(1.,0.,0.));
#117025=DIRECTION('center_axis',(-0.705731441901445,-0.0680810634340008,
-0.705200752065256));
#117026=DIRECTION('ref_axis',(0.701942068524995,0.0677158264241434,-0.709007686338128));
#117027=DIRECTION('center_axis',(0.,0.,1.));
#117028=DIRECTION('ref_axis',(1.,0.,0.));
#117029=DIRECTION('center_axis',(-0.699919472253843,-0.113157552317429,
-0.705200752065276));
#117030=DIRECTION('ref_axis',(0.696161285367009,0.112550279740369,-0.709007686338109));
#117031=DIRECTION('center_axis',(0.,0.,1.));
#117032=DIRECTION('ref_axis',(1.,0.,0.));
#117033=DIRECTION('center_axis',(-0.691231383362506,-0.157769052546184,
-0.705200752065279));
#117034=DIRECTION('ref_axis',(0.687519826161262,0.156922239815375,-0.709007686338106));
#117035=DIRECTION('center_axis',(0.,0.,1.));
#117036=DIRECTION('ref_axis',(1.,0.,0.));
#117037=DIRECTION('center_axis',(-0.679702876448284,-0.20173224589665,-0.70520075206527));
#117038=DIRECTION('ref_axis',(0.676053200517185,0.200649372747448,-0.709007686338115));
#117039=DIRECTION('center_axis',(0.,0.,1.));
#117040=DIRECTION('ref_axis',(1.,0.,0.));
#117041=DIRECTION('center_axis',(-0.665381324618884,-0.244866478177317,
-0.705200752065294));
#117042=DIRECTION('ref_axis',(0.661808527259463,0.243551994367051,-0.709007686338091));
#117043=DIRECTION('center_axis',(0.,0.,1.));
#117044=DIRECTION('ref_axis',(1.,0.,0.));
#117045=DIRECTION('center_axis',(-0.648325578202812,-0.286994501575426,
-0.705200752065298));
#117046=DIRECTION('ref_axis',(0.644844340805595,0.285453808600464,-0.709007686338087));
#117047=DIRECTION('center_axis',(0.,0.,1.));
#117048=DIRECTION('ref_axis',(1.,0.,0.));
#117049=DIRECTION('center_axis',(-0.628605722920495,-0.327943203006455,
-0.705200752065303));
#117050=DIRECTION('ref_axis',(0.625230350636678,0.326182631904669,-0.709007686338082));
#117051=DIRECTION('center_axis',(0.,0.,1.));
#117052=DIRECTION('ref_axis',(1.,0.,0.));
#117053=DIRECTION('center_axis',(-0.606302791887218,-0.367544315472729,
-0.705200752065288));
#117054=DIRECTION('ref_axis',(0.603047154845577,0.365571100808246,-0.709007686338097));
#117055=DIRECTION('center_axis',(0.,0.,1.));
#117056=DIRECTION('ref_axis',(1.,0.,0.));
#117057=DIRECTION('center_axis',(-0.581508432630516,-0.405635109508724,
-0.705200752065287));
#117058=DIRECTION('ref_axis',(0.578385908942077,0.403457359643798,-0.709007686338099));
#117059=DIRECTION('center_axis',(0.,0.,1.));
#117060=DIRECTION('ref_axis',(1.,0.,0.));
#117061=DIRECTION('center_axis',(-0.55432453049095,-0.442059061871284,-0.705200752065303));
#117062=DIRECTION('ref_axis',(0.551347951275536,0.439685725647067,-0.709007686338082));
#117063=DIRECTION('center_axis',(0.,0.,1.));
#117064=DIRECTION('ref_axis',(1.,0.,0.));
#117065=DIRECTION('center_axis',(-0.524862789953383,-0.476666498727248,
-0.705200752065295));
#117066=DIRECTION('ref_axis',(0.522044386612722,0.474107328692201,-0.709007686338091));
#117067=DIRECTION('center_axis',(0.,0.,1.));
#117068=DIRECTION('ref_axis',(1.,0.,0.));
#117069=DIRECTION('center_axis',(-0.49324427562918,-0.50931521069529,-0.705200752065295));
#117070=DIRECTION('ref_axis',(0.490595629587509,0.506580723027578,-0.70900768633809));
#117071=DIRECTION('center_axis',(0.,0.,1.));
#117072=DIRECTION('ref_axis',(1.,0.,0.));
#117073=DIRECTION('center_axis',(-0.459598914775862,-0.539871037214824,
-0.705200752065283));
#117074=DIRECTION('ref_axis',(0.457130909888059,0.536972468510637,-0.709007686338102));
#117075=DIRECTION('center_axis',(0.,0.,1.));
#117076=DIRECTION('ref_axis',(1.,0.,0.));
#117077=DIRECTION('center_axis',(-0.424064963398045,-0.568208417840474,
-0.705200752065282));
#117078=DIRECTION('ref_axis',(0.421787741225687,0.565157678940332,-0.709007686338103));
#117079=DIRECTION('center_axis',(0.,0.,1.));
#117080=DIRECTION('ref_axis',(1.,0.,0.));
#117081=DIRECTION('center_axis',(-0.386788438123993,-0.594210908196879,
-0.705200752065284));
#117082=DIRECTION('ref_axis',(0.384711356261092,0.59102053524158,-0.709007686338101));
#117083=DIRECTION('center_axis',(0.,0.,1.));
#117084=DIRECTION('ref_axis',(1.,0.,0.));
#117085=DIRECTION('center_axis',(-0.347922516191811,-0.617771658473671,
-0.705200752065289));
#117086=DIRECTION('ref_axis',(0.346054109813453,0.614454761389899,-0.709007686338097));
#117087=DIRECTION('center_axis',(0.,0.,1.));
#117088=DIRECTION('ref_axis',(1.,0.,0.));
#117089=DIRECTION('center_axis',(-0.30762690601146,-0.638793852494167,-0.705200752065309));
#117090=DIRECTION('ref_axis',(0.305974852800018,0.635364061123648,-0.709007686338077));
#117091=DIRECTION('center_axis',(0.,0.,1.));
#117092=DIRECTION('ref_axis',(1.,0.,0.));
#117093=DIRECTION('center_axis',(-0.266067190888571,-0.657191105553954,
-0.70520075206528));
#117094=DIRECTION('ref_axis',(0.264638279485338,0.653662513644868,-0.709007686338105));
#117095=DIRECTION('center_axis',(0.,0.,1.));
#117096=DIRECTION('ref_axis',(1.,0.,0.));
#117097=DIRECTION('center_axis',(-0.223414148607049,-0.672887819393935,
-0.705200752065299));
#117098=DIRECTION('ref_axis',(0.22221425071552,0.669274926687422,-0.709007686338086));
#117099=DIRECTION('center_axis',(0.,0.,1.));
#117100=DIRECTION('ref_axis',(1.,0.,0.));
#117101=DIRECTION('center_axis',(-0.179843049666729,-0.685819492850059,
-0.705200752065295));
#117102=DIRECTION('ref_axis',(0.178877095924088,0.68213714549735,-0.70900768633809));
#117103=DIRECTION('center_axis',(0.,0.,1.));
#117104=DIRECTION('ref_axis',(1.,0.,0.));
#117105=DIRECTION('center_axis',(-0.135532937059131,-0.695932986902283,
-0.705200752065249));
#117106=DIRECTION('ref_axis',(0.134804896777495,0.692196316458165,-0.709007686338136));
#117107=DIRECTION('center_axis',(0.,0.,1.));
#117108=DIRECTION('ref_axis',(1.,0.,0.));
#117109=DIRECTION('center_axis',(-0.0906658905414127,-0.703186743034061,
-0.705200752065312));
#117110=DIRECTION('ref_axis',(0.0901787553939383,0.699411104279259,-0.709007686338073));
#117111=DIRECTION('center_axis',(0.,0.,1.));
#117112=DIRECTION('ref_axis',(1.,0.,0.));
#117113=DIRECTION('center_axis',(-0.0454262784316981,-0.707550954005724,
-0.705200752065279));
#117114=DIRECTION('ref_axis',(0.045182050161025,0.703751861849567,-0.709007686338106));
#117115=DIRECTION('center_axis',(0.,0.,1.));
#117116=DIRECTION('ref_axis',(1.,0.,0.));
#117117=DIRECTION('center_axis',(0.,-0.709007686338126,-0.705200752065295));
#117118=DIRECTION('ref_axis',(-3.17807545014534E-7,0.705200752065259,-0.70900768633809));
#117119=DIRECTION('center_axis',(0.,0.,1.));
#117120=DIRECTION('ref_axis',(1.,0.,0.));
#117121=DIRECTION('center_axis',(0.0454262784316969,-0.707550954005706,
-0.705200752065298));
#117122=DIRECTION('ref_axis',(-0.0451826844697783,0.703751821125613,-0.709007686338088));
#117123=DIRECTION('center_axis',(0.,0.,1.));
#117124=DIRECTION('ref_axis',(1.,0.,0.));
#117125=DIRECTION('center_axis',(0.0906658905414092,-0.703186743034074,
-0.7052007520653));
#117126=DIRECTION('ref_axis',(-0.0901793857898937,0.699411022998689,-0.709007686338085));
#117127=DIRECTION('center_axis',(0.,0.,1.));
#117128=DIRECTION('ref_axis',(1.,0.,0.));
#117129=DIRECTION('center_axis',(0.135532937059137,-0.69593298690225,-0.70520075206528));
#117130=DIRECTION('ref_axis',(-0.134805520670637,0.692196194955019,-0.709007686338105));
#117131=DIRECTION('center_axis',(0.,0.,1.));
#117132=DIRECTION('ref_axis',(1.,0.,0.));
#117133=DIRECTION('center_axis',(0.179843049666742,-0.685819492850065,-0.705200752065287));
#117134=DIRECTION('ref_axis',(-0.17887771075135,0.682136984270647,-0.709007686338099));
#117135=DIRECTION('center_axis',(0.,0.,1.));
#117136=DIRECTION('ref_axis',(1.,0.,0.));
#117137=DIRECTION('center_axis',(0.22341414860707,-0.672887819393955,-0.705200752065273));
#117138=DIRECTION('ref_axis',(-0.222214853948978,0.669274726400087,-0.709007686338112));
#117139=DIRECTION('center_axis',(0.,0.,1.));
#117140=DIRECTION('ref_axis',(1.,0.,0.));
#117141=DIRECTION('center_axis',(0.266067190888564,-0.657191105553934,-0.705200752065302));
#117142=DIRECTION('ref_axis',(-0.264638868646705,0.653662275119889,-0.709007686338084));
#117143=DIRECTION('center_axis',(0.,0.,1.));
#117144=DIRECTION('ref_axis',(1.,0.,0.));
#117145=DIRECTION('center_axis',(0.307626906011474,-0.638793852494176,-0.705200752065295));
#117146=DIRECTION('ref_axis',(-0.305975425469023,0.635363785340775,-0.709007686338091));
#117147=DIRECTION('center_axis',(0.,0.,1.));
#117148=DIRECTION('ref_axis',(1.,0.,0.));
#117149=DIRECTION('center_axis',(0.347922516191819,-0.617771658473665,-0.705200752065291));
#117150=DIRECTION('ref_axis',(-0.346054663636103,0.614454449482796,-0.709007686338095));
#117151=DIRECTION('center_axis',(0.,0.,1.));
#117152=DIRECTION('ref_axis',(1.,0.,0.));
#117153=DIRECTION('center_axis',(0.386788438123997,-0.594210908196884,-0.705200752065278));
#117154=DIRECTION('ref_axis',(-0.384711888962051,0.591020188491674,-0.709007686338108));
#117155=DIRECTION('center_axis',(0.,0.,1.));
#117156=DIRECTION('ref_axis',(1.,0.,0.));
#117157=DIRECTION('center_axis',(0.424064963398043,-0.568208417840467,-0.705200752065289));
#117158=DIRECTION('ref_axis',(-0.421788250615591,0.565157298772775,-0.709007686338096));
#117159=DIRECTION('center_axis',(0.,0.,1.));
#117160=DIRECTION('ref_axis',(1.,0.,0.));
#117161=DIRECTION('center_axis',(0.45959891477585,-0.53987103721481,-0.705200752065301));
#117162=DIRECTION('ref_axis',(-0.457131393874177,0.536972056487271,-0.709007686338084));
#117163=DIRECTION('center_axis',(0.,0.,1.));
#117164=DIRECTION('ref_axis',(1.,0.,0.));
#117165=DIRECTION('center_axis',(0.493244275629187,-0.509315210695281,-0.705200752065297));
#117166=DIRECTION('ref_axis',(-0.490596086180762,0.506580280841674,-0.709007686338088));
#117167=DIRECTION('center_axis',(0.,0.,1.));
#117168=DIRECTION('ref_axis',(1.,0.,0.));
#117169=DIRECTION('center_axis',(0.524862789953382,-0.47666649872723,-0.705200752065308));
#117170=DIRECTION('ref_axis',(-0.522044813937081,0.47410685816061,-0.709007686338077));
#117171=DIRECTION('center_axis',(0.,0.,1.));
#117172=DIRECTION('ref_axis',(1.,0.,0.));
#117173=DIRECTION('center_axis',(0.554324530490965,-0.442059061871282,-0.705200752065292));
#117174=DIRECTION('ref_axis',(-0.55134834757427,0.439685228704155,-0.709007686338094));
#117175=DIRECTION('center_axis',(0.,0.,1.));
#117176=DIRECTION('ref_axis',(1.,0.,0.));
#117177=DIRECTION('center_axis',(0.581508432630509,-0.405635109508715,-0.705200752065298));
#117178=DIRECTION('ref_axis',(0.578386272587666,-0.40345683833052,0.709007686338087));
#117179=DIRECTION('center_axis',(0.,0.,1.));
#117180=DIRECTION('ref_axis',(1.,0.,0.));
#117181=DIRECTION('center_axis',(0.606302791887227,-0.367544315472725,-0.705200752065283));
#117182=DIRECTION('ref_axis',(0.603047484343378,-0.36557055726715,0.709007686338102));
#117183=DIRECTION('center_axis',(0.,0.,1.));
#117184=DIRECTION('ref_axis',(1.,0.,0.));
#117185=DIRECTION('center_axis',(0.628605722920507,-0.327943203006441,-0.705200752065299));
#117186=DIRECTION('ref_axis',(0.625230644632778,-0.326182068369178,0.709007686338086));
#117187=DIRECTION('center_axis',(0.,0.,1.));
#117188=DIRECTION('ref_axis',(1.,0.,0.));
#117189=DIRECTION('center_axis',(0.648325578202825,-0.286994501575435,-0.705200752065283));
#117190=DIRECTION('ref_axis',(0.644844598091824,-0.285453227386353,0.709007686338102));
#117191=DIRECTION('center_axis',(0.,0.,1.));
#117192=DIRECTION('ref_axis',(1.,0.,0.));
#117193=DIRECTION('center_axis',(0.665381324618895,-0.24486647817731,-0.705200752065287));
#117194=DIRECTION('ref_axis',(0.661808746778473,-0.243551397862965,0.709007686338098));
#117195=DIRECTION('center_axis',(0.,0.,1.));
#117196=DIRECTION('ref_axis',(1.,0.,0.));
#117197=DIRECTION('center_axis',(0.679702876448274,-0.201732245896636,-0.705200752065284));
#117198=DIRECTION('ref_axis',(0.6760533813671,-0.200648763404121,0.709007686338102));
#117199=DIRECTION('center_axis',(0.,0.,1.));
#117200=DIRECTION('ref_axis',(1.,0.,0.));
#117201=DIRECTION('center_axis',(0.69123138336251,-0.157769052546173,-0.705200752065278));
#117202=DIRECTION('ref_axis',(0.687519967598833,-0.15692162013688,0.709007686338107));
#117203=DIRECTION('center_axis',(0.,0.,1.));
#117204=DIRECTION('ref_axis',(1.,0.,0.));
#117205=DIRECTION('center_axis',(0.699919472253825,-0.113157552317415,-0.705200752065296));
#117206=DIRECTION('ref_axis',(0.696161386811017,-0.112549652273433,0.709007686338089));
#117207=DIRECTION('center_axis',(0.,0.,1.));
#117208=DIRECTION('ref_axis',(1.,0.,0.));
#117209=DIRECTION('center_axis',(0.705731441901455,-0.0680810634339902,
-0.705200752065247));
#117210=DIRECTION('ref_axis',(0.701942129558587,-0.0677151937470296,0.709007686338137));
#117211=DIRECTION('center_axis',(0.,0.,1.));
#117212=DIRECTION('ref_axis',(1.,0.,0.));
#117213=DIRECTION('center_axis',(0.708643409675344,-0.0227248148575675,
-0.705200752065248));
#117214=DIRECTION('ref_axis',(0.704838441529764,-0.0226024789643774,0.709007686338137));
#117215=DIRECTION('center_axis',(0.,0.,1.));
#117216=DIRECTION('ref_axis',(1.,0.,0.));
#117217=DIRECTION('center_axis',(0.,0.,1.));
#117218=DIRECTION('ref_axis',(1.,0.,0.));
#117219=DIRECTION('center_axis',(1.22464679914735E-16,-1.,0.));
#117220=DIRECTION('ref_axis',(-1.,-1.22464679914735E-16,0.));
#117221=DIRECTION('center_axis',(0.,0.,1.));
#117222=DIRECTION('ref_axis',(1.,0.,0.));
#117223=DIRECTION('center_axis',(0.,0.,1.));
#117224=DIRECTION('ref_axis',(1.,0.,0.));
#117225=DIRECTION('',(0.,0.,-1.));
#117226=DIRECTION('center_axis',(0.999875322485695,-0.015751302085643,0.00111174040829824));
#117227=DIRECTION('ref_axis',(0.00831475628134585,0.465340995336109,-0.885092437481861));
#117228=DIRECTION('center_axis',(0.,0.,-1.));
#117229=DIRECTION('ref_axis',(0.0320515775716446,0.999486216200688,0.));
#117230=DIRECTION('center_axis',(0.998830238638869,-0.0483416538578448,
0.00111305117022865));
#117231=DIRECTION('ref_axis',(-0.0215571677327655,-0.465780464937779,-0.884637692505631));
#117232=DIRECTION('',(0.,0.,1.));
#117233=DIRECTION('center_axis',(0.,0.,1.));
#117234=DIRECTION('ref_axis',(1.,0.,0.));
#117235=DIRECTION('',(0.,0.,-1.));
#117236=DIRECTION('center_axis',(0.996811782009738,-0.0797811712112251,
0.00111174040838231));
#117237=DIRECTION('ref_axis',(0.0381121726600761,0.463852174088461,-0.8850924374824));
#117238=DIRECTION('center_axis',(0.,0.,-1.));
#117239=DIRECTION('ref_axis',(0.0960230259076709,0.995379112949199,0.));
#117240=DIRECTION('center_axis',(0.993680774392475,-0.112237603858347,0.00111305117023333));
#117241=DIRECTION('ref_axis',(-0.0513555330708394,-0.463442296538108,-0.884637692506087));
#117242=DIRECTION('',(0.,0.,1.));
#117243=DIRECTION('center_axis',(0.,0.,1.));
#117244=DIRECTION('ref_axis',(1.,0.,0.));
#117245=DIRECTION('',(0.,0.,-1.));
#117246=DIRECTION('center_axis',(0.989652128106051,-0.143483202391184,0.00111174040840064));
#117247=DIRECTION('ref_axis',(0.0677529779465081,0.460457284764545,-0.88509243748133));
#117248=DIRECTION('center_axis',(0.,0.,-1.));
#117249=DIRECTION('ref_axis',(0.159599895033369,0.987181783414452,0.));
#117250=DIRECTION('center_axis',(0.984448062700241,-0.175672345469724,0.00111305117024819));
#117251=DIRECTION('ref_axis',(-0.0809428675080738,-0.459199744336065,-0.884637692505391));
#117252=DIRECTION('',(0.,0.,1.));
#117253=DIRECTION('center_axis',(0.,0.,1.));
#117254=DIRECTION('ref_axis',(1.,0.,0.));
#117255=DIRECTION('',(0.,0.,-1.));
#117256=DIRECTION('center_axis',(0.978425781328247,-0.206595630315535,0.00111174040841298));
#117257=DIRECTION('ref_axis',(0.0971153717128268,0.455170277684735,-0.885092437482933));
#117258=DIRECTION('center_axis',(0.,0.,-1.));
#117259=DIRECTION('ref_axis',(0.222520933956304,0.974927912181826,0.));
#117260=DIRECTION('center_axis',(0.971170042754934,-0.238385211731921,0.00111305117026388));
#117261=DIRECTION('ref_axis',(-0.110197590339834,-0.453070241883085,-0.884637692506541));
#117262=DIRECTION('',(0.,0.,1.));
#117263=DIRECTION('center_axis',(0.,0.,1.));
#117264=DIRECTION('ref_axis',(1.,0.,0.));
#117265=DIRECTION('',(0.,0.,-1.));
#117266=DIRECTION('center_axis',(0.963178873143288,-0.26885911248029,0.00111174040845783));
#117267=DIRECTION('ref_axis',(0.126078697585652,0.448012878301757,-0.885092437483724));
#117268=DIRECTION('center_axis',(0.,0.,-1.));
#117269=DIRECTION('ref_axis',(0.284527586631023,0.958667853036663,0.));
#117270=DIRECTION('center_axis',(0.953901276788614,-0.300118502025689,0.00111305117024521));
#117271=DIRECTION('ref_axis',(-0.138999487636299,-0.445078976625978,-0.884637692506044));
#117272=DIRECTION('',(0.,0.,1.));
#117273=DIRECTION('center_axis',(0.,0.,1.));
#117274=DIRECTION('ref_axis',(1.,0.,0.));
#117275=DIRECTION('',(0.,0.,-1.));
#117276=DIRECTION('center_axis',(0.943974056367375,-0.330017794881712,0.00111174040846252));
#117277=DIRECTION('ref_axis',(0.154523939046571,0.439014497904912,-0.885092437483696));
#117278=DIRECTION('center_axis',(0.,0.,-1.));
#117279=DIRECTION('ref_axis',(0.345365054421298,0.938468422049764,0.));
#117280=DIRECTION('center_axis',(0.932712725864775,-0.360618541019444,0.00111305117022834));
#117281=DIRECTION('ref_axis',(-0.16723020622334,-0.435258786385882,-0.884637692504897));
#117282=DIRECTION('',(0.,0.,1.));
#117283=DIRECTION('center_axis',(0.,0.,1.));
#117284=DIRECTION('ref_axis',(1.,0.,0.));
#117285=DIRECTION('',(0.,0.,-1.));
#117286=DIRECTION('center_axis',(0.920890247712054,-0.389820363375359,0.00111174040842101));
#117287=DIRECTION('ref_axis',(0.182334208497475,0.428212112769879,-0.885092437482524));
#117288=DIRECTION('center_axis',(0.,0.,-1.));
#117289=DIRECTION('ref_axis',(0.404783343122385,0.914412623015816,0.));
#117290=DIRECTION('center_axis',(0.907691458284136,-0.419636721075635,0.00111305117023417));
#117291=DIRECTION('ref_axis',(-0.194773740020739,-0.423650024426041,-0.884637692505892));
#117292=DIRECTION('',(0.,0.,1.));
#117293=DIRECTION('center_axis',(0.,0.,1.));
#117294=DIRECTION('ref_axis',(1.,0.,0.));
#117295=DIRECTION('',(0.,0.,-1.));
#117296=DIRECTION('center_axis',(0.894022303498553,-0.448021076379678,0.0011117404084274));
#117297=DIRECTION('ref_axis',(0.209395227573944,0.415650112209241,-0.885092437483059));
#117298=DIRECTION('center_axis',(0.,0.,-1.));
#117299=DIRECTION('ref_axis',(0.462538290240827,0.886599306373005,0.));
#117300=DIRECTION('center_axis',(0.878940291802186,-0.476930523833169,0.00111305117021906));
#117301=DIRECTION('ref_axis',(-0.221516906742537,-0.410300393645422,-0.884637692505599));
#117302=DIRECTION('',(0.,0.,1.));
#117303=DIRECTION('center_axis',(0.,0.,1.));
#117304=DIRECTION('ref_axis',(1.,0.,0.));
#117305=DIRECTION('',(0.,0.,-1.));
#117306=DIRECTION('center_axis',(0.863480629872782,-0.504380774680963,0.00111174040840051));
#117307=DIRECTION('ref_axis',(0.235595796746304,0.401380116183086,-0.885092437482282));
#117308=DIRECTION('center_axis',(0.,0.,-1.));
#117309=DIRECTION('ref_axis',(0.518392568310517,0.855142763005351,0.));
#117310=DIRECTION('center_axis',(0.846577371129118,-0.532264516766997,0.00111305117023412));
#117311=DIRECTION('ref_axis',(-0.247349812978024,-0.395264750536038,-0.884637692506611));
#117312=DIRECTION('',(0.,0.,1.));
#117313=DIRECTION('center_axis',(0.,0.,1.));
#117314=DIRECTION('ref_axis',(1.,0.,0.));
#117315=DIRECTION('',(0.,0.,-1.));
#117316=DIRECTION('center_axis',(0.829390729122881,-0.558667864189699,0.00111174040836604));
#117317=DIRECTION('ref_axis',(0.260828252253777,0.385460763162129,-0.885092437482498));
#117318=DIRECTION('center_axis',(0.,0.,-1.));
#117319=DIRECTION('ref_axis',(0.572116660122162,0.820172254596961,0.));
#117320=DIRECTION('center_axis',(0.810735682447807,-0.585411320631042,0.00111305117023414));
#117321=DIRECTION('ref_axis',(-0.27216630577768,-0.378604879785937,-0.884637692505585));
#117322=DIRECTION('',(0.,0.,1.));
#117323=DIRECTION('center_axis',(0.,0.,1.));
#117324=DIRECTION('ref_axis',(1.,0.,0.));
#117325=DIRECTION('',(0.,0.,-1.));
#117326=DIRECTION('center_axis',(0.791892683963227,-0.610659267610654,0.00111174040838973));
#117327=DIRECTION('ref_axis',(0.284988908526042,0.367957469185241,-0.885092437482056));
#117328=DIRECTION('center_axis',(0.,0.,-1.));
#117329=DIRECTION('ref_axis',(0.623489801858726,0.781831482468036,0.));
#117330=DIRECTION('center_axis',(0.77156250694505,-0.636152543808293,0.00111305117021684));
#117331=DIRECTION('ref_axis',(-0.295864408844889,-0.360389240370828,-0.884637692506826));
#117332=DIRECTION('',(0.,0.,1.));
#117333=DIRECTION('center_axis',(0.,0.,1.));
#117334=DIRECTION('ref_axis',(1.,0.,0.));
#117335=DIRECTION('',(0.,0.,-1.));
#117336=DIRECTION('center_axis',(0.751140581904703,-0.660141341115014,0.00111174040841524));
#117337=DIRECTION('ref_axis',(0.307978484242966,0.34894215904034,-0.885092437481912));
#117338=DIRECTION('center_axis',(0.,0.,-1.));
#117339=DIRECTION('ref_axis',(0.67230089026131,0.740277997075322,0.));
#117340=DIRECTION('center_axis',(0.729218815601603,-0.684279679728756,0.00111305117020348));
#117341=DIRECTION('ref_axis',(-0.318346741594962,-0.340692684265839,-0.884637692506716));
#117342=DIRECTION('',(0.,0.,1.));
#117343=DIRECTION('center_axis',(0.,0.,1.));
#117344=DIRECTION('ref_axis',(1.,0.,0.));
#117345=DIRECTION('',(0.,0.,-1.));
#117346=DIRECTION('center_axis',(0.707301882076007,-0.706910752248827,0.00111174040839121));
#117347=DIRECTION('ref_axis',(0.329702510308574,0.32849297071774,-0.885092437480549));
#117348=DIRECTION('center_axis',(0.,0.,-1.));
#117349=DIRECTION('ref_axis',(0.718349350097721,0.695682550603493,0.));
#117350=DIRECTION('center_axis',(0.68387860772793,-0.729594963667651,0.00111305117020451));
#117351=DIRECTION('ref_axis',(-0.339520919298581,-0.319596148842784,-0.88463769250666));
#117352=DIRECTION('',(0.,0.,1.));
#117353=DIRECTION('center_axis',(0.,0.,1.));
#117354=DIRECTION('ref_axis',(1.,0.,0.));
#117355=DIRECTION('',(0.,0.,-1.));
#117356=DIRECTION('center_axis',(0.66055672709807,-0.750775315469781,0.00111174040841501));
#117357=DIRECTION('ref_axis',(0.350071718032401,0.306693934311185,-0.885092437483549));
#117358=DIRECTION('center_axis',(0.,0.,-1.));
#117359=DIRECTION('ref_axis',(0.761445958369129,0.648228395307795,0.));
#117360=DIRECTION('center_axis',(0.635728195963613,-0.771912185403199,0.00111305117021925));
#117361=DIRECTION('ref_axis',(-0.359299932720418,-0.29718632429314,-0.884637692504811));
#117362=DIRECTION('',(0.,0.,1.));
#117363=DIRECTION('center_axis',(0.,0.,1.));
#117364=DIRECTION('ref_axis',(1.,0.,0.));
#117365=DIRECTION('',(0.,0.,-1.));
#117366=DIRECTION('center_axis',(0.61109720283957,-0.791554781878625,0.00111174040836773));
#117367=DIRECTION('ref_axis',(0.369002405982045,0.283634626748089,-0.885092437482625));
#117368=DIRECTION('center_axis',(0.,0.,-1.));
#117369=DIRECTION('ref_axis',(0.801413621867952,0.598110530491223,0.));
#117370=DIRECTION('center_axis',(0.584965440678803,-0.811057454394291,0.00111305117022841));
#117371=DIRECTION('ref_axis',(-0.377602505644605,-0.273555297386895,-0.884637692506081));
#117372=DIRECTION('',(0.,0.,1.));
#117373=DIRECTION('center_axis',(0.,0.,1.));
#117374=DIRECTION('ref_axis',(1.,0.,0.));
#117375=DIRECTION('',(0.,0.,-1.));
#117376=DIRECTION('center_axis',(0.559126549094596,-0.829081579900816,0.00111174040838601));
#117377=DIRECTION('ref_axis',(0.386416783895308,0.259409803664243,-0.885092437481468));
#117378=DIRECTION('center_axis',(0.,0.,-1.));
#117379=DIRECTION('ref_axis',(0.838088104891836,0.545534901210556,0.));
#117380=DIRECTION('center_axis',(0.531798936923567,-0.846869914333988,0.00111305117024416));
#117381=DIRECTION('ref_axis',(-0.39435342887895,-0.24880017308748,-0.884637692506404));
#117382=DIRECTION('',(0.,0.,1.));
#117383=DIRECTION('center_axis',(0.,0.,1.));
#117384=DIRECTION('ref_axis',(1.,0.,0.));
#117385=DIRECTION('',(0.,0.,-1.));
#117386=DIRECTION('center_axis',(0.504858324427174,-0.86320150387372,0.00111174040834681));
#117387=DIRECTION('ref_axis',(0.402243292355672,0.234119010052661,-0.885092437481437));
#117388=DIRECTION('center_axis',(0.,0.,-1.));
#117389=DIRECTION('ref_axis',(0.871318704123385,0.490717552003945,0.));
#117390=DIRECTION('center_axis',(0.476447157265946,-0.879202404142693,0.00111305117023455));
#117391=DIRECTION('ref_axis',(-0.409483869284568,-0.223022675508913,-0.884637692507269));
#117392=DIRECTION('',(0.,0.,1.));
#117393=DIRECTION('center_axis',(0.,0.,1.));
#117394=DIRECTION('ref_axis',(1.,0.,0.));
#117395=DIRECTION('',(0.,0.,-1.));
#117396=DIRECTION('center_axis',(0.448515528612856,-0.893774347711096,0.00111174040839922));
#117397=DIRECTION('ref_axis',(0.416416896849112,0.20786617121142,-0.885092437480098));
#117398=DIRECTION('center_axis',(0.,0.,-1.));
#117399=DIRECTION('ref_axis',(0.900968867902415,0.433883739117566,0.));
#117400=DIRECTION('center_axis',(0.419137554041588,-0.907922062684417,0.00111305117024988));
#117401=DIRECTION('ref_axis',(-0.422931652641499,-0.196328729920701,-0.884637692505613));
#117402=DIRECTION('',(0.,0.,1.));
#117403=DIRECTION('center_axis',(0.,0.,1.));
#117404=DIRECTION('ref_axis',(1.,0.,0.));
#117405=DIRECTION('',(0.,0.,-1.));
#117406=DIRECTION('center_axis',(0.390329686285115,-0.920674481039758,0.00111174040847326));
#117407=DIRECTION('ref_axis',(0.42887935498825,0.1807591656834,-0.885092437481139));
#117408=DIRECTION('center_axis',(0.,0.,-1.));
#117409=DIRECTION('ref_axis',(0.926916757346019,0.375267004879382,0.));
#117410=DIRECTION('center_axis',(0.360105624702917,-0.932910874721918,0.00111305117025848));
#117411=DIRECTION('ref_axis',(-0.434641519116407,-0.168828027467345,-0.88463769250562));
#117412=DIRECTION('',(0.,0.,1.));
#117413=DIRECTION('center_axis',(0.,0.,1.));
#117414=DIRECTION('ref_axis',(1.,0.,0.));
#117415=DIRECTION('',(0.,0.,-1.));
#117416=DIRECTION('center_axis',(0.330539895551113,-0.943791365441708,0.00111174040842785));
#117417=DIRECTION('ref_axis',(0.439579455860902,0.152909381970445,-0.885092437483481));
#117418=DIRECTION('center_axis',(0.,0.,-1.));
#117419=DIRECTION('ref_axis',(0.949055747010666,0.315108218023628,0.));
#117420=DIRECTION('center_axis',(0.29959394410987,-0.95406615586645,0.00111305117019356));
#117421=DIRECTION('ref_axis',(-0.444565350357212,-0.140633574434986,-0.884637692506604));
#117422=DIRECTION('',(0.,0.,1.));
#117423=DIRECTION('center_axis',(0.,0.,1.));
#117424=DIRECTION('ref_axis',(1.,0.,0.));
#117425=DIRECTION('',(0.,0.,-1.));
#117426=DIRECTION('center_axis',(0.269391845485697,-0.963030008680454,0.00111174040839746));
#117427=DIRECTION('ref_axis',(0.448473230463594,0.124431260809614,-0.885092437483723));
#117428=DIRECTION('center_axis',(0.,0.,-1.));
#117429=DIRECTION('ref_axis',(0.967294863039028,0.253654583909515,0.));
#117430=DIRECTION('center_axis',(0.237851167737837,-0.971300974529955,0.00111305117021558));
#117431=DIRECTION('ref_axis',(-0.452662367216689,-0.111861227880374,-0.884637692506304));
#117432=DIRECTION('',(0.,0.,1.));
#117433=DIRECTION('center_axis',(0.,0.,1.));
#117434=DIRECTION('ref_axis',(1.,0.,0.));
#117435=DIRECTION('',(0.,0.,-1.));
#117436=DIRECTION('center_axis',(0.207136806542801,-0.978311355044249,0.00111174040839084));
#117437=DIRECTION('ref_axis',(0.455524132365643,0.0954418249078427,-0.885092437483673));
#117438=DIRECTION('center_axis',(0.,0.,-1.));
#117439=DIRECTION('ref_axis',(0.981559156991064,0.19115862870138,0.));
#117440=DIRECTION('center_axis',(0.175131009898625,-0.984544509145717,0.00111305117022153));
#117441=DIRECTION('ref_axis',(-0.458899297309475,-0.0826292195454268,-0.884637692508173));
#117442=DIRECTION('',(0.,0.,1.));
#117443=DIRECTION('center_axis',(0.,0.,1.));
#117444=DIRECTION('ref_axis',(1.,0.,0.));
#117445=DIRECTION('',(0.,0.,-1.));
#117446=DIRECTION('center_axis',(0.144030598031156,-0.989572610203037,0.00111174040831266));
#117447=DIRECTION('ref_axis',(0.460703187901393,0.0660601980758584,-0.885092437481912));
#117448=DIRECTION('center_axis',(0.,0.,-1.));
#117449=DIRECTION('ref_axis',(0.991790013823245,0.127877161684513,0.));
#117450=DIRECTION('center_axis',(0.111691201174308,-0.993742339189255,0.00111305117022928));
#117451=DIRECTION('ref_axis',(-0.463250511766096,-0.0530576700250649,-0.884637692504655));
#117452=DIRECTION('',(0.,0.,1.));
#117453=DIRECTION('center_axis',(0.,0.,1.));
#117454=DIRECTION('ref_axis',(1.,0.,0.));
#117455=DIRECTION('',(0.,0.,-1.));
#117456=DIRECTION('center_axis',(0.0803325368976722,-0.996767499243855,
0.00111174040833762));
#117457=DIRECTION('ref_axis',(0.463989115216096,0.0364071157194459,-0.885092437480953));
#117458=DIRECTION('center_axis',(0.,0.,-1.));
#117459=DIRECTION('ref_axis',(0.997945392750336,0.0640702199807201,0.));
#117460=DIRECTION('center_axis',(0.0477924293465913,-0.99885666880401,0.00111305117018364));
#117461=DIRECTION('ref_axis',(-0.465698130493557,-0.023268095156349,-0.884637692506148));
#117462=DIRECTION('',(0.,0.,1.));
#117463=DIRECTION('center_axis',(0.,0.,1.));
#117464=DIRECTION('ref_axis',(1.,0.,0.));
#117465=DIRECTION('',(0.,0.,-1.));
#117466=DIRECTION('center_axis',(0.0163043721387329,-0.999866456824323,
0.00111174040837426));
#117467=DIRECTION('ref_axis',(0.465368411727477,0.00660442871490491,-0.885092437481868));
#117468=DIRECTION('center_axis',(0.,0.,-1.));
#117469=DIRECTION('ref_axis',(1.,0.,0.));
#117470=DIRECTION('center_axis',(-0.0163027318246417,-0.99986648211256,
0.00111305117021138));
#117471=DIRECTION('ref_axis',(-0.466232095712976,0.00661709330591105,-0.884637692506524));
#117472=DIRECTION('',(0.,0.,1.));
#117473=DIRECTION('center_axis',(0.,0.,1.));
#117474=DIRECTION('ref_axis',(1.,0.,0.));
#117475=DIRECTION('',(0.,0.,-1.));
#117476=DIRECTION('center_axis',(-0.0477907907824984,-0.998856748663014,
0.0011117404083719));
#117477=DIRECTION('ref_axis',(0.464835409613913,-0.0232253973035688,-0.885092437482751));
#117478=DIRECTION('center_axis',(0.,0.,-1.));
#117479=DIRECTION('ref_axis',(0.997945392750337,-0.0640702199807057,0.));
#117480=DIRECTION('center_axis',(-0.080330901573938,-0.996767629575425,
0.00111305117021671));
#117481=DIRECTION('ref_axis',(-0.464850213245993,0.0364750907124789,-0.884637692506187));
#117482=DIRECTION('',(0.,0.,1.));
#117483=DIRECTION('center_axis',(0.,0.,1.));
#117484=DIRECTION('ref_axis',(1.,0.,0.));
#117485=DIRECTION('',(0.,0.,-1.));
#117486=DIRECTION('center_axis',(-0.111689571093344,-0.993742523867349,
0.0011117404083511));
#117487=DIRECTION('ref_axis',(0.462392299100626,-0.0529597851830607,-0.885092437480855));
#117488=DIRECTION('center_axis',(0.,0.,-1.));
#117489=DIRECTION('ref_axis',(0.991790013823247,-0.127877161684499,0.));
#117490=DIRECTION('center_axis',(-0.144028974417756,-0.989572845042376,
0.0011130511702303));
#117491=DIRECTION('ref_axis',(-0.461558161541928,0.0661832041473919,-0.884637692506271));
#117492=DIRECTION('',(0.,0.,1.));
#117493=DIRECTION('center_axis',(0.,0.,1.));
#117494=DIRECTION('ref_axis',(1.,0.,0.));
#117495=DIRECTION('',(0.,0.,-1.));
#117496=DIRECTION('center_axis',(-0.175129394999318,-0.984544797883995,
0.00111174040840423));
#117497=DIRECTION('ref_axis',(0.458049119438637,-0.082476549944404,-0.885092437483655));
#117498=DIRECTION('center_axis',(0.,0.,-1.));
#117499=DIRECTION('ref_axis',(0.981559156991067,-0.191158628701366,0.));
#117500=DIRECTION('center_axis',(-0.207135201311547,-0.978311693426342,
0.00111305117022879));
#117501=DIRECTION('ref_axis',(-0.456369468349654,0.0956193566005051,-0.884637692505559));
#117502=DIRECTION('',(0.,0.,1.));
#117503=DIRECTION('center_axis',(0.,0.,1.));
#117504=DIRECTION('ref_axis',(1.,0.,0.));
#117505=DIRECTION('',(0.,0.,-1.));
#117506=DIRECTION('center_axis',(-0.237849574656071,-0.971301366141936,
0.00111174040845007));
#117507=DIRECTION('ref_axis',(0.451823717701448,-0.111654400872045,-0.885092437482293));
#117508=DIRECTION('center_axis',(0.,0.,-1.));
#117509=DIRECTION('ref_axis',(0.967294863039031,-0.253654583909501,0.));
#117510=DIRECTION('center_axis',(-0.269390265232804,-0.963030449214817,
0.0011130511702463));
#117511=DIRECTION('ref_axis',(-0.449305455119068,0.124662588606691,-0.884637692505879));
#117512=DIRECTION('',(0.,0.,1.));
#117513=DIRECTION('center_axis',(0.,0.,1.));
#117514=DIRECTION('ref_axis',(1.,0.,0.));
#117515=DIRECTION('',(0.,0.,-1.));
#117516=DIRECTION('center_axis',(-0.299592379391908,-0.954066648742927,
0.00111174040843038));
#117517=DIRECTION('ref_axis',(0.443741675391016,-0.140373439916541,-0.885092437481629));
#117518=DIRECTION('center_axis',(0.,0.,-1.));
#117519=DIRECTION('ref_axis',(0.949055747010671,-0.315108218023615,0.));
#117520=DIRECTION('center_axis',(-0.33053834677016,-0.943791906318094,0.00111305117024269));
#117521=DIRECTION('ref_axis',(-0.440395149396347,0.153193555295706,-0.884637692506956));
#117522=DIRECTION('',(0.,0.,1.));
#117523=DIRECTION('center_axis',(0.,0.,1.));
#117524=DIRECTION('ref_axis',(1.,0.,0.));
#117525=DIRECTION('',(0.,0.,-1.));
#117526=DIRECTION('center_axis',(-0.360104094778504,-0.932911466837566,
0.00111174040845034));
#117527=DIRECTION('ref_axis',(0.433836203352379,-0.168515654385977,-0.885092437481905));
#117528=DIRECTION('center_axis',(0.,0.,-1.));
#117529=DIRECTION('ref_axis',(0.926916757346024,-0.375267004879368,0.));
#117530=DIRECTION('center_axis',(-0.390328175340464,-0.920675120035551,
0.0011130511702119));
#117531=DIRECTION('ref_axis',(-0.429675165543775,0.18109501680736,-0.884637692506074));
#117532=DIRECTION('',(0.,0.,1.));
#117533=DIRECTION('center_axis',(0.,0.,1.));
#117534=DIRECTION('ref_axis',(1.,0.,0.));
#117535=DIRECTION('',(0.,0.,-1.));
#117536=DIRECTION('center_axis',(-0.419136065197508,-0.907922751606112,
0.00111174040842796));
#117537=DIRECTION('ref_axis',(0.422148005297344,-0.195965401885244,-0.885092437481774));
#117538=DIRECTION('center_axis',(0.,0.,-1.));
#117539=DIRECTION('ref_axis',(0.900968867902422,-0.433883739117553,0.));
#117540=DIRECTION('center_axis',(-0.448514061713085,-0.893775082200619,
0.00111305117023053));
#117541=DIRECTION('ref_axis',(-0.417189554269875,0.2082523200498,-0.884637692505796));
#117542=DIRECTION('',(0.,0.,1.));
#117543=DIRECTION('center_axis',(0.,0.,1.));
#117544=DIRECTION('ref_axis',(1.,0.,0.));
#117545=DIRECTION('',(0.,0.,-1.));
#117546=DIRECTION('center_axis',(-0.476445715620178,-0.879203187039515,
0.00111174040833913));
#117547=DIRECTION('ref_axis',(0.408725110535429,-0.22260988551223,-0.885092437483246));
#117548=DIRECTION('center_axis',(0.,0.,-1.));
#117549=DIRECTION('ref_axis',(0.871318704123392,-0.490717552003933,0.));
#117550=DIRECTION('center_axis',(-0.504856907600188,-0.86320233083876,0.00111305117023049));
#117551=DIRECTION('ref_axis',(-0.402989621631756,0.234553869839961,-0.884637692504786));
#117552=DIRECTION('',(0.,0.,1.));
#117553=DIRECTION('center_axis',(0.,0.,1.));
#117554=DIRECTION('ref_axis',(1.,0.,0.));
#117555=DIRECTION('',(0.,0.,-1.));
#117556=DIRECTION('center_axis',(-0.531797548400216,-0.846870787988808,
0.00111174040840245));
#117557=DIRECTION('ref_axis',(0.393622676626104,-0.248339617371704,-0.885092437482875));
#117558=DIRECTION('center_axis',(0.,0.,-1.));
#117559=DIRECTION('ref_axis',(0.838088104891844,-0.545534901210544,0.));
#117560=DIRECTION('center_axis',(-0.5591251881625,-0.829082495943161,0.00111305117022958));
#117561=DIRECTION('ref_axis',(-0.387133718195221,0.259891587466167,-0.88463769250505));
#117562=DIRECTION('',(0.,0.,1.));
#117563=DIRECTION('center_axis',(0.,0.,1.));
#117564=DIRECTION('ref_axis',(1.,0.,0.));
#117565=DIRECTION('',(0.,0.,-1.));
#117566=DIRECTION('center_axis',(-0.584964110983601,-0.811058415217073,
0.00111174040840115));
#117567=DIRECTION('ref_axis',(0.376902762709354,-0.273048868476615,-0.885092437480796));
#117568=DIRECTION('center_axis',(0.,0.,-1.));
#117569=DIRECTION('ref_axis',(0.80141362186796,-0.598110530491212,0.));
#117570=DIRECTION('center_axis',(-0.611095903394664,-0.791555783234102,
0.00111305117022297));
#117571=DIRECTION('ref_axis',(-0.369686999267188,0.284161354810104,-0.884637692507678));
#117572=DIRECTION('',(0.,0.,1.));
#117573=DIRECTION('center_axis',(0.,0.,1.));
#117574=DIRECTION('ref_axis',(1.,0.,0.));
#117575=DIRECTION('',(0.,0.,-1.));
#117576=DIRECTION('center_axis',(-0.635726930560603,-0.771913229445679,
0.00111174040844382));
#117577=DIRECTION('ref_axis',(0.358634074491183,-0.296636103209566,-0.885092437481248));
#117578=DIRECTION('center_axis',(0.,0.,-1.));
#117579=DIRECTION('ref_axis',(0.761445958369138,-0.648228395307784,0.));
#117580=DIRECTION('center_axis',(-0.660555494480139,-0.750776398023534,
0.00111305117020747));
#117581=DIRECTION('ref_axis',(-0.350721157168823,0.307263442200289,-0.884637692505464));
#117582=DIRECTION('',(0.,0.,1.));
#117583=DIRECTION('center_axis',(0.,0.,1.));
#117584=DIRECTION('ref_axis',(1.,0.,0.));
#117585=DIRECTION('',(0.,0.,-1.));
#117586=DIRECTION('center_axis',(-0.683877411816869,-0.729596086639673,
0.00111174040844086));
#117587=DIRECTION('ref_axis',(0.338891681935284,-0.319004396566983,-0.885092437480973));
#117588=DIRECTION('center_axis',(0.,0.,-1.));
#117589=DIRECTION('ref_axis',(0.718349350097731,-0.695682550603482,0.));
#117590=DIRECTION('center_axis',(-0.707300721350047,-0.70691191155249,0.00111305117022843));
#117591=DIRECTION('ref_axis',(-0.330314126603104,0.329102918196251,-0.884637692505322));
#117592=DIRECTION('',(0.,0.,1.));
#117593=DIRECTION('center_axis',(0.,0.,1.));
#117594=DIRECTION('ref_axis',(1.,0.,0.));
#117595=DIRECTION('',(0.,0.,-1.));
#117596=DIRECTION('center_axis',(-0.729217694096715,-0.684280877015816,
0.00111174040841947));
#117597=DIRECTION('ref_axis',(0.317756710764416,-0.340061832430751,-0.885092437482108));
#117598=DIRECTION('center_axis',(0.,0.,-1.));
#117599=DIRECTION('ref_axis',(0.672300890261321,-0.740277997075312,0.));
#117600=DIRECTION('center_axis',(-0.751139497840457,-0.660142572404688,
0.00111305117020688));
#117601=DIRECTION('ref_axis',(-0.308549764438105,0.349590039708122,-0.884637692505844));
#117602=DIRECTION('',(0.,0.,1.));
#117603=DIRECTION('center_axis',(0.,0.,1.));
#117604=DIRECTION('ref_axis',(1.,0.,0.));
#117605=DIRECTION('',(0.,0.,-1.));
#117606=DIRECTION('center_axis',(-0.771561464454877,-0.636153810490442,
0.00111174040844761));
#117607=DIRECTION('ref_axis',(0.295316009111902,-0.359721881283532,-0.885092437482129));
#117608=DIRECTION('center_axis',(0.,0.,-1.));
#117609=DIRECTION('ref_axis',(0.623489801858737,-0.781831482468027,0.));
#117610=DIRECTION('center_axis',(-0.791891681015239,-0.610660565826836,
0.00111305117025773));
#117611=DIRECTION('ref_axis',(-0.285517505108882,0.368640620761629,-0.884637692505175));
#117612=DIRECTION('',(0.,0.,1.));
#117613=DIRECTION('center_axis',(0.,0.,1.));
#117614=DIRECTION('ref_axis',(1.,0.,0.));
#117615=DIRECTION('',(0.,0.,-1.));
#117616=DIRECTION('center_axis',(-0.810734723256083,-0.58541265150332,0.00111174040839212));
#117617=DIRECTION('ref_axis',(0.27166179063417,-0.37790375576757,-0.885092437481081));
#117618=DIRECTION('center_axis',(0.,0.,-1.));
#117619=DIRECTION('ref_axis',(0.572116660122174,-0.820172254596953,0.));
#117620=DIRECTION('center_axis',(-0.829389811412563,-0.558669223997641,
0.0011130511702312));
#117621=DIRECTION('ref_axis',(-0.261311993106491,0.386176378429736,-0.884637692505585));
#117622=DIRECTION('',(0.,0.,1.));
#117623=DIRECTION('center_axis',(0.,0.,1.));
#117624=DIRECTION('ref_axis',(1.,0.,0.));
#117625=DIRECTION('',(0.,0.,-1.));
#117626=DIRECTION('center_axis',(-0.846576499177438,-0.532265906360475,
0.00111174040837876));
#117627=DIRECTION('ref_axis',(0.24689125558553,-0.394532742656637,-0.885092437481663));
#117628=DIRECTION('center_axis',(0.,0.,-1.));
#117629=DIRECTION('ref_axis',(0.518392568310529,-0.855142763005344,0.));
#117630=DIRECTION('center_axis',(-0.863479801171224,-0.504382190492881,
0.00111305117024995));
#117631=DIRECTION('ref_axis',(-0.236032694073528,0.402125254524605,-0.884637692505759));
#117632=DIRECTION('',(0.,0.,1.));
#117633=DIRECTION('center_axis',(0.,0.,1.));
#117634=DIRECTION('ref_axis',(1.,0.,0.));
#117635=DIRECTION('',(0.,0.,-1.));
#117636=DIRECTION('center_axis',(-0.878939510673589,-0.476931966437705,
0.00111174040842802));
#117637=DIRECTION('ref_axis',(0.221106191408716,-0.409540509877175,-0.885092437483383));
#117638=DIRECTION('center_axis',(0.,0.,-1.));
#117639=DIRECTION('ref_axis',(0.462538290240839,-0.886599306372998,0.));
#117640=DIRECTION('center_axis',(-0.894021567211032,-0.448022542377749,
0.00111305117021993));
#117641=DIRECTION('ref_axis',(-0.20978348607306,0.416421711695626,-0.884637692504406));
#117642=DIRECTION('',(0.,0.,1.));
#117643=DIRECTION('center_axis',(0.,0.,1.));
#117644=DIRECTION('ref_axis',(1.,0.,0.));
#117645=DIRECTION('',(0.,0.,-1.));
#117646=DIRECTION('center_axis',(-0.90769077118845,-0.41963821076325,0.00111174040843185));
#117647=DIRECTION('ref_axis',(0.194412554465174,-0.422865387297326,-0.885092437484475));
#117648=DIRECTION('center_axis',(0.,0.,-1.));
#117649=DIRECTION('ref_axis',(0.404783343122398,-0.914412623015811,0.));
#117650=DIRECTION('center_axis',(-0.920889606864142,-0.389821873535463,
0.00111305117023524));
#117651=DIRECTION('ref_axis',(-0.182672232726664,0.429007002724181,-0.884637692507091));
#117652=DIRECTION('',(0.,0.,1.));
#117653=DIRECTION('center_axis',(0.,0.,1.));
#117654=DIRECTION('ref_axis',(1.,0.,0.));
#117655=DIRECTION('',(0.,0.,-1.));
#117656=DIRECTION('center_axis',(-0.932712135625445,-0.360620071668627,
0.00111174040843274));
#117657=DIRECTION('ref_axis',(0.166920034636322,-0.434452620142095,-0.88509243748248));
#117658=DIRECTION('center_axis',(0.,0.,-1.));
#117659=DIRECTION('ref_axis',(0.345365054421312,-0.938468422049759,0.));
#117660=DIRECTION('center_axis',(-0.94397351359246,-0.330019342998253,0.00111305117020751));
#117661=DIRECTION('ref_axis',(-0.154810339995289,0.439829411961803,-0.884637692506869));
#117662=DIRECTION('',(0.,0.,1.));
#117663=DIRECTION('center_axis',(0.,0.,1.));
#117664=DIRECTION('ref_axis',(1.,0.,0.));
#117665=DIRECTION('',(0.,0.,-1.));
#117666=DIRECTION('center_axis',(-0.953900785830999,-0.300120067346832,
0.00111174040841854));
#117667=DIRECTION('ref_axis',(0.138741604580049,-0.444254593979597,-0.885092437481293));
#117668=DIRECTION('center_axis',(0.,0.,-1.));
#117669=DIRECTION('ref_axis',(0.284527586631037,-0.958667853036659,0.));
#117670=DIRECTION('center_axis',(-0.963178430671724,-0.268860692191788,
0.00111305117022739));
#117671=DIRECTION('ref_axis',(-0.126312298370754,0.44884446780464,-0.884637692505506));
#117672=DIRECTION('',(0.,0.,1.));
#117673=DIRECTION('center_axis',(0.,0.,1.));
#117674=DIRECTION('ref_axis',(1.,0.,0.));
#117675=DIRECTION('',(0.,0.,-1.));
#117676=DIRECTION('center_axis',(-0.971169653096488,-0.23838680529281,0.00111174040838518));
#117677=DIRECTION('ref_axis',(0.109993055508693,-0.452231030391505,-0.885092437483735));
#117678=DIRECTION('center_axis',(0.,0.,-1.));
#117679=DIRECTION('ref_axis',(0.222520933956318,-0.974927912181823,0.));
#117680=DIRECTION('center_axis',(-0.978425440978236,-0.206597235130671,
0.00111305117026458));
#117681=DIRECTION('ref_axis',(-0.0972952124163602,0.456015125444704,-0.884637692508355));
#117682=DIRECTION('',(0.,0.,1.));
#117683=DIRECTION('center_axis',(0.,0.,1.));
#117684=DIRECTION('ref_axis',(1.,0.,0.));
#117685=DIRECTION('',(0.,0.,-1.));
#117686=DIRECTION('center_axis',(-0.984447775942192,-0.175673960721946,
0.00111174040835251));
#117687=DIRECTION('ref_axis',(0.0807925213806202,-0.45834915250323,-0.885092437482398));
#117688=DIRECTION('center_axis',(0.,0.,-1.));
#117689=DIRECTION('ref_axis',(0.159599895033383,-0.98718178341445,0.));
#117690=DIRECTION('center_axis',(-0.989651891276182,-0.143484825715362,
0.00111305117019654));
#117691=DIRECTION('ref_axis',(-0.0678783195668276,0.461311919132307,-0.884637692504254));
#117692=DIRECTION('',(0.,0.,1.));
#117693=DIRECTION('center_axis',(0.,0.,1.));
#117694=DIRECTION('ref_axis',(1.,0.,0.));
#117695=DIRECTION('',(0.,0.,-1.));
#117696=DIRECTION('center_axis',(-0.993680591713171,-0.112239234164467,
0.00111174040842588));
#117697=DIRECTION('ref_axis',(0.0512599934516135,-0.462583819630076,-0.885092437481979));
#117698=DIRECTION('center_axis',(0.,0.,-1.));
#117699=DIRECTION('ref_axis',(0.0960230259076855,-0.995379112949198,0.));
#117700=DIRECTION('center_axis',(-0.996811649673197,-0.0797828063738752,
0.00111305117024778));
#117701=DIRECTION('ref_axis',(-0.0381825001404204,0.464713083179655,-0.884637692507326));
#117702=DIRECTION('',(0.,0.,1.));
#117703=DIRECTION('center_axis',(0.,0.,1.));
#117704=DIRECTION('ref_axis',(1.,0.,0.));
#117705=DIRECTION('',(0.,0.,-1.));
#117706=DIRECTION('center_axis',(-0.998830160788971,-0.0483432925186426,
0.00111174040839743));
#117707=DIRECTION('ref_axis',(0.0215168272142622,-0.464917630617288,-0.885092437482006));
#117708=DIRECTION('center_axis',(0.,0.,-1.));
#117709=DIRECTION('ref_axis',(0.0320515775716588,-0.999486216200688,0.));
#117710=DIRECTION('center_axis',(-0.999875295186283,-0.0157529423675828,
0.00111305117023515));
#117711=DIRECTION('ref_axis',(-0.00832978063163596,0.466204641497983,-0.884637692504884));
#117712=DIRECTION('',(0.,0.,1.));
#117713=DIRECTION('center_axis',(0.,0.,1.));
#117714=DIRECTION('ref_axis',(1.,0.,0.));
#117715=DIRECTION('',(0.,0.,-1.));
#117716=DIRECTION('center_axis',(0.,0.,1.));
#117717=DIRECTION('ref_axis',(1.,0.,0.));
#117718=DIRECTION('',(0.,0.,-1.));
#117719=DIRECTION('center_axis',(-0.999875322485693,0.0157513020857083,
0.00111174040835038));
#117720=DIRECTION('ref_axis',(0.00831475628145211,0.46534099533807,0.885092437480829));
#117721=DIRECTION('center_axis',(0.,0.,-1.));
#117722=DIRECTION('ref_axis',(-0.0320515775716516,-0.999486216200688,0.));
#117723=DIRECTION('center_axis',(-0.998830238638868,0.0483416538578713,
0.00111305117023196));
#117724=DIRECTION('ref_axis',(-0.0215571677330446,-0.465780464943283,0.884637692502727));
#117725=DIRECTION('',(0.,0.,1.));
#117726=DIRECTION('center_axis',(0.,0.,1.));
#117727=DIRECTION('ref_axis',(1.,0.,0.));
#117728=DIRECTION('',(0.,0.,-1.));
#117729=DIRECTION('center_axis',(-0.996811782009744,0.0797811712111581,
0.00111174040832857));
#117730=DIRECTION('ref_axis',(0.0381121726602704,0.463852174091903,0.885092437480588));
#117731=DIRECTION('center_axis',(0.,0.,-1.));
#117732=DIRECTION('ref_axis',(-0.0960230259076784,-0.995379112949199,0.));
#117733=DIRECTION('center_axis',(-0.99368077439247,0.112237603858393,0.00111305117019787));
#117734=DIRECTION('ref_axis',(-0.0513555330715939,-0.463442296544281,0.884637692502809));
#117735=DIRECTION('',(0.,0.,1.));
#117736=DIRECTION('center_axis',(0.,0.,1.));
#117737=DIRECTION('ref_axis',(1.,0.,0.));
#117738=DIRECTION('',(0.,0.,-1.));
#117739=DIRECTION('center_axis',(-0.989652128106054,0.143483202391165,0.00111174040836139));
#117740=DIRECTION('ref_axis',(0.0677529779465448,0.460457284765106,0.885092437481036));
#117741=DIRECTION('center_axis',(0.,0.,-1.));
#117742=DIRECTION('ref_axis',(-0.159599895033376,-0.987181783414451,0.));
#117743=DIRECTION('center_axis',(-0.984448062700232,0.17567234546978,0.00111305117020119));
#117744=DIRECTION('ref_axis',(-0.0809428675080601,-0.459199744335604,0.884637692505632));
#117745=DIRECTION('',(0.,0.,1.));
#117746=DIRECTION('center_axis',(0.,0.,1.));
#117747=DIRECTION('ref_axis',(1.,0.,0.));
#117748=DIRECTION('',(0.,0.,-1.));
#117749=DIRECTION('center_axis',(-0.978425781328237,0.206595630315586,0.0011117404084298));
#117750=DIRECTION('ref_axis',(0.0971153717123804,0.455170277682427,0.885092437484169));
#117751=DIRECTION('center_axis',(0.,0.,-1.));
#117752=DIRECTION('ref_axis',(-0.222520933956311,-0.974927912181824,0.));
#117753=DIRECTION('center_axis',(-0.971170042754915,0.238385211731998,0.00111305117020032));
#117754=DIRECTION('ref_axis',(-0.110197590340416,-0.453070241885056,0.884637692505459));
#117755=DIRECTION('',(0.,0.,1.));
#117756=DIRECTION('center_axis',(0.,0.,1.));
#117757=DIRECTION('ref_axis',(1.,0.,0.));
#117758=DIRECTION('',(0.,0.,-1.));
#117759=DIRECTION('center_axis',(-0.963178873143292,0.268859112480276,0.00111174040842531));
#117760=DIRECTION('ref_axis',(0.126078697585534,0.448012878301467,0.885092437483888));
#117761=DIRECTION('center_axis',(0.,0.,-1.));
#117762=DIRECTION('ref_axis',(-0.28452758663103,-0.958667853036661,0.));
#117763=DIRECTION('center_axis',(-0.953901276788603,0.300118502025727,0.00111305117022384));
#117764=DIRECTION('ref_axis',(-0.138999487636523,-0.445078976626565,0.884637692505714));
#117765=DIRECTION('',(0.,0.,1.));
#117766=DIRECTION('center_axis',(0.,0.,1.));
#117767=DIRECTION('ref_axis',(1.,0.,0.));
#117768=DIRECTION('',(0.,0.,-1.));
#117769=DIRECTION('center_axis',(-0.943974056367406,0.330017794881624,0.00111174040836656));
#117770=DIRECTION('ref_axis',(0.154523939047705,0.439014497908551,0.885092437481693));
#117771=DIRECTION('center_axis',(0.,0.,-1.));
#117772=DIRECTION('ref_axis',(-0.345365054421305,-0.938468422049761,0.));
#117773=DIRECTION('center_axis',(-0.932712725864767,0.360618541019467,0.00111305117019595));
#117774=DIRECTION('ref_axis',(-0.1672302062231,-0.435258786385151,0.884637692505302));
#117775=DIRECTION('',(0.,0.,1.));
#117776=DIRECTION('center_axis',(0.,0.,1.));
#117777=DIRECTION('ref_axis',(1.,0.,0.));
#117778=DIRECTION('',(0.,0.,-1.));
#117779=DIRECTION('center_axis',(-0.920890247712068,0.389820363375324,0.00111174040842408));
#117780=DIRECTION('ref_axis',(0.182334208498282,0.428212112771826,0.885092437481416));
#117781=DIRECTION('center_axis',(0.,0.,-1.));
#117782=DIRECTION('ref_axis',(-0.404783343122391,-0.914412623015814,0.));
#117783=DIRECTION('center_axis',(-0.90769145828413,0.41963672107565,0.00111305117023458));
#117784=DIRECTION('ref_axis',(-0.194773740019573,-0.423650024423506,0.884637692507363));
#117785=DIRECTION('',(0.,0.,1.));
#117786=DIRECTION('center_axis',(0.,0.,1.));
#117787=DIRECTION('ref_axis',(1.,0.,0.));
#117788=DIRECTION('',(0.,0.,-1.));
#117789=DIRECTION('center_axis',(-0.894022303498565,0.448021076379655,0.00111174040838539));
#117790=DIRECTION('ref_axis',(0.209395227575178,0.415650112211817,0.885092437481557));
#117791=DIRECTION('center_axis',(0.,0.,-1.));
#117792=DIRECTION('ref_axis',(-0.462538290240833,-0.886599306373001,0.));
#117793=DIRECTION('center_axis',(-0.878940291802164,0.476930523833209,0.0011130511702021));
#117794=DIRECTION('ref_axis',(-0.221516906744134,-0.410300393648285,0.884637692503871));
#117795=DIRECTION('',(0.,0.,1.));
#117796=DIRECTION('center_axis',(0.,0.,1.));
#117797=DIRECTION('ref_axis',(1.,0.,0.));
#117798=DIRECTION('',(0.,0.,-1.));
#117799=DIRECTION('center_axis',(-0.863480629872792,0.504380774680945,0.0011117404083924));
#117800=DIRECTION('ref_axis',(0.235595796745034,0.401380116180943,0.885092437483592));
#117801=DIRECTION('center_axis',(0.,0.,-1.));
#117802=DIRECTION('ref_axis',(-0.518392568310523,-0.855142763005347,0.));
#117803=DIRECTION('center_axis',(-0.846577371129116,0.532264516766999,0.00111305117022969));
#117804=DIRECTION('ref_axis',(-0.247349812978163,-0.39526475053625,0.884637692506477));
#117805=DIRECTION('',(0.,0.,1.));
#117806=DIRECTION('center_axis',(0.,0.,1.));
#117807=DIRECTION('ref_axis',(1.,0.,0.));
#117808=DIRECTION('',(0.,0.,-1.));
#117809=DIRECTION('center_axis',(-0.829390729122839,0.558667864189761,0.00111174040843866));
#117810=DIRECTION('ref_axis',(0.260828252254867,0.385460763163573,0.885092437481548));
#117811=DIRECTION('center_axis',(0.,0.,-1.));
#117812=DIRECTION('ref_axis',(-0.572116660122168,-0.820172254596957,0.));
#117813=DIRECTION('center_axis',(-0.810735682447803,0.585411320631048,0.0011130511702297));
#117814=DIRECTION('ref_axis',(-0.272166305775388,-0.378604879782754,0.884637692507653));
#117815=DIRECTION('',(0.,0.,1.));
#117816=DIRECTION('center_axis',(0.,0.,1.));
#117817=DIRECTION('ref_axis',(1.,0.,0.));
#117818=DIRECTION('',(0.,0.,-1.));
#117819=DIRECTION('center_axis',(-0.791892683963201,0.610659267610688,0.00111174040839811));
#117820=DIRECTION('ref_axis',(0.284988908527034,0.367957469186484,0.88509243748122));
#117821=DIRECTION('center_axis',(0.,0.,-1.));
#117822=DIRECTION('ref_axis',(-0.623489801858732,-0.781831482468031,0.));
#117823=DIRECTION('center_axis',(-0.771562506945055,0.636152543808287,0.00111305117023686));
#117824=DIRECTION('ref_axis',(-0.295864408845534,-0.360389240371643,0.884637692506278));
#117825=DIRECTION('',(0.,0.,1.));
#117826=DIRECTION('center_axis',(0.,0.,1.));
#117827=DIRECTION('ref_axis',(1.,0.,0.));
#117828=DIRECTION('',(0.,0.,-1.));
#117829=DIRECTION('center_axis',(-0.751140581904671,0.66014134111505,0.00111174040842861));
#117830=DIRECTION('ref_axis',(0.307978484240853,0.348942159037881,0.885092437483616));
#117831=DIRECTION('center_axis',(0.,0.,-1.));
#117832=DIRECTION('ref_axis',(-0.672300890261315,-0.740277997075317,0.));
#117833=DIRECTION('center_axis',(-0.729218815601615,0.684279679728743,0.00111305117020919));
#117834=DIRECTION('ref_axis',(-0.318346741595325,-0.340692684266245,0.88463769250643));
#117835=DIRECTION('',(0.,0.,1.));
#117836=DIRECTION('center_axis',(0.,0.,1.));
#117837=DIRECTION('ref_axis',(1.,0.,0.));
#117838=DIRECTION('',(0.,0.,-1.));
#117839=DIRECTION('center_axis',(-0.707301882075936,0.706910752248898,0.00111174040847968));
#117840=DIRECTION('ref_axis',(0.329702510302864,0.328492970711844,0.885092437484864));
#117841=DIRECTION('center_axis',(0.,0.,-1.));
#117842=DIRECTION('ref_axis',(-0.718349350097726,-0.695682550603488,0.));
#117843=DIRECTION('center_axis',(-0.683878607727921,0.729594963667659,0.00111305117020185));
#117844=DIRECTION('ref_axis',(-0.339520919299509,-0.319596148843642,0.884637692505994));
#117845=DIRECTION('',(0.,0.,1.));
#117846=DIRECTION('center_axis',(0.,0.,1.));
#117847=DIRECTION('ref_axis',(1.,0.,0.));
#117848=DIRECTION('',(0.,0.,-1.));
#117849=DIRECTION('center_axis',(-0.660556727098059,0.750775315469792,0.00111174040841113));
#117850=DIRECTION('ref_axis',(0.350071718034447,0.306693934312982,0.885092437482117));
#117851=DIRECTION('center_axis',(0.,0.,-1.));
#117852=DIRECTION('ref_axis',(-0.761445958369133,-0.64822839530779,0.));
#117853=DIRECTION('center_axis',(-0.635728195963607,0.771912185403204,0.0011130511702301));
#117854=DIRECTION('ref_axis',(-0.359299932716183,-0.297186324289664,0.884637692507699));
#117855=DIRECTION('',(0.,0.,1.));
#117856=DIRECTION('center_axis',(0.,0.,1.));
#117857=DIRECTION('ref_axis',(1.,0.,0.));
#117858=DIRECTION('',(0.,0.,-1.));
#117859=DIRECTION('center_axis',(-0.611097202839554,0.791554781878637,0.00111174040838367));
#117860=DIRECTION('ref_axis',(0.369002405982202,0.283634626748181,0.88509243748253));
#117861=DIRECTION('center_axis',(0.,0.,-1.));
#117862=DIRECTION('ref_axis',(-0.801413621867956,-0.598110530491217,0.));
#117863=DIRECTION('center_axis',(-0.584965440678792,0.811057454394299,0.00111305117022861));
#117864=DIRECTION('ref_axis',(-0.377602505645107,-0.273555297387249,0.884637692505757));
#117865=DIRECTION('',(0.,0.,1.));
#117866=DIRECTION('center_axis',(0.,0.,1.));
#117867=DIRECTION('ref_axis',(1.,0.,0.));
#117868=DIRECTION('',(0.,0.,-1.));
#117869=DIRECTION('center_axis',(-0.559126549094541,0.829081579900853,0.00111174040843286));
#117870=DIRECTION('ref_axis',(0.386416783897541,0.259409803665663,0.885092437480077));
#117871=DIRECTION('center_axis',(0.,0.,-1.));
#117872=DIRECTION('ref_axis',(-0.83808810489184,-0.54553490121055,0.));
#117873=DIRECTION('center_axis',(-0.531798936923542,0.846869914334004,0.0011130511702308));
#117874=DIRECTION('ref_axis',(-0.394353428875946,-0.248800173085565,0.884637692508282));
#117875=DIRECTION('',(0.,0.,1.));
#117876=DIRECTION('center_axis',(0.,0.,1.));
#117877=DIRECTION('ref_axis',(1.,0.,0.));
#117878=DIRECTION('',(0.,0.,-1.));
#117879=DIRECTION('center_axis',(-0.504858324427129,0.863201503873746,0.00111174040838814));
#117880=DIRECTION('ref_axis',(0.40224329235191,0.234119010050388,0.885092437483748));
#117881=DIRECTION('center_axis',(0.,0.,-1.));
#117882=DIRECTION('ref_axis',(-0.871318704123389,-0.490717552003939,0.));
#117883=DIRECTION('center_axis',(-0.476447157265943,0.879202404142695,0.00111305117023216));
#117884=DIRECTION('ref_axis',(-0.40948386928874,-0.223022675511165,0.88463769250477));
#117885=DIRECTION('',(0.,0.,1.));
#117886=DIRECTION('center_axis',(0.,0.,1.));
#117887=DIRECTION('ref_axis',(1.,0.,0.));
#117888=DIRECTION('',(0.,0.,-1.));
#117889=DIRECTION('center_axis',(-0.448515528612877,0.893774347711085,0.00111174040835437));
#117890=DIRECTION('ref_axis',(0.416416896846687,0.207866171210257,0.885092437481512));
#117891=DIRECTION('center_axis',(0.,0.,-1.));
#117892=DIRECTION('ref_axis',(-0.900968867902419,-0.433883739117559,0.));
#117893=DIRECTION('center_axis',(-0.419137554041534,0.907922062684443,0.00111305117022494));
#117894=DIRECTION('ref_axis',(-0.422931652641721,-0.196328729920749,0.884637692505496));
#117895=DIRECTION('',(0.,0.,1.));
#117896=DIRECTION('center_axis',(0.,0.,1.));
#117897=DIRECTION('ref_axis',(1.,0.,0.));
#117898=DIRECTION('',(0.,0.,-1.));
#117899=DIRECTION('center_axis',(-0.3903296862852,0.920674481039722,0.00111174040838437));
#117900=DIRECTION('ref_axis',(0.428879354989089,0.180759165683889,0.885092437480632));
#117901=DIRECTION('center_axis',(0.,0.,-1.));
#117902=DIRECTION('ref_axis',(-0.926916757346021,-0.375267004879375,0.));
#117903=DIRECTION('center_axis',(-0.360105624702816,0.932910874721957,0.00111305117018534));
#117904=DIRECTION('ref_axis',(-0.434641519118859,-0.168828027468166,0.884637692504258));
#117905=DIRECTION('',(0.,0.,1.));
#117906=DIRECTION('center_axis',(0.,0.,1.));
#117907=DIRECTION('ref_axis',(1.,0.,0.));
#117908=DIRECTION('',(0.,0.,-1.));
#117909=DIRECTION('center_axis',(-0.330539895551137,0.9437913654417,0.00111174040838563));
#117910=DIRECTION('ref_axis',(0.439579455865073,0.15290938197196,0.885092437481148));
#117911=DIRECTION('center_axis',(0.,0.,-1.));
#117912=DIRECTION('ref_axis',(-0.949055747010669,-0.315108218023621,0.));
#117913=DIRECTION('center_axis',(-0.299593944109832,0.954066155866462,0.00111305117019288));
#117914=DIRECTION('ref_axis',(-0.444565350358382,-0.140633574435332,0.884637692505961));
#117915=DIRECTION('',(0.,0.,1.));
#117916=DIRECTION('center_axis',(0.,0.,1.));
#117917=DIRECTION('ref_axis',(1.,0.,0.));
#117918=DIRECTION('',(0.,0.,-1.));
#117919=DIRECTION('center_axis',(-0.269391845485652,0.963030008680466,0.0011117404084127));
#117920=DIRECTION('ref_axis',(0.448473230466308,0.124431260810338,0.885092437482246));
#117921=DIRECTION('center_axis',(0.,0.,-1.));
#117922=DIRECTION('ref_axis',(-0.967294863039029,-0.253654583909508,0.));
#117923=DIRECTION('center_axis',(-0.237851167737863,0.971300974529948,0.00111305117023085));
#117924=DIRECTION('ref_axis',(-0.452662367215052,-0.11186122788,0.884637692507189));
#117925=DIRECTION('',(0.,0.,1.));
#117926=DIRECTION('center_axis',(0.,0.,1.));
#117927=DIRECTION('ref_axis',(1.,0.,0.));
#117928=DIRECTION('',(0.,0.,-1.));
#117929=DIRECTION('center_axis',(-0.207136806542691,0.978311355044272,0.00111174040845613));
#117930=DIRECTION('ref_axis',(0.455524132369569,0.095441824908564,0.885092437481574));
#117931=DIRECTION('center_axis',(0.,0.,-1.));
#117932=DIRECTION('ref_axis',(-0.981559156991065,-0.191158628701373,0.));
#117933=DIRECTION('center_axis',(-0.175131009898648,0.984544509145713,0.00111305117023712));
#117934=DIRECTION('ref_axis',(-0.458899297314163,-0.0826292195462833,0.884637692505661));
#117935=DIRECTION('',(0.,0.,1.));
#117936=DIRECTION('center_axis',(0.,0.,1.));
#117937=DIRECTION('ref_axis',(1.,0.,0.));
#117938=DIRECTION('',(0.,0.,-1.));
#117939=DIRECTION('center_axis',(-0.144030598031138,0.98957261020304,0.00111174040835033));
#117940=DIRECTION('ref_axis',(0.460703187898021,0.0660601980753236,0.885092437483707));
#117941=DIRECTION('center_axis',(0.,0.,-1.));
#117942=DIRECTION('ref_axis',(-0.991790013823246,-0.127877161684506,0.));
#117943=DIRECTION('center_axis',(-0.111691201174306,0.993742339189255,0.00111305117022436));
#117944=DIRECTION('ref_axis',(-0.463250511765016,-0.0530576700249386,0.884637692505229));
#117945=DIRECTION('',(0.,0.,1.));
#117946=DIRECTION('center_axis',(0.,0.,1.));
#117947=DIRECTION('ref_axis',(1.,0.,0.));
#117948=DIRECTION('',(0.,0.,-1.));
#117949=DIRECTION('center_axis',(-0.0803325368976281,0.996767499243859,
0.00111174040834946));
#117950=DIRECTION('ref_axis',(0.463989115215465,0.0364071157193635,0.885092437481288));
#117951=DIRECTION('center_axis',(0.,0.,-1.));
#117952=DIRECTION('ref_axis',(-0.997945392750336,-0.0640702199807131,0.));
#117953=DIRECTION('center_axis',(-0.0477924293466603,0.998856668804007,
0.00111305117023892));
#117954=DIRECTION('ref_axis',(-0.465698130493318,-0.0232680951564189,0.884637692506271));
#117955=DIRECTION('',(0.,0.,1.));
#117956=DIRECTION('center_axis',(0.,0.,1.));
#117957=DIRECTION('ref_axis',(1.,0.,0.));
#117958=DIRECTION('',(0.,0.,-1.));
#117959=DIRECTION('center_axis',(-0.0163043721387329,0.999866456824323,
0.00111174040837426));
#117960=DIRECTION('ref_axis',(0.465368411727477,0.00660442871490491,0.885092437481868));
#117961=DIRECTION('center_axis',(0.,0.,-1.));
#117962=DIRECTION('ref_axis',(-1.,0.,0.));
#117963=DIRECTION('center_axis',(0.016302731824642,0.99986648211256,0.0011130511702149));
#117964=DIRECTION('ref_axis',(-0.466232095711021,0.00661709330587505,0.884637692507555));
#117965=DIRECTION('',(0.,0.,1.));
#117966=DIRECTION('center_axis',(0.,0.,1.));
#117967=DIRECTION('ref_axis',(1.,0.,0.));
#117968=DIRECTION('',(0.,0.,-1.));
#117969=DIRECTION('center_axis',(0.0477907907825636,0.998856748663011,0.00111174040842402));
#117970=DIRECTION('ref_axis',(0.464835409616116,-0.0232253973037494,0.885092437481589));
#117971=DIRECTION('center_axis',(0.,0.,-1.));
#117972=DIRECTION('ref_axis',(-0.997945392750337,0.0640702199806987,0.));
#117973=DIRECTION('center_axis',(0.0803309015739928,0.99676762957542,0.00111305117017054));
#117974=DIRECTION('ref_axis',(-0.464850213248175,0.0364750907127227,0.88463769250503));
#117975=DIRECTION('',(0.,0.,1.));
#117976=DIRECTION('center_axis',(0.,0.,1.));
#117977=DIRECTION('ref_axis',(1.,0.,0.));
#117978=DIRECTION('',(0.,0.,-1.));
#117979=DIRECTION('center_axis',(0.111689571093429,0.99374252386734,0.00111174040844294));
#117980=DIRECTION('ref_axis',(0.462392299099744,-0.0529597851830843,0.885092437481314));
#117981=DIRECTION('center_axis',(0.,0.,-1.));
#117982=DIRECTION('ref_axis',(-0.991790013823248,0.127877161684492,0.));
#117983=DIRECTION('center_axis',(0.144028974417742,0.989572845042378,0.00111305117021856));
#117984=DIRECTION('ref_axis',(-0.461558161541436,0.066183204147324,0.884637692506533));
#117985=DIRECTION('',(0.,0.,1.));
#117986=DIRECTION('center_axis',(0.,0.,1.));
#117987=DIRECTION('ref_axis',(1.,0.,0.));
#117988=DIRECTION('',(0.,0.,-1.));
#117989=DIRECTION('center_axis',(0.175129394999254,0.984544797884007,0.00111174040835243));
#117990=DIRECTION('ref_axis',(0.45804911944098,-0.0824765499447419,0.885092437482411));
#117991=DIRECTION('center_axis',(0.,0.,-1.));
#117992=DIRECTION('ref_axis',(-0.981559156991068,0.191158628701359,0.));
#117993=DIRECTION('center_axis',(0.207135201311576,0.978311693426336,0.00111305117018698));
#117994=DIRECTION('ref_axis',(-0.456369468348504,0.0956193566003131,0.884637692506173));
#117995=DIRECTION('',(0.,0.,1.));
#117996=DIRECTION('center_axis',(0.,0.,1.));
#117997=DIRECTION('ref_axis',(1.,0.,0.));
#117998=DIRECTION('',(0.,0.,-1.));
#117999=DIRECTION('center_axis',(0.237849574656022,0.971301366141948,0.00111174040843417));
#118000=DIRECTION('ref_axis',(0.45182371770191,-0.111654400872119,0.885092437482048));
#118001=DIRECTION('center_axis',(0.,0.,-1.));
#118002=DIRECTION('ref_axis',(-0.967294863039033,0.253654583909494,0.));
#118003=DIRECTION('center_axis',(0.269390265232794,0.96303044921482,0.00111305117023979));
#118004=DIRECTION('ref_axis',(-0.449305455119629,0.12466258860685,0.884637692505571));
#118005=DIRECTION('',(0.,0.,1.));
#118006=DIRECTION('center_axis',(0.,0.,1.));
#118007=DIRECTION('ref_axis',(1.,0.,0.));
#118008=DIRECTION('',(0.,0.,-1.));
#118009=DIRECTION('center_axis',(0.299592379391923,0.954066648742922,0.00111174040846479));
#118010=DIRECTION('ref_axis',(0.443741675387824,-0.14037343991558,0.885092437483382));
#118011=DIRECTION('center_axis',(0.,0.,-1.));
#118012=DIRECTION('ref_axis',(-0.949055747010673,0.315108218023608,0.));
#118013=DIRECTION('center_axis',(0.330538346770186,0.943791906318085,0.00111305117021856));
#118014=DIRECTION('ref_axis',(-0.440395149399512,0.153193555296853,0.884637692505181));
#118015=DIRECTION('',(0.,0.,1.));
#118016=DIRECTION('center_axis',(0.,0.,1.));
#118017=DIRECTION('ref_axis',(1.,0.,0.));
#118018=DIRECTION('',(0.,0.,-1.));
#118019=DIRECTION('center_axis',(0.360104094778424,0.932911466837597,0.00111174040835927));
#118020=DIRECTION('ref_axis',(0.433836203352636,-0.168515654385946,0.885092437481785));
#118021=DIRECTION('center_axis',(0.,0.,-1.));
#118022=DIRECTION('ref_axis',(-0.926916757346027,0.375267004879361,0.));
#118023=DIRECTION('center_axis',(0.390328175340436,0.920675120035563,0.00111305117023836));
#118024=DIRECTION('ref_axis',(-0.429675165541279,0.181095016806259,0.884637692507512));
#118025=DIRECTION('',(0.,0.,1.));
#118026=DIRECTION('center_axis',(0.,0.,1.));
#118027=DIRECTION('ref_axis',(1.,0.,0.));
#118028=DIRECTION('',(0.,0.,-1.));
#118029=DIRECTION('center_axis',(0.419136065197424,0.907922751606151,0.00111174040833283));
#118030=DIRECTION('ref_axis',(0.422148005295169,-0.195965401884101,0.885092437483065));
#118031=DIRECTION('center_axis',(0.,0.,-1.));
#118032=DIRECTION('ref_axis',(-0.900968867902425,0.433883739117546,0.));
#118033=DIRECTION('center_axis',(0.448514061713074,0.893775082200625,0.00111305117023013));
#118034=DIRECTION('ref_axis',(-0.41718955427032,0.208252320050018,0.884637692505534));
#118035=DIRECTION('',(0.,0.,1.));
#118036=DIRECTION('center_axis',(0.,0.,1.));
#118037=DIRECTION('ref_axis',(1.,0.,0.));
#118038=DIRECTION('',(0.,0.,-1.));
#118039=DIRECTION('center_axis',(0.476445715620265,0.879203187039468,0.00111174040839801));
#118040=DIRECTION('ref_axis',(0.408725110535094,-0.222609885512161,0.885092437483418));
#118041=DIRECTION('center_axis',(0.,0.,-1.));
#118042=DIRECTION('ref_axis',(-0.871318704123396,0.490717552003926,0.));
#118043=DIRECTION('center_axis',(0.504856907600187,0.86320233083876,0.00111305117021984));
#118044=DIRECTION('ref_axis',(-0.402989621629229,0.234553869838492,0.884637692506327));
#118045=DIRECTION('',(0.,0.,1.));
#118046=DIRECTION('center_axis',(0.,0.,1.));
#118047=DIRECTION('ref_axis',(1.,0.,0.));
#118048=DIRECTION('',(0.,0.,-1.));
#118049=DIRECTION('center_axis',(0.531797548400194,0.846870787988822,0.00111174040839575));
#118050=DIRECTION('ref_axis',(0.39362267662406,-0.248339617370401,0.885092437484149));
#118051=DIRECTION('center_axis',(0.,0.,-1.));
#118052=DIRECTION('ref_axis',(-0.838088104891848,0.545534901210538,0.));
#118053=DIRECTION('center_axis',(0.559125188162458,0.82908249594319,0.00111305117024803));
#118054=DIRECTION('ref_axis',(-0.387133718194512,0.259891587465639,0.884637692505515));
#118055=DIRECTION('',(0.,0.,1.));
#118056=DIRECTION('center_axis',(0.,0.,1.));
#118057=DIRECTION('ref_axis',(1.,0.,0.));
#118058=DIRECTION('',(0.,0.,-1.));
#118059=DIRECTION('center_axis',(0.584964110983611,0.811058415217065,0.00111174040840853));
#118060=DIRECTION('ref_axis',(0.376902762707542,-0.273048868475325,0.885092437481966));
#118061=DIRECTION('center_axis',(0.,0.,-1.));
#118062=DIRECTION('ref_axis',(-0.801413621867964,0.598110530491206,0.));
#118063=DIRECTION('center_axis',(0.61109590339468,0.791555783234089,0.00111305117019012));
#118064=DIRECTION('ref_axis',(-0.369686999269125,0.28416135481165,0.884637692506372));
#118065=DIRECTION('',(0.,0.,1.));
#118066=DIRECTION('center_axis',(0.,0.,1.));
#118067=DIRECTION('ref_axis',(1.,0.,0.));
#118068=DIRECTION('',(0.,0.,-1.));
#118069=DIRECTION('center_axis',(0.635726930560454,0.771913229445802,0.00111174040830727));
#118070=DIRECTION('ref_axis',(0.358634074488608,-0.296636103207175,0.885092437483093));
#118071=DIRECTION('center_axis',(0.,0.,-1.));
#118072=DIRECTION('ref_axis',(-0.761445958369143,0.648228395307779,0.));
#118073=DIRECTION('center_axis',(0.660555494480137,0.750776398023536,0.0011130511702097));
#118074=DIRECTION('ref_axis',(-0.350721157168176,0.307263442199714,0.88463769250592));
#118075=DIRECTION('',(0.,0.,1.));
#118076=DIRECTION('center_axis',(0.,0.,1.));
#118077=DIRECTION('ref_axis',(1.,0.,0.));
#118078=DIRECTION('',(0.,0.,-1.));
#118079=DIRECTION('center_axis',(0.683877411816847,0.729596086639694,0.00111174040843297));
#118080=DIRECTION('ref_axis',(0.338891681935678,-0.319004396567322,0.8850924374807));
#118081=DIRECTION('center_axis',(0.,0.,-1.));
#118082=DIRECTION('ref_axis',(-0.718349350097736,0.695682550603478,0.));
#118083=DIRECTION('center_axis',(0.707300721350063,0.706911911552474,0.00111305117020991));
#118084=DIRECTION('ref_axis',(-0.330314126601671,0.329102918194854,0.884637692506377));
#118085=DIRECTION('',(0.,0.,1.));
#118086=DIRECTION('center_axis',(0.,0.,1.));
#118087=DIRECTION('ref_axis',(1.,0.,0.));
#118088=DIRECTION('',(0.,0.,-1.));
#118089=DIRECTION('center_axis',(0.729217694096672,0.684280877015861,0.00111174040837837));
#118090=DIRECTION('ref_axis',(0.317756710765229,-0.34006183243152,0.885092437481521));
#118091=DIRECTION('center_axis',(0.,0.,-1.));
#118092=DIRECTION('ref_axis',(-0.672300890261326,0.740277997075307,0.));
#118093=DIRECTION('center_axis',(0.751139497840413,0.660142572404738,0.00111305117025266));
#118094=DIRECTION('ref_axis',(-0.308549764436205,0.349590039705849,0.884637692507405));
#118095=DIRECTION('',(0.,0.,1.));
#118096=DIRECTION('center_axis',(0.,0.,1.));
#118097=DIRECTION('ref_axis',(1.,0.,0.));
#118098=DIRECTION('',(0.,0.,-1.));
#118099=DIRECTION('center_axis',(0.77156146445479,0.636153810490548,0.00111174040834627));
#118100=DIRECTION('ref_axis',(0.29531600911316,-0.359721881284815,0.885092437481187));
#118101=DIRECTION('center_axis',(0.,0.,-1.));
#118102=DIRECTION('ref_axis',(-0.623489801858743,0.781831482468022,0.));
#118103=DIRECTION('center_axis',(0.791891681015259,0.610660565826811,0.00111305117023235));
#118104=DIRECTION('ref_axis',(-0.285517505107271,0.368640620759599,0.884637692506541));
#118105=DIRECTION('',(0.,0.,1.));
#118106=DIRECTION('center_axis',(0.,0.,1.));
#118107=DIRECTION('ref_axis',(1.,0.,0.));
#118108=DIRECTION('',(0.,0.,-1.));
#118109=DIRECTION('center_axis',(0.810734723256142,0.585412651503238,0.0011117404084541));
#118110=DIRECTION('ref_axis',(0.271661790633098,-0.37790375576626,0.885092437481969));
#118111=DIRECTION('center_axis',(0.,0.,-1.));
#118112=DIRECTION('ref_axis',(-0.57211666012218,0.820172254596949,0.));
#118113=DIRECTION('center_axis',(0.829389811412555,0.558669223997653,0.0011130511702394));
#118114=DIRECTION('ref_axis',(-0.2613119931069,0.386176378430318,0.88463769250521));
#118115=DIRECTION('',(0.,0.,1.));
#118116=DIRECTION('center_axis',(0.,0.,1.));
#118117=DIRECTION('ref_axis',(1.,0.,0.));
#118118=DIRECTION('',(0.,0.,-1.));
#118119=DIRECTION('center_axis',(0.846576499177451,0.532265906360454,0.00111174040841854));
#118120=DIRECTION('ref_axis',(0.246891255584571,-0.394532742655201,0.885092437482571));
#118121=DIRECTION('center_axis',(0.,0.,-1.));
#118122=DIRECTION('ref_axis',(-0.518392568310535,0.85514276300534,0.));
#118123=DIRECTION('center_axis',(0.863479801171241,0.50438219049285,0.00111305117019087));
#118124=DIRECTION('ref_axis',(-0.236032694072651,0.402125254523237,0.884637692506615));
#118125=DIRECTION('',(0.,0.,1.));
#118126=DIRECTION('center_axis',(0.,0.,1.));
#118127=DIRECTION('ref_axis',(1.,0.,0.));
#118128=DIRECTION('',(0.,0.,-1.));
#118129=DIRECTION('center_axis',(0.878939510673582,0.476931966437718,0.00111174040838566));
#118130=DIRECTION('ref_axis',(0.221106191409744,-0.409540509878976,0.885092437482293));
#118131=DIRECTION('center_axis',(0.,0.,-1.));
#118132=DIRECTION('ref_axis',(-0.462538290240846,0.886599306372994,0.));
#118133=DIRECTION('center_axis',(0.894021567211031,0.448022542377751,0.00111305117023196));
#118134=DIRECTION('ref_axis',(-0.209783486071203,0.416421711691889,0.884637692506605));
#118135=DIRECTION('',(0.,0.,1.));
#118136=DIRECTION('center_axis',(0.,0.,1.));
#118137=DIRECTION('ref_axis',(1.,0.,0.));
#118138=DIRECTION('',(0.,0.,-1.));
#118139=DIRECTION('center_axis',(0.90769077118846,0.419638210763228,0.00111174040845409));
#118140=DIRECTION('ref_axis',(0.194412554467475,-0.422865387302372,0.885092437481558));
#118141=DIRECTION('center_axis',(0.,0.,-1.));
#118142=DIRECTION('ref_axis',(-0.404783343122404,0.914412623015808,0.));
#118143=DIRECTION('center_axis',(0.92088960686414,0.389821873535468,0.0011130511702349));
#118144=DIRECTION('ref_axis',(-0.182672232728254,0.429007002727937,0.884637692504941));
#118145=DIRECTION('',(0.,0.,1.));
#118146=DIRECTION('center_axis',(0.,0.,1.));
#118147=DIRECTION('ref_axis',(1.,0.,0.));
#118148=DIRECTION('',(0.,0.,-1.));
#118149=DIRECTION('center_axis',(0.932712135625401,0.360620071668741,0.00111174040835477));
#118150=DIRECTION('ref_axis',(0.166920034636893,-0.434452620143221,0.88509243748182));
#118151=DIRECTION('center_axis',(0.,0.,-1.));
#118152=DIRECTION('ref_axis',(-0.345365054421319,0.938468422049756,0.));
#118153=DIRECTION('center_axis',(0.943973513592441,0.330019342998308,0.00111305117024185));
#118154=DIRECTION('ref_axis',(-0.154810339995216,0.439829411961417,0.884637692507074));
#118155=DIRECTION('',(0.,0.,1.));
#118156=DIRECTION('center_axis',(0.,0.,1.));
#118157=DIRECTION('ref_axis',(1.,0.,0.));
#118158=DIRECTION('',(0.,0.,-1.));
#118159=DIRECTION('center_axis',(0.953900785830986,0.300120067346872,0.00111174040840669));
#118160=DIRECTION('ref_axis',(0.13874160457993,-0.44425459397912,0.885092437481551));
#118161=DIRECTION('center_axis',(0.,0.,-1.));
#118162=DIRECTION('ref_axis',(-0.284527586631043,0.958667853036657,0.));
#118163=DIRECTION('center_axis',(0.963178430671713,0.268860692191828,0.0011130511702472));
#118164=DIRECTION('ref_axis',(-0.126312298370385,0.448844467803181,0.884637692506299));
#118165=DIRECTION('',(0.,0.,1.));
#118166=DIRECTION('center_axis',(0.,0.,1.));
#118167=DIRECTION('ref_axis',(1.,0.,0.));
#118168=DIRECTION('',(0.,0.,-1.));
#118169=DIRECTION('center_axis',(0.971169653096497,0.238386805292774,0.00111174040839145));
#118170=DIRECTION('ref_axis',(0.109993055509511,-0.452231030394927,0.885092437481884));
#118171=DIRECTION('center_axis',(0.,0.,-1.));
#118172=DIRECTION('ref_axis',(-0.222520933956325,0.974927912181821,0.));
#118173=DIRECTION('center_axis',(0.978425440978244,0.20659723513063,0.0011130511702072));
#118174=DIRECTION('ref_axis',(-0.0972952124173608,0.456015125449797,0.884637692505619));
#118175=DIRECTION('',(0.,0.,1.));
#118176=DIRECTION('center_axis',(0.,0.,1.));
#118177=DIRECTION('ref_axis',(1.,0.,0.));
#118178=DIRECTION('',(0.,0.,-1.));
#118179=DIRECTION('center_axis',(0.984447775942196,0.175673960721926,0.00111174040839208));
#118180=DIRECTION('ref_axis',(0.080792521380986,-0.458349152505527,0.885092437481175));
#118181=DIRECTION('center_axis',(0.,0.,-1.));
#118182=DIRECTION('ref_axis',(-0.15959989503339,0.987181783414448,0.));
#118183=DIRECTION('center_axis',(0.989651891276176,0.143484825715403,0.00111305117024872));
#118184=DIRECTION('ref_axis',(-0.0678783195662134,0.461311919127594,0.884637692506759));
#118185=DIRECTION('',(0.,0.,1.));
#118186=DIRECTION('center_axis',(0.,0.,1.));
#118187=DIRECTION('ref_axis',(1.,0.,0.));
#118188=DIRECTION('',(0.,0.,-1.));
#118189=DIRECTION('center_axis',(0.993680591713164,0.112239234164531,0.00111174040837401));
#118190=DIRECTION('ref_axis',(0.0512599934515281,-0.46258381962865,0.885092437482728));
#118191=DIRECTION('center_axis',(0.,0.,-1.));
#118192=DIRECTION('ref_axis',(-0.0960230259076927,0.995379112949197,0.));
#118193=DIRECTION('center_axis',(0.996811649673195,0.0797828063739037,0.00111305117025078));
#118194=DIRECTION('ref_axis',(-0.0381825001405106,0.464713083180589,0.884637692506832));
#118195=DIRECTION('',(0.,0.,1.));
#118196=DIRECTION('center_axis',(0.,0.,1.));
#118197=DIRECTION('ref_axis',(1.,0.,0.));
#118198=DIRECTION('',(0.,0.,-1.));
#118199=DIRECTION('center_axis',(0.998830160788972,0.048343292518622,0.00111174040843717));
#118200=DIRECTION('ref_axis',(0.0215168272142989,-0.464917630618952,0.885092437481131));
#118201=DIRECTION('center_axis',(0.,0.,-1.));
#118202=DIRECTION('ref_axis',(-0.0320515775716664,0.999486216200688,0.));
#118203=DIRECTION('center_axis',(0.999875295186283,0.0157529423675647,0.00111305117019787));
#118204=DIRECTION('ref_axis',(-0.00832978063156192,0.466204641495832,0.884637692506019));
#118205=DIRECTION('',(0.,0.,1.));
#118206=DIRECTION('center_axis',(0.,0.,1.));
#118207=DIRECTION('ref_axis',(1.,0.,0.));
#118208=DIRECTION('center_axis',(-0.361755711857553,-0.932272915508417,
0.000126284884494543));
#118209=DIRECTION('ref_axis',(0.931874611709867,-0.361597189609634,0.029277645345883));
#118210=DIRECTION('center_axis',(-0.363356221121508,0.931650066446612,-0.000640517230190088));
#118211=DIRECTION('ref_axis',(0.727365888769779,0.283252870473557,-0.625065336762998));
#118212=DIRECTION('center_axis',(0.,0.,1.));
#118213=DIRECTION('ref_axis',(1.,0.,0.));
#118214=DIRECTION('center_axis',(0.14057796820823,0.990069403926878,-0.000640517230188182));
#118215=DIRECTION('ref_axis',(0.772764658753017,-0.110127684298105,-0.625065336851653));
#118216=DIRECTION('center_axis',(-0.772687200962828,-0.63478695128394,0.000126284884494751));
#118217=DIRECTION('ref_axis',(0.634517691386154,-0.772353622901137,0.0292776452173503));
#118218=DIRECTION('center_axis',(0.,0.,1.));
#118219=DIRECTION('ref_axis',(1.,0.,0.));
#118220=DIRECTION('center_axis',(-0.811770571847688,-0.583976474469825,
0.000126284884456442));
#118221=DIRECTION('ref_axis',(0.583729140212326,-0.811420427613029,0.0292776453846311));
#118222=DIRECTION('center_axis',(0.203723100201392,0.979028338804353,-0.000640517230187342));
#118223=DIRECTION('ref_axis',(0.764121025944983,-0.159412616843564,-0.625065336824778));
#118224=DIRECTION('center_axis',(0.,0.,1.));
#118225=DIRECTION('ref_axis',(1.,0.,0.));
#118226=DIRECTION('center_axis',(-0.847518203328563,-0.530766313059573,
0.000126284884449419));
#118227=DIRECTION('ref_axis',(0.530541920796553,-0.84715293174505,0.029277645282204));
#118228=DIRECTION('center_axis',(0.266031090277401,0.963964236236747,-0.000640517230154732));
#118229=DIRECTION('ref_axis',(0.752337455993016,-0.208042488770549,-0.62506533672578));
#118230=DIRECTION('center_axis',(0.,0.,1.));
#118231=DIRECTION('ref_axis',(1.,0.,0.));
#118232=DIRECTION('center_axis',(-0.879783200719837,-0.475375119020008,
0.000126284884469973));
#118233=DIRECTION('ref_axis',(0.47517459082445,-0.879404302762036,0.0292776453703841));
#118234=DIRECTION('center_axis',(0.327245901539894,0.944938997852782,-0.000640517230163509));
#118235=DIRECTION('ref_axis',(0.737462369919026,-0.255817469448713,-0.625065336807497));
#118236=DIRECTION('center_axis',(0.,0.,1.));
#118237=DIRECTION('ref_axis',(1.,0.,0.));
#118238=DIRECTION('center_axis',(-0.908432980226483,-0.418030506648687,
0.000126284884465053));
#118239=DIRECTION('ref_axis',(0.417854666536792,-0.908042012872807,0.0292776452490184));
#118240=DIRECTION('center_axis',(0.387115989199014,0.922030802437829,-0.00064051723013517));
#118241=DIRECTION('ref_axis',(0.719556892879681,-0.302541241304193,-0.625065336760452));
#118242=DIRECTION('center_axis',(0.,0.,1.));
#118243=DIRECTION('ref_axis',(1.,0.,0.));
#118244=DIRECTION('center_axis',(-0.933349813759075,-0.358968117258382,
0.000126284884510345));
#118245=DIRECTION('ref_axis',(0.358817687792907,-0.932948383574305,0.0292776452783369));
#118246=DIRECTION('center_axis',(0.445395334222083,0.895333784680818,-0.000640517230242528));
#118247=DIRECTION('ref_axis',(0.698694602122832,-0.348021806259692,-0.625065336850603));
#118248=DIRECTION('center_axis',(0.,0.,1.));
#118249=DIRECTION('ref_axis',(1.,0.,0.));
#118250=DIRECTION('center_axis',(-0.954431312704106,-0.298430650875619,
0.000126284884428326));
#118251=DIRECTION('ref_axis',(0.298306250203974,-0.954021069252139,0.0292776452647741));
#118252=DIRECTION('center_axis',(0.501844454280421,0.864957648353759,-0.000640517230093126));
#118253=DIRECTION('ref_axis',(0.674961225544822,-0.39207227505014,-0.625065336703324));
#118254=DIRECTION('center_axis',(0.,0.,1.));
#118255=DIRECTION('ref_axis',(1.,0.,0.));
#118256=DIRECTION('center_axis',(-0.971590848660291,-0.236666868935438,
0.000126284884461063));
#118257=DIRECTION('ref_axis',(0.236569008246495,-0.971173477718955,0.0292776452697189));
#118258=DIRECTION('center_axis',(0.556231387830254,0.831027215517102,-0.000640517230226317));
#118259=DIRECTION('ref_axis',(0.648454288320632,-0.434511634652827,-0.625065336832807));
#118260=DIRECTION('center_axis',(0.,0.,1.));
#118261=DIRECTION('ref_axis',(1.,0.,0.));
#118262=DIRECTION('center_axis',(-0.984757909413755,-0.17393057206592,0.000126284884500403));
#118263=DIRECTION('ref_axis',(0.173859653489982,-0.984335126048153,0.0292776453306897));
#118264=DIRECTION('center_axis',(0.608332647296512,0.793681913596937,-0.000640517230195856));
#118265=DIRECTION('ref_axis',(0.619282713433725,-0.475165492807053,-0.625065336814955));
#118266=DIRECTION('center_axis',(0.,0.,1.));
#118267=DIRECTION('ref_axis',(1.,0.,0.));
#118268=DIRECTION('center_axis',(-0.993878388687547,-0.110479557167707,
0.000126284884483687));
#118269=DIRECTION('ref_axis',(0.110435872124621,-0.993451930205023,0.0292776453969324));
#118270=DIRECTION('center_axis',(0.657934137428239,0.753075202449421,-0.000640517230047103));
#118271=DIRECTION('ref_axis',(0.58756637302375,-0.513866794015637,-0.625065336824725));
#118272=DIRECTION('center_axis',(0.,0.,1.));
#118273=DIRECTION('ref_axis',(1.,0.,0.));
#118274=DIRECTION('center_axis',(-0.998914808475977,-0.046574558071235,
0.000126284884446421));
#118275=DIRECTION('ref_axis',(0.0465582860727343,-0.998486427292382,0.0292776452411194));
#118276=DIRECTION('center_axis',(0.704832035062552,0.709373943761159,-0.000640517230105989));
#118277=DIRECTION('ref_axis',(0.553435596395122,-0.550456506382256,-0.625065336764259));
#118278=DIRECTION('center_axis',(0.,0.,1.));
#118279=DIRECTION('ref_axis',(1.,0.,0.));
#118280=DIRECTION('center_axis',(-0.999846473049816,0.0175218258743651,
0.000126284884492773));
#118281=DIRECTION('ref_axis',(0.0175106179635939,0.999417929469137,-0.0292776452973284));
#118282=DIRECTION('center_axis',(0.748833626678851,0.662757715377707,-0.000640517230120071));
#118283=DIRECTION('ref_axis',(0.517030634109736,-0.58478427481117,-0.625065336845404));
#118284=DIRECTION('center_axis',(0.,0.,1.));
#118285=DIRECTION('ref_axis',(1.,0.,0.));
#118286=DIRECTION('center_axis',(-0.996669553999495,0.0815462088792301,
0.000126284884460216));
#118287=DIRECTION('ref_axis',(0.0815075671148035,0.996242609000576,-0.029277645307502));
#118288=DIRECTION('center_axis',(0.789758100298867,0.61341807338063,-0.000640517230110011));
#118289=DIRECTION('ref_axis',(0.478501082104711,-0.616709039280961,-0.625065336819899));
#118290=DIRECTION('center_axis',(0.,0.,1.));
#118291=DIRECTION('ref_axis',(1.,0.,0.));
#118292=DIRECTION('center_axis',(-0.989397105966853,0.145235501020045,0.000126284884481098));
#118293=DIRECTION('ref_axis',(0.145169584189564,0.988973513960531,-0.0292776452398204));
#118294=DIRECTION('center_axis',(0.82743728848207,0.561557764942412,-0.000640517230185528));
#118295=DIRECTION('ref_axis',(0.438005266458827,-0.646099613946308,-0.625065336915081));
#118296=DIRECTION('center_axis',(0.,0.,1.));
#118297=DIRECTION('ref_axis',(1.,0.,0.));
#118298=DIRECTION('center_axis',(-0.97805901300076,0.208327989334383,0.000126284884461078));
#118299=DIRECTION('ref_axis',(0.208235068303793,0.97764051461419,-0.0292776452846884));
#118300=DIRECTION('center_axis',(0.861716359362257,0.507389895194155,-0.000640517230175486));
#118301=DIRECTION('ref_axis',(0.395709593338075,-0.672835226889058,-0.62506533674278));
#118302=DIRECTION('center_axis',(0.,0.,1.));
#118303=DIRECTION('ref_axis',(1.,0.,0.));
#118304=DIRECTION('center_axis',(-0.962701865757276,0.270564413254197,0.00012628488448173));
#118305=DIRECTION('ref_axis',(0.270444869856439,0.962290180692441,-0.0292776452475763));
#118306=DIRECTION('center_axis',(0.892454452884261,0.451137051531718,-0.000640517230158825));
#118307=DIRECTION('ref_axis',(0.351787864496278,-0.696806015358918,-0.625065336867096));
#118308=DIRECTION('center_axis',(0.,0.,1.));
#118309=DIRECTION('ref_axis',(1.,0.,0.));
#118310=DIRECTION('center_axis',(-0.94338877004846,0.331689029964185,0.000126284884468416));
#118311=DIRECTION('ref_axis',(0.331543355428736,0.942985590007218,-0.0292776452228328));
#118312=DIRECTION('center_axis',(0.919525259628521,0.39303038895584,-0.000640517230085256));
#118313=DIRECTION('ref_axis',(0.306420563932946,-0.717913478582981,-0.625065336799201));
#118314=DIRECTION('center_axis',(0.,0.,1.));
#118315=DIRECTION('ref_axis',(1.,0.,0.));
#118316=DIRECTION('center_axis',(-0.920199087527283,0.391450665302901,0.000126284884478618));
#118317=DIRECTION('ref_axis',(0.391279458236672,0.919806069260345,-0.0292776452921088));
#118318=DIRECTION('center_axis',(0.942817539843289,0.33330868020729,-0.000640517230158263));
#118319=DIRECTION('ref_axis',(0.259794115496682,-0.736070881214429,-0.625065336890081));
#118320=DIRECTION('center_axis',(0.,0.,1.));
#118321=DIRECTION('ref_axis',(1.,0.,0.));
#118322=DIRECTION('center_axis',(-0.893228109573398,0.449603745891936,0.000126284884511285));
#118323=DIRECTION('ref_axis',(0.449407709821742,0.892846868078202,-0.0292776453240885));
#118324=DIRECTION('center_axis',(0.962235580553193,0.272217334597077,-0.000640517230136661));
#118325=DIRECTION('ref_axis',(0.212100117373058,-0.751203610882064,-0.625065336751353));
#118326=DIRECTION('center_axis',(0.,0.,1.));
#118327=DIRECTION('ref_axis',(1.,0.,0.));
#118328=DIRECTION('center_axis',(-0.862586665720392,0.505909308249518,0.000126284884486337));
#118329=DIRECTION('ref_axis',(0.505689248728111,0.862218767597701,-0.0292776454500831));
#118330=DIRECTION('center_axis',(0.977699588863675,0.210007389568744,-0.000640517230195052));
#118331=DIRECTION('ref_axis',(0.163534554311268,-0.763249483566092,-0.62506533689072));
#118332=DIRECTION('center_axis',(0.,0.,1.));
#118333=DIRECTION('ref_axis',(1.,0.,0.));
#118334=DIRECTION('center_axis',(-0.828400668233655,0.560135980742322,0.000126284884450437));
#118335=DIRECTION('ref_axis',(0.559892802045009,0.828047625261779,-0.0292776453376336));
#118336=DIRECTION('center_axis',(0.98914601984768,0.146934479129885,-0.000640517230091587));
#118337=DIRECTION('ref_axis',(0.114296992727732,-0.772159000577822,-0.625065336808926));
#118338=DIRECTION('center_axis',(0.,0.,1.));
#118339=DIRECTION('ref_axis',(1.,0.,0.));
#118340=DIRECTION('center_axis',(-0.790810594709803,0.612060934341391,0.000126284884451835));
#118341=DIRECTION('ref_axis',(0.611795635740747,0.790473857616266,-0.0292776452918216));
#118342=DIRECTION('center_axis',(0.996527837664906,0.0832577833994178,-0.000640517230214658));
#118343=DIRECTION('ref_axis',(0.0645897602651711,-0.77789555049683,-0.625065336893769));
#118344=DIRECTION('center_axis',(0.,0.,1.));
#118345=DIRECTION('ref_axis',(1.,0.,0.));
#118346=DIRECTION('center_axis',(-0.749970910824048,0.661470798274478,0.000126284884518839));
#118347=DIRECTION('ref_axis',(0.661184469937621,0.749651863331586,-0.0292776453422865));
#118348=DIRECTION('center_axis',(0.999814708842655,0.0192389635779676,-0.000640517230218305));
#118349=DIRECTION('ref_axis',(0.0146171146338988,-0.780435560846329,-0.625065336845881));
#118350=DIRECTION('center_axis',(0.,0.,1.));
#118351=DIRECTION('ref_axis',(1.,0.,0.));
#118352=DIRECTION('center_axis',(-0.706049435597256,0.708162536812647,0.000126284884441525));
#118353=DIRECTION('ref_axis',(0.70785635532787,0.705749388744407,-0.0292776452065499));
#118354=DIRECTION('center_axis',(0.998993126922184,-0.0448589132716746,
-0.000640517230175121));
#118355=DIRECTION('ref_axis',(0.0354155958618559,0.779768594076331,0.62506533679446));
#118356=DIRECTION('center_axis',(0.,0.,1.));
#118357=DIRECTION('ref_axis',(1.,0.,0.));
#118358=DIRECTION('center_axis',(-0.659226651792583,0.751944283586536,0.000126284884470978));
#118359=DIRECTION('ref_axis',(0.751619507115029,0.658946838531902,-0.0292776452771253));
#118360=DIRECTION('center_axis',(0.994066467959853,-0.108772455224202,-0.000640517230255248));
#118361=DIRECTION('ref_axis',(0.0853027760737053,0.77589739081015,0.625065336847374));
#118362=DIRECTION('center_axis',(0.,0.,1.));
#118363=DIRECTION('ref_axis',(1.,0.,0.));
#118364=DIRECTION('center_axis',(-0.60969496427202,0.792636130007627,0.000126284884468304));
#118365=DIRECTION('ref_axis',(0.792294093126352,0.609436534417136,-0.0292776453070061));
#118366=DIRECTION('center_axis',(0.985054976653998,-0.172239027827231,-0.000640517230033179));
#118367=DIRECTION('ref_axis',(0.134839428896953,0.768837858855506,0.625065336749068));
#118368=DIRECTION('center_axis',(0.,0.,1.));
#118369=DIRECTION('ref_axis',(1.,0.,0.));
#118370=DIRECTION('center_axis',(-0.557657909364172,0.830070864550557,0.000126284884498765));
#118371=DIRECTION('ref_axis',(0.829712972761951,0.557421924858611,-0.0292776453535321));
#118372=DIRECTION('center_axis',(0.97199568315554,-0.234997833319103,-0.000640517230122774));
#118373=DIRECTION('ref_axis',(0.183821997560134,0.758619007083397,0.625065336828721));
#118374=DIRECTION('center_axis',(0.,0.,1.));
#118375=DIRECTION('ref_axis',(1.,0.,0.));
#118376=DIRECTION('center_axis',(-0.503329318489423,0.864094659861465,0.000126284884503691));
#118377=DIRECTION('ref_axis',(0.863722383821058,0.503116749045148,-0.0292776453409534));
#118378=DIRECTION('center_axis',(0.954942250902603,-0.29679098230699,-0.000640517230234924));
#118379=DIRECTION('ref_axis',(0.232049202209861,0.745282827129038,0.625065336857128));
#118380=DIRECTION('center_axis',(0.,0.,1.));
#118381=DIRECTION('ref_axis',(1.,0.,0.));
#118382=DIRECTION('center_axis',(-0.446932439481191,0.894567704867284,0.000126284884495058));
#118383=DIRECTION('ref_axis',(0.894182574335424,0.446744158590724,-0.0292776453961113));
#118384=DIRECTION('center_axis',(0.933964756106179,-0.357364553487335,-0.000640517230227479));
#118385=DIRECTION('ref_axis',(0.279322866935046,0.728884120240152,0.625065336800023));
#118386=DIRECTION('center_axis',(0.,0.,1.));
#118387=DIRECTION('ref_axis',(1.,0.,0.));
#118388=DIRECTION('center_axis',(-0.388699019212414,0.921364779289634,0.000126284884490976));
#118389=DIRECTION('ref_axis',(0.920968376854869,0.388535800564453,-0.0292776452784002));
#118390=DIRECTION('center_axis',(0.909149399791967,-0.416469637063238,-0.000640517230049945));
#118391=DIRECTION('ref_axis',(0.325448734069691,0.709490272107199,0.625065336807032));
#118392=DIRECTION('center_axis',(0.,0.,1.));
#118393=DIRECTION('ref_axis',(1.,0.,0.));
#118394=DIRECTION('center_axis',(-0.328868351297934,0.944375768201783,0.000126284884436866));
#118395=DIRECTION('ref_axis',(0.943969722761784,0.328730865590743,-0.0292776453459248));
#118396=DIRECTION('center_axis',(0.880598153582212,-0.473863357567639,-0.000640517230077695));
#118397=DIRECTION('ref_axis',(0.370237262513772,0.687180976200024,0.625065336900943));
#118398=DIRECTION('center_axis',(0.,0.,1.));
#118399=DIRECTION('ref_axis',(1.,0.,0.));
#118400=DIRECTION('center_axis',(-0.267686292786117,0.963506114514357,0.000126284884480119));
#118401=DIRECTION('ref_axis',(0.963092094599988,0.267575104979056,-0.0292776453024285));
#118402=DIRECTION('center_axis',(0.848428340671705,-0.529309871892387,-0.000640517230104159));
#118403=DIRECTION('ref_axis',(0.413504406671045,0.662047906345087,0.625065336879044));
#118404=DIRECTION('center_axis',(0.,0.,1.));
#118405=DIRECTION('ref_axis',(1.,0.,0.));
#118406=DIRECTION('center_axis',(-0.205404253878637,0.978677207531006,0.000126284884487081));
#118407=DIRECTION('ref_axis',(0.978256914438321,0.20531982086597,-0.0292776452806701));
#118408=DIRECTION('center_axis',(0.812772153722126,-0.582581338416855,-0.00064051723019751));
#118409=DIRECTION('ref_axis',(0.455072372561575,0.634194339681601,0.625065336782482));
#118410=DIRECTION('center_axis',(0.,0.,1.));
#118411=DIRECTION('ref_axis',(1.,0.,0.));
#118412=DIRECTION('center_axis',(-0.142278164832865,0.989826705976314,0.000126284884472221));
#118413=DIRECTION('ref_axis',(0.989401866778534,0.142220833567693,-0.0292776453025551));
#118414=DIRECTION('center_axis',(0.773776111653791,-0.633458853258534,-0.000640517230214162));
#118415=DIRECTION('ref_axis',(0.494770348363902,0.603734732308235,0.625065336892526));
#118416=DIRECTION('center_axis',(0.,0.,1.));
#118417=DIRECTION('ref_axis',(1.,0.,0.));
#118418=DIRECTION('center_axis',(-0.0785674242892295,0.996908794169599,
0.00012628488446824));
#118419=DIRECTION('ref_axis',(0.996481154625446,0.07853743035835,-0.0292776452100469));
#118420=DIRECTION('center_axis',(0.731600457568146,-0.681733349795767,-0.000640517230208434));
#118421=DIRECTION('ref_axis',(0.532435206693651,0.570794249453564,0.62506533695593));
#118422=DIRECTION('center_axis',(0.,0.,1.));
#118423=DIRECTION('ref_axis',(1.,0.,0.));
#118424=DIRECTION('center_axis',(-0.0145338333465579,0.999894370291374,
0.000126284884474479));
#118425=DIRECTION('ref_axis',(0.999465687656448,0.0145313000010485,-0.0292776453579056));
#118426=DIRECTION('center_axis',(0.686418500274563,-0.727206457767324,-0.000640517230213062));
#118427=DIRECTION('ref_axis',(0.567912174657105,0.535508250701133,0.625065336830679));
#118428=DIRECTION('center_axis',(0.,0.,1.));
#118429=DIRECTION('ref_axis',(1.,0.,0.));
#118430=DIRECTION('center_axis',(0.0495594802348922,0.99877116596895,0.000126284884456217));
#118431=DIRECTION('ref_axis',(0.99834320179932,-0.0495345425848042,-0.0292776452604417));
#118432=DIRECTION('center_axis',(0.638415902127094,-0.769691318418577,-0.00064051723024534));
#118433=DIRECTION('ref_axis',(0.601055469620602,0.498021733615997,0.625065336813101));
#118434=DIRECTION('center_axis',(0.,0.,1.));
#118435=DIRECTION('ref_axis',(1.,0.,0.));
#118436=DIRECTION('center_axis',(0.113449143281512,0.993543796689818,0.000126284884464334));
#118437=DIRECTION('ref_axis',(0.993118309578601,-0.113396837109937,-0.029277645281071));
#118438=DIRECTION('center_axis',(0.587789916097745,-0.809013352344375,-0.000640517230114493));
#118439=DIRECTION('ref_axis',(0.631728898747964,0.458488738410268,0.625065336775001));
#118440=DIRECTION('center_axis',(0.,0.,1.));
#118441=DIRECTION('ref_axis',(1.,0.,0.));
#118442=DIRECTION('center_axis',(0.17687261946363,0.984233742835614,0.000126284884474159));
#118443=DIRECTION('ref_axis',(0.983812481197468,-0.176793159707189,-0.0292776454112945));
#118444=DIRECTION('center_axis',(0.534748575223039,-0.845010976872258,-0.000640517230234913));
#118445=DIRECTION('ref_axis',(0.659806418230897,0.417071714568949,0.625065336879139));
#118446=DIRECTION('center_axis',(0.,0.,1.));
#118447=DIRECTION('ref_axis',(1.,0.,0.));
#118448=DIRECTION('center_axis',(0.239569288113328,0.970879261414622,0.00012628488447836));
#118449=DIRECTION('ref_axis',(0.970463956311392,-0.239463001290564,-0.0292776452836567));
#118450=DIRECTION('center_axis',(0.479509837749238,-0.877536270042086,-0.000640517230187807));
#118451=DIRECTION('ref_axis',(0.68517265178832,0.373940853698649,0.625065336726079));
#118452=DIRECTION('center_axis',(0.,0.,1.));
#118453=DIRECTION('ref_axis',(1.,0.,0.));
#118454=DIRECTION('center_axis',(0.301281515170711,0.95353522885553,0.000126284884482297));
#118455=DIRECTION('ref_axis',(0.953127586862438,-0.301148838036668,-0.0292776452425659));
#118456=DIRECTION('center_axis',(0.422300691497727,-0.906455578447295,-0.000640517230230884));
#118457=DIRECTION('ref_axis',(0.707723363756038,0.329273389542445,0.625065336851331));
#118458=DIRECTION('center_axis',(0.,0.,1.));
#118459=DIRECTION('ref_axis',(-1.,-4.31842741858589E-15,0.));
#118460=DIRECTION('center_axis',(0.361755711857575,0.932272915508408,0.000126284884481746));
#118461=DIRECTION('ref_axis',(0.931874611712475,-0.361597189610684,-0.0292776452498897));
#118462=DIRECTION('center_axis',(0.363356221121569,-0.931650066446588,-0.000640517230229525));
#118463=DIRECTION('ref_axis',(0.727365888744316,0.283252870463631,0.625065336797126));
#118464=DIRECTION('center_axis',(0.,0.,1.));
#118465=DIRECTION('ref_axis',(1.,0.,0.));
#118466=DIRECTION('center_axis',(0.420743376728019,0.907179692779568,0.000126284884514263));
#118467=DIRECTION('ref_axis',(0.906792363896192,-0.420559660770008,-0.0292776452702861));
#118468=DIRECTION('center_axis',(0.302918642092976,-0.953016204484596,-0.0006405172301338));
#118469=DIRECTION('ref_axis',(0.744019511233333,0.236068404562933,0.62506533680186));
#118470=DIRECTION('center_axis',(0.,0.,1.));
#118471=DIRECTION('ref_axis',(1.,0.,0.));
#118472=DIRECTION('center_axis',(0.478002116814432,0.878358674103609,0.000126284884485614));
#118473=DIRECTION('ref_axis',(0.877983911747608,-0.477793962072038,-0.0292776453949441));
#118474=DIRECTION('center_axis',(0.241236305388488,-0.970466194516939,-0.000640517230195009));
#118475=DIRECTION('ref_axis',(0.757615797893118,0.187913882935597,0.625065336891145));
#118476=DIRECTION('center_axis',(0.,0.,1.));
#118477=DIRECTION('ref_axis',(1.,0.,0.));
#118478=DIRECTION('center_axis',(0.533296643671695,0.845928291228419,0.000126284884457567));
#118479=DIRECTION('ref_axis',(0.845567635386527,-0.533064905501832,-0.0292776452120096));
#118480=DIRECTION('center_axis',(0.178562676959983,-0.983928330791711,-0.000640517230183268));
#118481=DIRECTION('ref_axis',(0.768098878849436,0.138987182886634,0.625065336827661));
#118482=DIRECTION('center_axis',(0.,0.,1.));
#118483=DIRECTION('ref_axis',(1.,0.,0.));
#118484=DIRECTION('center_axis',(0.586399740228354,0.810021807553505,0.000126284884436625));
#118485=DIRECTION('ref_axis',(0.809676740231543,-0.586145370889048,-0.0292776452837664));
#118486=DIRECTION('center_axis',(0.115155296190304,-0.993347294503288,-0.000640517230180079));
#118487=DIRECTION('ref_axis',(0.775425676711713,0.0894893546788511,0.625065336821156));
#118488=DIRECTION('center_axis',(0.,0.,1.));
#118489=DIRECTION('ref_axis',(1.,0.,0.));
#118490=DIRECTION('center_axis',(0.637093194469948,0.770786770522305,0.000126284884462103));
#118491=DIRECTION('ref_axis',(0.770458709676092,-0.63681723921917,-0.0292776453548837));
#118492=DIRECTION('center_axis',(0.0512747176077349,-0.99868438110943,-0.000640517230136019));
#118493=DIRECTION('ref_axis',(0.779566084139717,0.0396237955165384,0.625065336815226));
#118494=DIRECTION('center_axis',(0.,0.,1.));
#118495=DIRECTION('ref_axis',(1.,0.,0.));
#118496=DIRECTION('center_axis',(0.685168696119518,0.728384405317692,0.000126284884426764));
#118497=DIRECTION('ref_axis',(0.7280746990243,-0.68487228892067,-0.0292776452133255));
#118498=DIRECTION('center_axis',(-0.0128165597878282,-0.999917659376452,
-0.000640517230123854));
#118499=DIRECTION('ref_axis',(0.780503087305324,-0.0104045863213432,0.625065336817152));
#118500=DIRECTION('center_axis',(0.,0.,1.));
#118501=DIRECTION('ref_axis',(1.,0.,0.));
#118502=DIRECTION('center_axis',(0.730428692628412,0.682988952353753,0.000126284884449094));
#118503=DIRECTION('ref_axis',(0.682698873258233,-0.730113051478129,-0.0292776452815721));
#118504=DIRECTION('center_axis',(-0.0768551711899076,-0.997042061499437,
-0.000640517230164196));
#118505=DIRECTION('ref_axis',(0.77823283585057,-0.0603902134806393,0.625065336840671));
#118506=DIRECTION('center_axis',(0.,0.,1.));
#118507=DIRECTION('ref_axis',(1.,0.,0.));
#118508=DIRECTION('center_axis',(0.772687200962842,0.634786951283922,0.00012628488448787));
#118509=DIRECTION('ref_axis',(0.634517691386124,-0.772353622901137,-0.02927764521803));
#118510=DIRECTION('center_axis',(-0.140577968208273,-0.990069403926872,
-0.000640517230174936));
#118511=DIRECTION('ref_axis',(0.77276465884658,-0.110127684311339,0.62506533673365));
#118512=DIRECTION('center_axis',(0.,0.,1.));
#118513=DIRECTION('ref_axis',(1.,0.,0.));
#118514=DIRECTION('center_axis',(0.811770571847666,0.583976474469855,0.000126284884490396));
#118515=DIRECTION('ref_axis',(0.58372914021539,-0.811420427617263,-0.0292776452061936));
#118516=DIRECTION('center_axis',(-0.203723100201364,-0.979028338804359,
-0.000640517230211191));
#118517=DIRECTION('ref_axis',(0.764121025913825,-0.159412616837099,0.625065336864517));
#118518=DIRECTION('center_axis',(0.,0.,1.));
#118519=DIRECTION('ref_axis',(1.,0.,0.));
#118520=DIRECTION('center_axis',(0.847518203328528,0.530766313059629,0.000126284884478973));
#118521=DIRECTION('ref_axis',(0.530541920795968,-0.847152931743979,-0.0292776453237979));
#118522=DIRECTION('center_axis',(-0.266031090277392,-0.96396423623675,-0.000640517230166038));
#118523=DIRECTION('ref_axis',(0.752337455883405,-0.208042488740392,0.625065336867747));
#118524=DIRECTION('center_axis',(0.,0.,1.));
#118525=DIRECTION('ref_axis',(1.,0.,0.));
#118526=DIRECTION('center_axis',(0.879783200719825,0.47537511902003,0.000126284884493913));
#118527=DIRECTION('ref_axis',(0.475174590823935,-0.879404302761019,-0.0292776454092863));
#118528=DIRECTION('center_axis',(-0.32724590153985,-0.944938997852797,-0.000640517230195817));
#118529=DIRECTION('ref_axis',(0.737462369950221,-0.255817469459471,0.62506533676629));
#118530=DIRECTION('center_axis',(0.,0.,1.));
#118531=DIRECTION('ref_axis',(1.,0.,0.));
#118532=DIRECTION('center_axis',(0.908432980226467,0.418030506648722,0.000126284884497972));
#118533=DIRECTION('ref_axis',(0.417854666536127,-0.908042012871251,-0.0292776453067762));
#118534=DIRECTION('center_axis',(-0.387115989198804,-0.922030802437917,
-0.000640517230236988));
#118535=DIRECTION('ref_axis',(0.719556892801567,-0.302541241271347,0.625065336866272));
#118536=DIRECTION('center_axis',(0.,0.,1.));
#118537=DIRECTION('ref_axis',(1.,0.,0.));
#118538=DIRECTION('center_axis',(0.933349813759075,0.358968117258384,0.000126284884506072));
#118539=DIRECTION('ref_axis',(0.358817687792876,-0.932948383574218,-0.0292776452814723));
#118540=DIRECTION('center_axis',(-0.445395334222409,-0.895333784680656,
-0.000640517230092827));
#118541=DIRECTION('ref_axis',(0.698694602184768,-0.348021806290653,0.625065336764134));
#118542=DIRECTION('center_axis',(0.,0.,1.));
#118543=DIRECTION('ref_axis',(1.,0.,0.));
#118544=DIRECTION('center_axis',(0.954431312704091,0.298430650875666,0.000126284884468639));
#118545=DIRECTION('ref_axis',(0.298306250203729,-0.954021069251171,-0.0292776452988035));
#118546=DIRECTION('center_axis',(-0.501844454280232,-0.864957648353868,
-0.00064051723019065));
#118547=DIRECTION('ref_axis',(0.674961225480966,-0.392072275013033,0.625065336795552));
#118548=DIRECTION('center_axis',(0.,0.,1.));
#118549=DIRECTION('ref_axis',(1.,0.,0.));
#118550=DIRECTION('center_axis',(0.971590848660297,0.236666868935413,0.000126284884465081));
#118551=DIRECTION('ref_axis',(0.236569008247039,-0.97117347772134,-0.029277645186219));
#118552=DIRECTION('center_axis',(-0.556231387830428,-0.831027215516985,
-0.000640517230122861));
#118553=DIRECTION('ref_axis',(0.648454288298381,-0.434511634638079,0.625065336866143));
#118554=DIRECTION('center_axis',(0.,0.,1.));
#118555=DIRECTION('ref_axis',(1.,0.,0.));
#118556=DIRECTION('center_axis',(0.984757909413759,0.173930572065897,0.000126284884492896));
#118557=DIRECTION('ref_axis',(0.173859653489961,-0.984335126048177,-0.029277645330005));
#118558=DIRECTION('center_axis',(-0.608332647296499,-0.793681913596947,
-0.000640517230193171));
#118559=DIRECTION('ref_axis',(0.619282713485376,-0.475165492846558,0.625065336733751));
#118560=DIRECTION('center_axis',(0.,0.,1.));
#118561=DIRECTION('ref_axis',(1.,0.,0.));
#118562=DIRECTION('center_axis',(0.993878388687544,0.110479557167738,0.000126284884499037));
#118563=DIRECTION('ref_axis',(0.110435872124856,-0.993451930206933,-0.029277645331228));
#118564=DIRECTION('center_axis',(-0.657934137428163,-0.753075202449488,
-0.000640517230102684));
#118565=DIRECTION('ref_axis',(0.587566373093202,-0.513866794076159,0.625065336709684));
#118566=DIRECTION('center_axis',(0.,0.,1.));
#118567=DIRECTION('ref_axis',(1.,0.,0.));
#118568=DIRECTION('center_axis',(0.998914808475976,0.0465745580712427,0.00012628488445277));
#118569=DIRECTION('ref_axis',(0.0465582860724865,-0.998486427286337,-0.0292776454476564));
#118570=DIRECTION('center_axis',(-0.704832035062462,-0.709373943761248,
-0.000640517230175122));
#118571=DIRECTION('ref_axis',(0.553435596364022,-0.550456506351326,0.625065336819034));
#118572=DIRECTION('center_axis',(0.,0.,1.));
#118573=DIRECTION('ref_axis',(1.,0.,0.));
#118574=DIRECTION('center_axis',(0.999846473049815,-0.0175218258744245,
0.000126284884473359));
#118575=DIRECTION('ref_axis',(0.0175106179635388,0.999417929463863,0.0292776454773875));
#118576=DIRECTION('center_axis',(-0.748833626678827,-0.662757715377734,
-0.000640517230154864));
#118577=DIRECTION('ref_axis',(0.517030634121038,-0.584784274823909,0.625065336824138));
#118578=DIRECTION('center_axis',(0.,0.,1.));
#118579=DIRECTION('ref_axis',(1.,0.,0.));
#118580=DIRECTION('center_axis',(0.996669553999503,-0.0815462088791361,
0.000126284884502308));
#118581=DIRECTION('ref_axis',(0.0815075671145944,0.996242608999261,0.0292776453528275));
#118582=DIRECTION('center_axis',(-0.789758100298809,-0.613418073380703,
-0.000640517230177985));
#118583=DIRECTION('ref_axis',(0.478501082108721,-0.616709039286066,0.625065336811793));
#118584=DIRECTION('center_axis',(0.,0.,1.));
#118585=DIRECTION('ref_axis',(1.,0.,0.));
#118586=DIRECTION('center_axis',(0.989397105966854,-0.145235501020041,0.000126284884492392));
#118587=DIRECTION('ref_axis',(0.145169584189202,0.988973513958171,0.0292776453213211));
#118588=DIRECTION('center_axis',(-0.827437288482004,-0.56155776494251,-0.000640517230231779));
#118589=DIRECTION('ref_axis',(0.438005266472051,-0.646099613965648,0.625065336885824));
#118590=DIRECTION('center_axis',(0.,0.,1.));
#118591=DIRECTION('ref_axis',(1.,0.,0.));
#118592=DIRECTION('center_axis',(0.978059013000762,-0.208327989334377,0.000126284884459322));
#118593=DIRECTION('ref_axis',(0.208235068303449,0.977640514612639,0.0292776453389273));
#118594=DIRECTION('center_axis',(-0.861716359362261,-0.507389895194147,
-0.000640517230179385));
#118595=DIRECTION('ref_axis',(0.395709593315104,-0.672835226850135,0.62506533679922));
#118596=DIRECTION('center_axis',(0.,0.,1.));
#118597=DIRECTION('ref_axis',(1.,0.,0.));
#118598=DIRECTION('center_axis',(0.076855171189824,0.997042061499444,-0.00064051723019405));
#118599=DIRECTION('ref_axis',(0.778232835837226,-0.0603902134795745,-0.625065336857388));
#118600=DIRECTION('center_axis',(-0.730428692628325,-0.682988952353846,
0.000126284884508401));
#118601=DIRECTION('ref_axis',(0.682698873257609,-0.730113051477267,0.0292776453176158));
#118602=DIRECTION('center_axis',(0.,0.,1.));
#118603=DIRECTION('ref_axis',(1.,0.,0.));
#118604=DIRECTION('center_axis',(0.0128165597878328,0.999917659376452,-0.000640517230111141));
#118605=DIRECTION('ref_axis',(0.780503087340716,-0.0104045863217641,-0.625065336772952));
#118606=DIRECTION('center_axis',(-0.685168696119438,-0.728384405317767,
0.000126284884473155));
#118607=DIRECTION('ref_axis',(0.728074699020922,-0.684872288917312,0.0292776453758732));
#118608=DIRECTION('center_axis',(0.,0.,1.));
#118609=DIRECTION('ref_axis',(1.,0.,0.));
#118610=DIRECTION('center_axis',(-0.0512747176076207,0.998684381109436,
-0.000640517230077118));
#118611=DIRECTION('ref_axis',(0.779566084098042,0.0396237955143128,-0.625065336867343));
#118612=DIRECTION('center_axis',(-0.637093194469926,-0.770786770522324,
0.000126284884463446));
#118613=DIRECTION('ref_axis',(0.770458709677825,-0.636817239220578,0.0292776452786474));
#118614=DIRECTION('center_axis',(0.,0.,1.));
#118615=DIRECTION('ref_axis',(1.,0.,0.));
#118616=DIRECTION('center_axis',(-0.115155296190241,0.993347294503295,-0.000640517230157329));
#118617=DIRECTION('ref_axis',(0.775425676771399,0.0894893546857832,-0.62506533674612));
#118618=DIRECTION('center_axis',(-0.586399740228206,-0.810021807553612,
0.000126284884506732));
#118619=DIRECTION('ref_axis',(0.809676740229673,-0.586145370887453,0.0292776453674271));
#118620=DIRECTION('center_axis',(0.,0.,1.));
#118621=DIRECTION('ref_axis',(1.,0.,0.));
#118622=DIRECTION('center_axis',(-0.178562676960012,0.983928330791706,-0.000640517230193345));
#118623=DIRECTION('ref_axis',(0.768098878947061,0.13898718290445,-0.625065336703734));
#118624=DIRECTION('center_axis',(-0.533296643671567,-0.8459282912285,0.000126284884524021));
#118625=DIRECTION('ref_axis',(0.845567635383503,-0.533064905499726,0.0292776453376993));
#118626=DIRECTION('center_axis',(0.,0.,1.));
#118627=DIRECTION('ref_axis',(1.,0.,0.));
#118628=DIRECTION('center_axis',(-0.241236305388322,0.970466194516981,-0.00064051723011321));
#118629=DIRECTION('ref_axis',(0.757615797916166,0.187913882941261,-0.625065336861507));
#118630=DIRECTION('center_axis',(-0.478002116814468,-0.87835867410359,0.000126284884448764));
#118631=DIRECTION('ref_axis',(0.877983911749062,-0.477793962072885,0.0292776453375163));
#118632=DIRECTION('center_axis',(0.,0.,1.));
#118633=DIRECTION('ref_axis',(1.,0.,0.));
#118634=DIRECTION('center_axis',(-0.302918642093179,0.953016204484531,-0.00064051723023523));
#118635=DIRECTION('ref_axis',(0.744019511174325,0.236068404544233,-0.625065336879161));
#118636=DIRECTION('center_axis',(-0.420743376728091,-0.907179692779535,
0.000126284884464857));
#118637=DIRECTION('ref_axis',(0.906792363893399,-0.420559660768787,0.0292776453743162));
#118638=DIRECTION('center_axis',(0.,0.,1.));
#118639=DIRECTION('ref_axis',(1.,0.,0.));
#118640=DIRECTION('center_axis',(-0.42230069149759,0.906455578447358,-0.000640517230146995));
#118641=DIRECTION('ref_axis',(0.707723363773355,0.329273389550458,-0.625065336827504));
#118642=DIRECTION('center_axis',(-0.301281515170749,-0.953535228855518,
0.000126284884461136));
#118643=DIRECTION('ref_axis',(0.953127586860523,-0.301148838036096,0.0292776453107957));
#118644=DIRECTION('center_axis',(0.,0.,1.));
#118645=DIRECTION('ref_axis',(1.,0.,0.));
#118646=DIRECTION('center_axis',(-0.479509837749294,0.877536270042056,-0.00064051723022099));
#118647=DIRECTION('ref_axis',(0.685172651693589,0.373940853646821,-0.625065336860926));
#118648=DIRECTION('center_axis',(-0.239569288113379,-0.970879261414609,
0.000126284884448227));
#118649=DIRECTION('ref_axis',(0.970463956312834,-0.239463001290981,0.0292776452324618));
#118650=DIRECTION('center_axis',(0.,0.,1.));
#118651=DIRECTION('ref_axis',(1.,0.,0.));
#118652=DIRECTION('center_axis',(-0.534748575222834,0.845010976872388,-0.000640517230120457));
#118653=DIRECTION('ref_axis',(0.659806418276669,0.417071714597827,-0.625065336811554));
#118654=DIRECTION('center_axis',(-0.176872619463615,-0.984233742835617,
0.000126284884477445));
#118655=DIRECTION('ref_axis',(0.983812481200434,-0.176793159707719,0.0292776453084223));
#118656=DIRECTION('center_axis',(0.,0.,1.));
#118657=DIRECTION('ref_axis',(1.,0.,0.));
#118658=DIRECTION('center_axis',(-0.587789916097922,0.809013352344247,-0.000640517230203535));
#118659=DIRECTION('ref_axis',(0.631728898720485,0.458488738390412,-0.625065336817337));
#118660=DIRECTION('center_axis',(-0.113449143281533,-0.993543796689816,
0.000126284884456771));
#118661=DIRECTION('ref_axis',(0.993118309577297,-0.113396837109804,0.0292776453258326));
#118662=DIRECTION('center_axis',(0.,0.,1.));
#118663=DIRECTION('ref_axis',(1.,0.,0.));
#118664=DIRECTION('center_axis',(-0.638415902126943,0.769691318418702,-0.000640517230140775));
#118665=DIRECTION('ref_axis',(0.601055469599138,0.498021733598052,-0.625065336848038));
#118666=DIRECTION('center_axis',(-0.0495594802348531,-0.998771165968952,
0.000126284884467267));
#118667=DIRECTION('ref_axis',(0.998343201794375,-0.0495345425844979,0.0292776454296004));
#118668=DIRECTION('center_axis',(0.,0.,1.));
#118669=DIRECTION('ref_axis',(1.,0.,0.));
#118670=DIRECTION('center_axis',(-0.686418500274535,0.72720645776735,-0.000640517230207348));
#118671=DIRECTION('ref_axis',(0.567912174657334,0.535508250701313,-0.625065336830317));
#118672=DIRECTION('center_axis',(0.0145338333465769,-0.999894370291373,
0.000126284884478989));
#118673=DIRECTION('ref_axis',(0.999465687656356,0.0145313000010667,0.0292776453610361));
#118674=DIRECTION('center_axis',(0.,0.,1.));
#118675=DIRECTION('ref_axis',(1.,0.,0.));
#118676=DIRECTION('center_axis',(-0.731600457568012,0.68173334979591,-0.000640517230123058));
#118677=DIRECTION('ref_axis',(0.532435206756676,0.570794249521162,-0.625065336840516));
#118678=DIRECTION('center_axis',(0.0785674242892662,-0.996908794169596,
0.000126284884477587));
#118679=DIRECTION('ref_axis',(0.996481154621252,0.0785374303580749,0.0292776453535325));
#118680=DIRECTION('center_axis',(0.,0.,1.));
#118681=DIRECTION('ref_axis',(1.,0.,0.));
#118682=DIRECTION('center_axis',(-0.773776111653631,0.63345885325873,-0.000640517230106446));
#118683=DIRECTION('ref_axis',(0.494770348382416,0.60373473233068,-0.625065336856192));
#118684=DIRECTION('center_axis',(0.142278164832833,-0.989826705976318,0.00012628488445795));
#118685=DIRECTION('ref_axis',(0.989401866783126,0.1422208335683,0.0292776451444397));
#118686=DIRECTION('center_axis',(0.,0.,1.));
#118687=DIRECTION('ref_axis',(1.,0.,0.));
#118688=DIRECTION('center_axis',(-0.812772153722213,0.582581338416733,-0.000640517230245157));
#118689=DIRECTION('ref_axis',(0.455072372516387,0.634194339618601,-0.6250653368793));
#118690=DIRECTION('center_axis',(0.205404253878618,-0.97867720753101,0.00012628488447263));
#118691=DIRECTION('ref_axis',(0.978256914435842,0.20531982086544,0.0292776453672486));
#118692=DIRECTION('center_axis',(0.,0.,1.));
#118693=DIRECTION('ref_axis',(1.,0.,0.));
#118694=DIRECTION('center_axis',(-0.848428340671752,0.529309871892312,-0.000640517230142603));
#118695=DIRECTION('ref_axis',(0.413504406708692,0.662047906405623,-0.625065336790022));
#118696=DIRECTION('center_axis',(0.26768629278616,-0.963506114514345,0.00012628488448624));
#118697=DIRECTION('ref_axis',(0.963092094599376,0.267575104978935,0.0292776453236817));
#118698=DIRECTION('center_axis',(0.,0.,1.));
#118699=DIRECTION('ref_axis',(1.,0.,0.));
#118700=DIRECTION('center_axis',(-0.880598153582283,0.473863357567508,-0.00064051723016054));
#118701=DIRECTION('ref_axis',(0.370237262580095,0.687180976323646,-0.625065336725752));
#118702=DIRECTION('center_axis',(0.328868351298007,-0.944375768201757,0.000126284884457867));
#118703=DIRECTION('ref_axis',(0.943969722761657,0.328730865590781,0.0292776453495876));
#118704=DIRECTION('center_axis',(0.,0.,1.));
#118705=DIRECTION('ref_axis',(1.,0.,0.));
#118706=DIRECTION('center_axis',(-0.909149399792093,0.416469637062962,-0.000640517230189422));
#118707=DIRECTION('ref_axis',(0.325448734056368,0.709490272078413,-0.625065336846642));
#118708=DIRECTION('center_axis',(0.388699019212475,-0.921364779289608,0.000126284884524275));
#118709=DIRECTION('ref_axis',(0.920968376853952,0.388535800564144,0.0292776453113384));
#118710=DIRECTION('center_axis',(0.,0.,1.));
#118711=DIRECTION('ref_axis',(1.,0.,0.));
#118712=DIRECTION('center_axis',(-0.933964756106238,0.357364553487182,-0.000640517230307371));
#118713=DIRECTION('ref_axis',(0.279322866946701,0.728884120270902,-0.625065336758957));
#118714=DIRECTION('center_axis',(0.446932439481096,-0.894567704867331,0.000126284884460302));
#118715=DIRECTION('ref_axis',(0.894182574336947,0.446744158591356,0.0292776453399457));
#118716=DIRECTION('center_axis',(0.,0.,1.));
#118717=DIRECTION('ref_axis',(1.,0.,0.));
#118718=DIRECTION('center_axis',(-0.954942250902568,0.296790982307101,-0.000640517230162724));
#118719=DIRECTION('ref_axis',(0.232049202230339,0.745282827194961,-0.625065336770925));
#118720=DIRECTION('center_axis',(0.503329318489387,-0.864094659861486,0.000126284884485404));
#118721=DIRECTION('ref_axis',(0.863722383823579,0.503116749046554,0.0292776452424264));
#118722=DIRECTION('center_axis',(0.,0.,1.));
#118723=DIRECTION('ref_axis',(1.,0.,0.));
#118724=DIRECTION('center_axis',(-0.971995683155537,0.234997833319116,-0.000640517230128928));
#118725=DIRECTION('ref_axis',(0.18382199756744,0.758619007113659,-0.625065336789845));
#118726=DIRECTION('center_axis',(0.557657909364124,-0.830070864550589,0.000126284884479074));
#118727=DIRECTION('ref_axis',(0.829712972761687,0.557421924858367,0.0292776453656659));
#118728=DIRECTION('center_axis',(0.,0.,1.));
#118729=DIRECTION('ref_axis',(1.,0.,0.));
#118730=DIRECTION('center_axis',(-0.98505497665405,0.172239027826935,-0.000640517230198739));
#118731=DIRECTION('ref_axis',(0.134839428888974,0.768837858810419,-0.625065336806246));
#118732=DIRECTION('center_axis',(0.609694964272102,-0.792636130007564,0.000126284884514757));
#118733=DIRECTION('ref_axis',(0.792294093126998,0.60943653441776,0.0292776452765282));
#118734=DIRECTION('center_axis',(0.,0.,1.));
#118735=DIRECTION('ref_axis',(1.,0.,0.));
#118736=DIRECTION('center_axis',(-0.994066467959822,0.108772455224486,-0.000640517230136566));
#118737=DIRECTION('ref_axis',(0.0853027760785172,0.775897390853078,-0.62506533679343));
#118738=DIRECTION('center_axis',(0.659226651792606,-0.751944283586515,0.000126284884470909));
#118739=DIRECTION('ref_axis',(0.751619507115677,0.658946838532506,0.0292776452468731));
#118740=DIRECTION('center_axis',(0.,0.,1.));
#118741=DIRECTION('ref_axis',(1.,0.,0.));
#118742=DIRECTION('center_axis',(-0.998993126922188,0.0448589132715698,
-0.00064051723020566));
#118743=DIRECTION('ref_axis',(0.0354155958590675,0.77976859401453,-0.625065336871715));
#118744=DIRECTION('center_axis',(0.706049435597307,-0.708162536812597,0.000126284884470886));
#118745=DIRECTION('ref_axis',(0.707856355326067,0.705749388742727,0.0292776452906457));
#118746=DIRECTION('center_axis',(0.,0.,1.));
#118747=DIRECTION('ref_axis',(1.,0.,0.));
#118748=DIRECTION('center_axis',(-0.999814708842659,-0.0192389635777686,
-0.000640517230114542));
#118749=DIRECTION('ref_axis',(0.0146171146340831,-0.780435560860042,0.625065336828756));
#118750=DIRECTION('center_axis',(0.749970910823934,-0.661470798274608,0.000126284884429514));
#118751=DIRECTION('ref_axis',(0.661184469940119,0.74965186333413,0.0292776452207336));
#118752=DIRECTION('center_axis',(0.,0.,1.));
#118753=DIRECTION('ref_axis',(1.,0.,0.));
#118754=DIRECTION('center_axis',(-0.996527837664922,-0.083257783399226,
-0.000640517230122777));
#118755=DIRECTION('ref_axis',(0.0645897602705995,-0.777895550562288,0.625065336811746));
#118756=DIRECTION('center_axis',(0.790810594709797,-0.612060934341398,0.000126284884444494));
#118757=DIRECTION('ref_axis',(0.611795635740334,0.79047385761572,0.0292776453151959));
#118758=DIRECTION('center_axis',(0.,0.,1.));
#118759=DIRECTION('ref_axis',(1.,0.,0.));
#118760=DIRECTION('center_axis',(-0.989146019847667,-0.146934479129973,
-0.000640517230129196));
#118761=DIRECTION('ref_axis',(0.114296992734883,-0.772159000625384,0.625065336748863));
#118762=DIRECTION('center_axis',(0.828400668233701,-0.560135980742254,0.00012628488448557));
#118763=DIRECTION('ref_axis',(0.559892802046617,0.828047625264283,0.0292776452360898));
#118764=DIRECTION('center_axis',(0.,0.,1.));
#118765=DIRECTION('ref_axis',(1.,0.,0.));
#118766=DIRECTION('center_axis',(-0.977699588863672,-0.210007389568759,
-0.000640517230193698));
#118767=DIRECTION('ref_axis',(0.163534554324716,-0.763249483628396,0.625065336811123));
#118768=DIRECTION('center_axis',(0.862586665720386,-0.505909308249527,0.000126284884483891));
#118769=DIRECTION('ref_axis',(0.505689248729257,0.862218767599615,0.0292776453739221));
#118770=DIRECTION('center_axis',(0.,0.,1.));
#118771=DIRECTION('ref_axis',(1.,0.,0.));
#118772=DIRECTION('center_axis',(-0.962235580553159,-0.2722173345972,-0.000640517230194249));
#118773=DIRECTION('ref_axis',(0.212100117352834,-0.751203610810562,0.625065336844148));
#118774=DIRECTION('center_axis',(0.893228109573352,-0.44960374589203,0.000126284884462287));
#118775=DIRECTION('ref_axis',(0.449407709822873,0.892846868080192,0.0292776452460509));
#118776=DIRECTION('center_axis',(0.,0.,1.));
#118777=DIRECTION('ref_axis',(1.,0.,0.));
#118778=DIRECTION('center_axis',(-0.942817539843282,-0.333308680207309,
-0.000640517230161676));
#118779=DIRECTION('ref_axis',(0.259794115520574,-0.736070881281797,0.625065336800819));
#118780=DIRECTION('center_axis',(0.920199087527283,-0.391450665302901,0.000126284884478618));
#118781=DIRECTION('ref_axis',(0.391279458236672,0.919806069260345,0.0292776452921088));
#118782=DIRECTION('center_axis',(0.,0.,1.));
#118783=DIRECTION('ref_axis',(1.,0.,0.));
#118784=DIRECTION('center_axis',(0.962701865757272,-0.270564413254211,0.00012628488448324));
#118785=DIRECTION('ref_axis',(0.27044486985633,0.962290180692004,0.0292776452629509));
#118786=DIRECTION('center_axis',(-0.892454452884192,-0.451137051531855,
-0.00064051723023769));
#118787=DIRECTION('ref_axis',(0.351787864490119,-0.696806015346603,0.62506533688429));
#118788=DIRECTION('center_axis',(0.,0.,1.));
#118789=DIRECTION('ref_axis',(1.,0.,0.));
#118790=DIRECTION('',(0.,0.,1.));
#118791=DIRECTION('',(0.,0.,1.));
#118792=DIRECTION('center_axis',(0.,0.,-1.));
#118793=DIRECTION('ref_axis',(-1.,0.,0.));
#118794=DIRECTION('center_axis',(-0.878337211800797,-0.47804156970498,0.));
#118795=DIRECTION('ref_axis',(0.47804156970498,-0.878337211800797,0.));
#118796=DIRECTION('center_axis',(0.878337211800815,0.478041569704948,-1.94241554282581E-14));
#118797=DIRECTION('ref_axis',(0.477399717843322,-0.877157895167585,-0.0518028604257383));
#118798=DIRECTION('',(0.,0.,1.));
#118799=DIRECTION('center_axis',(0.878337211800797,-0.47804156970498,0.));
#118800=DIRECTION('ref_axis',(0.47804156970498,0.878337211800797,0.));
#118801=DIRECTION('center_axis',(-0.878334869807783,0.478045872772184,2.28597554380844E-6));
#118802=DIRECTION('ref_axis',(0.452531252665384,0.831457268774235,-0.322326349471446));
#118803=DIRECTION('',(0.,0.,-1.));
#118804=DIRECTION('center_axis',(0.,0.,-1.));
#118805=DIRECTION('ref_axis',(-1.,0.,0.));
#118806=DIRECTION('',(-1.50231459873716E-16,-1.,0.));
#118807=DIRECTION('',(-0.866025403784439,-0.5,0.));
#118808=DIRECTION('center_axis',(0.,0.,-1.));
#118809=DIRECTION('ref_axis',(-1.,0.,0.));
#118810=DIRECTION('',(-0.866025403784439,-0.5,0.));
#118811=DIRECTION('',(-0.866025403784439,0.5,0.));
#118812=DIRECTION('center_axis',(0.,0.,-1.));
#118813=DIRECTION('ref_axis',(-1.,0.,0.));
#118814=DIRECTION('',(-0.866025403784439,0.5,0.));
#118815=DIRECTION('',(4.50694379621148E-16,1.,0.));
#118816=DIRECTION('center_axis',(0.,0.,-1.));
#118817=DIRECTION('ref_axis',(-1.,0.,0.));
#118818=DIRECTION('',(4.50694379621148E-16,1.,0.));
#118819=DIRECTION('',(0.866025403784439,0.5,0.));
#118820=DIRECTION('center_axis',(0.,0.,-1.));
#118821=DIRECTION('ref_axis',(-1.,0.,0.));
#118822=DIRECTION('',(0.866025403784439,0.5,0.));
#118823=DIRECTION('',(0.866025403784438,-0.5,0.));
#118824=DIRECTION('center_axis',(0.,0.,-1.));
#118825=DIRECTION('ref_axis',(-1.,0.,0.));
#118826=DIRECTION('center_axis',(0.,0.,1.));
#118827=DIRECTION('ref_axis',(1.,0.,0.));
#118828=DIRECTION('center_axis',(0.,0.,1.));
#118829=DIRECTION('ref_axis',(1.,0.,0.));
#118830=DIRECTION('center_axis',(0.,0.,1.));
#118831=DIRECTION('ref_axis',(1.,0.,0.));
#118832=DIRECTION('center_axis',(0.,0.,1.));
#118833=DIRECTION('ref_axis',(1.,0.,0.));
#118834=DIRECTION('center_axis',(0.,0.,1.));
#118835=DIRECTION('ref_axis',(1.,0.,0.));
#118836=DIRECTION('center_axis',(0.,0.,1.));
#118837=DIRECTION('ref_axis',(1.,0.,0.));
#118838=DIRECTION('center_axis',(0.943388770048457,-0.331689029964193,0.000126284884467552));
#118839=DIRECTION('ref_axis',(0.331543355428355,0.942985590006125,0.0292776452623501));
#118840=DIRECTION('center_axis',(-0.919525259628521,-0.39303038895584,-0.000640517230085256));
#118841=DIRECTION('ref_axis',(0.306420563932946,-0.717913478582981,0.625065336799201));
#118842=DIRECTION('center_axis',(0.5,0.866025403784439,0.));
#118843=DIRECTION('ref_axis',(-0.866025403784439,0.5,0.));
#118844=DIRECTION('',(0.,0.,1.));
#118845=DIRECTION('',(0.,0.,1.));
#118846=DIRECTION('center_axis',(1.,-4.50694379621148E-16,0.));
#118847=DIRECTION('ref_axis',(4.50694379621148E-16,1.,0.));
#118848=DIRECTION('',(0.,0.,1.));
#118849=DIRECTION('center_axis',(0.5,-0.866025403784439,0.));
#118850=DIRECTION('ref_axis',(0.866025403784439,0.5,0.));
#118851=DIRECTION('',(0.,0.,1.));
#118852=DIRECTION('center_axis',(-0.5,-0.866025403784439,0.));
#118853=DIRECTION('ref_axis',(0.866025403784439,-0.5,0.));
#118854=DIRECTION('',(0.,0.,1.));
#118855=DIRECTION('',(0.866025403784438,-0.5,0.));
#118856=DIRECTION('center_axis',(-1.,1.50231459873716E-16,0.));
#118857=DIRECTION('ref_axis',(-1.50231459873716E-16,-1.,0.));
#118858=DIRECTION('',(0.,0.,1.));
#118859=DIRECTION('',(-1.50231459873716E-16,-1.,0.));
#118860=DIRECTION('center_axis',(-0.5,0.866025403784439,0.));
#118861=DIRECTION('ref_axis',(-0.866025403784439,-0.5,0.));
#118862=DIRECTION('center_axis',(0.,0.,-1.));
#118863=DIRECTION('ref_axis',(-1.,0.,0.));
#118864=DIRECTION('center_axis',(0.,0.,1.));
#118865=DIRECTION('ref_axis',(1.,0.,0.));
#118866=DIRECTION('center_axis',(0.,0.,1.));
#118867=DIRECTION('ref_axis',(1.,0.,0.));
#118868=DIRECTION('center_axis',(0.,0.,1.));
#118869=DIRECTION('ref_axis',(1.,0.,0.));
#118870=DIRECTION('center_axis',(0.,0.,1.));
#118871=DIRECTION('ref_axis',(-1.,-1.22464679914735E-16,0.));
#118872=DIRECTION('center_axis',(0.,0.,1.));
#118873=DIRECTION('ref_axis',(1.,0.,0.));
#118874=DIRECTION('center_axis',(0.,0.,-1.));
#118875=DIRECTION('ref_axis',(-1.,0.,0.));
#118876=DIRECTION('center_axis',(0.,0.,1.));
#118877=DIRECTION('ref_axis',(1.,0.,0.));
#118878=DIRECTION('center_axis',(0.,0.,1.));
#118879=DIRECTION('ref_axis',(-5.9042332696092E-17,1.,0.));
#118880=DIRECTION('center_axis',(0.,0.,-1.));
#118881=DIRECTION('ref_axis',(1.,0.,0.));
#118882=DIRECTION('center_axis',(0.,0.,1.));
#118883=DIRECTION('ref_axis',(1.,0.,0.));
#118884=DIRECTION('center_axis',(-0.942660163734981,0.236130725428042,-0.235868811452395));
#118885=DIRECTION('ref_axis',(0.333754100353815,0.666661575414249,-0.666461209946391));
#118886=DIRECTION('center_axis',(0.,0.,1.));
#118887=DIRECTION('ref_axis',(1.,0.,0.));
#118888=DIRECTION('center_axis',(0.,0.,1.));
#118889=DIRECTION('ref_axis',(1.,0.,0.));
#118890=DIRECTION('center_axis',(0.,0.,-1.));
#118891=DIRECTION('ref_axis',(-1.,0.,0.));
#118892=DIRECTION('center_axis',(-0.942660163734966,-0.236130725428143,
0.235868811452354));
#118893=DIRECTION('ref_axis',(0.333754100353857,-0.6666615754131,0.666461209947519));
#118894=DIRECTION('center_axis',(0.999898588892179,0.0142412054064829,-6.76296429840134E-17));
#118895=DIRECTION('ref_axis',(0.0142412054064829,-0.999898588892179,-3.2740809054583E-33));
#118896=DIRECTION('center_axis',(0.357599031314712,-0.657040215773436,0.663642288932205));
#118897=DIRECTION('ref_axis',(-4.21884749357559E-15,-0.710632718732581,
-0.703563173472532));
#118898=DIRECTION('center_axis',(0.,0.,-1.));
#118899=DIRECTION('ref_axis',(-1.,0.,0.));
#118900=DIRECTION('center_axis',(0.999898588892179,-0.0142412054064834,
-1.38914942345546E-16));
#118901=DIRECTION('ref_axis',(0.0142412054064834,0.999898588892179,3.85185988877447E-34));
#118902=DIRECTION('center_axis',(0.358627514811599,-0.658929916134845,0.661209249211309));
#118903=DIRECTION('ref_axis',(9.74220704108575E-15,-0.70832660567291,-0.705884848750767));
#118904=DIRECTION('center_axis',(0.,0.,1.));
#118905=DIRECTION('ref_axis',(-1.,0.,0.));
#118906=DIRECTION('center_axis',(0.358627514811598,0.658929916134846,-0.661209249211308));
#118907=DIRECTION('ref_axis',(9.24260668000443E-15,0.708326605672909,0.705884848750768));
#118908=DIRECTION('center_axis',(0.,0.,1.));
#118909=DIRECTION('ref_axis',(1.,0.,0.));
#118910=DIRECTION('center_axis',(0.,0.,1.));
#118911=DIRECTION('ref_axis',(1.,0.,0.));
#118912=DIRECTION('center_axis',(0.35759903131472,0.657040215773453,-0.663642288932184));
#118913=DIRECTION('ref_axis',(-5.60662627435704E-15,0.710632718732561,0.703563173472552));
#118914=DIRECTION('center_axis',(0.907160802328706,-0.4207841236529,0.));
#118915=DIRECTION('ref_axis',(0.4207841236529,0.907160802328706,0.));
#118916=DIRECTION('',(0.,0.,1.));
#118917=DIRECTION('center_axis',(-0.907158740845994,0.420788567931076,2.28597559952643E-6));
#118918=DIRECTION('ref_axis',(0.398329828542875,0.858742727515624,-0.322326349577615));
#118919=DIRECTION('',(0.,0.,-1.));
#118920=DIRECTION('center_axis',(-0.845904345266859,-0.533334640407547,
0.));
#118921=DIRECTION('ref_axis',(0.533334640407547,-0.845904345266859,0.));
#118922=DIRECTION('center_axis',(0.845904345266846,0.533334640407567,1.08502118212513E-14));
#118923=DIRECTION('ref_axis',(0.532618548222918,-0.844768575255463,-0.0518028604399965));
#118924=DIRECTION('',(0.,0.,1.));
#118925=DIRECTION('',(0.,0.,1.));
#118926=DIRECTION('center_axis',(0.,0.,1.));
#118927=DIRECTION('ref_axis',(0.997945392750336,0.0640702199807127,0.));
#118928=DIRECTION('center_axis',(0.,0.,-1.));
#118929=DIRECTION('ref_axis',(-0.997945392750336,-0.0640702199807127,0.));
#118930=DIRECTION('center_axis',(-0.955852314850969,0.175249125470288,-0.23586881145235));
#118931=DIRECTION('ref_axis',(0.290355212970421,0.686675546334093,-0.666461209949743));
#118932=DIRECTION('center_axis',(-0.925594419806206,-0.296042013585335,
0.23586881145237));
#118933=DIRECTION('ref_axis',(0.375781520548681,-0.643908149072147,0.66646120995344));
#118934=DIRECTION('center_axis',(0.,0.,-1.));
#118935=DIRECTION('ref_axis',(-0.997945392750336,-0.0640702199807131,0.));
#118936=DIRECTION('center_axis',(0.996931752839329,0.0782756678713373,-6.76296429840134E-17));
#118937=DIRECTION('ref_axis',(0.0782756678713373,-0.996931752839329,-6.93889390390711E-14));
#118938=DIRECTION('center_axis',(0.,0.,1.));
#118939=DIRECTION('ref_axis',(0.997945392750336,0.0640702199807131,0.));
#118940=DIRECTION('center_axis',(0.998756627165696,0.0498517772261152,-1.38914942345546E-16));
#118941=DIRECTION('ref_axis',(-0.0498517772261152,0.998756627165696,-2.31111593326468E-32));
#118942=DIRECTION('center_axis',(0.,0.,-1.));
#118943=DIRECTION('ref_axis',(-0.997945392750337,-0.0640702199806997,0.));
#118944=DIRECTION('center_axis',(0.,0.,1.));
#118945=DIRECTION('ref_axis',(0.997945392750337,0.0640702199806998,0.));
#118946=DIRECTION('center_axis',(0.,0.,1.));
#118947=DIRECTION('ref_axis',(0.997945392750337,0.0640702199806998,0.));
#118948=DIRECTION('center_axis',(0.398961016913279,-0.632778807581564,0.663642288932205));
#118949=DIRECTION('ref_axis',(0.0455303946146861,-0.709172647596825,-0.703563173472533));
#118950=DIRECTION('center_axis',(0.400108460798371,-0.634598730187018,0.661209249211309));
#118951=DIRECTION('ref_axis',(0.0453826414436699,-0.706871272693763,-0.705884848750769));
#118952=DIRECTION('center_axis',(0.315672891441105,0.68055341771725,-0.661209249211308));
#118953=DIRECTION('ref_axis',(-0.0453826414436428,0.706871272693764,0.705884848750769));
#118954=DIRECTION('center_axis',(0.314767594591728,0.678601704784028,-0.663642288932184));
#118955=DIRECTION('ref_axis',(-0.0455303946146921,0.709172647596805,0.703563173472552));
#118956=DIRECTION('center_axis',(0.,0.,1.));
#118957=DIRECTION('ref_axis',(0.997945392750337,0.0640702199806998,0.));
#118958=DIRECTION('center_axis',(0.,0.,1.));
#118959=DIRECTION('ref_axis',(0.997945392750337,0.0640702199806998,0.));
#118960=DIRECTION('center_axis',(0.,0.,1.));
#118961=DIRECTION('ref_axis',(-0.997945392750335,-0.0640702199807343,0.));
#118962=DIRECTION('center_axis',(0.,0.,-1.));
#118963=DIRECTION('ref_axis',(0.997945392750336,0.0640702199807131,0.));
#118964=DIRECTION('center_axis',(0.845904345266866,-0.533334640407535,0.));
#118965=DIRECTION('ref_axis',(0.533334640407535,0.845904345266866,0.));
#118966=DIRECTION('',(0.,0.,1.));
#118967=DIRECTION('center_axis',(-0.845901732387246,0.533338784581648,2.28597556045616E-6));
#118968=DIRECTION('ref_axis',(0.504873128786825,0.800755173733894,-0.322326349477363));
#118969=DIRECTION('',(0.,0.,-1.));
#118970=DIRECTION('center_axis',(-0.907160802328699,-0.420784123652913,
0.));
#118971=DIRECTION('ref_axis',(0.420784123652913,-0.907160802328699,0.));
#118972=DIRECTION('center_axis',(0.907160802328718,0.420784123652874,-2.15297035264327E-14));
#118973=DIRECTION('ref_axis',(0.420219149620008,-0.905942785136197,-0.0518028604645239));
#118974=DIRECTION('',(0.,0.,1.));
#118975=DIRECTION('',(0.,0.,1.));
#118976=DIRECTION('center_axis',(0.,0.,1.));
#118977=DIRECTION('ref_axis',(0.997945392750336,-0.0640702199807125,0.));
#118978=DIRECTION('center_axis',(0.,0.,-1.));
#118979=DIRECTION('ref_axis',(-0.997945392750336,0.0640702199807125,0.));
#118980=DIRECTION('center_axis',(-0.92559441980614,0.296042013585654,-0.23586881145223));
#118981=DIRECTION('ref_axis',(0.375781520549103,0.643908149076686,-0.666461209948816));
#118982=DIRECTION('center_axis',(-0.95585231485097,-0.175249125470276,0.235868811452355));
#118983=DIRECTION('ref_axis',(0.290355212970749,-0.686675546328891,0.66646120995496));
#118984=DIRECTION('center_axis',(0.,0.,-1.));
#118985=DIRECTION('ref_axis',(-0.997945392750337,0.0640702199806987,0.));
#118986=DIRECTION('center_axis',(0.998756627165697,-0.0498517772261013,
-6.76296429840134E-17));
#118987=DIRECTION('ref_axis',(-0.0498517772261013,-0.998756627165697,-7.04890359645728E-32));
#118988=DIRECTION('center_axis',(0.,0.,1.));
#118989=DIRECTION('ref_axis',(0.997945392750337,-0.0640702199806987,0.));
#118990=DIRECTION('center_axis',(0.99693175283933,-0.0782756678713235,-1.38914942345546E-16));
#118991=DIRECTION('ref_axis',(0.0782756678713235,0.99693175283933,-1.27881748307313E-31));
#118992=DIRECTION('center_axis',(0.,0.,-1.));
#118993=DIRECTION('ref_axis',(-0.997945392750337,0.0640702199806997,0.));
#118994=DIRECTION('center_axis',(0.,0.,1.));
#118995=DIRECTION('ref_axis',(0.997945392750337,-0.0640702199806996,0.));
#118996=DIRECTION('center_axis',(0.,0.,1.));
#118997=DIRECTION('ref_axis',(0.997945392750337,-0.0640702199806997,0.));
#118998=DIRECTION('center_axis',(0.31476759459173,-0.678601704784007,0.663642288932205));
#118999=DIRECTION('ref_axis',(-0.0455303946146791,-0.709172647596825,-0.703563173472533));
#119000=DIRECTION('center_axis',(0.315672891441116,-0.680553417717245,0.661209249211309));
#119001=DIRECTION('ref_axis',(-0.0453826414436315,-0.706871272693765,-0.705884848750768));
#119002=DIRECTION('center_axis',(0.400108460798361,0.634598730187025,-0.661209249211308));
#119003=DIRECTION('ref_axis',(0.0453826414436588,0.706871272693763,0.70588484875077));
#119004=DIRECTION('center_axis',(0.39896101691328,0.632778807581586,-0.663642288932184));
#119005=DIRECTION('ref_axis',(0.0455303946146747,0.709172647596805,0.703563173472553));
#119006=DIRECTION('center_axis',(0.,0.,1.));
#119007=DIRECTION('ref_axis',(0.997945392750337,-0.0640702199806997,0.));
#119008=DIRECTION('center_axis',(0.,0.,1.));
#119009=DIRECTION('ref_axis',(0.997945392750337,-0.0640702199806997,0.));
#119010=DIRECTION('center_axis',(0.,0.,1.));
#119011=DIRECTION('ref_axis',(-0.997945392750337,0.0640702199806997,0.));
#119012=DIRECTION('center_axis',(0.,0.,-1.));
#119013=DIRECTION('ref_axis',(0.997945392750337,-0.0640702199806987,0.));
#119014=DIRECTION('center_axis',(0.809995476332314,-0.586436124672745,0.));
#119015=DIRECTION('ref_axis',(0.586436124672745,0.809995476332314,0.));
#119016=DIRECTION('',(0.,0.,1.));
#119017=DIRECTION('center_axis',(-0.809992603302981,0.586440092924448,2.28597557991567E-6));
#119018=DIRECTION('ref_axis',(0.555140372897279,0.766762603882455,-0.322326349631654));
#119019=DIRECTION('',(0.,0.,-1.));
#119020=DIRECTION('center_axis',(-0.932256674534458,-0.361797585378833,
0.));
#119021=DIRECTION('ref_axis',(0.361797585378833,-0.932256674534458,0.));
#119022=DIRECTION('center_axis',(0.932256674534446,0.361797585378863,9.65517100877403E-15));
#119023=DIRECTION('ref_axis',(0.361311810776095,-0.9310049618806,-0.0518028604171809));
#119024=DIRECTION('',(0.,0.,1.));
#119025=DIRECTION('',(0.,0.,1.));
#119026=DIRECTION('center_axis',(0.,0.,1.));
#119027=DIRECTION('ref_axis',(0.991790013823251,-0.127877161684469,0.));
#119028=DIRECTION('center_axis',(0.,0.,-1.));
#119029=DIRECTION('ref_axis',(-0.991790013823251,0.127877161684469,0.));
#119030=DIRECTION('center_axis',(-0.904725209867088,0.354736801607889,-0.23586881145238));
#119031=DIRECTION('ref_axis',(0.416264773871857,0.618508766043805,-0.666461209944271));
#119032=DIRECTION('center_axis',(-0.96511666377558,-0.113647389264867,0.235868811452411));
#119033=DIRECTION('ref_axis',(0.245763193736037,-0.703867820144193,0.666461209951581));
#119034=DIRECTION('center_axis',(0.,0.,-1.));
#119035=DIRECTION('ref_axis',(-0.991790013823248,0.127877161684492,0.));
#119036=DIRECTION('center_axis',(0.993510560225567,-0.113739908212905,-6.76296429840134E-17));
#119037=DIRECTION('ref_axis',(-0.113739908212905,-0.993510560225567,2.46519032881566E-32));
#119038=DIRECTION('center_axis',(0.,0.,1.));
#119039=DIRECTION('ref_axis',(0.991790013823248,-0.127877161684492,0.));
#119040=DIRECTION('center_axis',(0.989868310372873,-0.141988478826816,-1.38914942345546E-16));
#119041=DIRECTION('ref_axis',(0.141988478826816,0.989868310372873,1.41748443906901E-31));
#119042=DIRECTION('center_axis',(0.,0.,-1.));
#119043=DIRECTION('ref_axis',(-0.99179001382325,0.127877161684477,0.));
#119044=DIRECTION('center_axis',(0.,0.,1.));
#119045=DIRECTION('ref_axis',(0.99179001382325,-0.127877161684477,0.));
#119046=DIRECTION('center_axis',(0.,0.,1.));
#119047=DIRECTION('ref_axis',(0.99179001382325,-0.127877161684477,0.));
#119048=DIRECTION('center_axis',(0.270642710305125,-0.697374673830015,0.663642288932205));
#119049=DIRECTION('ref_axis',(-0.0908736950716529,-0.704798433935037,-0.703563173472534));
#119050=DIRECTION('center_axis',(0.271421100448069,-0.699380379327999,0.661209249211309));
#119051=DIRECTION('ref_axis',(-0.0905787958790508,-0.702511254031711,-0.705884848750768));
#119052=DIRECTION('center_axis',(0.439945275296716,0.60765984193586,-0.661209249211308));
#119053=DIRECTION('ref_axis',(0.0905787958790733,0.702511254031707,0.705884848750769));
#119054=DIRECTION('center_axis',(0.438683586116482,0.605917175538733,-0.663642288932184));
#119055=DIRECTION('ref_axis',(0.0908736950716462,0.704798433935021,0.703563173472551));
#119056=DIRECTION('center_axis',(0.,0.,1.));
#119057=DIRECTION('ref_axis',(0.99179001382325,-0.127877161684477,0.));
#119058=DIRECTION('center_axis',(0.,0.,1.));
#119059=DIRECTION('ref_axis',(0.99179001382325,-0.127877161684477,0.));
#119060=DIRECTION('center_axis',(0.,0.,1.));
#119061=DIRECTION('ref_axis',(-0.991790013823245,0.127877161684512,0.));
#119062=DIRECTION('center_axis',(0.,0.,-1.));
#119063=DIRECTION('ref_axis',(0.991790013823248,-0.127877161684492,0.));
#119064=DIRECTION('center_axis',(0.770758162242027,-0.637127817111522,0.));
#119065=DIRECTION('ref_axis',(0.637127817111522,0.770758162242027,0.));
#119066=DIRECTION('',(0.,0.,1.));
#119067=DIRECTION('center_axis',(-0.770755040868878,0.637131593134407,2.28597557558209E-6));
#119068=DIRECTION('ref_axis',(0.6031264261884,0.729619242092798,-0.322326349529696));
#119069=DIRECTION('',(0.,0.,-1.));
#119070=DIRECTION('center_axis',(-0.953521704096125,-0.301324343221092,
0.));
#119071=DIRECTION('ref_axis',(0.301324343221092,-0.953521704096125,0.));
#119072=DIRECTION('center_axis',(0.953521704096107,0.301324343221148,2.82636636602641E-14));
#119073=DIRECTION('ref_axis',(0.3009197642001,-0.952241439536436,-0.0518028603779049));
#119074=DIRECTION('',(0.,0.,1.));
#119075=DIRECTION('',(0.,0.,1.));
#119076=DIRECTION('center_axis',(0.,0.,1.));
#119077=DIRECTION('ref_axis',(0.981559156991069,-0.191158628701354,0.));
#119078=DIRECTION('center_axis',(0.,0.,-1.));
#119079=DIRECTION('ref_axis',(-0.981559156991069,0.191158628701354,0.));
#119080=DIRECTION('center_axis',(-0.880138289977599,0.411973900022062,-0.235868811452301));
#119081=DIRECTION('ref_axis',(0.455037505948351,0.59056779780744,-0.666461209953869));
#119082=DIRECTION('center_axis',(-0.970415141311856,-0.0515786515599852,
0.235868811452352));
#119083=DIRECTION('ref_axis',(0.200161280821658,-0.718167750108659,0.666461209946761));
#119084=DIRECTION('center_axis',(0.,0.,-1.));
#119085=DIRECTION('ref_axis',(-0.981559156991068,0.191158628701359,0.));
#119086=DIRECTION('center_axis',(0.984181945286123,-0.177160657519729,-6.76296429840134E-17));
#119087=DIRECTION('ref_axis',(-0.177160657519728,-0.984181945286123,-1.86430018616684E-31));
#119088=DIRECTION('center_axis',(0.,0.,1.));
#119089=DIRECTION('ref_axis',(0.981559156991068,-0.191158628701359,0.));
#119090=DIRECTION('center_axis',(0.978737286693008,-0.205117828666377,-1.38914942345546E-16));
#119091=DIRECTION('ref_axis',(0.205117828666377,0.978737286693008,2.65007960347684E-31));
#119092=DIRECTION('center_axis',(0.,0.,-1.));
#119093=DIRECTION('ref_axis',(-0.981559156991067,0.191158628701365,0.));
#119094=DIRECTION('center_axis',(0.,0.,1.));
#119095=DIRECTION('ref_axis',(0.981559156991067,-0.191158628701365,0.));
#119096=DIRECTION('center_axis',(0.,0.,1.));
#119097=DIRECTION('ref_axis',(0.981559156991067,-0.191158628701365,0.));
#119098=DIRECTION('center_axis',(0.225405697069196,-0.713281980754858,0.663642288932205));
#119099=DIRECTION('ref_axis',(-0.135843576023237,-0.697528052329422,-0.703563173472533));
#119100=DIRECTION('center_axis',(0.226053981933637,-0.715333436943475,0.661209249211309));
#119101=DIRECTION('ref_axis',(-0.135402742613109,-0.695264465938648,-0.705884848750768));
#119102=DIRECTION('center_axis',(0.477974260290913,0.578223949051553,-0.661209249211308));
#119103=DIRECTION('ref_axis',(0.135402742613123,0.695264465938647,0.705884848750766));
#119104=DIRECTION('center_axis',(0.476603510366998,0.576565699852764,-0.663642288932184));
#119105=DIRECTION('ref_axis',(0.135843576023234,0.697528052329402,0.703563173472553));
#119106=DIRECTION('center_axis',(0.,0.,1.));
#119107=DIRECTION('ref_axis',(0.981559156991067,-0.191158628701365,0.));
#119108=DIRECTION('center_axis',(0.,0.,1.));
#119109=DIRECTION('ref_axis',(0.981559156991067,-0.191158628701365,0.));
#119110=DIRECTION('center_axis',(0.,0.,1.));
#119111=DIRECTION('ref_axis',(-0.981559156991053,0.191158628701434,0.));
#119112=DIRECTION('center_axis',(0.,0.,-1.));
#119113=DIRECTION('ref_axis',(0.981559156991068,-0.191158628701359,0.));
#119114=DIRECTION('center_axis',(0.72835363753598,-0.685201414686299,0.));
#119115=DIRECTION('ref_axis',(0.685201414686299,0.72835363753598,0.));
#119116=DIRECTION('',(0.,0.,1.));
#119117=DIRECTION('center_axis',(-0.728350280645418,0.685204982963868,2.28597556927344E-6));
#119118=DIRECTION('ref_axis',(0.64863410361422,0.689477718317584,-0.322326349484735));
#119119=DIRECTION('',(0.,0.,-1.));
#119120=DIRECTION('center_axis',(-0.970868508445896,-0.239612894703187,
0.));
#119121=DIRECTION('ref_axis',(0.239612894703187,-0.970868508445896,0.));
#119122=DIRECTION('center_axis',(0.970868508445893,0.2396128947032,6.25973758918642E-15));
#119123=DIRECTION('ref_axis',(0.239291173764822,-0.969564952859012,-0.0518028604012878));
#119124=DIRECTION('',(0.,0.,1.));
#119125=DIRECTION('',(0.,0.,1.));
#119126=DIRECTION('center_axis',(0.,0.,1.));
#119127=DIRECTION('ref_axis',(0.967294863039036,-0.253654583909484,0.));
#119128=DIRECTION('center_axis',(0.,0.,-1.));
#119129=DIRECTION('ref_axis',(-0.967294863039036,0.253654583909484,0.));
#119130=DIRECTION('center_axis',(-0.851934693065667,0.467518109312524,-0.235868811452362));
#119131=DIRECTION('ref_axis',(0.491940391308073,0.560200059820671,-0.666461209956421));
#119132=DIRECTION('center_axis',(-0.971725974879091,0.0107020338878708,
0.235868811452347));
#119133=DIRECTION('ref_axis',(0.153736862270404,-0.729516574736984,0.666461209946437));
#119134=DIRECTION('center_axis',(0.,0.,-1.));
#119135=DIRECTION('ref_axis',(-0.967294863039033,0.253654583909494,0.));
#119136=DIRECTION('center_axis',(0.970809115627134,-0.239853415683961,-6.76296429840134E-17));
#119137=DIRECTION('ref_axis',(-0.239853415683961,-0.970809115627134,2.49600520792586E-31));
#119138=DIRECTION('center_axis',(0.,0.,1.));
#119139=DIRECTION('ref_axis',(0.967294863039033,-0.253654583909494,0.));
#119140=DIRECTION('center_axis',(0.963584421563631,-0.267404305350311,-1.38914942345546E-16));
#119141=DIRECTION('ref_axis',(0.267404305350311,0.963584421563631,-5.17689969051289E-31));
#119142=DIRECTION('center_axis',(0.,0.,-1.));
#119143=DIRECTION('ref_axis',(-0.967294863039033,0.253654583909495,0.));
#119144=DIRECTION('center_axis',(0.,0.,1.));
#119145=DIRECTION('ref_axis',(0.967294863039033,-0.253654583909495,0.));
#119146=DIRECTION('center_axis',(0.,0.,1.));
#119147=DIRECTION('ref_axis',(0.967294863039033,-0.253654583909495,0.));
#119148=DIRECTION('center_axis',(0.17924244347464,-0.726258259022274,0.663642288932205));
#119149=DIRECTION('ref_axis',(-0.180255246582584,-0.687391378337487,-0.703563173472534));
#119150=DIRECTION('center_axis',(0.179757959119013,-0.728347036028008,0.661209249211309));
#119151=DIRECTION('ref_axis',(-0.179670290433975,-0.685160687021283,-0.705884848750768));
#119152=DIRECTION('center_axis',(0.514039146524416,0.546412009931945,-0.661209249211308));
#119153=DIRECTION('ref_axis',(0.179670290433995,0.685160687021278,0.705884848750768));
#119154=DIRECTION('center_axis',(0.512564968562283,0.544844992033145,-0.663642288932184));
#119155=DIRECTION('ref_axis',(0.18025524658258,0.687391378337467,0.703563173472554));
#119156=DIRECTION('center_axis',(0.,0.,1.));
#119157=DIRECTION('ref_axis',(0.967294863039033,-0.253654583909495,0.));
#119158=DIRECTION('center_axis',(0.,0.,1.));
#119159=DIRECTION('ref_axis',(0.967294863039033,-0.253654583909495,0.));
#119160=DIRECTION('center_axis',(0.,0.,1.));
#119161=DIRECTION('ref_axis',(-0.967294863039023,0.253654583909532,0.));
#119162=DIRECTION('center_axis',(0.,0.,-1.));
#119163=DIRECTION('ref_axis',(0.967294863039033,-0.253654583909494,0.));
#119164=DIRECTION('center_axis',(0.682956151501933,-0.730459372672888,0.));
#119165=DIRECTION('ref_axis',(0.730459372672888,0.682956151501933,0.));
#119166=DIRECTION('',(0.,0.,1.));
#119167=DIRECTION('center_axis',(-0.68295257288816,0.730462718542307,2.28597555346301E-6));
#119168=DIRECTION('ref_axis',(0.691476404350399,0.646502982678044,-0.322326349551254));
#119169=DIRECTION('',(0.,0.,-1.));
#119170=DIRECTION('center_axis',(-0.984225805843822,-0.176916825404141,
0.));
#119171=DIRECTION('ref_axis',(0.176916825404141,-0.984225805843822,0.));
#119172=DIRECTION('center_axis',(0.98422580584382,0.176916825404152,4.71377209367484E-15));
#119173=DIRECTION('ref_axis',(0.176679284569281,-0.982904315821103,-0.0518028603875932));
#119174=DIRECTION('',(0.,0.,1.));
#119175=DIRECTION('',(0.,0.,1.));
#119176=DIRECTION('center_axis',(0.,0.,1.));
#119177=DIRECTION('ref_axis',(0.949055747010676,-0.315108218023599,0.));
#119178=DIRECTION('center_axis',(0.,0.,-1.));
#119179=DIRECTION('ref_axis',(-0.949055747010676,0.315108218023599,0.));
#119180=DIRECTION('center_axis',(-0.820230313760466,0.521141186409628,-0.23586881145241));
#119181=DIRECTION('ref_axis',(0.526821788086614,0.527530339649154,-0.666461209934135));
#119182=DIRECTION('center_axis',(-0.969043777980991,0.0729387423828848,
0.235868811452321));
#119183=DIRECTION('ref_axis',(0.106680705972949,-0.737867659286837,0.666461209937741));
#119184=DIRECTION('center_axis',(0.,0.,-1.));
#119185=DIRECTION('ref_axis',(-0.949055747010673,0.315108218023608,0.));
#119186=DIRECTION('center_axis',(0.95344702307413,-0.301560564714753,-6.76296429840134E-17));
#119187=DIRECTION('ref_axis',(-0.301560564714752,-0.953447023074129,4.31408307542741E-31));
#119188=DIRECTION('center_axis',(0.,0.,1.));
#119189=DIRECTION('ref_axis',(0.949055747010673,-0.315108218023608,0.));
#119190=DIRECTION('center_axis',(0.944471981357839,-0.328591960385517,-1.38914942345546E-16));
#119191=DIRECTION('ref_axis',(0.328591960385517,0.944471981357839,-5.54667823983524E-32));
#119192=DIRECTION('center_axis',(0.,0.,-1.));
#119193=DIRECTION('ref_axis',(-0.949055747010673,0.315108218023608,0.));
#119194=DIRECTION('center_axis',(0.,0.,1.));
#119195=DIRECTION('ref_axis',(0.949055747010673,-0.315108218023608,0.));
#119196=DIRECTION('center_axis',(0.,0.,1.));
#119197=DIRECTION('ref_axis',(0.949055747010673,-0.315108218023608,0.));
#119198=DIRECTION('center_axis',(0.132342644232462,-0.73625018632146,0.663642288932205));
#119199=DIRECTION('ref_axis',(-0.223926209669094,-0.674430065726974,-0.703563173472534));
#119200=DIRECTION('center_axis',(0.132723272292407,-0.738367700911553,0.661209249211309));
#119201=DIRECTION('ref_axis',(-0.223199534492288,-0.672241435874441,-0.705884848750768));
#119202=DIRECTION('center_axis',(0.547991735643799,0.512354746658518,-0.661209249211308));
#119203=DIRECTION('ref_axis',(0.223199534492304,0.672241435874438,0.705884848750766));
#119204=DIRECTION('center_axis',(0.546420187356905,0.510885399272378,-0.663642288932184));
#119205=DIRECTION('ref_axis',(0.223926209669088,0.674430065726956,0.703563173472553));
#119206=DIRECTION('center_axis',(0.,0.,1.));
#119207=DIRECTION('ref_axis',(0.949055747010673,-0.315108218023608,0.));
#119208=DIRECTION('center_axis',(0.,0.,1.));
#119209=DIRECTION('ref_axis',(0.949055747010673,-0.315108218023608,0.));
#119210=DIRECTION('center_axis',(0.,0.,1.));
#119211=DIRECTION('ref_axis',(-0.949055747010673,0.315108218023608,0.));
#119212=DIRECTION('center_axis',(0.,0.,-1.));
#119213=DIRECTION('ref_axis',(0.949055747010673,-0.315108218023608,0.));
#119214=DIRECTION('center_axis',(0.634752252147729,-0.772715716414119,0.));
#119215=DIRECTION('ref_axis',(0.772715716414119,0.634752252147729,0.));
#119216=DIRECTION('',(0.,0.,1.));
#119217=DIRECTION('center_axis',(-0.634748466516036,0.7727188261265,2.28597554464543E-6));
#119218=DIRECTION('ref_axis',(0.731477280222137,0.600871627613825,-0.32232634960167));
#119219=DIRECTION('',(0.,0.,-1.));
#119220=DIRECTION('center_axis',(-0.993538708289762,-0.11349376692097,0.));
#119221=DIRECTION('ref_axis',(0.11349376692097,-0.993538708289762,0.));
#119222=DIRECTION('center_axis',(0.993538708289754,0.113493766921037,4.01381961779349E-14));
#119223=DIRECTION('ref_axis',(0.113341382295796,-0.992204714116904,-0.0518028603792472));
#119224=DIRECTION('',(0.,0.,1.));
#119225=DIRECTION('',(0.,0.,1.));
#119226=DIRECTION('center_axis',(0.,0.,1.));
#119227=DIRECTION('ref_axis',(0.926916757346023,-0.375267004879372,0.));
#119228=DIRECTION('center_axis',(0.,0.,-1.));
#119229=DIRECTION('ref_axis',(-0.926916757346023,0.375267004879372,0.));
#119230=DIRECTION('center_axis',(-0.785155432156975,0.5726227825877,-0.235868811452283));
#119231=DIRECTION('ref_axis',(0.559538361126876,0.492692884129058,-0.666461209941013));
#119232=DIRECTION('center_axis',(-0.962379572339952,0.13487572994007,0.235868811452266));
#119233=DIRECTION('ref_axis',(0.059186175777223,-0.74318668733606,0.666461209946476));
#119234=DIRECTION('center_axis',(0.,0.,-1.));
#119235=DIRECTION('ref_axis',(-0.926916757346027,0.375267004879361,0.));
#119236=DIRECTION('center_axis',(0.932167012189569,-0.362028536700592,-6.76296429840134E-17));
#119237=DIRECTION('ref_axis',(-0.362028536700592,-0.932167012189569,3.6669706141133E-31));
#119238=DIRECTION('center_axis',(0.,0.,1.));
#119239=DIRECTION('ref_axis',(0.926916757346027,-0.375267004879361,0.));
#119240=DIRECTION('center_axis',(0.921478503192044,-0.388429360572744,-1.38914942345546E-16));
#119241=DIRECTION('ref_axis',(0.388429360572744,0.921478503192044,-5.91645678915759E-31));
#119242=DIRECTION('center_axis',(0.,0.,-1.));
#119243=DIRECTION('ref_axis',(-0.926916757346032,0.375267004879348,0.));
#119244=DIRECTION('center_axis',(0.,0.,1.));
#119245=DIRECTION('ref_axis',(0.926916757346034,-0.375267004879345,0.));
#119246=DIRECTION('center_axis',(0.,0.,1.));
#119247=DIRECTION('ref_axis',(0.926916757346032,-0.375267004879348,0.));
#119248=DIRECTION('center_axis',(0.084899020677726,-0.74321670367988,0.663642288932205));
#119249=DIRECTION('ref_axis',(-0.266677011928052,-0.658697375311594,-0.703563173472533));
#119250=DIRECTION('center_axis',(0.0851431970709001,-0.745354254532677,
0.661209249211309));
#119251=DIRECTION('ref_axis',(-0.265811603787226,-0.656559800472256,-0.705884848750768));
#119252=DIRECTION('center_axis',(0.579692509177563,0.476192107831323,-0.661209249211308));
#119253=DIRECTION('ref_axis',(0.265811603787246,0.656559800472247,0.705884848750769));
#119254=DIRECTION('center_axis',(0.578030048394914,0.474826468821427,-0.663642288932184));
#119255=DIRECTION('ref_axis',(0.266677011928042,0.658697375311578,0.703563173472553));
#119256=DIRECTION('center_axis',(0.,0.,1.));
#119257=DIRECTION('ref_axis',(0.926916757346032,-0.375267004879348,0.));
#119258=DIRECTION('center_axis',(0.,0.,1.));
#119259=DIRECTION('ref_axis',(0.926916757346032,-0.375267004879348,0.));
#119260=DIRECTION('center_axis',(0.,0.,1.));
#119261=DIRECTION('ref_axis',(-0.92691675734602,0.375267004879378,0.));
#119262=DIRECTION('center_axis',(0.,0.,-1.));
#119263=DIRECTION('ref_axis',(0.926916757346027,-0.375267004879361,0.));
#119264=DIRECTION('center_axis',(0.583940019635519,-0.811796805529604,0.));
#119265=DIRECTION('ref_axis',(0.811796805529604,0.583940019635519,0.));
#119266=DIRECTION('',(0.,0.,1.));
#119267=DIRECTION('center_axis',(-0.583936042541851,0.811799666306495,2.28597553788018E-6));
#119268=DIRECTION('ref_axis',(0.768472359063816,0.552771162159179,-0.322326349590107));
#119269=DIRECTION('',(0.,0.,-1.));
#119270=DIRECTION('center_axis',(-0.998768947069955,-0.0496043382051838,
0.));
#119271=DIRECTION('ref_axis',(0.0496043382051838,-0.998768947069955,0.));
#119272=DIRECTION('center_axis',(0.998768947069955,0.0496043382051736,2.70781072986654E-15));
#119273=DIRECTION('ref_axis',(0.0495377359703026,-0.997427930408881,-0.0518028604923819));
#119274=DIRECTION('',(0.,0.,1.));
#119275=DIRECTION('',(0.,0.,1.));
#119276=DIRECTION('center_axis',(0.,0.,1.));
#119277=DIRECTION('ref_axis',(0.900968867902423,-0.433883739117549,0.));
#119278=DIRECTION('center_axis',(0.,0.,-1.));
#119279=DIRECTION('ref_axis',(-0.900968867902423,0.433883739117549,0.));
#119280=DIRECTION('center_axis',(-0.746854178467622,0.621751348924587,-0.235868811452277));
#119281=DIRECTION('ref_axis',(0.589955671021752,0.455830847870496,-0.666461209943188));
#119282=DIRECTION('center_axis',(-0.951760742606293,0.196258484192558,0.23586881145238));
#119283=DIRECTION('ref_axis',(0.0114484368870036,-0.745451801882072,0.666461209946698));
#119284=DIRECTION('center_axis',(0.,0.,-1.));
#119285=DIRECTION('ref_axis',(-0.900968867902425,0.433883739117546,0.));
#119286=DIRECTION('center_axis',(0.907056527102724,-0.421008855774252,-6.76296429840134E-17));
#119287=DIRECTION('ref_axis',(-0.421008855774252,-0.907056527102724,-4.77630626208034E-31));
#119288=DIRECTION('center_axis',(0.,0.,1.));
#119289=DIRECTION('ref_axis',(0.900968867902425,-0.433883739117546,0.));
#119290=DIRECTION('center_axis',(0.894698472200112,-0.446670621199542,-1.38914942345546E-16));
#119291=DIRECTION('ref_axis',(0.446670621199542,0.894698472200112,1.0230539864585E-30));
#119292=DIRECTION('center_axis',(0.,0.,-1.));
#119293=DIRECTION('ref_axis',(-0.900968867902428,0.433883739117539,0.));
#119294=DIRECTION('center_axis',(0.,0.,1.));
#119295=DIRECTION('ref_axis',(0.900968867902428,-0.433883739117539,0.));
#119296=DIRECTION('center_axis',(0.,0.,1.));
#119297=DIRECTION('ref_axis',(0.900968867902428,-0.433883739117539,0.));
#119298=DIRECTION('center_axis',(0.0371065288362414,-0.747129184183397,
0.663642288932205));
#119299=DIRECTION('ref_axis',(-0.308331981142967,-0.640257956090913,-0.703563173472531));
#119300=DIRECTION('center_axis',(0.0372132501894693,-0.74927798764394,0.661209249211309));
#119301=DIRECTION('ref_axis',(-0.307331396185796,-0.638180220018293,-0.705884848750767));
#119302=DIRECTION('center_axis',(0.609011201847464,0.438072693490162,-0.661209249211308));
#119303=DIRECTION('ref_axis',(0.307331396185818,0.638180220018277,0.705884848750771));
#119304=DIRECTION('center_axis',(0.607264659977013,0.436816374560129,-0.663642288932184));
#119305=DIRECTION('ref_axis',(0.308331981142939,0.640257956090907,0.703563173472549));
#119306=DIRECTION('center_axis',(0.,0.,1.));
#119307=DIRECTION('ref_axis',(0.900968867902428,-0.433883739117539,0.));
#119308=DIRECTION('center_axis',(0.,0.,1.));
#119309=DIRECTION('ref_axis',(0.900968867902428,-0.433883739117539,0.));
#119310=DIRECTION('center_axis',(0.,0.,1.));
#119311=DIRECTION('ref_axis',(-0.900968867902391,0.433883739117616,0.));
#119312=DIRECTION('center_axis',(0.,0.,-1.));
#119313=DIRECTION('ref_axis',(0.900968867902425,-0.433883739117546,0.));
#119314=DIRECTION('center_axis',(0.530728252327885,-0.847542047441299,0.));
#119315=DIRECTION('ref_axis',(0.847542047441299,0.530728252327885,0.));
#119316=DIRECTION('',(0.,0.,1.));
#119317=DIRECTION('center_axis',(-0.530724100114921,0.847544647527186,2.28597557003377E-6));
#119318=DIRECTION('ref_axis',(0.802309620145797,0.502399241429844,-0.322326349577915));
#119319=DIRECTION('',(0.,0.,-1.));
#119320=DIRECTION('center_axis',(-0.99989503001137,0.0144889253763841,0.));
#119321=DIRECTION('ref_axis',(-0.0144889253763841,-0.99989503001137,0.));
#119322=DIRECTION('center_axis',(0.999895030011368,-0.0144889253764847,
-4.6873341868105E-14));
#119323=DIRECTION('ref_axis',(0.0144694715375623,0.998552501400717,0.05180286034375));
#119324=DIRECTION('',(0.,0.,1.));
#119325=DIRECTION('',(0.,0.,1.));
#119326=DIRECTION('center_axis',(0.,0.,1.));
#119327=DIRECTION('ref_axis',(0.871318704123387,-0.490717552003943,0.));
#119328=DIRECTION('center_axis',(0.,0.,-1.));
#119329=DIRECTION('ref_axis',(-0.871318704123387,0.490717552003943,0.));
#119330=DIRECTION('center_axis',(-0.705483940759205,0.668325005603511,-0.235868811452319));
#119331=DIRECTION('ref_axis',(0.61794872651875,0.417095704882099,-0.666461209946056));
#119332=DIRECTION('center_axis',(-0.937230923829315,0.256834770235852,0.235868811452352));
#119333=DIRECTION('ref_axis',(-0.0363363460779518,-0.744653695061158,0.666461209963091));
#119334=DIRECTION('center_axis',(0.,0.,-1.));
#119335=DIRECTION('ref_axis',(-0.871318704123396,0.490717552003926,0.));
#119336=DIRECTION('center_axis',(0.878218752183,-0.478259159153418,-6.76296429840134E-17));
#119337=DIRECTION('ref_axis',(-0.478259159153418,-0.878218752183,-8.62816615085482E-32));
#119338=DIRECTION('center_axis',(0.,0.,1.));
#119339=DIRECTION('ref_axis',(0.871318704123396,-0.490717552003926,0.));
#119340=DIRECTION('center_axis',(0.864241933273691,-0.503076416433282,-1.38914942345546E-16));
#119341=DIRECTION('ref_axis',(0.503076416433282,0.864241933273691,-4.31408307542741E-31));
#119342=DIRECTION('center_axis',(0.,0.,-1.));
#119343=DIRECTION('ref_axis',(-0.871318704123396,0.490717552003927,0.));
#119344=DIRECTION('center_axis',(0.,0.,1.));
#119345=DIRECTION('ref_axis',(0.871318704123396,-0.490717552003927,0.));
#119346=DIRECTION('center_axis',(0.,0.,1.));
#119347=DIRECTION('ref_axis',(0.871318704123396,-0.490717552003927,0.));
#119348=DIRECTION('center_axis',(-0.0108384416915561,-0.747971550610398,
0.663642288932205));
#119349=DIRECTION('ref_axis',(-0.348719948110342,-0.619187579593758,-0.703563173472534));
#119350=DIRECTION('center_axis',(-0.0108696139192065,-0.750122776784351,
0.661209249211309));
#119351=DIRECTION('ref_axis',(-0.347588297955049,-0.617178220151049,-0.705884848750768));
#119352=DIRECTION('center_axis',(0.63582733685648,0.398153144485152,-0.661209249211308));
#119353=DIRECTION('ref_axis',(0.347588297955068,0.617178220151039,0.705884848750768));
#119354=DIRECTION('center_axis',(0.634003890813404,0.397011308118946,-0.663642288932184));
#119355=DIRECTION('ref_axis',(0.348719948110339,0.619187579593737,0.703563173472554));
#119356=DIRECTION('center_axis',(0.,0.,1.));
#119357=DIRECTION('ref_axis',(0.871318704123396,-0.490717552003927,0.));
#119358=DIRECTION('center_axis',(0.,0.,1.));
#119359=DIRECTION('ref_axis',(0.871318704123396,-0.490717552003927,0.));
#119360=DIRECTION('center_axis',(0.,0.,1.));
#119361=DIRECTION('ref_axis',(-0.871318704123415,0.490717552003893,0.));
#119362=DIRECTION('center_axis',(0.,0.,-1.));
#119363=DIRECTION('ref_axis',(0.871318704123396,-0.490717552003926,0.));
#119364=DIRECTION('center_axis',(0.475335608790583,-0.879804557282858,0.));
#119365=DIRECTION('ref_axis',(0.879804557282858,0.475335608790583,0.));
#119366=DIRECTION('',(0.,0.,1.));
#119367=DIRECTION('center_axis',(-0.475331298520572,0.879806885993467,2.28597565699215E-6));
#119368=DIRECTION('ref_axis',(0.832850018902371,0.449962854451761,-0.322326349571275));
#119369=DIRECTION('',(0.,0.,-1.));
#119370=DIRECTION('center_axis',(-0.996912329797656,0.0785226508557165,
0.));
#119371=DIRECTION('ref_axis',(-0.0785226508557165,-0.996912329797657,0.));
#119372=DIRECTION('center_axis',(0.996912329797651,-0.0785226508557882,
-4.24618866466413E-14));
#119373=DIRECTION('ref_axis',(0.0784172208830047,0.99557380596211,0.0518028604529189));
#119374=DIRECTION('',(0.,0.,1.));
#119375=DIRECTION('',(0.,0.,1.));
#119376=DIRECTION('center_axis',(0.,0.,1.));
#119377=DIRECTION('ref_axis',(0.83808810489185,-0.545534901210534,0.));
#119378=DIRECTION('center_axis',(0.,0.,-1.));
#119379=DIRECTION('ref_axis',(-0.83808810489185,0.545534901210534,0.));
#119380=DIRECTION('center_axis',(-0.66121471821246,0.712152371479069,-0.235868811452374));
#119381=DIRECTION('ref_axis',(0.64340249813794,0.376646626159565,-0.666461209968348));
#119382=DIRECTION('center_axis',(-0.918849822150842,0.316355667117557,0.235868811452406));
#119383=DIRECTION('ref_axis',(-0.0839718152189302,-0.740795646508069,0.666461209946633));
#119384=DIRECTION('center_axis',(0.,0.,-1.));
#119385=DIRECTION('ref_axis',(-0.838088104891848,0.545534901210538,0.));
#119386=DIRECTION('center_axis',(0.845772188033224,-0.533544193061356,-6.76296429840134E-17));
#119387=DIRECTION('ref_axis',(-0.533544193061356,-0.845772188033224,-4.93038065763132E-32));
#119388=DIRECTION('center_axis',(0.,0.,1.));
#119389=DIRECTION('ref_axis',(0.838088104891848,-0.545534901210538,0.));
#119390=DIRECTION('center_axis',(0.830234038864134,-0.557414962762346,-1.38914942345546E-16));
#119391=DIRECTION('ref_axis',(0.557414962762346,0.830234038864134,1.72563323017096E-30));
#119392=DIRECTION('center_axis',(0.,0.,-1.));
#119393=DIRECTION('ref_axis',(-0.838088104891851,0.545534901210533,0.));
#119394=DIRECTION('center_axis',(0.,0.,1.));
#119395=DIRECTION('ref_axis',(0.838088104891851,-0.545534901210533,0.));
#119396=DIRECTION('center_axis',(0.,0.,1.));
#119397=DIRECTION('ref_axis',(0.838088104891851,-0.545534901210533,0.));
#119398=DIRECTION('center_axis',(-0.058738874737605,-0.745740341496545,
0.663642288932205));
#119399=DIRECTION('ref_axis',(-0.387674950010748,-0.595572828516731,-0.703563173472535));
#119400=DIRECTION('center_axis',(-0.0589078124527641,-0.747885150534123,
0.661209249211309));
#119401=DIRECTION('ref_axis',(-0.38641688485055,-0.593640102592892,-0.70588484875077));
#119402=DIRECTION('center_axis',(0.660030720953817,0.356597498805871,-0.661209249211308));
#119403=DIRECTION('ref_axis',(0.386416884850569,0.593640102592884,0.705884848750766));
#119404=DIRECTION('center_axis',(0.658137863669036,0.355574837054044,-0.663642288932184));
#119405=DIRECTION('ref_axis',(0.387674950010745,0.595572828516711,0.703563173472554));
#119406=DIRECTION('center_axis',(0.,0.,1.));
#119407=DIRECTION('ref_axis',(0.838088104891851,-0.545534901210533,0.));
#119408=DIRECTION('center_axis',(0.,0.,1.));
#119409=DIRECTION('ref_axis',(0.838088104891851,-0.545534901210533,0.));
#119410=DIRECTION('center_axis',(0.,0.,1.));
#119411=DIRECTION('ref_axis',(-0.838088104891867,0.545534901210509,0.));
#119412=DIRECTION('center_axis',(0.,0.,-1.));
#119413=DIRECTION('ref_axis',(0.838088104891848,-0.545534901210538,0.));
#119414=DIRECTION('center_axis',(0.417989709277592,-0.908451761481056,0.));
#119415=DIRECTION('ref_axis',(0.908451761481056,0.417989709277592,0.));
#119416=DIRECTION('',(0.,0.,1.));
#119417=DIRECTION('center_axis',(-0.41798525866263,0.908453809247068,2.28597557900283E-6));
#119418=DIRECTION('ref_axis',(0.859968058305883,0.395677473597326,-0.322326349498837));
#119419=DIRECTION('',(0.,0.,-1.));
#119420=DIRECTION('center_axis',(-0.989833102983781,0.142233709919626,0.));
#119421=DIRECTION('ref_axis',(-0.142233709919626,-0.989833102983781,0.));
#119422=DIRECTION('center_axis',(0.989833102983778,-0.142233709919645,-2.73152185709842E-15));
#119423=DIRECTION('ref_axis',(0.142042737047654,0.988504084211958,0.051802860425751));
#119424=DIRECTION('',(0.,0.,1.));
#119425=DIRECTION('',(0.,0.,1.));
#119426=DIRECTION('center_axis',(0.,0.,1.));
#119427=DIRECTION('ref_axis',(0.801413621867962,-0.59811053049121,0.));
#119428=DIRECTION('center_axis',(0.,0.,-1.));
#119429=DIRECTION('ref_axis',(-0.801413621867962,0.59811053049121,0.));
#119430=DIRECTION('center_axis',(-0.614228422558396,0.753053350504116,-0.235868811452362));
#119431=DIRECTION('ref_axis',(0.666212390911554,0.334649825702797,-0.666461209938732));
#119432=DIRECTION('center_axis',(-0.896692969460608,0.374576590704729,0.235868811452338));
#119433=DIRECTION('ref_axis',(-0.131262226158804,-0.733893509739356,0.666461209933695));
#119434=DIRECTION('center_axis',(0.,0.,-1.));
#119435=DIRECTION('ref_axis',(-0.801413621867964,0.598110530491206,0.));
#119436=DIRECTION('center_axis',(0.809850164545254,-0.586636779435134,-6.76296429840134E-17));
#119437=DIRECTION('ref_axis',(-0.586636779435134,-0.809850164545254,-1.04770588974666E-31));
#119438=DIRECTION('center_axis',(0.,0.,1.));
#119439=DIRECTION('ref_axis',(0.801413621867964,-0.598110530491206,0.));
#119440=DIRECTION('center_axis',(0.792814534704242,-0.609462971444285,-1.38914942345546E-16));
#119441=DIRECTION('ref_axis',(0.609462971444284,0.792814534704242,-1.01072803481442E-30));
#119442=DIRECTION('center_axis',(0.,0.,-1.));
#119443=DIRECTION('ref_axis',(-0.801413621867966,0.598110530491204,0.));
#119444=DIRECTION('center_axis',(0.,0.,1.));
#119445=DIRECTION('ref_axis',(0.801413621867966,-0.598110530491204,0.));
#119446=DIRECTION('center_axis',(0.,0.,1.));
#119447=DIRECTION('ref_axis',(0.801413621867966,-0.598110530491204,0.));
#119448=DIRECTION('center_axis',(-0.106397937147908,-0.740444725358682,
0.663642288932205));
#119449=DIRECTION('ref_axis',(-0.425036912385557,-0.569510740937353,-0.703563173472532));
#119450=DIRECTION('center_axis',(-0.106703946149267,-0.742574303779488,
0.661209249211309));
#119451=DIRECTION('ref_axis',(-0.423657601880047,-0.567662590517776,-0.705884848750769));
#119452=DIRECTION('center_axis',(0.681521897242608,0.313576517514073,-0.661209249211308));
#119453=DIRECTION('ref_axis',(0.423657601880068,0.56766259051776,0.705884848750769));
#119454=DIRECTION('center_axis',(0.679567406872722,0.312677232713123,-0.663642288932184));
#119455=DIRECTION('ref_axis',(0.425036912385534,0.569510740937346,0.703563173472551));
#119456=DIRECTION('center_axis',(0.,0.,1.));
#119457=DIRECTION('ref_axis',(0.801413621867966,-0.598110530491204,0.));
#119458=DIRECTION('center_axis',(0.,0.,1.));
#119459=DIRECTION('ref_axis',(0.801413621867966,-0.598110530491204,0.));
#119460=DIRECTION('center_axis',(0.,0.,1.));
#119461=DIRECTION('ref_axis',(-0.801413621867943,0.598110530491235,0.));
#119462=DIRECTION('center_axis',(0.,0.,-1.));
#119463=DIRECTION('ref_axis',(0.801413621867964,-0.598110530491206,0.));
#119464=DIRECTION('center_axis',(0.358926200390668,-0.933365942529037,0.));
#119465=DIRECTION('ref_axis',(0.933365942529037,0.358926200390668,0.));
#119466=DIRECTION('',(0.,0.,1.));
#119467=DIRECTION('center_axis',(-0.358921627719167,0.933367700935809,2.28597557391108E-6));
#119468=DIRECTION('ref_axis',(0.883552304462217,0.339766169115136,-0.322326349534645));
#119469=DIRECTION('',(0.,0.,-1.));
#119470=DIRECTION('center_axis',(-0.97868643963121,0.205360300160442,0.));
#119471=DIRECTION('ref_axis',(-0.205360300160442,-0.97868643963121,0.));
#119472=DIRECTION('center_axis',(0.978686439631201,-0.205360300160485,-1.98414712675372E-14));
#119473=DIRECTION('ref_axis',(0.205084569137981,0.977372387146371,0.0518028603968221));
#119474=DIRECTION('',(0.,0.,1.));
#119475=DIRECTION('',(0.,0.,1.));
#119476=DIRECTION('center_axis',(0.,0.,1.));
#119477=DIRECTION('ref_axis',(0.761445958369139,-0.648228395307783,0.));
#119478=DIRECTION('center_axis',(0.,0.,-1.));
#119479=DIRECTION('ref_axis',(-0.761445958369139,0.648228395307783,0.));
#119480=DIRECTION('center_axis',(-0.564718130564452,0.790859871782495,-0.235868811452398));
#119481=DIRECTION('ref_axis',(0.686284674041221,0.291277877291778,-0.666461209956387));
#119482=DIRECTION('center_axis',(-0.870851413018789,0.431258298734362,0.235868811452302));
#119483=DIRECTION('ref_axis',(-0.178013252440605,-0.723975647099069,0.666461209946237));
#119484=DIRECTION('center_axis',(0.,0.,-1.));
#119485=DIRECTION('ref_axis',(-0.761445958369143,0.648228395307779,0.));
#119486=DIRECTION('center_axis',(0.770600293018851,-0.637318749449018,-6.76296429840134E-17));
#119487=DIRECTION('ref_axis',(-0.637318749449018,-0.770600293018851,-5.73156751449641E-31));
#119488=DIRECTION('center_axis',(0.,0.,1.));
#119489=DIRECTION('ref_axis',(0.761445958369143,-0.648228395307779,0.));
#119490=DIRECTION('center_axis',(0.752137185563065,-0.659006566047161,-1.38914942345546E-16));
#119491=DIRECTION('ref_axis',(0.659006566047161,0.752137185563065,2.2186712959341E-31));
#119492=DIRECTION('center_axis',(0.,0.,-1.));
#119493=DIRECTION('ref_axis',(-0.761445958369147,0.648228395307773,0.));
#119494=DIRECTION('center_axis',(0.,0.,1.));
#119495=DIRECTION('ref_axis',(0.761445958369147,-0.648228395307773,0.));
#119496=DIRECTION('center_axis',(0.,0.,1.));
#119497=DIRECTION('ref_axis',(0.761445958369147,-0.648228395307773,0.));
#119498=DIRECTION('center_axis',(-0.153619787612184,-0.732106463019424,
0.663642288932205));
#119499=DIRECTION('ref_axis',(-0.460652306917222,-0.5411084115638,-0.703563173472534));
#119500=DIRECTION('center_axis',(-0.154061610443117,-0.734212059928935,
0.661209249211309));
#119501=DIRECTION('ref_axis',(-0.459157418949154,-0.539352431094975,-0.705884848750766));
#119502=DIRECTION('center_axis',(0.700212553869642,0.269266983049857,-0.661209249211308));
#119503=DIRECTION('ref_axis',(0.45915741894917,0.539352431094954,0.705884848750772));
#119504=DIRECTION('center_axis',(0.698204461834817,0.268494770553928,-0.663642288932184));
#119505=DIRECTION('ref_axis',(0.460652306917214,0.54110841156378,0.703563173472555));
#119506=DIRECTION('center_axis',(0.,0.,1.));
#119507=DIRECTION('ref_axis',(0.761445958369147,-0.648228395307773,0.));
#119508=DIRECTION('center_axis',(0.,0.,1.));
#119509=DIRECTION('ref_axis',(0.761445958369147,-0.648228395307773,0.));
#119510=DIRECTION('center_axis',(0.,0.,1.));
#119511=DIRECTION('ref_axis',(-0.761445958369123,0.648228395307802,0.));
#119512=DIRECTION('center_axis',(0.,0.,-1.));
#119513=DIRECTION('ref_axis',(0.761445958369143,-0.648228395307779,0.));
#119514=DIRECTION('center_axis',(0.29838778675691,-0.9544447227128,0.));
#119515=DIRECTION('ref_axis',(0.9544447227128,0.29838778675691,0.));
#119516=DIRECTION('',(0.,0.,1.));
#119517=DIRECTION('center_axis',(-0.298383110818907,0.954446184534679,2.2859755847042E-6));
#119518=DIRECTION('ref_axis',(0.903505844681347,0.282458692567024,-0.322326349558911));
#119519=DIRECTION('',(0.,0.,-1.));
#119520=DIRECTION('center_axis',(-0.963518143770611,0.267643020878251,0.));
#119521=DIRECTION('ref_axis',(-0.267643020878251,-0.963518143770611,0.));
#119522=DIRECTION('center_axis',(0.963518143770624,-0.267643020878204,2.53424527853122E-14));
#119523=DIRECTION('ref_axis',(0.267283664743288,0.962224457296271,0.0518028603678789));
#119524=DIRECTION('',(0.,0.,1.));
#119525=DIRECTION('',(0.,0.,1.));
#119526=DIRECTION('center_axis',(0.,0.,1.));
#119527=DIRECTION('ref_axis',(0.718349350097745,-0.695682550603468,0.));
#119528=DIRECTION('center_axis',(0.,0.,-1.));
#119529=DIRECTION('ref_axis',(-0.718349350097745,0.695682550603468,0.));
#119530=DIRECTION('center_axis',(-0.512887290640128,0.825416580209004,-0.235868811452262));
#119531=DIRECTION('ref_axis',(0.703536866256498,0.246709005626625,-0.666461209944516));
#119532=DIRECTION('center_axis',(-0.841431341323772,0.486167873909974,0.235868811452326));
#119533=DIRECTION('ref_axis',(-0.224032784085981,-0.711082813236446,0.666461209954807));
#119534=DIRECTION('center_axis',(0.,0.,-1.));
#119535=DIRECTION('ref_axis',(-0.718349350097736,0.695682550603477,0.));
#119536=DIRECTION('center_axis',(0.72818385959519,-0.685381840016973,-6.76296429840134E-17));
#119537=DIRECTION('ref_axis',(-0.685381840016973,-0.72818385959519,6.93889390390717E-14));
#119538=DIRECTION('center_axis',(0.,0.,1.));
#119539=DIRECTION('ref_axis',(0.718349350097736,-0.695682550603477,0.));
#119540=DIRECTION('center_axis',(0.70836914339349,-0.705842161313684,-1.38914942345546E-16));
#119541=DIRECTION('ref_axis',(0.705842161313684,0.70836914339349,3.32800694390114E-31));
#119542=DIRECTION('center_axis',(0.,0.,-1.));
#119543=DIRECTION('ref_axis',(-0.718349350097744,0.69568255060347,0.));
#119544=DIRECTION('center_axis',(0.,0.,1.));
#119545=DIRECTION('ref_axis',(0.718349350097744,-0.69568255060347,0.));
#119546=DIRECTION('center_axis',(0.,0.,1.));
#119547=DIRECTION('ref_axis',(0.718349350097744,-0.69568255060347,0.));
#119548=DIRECTION('center_axis',(-0.20021038141782,-0.720759818187276,0.663642288932205));
#119549=DIRECTION('ref_axis',(-0.494374782310168,-0.510482551659734,-0.703563173472532));
#119550=DIRECTION('center_axis',(-0.200786202533545,-0.722832781236141,
0.661209249211309));
#119551=DIRECTION('ref_axis',(-0.492770459694828,-0.508825956842077,-0.705884848750767));
#119552=DIRECTION('center_axis',(0.716025886917703,0.223850972794703,-0.661209249211308));
#119553=DIRECTION('ref_axis',(0.492770459694841,0.508825956842061,0.705884848750769));
#119554=DIRECTION('center_axis',(0.713972444898844,0.223209005790579,-0.663642288932184));
#119555=DIRECTION('ref_axis',(0.494374782310151,0.510482551659721,0.703563173472554));
#119556=DIRECTION('center_axis',(0.,0.,1.));
#119557=DIRECTION('ref_axis',(0.718349350097735,-0.695682550603479,0.));
#119558=DIRECTION('center_axis',(0.,0.,1.));
#119559=DIRECTION('ref_axis',(0.718349350097735,-0.695682550603479,0.));
#119560=DIRECTION('center_axis',(0.,0.,1.));
#119561=DIRECTION('ref_axis',(-0.718349350097761,0.695682550603452,0.));
#119562=DIRECTION('center_axis',(0.,0.,-1.));
#119563=DIRECTION('ref_axis',(0.718349350097736,-0.695682550603478,0.));
#119564=DIRECTION('center_axis',(0.236623233703389,-0.971601484803184,0.));
#119565=DIRECTION('ref_axis',(0.971601484803184,0.236623233703389,0.));
#119566=DIRECTION('',(0.,0.,1.));
#119567=DIRECTION('center_axis',(-0.236618473713347,0.971602644033218,2.28597559428171E-6));
#119568=DIRECTION('ref_axis',(0.919746685602177,0.223990532669675,-0.322326349525081));
#119569=DIRECTION('',(0.,0.,-1.));
#119570=DIRECTION('center_axis',(-0.944390545183265,0.328825939014024,0.));
#119571=DIRECTION('ref_axis',(-0.328825939014024,-0.944390545183266,0.));
#119572=DIRECTION('center_axis',(0.944390545183307,-0.328825939013906,4.97743982849312E-14));
#119573=DIRECTION('ref_axis',(0.328384434437419,0.943122540752338,0.0518028603850272));
#119574=DIRECTION('',(0.,0.,1.));
#119575=DIRECTION('',(0.,0.,1.));
#119576=DIRECTION('center_axis',(0.,0.,1.));
#119577=DIRECTION('ref_axis',(0.672300890261307,-0.740277997075324,0.));
#119578=DIRECTION('center_axis',(0.,0.,-1.));
#119579=DIRECTION('ref_axis',(-0.672300890261307,0.740277997075324,0.));
#119580=DIRECTION('center_axis',(-0.458948886825295,0.856581474855607,-0.235868811452501));
#119581=DIRECTION('ref_axis',(0.717898074561625,0.201126353720061,-0.666461209958978));
#119582=DIRECTION('center_axis',(-0.808553647760812,0.539079681008978,0.235868811452348));
#119583=DIRECTION('ref_axis',(-0.269131716978108,-0.695267987579348,0.66646120994682));
#119584=DIRECTION('center_axis',(0.,0.,-1.));
#119585=DIRECTION('ref_axis',(-0.672300890261326,0.740277997075307,0.));
#119586=DIRECTION('center_axis',(0.682775162497505,-0.730628549590355,-6.76296429840134E-17));
#119587=DIRECTION('ref_axis',(-0.730628549590355,-0.682775162497505,-7.33394122822659E-31));
#119588=DIRECTION('center_axis',(0.,0.,1.));
#119589=DIRECTION('ref_axis',(0.672300890261326,-0.740277997075307,0.));
#119590=DIRECTION('center_axis',(0.661690260469006,-0.749777299736701,-1.38914942345546E-16));
#119591=DIRECTION('ref_axis',(0.749777299736701,0.661690260469006,-1.04770588974666E-30));
#119592=DIRECTION('center_axis',(0.,0.,-1.));
#119593=DIRECTION('ref_axis',(-0.672300890261324,0.740277997075309,0.));
#119594=DIRECTION('center_axis',(0.,0.,1.));
#119595=DIRECTION('ref_axis',(0.672300890261324,-0.740277997075309,0.));
#119596=DIRECTION('center_axis',(0.,0.,1.));
#119597=DIRECTION('ref_axis',(0.672300890261324,-0.740277997075309,0.));
#119598=DIRECTION('center_axis',(-0.245978267821218,-0.7064514166597,0.663642288932205));
#119599=DIRECTION('ref_axis',(-0.52606576567953,-0.477759009452743,-0.703563173472534));
#119600=DIRECTION('center_axis',(-0.246685721049257,-0.708483227598103,
0.661209249211309));
#119601=DIRECTION('ref_axis',(-0.524358600922692,-0.476208607589685,-0.705884848750766));
#119602=DIRECTION('center_axis',(0.728896916009348,0.177515110876453,-0.661209249211308));
#119603=DIRECTION('ref_axis',(0.524358600922699,0.476208607589672,0.705884848750769));
#119604=DIRECTION('center_axis',(0.726806562040174,0.177006027344255,-0.663642288932184));
#119605=DIRECTION('ref_axis',(0.526065765679518,0.47775900945273,0.703563173472553));
#119606=DIRECTION('center_axis',(0.,0.,1.));
#119607=DIRECTION('ref_axis',(0.672300890261324,-0.740277997075309,0.));
#119608=DIRECTION('center_axis',(0.,0.,1.));
#119609=DIRECTION('ref_axis',(0.672300890261324,-0.740277997075309,0.));
#119610=DIRECTION('center_axis',(0.,0.,1.));
#119611=DIRECTION('ref_axis',(-0.672300890261287,0.740277997075342,0.));
#119612=DIRECTION('center_axis',(0.,0.,-1.));
#119613=DIRECTION('ref_axis',(0.672300890261326,-0.740277997075307,0.));
#119614=DIRECTION('center_axis',(0.173886345027055,-0.984765727984647,0.));
#119615=DIRECTION('ref_axis',(0.984765727984647,0.173886345027055,0.));
#119616=DIRECTION('',(0.,0.,1.));
#119617=DIRECTION('center_axis',(-0.173881520544928,0.984766579859287,2.28597550967989E-6));
#119618=DIRECTION('ref_axis',(0.932208090064288,0.164601947618861,-0.322326349619095));
#119619=DIRECTION('',(0.,0.,-1.));
#119620=DIRECTION('center_axis',(-0.921382243274625,0.388657640833446,0.));
#119621=DIRECTION('ref_axis',(-0.388657640833446,-0.921382243274625,0.));
#119622=DIRECTION('center_axis',(0.92138224327465,-0.388657640833387,2.24022730085659E-14));
#119623=DIRECTION('ref_axis',(0.388135802052356,0.920145131389595,0.0518028603959105));
#119624=DIRECTION('',(0.,0.,1.));
#119625=DIRECTION('',(0.,0.,1.));
#119626=DIRECTION('center_axis',(0.,0.,1.));
#119627=DIRECTION('ref_axis',(0.623489801858758,-0.781831482468011,0.));
#119628=DIRECTION('center_axis',(0.,0.,-1.));
#119629=DIRECTION('ref_axis',(-0.623489801858758,0.781831482468011,0.));
#119630=DIRECTION('center_axis',(-0.403124563589482,0.884226492486425,-0.235868811452349));
#119631=DIRECTION('ref_axis',(0.729309285704228,0.154717230497998,-0.666461209953451));
#119632=DIRECTION('center_axis',(-0.772353433824917,0.589776294066571,0.235868811452385));
#119633=DIRECTION('ref_axis',(-0.313124729919898,-0.676596156628014,0.666461209935575));
#119634=DIRECTION('center_axis',(0.,0.,-1.));
#119635=DIRECTION('ref_axis',(-0.623489801858743,0.781831482468022,0.));
#119636=DIRECTION('center_axis',(0.634560795802304,-0.772872949734138,-6.76296429840134E-17));
#119637=DIRECTION('ref_axis',(-0.772872949734138,-0.634560795802304,9.86076131526265E-31));
#119638=DIRECTION('center_axis',(0.,0.,1.));
#119639=DIRECTION('ref_axis',(0.623489801858743,-0.781831482468022,0.));
#119640=DIRECTION('center_axis',(0.612292350332139,-0.790631442408374,-1.38914942345546E-16));
#119641=DIRECTION('ref_axis',(0.790631442408374,0.612292350332139,4.43734259186819E-31));
#119642=DIRECTION('center_axis',(0.,0.,-1.));
#119643=DIRECTION('ref_axis',(-0.623489801858737,0.781831482468027,0.));
#119644=DIRECTION('center_axis',(0.,0.,1.));
#119645=DIRECTION('ref_axis',(0.623489801858737,-0.781831482468027,0.));
#119646=DIRECTION('center_axis',(0.,0.,1.));
#119647=DIRECTION('ref_axis',(0.623489801858737,-0.781831482468027,0.));
#119648=DIRECTION('center_axis',(-0.290735376759967,-0.689240054727715,
0.663642288932205));
#119649=DIRECTION('ref_axis',(-0.55559503197698,-0.443072252996912,-0.703563173472531));
#119650=DIRECTION('center_axis',(-0.291571555023257,-0.691222364408688,
0.661209249211309));
#119651=DIRECTION('ref_axis',(-0.553792040184789,-0.441634415022285,-0.705884848750767));
#119652=DIRECTION('center_axis',(0.738772751325213,0.130449801290739,-0.661209249211308));
#119653=DIRECTION('ref_axis',(0.553792040184798,0.441634415022272,0.705884848750768));
#119654=DIRECTION('center_axis',(0.736654075118561,0.130075693163899,-0.663642288932184));
#119655=DIRECTION('ref_axis',(0.555595031976954,0.443072252996912,0.703563173472551));
#119656=DIRECTION('center_axis',(0.,0.,1.));
#119657=DIRECTION('ref_axis',(0.623489801858737,-0.781831482468027,0.));
#119658=DIRECTION('center_axis',(0.,0.,1.));
#119659=DIRECTION('ref_axis',(0.623489801858737,-0.781831482468027,0.));
#119660=DIRECTION('center_axis',(0.,0.,1.));
#119661=DIRECTION('ref_axis',(-0.623489801858669,0.781831482468081,0.));
#119662=DIRECTION('center_axis',(0.,0.,-1.));
#119663=DIRECTION('ref_axis',(0.623489801858743,-0.781831482468022,0.));
#119664=DIRECTION('center_axis',(0.110434920060502,-0.993883357558235,0.));
#119665=DIRECTION('ref_axis',(0.993883357558235,0.110434920060502,0.));
#119666=DIRECTION('',(0.,0.,1.));
#119667=DIRECTION('center_axis',(-0.110430050910949,0.993883898576981,2.2859755452158E-6));
#119668=DIRECTION('ref_axis',(0.940838851613951,0.104536977872,-0.322326349452121));
#119669=DIRECTION('',(0.,0.,-1.));
#119670=DIRECTION('center_axis',(-0.894587784092498,0.44689226503988,0.));
#119671=DIRECTION('ref_axis',(-0.44689226503988,-0.894587784092498,0.));
#119672=DIRECTION('center_axis',(0.894587784092481,-0.446892265039914,-4.03278851957784E-14));
#119673=DIRECTION('ref_axis',(0.446292236401178,0.893386648310297,0.0518028604319265));
#119674=DIRECTION('',(0.,0.,1.));
#119675=DIRECTION('',(0.,0.,1.));
#119676=DIRECTION('center_axis',(0.,0.,1.));
#119677=DIRECTION('ref_axis',(0.572116660122175,-0.820172254596952,0.));
#119678=DIRECTION('center_axis',(0.,0.,-1.));
#119679=DIRECTION('ref_axis',(-0.572116660122175,0.820172254596952,0.));
#119680=DIRECTION('center_axis',(-0.345643715052168,0.908238033793455,-0.235868811452328));
#119681=DIRECTION('ref_axis',(0.737723608568493,0.107672340997408,-0.666461209932595));
#119682=DIRECTION('center_axis',(-0.732979453960528,0.638049389824842,0.235868811452201));
#119683=DIRECTION('ref_axis',(-0.355831046170335,-0.655144046930467,0.666461209938654));
#119684=DIRECTION('center_axis',(0.,0.,-1.));
#119685=DIRECTION('ref_axis',(-0.57211666012218,0.820172254596949,0.));
#119686=DIRECTION('center_axis',(0.583738882684287,-0.811941449146735,-6.76296429840134E-17));
#119687=DIRECTION('ref_axis',(-0.811941449146735,-0.583738882684287,-4.80712114119054E-31));
#119688=DIRECTION('center_axis',(0.,0.,1.));
#119689=DIRECTION('ref_axis',(0.57211666012218,-0.820172254596949,0.));
#119690=DIRECTION('center_axis',(0.56037839959146,-0.828236710893277,-1.38914942345546E-16));
#119691=DIRECTION('ref_axis',(0.828236710893277,0.56037839959146,1.45446229400124E-30));
#119692=DIRECTION('center_axis',(0.,0.,-1.));
#119693=DIRECTION('ref_axis',(-0.572116660122189,0.820172254596943,0.));
#119694=DIRECTION('center_axis',(0.,0.,1.));
#119695=DIRECTION('ref_axis',(0.572116660122189,-0.820172254596943,0.));
#119696=DIRECTION('center_axis',(0.,0.,1.));
#119697=DIRECTION('ref_axis',(0.572116660122189,-0.820172254596943,0.));
#119698=DIRECTION('center_axis',(-0.334297791673065,-0.669196457569327,
0.663642288932205));
#119699=DIRECTION('ref_axis',(-0.582841239113249,-0.406564817614837,-0.703563173472537));
#119700=DIRECTION('center_axis',(-0.335259258935764,-0.671121120257186,
0.661209249211309));
#119701=DIRECTION('ref_axis',(-0.580949829165753,-0.40524545191327,-0.705884848750766));
#119702=DIRECTION('center_axis',(0.745612810939624,0.0828484454901269,-0.661209249211308));
#119703=DIRECTION('ref_axis',(0.580949829165761,0.405245451913251,0.70588484875077));
#119704=DIRECTION('center_axis',(0.743474518590483,0.082610850059185,-0.663642288932184));
#119705=DIRECTION('ref_axis',(0.582841239113242,0.406564817614819,0.703563173472553));
#119706=DIRECTION('center_axis',(0.,0.,1.));
#119707=DIRECTION('ref_axis',(0.572116660122189,-0.820172254596943,0.));
#119708=DIRECTION('center_axis',(0.,0.,1.));
#119709=DIRECTION('ref_axis',(0.572116660122189,-0.820172254596943,0.));
#119710=DIRECTION('center_axis',(0.,0.,1.));
#119711=DIRECTION('ref_axis',(-0.572116660122197,0.820172254596937,0.));
#119712=DIRECTION('center_axis',(0.,0.,-1.));
#119713=DIRECTION('ref_axis',(0.57211666012218,-0.820172254596949,0.));
#119714=DIRECTION('center_axis',(0.0465296943192034,-0.998916907228305,
0.));
#119715=DIRECTION('ref_axis',(0.998916907228305,0.0465296943192034,0.));
#119716=DIRECTION('',(0.,0.,1.));
#119717=DIRECTION('center_axis',(-0.0465248005107585,0.998917135167982,
2.28597549106619E-6));
#119718=DIRECTION('ref_axis',(0.945603504432372,0.0440424432490359,-0.322326349524629));
#119719=DIRECTION('',(0.,0.,-1.));
#119720=DIRECTION('center_axis',(-0.864117271817056,0.503290513071176,0.));
#119721=DIRECTION('ref_axis',(-0.503290513071176,-0.864117271817056,0.));
#119722=DIRECTION('center_axis',(0.864117271817016,-0.503290513071245,-2.23453663032148E-14));
#119723=DIRECTION('ref_axis',(0.502614760223022,0.862957047865909,0.0518028603892732));
#119724=DIRECTION('',(0.,0.,1.));
#119725=DIRECTION('',(0.,0.,1.));
#119726=DIRECTION('center_axis',(0.,0.,1.));
#119727=DIRECTION('ref_axis',(0.518392568310538,-0.855142763005338,0.));
#119728=DIRECTION('center_axis',(0.,0.,-1.));
#119729=DIRECTION('ref_axis',(-0.518392568310538,0.855142763005338,0.));
#119730=DIRECTION('center_axis',(-0.286742542349322,0.92851743020319,-0.235868811452281));
#119731=DIRECTION('ref_axis',(0.743106466860159,0.0601850027344822,-0.66646120994133));
#119732=DIRECTION('center_axis',(-0.690593504295639,0.683700603779688,0.235868811452381));
#119733=DIRECTION('ref_axis',(-0.39707517632656,-0.630999809816269,0.666461209941782));
#119734=DIRECTION('center_axis',(0.,0.,-1.));
#119735=DIRECTION('ref_axis',(-0.518392568310535,0.85514276300534,0.));
#119736=DIRECTION('center_axis',(0.530518261285723,-0.847673506983894,-6.76296429840134E-17));
#119737=DIRECTION('ref_axis',(-0.847673506983894,-0.530518261285723,6.93889390390721E-14));
#119738=DIRECTION('center_axis',(0.,0.,1.));
#119739=DIRECTION('ref_axis',(0.518392568310535,-0.85514276300534,0.));
#119740=DIRECTION('center_axis',(0.50616173380607,-0.862438577076903,-1.38914942345546E-16));
#119741=DIRECTION('ref_axis',(0.862438577076903,0.50616173380607,-2.46519032881566E-31));
#119742=DIRECTION('center_axis',(0.,0.,-1.));
#119743=DIRECTION('ref_axis',(-0.518392568310539,0.855142763005338,0.));
#119744=DIRECTION('center_axis',(0.,0.,1.));
#119745=DIRECTION('ref_axis',(0.518392568310539,-0.855142763005338,0.));
#119746=DIRECTION('center_axis',(0.,0.,1.));
#119747=DIRECTION('ref_axis',(0.518392568310539,-0.855142763005338,0.));
#119748=DIRECTION('center_axis',(-0.376486505253528,-0.646402988624595,
0.663642288932205));
#119749=DIRECTION('ref_axis',(-0.60769242657897,-0.368386720189285,-0.703563173472535));
#119750=DIRECTION('center_axis',(-0.377569310640418,-0.648262095467517,
0.661209249211309));
#119751=DIRECTION('ref_axis',(-0.605720370685326,-0.367191248317468,-0.705884848750766));
#119752=DIRECTION('center_axis',(0.749388987580438,0.0349066476560596,-0.661209249211308));
#119753=DIRECTION('ref_axis',(0.605720370685331,0.367191248317453,0.705884848750769));
#119754=DIRECTION('center_axis',(0.747239865790733,0.0348065412516053,-0.663642288932184));
#119755=DIRECTION('ref_axis',(0.607692426578956,0.368386720189279,0.703563173472551));
#119756=DIRECTION('center_axis',(0.,0.,1.));
#119757=DIRECTION('ref_axis',(0.518392568310539,-0.855142763005338,0.));
#119758=DIRECTION('center_axis',(0.,0.,1.));
#119759=DIRECTION('ref_axis',(0.518392568310539,-0.855142763005338,0.));
#119760=DIRECTION('center_axis',(0.,0.,1.));
#119761=DIRECTION('ref_axis',(-0.518392568310514,0.855142763005353,0.));
#119762=DIRECTION('center_axis',(0.,0.,-1.));
#119763=DIRECTION('ref_axis',(0.518392568310535,-0.85514276300534,0.));
#119764=DIRECTION('center_axis',(-0.0175667319166402,-0.999845693059568,
0.));
#119765=DIRECTION('ref_axis',(0.999845693059568,-0.0175667319166402,0.));
#119766=DIRECTION('',(0.,0.,1.));
#119767=DIRECTION('center_axis',(0.0175716302745468,0.999845606983533,2.2859755779574E-6));
#119768=DIRECTION('ref_axis',(0.946482469611886,-0.016633071217235,-0.322326349619865));
#119769=DIRECTION('',(0.,0.,-1.));
#119770=DIRECTION('center_axis',(-0.830095916319145,0.557620632428785,0.));
#119771=DIRECTION('ref_axis',(-0.557620632428785,-0.830095916319145,0.));
#119772=DIRECTION('center_axis',(0.830095916319116,-0.557620632428829,-3.21712574280547E-14));
#119773=DIRECTION('ref_axis',(0.556871932182353,0.828981371804431,0.0518028604300564));
#119774=DIRECTION('',(0.,0.,1.));
#119775=DIRECTION('',(0.,0.,1.));
#119776=DIRECTION('center_axis',(0.,0.,1.));
#119777=DIRECTION('ref_axis',(0.46253829024085,-0.886599306372992,0.));
#119778=DIRECTION('center_axis',(0.,0.,-1.));
#119779=DIRECTION('ref_axis',(-0.46253829024085,0.886599306372992,0.));
#119780=DIRECTION('center_axis',(-0.226663083034188,0.944981349325736,-0.235868811452359));
#119781=DIRECTION('ref_axis',(0.745435741273968,0.0124503513820484,-0.666461209960335));
#119782=DIRECTION('center_axis',(-0.645369757790036,0.72654234530004,0.235868811452359));
#119783=DIRECTION('ref_axis',(-0.436687639408886,-0.604262659134024,0.666461209946816));
#119784=DIRECTION('center_axis',(0.,0.,-1.));
#119785=DIRECTION('ref_axis',(-0.462538290240846,0.886599306372994,0.));
#119786=DIRECTION('center_axis',(0.475117626555726,-0.879922292555458,-6.76296429840134E-17));
#119787=DIRECTION('ref_axis',(-0.879922292555458,-0.475117626555726,-4.99201041585171E-31));
#119788=DIRECTION('center_axis',(0.,0.,1.));
#119789=DIRECTION('ref_axis',(0.462538290240846,-0.886599306372994,0.));
#119790=DIRECTION('center_axis',(0.449865140885119,-0.893096498154825,-1.38914942345546E-16));
#119791=DIRECTION('ref_axis',(0.893096498154825,0.449865140885119,-6.16297582203916E-32));
#119792=DIRECTION('center_axis',(0.,0.,-1.));
#119793=DIRECTION('ref_axis',(-0.46253829024085,0.886599306372993,0.));
#119794=DIRECTION('center_axis',(0.,0.,1.));
#119795=DIRECTION('ref_axis',(0.46253829024085,-0.886599306372993,0.));
#119796=DIRECTION('center_axis',(0.,0.,1.));
#119797=DIRECTION('ref_axis',(0.46253829024085,-0.886599306372993,0.));
#119798=DIRECTION('center_axis',(-0.417128155027802,-0.6209533111466,0.663642288932205));
#119799=DIRECTION('ref_axis',(-0.63004647551427,-0.328694842711761,-0.70356317347253));
#119800=DIRECTION('center_axis',(-0.418327849059288,-0.62273922267579,0.661209249211309));
#119801=DIRECTION('ref_axis',(-0.628001877275145,-0.327628177120048,-0.705884848750764));
#119802=DIRECTION('center_axis',(0.75008576412785,-0.0131785890806782,-0.661209249211308));
#119803=DIRECTION('ref_axis',(0.628001877275145,0.327628177120031,0.705884848750771));
#119804=DIRECTION('center_axis',(0.747934644099999,-0.0131407950999565,
-0.663642288932184));
#119805=DIRECTION('ref_axis',(0.630046475514241,0.328694842711771,0.703563173472551));
#119806=DIRECTION('center_axis',(0.,0.,1.));
#119807=DIRECTION('ref_axis',(0.46253829024085,-0.886599306372993,0.));
#119808=DIRECTION('center_axis',(0.,0.,1.));
#119809=DIRECTION('ref_axis',(0.46253829024085,-0.886599306372993,0.));
#119810=DIRECTION('center_axis',(0.,0.,1.));
#119811=DIRECTION('ref_axis',(-0.46253829024085,0.886599306372993,0.));
#119812=DIRECTION('center_axis',(0.,0.,-1.));
#119813=DIRECTION('ref_axis',(0.462538290240846,-0.886599306372994,0.));
#119814=DIRECTION('center_axis',(-0.0815909726829869,-0.996665898471822,
0.));
#119815=DIRECTION('ref_axis',(0.996665898471822,-0.0815909726829869,0.));
#119816=DIRECTION('',(0.,0.,1.));
#119817=DIRECTION('center_axis',(0.0815958554617184,0.996665498733775,2.28597554272536E-6));
#119818=DIRECTION('ref_axis',(0.943472135374849,-0.0772402368275582,-0.322326349506282));
#119819=DIRECTION('',(0.,0.,-1.));
#119820=DIRECTION('center_axis',(-0.792663518646063,0.609659368998495,0.));
#119821=DIRECTION('ref_axis',(-0.609659368998495,-0.792663518646063,0.));
#119822=DIRECTION('center_axis',(0.792663518646077,-0.609659368998476,2.23833041067856E-15));
#119823=DIRECTION('ref_axis',(0.608840797926023,0.79159923347382,0.051802860388826));
#119824=DIRECTION('',(0.,0.,1.));
#119825=DIRECTION('',(0.,0.,1.));
#119826=DIRECTION('center_axis',(0.,0.,1.));
#119827=DIRECTION('ref_axis',(0.40478334312238,-0.914412623015818,0.));
#119828=DIRECTION('center_axis',(0.,0.,-1.));
#119829=DIRECTION('ref_axis',(-0.40478334312238,0.914412623015818,0.));
#119830=DIRECTION('center_axis',(-0.165652216491324,0.957562137386193,-0.235868811452249));
#119831=DIRECTION('ref_axis',(0.744701860367215,-0.0353354611165464,-0.666461209938951));
#119832=DIRECTION('center_axis',(-0.597494048518295,0.766398568480695,0.235868811452383));
#119833=DIRECTION('ref_axis',(-0.474505659318943,-0.575042463575424,0.666461209943536));
#119834=DIRECTION('center_axis',(0.,0.,-1.));
#119835=DIRECTION('ref_axis',(-0.404783343122404,0.914412623015808,0.));
#119836=DIRECTION('center_axis',(0.4177646315858,-0.908555288684173,-6.76296429840134E-17));
#119837=DIRECTION('ref_axis',(-0.908555288684173,-0.4177646315858,-6.44030973403092E-31));
#119838=DIRECTION('center_axis',(0.,0.,1.));
#119839=DIRECTION('ref_axis',(0.404783343122404,-0.914412623015808,0.));
#119840=DIRECTION('center_axis',(0.391719955604501,-0.920084494153231,-1.38914942345546E-16));
#119841=DIRECTION('ref_axis',(0.920084494153231,0.391719955604501,3.75941525144388E-31));
#119842=DIRECTION('center_axis',(0.,0.,-1.));
#119843=DIRECTION('ref_axis',(-0.40478334312241,0.914412623015806,0.));
#119844=DIRECTION('center_axis',(0.,0.,1.));
#119845=DIRECTION('ref_axis',(0.40478334312241,-0.914412623015806,0.));
#119846=DIRECTION('center_axis',(0.,0.,1.));
#119847=DIRECTION('ref_axis',(0.40478334312241,-0.914412623015806,0.));
#119848=DIRECTION('center_axis',(-0.456055735739358,-0.592952003319035,
0.663642288932205));
#119849=DIRECTION('ref_axis',(-0.649811528337108,-0.287652287620744,-0.703563173472535));
#119850=DIRECTION('center_axis',(-0.457367388615331,-0.594657380840943,
0.661209249211309));
#119851=DIRECTION('ref_axis',(-0.647702789445248,-0.286718811466832,-0.705884848750766));
#119852=DIRECTION('center_axis',(0.747700277377569,-0.0612096721680857,
-0.661209249211308));
#119853=DIRECTION('ref_axis',(0.647702789445253,0.286718811466814,0.705884848750769));
#119854=DIRECTION('center_axis',(0.745555998525181,-0.0610341331057615,
-0.663642288932184));
#119855=DIRECTION('ref_axis',(0.649811528337093,0.28765228762074,0.70356317347255));
#119856=DIRECTION('center_axis',(0.,0.,1.));
#119857=DIRECTION('ref_axis',(0.40478334312241,-0.914412623015806,0.));
#119858=DIRECTION('center_axis',(0.,0.,1.));
#119859=DIRECTION('ref_axis',(0.40478334312241,-0.914412623015806,0.));
#119860=DIRECTION('center_axis',(0.,0.,1.));
#119861=DIRECTION('ref_axis',(-0.404783343122445,0.91441262301579,0.));
#119862=DIRECTION('center_axis',(0.,0.,-1.));
#119863=DIRECTION('ref_axis',(0.404783343122404,-0.914412623015808,0.));
#119864=DIRECTION('center_axis',(-0.14527993864137,-0.98939058992309,0.));
#119865=DIRECTION('ref_axis',(0.98939058992309,-0.14527993864137,0.));
#119866=DIRECTION('',(0.,0.,1.));
#119867=DIRECTION('center_axis',(0.145284785776622,0.989389878165638,2.28597555524793E-6));
#119868=DIRECTION('ref_axis',(0.936584871728724,-0.137530005737331,-0.322326349482602));
#119869=DIRECTION('',(0.,0.,-1.));
#119870=DIRECTION('center_axis',(-0.751973896549073,0.659192884449464,0.));
#119871=DIRECTION('ref_axis',(-0.659192884449464,-0.751973896549073,0.));
#119872=DIRECTION('center_axis',(0.751973896549014,-0.659192884449531,-3.70652340886886E-14));
#119873=DIRECTION('ref_axis',(0.658307806233437,0.750964244092793,0.051802860406156));
#119874=DIRECTION('',(0.,0.,1.));
#119875=DIRECTION('',(0.,0.,1.));
#119876=DIRECTION('center_axis',(0.,0.,1.));
#119877=DIRECTION('ref_axis',(0.345365054421307,-0.938468422049761,0.));
#119878=DIRECTION('center_axis',(0.,0.,-1.));
#119879=DIRECTION('ref_axis',(-0.345365054421307,0.938468422049761,0.));
#119880=DIRECTION('center_axis',(-0.103960649459011,0.966208097227576,-0.235868811452315));
#119881=DIRECTION('ref_axis',(0.740907839753009,-0.0829760726379563,-0.666461209945567));
#119882=DIRECTION('center_axis',(-0.547163108039041,0.803105495551539,0.235868811452412));
#119883=DIRECTION('ref_axis',(-0.510373833681244,-0.543459295182668,0.666461209953789));
#119884=DIRECTION('center_axis',(0.,0.,-1.));
#119885=DIRECTION('ref_axis',(-0.345365054421319,0.938468422049756,0.));
#119886=DIRECTION('center_axis',(0.358694952134456,-0.933454836247186,-6.76296429840134E-17));
#119887=DIRECTION('ref_axis',(-0.933454836247186,-0.358694952134456,2.1570415377137E-31));
#119888=DIRECTION('center_axis',(0.,0.,1.));
#119889=DIRECTION('ref_axis',(0.345365054421319,-0.938468422049756,0.));
#119890=DIRECTION('center_axis',(0.331965109002638,-0.943291665607657,-1.38914942345546E-16));
#119891=DIRECTION('ref_axis',(0.943291665607656,0.331965109002638,-2.03378202127292E-31));
#119892=DIRECTION('center_axis',(0.,0.,-1.));
#119893=DIRECTION('ref_axis',(-0.345365054421309,0.93846842204976,0.));
#119894=DIRECTION('center_axis',(0.,0.,1.));
#119895=DIRECTION('ref_axis',(0.345365054421309,-0.93846842204976,0.));
#119896=DIRECTION('center_axis',(0.,0.,1.));
#119897=DIRECTION('ref_axis',(0.345365054421309,-0.93846842204976,0.));
#119898=DIRECTION('center_axis',(-0.493109285609112,-0.562514128522027,
0.663642288932205));
#119899=DIRECTION('ref_axis',(-0.666906366205899,-0.245427707578639,-0.70356317347253));
#119900=DIRECTION('center_axis',(-0.494527507466555,-0.564131964274613,
0.661209249211309));
#119901=DIRECTION('ref_axis',(-0.664742151921718,-0.244631256716294,-0.705884848750765));
#119902=DIRECTION('center_axis',(0.742242329806337,-0.10898923158312,-0.661209249211308));
#119903=DIRECTION('ref_axis',(0.664742151921719,0.244631256716282,0.705884848750769));
#119904=DIRECTION('center_axis',(0.740113703431163,-0.108676668766854,-0.663642288932184));
#119905=DIRECTION('ref_axis',(0.666906366205873,0.245427707578649,0.703563173472551));
#119906=DIRECTION('center_axis',(0.,0.,1.));
#119907=DIRECTION('ref_axis',(0.345365054421309,-0.93846842204976,0.));
#119908=DIRECTION('center_axis',(0.,0.,1.));
#119909=DIRECTION('ref_axis',(0.345365054421309,-0.93846842204976,0.));
#119910=DIRECTION('center_axis',(0.,0.,1.));
#119911=DIRECTION('ref_axis',(-0.345365054421342,0.938468422049748,0.));
#119912=DIRECTION('center_axis',(0.,0.,-1.));
#119913=DIRECTION('ref_axis',(0.345365054421319,-0.938468422049756,0.));
#119914=DIRECTION('center_axis',(-0.208371918169427,-0.978049663216748,
0.));
#119915=DIRECTION('ref_axis',(0.978049663216748,-0.208371918169427,0.));
#119916=DIRECTION('',(0.,0.,1.));
#119917=DIRECTION('center_axis',(0.208376709743215,0.978048642364666,2.28597553727221E-6));
#119918=DIRECTION('ref_axis',(0.925848979935386,-0.19725463435178,-0.322326349495898));
#119919=DIRECTION('',(0.,0.,-1.));
#119920=DIRECTION('center_axis',(-0.708194252413267,0.706017634941801,0.));
#119921=DIRECTION('ref_axis',(-0.706017634941801,-0.708194252413267,0.));
#119922=DIRECTION('center_axis',(0.708194252413259,-0.706017634941809,-1.13434032676751E-14));
#119923=DIRECTION('ref_axis',(0.705069686558746,0.707243381552184,0.051802860409279));
#119924=DIRECTION('',(0.,0.,1.));
#119925=DIRECTION('',(0.,0.,1.));
#119926=DIRECTION('center_axis',(0.,0.,1.));
#119927=DIRECTION('ref_axis',(0.28452758663103,-0.958667853036661,0.));
#119928=DIRECTION('center_axis',(0.,0.,-1.));
#119929=DIRECTION('ref_axis',(-0.28452758663103,0.958667853036661,0.));
#119930=DIRECTION('center_axis',(-0.0418418858186911,0.97088370074647,-0.235868811452413));
#119931=DIRECTION('ref_axis',(0.734069269906997,-0.130275717675883,-0.666461209945667));
#119932=DIRECTION('center_axis',(-0.494583756983052,0.836512289875412,0.235868811452306));
#119933=DIRECTION('ref_axis',(-0.544144772509927,-0.509642935982952,0.666461209938581));
#119934=DIRECTION('center_axis',(0.,0.,-1.));
#119935=DIRECTION('ref_axis',(-0.284527586631043,0.958667853036657,0.));
#119936=DIRECTION('center_axis',(0.298151318184964,-0.954518617662625,-6.76296429840134E-17));
#119937=DIRECTION('ref_axis',(-0.954518617662625,-0.298151318184964,-1.87970762572194E-31));
#119938=DIRECTION('center_axis',(0.,0.,1.));
#119939=DIRECTION('ref_axis',(0.284527586631043,-0.958667853036657,0.));
#119940=DIRECTION('center_axis',(0.27084614656159,-0.962622649272672,-1.38914942345546E-16));
#119941=DIRECTION('ref_axis',(0.962622649272672,0.27084614656159,5.8548270309372E-31));
#119942=DIRECTION('center_axis',(0.,0.,-1.));
#119943=DIRECTION('ref_axis',(-0.284527586631029,0.958667853036662,0.));
#119944=DIRECTION('center_axis',(0.,0.,1.));
#119945=DIRECTION('ref_axis',(0.284527586631029,-0.958667853036662,0.));
#119946=DIRECTION('center_axis',(0.,0.,1.));
#119947=DIRECTION('ref_axis',(0.284527586631029,-0.958667853036662,0.));
#119948=DIRECTION('center_axis',(-0.528136543652689,-0.529764762512019,
0.663642288932205));
#119949=DIRECTION('ref_axis',(-0.681260742764966,-0.202194612442037,-0.703563173472533));
#119950=DIRECTION('center_axis',(-0.529655506713783,-0.531288408461151,
0.661209249211309));
#119951=DIRECTION('ref_axis',(-0.679049946309191,-0.201538459658678,-0.705884848750767));
#119952=DIRECTION('center_axis',(0.73373434929145,-0.156320930867464,-0.661209249211308));
#119953=DIRECTION('ref_axis',(0.679049946309194,0.201538459658659,0.705884848750769));
#119954=DIRECTION('center_axis',(0.731630122375854,-0.155872628684911,-0.663642288932184));
#119955=DIRECTION('ref_axis',(0.681260742764946,0.202194612442041,0.703563173472551));
#119956=DIRECTION('center_axis',(0.,0.,1.));
#119957=DIRECTION('ref_axis',(0.284527586631029,-0.958667853036662,0.));
#119958=DIRECTION('center_axis',(0.,0.,1.));
#119959=DIRECTION('ref_axis',(0.284527586631029,-0.958667853036662,0.));
#119960=DIRECTION('center_axis',(0.,0.,1.));
#119961=DIRECTION('ref_axis',(-0.284527586631029,0.958667853036662,0.));
#119962=DIRECTION('center_axis',(0.,0.,-1.));
#119963=DIRECTION('ref_axis',(0.284527586631043,-0.958667853036657,0.));
#119964=DIRECTION('center_axis',(-0.270607652790088,-0.962689720653253,
0.));
#119965=DIRECTION('ref_axis',(0.962689720653253,-0.270607652790088,0.));
#119966=DIRECTION('',(0.,0.,1.));
#119967=DIRECTION('center_axis',(0.270612369112889,0.962688394901426,2.28597555798509E-6));
#119968=DIRECTION('ref_axis',(0.911308576064988,-0.256168701355266,-0.322326349584331));
#119969=DIRECTION('',(0.,0.,-1.));
#119970=DIRECTION('center_axis',(-0.661504486187105,0.749941207531853,0.));
#119971=DIRECTION('ref_axis',(-0.749941207531853,-0.661504486187105,0.));
#119972=DIRECTION('center_axis',(0.661504486187064,-0.749941207531889,-2.68599649281396E-14));
#119973=DIRECTION('ref_axis',(0.748934284305921,0.660616304254221,0.0518028603908362));
#119974=DIRECTION('',(0.,0.,1.));
#119975=DIRECTION('',(0.,0.,1.));
#119976=DIRECTION('center_axis',(0.,0.,1.));
#119977=DIRECTION('ref_axis',(0.222520933956302,-0.974927912181827,0.));
#119978=DIRECTION('center_axis',(0.,0.,-1.));
#119979=DIRECTION('ref_axis',(-0.222520933956302,0.974927912181827,0.));
#119980=DIRECTION('center_axis',(0.0204488151059505,0.97156973488516,-0.235868811452347));
#119981=DIRECTION('ref_axis',(0.724214251961581,-0.17704003184875,-0.66646120995803));
#119982=DIRECTION('center_axis',(-0.439972055181341,0.866481675769055,0.235868811452378));
#119983=DIRECTION('ref_axis',(-0.57567970371943,-0.473732344632131,0.666461209955128));
#119984=DIRECTION('center_axis',(0.,0.,-1.));
#119985=DIRECTION('ref_axis',(-0.222520933956325,0.974927912181821,0.));
#119986=DIRECTION('center_axis',(0.236382516515794,-0.971660077334486,-6.76296429840134E-17));
#119987=DIRECTION('ref_axis',(-0.971660077334487,-0.236382516515794,-1.29422492262822E-31));
#119988=DIRECTION('center_axis',(0.,0.,1.));
#119989=DIRECTION('ref_axis',(0.222520933956325,-0.974927912181821,0.));
#119990=DIRECTION('center_axis',(0.208614219208004,-0.977998009989916,-1.38914942345546E-16));
#119991=DIRECTION('ref_axis',(0.977998009989915,0.208614219208004,6.77927340424307E-31));
#119992=DIRECTION('center_axis',(0.,0.,-1.));
#119993=DIRECTION('ref_axis',(-0.222520933956319,0.974927912181823,0.));
#119994=DIRECTION('center_axis',(0.,0.,1.));
#119995=DIRECTION('ref_axis',(0.222520933956319,-0.974927912181823,0.));
#119996=DIRECTION('center_axis',(0.,0.,1.));
#119997=DIRECTION('ref_axis',(0.222520933956319,-0.974927912181823,0.));
#119998=DIRECTION('center_axis',(-0.560993575353463,-0.494838479458664,
0.663642288932205));
#119999=DIRECTION('ref_axis',(-0.692815672802044,-0.1581306562723,-0.703563173472534));
#120000=DIRECTION('center_axis',(-0.562607037873173,-0.496261674616316,
0.661209249211309));
#120001=DIRECTION('ref_axis',(-0.690567378811524,-0.157617497840459,-0.705884848750767));
#120002=DIRECTION('center_axis',(0.7222112969498,-0.203010273916138,-0.661209249211308));
#120003=DIRECTION('ref_axis',(0.690567378811528,0.157617497840441,0.705884848750768));
#120004=DIRECTION('center_axis',(0.720140116213534,-0.202428074537128,-0.663642288932184));
#120005=DIRECTION('ref_axis',(0.692815672802026,0.158130656272298,0.703563173472552));
#120006=DIRECTION('center_axis',(0.,0.,1.));
#120007=DIRECTION('ref_axis',(0.222520933956319,-0.974927912181823,0.));
#120008=DIRECTION('center_axis',(0.,0.,1.));
#120009=DIRECTION('ref_axis',(0.222520933956319,-0.974927912181823,0.));
#120010=DIRECTION('center_axis',(0.,0.,1.));
#120011=DIRECTION('ref_axis',(-0.222520933956353,0.974927912181815,0.));
#120012=DIRECTION('center_axis',(0.,0.,-1.));
#120013=DIRECTION('ref_axis',(0.222520933956325,-0.974927912181821,0.));
#120014=DIRECTION('center_axis',(-0.331731402520277,-0.943373879531297,
0.));
#120015=DIRECTION('ref_axis',(0.943373879531297,-0.331731402520277,0.));
#120016=DIRECTION('',(0.,0.,1.));
#120017=DIRECTION('center_axis',(0.331736024211709,0.943372254327518,2.28597557033843E-6));
#120018=DIRECTION('ref_axis',(0.893023409828756,-0.314030116229774,-0.322326349525658));
#120019=DIRECTION('',(0.,0.,-1.));
#120020=DIRECTION('center_axis',(-0.612096456134932,0.790783110838274,0.));
#120021=DIRECTION('ref_axis',(-0.790783110838274,-0.612096456134932,0.));
#120022=DIRECTION('center_axis',(0.612096456134955,-0.790783110838255,8.80157042843185E-15));
#120023=DIRECTION('ref_axis',(0.789721350432804,0.61127461286019,0.0518028603767528));
#120024=DIRECTION('',(0.,0.,1.));
#120025=DIRECTION('',(0.,0.,1.));
#120026=DIRECTION('center_axis',(0.,0.,1.));
#120027=DIRECTION('ref_axis',(0.159599895033413,-0.987181783414445,0.));
#120028=DIRECTION('center_axis',(0.,0.,-1.));
#120029=DIRECTION('ref_axis',(-0.159599895033413,0.987181783414445,0.));
#120030=DIRECTION('center_axis',(0.0826554874630245,0.968263380582131,-0.235868811452285));
#120031=DIRECTION('ref_axis',(0.711383282330738,-0.223076850551026,-0.666461209950423));
#120032=DIRECTION('center_axis',(-0.383552413831434,0.892890502597124,0.235868811452331));
#120033=DIRECTION('ref_axis',(-0.60484904357645,-0.435875085469539,0.666461209937664));
#120034=DIRECTION('center_axis',(0.,0.,-1.));
#120035=DIRECTION('ref_axis',(-0.15959989503339,0.987181783414449,0.));
#120036=DIRECTION('center_axis',(0.17364236838237,-0.984808777328148,-6.76296429840134E-17));
#120037=DIRECTION('ref_axis',(-0.984808777328148,-0.17364236838237,9.09038933750775E-32));
#120038=DIRECTION('center_axis',(0.,0.,1.));
#120039=DIRECTION('ref_axis',(0.15959989503339,-0.987181783414448,0.));
#120040=DIRECTION('center_axis',(0.145525051280083,-0.989354567104195,-1.38914942345546E-16));
#120041=DIRECTION('ref_axis',(0.989354567104195,0.145525051280083,4.25245331720702E-31));
#120042=DIRECTION('center_axis',(0.,0.,-1.));
#120043=DIRECTION('ref_axis',(-0.159599895033397,0.987181783414447,0.));
#120044=DIRECTION('center_axis',(0.,0.,1.));
#120045=DIRECTION('ref_axis',(0.159599895033398,-0.987181783414447,0.));
#120046=DIRECTION('center_axis',(0.,0.,1.));
#120047=DIRECTION('ref_axis',(0.159599895033398,-0.987181783414447,0.));
#120048=DIRECTION('center_axis',(-0.591545364120365,-0.457878798950692,
0.663642288932205));
#120049=DIRECTION('ref_axis',(-0.701523674631087,-0.113416907317011,-0.703563173472533));
#120050=DIRECTION('center_axis',(-0.593246696035112,-0.459195695102688,
0.661209249211309));
#120051=DIRECTION('ref_axis',(-0.699247121828083,-0.113048851914766,-0.705884848750768));
#120052=DIRECTION('center_axis',(0.707720523475147,-0.248865404203723,-0.661209249211308));
#120053=DIRECTION('ref_axis',(0.699247121828087,0.113048851914743,0.705884848750769));
#120054=DIRECTION('center_axis',(0.705690899844122,-0.248151700010386,-0.663642288932184));
#120055=DIRECTION('ref_axis',(0.701523674631067,0.113416907317012,0.703563173472553));
#120056=DIRECTION('center_axis',(0.,0.,1.));
#120057=DIRECTION('ref_axis',(0.159599895033398,-0.987181783414447,0.));
#120058=DIRECTION('center_axis',(0.,0.,1.));
#120059=DIRECTION('ref_axis',(0.159599895033398,-0.987181783414447,0.));
#120060=DIRECTION('center_axis',(0.,0.,1.));
#120061=DIRECTION('ref_axis',(-0.159599895033398,0.987181783414447,0.));
#120062=DIRECTION('center_axis',(0.,0.,-1.));
#120063=DIRECTION('ref_axis',(0.15959989503339,-0.987181783414448,0.));
#120064=DIRECTION('center_axis',(-0.391491996761346,-0.920181512785284,
0.));
#120065=DIRECTION('ref_axis',(0.920181512785284,-0.391491996761346,0.));
#120066=DIRECTION('',(0.,0.,1.));
#120067=DIRECTION('center_axis',(0.391496504829889,0.920179594807859,2.28597558341214E-6));
#120068=DIRECTION('ref_axis',(0.871068618823477,-0.370601113989528,-0.322326349544497));
#120069=DIRECTION('',(0.,0.,-1.));
#120070=DIRECTION('center_axis',(-0.560173190450223,0.828375516719813,0.));
#120071=DIRECTION('ref_axis',(-0.828375516719814,-0.560173190450223,0.));
#120072=DIRECTION('center_axis',(0.560173190450257,-0.82837551671979,1.65788201604461E-14));
#120073=DIRECTION('ref_axis',(0.827263282131684,0.559421062960764,0.051802860466998));
#120074=DIRECTION('',(0.,0.,1.));
#120075=DIRECTION('',(0.,0.,1.));
#120076=DIRECTION('center_axis',(0.,0.,1.));
#120077=DIRECTION('ref_axis',(0.096023025907694,-0.995379112949197,0.));
#120078=DIRECTION('center_axis',(0.,0.,-1.));
#120079=DIRECTION('ref_axis',(-0.096023025907694,0.995379112949197,0.));
#120080=DIRECTION('center_axis',(0.144522510692308,0.960978224356439,-0.235868811452334));
#120081=DIRECTION('ref_axis',(-0.695629086194335,0.26819699862612,0.666461209950268));
#120082=DIRECTION('center_axis',(-0.325556673341165,0.915630250825671,0.235868811452369));
#120083=DIRECTION('ref_axis',(-0.631532928946986,-0.396226722080935,0.666461209947465));
#120084=DIRECTION('center_axis',(0.,0.,-1.));
#120085=DIRECTION('ref_axis',(-0.0960230259076927,0.995379112949197,0.));
#120086=DIRECTION('center_axis',(0.110188686511091,-0.993910686814947,-6.76296429840134E-17));
#120087=DIRECTION('ref_axis',(-0.993910686814947,-0.110188686511091,-2.00296714216273E-32));
#120088=DIRECTION('center_axis',(0.,0.,1.));
#120089=DIRECTION('ref_axis',(0.0960230259076927,-0.995379112949197,0.));
#120090=DIRECTION('center_axis',(0.0818378897014263,-0.996645654086355,
-1.38914942345546E-16));
#120091=DIRECTION('ref_axis',(0.996645654086354,0.0818378897014263,5.8548270309372E-32));
#120092=DIRECTION('center_axis',(0.,0.,-1.));
#120093=DIRECTION('ref_axis',(-0.0960230259076935,0.995379112949197,0.));
#120094=DIRECTION('center_axis',(0.,0.,1.));
#120095=DIRECTION('ref_axis',(0.0960230259076935,-0.995379112949197,0.));
#120096=DIRECTION('center_axis',(0.,0.,1.));
#120097=DIRECTION('ref_axis',(0.0960230259076935,-0.995379112949197,0.));
#120098=DIRECTION('center_axis',(-0.619666366100014,-0.419037596243138,
0.663642288932205));
#120099=DIRECTION('ref_axis',(-0.707348965204713,-0.0682371039617093,-0.703563173472532));
#120100=DIRECTION('center_axis',(-0.621448576272025,-0.420242781980715,
0.661209249211309));
#120101=DIRECTION('ref_axis',(-0.705053508433015,-0.0680156640076522,-0.705884848750769));
#120102=DIRECTION('center_axis',(0.690321574563957,-0.293697893163974,-0.661209249211308));
#120103=DIRECTION('ref_axis',(0.705053508433017,0.0680156640076259,0.705884848750769));
#120104=DIRECTION('center_axis',(0.688341848197028,-0.292855616919928,-0.663642288932184));
#120105=DIRECTION('ref_axis',(0.707348965204693,0.0682371039617151,0.703563173472552));
#120106=DIRECTION('center_axis',(0.,0.,1.));
#120107=DIRECTION('ref_axis',(0.0960230259076933,-0.995379112949197,0.));
#120108=DIRECTION('center_axis',(0.,0.,1.));
#120109=DIRECTION('ref_axis',(0.0960230259076933,-0.995379112949197,0.));
#120110=DIRECTION('center_axis',(0.,0.,1.));
#120111=DIRECTION('ref_axis',(-0.0960230259076933,0.995379112949197,0.));
#120112=DIRECTION('center_axis',(0.,0.,-1.));
#120113=DIRECTION('ref_axis',(0.0960230259076927,-0.995379112949197,0.));
#120114=DIRECTION('center_axis',(-0.449643866412953,-0.893207922824921,
0.));
#120115=DIRECTION('ref_axis',(0.893207922824921,-0.449643866412953,0.));
#120116=DIRECTION('',(0.,0.,1.));
#120117=DIRECTION('center_axis',(0.449648242333875,0.893205719955281,2.28597553924879E-6));
#120118=DIRECTION('ref_axis',(0.845534420026475,-0.425649232280533,-0.322326349542641));
#120119=DIRECTION('',(0.,0.,-1.));
#120120=DIRECTION('center_axis',(-0.505948052969182,0.86256394991716,0.));
#120121=DIRECTION('ref_axis',(-0.862563949917161,-0.505948052969182,0.));
#120122=DIRECTION('center_axis',(0.505948052969246,-0.862563949917123,4.09728278564901E-14));
#120123=DIRECTION('ref_axis',(0.861405811564763,0.505268731923542,0.0518028603730392));
#120124=DIRECTION('',(0.,0.,1.));
#120125=DIRECTION('',(0.,0.,1.));
#120126=DIRECTION('center_axis',(0.,0.,1.));
#120127=DIRECTION('ref_axis',(0.0320515775716953,-0.999486216200687,0.));
#120128=DIRECTION('center_axis',(0.,0.,-1.));
#120129=DIRECTION('ref_axis',(-0.0320515775716953,0.999486216200687,0.));
#120130=DIRECTION('center_axis',(0.205795659925261,0.94974420247769,-0.235868811452346));
#120131=DIRECTION('ref_axis',(-0.677016400916227,0.312215067706304,0.666461209964681));
#120132=DIRECTION('center_axis',(-0.266223150648821,0.934607477951421,0.235868811452256));
#120133=DIRECTION('ref_axis',(-0.655621710062707,-0.354950178102783,0.666461209943425));
#120134=DIRECTION('center_axis',(0.,0.,-1.));
#120135=DIRECTION('ref_axis',(-0.0320515775716664,0.999486216200688,0.));
#120136=DIRECTION('center_axis',(0.0462822156915398,-0.998928404096451,
-6.76296429840134E-17));
#120137=DIRECTION('ref_axis',(-0.998928404096451,-0.0462822156915398,6.39408741536562E-32));
#120138=DIRECTION('center_axis',(0.,0.,1.));
#120139=DIRECTION('ref_axis',(0.0320515775716664,-0.999486216200687,0.));
#120140=DIRECTION('center_axis',(0.0178144386798146,-0.999841310296051,
-1.38914942345546E-16));
#120141=DIRECTION('ref_axis',(0.999841310296051,0.0178144386798146,1.54074395550979E-33));
#120142=DIRECTION('center_axis',(0.,0.,-1.));
#120143=DIRECTION('ref_axis',(-0.0320515775716762,0.999486216200687,0.));
#120144=DIRECTION('center_axis',(0.,0.,1.));
#120145=DIRECTION('ref_axis',(0.0320515775716762,-0.999486216200687,0.));
#120146=DIRECTION('center_axis',(0.,0.,1.));
#120147=DIRECTION('ref_axis',(0.0320515775716762,-0.999486216200687,0.));
#120148=DIRECTION('center_axis',(-0.645241026063339,-0.378474478169339,
0.663642288932205));
#120149=DIRECTION('ref_axis',(-0.710267607154434,-0.0227768997094196,-0.703563173472533));
#120150=DIRECTION('center_axis',(-0.647096791008734,-0.379563001125789,
0.661209249211309));
#120151=DIRECTION('ref_axis',(-0.707962678938293,-0.0227029851478096,-0.705884848750767));
#120152=DIRECTION('center_axis',(0.670085946229371,-0.337323514483213,-0.661209249211308));
#120153=DIRECTION('ref_axis',(0.707962678938293,0.022702985147791,0.705884848750768));
#120154=DIRECTION('center_axis',(0.668164252246828,-0.336356127282214,-0.663642288932184));
#120155=DIRECTION('ref_axis',(0.710267607154415,0.0227768997094241,0.703563173472553));
#120156=DIRECTION('center_axis',(0.,0.,1.));
#120157=DIRECTION('ref_axis',(0.0320515775716762,-0.999486216200687,0.));
#120158=DIRECTION('center_axis',(0.,0.,1.));
#120159=DIRECTION('ref_axis',(0.0320515775716762,-0.999486216200687,0.));
#120160=DIRECTION('center_axis',(0.,0.,1.));
#120161=DIRECTION('ref_axis',(-0.0320515775716415,0.999486216200688,0.));
#120162=DIRECTION('center_axis',(0.,0.,-1.));
#120163=DIRECTION('ref_axis',(0.0320515775716664,-0.999486216200688,0.));
#120164=DIRECTION('center_axis',(-0.505948052969163,-0.862563949917171,
0.));
#120165=DIRECTION('ref_axis',(0.862563949917172,-0.505948052969163,0.));
#120166=DIRECTION('',(0.,0.,1.));
#120167=DIRECTION('center_axis',(0.505952278760864,0.862561471207394,2.28597549516116E-6));
#120168=DIRECTION('ref_axis',(0.816525738978556,-0.478948266602592,-0.322326349378848));
#120169=DIRECTION('',(0.,0.,-1.));
#120170=DIRECTION('center_axis',(-0.449643866412973,0.893207922824911,0.));
#120171=DIRECTION('ref_axis',(-0.893207922824911,-0.449643866412973,0.));
#120172=DIRECTION('center_axis',(0.449643866412962,-0.893207922824917,-1.47198677854773E-14));
#120173=DIRECTION('ref_axis',(0.892008639741106,0.449040143283163,0.0518028604177202));
#120174=DIRECTION('',(0.,0.,1.));
#120175=DIRECTION('',(0.,0.,1.));
#120176=DIRECTION('center_axis',(0.,0.,1.));
#120177=DIRECTION('ref_axis',(-0.0320515775716322,-0.999486216200689,0.));
#120178=DIRECTION('center_axis',(0.,0.,-1.));
#120179=DIRECTION('ref_axis',(0.0320515775716322,0.999486216200689,0.));
#120180=DIRECTION('center_axis',(0.266223150648561,0.934607477951468,-0.235868811452362));
#120181=DIRECTION('ref_axis',(-0.655621710047066,0.354950178102169,0.666461209959138));
#120182=DIRECTION('center_axis',(-0.205795659925299,0.949744202477684,0.235868811452338));
#120183=DIRECTION('ref_axis',(-0.677016400940734,-0.312215067705544,0.666461209940142));
#120184=DIRECTION('center_axis',(0.,0.,-1.));
#120185=DIRECTION('ref_axis',(0.0320515775716446,0.999486216200688,0.));
#120186=DIRECTION('center_axis',(-0.0178144386797932,-0.999841310296051,
-6.76296429840134E-17));
#120187=DIRECTION('ref_axis',(-0.999841310296051,0.0178144386797932,-1.30963236218332E-32));
#120188=DIRECTION('center_axis',(0.,0.,1.));
#120189=DIRECTION('ref_axis',(-0.0320515775716446,-0.999486216200688,0.));
#120190=DIRECTION('center_axis',(-0.0462822156915185,-0.998928404096452,
-1.38914942345546E-16));
#120191=DIRECTION('ref_axis',(0.998928404096452,-0.0462822156915185,8.78224054640579E-32));
#120192=DIRECTION('center_axis',(0.,0.,-1.));
#120193=DIRECTION('ref_axis',(0.0320515775716415,0.999486216200688,0.));
#120194=DIRECTION('center_axis',(0.,0.,1.));
#120195=DIRECTION('ref_axis',(-0.0320515775716415,-0.999486216200688,0.));
#120196=DIRECTION('center_axis',(0.,0.,1.));
#120197=DIRECTION('ref_axis',(-0.0320515775716415,-0.999486216200688,0.));
#120198=DIRECTION('center_axis',(-0.668164252246804,-0.33635612728222,0.663642288932205));
#120199=DIRECTION('ref_axis',(-0.710267607154435,0.022776899709407,-0.703563173472533));
#120200=DIRECTION('center_axis',(-0.670085946229363,-0.337323514483229,
0.661209249211309));
#120201=DIRECTION('ref_axis',(-0.707962678938294,0.0227029851477752,-0.705884848750767));
#120202=DIRECTION('center_axis',(0.647096791008744,-0.379563001125774,-0.661209249211308));
#120203=DIRECTION('ref_axis',(0.707962678938293,-0.022702985147794,0.705884848750768));
#120204=DIRECTION('center_axis',(0.645241026063363,-0.378474478169334,-0.663642288932184));
#120205=DIRECTION('ref_axis',(0.710267607154415,-0.0227768997094036,0.703563173472553));
#120206=DIRECTION('center_axis',(0.,0.,1.));
#120207=DIRECTION('ref_axis',(-0.0320515775716415,-0.999486216200688,0.));
#120208=DIRECTION('center_axis',(0.,0.,1.));
#120209=DIRECTION('ref_axis',(-0.0320515775716415,-0.999486216200688,0.));
#120210=DIRECTION('center_axis',(0.,0.,1.));
#120211=DIRECTION('ref_axis',(0.0320515775716068,0.999486216200689,0.));
#120212=DIRECTION('center_axis',(0.,0.,-1.));
#120213=DIRECTION('ref_axis',(-0.0320515775716446,-0.999486216200688,0.));
#120214=DIRECTION('center_axis',(-0.560173190450205,-0.828375516719826,
0.));
#120215=DIRECTION('ref_axis',(0.828375516719826,-0.560173190450205,0.));
#120216=DIRECTION('',(0.,0.,1.));
#120217=DIRECTION('center_axis',(0.560177248748154,0.828372772355371,2.28597553347141E-6));
#120218=DIRECTION('ref_axis',(0.784161778440321,-0.530279199714647,-0.322326349502033));
#120219=DIRECTION('',(0.,0.,-1.));
#120220=DIRECTION('center_axis',(-0.391491996761366,0.920181512785276,0.));
#120221=DIRECTION('ref_axis',(-0.920181512785276,-0.391491996761366,0.));
#120222=DIRECTION('center_axis',(0.391491996761285,-0.92018151278531,-3.69893584815328E-14));
#120223=DIRECTION('ref_axis',(0.918946013078971,0.390966352374483,0.0518028605122913));
#120224=DIRECTION('',(0.,0.,1.));
#120225=DIRECTION('',(0.,0.,1.));
#120226=DIRECTION('center_axis',(0.,0.,1.));
#120227=DIRECTION('ref_axis',(-0.0960230259076932,-0.995379112949197,0.));
#120228=DIRECTION('center_axis',(0.,0.,-1.));
#120229=DIRECTION('ref_axis',(0.0960230259076932,0.995379112949197,0.));
#120230=DIRECTION('center_axis',(0.325556673341087,0.915630250825694,-0.235868811452387));
#120231=DIRECTION('ref_axis',(-0.631532928939842,0.3962267220802,0.666461209954672));
#120232=DIRECTION('center_axis',(-0.144522510692294,0.960978224356439,0.235868811452346));
#120233=DIRECTION('ref_axis',(-0.695629086202631,-0.26819699862532,0.666461209941931));
#120234=DIRECTION('center_axis',(0.,0.,-1.));
#120235=DIRECTION('ref_axis',(0.096023025907671,0.995379112949199,0.));
#120236=DIRECTION('center_axis',(-0.081837889701405,-0.996645654086356,
-6.76296429840134E-17));
#120237=DIRECTION('ref_axis',(-0.996645654086356,0.081837889701405,4.77630626208035E-32));
#120238=DIRECTION('center_axis',(0.,0.,1.));
#120239=DIRECTION('ref_axis',(-0.096023025907671,-0.995379112949199,0.));
#120240=DIRECTION('center_axis',(-0.11018868651107,-0.99391068681495,-1.38914942345546E-16));
#120241=DIRECTION('ref_axis',(0.99391068681495,-0.11018868651107,-6.16297582203915E-32));
#120242=DIRECTION('center_axis',(0.,0.,-1.));
#120243=DIRECTION('ref_axis',(0.0960230259076587,0.9953791129492,0.));
#120244=DIRECTION('center_axis',(0.,0.,1.));
#120245=DIRECTION('ref_axis',(-0.0960230259076587,-0.9953791129492,0.));
#120246=DIRECTION('center_axis',(0.,0.,1.));
#120247=DIRECTION('ref_axis',(-0.0960230259076587,-0.9953791129492,0.));
#120248=DIRECTION('center_axis',(-0.688341848197004,-0.292855616919936,
0.663642288932205));
#120249=DIRECTION('ref_axis',(-0.707348965204713,0.0682371039616992,-0.703563173472533));
#120250=DIRECTION('center_axis',(-0.69032157456395,-0.29369789316399,0.661209249211309));
#120251=DIRECTION('ref_axis',(-0.705053508433019,0.0680156640076101,-0.705884848750768));
#120252=DIRECTION('center_axis',(0.621448576272035,-0.4202427819807,-0.661209249211308));
#120253=DIRECTION('ref_axis',(0.705053508433016,-0.068015664007635,0.705884848750769));
#120254=DIRECTION('center_axis',(0.619666366100039,-0.419037596243135,-0.663642288932184));
#120255=DIRECTION('ref_axis',(0.707348965204694,-0.0682371039616922,0.703563173472553));
#120256=DIRECTION('center_axis',(0.,0.,1.));
#120257=DIRECTION('ref_axis',(-0.0960230259076587,-0.9953791129492,0.));
#120258=DIRECTION('center_axis',(0.,0.,1.));
#120259=DIRECTION('ref_axis',(-0.0960230259076587,-0.9953791129492,0.));
#120260=DIRECTION('center_axis',(0.,0.,1.));
#120261=DIRECTION('ref_axis',(0.0960230259076239,0.995379112949204,0.));
#120262=DIRECTION('center_axis',(0.,0.,-1.));
#120263=DIRECTION('ref_axis',(-0.0960230259076709,-0.995379112949199,0.));
#120264=DIRECTION('center_axis',(-0.612096456134915,-0.790783110838286,
0.));
#120265=DIRECTION('ref_axis',(0.790783110838286,-0.612096456134915,0.));
#120266=DIRECTION('',(0.,0.,1.));
#120267=DIRECTION('center_axis',(0.612100330262687,0.79078011209633,2.28597557930745E-6));
#120268=DIRECTION('ref_axis',(0.748575528964249,-0.579431101853004,-0.322326349592007));
#120269=DIRECTION('',(0.,0.,-1.));
#120270=DIRECTION('center_axis',(-0.331731402520297,0.94337387953129,0.));
#120271=DIRECTION('ref_axis',(-0.94337387953129,-0.331731402520297,0.));
#120272=DIRECTION('center_axis',(0.331731402520233,-0.943373879531312,-3.55097841422777E-14));
#120273=DIRECTION('ref_axis',(0.942107240142804,0.331285996865109,0.0518028604576939));
#120274=DIRECTION('',(0.,0.,1.));
#120275=DIRECTION('',(0.,0.,1.));
#120276=DIRECTION('center_axis',(0.,0.,1.));
#120277=DIRECTION('ref_axis',(-0.159599895033352,-0.987181783414455,0.));
#120278=DIRECTION('center_axis',(0.,0.,-1.));
#120279=DIRECTION('ref_axis',(0.159599895033352,0.987181783414455,0.));
#120280=DIRECTION('center_axis',(0.383552413831463,0.89289050259712,-0.235868811452298));
#120281=DIRECTION('ref_axis',(-0.604849043555148,0.435875085466088,0.666461209959254));
#120282=DIRECTION('center_axis',(-0.0826554874630613,0.968263380582129,
0.23586881145228));
#120283=DIRECTION('ref_axis',(0.711383282352891,0.223076850547471,-0.666461209927966));
#120284=DIRECTION('center_axis',(0.,0.,-1.));
#120285=DIRECTION('ref_axis',(0.159599895033369,0.987181783414452,0.));
#120286=DIRECTION('center_axis',(-0.145525051280062,-0.989354567104198,
-6.76296429840134E-17));
#120287=DIRECTION('ref_axis',(-0.989354567104198,0.145525051280062,-1.38666955995881E-32));
#120288=DIRECTION('center_axis',(0.,0.,1.));
#120289=DIRECTION('ref_axis',(-0.159599895033369,-0.987181783414452,0.));
#120290=DIRECTION('center_axis',(-0.17364236838235,-0.984808777328152,-1.38914942345546E-16));
#120291=DIRECTION('ref_axis',(0.984808777328151,-0.173642368382349,6.47112461314111E-32));
#120292=DIRECTION('center_axis',(0.,0.,-1.));
#120293=DIRECTION('ref_axis',(0.159599895033363,0.987181783414453,0.));
#120294=DIRECTION('center_axis',(0.,0.,1.));
#120295=DIRECTION('ref_axis',(-0.159599895033363,-0.987181783414453,0.));
#120296=DIRECTION('center_axis',(0.,0.,1.));
#120297=DIRECTION('ref_axis',(-0.159599895033363,-0.987181783414453,0.));
#120298=DIRECTION('center_axis',(-0.705690899844099,-0.248151700010395,
0.663642288932205));
#120299=DIRECTION('ref_axis',(-0.701523674631089,0.113416907316999,-0.703563173472533));
#120300=DIRECTION('center_axis',(-0.70772052347514,-0.24886540420374,0.661209249211309));
#120301=DIRECTION('ref_axis',(-0.69924712182809,0.113048851914729,-0.705884848750768));
#120302=DIRECTION('center_axis',(0.593246696035123,-0.459195695102674,-0.661209249211308));
#120303=DIRECTION('ref_axis',(0.699247121828084,-0.113048851914753,0.70588484875077));
#120304=DIRECTION('center_axis',(0.591545364120389,-0.457878798950691,-0.663642288932184));
#120305=DIRECTION('ref_axis',(0.701523674631069,-0.113416907316995,0.703563173472554));
#120306=DIRECTION('center_axis',(0.,0.,1.));
#120307=DIRECTION('ref_axis',(-0.159599895033363,-0.987181783414453,0.));
#120308=DIRECTION('center_axis',(0.,0.,1.));
#120309=DIRECTION('ref_axis',(-0.159599895033363,-0.987181783414453,0.));
#120310=DIRECTION('center_axis',(0.,0.,1.));
#120311=DIRECTION('ref_axis',(0.159599895033294,0.987181783414464,0.));
#120312=DIRECTION('center_axis',(0.,0.,-1.));
#120313=DIRECTION('ref_axis',(-0.159599895033369,-0.987181783414452,0.));
#120314=DIRECTION('center_axis',(-0.661504486187089,-0.749941207531868,
0.));
#120315=DIRECTION('ref_axis',(0.749941207531868,-0.661504486187089,0.));
#120316=DIRECTION('',(0.,0.,1.));
#120317=DIRECTION('center_axis',(0.661508160225006,0.749937966734918,2.28597557930792E-6));
#120318=DIRECTION('ref_axis',(0.709913222114901,-0.626201997339955,-0.32232634951845));
#120319=DIRECTION('',(0.,0.,-1.));
#120320=DIRECTION('center_axis',(-0.270607652790109,0.962689720653247,0.));
#120321=DIRECTION('ref_axis',(-0.962689720653248,-0.270607652790109,0.));
#120322=DIRECTION('center_axis',(0.270607652790095,-0.962689720653252,-1.3695547089062E-14));
#120323=DIRECTION('ref_axis',(0.961397146474936,0.270244316133488,0.0518028604171078));
#120324=DIRECTION('',(0.,0.,1.));
#120325=DIRECTION('',(0.,0.,1.));
#120326=DIRECTION('center_axis',(0.,0.,1.));
#120327=DIRECTION('ref_axis',(-0.222520933956302,-0.974927912181827,0.));
#120328=DIRECTION('center_axis',(0.,0.,-1.));
#120329=DIRECTION('ref_axis',(0.222520933956302,0.974927912181827,0.));
#120330=DIRECTION('center_axis',(0.439972055181506,0.866481675768994,-0.235868811452296));
#120331=DIRECTION('ref_axis',(-0.575679703725262,0.473732344633531,0.666461209949095));
#120332=DIRECTION('center_axis',(-0.0204488151061702,0.971569734885175,
0.235868811452267));
#120333=DIRECTION('ref_axis',(0.724214251971472,0.177040031846594,-0.666461209947854));
#120334=DIRECTION('center_axis',(0.,0.,-1.));
#120335=DIRECTION('ref_axis',(0.222520933956304,0.974927912181826,0.));
#120336=DIRECTION('center_axis',(-0.208614219207983,-0.97799800998992,-6.76296429840134E-17));
#120337=DIRECTION('ref_axis',(-0.97799800998992,0.208614219207983,3.85185988877447E-32));
#120338=DIRECTION('center_axis',(0.,0.,1.));
#120339=DIRECTION('ref_axis',(-0.222520933956304,-0.974927912181826,0.));
#120340=DIRECTION('center_axis',(-0.236382516515774,-0.971660077334491,
-1.38914942345546E-16));
#120341=DIRECTION('ref_axis',(0.971660077334492,-0.236382516515774,3.57452597678271E-31));
#120342=DIRECTION('center_axis',(0.,0.,-1.));
#120343=DIRECTION('ref_axis',(0.222520933956319,0.974927912181823,0.));
#120344=DIRECTION('center_axis',(0.,0.,1.));
#120345=DIRECTION('ref_axis',(-0.222520933956319,-0.974927912181823,0.));
#120346=DIRECTION('center_axis',(0.,0.,1.));
#120347=DIRECTION('ref_axis',(-0.222520933956319,-0.974927912181823,0.));
#120348=DIRECTION('center_axis',(-0.720140116213512,-0.202428074537138,
0.663642288932205));
#120349=DIRECTION('ref_axis',(-0.692815672802049,0.158130656272285,-0.703563173472532));
#120350=DIRECTION('center_axis',(-0.722211296949795,-0.203010273916155,
0.661209249211309));
#120351=DIRECTION('ref_axis',(-0.690567378811532,0.157617497840423,-0.705884848750768));
#120352=DIRECTION('center_axis',(0.562607037873186,-0.496261674616303,-0.661209249211308));
#120353=DIRECTION('ref_axis',(0.690567378811527,-0.157617497840443,0.705884848750768));
#120354=DIRECTION('center_axis',(0.560993575353487,-0.494838479458664,-0.663642288932184));
#120355=DIRECTION('ref_axis',(0.692815672802032,-0.158130656272272,0.703563173472552));
#120356=DIRECTION('center_axis',(0.,0.,1.));
#120357=DIRECTION('ref_axis',(-0.222520933956319,-0.974927912181823,0.));
#120358=DIRECTION('center_axis',(0.,0.,1.));
#120359=DIRECTION('ref_axis',(-0.222520933956319,-0.974927912181823,0.));
#120360=DIRECTION('center_axis',(0.,0.,1.));
#120361=DIRECTION('ref_axis',(0.222520933956214,0.974927912181846,0.));
#120362=DIRECTION('center_axis',(0.,0.,-1.));
#120363=DIRECTION('ref_axis',(-0.222520933956304,-0.974927912181826,0.));
#120364=DIRECTION('center_axis',(-0.708194252413252,-0.706017634941816,
0.));
#120365=DIRECTION('ref_axis',(0.706017634941816,-0.708194252413252,0.));
#120366=DIRECTION('',(0.,0.,1.));
#120367=DIRECTION('center_axis',(0.708197711263826,0.706014165407078,2.2859755326348E-6));
#120368=DIRECTION('ref_axis',(0.668333729574852,-0.670399694519265,-0.322326349374426));
#120369=DIRECTION('',(0.,0.,-1.));
#120370=DIRECTION('center_axis',(-0.208371918169447,0.978049663216743,0.));
#120371=DIRECTION('ref_axis',(-0.978049663216743,-0.208371918169447,0.));
#120372=DIRECTION('center_axis',(0.208371918169387,-0.978049663216756,-3.18487860976942E-14));
#120373=DIRECTION('ref_axis',(0.976736465712491,0.208092143539129,0.051802860391711));
#120374=DIRECTION('',(0.,0.,1.));
#120375=DIRECTION('',(0.,0.,1.));
#120376=DIRECTION('center_axis',(0.,0.,1.));
#120377=DIRECTION('ref_axis',(-0.28452758663103,-0.958667853036661,0.));
#120378=DIRECTION('center_axis',(0.,0.,-1.));
#120379=DIRECTION('ref_axis',(0.28452758663103,0.958667853036661,0.));
#120380=DIRECTION('center_axis',(0.494583756983005,0.83651228987544,-0.235868811452307));
#120381=DIRECTION('ref_axis',(-0.544144772498854,0.509642935979625,0.666461209950166));
#120382=DIRECTION('center_axis',(0.0418418858184532,0.9708837007465,0.235868811452332));
#120383=DIRECTION('ref_axis',(0.734069269910964,0.13027571767482,-0.666461209941504));
#120384=DIRECTION('center_axis',(0.,0.,-1.));
#120385=DIRECTION('ref_axis',(0.284527586631023,0.958667853036663,0.));
#120386=DIRECTION('center_axis',(-0.27084614656157,-0.962622649272678,-6.76296429840134E-17));
#120387=DIRECTION('ref_axis',(-0.962622649272678,0.27084614656157,2.46519032881566E-32));
#120388=DIRECTION('center_axis',(0.,0.,1.));
#120389=DIRECTION('ref_axis',(-0.284527586631023,-0.958667853036663,0.));
#120390=DIRECTION('center_axis',(-0.298151318184945,-0.954518617662631,
-1.38914942345546E-16));
#120391=DIRECTION('ref_axis',(0.954518617662631,-0.298151318184945,1.60237371373018E-31));
#120392=DIRECTION('center_axis',(0.,0.,-1.));
#120393=DIRECTION('ref_axis',(0.284527586631027,0.958667853036662,0.));
#120394=DIRECTION('center_axis',(0.,0.,1.));
#120395=DIRECTION('ref_axis',(-0.284527586631027,-0.958667853036662,0.));
#120396=DIRECTION('center_axis',(0.,0.,1.));
#120397=DIRECTION('ref_axis',(-0.284527586631027,-0.958667853036662,0.));
#120398=DIRECTION('center_axis',(-0.731630122375833,-0.155872628684923,
0.663642288932205));
#120399=DIRECTION('ref_axis',(-0.681260742764969,0.202194612442027,-0.703563173472532));
#120400=DIRECTION('center_axis',(-0.733734349291446,-0.156320930867481,
0.661209249211309));
#120401=DIRECTION('ref_axis',(-0.679049946309199,0.20153845965865,-0.705884848750767));
#120402=DIRECTION('center_axis',(0.529655506713796,-0.531288408461139,-0.661209249211308));
#120403=DIRECTION('ref_axis',(0.679049946309191,-0.201538459658669,0.705884848750769));
#120404=DIRECTION('center_axis',(0.528136543652713,-0.529764762512021,-0.663642288932184));
#120405=DIRECTION('ref_axis',(0.681260742764956,-0.202194612442008,0.70356317347255));
#120406=DIRECTION('center_axis',(0.,0.,1.));
#120407=DIRECTION('ref_axis',(-0.284527586631027,-0.958667853036662,0.));
#120408=DIRECTION('center_axis',(0.,0.,1.));
#120409=DIRECTION('ref_axis',(-0.284527586631027,-0.958667853036662,0.));
#120410=DIRECTION('center_axis',(0.,0.,1.));
#120411=DIRECTION('ref_axis',(0.284527586631061,0.958667853036652,0.));
#120412=DIRECTION('center_axis',(0.,0.,-1.));
#120413=DIRECTION('ref_axis',(-0.284527586631023,-0.958667853036663,0.));
#120414=DIRECTION('center_axis',(-0.751973896549059,-0.65919288444948,0.));
#120415=DIRECTION('ref_axis',(0.65919288444948,-0.751973896549059,0.));
#120416=DIRECTION('',(0.,0.,1.));
#120417=DIRECTION('center_axis',(0.751977125999241,0.659189200433909,2.28597558120709E-6));
#120418=DIRECTION('ref_axis',(0.62400791032486,-0.711842575497053,-0.322326349468552));
#120419=DIRECTION('',(0.,0.,-1.));
#120420=DIRECTION('center_axis',(-0.145279938641391,0.989390589923087,0.));
#120421=DIRECTION('ref_axis',(-0.989390589923087,-0.145279938641391,0.));
#120422=DIRECTION('center_axis',(0.145279938641321,-0.989390589923097,-3.55951442003013E-14));
#120423=DIRECTION('ref_axis',(0.988062165298661,0.145084875690556,0.0518028604536278));
#120424=DIRECTION('',(0.,0.,1.));
#120425=DIRECTION('',(0.,0.,1.));
#120426=DIRECTION('center_axis',(0.,0.,1.));
#120427=DIRECTION('ref_axis',(-0.345365054421307,-0.938468422049761,0.));
#120428=DIRECTION('center_axis',(0.,0.,-1.));
#120429=DIRECTION('ref_axis',(0.345365054421307,0.938468422049761,0.));
#120430=DIRECTION('center_axis',(0.547163108039205,0.803105495551452,-0.235868811452329));
#120431=DIRECTION('ref_axis',(-0.510373833698617,0.543459295189141,0.666461209935206));
#120432=DIRECTION('center_axis',(0.10396064945919,0.966208097227539,0.235868811452387));
#120433=DIRECTION('ref_axis',(0.740907839746693,0.0829760726401972,-0.66646120995231));
#120434=DIRECTION('center_axis',(0.,0.,-1.));
#120435=DIRECTION('ref_axis',(0.345365054421298,0.938468422049764,0.));
#120436=DIRECTION('center_axis',(-0.331965109002618,-0.943291665607664,
-6.76296429840134E-17));
#120437=DIRECTION('ref_axis',(-0.943291665607663,0.331965109002618,1.10933564796705E-31));
#120438=DIRECTION('center_axis',(0.,0.,1.));
#120439=DIRECTION('ref_axis',(-0.345365054421298,-0.938468422049764,0.));
#120440=DIRECTION('center_axis',(-0.358694952134436,-0.933454836247193,
-1.38914942345546E-16));
#120441=DIRECTION('ref_axis',(0.933454836247194,-0.358694952134436,1.14631350289928E-30));
#120442=DIRECTION('center_axis',(0.,0.,-1.));
#120443=DIRECTION('ref_axis',(0.345365054421306,0.938468422049761,0.));
#120444=DIRECTION('center_axis',(0.,0.,1.));
#120445=DIRECTION('ref_axis',(-0.345365054421306,-0.938468422049761,0.));
#120446=DIRECTION('center_axis',(0.,0.,1.));
#120447=DIRECTION('ref_axis',(-0.345365054421306,-0.938468422049761,0.));
#120448=DIRECTION('center_axis',(-0.740113703431142,-0.108676668766867,
0.663642288932205));
#120449=DIRECTION('ref_axis',(-0.666906366205898,0.245427707578635,-0.703563173472533));
#120450=DIRECTION('center_axis',(-0.742242329806334,-0.108989231583138,
0.661209249211309));
#120451=DIRECTION('ref_axis',(-0.664742151921725,0.24463125671627,-0.705884848750767));
#120452=DIRECTION('center_axis',(0.494527507466569,-0.564131964274601,-0.661209249211308));
#120453=DIRECTION('ref_axis',(0.664742151921719,-0.244631256716284,0.705884848750767));
#120454=DIRECTION('center_axis',(0.493109285609137,-0.56251412852203,-0.663642288932184));
#120455=DIRECTION('ref_axis',(0.66690636620588,-0.245427707578625,0.703563173472553));
#120456=DIRECTION('center_axis',(0.,0.,1.));
#120457=DIRECTION('ref_axis',(-0.345365054421309,-0.93846842204976,0.));
#120458=DIRECTION('center_axis',(0.,0.,1.));
#120459=DIRECTION('ref_axis',(-0.345365054421309,-0.93846842204976,0.));
#120460=DIRECTION('center_axis',(0.,0.,1.));
#120461=DIRECTION('ref_axis',(0.345365054421242,0.938468422049785,0.));
#120462=DIRECTION('center_axis',(0.,0.,-1.));
#120463=DIRECTION('ref_axis',(-0.345365054421298,-0.938468422049764,0.));
#120464=DIRECTION('center_axis',(-0.79266351864605,-0.609659368998511,0.));
#120465=DIRECTION('ref_axis',(0.609659368998511,-0.79266351864605,0.));
#120466=DIRECTION('',(0.,0.,1.));
#120467=DIRECTION('center_axis',(0.792666505425246,0.609655485640622,2.28597555338679E-6));
#120468=DIRECTION('ref_axis',(0.577117908741423,-0.750360342660638,-0.322326349484704));
#120469=DIRECTION('',(0.,0.,-1.));
#120470=DIRECTION('center_axis',(-0.0815909726830077,0.99666589847182,0.));
#120471=DIRECTION('ref_axis',(-0.99666589847182,-0.0815909726830077,0.));
#120472=DIRECTION('center_axis',(0.0815909726830078,-0.99666589847182,1.83998347318489E-15));
#120473=DIRECTION('ref_axis',(0.995327705518496,0.0814814229684379,0.0518028603295646));
#120474=DIRECTION('',(0.,0.,1.));
#120475=DIRECTION('',(0.,0.,1.));
#120476=DIRECTION('center_axis',(0.,0.,1.));
#120477=DIRECTION('ref_axis',(-0.40478334312238,-0.914412623015818,0.));
#120478=DIRECTION('center_axis',(0.,0.,-1.));
#120479=DIRECTION('ref_axis',(0.40478334312238,0.914412623015818,0.));
#120480=DIRECTION('center_axis',(0.597494048518593,0.766398568480514,-0.235868811452214));
#120481=DIRECTION('ref_axis',(-0.474505659311212,0.575042463572137,0.666461209951876));
#120482=DIRECTION('center_axis',(0.165652216491514,0.957562137386137,0.235868811452343));
#120483=DIRECTION('ref_axis',(0.744701860364663,0.0353354611175966,-0.666461209941747));
#120484=DIRECTION('center_axis',(0.,0.,-1.));
#120485=DIRECTION('ref_axis',(0.404783343122385,0.914412623015816,0.));
#120486=DIRECTION('center_axis',(-0.391719955604482,-0.920084494153239,
-6.76296429840134E-17));
#120487=DIRECTION('ref_axis',(-0.920084494153239,0.391719955604482,7.9810536895407E-31));
#120488=DIRECTION('center_axis',(0.,0.,1.));
#120489=DIRECTION('ref_axis',(-0.404783343122385,-0.914412623015816,0.));
#120490=DIRECTION('center_axis',(-0.417764631585781,-0.908555288684182,
-1.38914942345546E-16));
#120491=DIRECTION('ref_axis',(0.908555288684182,-0.417764631585781,-6.71764364602268E-31));
#120492=DIRECTION('center_axis',(0.,0.,-1.));
#120493=DIRECTION('ref_axis',(0.404783343122381,0.914412623015818,0.));
#120494=DIRECTION('center_axis',(0.,0.,1.));
#120495=DIRECTION('ref_axis',(-0.404783343122381,-0.914412623015818,0.));
#120496=DIRECTION('center_axis',(0.,0.,1.));
#120497=DIRECTION('ref_axis',(-0.404783343122381,-0.914412623015818,0.));
#120498=DIRECTION('center_axis',(-0.745555998525161,-0.0610341331057755,
0.663642288932205));
#120499=DIRECTION('ref_axis',(-0.64981152833712,0.287652287620717,-0.703563173472535));
#120500=DIRECTION('center_axis',(-0.747700277377567,-0.0612096721681029,
0.661209249211309));
#120501=DIRECTION('ref_axis',(-0.64770278944526,0.286718811466798,-0.705884848750769));
#120502=DIRECTION('center_axis',(0.457367388615345,-0.594657380840933,-0.661209249211308));
#120503=DIRECTION('ref_axis',(0.647702789445253,-0.286718811466818,0.705884848750767));
#120504=DIRECTION('center_axis',(0.456055735739382,-0.59295200331904,-0.663642288932184));
#120505=DIRECTION('ref_axis',(0.649811528337101,-0.287652287620715,0.703563173472553));
#120506=DIRECTION('center_axis',(0.,0.,1.));
#120507=DIRECTION('ref_axis',(-0.404783343122381,-0.914412623015818,0.));
#120508=DIRECTION('center_axis',(0.,0.,1.));
#120509=DIRECTION('ref_axis',(-0.404783343122381,-0.914412623015818,0.));
#120510=DIRECTION('center_axis',(0.,0.,1.));
#120511=DIRECTION('ref_axis',(0.404783343122381,0.914412623015818,0.));
#120512=DIRECTION('center_axis',(0.,0.,-1.));
#120513=DIRECTION('ref_axis',(-0.404783343122385,-0.914412623015816,0.));
#120514=DIRECTION('center_axis',(-0.830095916319133,-0.557620632428803,
0.));
#120515=DIRECTION('ref_axis',(0.557620632428803,-0.830095916319133,0.));
#120516=DIRECTION('',(0.,0.,1.));
#120517=DIRECTION('center_axis',(0.830098648154146,0.557616565685985,2.28597558462761E-6));
#120518=DIRECTION('ref_axis',(0.527856405870552,-0.78579471821007,-0.322326349550545));
#120519=DIRECTION('',(0.,0.,-1.));
#120520=DIRECTION('center_axis',(-0.017566731916662,0.999845693059568,0.));
#120521=DIRECTION('ref_axis',(-0.999845693059568,-0.017566731916662,0.));
#120522=DIRECTION('center_axis',(0.0175667319166711,-0.999845693059568,
8.91538383914289E-16));
#120523=DIRECTION('ref_axis',(0.998503230687169,0.0175431456005347,0.0518028604396023));
#120524=DIRECTION('',(0.,0.,1.));
#120525=DIRECTION('',(0.,0.,1.));
#120526=DIRECTION('center_axis',(0.,0.,1.));
#120527=DIRECTION('ref_axis',(-0.46253829024085,-0.886599306372992,0.));
#120528=DIRECTION('center_axis',(0.,0.,-1.));
#120529=DIRECTION('ref_axis',(0.46253829024085,0.886599306372992,0.));
#120530=DIRECTION('center_axis',(0.645369757790118,0.726542345299973,-0.235868811452341));
#120531=DIRECTION('ref_axis',(-0.436687639413051,0.604262659136266,0.666461209942054));
#120532=DIRECTION('center_axis',(0.226663083034076,0.944981349325769,0.235868811452334));
#120533=DIRECTION('ref_axis',(0.745435741282765,-0.0124503513865644,-0.666461209950411));
#120534=DIRECTION('center_axis',(0.,0.,-1.));
#120535=DIRECTION('ref_axis',(0.462538290240827,0.886599306373005,0.));
#120536=DIRECTION('center_axis',(-0.4498651408851,-0.893096498154835,-6.76296429840134E-17));
#120537=DIRECTION('ref_axis',(-0.893096498154835,0.4498651408851,-4.19082355898662E-31));
#120538=DIRECTION('center_axis',(0.,0.,1.));
#120539=DIRECTION('ref_axis',(-0.462538290240827,-0.886599306373005,0.));
#120540=DIRECTION('center_axis',(-0.475117626555707,-0.879922292555468,
-1.38914942345546E-16));
#120541=DIRECTION('ref_axis',(0.879922292555468,-0.475117626555707,-1.84889274661175E-31));
#120542=DIRECTION('center_axis',(0.,0.,-1.));
#120543=DIRECTION('ref_axis',(0.462538290240815,0.886599306373011,0.));
#120544=DIRECTION('center_axis',(0.,0.,1.));
#120545=DIRECTION('ref_axis',(-0.462538290240815,-0.886599306373011,0.));
#120546=DIRECTION('center_axis',(0.,0.,1.));
#120547=DIRECTION('ref_axis',(-0.462538290240815,-0.886599306373011,0.));
#120548=DIRECTION('center_axis',(-0.74793464409998,-0.0131407950999725,
0.663642288932205));
#120549=DIRECTION('ref_axis',(-0.630046475514267,0.328694842711764,-0.703563173472532));
#120550=DIRECTION('center_axis',(-0.750085764127849,-0.0131785890806962,
0.661209249211309));
#120551=DIRECTION('ref_axis',(-0.628001877275151,0.327628177120031,-0.705884848750766));
#120552=DIRECTION('center_axis',(0.418327849059303,-0.62273922267578,-0.661209249211308));
#120553=DIRECTION('ref_axis',(0.628001877275142,-0.327628177120044,0.705884848750768));
#120554=DIRECTION('center_axis',(0.417128155027826,-0.620953311146606,-0.663642288932184));
#120555=DIRECTION('ref_axis',(0.63004647551425,-0.328694842711749,0.703563173472554));
#120556=DIRECTION('center_axis',(0.,0.,1.));
#120557=DIRECTION('ref_axis',(-0.462538290240815,-0.886599306373011,0.));
#120558=DIRECTION('center_axis',(0.,0.,1.));
#120559=DIRECTION('ref_axis',(-0.462538290240815,-0.886599306373011,0.));
#120560=DIRECTION('center_axis',(0.,0.,1.));
#120561=DIRECTION('ref_axis',(0.462538290240815,0.886599306373011,0.));
#120562=DIRECTION('center_axis',(0.,0.,-1.));
#120563=DIRECTION('ref_axis',(-0.462538290240827,-0.886599306373005,0.));
#120564=DIRECTION('center_axis',(0.932256674534463,-0.361797585378819,0.));
#120565=DIRECTION('ref_axis',(0.361797585378819,0.932256674534463,0.));
#120566=DIRECTION('',(0.,0.,1.));
#120567=DIRECTION('center_axis',(-0.932254902033239,0.361802152605218,2.28597549637726E-6));
#120568=DIRECTION('ref_axis',(0.34249158175089,0.882499428274317,-0.322326349412015));
#120569=DIRECTION('',(0.,0.,-1.));
#120570=DIRECTION('center_axis',(-0.809995476332305,-0.586436124672757,
0.));
#120571=DIRECTION('ref_axis',(0.586436124672757,-0.809995476332305,0.));
#120572=DIRECTION('center_axis',(0.809995476332245,0.586436124672841,4.63599959635485E-14));
#120573=DIRECTION('ref_axis',(0.585648734744104,-0.808907920068986,-0.0518028603679146));
#120574=DIRECTION('',(0.,0.,1.));
#120575=DIRECTION('',(0.,0.,1.));
#120576=DIRECTION('center_axis',(0.,0.,1.));
#120577=DIRECTION('ref_axis',(0.991790013823243,0.127877161684531,0.));
#120578=DIRECTION('center_axis',(0.,0.,-1.));
#120579=DIRECTION('ref_axis',(-0.991790013823243,-0.127877161684531,0.));
#120580=DIRECTION('center_axis',(-0.965116663775573,0.113647389265203,-0.235868811452279));
#120581=DIRECTION('ref_axis',(0.245763193734801,0.703867820154899,-0.666461209940729));
#120582=DIRECTION('center_axis',(-0.904725209867097,-0.354736801607849,
0.235868811452407));
#120583=DIRECTION('ref_axis',(0.416264773870225,-0.618508766031246,0.666461209956945));
#120584=DIRECTION('center_axis',(0.,0.,-1.));
#120585=DIRECTION('ref_axis',(-0.991790013823246,-0.127877161684506,0.));
#120586=DIRECTION('center_axis',(0.989868310372871,0.14198847882683,-6.76296429840134E-17));
#120587=DIRECTION('ref_axis',(0.14198847882683,-0.989868310372871,-2.31111593326468E-32));
#120588=DIRECTION('center_axis',(0.,0.,1.));
#120589=DIRECTION('ref_axis',(0.991790013823246,0.127877161684506,0.));
#120590=DIRECTION('center_axis',(0.993510560225565,0.113739908212919,-1.38914942345546E-16));
#120591=DIRECTION('ref_axis',(-0.113739908212919,0.993510560225565,-3.57452597678271E-31));
#120592=DIRECTION('center_axis',(0.,0.,-1.));
#120593=DIRECTION('ref_axis',(-0.991790013823245,-0.127877161684511,0.));
#120594=DIRECTION('center_axis',(0.,0.,1.));
#120595=DIRECTION('ref_axis',(0.991790013823245,0.127877161684511,0.));
#120596=DIRECTION('center_axis',(0.,0.,1.));
#120597=DIRECTION('ref_axis',(0.991790013823245,0.127877161684512,0.));
#120598=DIRECTION('center_axis',(0.43868358611648,-0.605917175538711,0.663642288932205));
#120599=DIRECTION('ref_axis',(0.0908736950716699,-0.704798433935035,-0.703563173472534));
#120600=DIRECTION('center_axis',(0.439945275296726,-0.607659841935852,0.661209249211309));
#120601=DIRECTION('ref_axis',(0.0905787958790825,-0.702511254031707,-0.705884848750768));
#120602=DIRECTION('center_axis',(0.271421100448058,0.699380379328004,-0.661209249211308));
#120603=DIRECTION('ref_axis',(-0.0905787958790601,0.702511254031708,0.705884848750769));
#120604=DIRECTION('center_axis',(0.270642710305121,0.697374673830037,-0.663642288932184));
#120605=DIRECTION('ref_axis',(-0.090873695071669,0.704798433935017,0.703563173472552));
#120606=DIRECTION('center_axis',(0.,0.,1.));
#120607=DIRECTION('ref_axis',(0.991790013823245,0.127877161684511,0.));
#120608=DIRECTION('center_axis',(0.,0.,1.));
#120609=DIRECTION('ref_axis',(0.991790013823245,0.127877161684511,0.));
#120610=DIRECTION('center_axis',(0.,0.,1.));
#120611=DIRECTION('ref_axis',(-0.991790013823245,-0.127877161684511,0.));
#120612=DIRECTION('center_axis',(0.,0.,-1.));
#120613=DIRECTION('ref_axis',(0.991790013823246,0.127877161684506,0.));
#120614=DIRECTION('center_axis',(0.953521704096129,-0.301324343221078,0.));
#120615=DIRECTION('ref_axis',(0.301324343221078,0.953521704096129,0.));
#120616=DIRECTION('',(0.,0.,1.));
#120617=DIRECTION('center_axis',(-0.953520227859872,0.301329014628251,2.28597553491565E-6));
#120618=DIRECTION('ref_axis',(0.285245963560465,0.902629749531369,-0.322326349424615));
#120619=DIRECTION('',(0.,0.,-1.));
#120620=DIRECTION('center_axis',(-0.770758162242018,-0.637127817111533,
0.));
#120621=DIRECTION('ref_axis',(0.637127817111533,-0.770758162242018,0.));
#120622=DIRECTION('center_axis',(0.770758162241952,0.637127817111612,3.80136791779655E-14));
#120623=DIRECTION('ref_axis',(0.636272364989511,-0.769723288723939,-0.0518028604099999));
#120624=DIRECTION('',(0.,0.,1.));
#120625=DIRECTION('',(0.,0.,1.));
#120626=DIRECTION('center_axis',(0.,0.,1.));
#120627=DIRECTION('ref_axis',(0.981559156991069,0.191158628701354,0.));
#120628=DIRECTION('center_axis',(0.,0.,-1.));
#120629=DIRECTION('ref_axis',(-0.981559156991069,-0.191158628701354,0.));
#120630=DIRECTION('center_axis',(-0.970415141311867,0.051578651560199,-0.235868811452257));
#120631=DIRECTION('ref_axis',(0.20016128082009,0.718167750117156,-0.666461209938076));
#120632=DIRECTION('center_axis',(-0.880138289977527,-0.411973900022255,
0.235868811452231));
#120633=DIRECTION('ref_axis',(0.455037505952914,-0.590567797830352,0.66646120993045));
#120634=DIRECTION('center_axis',(0.,0.,-1.));
#120635=DIRECTION('ref_axis',(-0.981559156991065,-0.191158628701373,0.));
#120636=DIRECTION('center_axis',(0.978737286693005,0.205117828666391,-6.76296429840134E-17));
#120637=DIRECTION('ref_axis',(0.205117828666391,-0.978737286693005,-2.28030105415449E-31));
#120638=DIRECTION('center_axis',(0.,0.,1.));
#120639=DIRECTION('ref_axis',(0.981559156991065,0.191158628701373,0.));
#120640=DIRECTION('center_axis',(0.984181945286121,0.177160657519742,-1.38914942345546E-16));
#120641=DIRECTION('ref_axis',(-0.177160657519742,0.984181945286121,-2.40356057059527E-31));
#120642=DIRECTION('center_axis',(0.,0.,-1.));
#120643=DIRECTION('ref_axis',(-0.981559156991067,-0.191158628701365,0.));
#120644=DIRECTION('center_axis',(0.,0.,1.));
#120645=DIRECTION('ref_axis',(0.981559156991067,0.191158628701365,0.));
#120646=DIRECTION('center_axis',(0.,0.,1.));
#120647=DIRECTION('ref_axis',(0.981559156991067,0.191158628701365,0.));
#120648=DIRECTION('center_axis',(0.476603510366994,-0.576565699852742,0.663642288932205));
#120649=DIRECTION('ref_axis',(0.135843576023249,-0.69752805232942,-0.703563173472533));
#120650=DIRECTION('center_axis',(0.477974260290922,-0.578223949051545,0.661209249211309));
#120651=DIRECTION('ref_axis',(0.135402742613138,-0.695264465938644,-0.705884848750766));
#120652=DIRECTION('center_axis',(0.226053981933626,0.715333436943479,-0.661209249211308));
#120653=DIRECTION('ref_axis',(-0.135402742613124,0.695264465938645,0.705884848750768));
#120654=DIRECTION('center_axis',(0.225405697069191,0.713281980754879,-0.663642288932184));
#120655=DIRECTION('ref_axis',(-0.13584357602325,0.697528052329401,0.703563173472552));
#120656=DIRECTION('center_axis',(0.,0.,1.));
#120657=DIRECTION('ref_axis',(0.981559156991067,0.191158628701365,0.));
#120658=DIRECTION('center_axis',(0.,0.,1.));
#120659=DIRECTION('ref_axis',(0.981559156991067,0.191158628701365,0.));
#120660=DIRECTION('center_axis',(0.,0.,1.));
#120661=DIRECTION('ref_axis',(-0.981559156991073,-0.191158628701331,0.));
#120662=DIRECTION('center_axis',(0.,0.,-1.));
#120663=DIRECTION('ref_axis',(0.981559156991065,0.191158628701373,0.));
#120664=DIRECTION('center_axis',(0.9708685084459,-0.239612894703173,0.));
#120665=DIRECTION('ref_axis',(0.239612894703173,0.9708685084459,0.));
#120666=DIRECTION('',(0.,0.,1.));
#120667=DIRECTION('center_axis',(-0.97086733454081,0.239617651095234,2.28597555627519E-6));
#120668=DIRECTION('ref_axis',(0.226828208513217,0.919050971501784,-0.322326349534615));
#120669=DIRECTION('',(0.,0.,-1.));
#120670=DIRECTION('center_axis',(-0.72835363753597,-0.68520141468631,0.));
#120671=DIRECTION('ref_axis',(0.68520141468631,-0.72835363753597,0.));
#120672=DIRECTION('center_axis',(0.728353637535986,0.685201414686293,-1.66926335711597E-15));
#120673=DIRECTION('ref_axis',(0.684281415609636,-0.727375699283596,-0.0518028603744199));
#120674=DIRECTION('',(0.,0.,1.));
#120675=DIRECTION('',(0.,0.,1.));
#120676=DIRECTION('center_axis',(0.,0.,1.));
#120677=DIRECTION('ref_axis',(0.967294863039035,0.253654583909488,0.));
#120678=DIRECTION('center_axis',(0.,0.,-1.));
#120679=DIRECTION('ref_axis',(-0.967294863039035,-0.253654583909488,0.));
#120680=DIRECTION('center_axis',(-0.971725974879091,-0.0107020338879219,
-0.235868811452346));
#120681=DIRECTION('ref_axis',(0.153736862267503,0.729516574747913,-0.666461209935144));
#120682=DIRECTION('center_axis',(-0.851934693065551,-0.467518109312767,
0.235868811452302));
#120683=DIRECTION('ref_axis',(0.49194039131489,-0.560200059846077,0.666461209930034));
#120684=DIRECTION('center_axis',(0.,0.,-1.));
#120685=DIRECTION('ref_axis',(-0.967294863039029,-0.253654583909508,0.));
#120686=DIRECTION('center_axis',(0.963584421563627,0.267404305350324,-6.76296429840134E-17));
#120687=DIRECTION('ref_axis',(0.267404305350324,-0.963584421563627,-1.84889274661175E-32));
#120688=DIRECTION('center_axis',(0.,0.,1.));
#120689=DIRECTION('ref_axis',(0.967294863039029,0.253654583909508,0.));
#120690=DIRECTION('center_axis',(0.97080911562713,0.239853415683975,-1.38914942345546E-16));
#120691=DIRECTION('ref_axis',(-0.239853415683975,0.97080911562713,1.60237371373018E-31));
#120692=DIRECTION('center_axis',(0.,0.,-1.));
#120693=DIRECTION('ref_axis',(-0.967294863039032,-0.253654583909497,0.));
#120694=DIRECTION('center_axis',(0.,0.,1.));
#120695=DIRECTION('ref_axis',(0.967294863039032,0.253654583909497,0.));
#120696=DIRECTION('center_axis',(0.,0.,1.));
#120697=DIRECTION('ref_axis',(0.967294863039032,0.253654583909497,0.));
#120698=DIRECTION('center_axis',(0.512564968562278,-0.544844992033124,0.663642288932205));
#120699=DIRECTION('ref_axis',(0.180255246582588,-0.687391378337488,-0.703563173472531));
#120700=DIRECTION('center_axis',(0.514039146524425,-0.546412009931936,0.661209249211309));
#120701=DIRECTION('ref_axis',(0.179670290434003,-0.685160687021277,-0.705884848750767));
#120702=DIRECTION('center_axis',(0.179757959119001,0.728347036028012,-0.661209249211308));
#120703=DIRECTION('ref_axis',(-0.179670290433984,0.68516068702128,0.705884848750769));
#120704=DIRECTION('center_axis',(0.179242443474634,0.726258259022295,-0.663642288932184));
#120705=DIRECTION('ref_axis',(-0.180255246582597,0.687391378337464,0.703563173472552));
#120706=DIRECTION('center_axis',(0.,0.,1.));
#120707=DIRECTION('ref_axis',(0.967294863039032,0.253654583909497,0.));
#120708=DIRECTION('center_axis',(0.,0.,1.));
#120709=DIRECTION('ref_axis',(0.967294863039032,0.253654583909497,0.));
#120710=DIRECTION('center_axis',(0.,0.,1.));
#120711=DIRECTION('ref_axis',(-0.967294863039023,-0.25365458390953,0.));
#120712=DIRECTION('center_axis',(0.,0.,-1.));
#120713=DIRECTION('ref_axis',(0.967294863039029,0.253654583909508,0.));
#120714=DIRECTION('center_axis',(0.984225805843825,-0.176916825404127,0.));
#120715=DIRECTION('ref_axis',(0.176916825404127,0.984225805843824,0.));
#120716=DIRECTION('',(0.,0.,1.));
#120717=DIRECTION('center_axis',(-0.984224939093732,0.176921647236042,2.28597555699675E-6));
#120718=DIRECTION('ref_axis',(0.167478367719591,0.93169561596139,-0.322326349441536));
#120719=DIRECTION('',(0.,0.,-1.));
#120720=DIRECTION('center_axis',(-0.682956151501922,-0.730459372672898,
0.));
#120721=DIRECTION('ref_axis',(0.730459372672898,-0.682956151501922,0.));
#120722=DIRECTION('center_axis',(0.682956151501907,0.730459372672912,-3.56615353565696E-15));
#120723=DIRECTION('ref_axis',(0.729478607113612,-0.682039167071338,-0.0518028603864715));
#120724=DIRECTION('',(0.,0.,1.));
#120725=DIRECTION('',(0.,0.,1.));
#120726=DIRECTION('center_axis',(0.,0.,1.));
#120727=DIRECTION('ref_axis',(0.949055747010676,0.315108218023599,0.));
#120728=DIRECTION('center_axis',(0.,0.,-1.));
#120729=DIRECTION('ref_axis',(-0.949055747010676,-0.315108218023599,0.));
#120730=DIRECTION('center_axis',(-0.969043777980947,-0.0729387423831519,
-0.235868811452418));
#120731=DIRECTION('ref_axis',(0.106680705980105,0.737867659264888,-0.666461209960896));
#120732=DIRECTION('center_axis',(-0.820230313760265,-0.521141186410019,
0.235868811452246));
#120733=DIRECTION('ref_axis',(0.52682178808489,-0.527530339643357,0.666461209940087));
#120734=DIRECTION('center_axis',(0.,0.,-1.));
#120735=DIRECTION('ref_axis',(-0.949055747010669,-0.315108218023621,0.));
#120736=DIRECTION('center_axis',(0.944471981357835,0.32859196038553,-6.76296429840134E-17));
#120737=DIRECTION('ref_axis',(0.32859196038553,-0.944471981357835,1.60237371373018E-31));
#120738=DIRECTION('center_axis',(0.,0.,1.));
#120739=DIRECTION('ref_axis',(0.949055747010668,0.315108218023621,0.));
#120740=DIRECTION('center_axis',(0.953447023074125,0.301560564714766,-1.38914942345546E-16));
#120741=DIRECTION('ref_axis',(-0.301560564714766,0.953447023074125,-9.4909827659403E-31));
#120742=DIRECTION('center_axis',(0.,0.,-1.));
#120743=DIRECTION('ref_axis',(-0.949055747010673,-0.315108218023608,0.));
#120744=DIRECTION('center_axis',(0.,0.,1.));
#120745=DIRECTION('ref_axis',(0.949055747010673,0.315108218023608,0.));
#120746=DIRECTION('center_axis',(0.,0.,1.));
#120747=DIRECTION('ref_axis',(0.949055747010672,0.31510821802361,0.));
#120748=DIRECTION('center_axis',(0.546420187356898,-0.510885399272357,0.663642288932205));
#120749=DIRECTION('ref_axis',(0.223926209669101,-0.674430065726973,-0.703563173472532));
#120750=DIRECTION('center_axis',(0.547991735643807,-0.512354746658509,0.661209249211309));
#120751=DIRECTION('ref_axis',(0.223199534492313,-0.672241435874437,-0.705884848750765));
#120752=DIRECTION('center_axis',(0.132723272292395,0.738367700911556,-0.661209249211308));
#120753=DIRECTION('ref_axis',(-0.223199534492297,0.672241435874437,0.70588484875077));
#120754=DIRECTION('center_axis',(0.132342644232455,0.73625018632148,-0.663642288932184));
#120755=DIRECTION('ref_axis',(-0.223926209669108,0.674430065726951,0.703563173472551));
#120756=DIRECTION('center_axis',(0.,0.,1.));
#120757=DIRECTION('ref_axis',(0.949055747010673,0.315108218023608,0.));
#120758=DIRECTION('center_axis',(0.,0.,1.));
#120759=DIRECTION('ref_axis',(0.949055747010673,0.315108218023608,0.));
#120760=DIRECTION('center_axis',(0.,0.,1.));
#120761=DIRECTION('ref_axis',(-0.949055747010661,-0.315108218023644,0.));
#120762=DIRECTION('center_axis',(0.,0.,-1.));
#120763=DIRECTION('ref_axis',(0.949055747010669,0.315108218023621,0.));
#120764=DIRECTION('center_axis',(0.993538708289764,-0.113493766920956,0.));
#120765=DIRECTION('ref_axis',(0.113493766920956,0.993538708289764,0.));
#120766=DIRECTION('',(0.,0.,1.));
#120767=DIRECTION('center_axis',(-0.993538152256329,0.113498634378806,2.28597556007661E-6));
#120768=DIRECTION('ref_axis',(0.10744032238041,0.940511723247201,-0.322326349468011));
#120769=DIRECTION('',(0.,0.,-1.));
#120770=DIRECTION('center_axis',(-0.634752252147718,-0.772715716414129,
0.));
#120771=DIRECTION('ref_axis',(0.772715716414129,-0.634752252147718,0.));
#120772=DIRECTION('center_axis',(0.634752252147689,0.772715716414153,3.29300134994633E-14));
#120773=DIRECTION('ref_axis',(0.771678214545083,-0.633899989622142,-0.0518028604766313));
#120774=DIRECTION('',(0.,0.,1.));
#120775=DIRECTION('',(0.,0.,1.));
#120776=DIRECTION('center_axis',(0.,0.,1.));
#120777=DIRECTION('ref_axis',(0.926916757346018,0.375267004879383,0.));
#120778=DIRECTION('center_axis',(0.,0.,-1.));
#120779=DIRECTION('ref_axis',(-0.926916757346018,-0.375267004879383,0.));
#120780=DIRECTION('center_axis',(-0.962379572339892,-0.134875729940312,
-0.235868811452373));
#120781=DIRECTION('ref_axis',(0.0591861757772453,0.743186687335741,-0.66646120994683));
#120782=DIRECTION('center_axis',(-0.785155432157059,-0.572622782587562,
0.235868811452338));
#120783=DIRECTION('ref_axis',(0.55953836112639,-0.492692884128054,0.666461209942165));
#120784=DIRECTION('center_axis',(0.,0.,-1.));
#120785=DIRECTION('ref_axis',(-0.926916757346021,-0.375267004879375,0.));
#120786=DIRECTION('center_axis',(0.921478503192038,0.388429360572757,-6.76296429840134E-17));
#120787=DIRECTION('ref_axis',(0.388429360572757,-0.921478503192038,-1.63318859284038E-31));
#120788=DIRECTION('center_axis',(0.,0.,1.));
#120789=DIRECTION('ref_axis',(0.926916757346021,0.375267004879375,0.));
#120790=DIRECTION('center_axis',(0.932167012189564,0.362028536700605,-1.38914942345546E-16));
#120791=DIRECTION('ref_axis',(-0.362028536700605,0.932167012189564,4.62223186652937E-31));
#120792=DIRECTION('center_axis',(0.,0.,-1.));
#120793=DIRECTION('ref_axis',(-0.92691675734602,-0.375267004879378,0.));
#120794=DIRECTION('center_axis',(0.,0.,1.));
#120795=DIRECTION('ref_axis',(0.92691675734602,0.375267004879378,0.));
#120796=DIRECTION('center_axis',(0.,0.,1.));
#120797=DIRECTION('ref_axis',(0.92691675734602,0.375267004879378,0.));
#120798=DIRECTION('center_axis',(0.578030048394907,-0.474826468821406,0.663642288932205));
#120799=DIRECTION('ref_axis',(0.26667701192807,-0.658697375311585,-0.703563173472536));
#120800=DIRECTION('center_axis',(0.579692509177571,-0.476192107831313,0.661209249211309));
#120801=DIRECTION('ref_axis',(0.26581160378726,-0.656559800472242,-0.705884848750769));
#120802=DIRECTION('center_axis',(0.0851431970708876,0.745354254532679,-0.661209249211308));
#120803=DIRECTION('ref_axis',(-0.265811603787243,0.65655980047225,0.705884848750767));
#120804=DIRECTION('center_axis',(0.0848990206777172,0.7432167036799,-0.663642288932184));
#120805=DIRECTION('ref_axis',(-0.266677011928067,0.65869737531157,0.70356317347255));
#120806=DIRECTION('center_axis',(0.,0.,1.));
#120807=DIRECTION('ref_axis',(0.926916757346019,0.375267004879381,0.));
#120808=DIRECTION('center_axis',(0.,0.,1.));
#120809=DIRECTION('ref_axis',(0.926916757346019,0.375267004879381,0.));
#120810=DIRECTION('center_axis',(0.,0.,1.));
#120811=DIRECTION('ref_axis',(-0.926916757346005,-0.375267004879417,0.));
#120812=DIRECTION('center_axis',(0.,0.,-1.));
#120813=DIRECTION('ref_axis',(0.926916757346021,0.375267004879375,0.));
#120814=DIRECTION('center_axis',(0.998768947069955,-0.0496043382051697,
0.));
#120815=DIRECTION('ref_axis',(0.0496043382051697,0.998768947069955,0.));
#120816=DIRECTION('',(0.,0.,1.));
#120817=DIRECTION('center_axis',(-0.998768704038047,0.0496092312874756,
2.28597555336781E-6));
#120818=DIRECTION('ref_axis',(0.0469607817104218,0.945463066095288,-0.322326349575773));
#120819=DIRECTION('',(0.,0.,-1.));
#120820=DIRECTION('center_axis',(-0.583940019635507,-0.811796805529612,
0.));
#120821=DIRECTION('ref_axis',(0.811796805529613,-0.583940019635507,0.));
#120822=DIRECTION('center_axis',(0.583940019635613,0.811796805529536,-6.02452320704585E-14));
#120823=DIRECTION('ref_axis',(0.810706830674114,-0.583155981149456,-0.0518028604224596));
#120824=DIRECTION('',(0.,0.,1.));
#120825=DIRECTION('',(0.,0.,1.));
#120826=DIRECTION('center_axis',(0.,0.,1.));
#120827=DIRECTION('ref_axis',(0.900968867902417,0.433883739117562,0.));
#120828=DIRECTION('center_axis',(0.,0.,-1.));
#120829=DIRECTION('ref_axis',(-0.900968867902417,-0.433883739117562,0.));
#120830=DIRECTION('center_axis',(-0.951760742606324,-0.196258484192461,
-0.235868811452332));
#120831=DIRECTION('ref_axis',(0.0114484368858726,0.74545180188451,-0.66646120994399));
#120832=DIRECTION('center_axis',(-0.746854178467695,-0.621751348924477,
0.235868811452334));
#120833=DIRECTION('ref_axis',(0.589955671023616,-0.455830847874484,0.666461209938811));
#120834=DIRECTION('center_axis',(0.,0.,-1.));
#120835=DIRECTION('ref_axis',(-0.900968867902419,-0.433883739117559,0.));
#120836=DIRECTION('center_axis',(0.894698472200106,0.446670621199554,-6.76296429840134E-17));
#120837=DIRECTION('ref_axis',(0.446670621199554,-0.894698472200106,6.93889390390721E-14));
#120838=DIRECTION('center_axis',(0.,0.,1.));
#120839=DIRECTION('ref_axis',(0.900968867902419,0.433883739117559,0.));
#120840=DIRECTION('center_axis',(0.907056527102719,0.421008855774264,-1.38914942345546E-16));
#120841=DIRECTION('ref_axis',(-0.421008855774264,0.907056527102718,-1.26957301934007E-30));
#120842=DIRECTION('center_axis',(0.,0.,-1.));
#120843=DIRECTION('ref_axis',(-0.900968867902412,-0.433883739117574,0.));
#120844=DIRECTION('center_axis',(0.,0.,1.));
#120845=DIRECTION('ref_axis',(0.900968867902412,0.433883739117574,0.));
#120846=DIRECTION('center_axis',(0.,0.,1.));
#120847=DIRECTION('ref_axis',(0.900968867902412,0.433883739117574,0.));
#120848=DIRECTION('center_axis',(0.607264659977004,-0.43681637456011,0.663642288932205));
#120849=DIRECTION('ref_axis',(0.308331981142967,-0.640257956090912,-0.703563173472532));
#120850=DIRECTION('center_axis',(0.60901120184747,-0.438072693490152,0.661209249211309));
#120851=DIRECTION('ref_axis',(0.307331396185821,-0.63818022001828,-0.705884848750768));
#120852=DIRECTION('center_axis',(0.0372132501894571,0.749277987643942,-0.661209249211308));
#120853=DIRECTION('ref_axis',(-0.307331396185796,0.638180220018289,0.70588484875077));
#120854=DIRECTION('center_axis',(0.0371065288362318,0.747129184183417,-0.663642288932184));
#120855=DIRECTION('ref_axis',(-0.308331981142974,0.64025795609089,0.70356317347255));
#120856=DIRECTION('center_axis',(0.,0.,1.));
#120857=DIRECTION('ref_axis',(0.900968867902412,0.433883739117574,0.));
#120858=DIRECTION('center_axis',(0.,0.,1.));
#120859=DIRECTION('ref_axis',(0.900968867902412,0.433883739117574,0.));
#120860=DIRECTION('center_axis',(0.,0.,1.));
#120861=DIRECTION('ref_axis',(-0.900968867902445,-0.433883739117504,0.));
#120862=DIRECTION('center_axis',(0.,0.,-1.));
#120863=DIRECTION('ref_axis',(0.900968867902419,0.433883739117559,0.));
#120864=DIRECTION('center_axis',(0.999895030011369,0.0144889253763986,0.));
#120865=DIRECTION('ref_axis',(-0.0144889253763986,0.999895030011369,0.));
#120866=DIRECTION('',(0.,0.,1.));
#120867=DIRECTION('center_axis',(-0.999895100979656,-0.0144840267763469,
2.28597557413844E-6));
#120868=DIRECTION('ref_axis',(0.01371173088091,-0.946529298468286,0.322326349492845));
#120869=DIRECTION('',(0.,0.,-1.));
#120870=DIRECTION('center_axis',(-0.530728252327873,-0.847542047441306,
0.));
#120871=DIRECTION('ref_axis',(0.847542047441306,-0.530728252327873,0.));
#120872=DIRECTION('center_axis',(0.530728252327903,0.847542047441288,-2.55700796067318E-14));
#120873=DIRECTION('ref_axis',(0.846404078537503,-0.530015659661461,-0.0518028604297697));
#120874=DIRECTION('',(0.,0.,1.));
#120875=DIRECTION('',(0.,0.,1.));
#120876=DIRECTION('center_axis',(0.,0.,1.));
#120877=DIRECTION('ref_axis',(0.871318704123387,0.490717552003943,0.));
#120878=DIRECTION('center_axis',(0.,0.,-1.));
#120879=DIRECTION('ref_axis',(-0.871318704123387,-0.490717552003943,0.));
#120880=DIRECTION('center_axis',(-0.937230923829303,-0.256834770235895,
-0.235868811452356));
#120881=DIRECTION('ref_axis',(-0.0363363460881284,0.744653695079178,-0.666461209942402));
#120882=DIRECTION('center_axis',(-0.705483940759338,-0.668325005603341,
0.235868811452404));
#120883=DIRECTION('ref_axis',(0.617948726522513,-0.417095704888963,0.66646120993827));
#120884=DIRECTION('center_axis',(0.,0.,-1.));
#120885=DIRECTION('ref_axis',(-0.871318704123389,-0.490717552003939,0.));
#120886=DIRECTION('center_axis',(0.864241933273684,0.503076416433295,-6.76296429840134E-17));
#120887=DIRECTION('ref_axis',(0.503076416433295,-0.864241933273684,-1.54074395550979E-31));
#120888=DIRECTION('center_axis',(0.,0.,1.));
#120889=DIRECTION('ref_axis',(0.871318704123389,0.490717552003939,0.));
#120890=DIRECTION('center_axis',(0.878218752182993,0.478259159153431,-1.38914942345546E-16));
#120891=DIRECTION('ref_axis',(-0.478259159153431,0.878218752182993,-3.57452597678271E-31));
#120892=DIRECTION('center_axis',(0.,0.,-1.));
#120893=DIRECTION('ref_axis',(-0.871318704123391,-0.490717552003934,0.));
#120894=DIRECTION('center_axis',(0.,0.,1.));
#120895=DIRECTION('ref_axis',(0.871318704123391,0.490717552003934,0.));
#120896=DIRECTION('center_axis',(0.,0.,1.));
#120897=DIRECTION('ref_axis',(0.871318704123391,0.490717552003934,0.));
#120898=DIRECTION('center_axis',(0.634003890813394,-0.397011308118927,0.663642288932205));
#120899=DIRECTION('ref_axis',(0.34871994811035,-0.619187579593757,-0.703563173472531));
#120900=DIRECTION('center_axis',(0.635827336856486,-0.398153144485142,0.661209249211309));
#120901=DIRECTION('ref_axis',(0.347588297955079,-0.617178220151033,-0.705884848750768));
#120902=DIRECTION('center_axis',(-0.010869613919219,0.750122776784351,-0.661209249211308));
#120903=DIRECTION('ref_axis',(-0.347588297955064,0.617178220151042,0.705884848750767));
#120904=DIRECTION('center_axis',(-0.0108384416915672,0.747971550610416,
-0.663642288932184));
#120905=DIRECTION('ref_axis',(-0.34871994811035,0.619187579593734,0.703563173472552));
#120906=DIRECTION('center_axis',(0.,0.,1.));
#120907=DIRECTION('ref_axis',(0.871318704123391,0.490717552003934,0.));
#120908=DIRECTION('center_axis',(0.,0.,1.));
#120909=DIRECTION('ref_axis',(0.871318704123391,0.490717552003934,0.));
#120910=DIRECTION('center_axis',(0.,0.,1.));
#120911=DIRECTION('ref_axis',(-0.871318704123391,-0.490717552003934,0.));
#120912=DIRECTION('center_axis',(0.,0.,-1.));
#120913=DIRECTION('ref_axis',(0.871318704123389,0.490717552003939,0.));
#120914=DIRECTION('center_axis',(0.996912329797655,0.0785226508557306,0.));
#120915=DIRECTION('ref_axis',(-0.0785226508557306,0.996912329797655,0.));
#120916=DIRECTION('',(0.,0.,1.));
#120917=DIRECTION('center_axis',(-0.996912714474511,-0.0785177668673624,
2.28597554219387E-6));
#120918=DIRECTION('ref_axis',(0.0743278990302071,-0.94370603889449,0.322326349496635));
#120919=DIRECTION('',(0.,0.,-1.));
#120920=DIRECTION('center_axis',(-0.47533560879057,-0.879804557282865,0.));
#120921=DIRECTION('ref_axis',(0.879804557282865,-0.47533560879057,0.));
#120922=DIRECTION('center_axis',(0.475335608790533,0.879804557282885,3.13366257494963E-14));
#120923=DIRECTION('ref_axis',(0.878623270491977,-0.474697390141555,-0.051802860372563));
#120924=DIRECTION('',(0.,0.,1.));
#120925=DIRECTION('',(0.,0.,1.));
#120926=DIRECTION('center_axis',(0.,0.,1.));
#120927=DIRECTION('ref_axis',(0.838088104891841,0.545534901210548,0.));
#120928=DIRECTION('center_axis',(0.,0.,-1.));
#120929=DIRECTION('ref_axis',(-0.838088104891841,-0.545534901210548,0.));
#120930=DIRECTION('center_axis',(-0.918849822150867,-0.316355667117503,
-0.235868811452382));
#120931=DIRECTION('ref_axis',(-0.0839718152146669,0.740795646501562,-0.666461209954403));
#120932=DIRECTION('center_axis',(-0.661214718212259,-0.712152371479299,
0.235868811452244));
#120933=DIRECTION('ref_axis',(0.643402498151158,-0.376646626179641,0.666461209944242));
#120934=DIRECTION('center_axis',(0.,0.,-1.));
#120935=DIRECTION('ref_axis',(-0.83808810489184,-0.54553490121055,0.));
#120936=DIRECTION('center_axis',(0.830234038864126,0.557414962762358,-6.76296429840134E-17));
#120937=DIRECTION('ref_axis',(0.557414962762358,-0.830234038864126,-8.62816615085482E-32));
#120938=DIRECTION('center_axis',(0.,0.,1.));
#120939=DIRECTION('ref_axis',(0.83808810489184,0.54553490121055,0.));
#120940=DIRECTION('center_axis',(0.845772188033216,0.533544193061368,-1.38914942345546E-16));
#120941=DIRECTION('ref_axis',(-0.533544193061368,0.845772188033216,-2.46519032881566E-31));
#120942=DIRECTION('center_axis',(0.,0.,-1.));
#120943=DIRECTION('ref_axis',(-0.838088104891845,-0.545534901210541,0.));
#120944=DIRECTION('center_axis',(0.,0.,1.));
#120945=DIRECTION('ref_axis',(0.838088104891845,0.545534901210541,0.));
#120946=DIRECTION('center_axis',(0.,0.,1.));
#120947=DIRECTION('ref_axis',(0.838088104891845,0.545534901210541,0.));
#120948=DIRECTION('center_axis',(0.658137863669024,-0.355574837054025,0.663642288932205));
#120949=DIRECTION('ref_axis',(0.387674950010772,-0.595572828516713,-0.703563173472537));
#120950=DIRECTION('center_axis',(0.660030720953822,-0.35659749880586,0.661209249211309));
#120951=DIRECTION('ref_axis',(0.38641688485058,-0.593640102592878,-0.705884848750766));
#120952=DIRECTION('center_axis',(-0.0589078124527763,0.747885150534122,
-0.661209249211308));
#120953=DIRECTION('ref_axis',(-0.386416884850565,0.593640102592884,0.705884848750769));
#120954=DIRECTION('center_axis',(-0.0587388747376171,0.745740341496563,
-0.663642288932184));
#120955=DIRECTION('ref_axis',(-0.387674950010756,0.595572828516706,0.703563173472552));
#120956=DIRECTION('center_axis',(0.,0.,1.));
#120957=DIRECTION('ref_axis',(0.838088104891845,0.545534901210541,0.));
#120958=DIRECTION('center_axis',(0.,0.,1.));
#120959=DIRECTION('ref_axis',(0.838088104891845,0.545534901210541,0.));
#120960=DIRECTION('center_axis',(0.,0.,1.));
#120961=DIRECTION('ref_axis',(-0.838088104891825,-0.545534901210574,0.));
#120962=DIRECTION('center_axis',(0.,0.,-1.));
#120963=DIRECTION('ref_axis',(0.83808810489184,0.54553490121055,0.));
#120964=DIRECTION('center_axis',(0.989833102983779,0.14223370991964,0.));
#120965=DIRECTION('ref_axis',(-0.14223370991964,0.989833102983779,0.));
#120966=DIRECTION('',(0.,0.,1.));
#120967=DIRECTION('center_axis',(-0.989833799788485,-0.14222886061227,2.2859755500044E-6));
#120968=DIRECTION('ref_axis',(0.134638637897969,-0.937004888776007,0.322326349519926));
#120969=DIRECTION('',(0.,0.,-1.));
#120970=DIRECTION('center_axis',(-0.417989709277579,-0.908451761481062,
0.));
#120971=DIRECTION('ref_axis',(0.908451761481062,-0.417989709277579,0.));
#120972=DIRECTION('center_axis',(0.417989709277481,0.908451761481108,5.45355926330684E-14));
#120973=DIRECTION('ref_axis',(0.907232010961355,-0.417428487221712,-0.0518028603728525));
#120974=DIRECTION('',(0.,0.,1.));
#120975=DIRECTION('',(0.,0.,1.));
#120976=DIRECTION('center_axis',(0.,0.,1.));
#120977=DIRECTION('ref_axis',(0.801413621867962,0.59811053049121,0.));
#120978=DIRECTION('center_axis',(0.,0.,-1.));
#120979=DIRECTION('ref_axis',(-0.801413621867962,-0.59811053049121,0.));
#120980=DIRECTION('center_axis',(-0.896692969460631,-0.374576590704683,
-0.235868811452323));
#120981=DIRECTION('ref_axis',(-0.131262226152734,0.733893509731262,-0.666461209943803));
#120982=DIRECTION('center_axis',(-0.614228422558364,-0.753053350504152,
0.235868811452332));
#120983=DIRECTION('ref_axis',(0.666212390915799,-0.334649825708461,0.666461209931644));
#120984=DIRECTION('center_axis',(0.,0.,-1.));
#120985=DIRECTION('ref_axis',(-0.801413621867956,-0.598110530491217,0.));
#120986=DIRECTION('center_axis',(0.792814534704233,0.609462971444295,-6.76296429840134E-17));
#120987=DIRECTION('ref_axis',(0.609462971444295,-0.792814534704233,-4.93038065763132E-31));
#120988=DIRECTION('center_axis',(0.,0.,1.));
#120989=DIRECTION('ref_axis',(0.801413621867956,0.598110530491217,0.));
#120990=DIRECTION('center_axis',(0.809850164545245,0.586636779435145,-1.38914942345546E-16));
#120991=DIRECTION('ref_axis',(-0.586636779435145,0.809850164545245,-2.58844984525644E-31));
#120992=DIRECTION('center_axis',(0.,0.,-1.));
#120993=DIRECTION('ref_axis',(-0.801413621867959,-0.598110530491212,0.));
#120994=DIRECTION('center_axis',(0.,0.,1.));
#120995=DIRECTION('ref_axis',(0.801413621867959,0.598110530491212,0.));
#120996=DIRECTION('center_axis',(0.,0.,1.));
#120997=DIRECTION('ref_axis',(0.801413621867959,0.598110530491212,0.));
#120998=DIRECTION('center_axis',(0.679567406872709,-0.312677232713105,0.663642288932205));
#120999=DIRECTION('ref_axis',(0.42503691238556,-0.569510740937348,-0.703563173472534));
#121000=DIRECTION('center_axis',(0.681521897242613,-0.313576517514062,0.661209249211309));
#121001=DIRECTION('ref_axis',(0.423657601880077,-0.567662590517754,-0.705884848750768));
#121002=DIRECTION('center_axis',(-0.106703946149279,0.742574303779487,-0.661209249211308));
#121003=DIRECTION('ref_axis',(-0.423657601880061,0.567662590517767,0.705884848750768));
#121004=DIRECTION('center_axis',(-0.106397937147921,0.740444725358699,-0.663642288932184));
#121005=DIRECTION('ref_axis',(-0.425036912385554,0.569510740937331,0.703563173472552));
#121006=DIRECTION('center_axis',(0.,0.,1.));
#121007=DIRECTION('ref_axis',(0.801413621867959,0.598110530491212,0.));
#121008=DIRECTION('center_axis',(0.,0.,1.));
#121009=DIRECTION('ref_axis',(0.801413621867959,0.598110530491212,0.));
#121010=DIRECTION('center_axis',(0.,0.,1.));
#121011=DIRECTION('ref_axis',(-0.801413621867914,-0.598110530491273,0.));
#121012=DIRECTION('center_axis',(0.,0.,-1.));
#121013=DIRECTION('ref_axis',(0.801413621867956,0.598110530491217,0.));
#121014=DIRECTION('center_axis',(0.978686439631207,0.205360300160456,0.));
#121015=DIRECTION('ref_axis',(-0.205360300160456,0.978686439631207,0.));
#121016=DIRECTION('',(0.,0.,1.));
#121017=DIRECTION('center_axis',(-0.978687445700444,-0.205355505460931,
2.28597554707789E-6));
#121018=DIRECTION('ref_axis',(0.194396117720302,-0.926453384576079,0.322326349563298));
#121019=DIRECTION('',(0.,0.,-1.));
#121020=DIRECTION('center_axis',(-0.358926200390655,-0.933365942529042,
0.));
#121021=DIRECTION('ref_axis',(0.933365942529042,-0.358926200390655,0.));
#121022=DIRECTION('center_axis',(0.358926200390684,0.933365942529031,4.98882116956285E-15));
#121023=DIRECTION('ref_axis',(0.932112740497134,-0.358444281110008,-0.0518028603694038));
#121024=DIRECTION('',(0.,0.,1.));
#121025=DIRECTION('',(0.,0.,1.));
#121026=DIRECTION('center_axis',(0.,0.,1.));
#121027=DIRECTION('ref_axis',(0.761445958369139,0.648228395307783,0.));
#121028=DIRECTION('center_axis',(0.,0.,-1.));
#121029=DIRECTION('ref_axis',(-0.761445958369139,-0.648228395307783,0.));
#121030=DIRECTION('center_axis',(-0.870851413018747,-0.431258298734428,
-0.235868811452339));
#121031=DIRECTION('ref_axis',(-0.178013252440888,0.723975647099357,-0.666461209945848));
#121032=DIRECTION('center_axis',(-0.564718130564378,-0.790859871782574,
0.235868811452309));
#121033=DIRECTION('ref_axis',(0.68628467405606,-0.29127787730918,0.666461209933501));
#121034=DIRECTION('center_axis',(0.,0.,-1.));
#121035=DIRECTION('ref_axis',(-0.761445958369133,-0.64822839530779,0.));
#121036=DIRECTION('center_axis',(0.752137185563056,0.659006566047171,-6.76296429840134E-17));
#121037=DIRECTION('ref_axis',(0.659006566047171,-0.752137185563056,8.0118685686509E-32));
#121038=DIRECTION('center_axis',(0.,0.,1.));
#121039=DIRECTION('ref_axis',(0.761445958369133,0.64822839530779,0.));
#121040=DIRECTION('center_axis',(0.770600293018843,0.637318749449029,-1.38914942345546E-16));
#121041=DIRECTION('ref_axis',(-0.637318749449029,0.770600293018843,7.02579243712463E-31));
#121042=DIRECTION('center_axis',(0.,0.,-1.));
#121043=DIRECTION('ref_axis',(-0.76144595836914,-0.648228395307782,0.));
#121044=DIRECTION('center_axis',(0.,0.,1.));
#121045=DIRECTION('ref_axis',(0.76144595836914,0.648228395307782,0.));
#121046=DIRECTION('center_axis',(0.,0.,1.));
#121047=DIRECTION('ref_axis',(0.76144595836914,0.648228395307782,0.));
#121048=DIRECTION('center_axis',(0.698204461834803,-0.268494770553911,0.663642288932205));
#121049=DIRECTION('ref_axis',(0.46065230691723,-0.541108411563795,-0.703563173472532));
#121050=DIRECTION('center_axis',(0.700212553869646,-0.269266983049846,0.661209249211309));
#121051=DIRECTION('ref_axis',(0.459157418949173,-0.539352431094955,-0.705884848750768));
#121052=DIRECTION('center_axis',(-0.154061610443129,0.734212059928933,-0.661209249211308));
#121053=DIRECTION('ref_axis',(-0.459157418949153,0.539352431094971,0.705884848750769));
#121054=DIRECTION('center_axis',(-0.153619787612198,0.73210646301944,-0.663642288932184));
#121055=DIRECTION('ref_axis',(-0.46065230691723,0.541108411563772,0.70356317347255));
#121056=DIRECTION('center_axis',(0.,0.,1.));
#121057=DIRECTION('ref_axis',(0.76144595836914,0.648228395307782,0.));
#121058=DIRECTION('center_axis',(0.,0.,1.));
#121059=DIRECTION('ref_axis',(0.76144595836914,0.648228395307782,0.));
#121060=DIRECTION('center_axis',(0.,0.,1.));
#121061=DIRECTION('ref_axis',(-0.761445958369116,-0.648228395307811,0.));
#121062=DIRECTION('center_axis',(0.,0.,-1.));
#121063=DIRECTION('ref_axis',(0.761445958369133,0.64822839530779,0.));
#121064=DIRECTION('center_axis',(0.963518143770607,0.267643020878265,0.));
#121065=DIRECTION('ref_axis',(-0.267643020878265,0.963518143770607,0.));
#121066=DIRECTION('',(0.,0.,1.));
#121067=DIRECTION('center_axis',(-0.963519454970215,-0.267638300489063,
2.28597553609503E-6));
#121068=DIRECTION('ref_axis',(0.253354782203448,-0.912094884725178,0.322326349516771));
#121069=DIRECTION('',(0.,0.,-1.));
#121070=DIRECTION('center_axis',(-0.298387786756896,-0.954444722712804,
0.));
#121071=DIRECTION('ref_axis',(0.954444722712804,-0.298387786756896,0.));
#121072=DIRECTION('center_axis',(0.298387786756783,0.954444722712839,7.13989463202568E-14));
#121073=DIRECTION('ref_axis',(0.953163218841613,-0.297987150559883,-0.0518028604296759));
#121074=DIRECTION('',(0.,0.,1.));
#121075=DIRECTION('',(0.,0.,1.));
#121076=DIRECTION('center_axis',(0.,0.,1.));
#121077=DIRECTION('ref_axis',(0.718349350097714,0.6956825506035,0.));
#121078=DIRECTION('center_axis',(0.,0.,-1.));
#121079=DIRECTION('ref_axis',(-0.718349350097714,-0.6956825506035,0.));
#121080=DIRECTION('center_axis',(-0.84143134132374,-0.486167873910019,-0.235868811452348));
#121081=DIRECTION('ref_axis',(-0.224032784084857,0.711082813235251,-0.666461209956461));
#121082=DIRECTION('center_axis',(-0.512887290640372,-0.825416580208818,
0.235868811452382));
#121083=DIRECTION('ref_axis',(0.703536866258162,-0.246709005628528,0.666461209942055));
#121084=DIRECTION('center_axis',(0.,0.,-1.));
#121085=DIRECTION('ref_axis',(-0.718349350097726,-0.695682550603488,0.));
#121086=DIRECTION('center_axis',(0.70836914339348,0.705842161313694,-6.76296429840134E-17));
#121087=DIRECTION('ref_axis',(0.705842161313694,-0.70836914339348,4.93038065763132E-32));
#121088=DIRECTION('center_axis',(0.,0.,1.));
#121089=DIRECTION('ref_axis',(0.718349350097726,0.695682550603488,0.));
#121090=DIRECTION('center_axis',(0.728183859595181,0.685381840016984,-1.38914942345546E-16));
#121091=DIRECTION('ref_axis',(-0.685381840016983,0.728183859595181,-2.26797510251041E-30));
#121092=DIRECTION('center_axis',(0.,0.,-1.));
#121093=DIRECTION('ref_axis',(-0.718349350097727,-0.695682550603487,0.));
#121094=DIRECTION('center_axis',(0.,0.,1.));
#121095=DIRECTION('ref_axis',(0.718349350097727,0.695682550603487,0.));
#121096=DIRECTION('center_axis',(0.,0.,1.));
#121097=DIRECTION('ref_axis',(0.718349350097727,0.695682550603487,0.));
#121098=DIRECTION('center_axis',(0.71397244489883,-0.223209005790563,0.663642288932205));
#121099=DIRECTION('ref_axis',(0.49437478231017,-0.510482551659733,-0.703563173472532));
#121100=DIRECTION('center_axis',(0.716025886917706,-0.223850972794691,0.661209249211309));
#121101=DIRECTION('ref_axis',(0.492770459694845,-0.508825956842062,-0.705884848750766));
#121102=DIRECTION('center_axis',(-0.200786202533557,0.722832781236139,-0.661209249211308));
#121103=DIRECTION('ref_axis',(-0.492770459694827,0.508825956842073,0.70588484875077));
#121104=DIRECTION('center_axis',(-0.200210381417836,0.720759818187291,-0.663642288932184));
#121105=DIRECTION('ref_axis',(-0.494374782310162,0.510482551659712,0.703563173472552));
#121106=DIRECTION('center_axis',(0.,0.,1.));
#121107=DIRECTION('ref_axis',(0.718349350097718,0.695682550603496,0.));
#121108=DIRECTION('center_axis',(0.,0.,1.));
#121109=DIRECTION('ref_axis',(0.718349350097718,0.695682550603496,0.));
#121110=DIRECTION('center_axis',(0.,0.,1.));
#121111=DIRECTION('ref_axis',(-0.71834935009771,-0.695682550603505,0.));
#121112=DIRECTION('center_axis',(0.,0.,-1.));
#121113=DIRECTION('ref_axis',(0.718349350097726,0.695682550603488,0.));
#121114=DIRECTION('center_axis',(0.944390545183261,0.328825939014038,0.));
#121115=DIRECTION('ref_axis',(-0.328825939014038,0.944390545183261,0.));
#121116=DIRECTION('',(0.,0.,1.));
#121117=DIRECTION('center_axis',(-0.944392156125254,-0.328821312332196,
2.28597555969625E-6));
#121118=DIRECTION('ref_axis',(0.311272357538725,-0.893988391333502,0.322326349517413));
#121119=DIRECTION('',(0.,0.,-1.));
#121120=DIRECTION('center_axis',(-0.236623233703374,-0.971601484803187,
0.));
#121121=DIRECTION('ref_axis',(0.971601484803187,-0.236623233703375,0.));
#121122=DIRECTION('center_axis',(0.236623233703522,0.971601484803151,-7.0412563427439E-14));
#121123=DIRECTION('ref_axis',(0.970296945070278,-0.236305526891715,-0.051802860420206));
#121124=DIRECTION('',(0.,0.,1.));
#121125=DIRECTION('',(0.,0.,1.));
#121126=DIRECTION('center_axis',(0.,0.,1.));
#121127=DIRECTION('ref_axis',(0.672300890261307,0.740277997075324,0.));
#121128=DIRECTION('center_axis',(0.,0.,-1.));
#121129=DIRECTION('ref_axis',(-0.672300890261307,-0.740277997075324,0.));
#121130=DIRECTION('center_axis',(-0.808553647760786,-0.539079681009014,
-0.235868811452357));
#121131=DIRECTION('ref_axis',(-0.269131716968951,0.695267987570997,-0.66646120995923));
#121132=DIRECTION('center_axis',(-0.458948886824907,-0.856581474855869,
0.235868811452304));
#121133=DIRECTION('ref_axis',(0.717898074569612,-0.201126353727058,0.666461209948262));
#121134=DIRECTION('center_axis',(0.,0.,-1.));
#121135=DIRECTION('ref_axis',(-0.672300890261315,-0.740277997075317,0.));
#121136=DIRECTION('center_axis',(0.661690260468995,0.74977729973671,-6.76296429840134E-17));
#121137=DIRECTION('ref_axis',(0.74977729973671,-0.661690260468995,9.24446373305873E-32));
#121138=DIRECTION('center_axis',(0.,0.,1.));
#121139=DIRECTION('ref_axis',(0.672300890261315,0.740277997075317,0.));
#121140=DIRECTION('center_axis',(0.682775162497494,0.730628549590365,-1.38914942345546E-16));
#121141=DIRECTION('ref_axis',(-0.730628549590365,0.682775162497494,5.05364017407211E-31));
#121142=DIRECTION('center_axis',(0.,0.,-1.));
#121143=DIRECTION('ref_axis',(-0.672300890261315,-0.740277997075317,0.));
#121144=DIRECTION('center_axis',(0.,0.,1.));
#121145=DIRECTION('ref_axis',(0.672300890261315,0.740277997075317,0.));
#121146=DIRECTION('center_axis',(0.,0.,1.));
#121147=DIRECTION('ref_axis',(0.672300890261315,0.740277997075317,0.));
#121148=DIRECTION('center_axis',(0.726806562040158,-0.17700602734424,0.663642288932205));
#121149=DIRECTION('ref_axis',(0.52606576567954,-0.477759009452735,-0.703563173472532));
#121150=DIRECTION('center_axis',(0.72889691600935,-0.17751511087644,0.661209249211309));
#121151=DIRECTION('ref_axis',(0.524358600922709,-0.47620860758966,-0.705884848750769));
#121152=DIRECTION('center_axis',(-0.24668572104927,0.708483227598099,-0.661209249211308));
#121153=DIRECTION('ref_axis',(-0.524358600922702,0.476208607589674,0.705884848750765));
#121154=DIRECTION('center_axis',(-0.245978267821235,0.706451416659714,-0.663642288932184));
#121155=DIRECTION('ref_axis',(-0.526065765679537,0.477759009452712,0.70356317347255));
#121156=DIRECTION('center_axis',(0.,0.,1.));
#121157=DIRECTION('ref_axis',(0.672300890261315,0.740277997075317,0.));
#121158=DIRECTION('center_axis',(0.,0.,1.));
#121159=DIRECTION('ref_axis',(0.672300890261315,0.740277997075317,0.));
#121160=DIRECTION('center_axis',(0.,0.,1.));
#121161=DIRECTION('ref_axis',(-0.672300890261315,-0.740277997075317,0.));
#121162=DIRECTION('center_axis',(0.,0.,-1.));
#121163=DIRECTION('ref_axis',(0.672300890261315,0.740277997075317,0.));
#121164=DIRECTION('center_axis',(0.921382243274619,0.388657640833459,0.));
#121165=DIRECTION('ref_axis',(-0.388657640833459,0.921382243274619,0.));
#121166=DIRECTION('',(0.,0.,1.));
#121167=DIRECTION('center_axis',(-0.921384147339256,-0.388653126871104,
2.2859755282268E-6));
#121168=DIRECTION('ref_axis',(0.367910847994899,-0.872208307895385,0.3223263494751));
#121169=DIRECTION('',(0.,0.,-1.));
#121170=DIRECTION('center_axis',(-0.173886345027041,-0.98476572798465,0.));
#121171=DIRECTION('ref_axis',(0.98476572798465,-0.173886345027041,0.));
#121172=DIRECTION('center_axis',(0.173886345027122,0.984765727984635,-4.96795537759849E-14));
#121173=DIRECTION('ref_axis',(0.983443513024248,-0.173652873125871,-0.0518028604003333));
#121174=DIRECTION('',(0.,0.,1.));
#121175=DIRECTION('',(0.,0.,1.));
#121176=DIRECTION('center_axis',(0.,0.,1.));
#121177=DIRECTION('ref_axis',(0.623489801858719,0.781831482468041,0.));
#121178=DIRECTION('center_axis',(0.,0.,-1.));
#121179=DIRECTION('ref_axis',(-0.623489801858719,-0.781831482468041,0.));
#121180=DIRECTION('center_axis',(-0.772353433825047,-0.589776294066432,
-0.235868811452307));
#121181=DIRECTION('ref_axis',(-0.313124729920872,0.676596156628891,-0.666461209934227));
#121182=DIRECTION('center_axis',(-0.403124563589635,-0.884226492486333,
0.235868811452432));
#121183=DIRECTION('ref_axis',(0.729309285717962,-0.154717230509031,0.66646120993586));
#121184=DIRECTION('center_axis',(0.,0.,-1.));
#121185=DIRECTION('ref_axis',(-0.623489801858732,-0.781831482468031,0.));
#121186=DIRECTION('center_axis',(0.612292350332128,0.790631442408382,-6.76296429840134E-17));
#121187=DIRECTION('ref_axis',(0.790631442408382,-0.612292350332128,2.09541177949331E-31));
#121188=DIRECTION('center_axis',(0.,0.,1.));
#121189=DIRECTION('ref_axis',(0.623489801858732,0.781831482468031,0.));
#121190=DIRECTION('center_axis',(0.634560795802293,0.772872949734147,-1.38914942345546E-16));
#121191=DIRECTION('ref_axis',(-0.772872949734147,0.634560795802293,-9.73750179882187E-31));
#121192=DIRECTION('center_axis',(0.,0.,-1.));
#121193=DIRECTION('ref_axis',(-0.623489801858737,-0.781831482468027,0.));
#121194=DIRECTION('center_axis',(0.,0.,1.));
#121195=DIRECTION('ref_axis',(0.623489801858737,0.781831482468027,0.));
#121196=DIRECTION('center_axis',(0.,0.,1.));
#121197=DIRECTION('ref_axis',(0.623489801858737,0.781831482468027,0.));
#121198=DIRECTION('center_axis',(0.736654075118545,-0.130075693163885,0.663642288932205));
#121199=DIRECTION('ref_axis',(0.555595031976982,-0.443072252996905,-0.703563173472534));
#121200=DIRECTION('center_axis',(0.738772751325214,-0.130449801290727,0.661209249211309));
#121201=DIRECTION('ref_axis',(0.553792040184808,-0.441634415022259,-0.705884848750768));
#121202=DIRECTION('center_axis',(-0.291571555023269,0.691222364408683,-0.661209249211308));
#121203=DIRECTION('ref_axis',(-0.553792040184795,0.441634415022276,0.705884848750768));
#121204=DIRECTION('center_axis',(-0.290735376759984,0.689240054727728,-0.663642288932184));
#121205=DIRECTION('ref_axis',(-0.555595031976965,0.443072252996895,0.703563173472553));
#121206=DIRECTION('center_axis',(0.,0.,1.));
#121207=DIRECTION('ref_axis',(0.623489801858737,0.781831482468027,0.));
#121208=DIRECTION('center_axis',(0.,0.,1.));
#121209=DIRECTION('ref_axis',(0.623489801858737,0.781831482468027,0.));
#121210=DIRECTION('center_axis',(0.,0.,1.));
#121211=DIRECTION('ref_axis',(-0.623489801858745,-0.78183148246802,0.));
#121212=DIRECTION('center_axis',(0.,0.,-1.));
#121213=DIRECTION('ref_axis',(0.623489801858732,0.781831482468031,0.));
#121214=DIRECTION('center_axis',(0.894587784092491,0.446892265039893,0.));
#121215=DIRECTION('ref_axis',(-0.446892265039893,0.894587784092491,0.));
#121216=DIRECTION('',(0.,0.,1.));
#121217=DIRECTION('center_axis',(-0.894589973455614,-0.446887882345739,
2.2859755604554E-6));
#121218=DIRECTION('ref_axis',(0.423037513844087,-0.846844133396228,0.322326349548103));
#121219=DIRECTION('',(0.,0.,-1.));
#121220=DIRECTION('center_axis',(-0.110434920060487,-0.993883357558237,
0.));
#121221=DIRECTION('ref_axis',(0.993883357558237,-0.110434920060487,0.));
#121222=DIRECTION('center_axis',(0.110434920060531,0.993883357558232,-1.65883046113383E-14));
#121223=DIRECTION('ref_axis',(0.992548900634615,-0.110286642455757,-0.051802860392579));
#121224=DIRECTION('',(0.,0.,1.));
#121225=DIRECTION('',(0.,0.,1.));
#121226=DIRECTION('center_axis',(0.,0.,1.));
#121227=DIRECTION('ref_axis',(0.572116660122161,0.820172254596962,0.));
#121228=DIRECTION('center_axis',(0.,0.,-1.));
#121229=DIRECTION('ref_axis',(-0.572116660122161,-0.820172254596962,0.));
#121230=DIRECTION('center_axis',(-0.732979453960466,-0.638049389824897,
-0.235868811452243));
#121231=DIRECTION('ref_axis',(-0.355831046170119,0.655144046930282,-0.666461209938951));
#121232=DIRECTION('center_axis',(-0.345643715052351,-0.908238033793365,
0.235868811452408));
#121233=DIRECTION('ref_axis',(0.737723608565327,-0.107672340995304,0.66646120993644));
#121234=DIRECTION('center_axis',(0.,0.,-1.));
#121235=DIRECTION('ref_axis',(-0.572116660122168,-0.820172254596957,0.));
#121236=DIRECTION('center_axis',(0.560378399591449,0.828236710893285,-6.76296429840134E-17));
#121237=DIRECTION('ref_axis',(0.828236710893285,-0.560378399591449,7.33394122822659E-31));
#121238=DIRECTION('center_axis',(0.,0.,1.));
#121239=DIRECTION('ref_axis',(0.572116660122168,0.820172254596957,0.));
#121240=DIRECTION('center_axis',(0.583738882684276,0.811941449146743,-1.38914942345546E-16));
#121241=DIRECTION('ref_axis',(-0.811941449146743,0.583738882684276,9.73750179882187E-31));
#121242=DIRECTION('center_axis',(0.,0.,-1.));
#121243=DIRECTION('ref_axis',(-0.572116660122157,-0.820172254596965,0.));
#121244=DIRECTION('center_axis',(0.,0.,1.));
#121245=DIRECTION('ref_axis',(0.572116660122157,0.820172254596965,0.));
#121246=DIRECTION('center_axis',(0.,0.,1.));
#121247=DIRECTION('ref_axis',(0.572116660122157,0.820172254596965,0.));
#121248=DIRECTION('center_axis',(0.743474518590466,-0.0826108500591721,
0.663642288932205));
#121249=DIRECTION('ref_axis',(0.582841239113268,-0.406564817614812,-0.703563173472535));
#121250=DIRECTION('center_axis',(0.745612810939625,-0.0828484454901143,
0.661209249211309));
#121251=DIRECTION('ref_axis',(0.580949829165765,-0.405245451913252,-0.705884848750767));
#121252=DIRECTION('center_axis',(-0.335259258935775,0.67112112025718,-0.661209249211308));
#121253=DIRECTION('ref_axis',(-0.580949829165751,0.405245451913267,0.705884848750769));
#121254=DIRECTION('center_axis',(-0.334297791673084,0.669196457569339,-0.663642288932184));
#121255=DIRECTION('ref_axis',(-0.582841239113247,0.40656481761481,0.703563173472554));
#121256=DIRECTION('center_axis',(0.,0.,1.));
#121257=DIRECTION('ref_axis',(0.572116660122157,0.820172254596965,0.));
#121258=DIRECTION('center_axis',(0.,0.,1.));
#121259=DIRECTION('ref_axis',(0.572116660122157,0.820172254596965,0.));
#121260=DIRECTION('center_axis',(0.,0.,1.));
#121261=DIRECTION('ref_axis',(-0.572116660122118,-0.820172254596992,0.));
#121262=DIRECTION('center_axis',(0.,0.,-1.));
#121263=DIRECTION('ref_axis',(0.572116660122168,0.820172254596957,0.));
#121264=DIRECTION('center_axis',(0.864117271817049,0.503290513071188,0.));
#121265=DIRECTION('ref_axis',(-0.503290513071188,0.864117271817049,0.));
#121266=DIRECTION('',(0.,0.,1.));
#121267=DIRECTION('center_axis',(-0.864119737482087,-0.503286279654695,
2.28597557710273E-6));
#121268=DIRECTION('ref_axis',(0.476425827820026,-0.818000094733008,0.32232634953226));
#121269=DIRECTION('',(0.,0.,-1.));
#121270=DIRECTION('center_axis',(-0.0465296943191892,-0.998916907228305,
0.));
#121271=DIRECTION('ref_axis',(0.998916907228306,-0.0465296943191892,0.));
#121272=DIRECTION('center_axis',(0.0465296943190989,0.99891690722831,4.37256897280986E-14));
#121273=DIRECTION('ref_axis',(0.997575691911876,-0.0464672203152649,-0.0518028603719455));
#121274=DIRECTION('',(0.,0.,1.));
#121275=DIRECTION('',(0.,0.,1.));
#121276=DIRECTION('center_axis',(0.,0.,1.));
#121277=DIRECTION('ref_axis',(0.518392568310538,0.855142763005338,0.));
#121278=DIRECTION('center_axis',(0.,0.,-1.));
#121279=DIRECTION('ref_axis',(-0.518392568310538,-0.855142763005338,0.));
#121280=DIRECTION('center_axis',(-0.690593504295622,-0.683700603779703,
-0.23586881145239));
#121281=DIRECTION('ref_axis',(-0.397075176318766,0.630999809811531,-0.666461209950911));
#121282=DIRECTION('center_axis',(-0.28674254234948,-0.928517430203127,0.235868811452334));
#121283=DIRECTION('ref_axis',(0.743106466853929,-0.0601850027308018,0.666461209948609));
#121284=DIRECTION('center_axis',(0.,0.,-1.));
#121285=DIRECTION('ref_axis',(-0.518392568310523,-0.855142763005347,0.));
#121286=DIRECTION('center_axis',(0.506161733806058,0.86243857707691,-6.76296429840134E-17));
#121287=DIRECTION('ref_axis',(0.86243857707691,-0.506161733806058,-1.0538688655687E-30));
#121288=DIRECTION('center_axis',(0.,0.,1.));
#121289=DIRECTION('ref_axis',(0.518392568310523,0.855142763005347,0.));
#121290=DIRECTION('center_axis',(0.530518261285711,0.847673506983901,-1.38914942345546E-16));
#121291=DIRECTION('ref_axis',(-0.847673506983901,0.530518261285711,1.07235779303481E-30));
#121292=DIRECTION('center_axis',(0.,0.,-1.));
#121293=DIRECTION('ref_axis',(-0.518392568310514,-0.855142763005353,0.));
#121294=DIRECTION('center_axis',(0.,0.,1.));
#121295=DIRECTION('ref_axis',(0.518392568310514,0.855142763005353,0.));
#121296=DIRECTION('center_axis',(0.,0.,1.));
#121297=DIRECTION('ref_axis',(0.518392568310514,0.855142763005353,0.));
#121298=DIRECTION('center_axis',(0.747239865790714,-0.0348065412515937,
0.663642288932205));
#121299=DIRECTION('ref_axis',(0.60769242657898,-0.368386720189271,-0.703563173472533));
#121300=DIRECTION('center_axis',(0.749388987580438,-0.0349066476560473,
0.661209249211309));
#121301=DIRECTION('ref_axis',(0.605720370685339,-0.367191248317438,-0.70588484875077));
#121302=DIRECTION('center_axis',(-0.377569310640429,0.648262095467512,-0.661209249211308));
#121303=DIRECTION('ref_axis',(-0.605720370685332,0.367191248317457,0.705884848750766));
#121304=DIRECTION('center_axis',(-0.376486505253547,0.646402988624606,-0.663642288932184));
#121305=DIRECTION('ref_axis',(-0.607692426578967,0.368386720189258,0.703563173472552));
#121306=DIRECTION('center_axis',(0.,0.,1.));
#121307=DIRECTION('ref_axis',(0.518392568310514,0.855142763005353,0.));
#121308=DIRECTION('center_axis',(0.,0.,1.));
#121309=DIRECTION('ref_axis',(0.518392568310514,0.855142763005353,0.));
#121310=DIRECTION('center_axis',(0.,0.,1.));
#121311=DIRECTION('ref_axis',(-0.51839256831048,-0.855142763005373,0.));
#121312=DIRECTION('center_axis',(0.,0.,-1.));
#121313=DIRECTION('ref_axis',(0.518392568310523,0.855142763005347,0.));
#121314=DIRECTION('center_axis',(0.830095916319137,0.557620632428797,0.));
#121315=DIRECTION('ref_axis',(-0.557620632428797,0.830095916319137,0.));
#121316=DIRECTION('',(0.,0.,1.));
#121317=DIRECTION('center_axis',(-0.830098648154097,-0.557616565686059,
2.28597554586136E-6));
#121318=DIRECTION('ref_axis',(0.527856405890103,-0.785794718239048,0.322326349447883));
#121319=DIRECTION('',(0.,0.,-1.));
#121320=DIRECTION('center_axis',(0.0175667319166547,-0.999845693059568,
0.));
#121321=DIRECTION('ref_axis',(0.999845693059568,0.0175667319166547,0.));
#121322=DIRECTION('center_axis',(-0.0175667319166504,0.999845693059568,
-4.11269501834901E-15));
#121323=DIRECTION('ref_axis',(0.998503230691027,0.0175431456005816,-0.0518028603652222));
#121324=DIRECTION('',(0.,0.,1.));
#121325=DIRECTION('',(0.,0.,1.));
#121326=DIRECTION('center_axis',(0.,0.,1.));
#121327=DIRECTION('ref_axis',(0.46253829024085,0.886599306372992,0.));
#121328=DIRECTION('center_axis',(0.,0.,-1.));
#121329=DIRECTION('ref_axis',(-0.46253829024085,-0.886599306372992,0.));
#121330=DIRECTION('center_axis',(-0.64536975779005,-0.726542345300028,-0.235868811452357));
#121331=DIRECTION('ref_axis',(-0.436687639407675,0.604262659133404,-0.666461209948171));
#121332=DIRECTION('center_axis',(-0.226663083034028,-0.94498134932579,0.235868811452296));
#121333=DIRECTION('ref_axis',(0.745435741289,-0.012450351389804,0.666461209943377));
#121334=DIRECTION('center_axis',(0.,0.,-1.));
#121335=DIRECTION('ref_axis',(-0.462538290240833,-0.886599306373001,0.));
#121336=DIRECTION('center_axis',(0.449865140885107,0.893096498154832,-6.76296429840134E-17));
#121337=DIRECTION('ref_axis',(0.893096498154831,-0.449865140885107,6.47112461314111E-32));
#121338=DIRECTION('center_axis',(0.,0.,1.));
#121339=DIRECTION('ref_axis',(0.462538290240833,0.886599306373001,0.));
#121340=DIRECTION('center_axis',(0.475117626555714,0.879922292555465,-1.38914942345546E-16));
#121341=DIRECTION('ref_axis',(-0.879922292555465,0.475117626555714,-1.20794326111967E-30));
#121342=DIRECTION('center_axis',(0.,0.,-1.));
#121343=DIRECTION('ref_axis',(-0.462538290240822,-0.886599306373007,0.));
#121344=DIRECTION('center_axis',(0.,0.,1.));
#121345=DIRECTION('ref_axis',(0.462538290240822,0.886599306373007,0.));
#121346=DIRECTION('center_axis',(0.,0.,1.));
#121347=DIRECTION('ref_axis',(0.462538290240822,0.886599306373007,0.));
#121348=DIRECTION('center_axis',(0.74793464409998,0.0131407950999672,0.663642288932205));
#121349=DIRECTION('ref_axis',(0.630046475514265,-0.328694842711764,-0.703563173472533));
#121350=DIRECTION('center_axis',(0.750085764127849,0.0131785890806908,0.661209249211309));
#121351=DIRECTION('ref_axis',(0.628001877275149,-0.327628177120031,-0.705884848750767));
#121352=DIRECTION('center_axis',(-0.418327849059298,0.622739222675783,-0.661209249211308));
#121353=DIRECTION('ref_axis',(-0.628001877275143,0.327628177120045,0.705884848750767));
#121354=DIRECTION('center_axis',(-0.417128155027821,0.620953311146609,-0.663642288932184));
#121355=DIRECTION('ref_axis',(-0.630046475514251,0.32869484271175,0.703563173472552));
#121356=DIRECTION('center_axis',(0.,0.,1.));
#121357=DIRECTION('ref_axis',(0.462538290240822,0.886599306373007,0.));
#121358=DIRECTION('center_axis',(0.,0.,1.));
#121359=DIRECTION('ref_axis',(0.462538290240822,0.886599306373007,0.));
#121360=DIRECTION('center_axis',(0.,0.,1.));
#121361=DIRECTION('ref_axis',(-0.462538290240815,-0.886599306373011,0.));
#121362=DIRECTION('center_axis',(0.,0.,-1.));
#121363=DIRECTION('ref_axis',(0.462538290240833,0.886599306373001,0.));
#121364=DIRECTION('center_axis',(0.792663518646054,0.609659368998506,0.));
#121365=DIRECTION('ref_axis',(-0.609659368998506,0.792663518646054,0.));
#121366=DIRECTION('',(0.,0.,1.));
#121367=DIRECTION('center_axis',(-0.792666505425259,-0.609655485640606,
2.28597554274477E-6));
#121368=DIRECTION('ref_axis',(0.577117908749752,-0.750360342671505,0.322326349444494));
#121369=DIRECTION('',(0.,0.,-1.));
#121370=DIRECTION('center_axis',(0.081590972683001,-0.996665898471821,0.));
#121371=DIRECTION('ref_axis',(0.996665898471821,0.081590972683001,0.));
#121372=DIRECTION('center_axis',(-0.0815909726830444,0.996665898471817,
2.96721046178316E-14));
#121373=DIRECTION('ref_axis',(0.995327705513122,0.0814814229680361,-0.0518028604334566));
#121374=DIRECTION('',(0.,0.,1.));
#121375=DIRECTION('',(0.,0.,1.));
#121376=DIRECTION('center_axis',(0.,0.,1.));
#121377=DIRECTION('ref_axis',(0.40478334312238,0.914412623015818,0.));
#121378=DIRECTION('center_axis',(0.,0.,-1.));
#121379=DIRECTION('ref_axis',(-0.40478334312238,-0.914412623015818,0.));
#121380=DIRECTION('center_axis',(-0.597494048518314,-0.766398568480691,
-0.235868811452344));
#121381=DIRECTION('ref_axis',(-0.474505659308313,0.575042463570701,-0.666461209955181));
#121382=DIRECTION('center_axis',(-0.165652216491463,-0.957562137386155,
0.235868811452306));
#121383=DIRECTION('ref_axis',(0.744701860361022,0.0353354611192201,0.666461209945729));
#121384=DIRECTION('center_axis',(0.,0.,-1.));
#121385=DIRECTION('ref_axis',(-0.404783343122391,-0.914412623015814,0.));
#121386=DIRECTION('center_axis',(0.391719955604489,0.920084494153237,-6.76296429840134E-17));
#121387=DIRECTION('ref_axis',(0.920084494153237,-0.391719955604489,-7.48801562377757E-31));
#121388=DIRECTION('center_axis',(0.,0.,1.));
#121389=DIRECTION('ref_axis',(0.404783343122391,0.914412623015814,0.));
#121390=DIRECTION('center_axis',(0.417764631585787,0.908555288684179,-1.38914942345546E-16));
#121391=DIRECTION('ref_axis',(-0.908555288684179,0.417764631585787,5.7931972727168E-31));
#121392=DIRECTION('center_axis',(0.,0.,-1.));
#121393=DIRECTION('ref_axis',(-0.404783343122381,-0.914412623015818,0.));
#121394=DIRECTION('center_axis',(0.,0.,1.));
#121395=DIRECTION('ref_axis',(0.404783343122381,0.914412623015818,0.));
#121396=DIRECTION('center_axis',(0.,0.,1.));
#121397=DIRECTION('ref_axis',(0.404783343122381,0.914412623015818,0.));
#121398=DIRECTION('center_axis',(0.745555998525162,0.0610341331057705,0.663642288932205));
#121399=DIRECTION('ref_axis',(0.649811528337116,-0.287652287620733,-0.703563173472532));
#121400=DIRECTION('center_axis',(0.747700277377567,0.0612096721680979,0.661209249211309));
#121401=DIRECTION('ref_axis',(0.647702789445257,-0.286718811466814,-0.705884848750766));
#121402=DIRECTION('center_axis',(-0.457367388615341,0.594657380840936,-0.661209249211308));
#121403=DIRECTION('ref_axis',(-0.647702789445254,0.286718811466819,0.705884848750766));
#121404=DIRECTION('center_axis',(-0.456055735739378,0.592952003319043,-0.663642288932184));
#121405=DIRECTION('ref_axis',(-0.649811528337102,0.287652287620716,0.703563173472552));
#121406=DIRECTION('center_axis',(0.,0.,1.));
#121407=DIRECTION('ref_axis',(0.404783343122381,0.914412623015818,0.));
#121408=DIRECTION('center_axis',(0.,0.,1.));
#121409=DIRECTION('ref_axis',(0.404783343122381,0.914412623015818,0.));
#121410=DIRECTION('center_axis',(0.,0.,1.));
#121411=DIRECTION('ref_axis',(-0.40478334312241,-0.914412623015806,0.));
#121412=DIRECTION('center_axis',(0.,0.,-1.));
#121413=DIRECTION('ref_axis',(0.404783343122391,0.914412623015814,0.));
#121414=DIRECTION('center_axis',(0.751973896549063,0.659192884449475,0.));
#121415=DIRECTION('ref_axis',(-0.659192884449475,0.751973896549063,0.));
#121416=DIRECTION('',(0.,0.,1.));
#121417=DIRECTION('center_axis',(-0.751977125999198,-0.659189200433958,
2.28597553537158E-6));
#121418=DIRECTION('ref_axis',(0.624007910302061,-0.711842575470972,0.32232634957029));
#121419=DIRECTION('',(0.,0.,-1.));
#121420=DIRECTION('center_axis',(0.145279938641384,-0.989390589923088,0.));
#121421=DIRECTION('ref_axis',(0.989390589923088,0.145279938641384,0.));
#121422=DIRECTION('center_axis',(-0.145279938641383,0.989390589923088,1.57441884818865E-15));
#121423=DIRECTION('ref_axis',(0.988062165300268,0.145084875690857,-0.0518028604221298));
#121424=DIRECTION('',(0.,0.,1.));
#121425=DIRECTION('',(0.,0.,1.));
#121426=DIRECTION('center_axis',(0.,0.,1.));
#121427=DIRECTION('ref_axis',(0.345365054421307,0.938468422049761,0.));
#121428=DIRECTION('center_axis',(0.,0.,-1.));
#121429=DIRECTION('ref_axis',(-0.345365054421307,-0.938468422049761,0.));
#121430=DIRECTION('center_axis',(-0.547163108039054,-0.803105495551532,
-0.235868811452407));
#121431=DIRECTION('ref_axis',(-0.510373833685566,0.543459295184266,-0.666461209949176));
#121432=DIRECTION('center_axis',(-0.103960649459087,-0.96620809722756,0.235868811452349));
#121433=DIRECTION('ref_axis',(0.740907839755463,0.0829760726370221,0.666461209942956));
#121434=DIRECTION('center_axis',(0.,0.,-1.));
#121435=DIRECTION('ref_axis',(-0.345365054421305,-0.938468422049761,0.));
#121436=DIRECTION('center_axis',(0.331965109002625,0.943291665607661,-6.76296429840134E-17));
#121437=DIRECTION('ref_axis',(0.943291665607661,-0.331965109002625,6.16297582203915E-32));
#121438=DIRECTION('center_axis',(0.,0.,1.));
#121439=DIRECTION('ref_axis',(0.345365054421305,0.938468422049761,0.));
#121440=DIRECTION('center_axis',(0.358694952134443,0.933454836247191,-1.38914942345546E-16));
#121441=DIRECTION('ref_axis',(-0.933454836247191,0.358694952134442,1.17096540618744E-31));
#121442=DIRECTION('center_axis',(0.,0.,-1.));
#121443=DIRECTION('ref_axis',(-0.345365054421309,-0.93846842204976,0.));
#121444=DIRECTION('center_axis',(0.,0.,1.));
#121445=DIRECTION('ref_axis',(0.345365054421309,0.93846842204976,0.));
#121446=DIRECTION('center_axis',(0.,0.,1.));
#121447=DIRECTION('ref_axis',(0.345365054421309,0.93846842204976,0.));
#121448=DIRECTION('center_axis',(0.740113703431143,0.108676668766862,0.663642288932205));
#121449=DIRECTION('ref_axis',(0.666906366205896,-0.245427707578635,-0.703563173472534));
#121450=DIRECTION('center_axis',(0.742242329806335,0.108989231583133,0.661209249211309));
#121451=DIRECTION('ref_axis',(0.664742151921723,-0.24463125671627,-0.705884848750768));
#121452=DIRECTION('center_axis',(-0.494527507466565,0.564131964274605,-0.661209249211308));
#121453=DIRECTION('ref_axis',(-0.66474215192172,0.244631256716285,0.705884848750766));
#121454=DIRECTION('center_axis',(-0.493109285609133,0.562514128522034,-0.663642288932184));
#121455=DIRECTION('ref_axis',(-0.666906366205881,0.245427707578626,0.703563173472552));
#121456=DIRECTION('center_axis',(0.,0.,1.));
#121457=DIRECTION('ref_axis',(0.345365054421309,0.93846842204976,0.));
#121458=DIRECTION('center_axis',(0.,0.,1.));
#121459=DIRECTION('ref_axis',(0.345365054421309,0.93846842204976,0.));
#121460=DIRECTION('center_axis',(0.,0.,1.));
#121461=DIRECTION('ref_axis',(-0.345365054421273,-0.938468422049773,0.));
#121462=DIRECTION('center_axis',(0.,0.,-1.));
#121463=DIRECTION('ref_axis',(0.345365054421305,0.938468422049761,0.));
#121464=DIRECTION('center_axis',(0.708194252413257,0.706017634941811,0.));
#121465=DIRECTION('ref_axis',(-0.706017634941811,0.708194252413257,0.));
#121466=DIRECTION('',(0.,0.,1.));
#121467=DIRECTION('center_axis',(-0.708197711263846,-0.706014165407058,
2.28597556912132E-6));
#121468=DIRECTION('ref_axis',(0.668333729562862,-0.670399694507259,0.322326349424259));
#121469=DIRECTION('',(0.,0.,-1.));
#121470=DIRECTION('center_axis',(0.20837191816944,-0.978049663216745,0.));
#121471=DIRECTION('ref_axis',(0.978049663216745,0.20837191816944,0.));
#121472=DIRECTION('center_axis',(-0.208371918169327,0.978049663216769,-5.1823039677711E-14));
#121473=DIRECTION('ref_axis',(0.976736465708699,0.208092143538257,-0.0518028604667046));
#121474=DIRECTION('',(0.,0.,1.));
#121475=DIRECTION('',(0.,0.,1.));
#121476=DIRECTION('center_axis',(0.,0.,1.));
#121477=DIRECTION('ref_axis',(0.28452758663103,0.958667853036661,0.));
#121478=DIRECTION('center_axis',(0.,0.,-1.));
#121479=DIRECTION('ref_axis',(-0.28452758663103,-0.958667853036661,0.));
#121480=DIRECTION('center_axis',(-0.494583756982952,-0.836512289875464,
-0.23586881145233));
#121481=DIRECTION('ref_axis',(-0.544144772502367,0.509642935980642,-0.666461209946519));
#121482=DIRECTION('center_axis',(-0.0418418858185124,-0.970883700746492,
0.235868811452356));
#121483=DIRECTION('ref_axis',(0.734069269910053,0.130275717675065,0.66646120994246));
#121484=DIRECTION('center_axis',(0.,0.,-1.));
#121485=DIRECTION('ref_axis',(-0.28452758663103,-0.958667853036661,0.));
#121486=DIRECTION('center_axis',(0.270846146561577,0.962622649272676,-6.76296429840134E-17));
#121487=DIRECTION('ref_axis',(0.962622649272676,-0.270846146561577,-6.77927340424307E-32));
#121488=DIRECTION('center_axis',(0.,0.,1.));
#121489=DIRECTION('ref_axis',(0.28452758663103,0.958667853036661,0.));
#121490=DIRECTION('center_axis',(0.298151318184951,0.954518617662629,-1.38914942345546E-16));
#121491=DIRECTION('ref_axis',(-0.954518617662629,0.298151318184951,3.51289621856232E-31));
#121492=DIRECTION('center_axis',(0.,0.,-1.));
#121493=DIRECTION('ref_axis',(-0.284527586631029,-0.958667853036662,0.));
#121494=DIRECTION('center_axis',(0.,0.,1.));
#121495=DIRECTION('ref_axis',(0.284527586631029,0.958667853036662,0.));
#121496=DIRECTION('center_axis',(0.,0.,1.));
#121497=DIRECTION('ref_axis',(0.284527586631029,0.958667853036662,0.));
#121498=DIRECTION('center_axis',(0.731630122375834,0.155872628684918,0.663642288932205));
#121499=DIRECTION('ref_axis',(0.681260742764968,-0.202194612442027,-0.703563173472533));
#121500=DIRECTION('center_axis',(0.733734349291447,0.156320930867475,0.661209249211309));
#121501=DIRECTION('ref_axis',(0.679049946309197,-0.20153845965865,-0.705884848750768));
#121502=DIRECTION('center_axis',(-0.529655506713792,0.531288408461143,-0.661209249211308));
#121503=DIRECTION('ref_axis',(-0.679049946309192,0.20153845965867,0.705884848750768));
#121504=DIRECTION('center_axis',(-0.528136543652709,0.529764762512025,-0.663642288932184));
#121505=DIRECTION('ref_axis',(-0.681260742764954,0.202194612442015,0.703563173472551));
#121506=DIRECTION('center_axis',(0.,0.,1.));
#121507=DIRECTION('ref_axis',(0.284527586631029,0.958667853036662,0.));
#121508=DIRECTION('center_axis',(0.,0.,1.));
#121509=DIRECTION('ref_axis',(0.284527586631029,0.958667853036662,0.));
#121510=DIRECTION('center_axis',(0.,0.,1.));
#121511=DIRECTION('ref_axis',(-0.284527586631029,-0.958667853036662,0.));
#121512=DIRECTION('center_axis',(0.,0.,-1.));
#121513=DIRECTION('ref_axis',(0.28452758663103,0.958667853036661,0.));
#121514=DIRECTION('center_axis',(0.661504486187094,0.749941207531863,0.));
#121515=DIRECTION('ref_axis',(-0.749941207531863,0.661504486187094,0.));
#121516=DIRECTION('',(0.,0.,1.));
#121517=DIRECTION('center_axis',(-0.661508160224924,-0.74993796673499,2.28597553179878E-6));
#121518=DIRECTION('ref_axis',(0.709913222118179,-0.626201997342729,0.32232634950584));
#121519=DIRECTION('',(0.,0.,-1.));
#121520=DIRECTION('center_axis',(0.270607652790102,-0.962689720653249,0.));
#121521=DIRECTION('ref_axis',(0.962689720653249,0.270607652790102,0.));
#121522=DIRECTION('center_axis',(-0.27060765279011,0.962689720653247,2.92121087495402E-15));
#121523=DIRECTION('ref_axis',(0.96139714648011,0.27024431613496,-0.0518028603133916));
#121524=DIRECTION('',(0.,0.,1.));
#121525=DIRECTION('',(0.,0.,1.));
#121526=DIRECTION('center_axis',(0.,0.,1.));
#121527=DIRECTION('ref_axis',(0.222520933956302,0.974927912181827,0.));
#121528=DIRECTION('center_axis',(0.,0.,-1.));
#121529=DIRECTION('ref_axis',(-0.222520933956302,-0.974927912181827,0.));
#121530=DIRECTION('center_axis',(-0.439972055181329,-0.866481675769066,
-0.235868811452358));
#121531=DIRECTION('ref_axis',(-0.575679703722719,0.473732344632858,-0.66646120995177));
#121532=DIRECTION('center_axis',(0.0204488151059282,-0.971569734885157,
0.235868811452361));
#121533=DIRECTION('ref_axis',(0.724214251973394,0.17704003184605,0.666461209945911));
#121534=DIRECTION('center_axis',(0.,0.,-1.));
#121535=DIRECTION('ref_axis',(-0.222520933956311,-0.974927912181824,0.));
#121536=DIRECTION('center_axis',(0.208614219207991,0.977998009989918,-6.76296429840134E-17));
#121537=DIRECTION('ref_axis',(0.977998009989918,-0.208614219207991,-3.23556230657056E-32));
#121538=DIRECTION('center_axis',(0.,0.,1.));
#121539=DIRECTION('ref_axis',(0.222520933956311,0.974927912181824,0.));
#121540=DIRECTION('center_axis',(0.236382516515781,0.97166007733449,-1.38914942345546E-16));
#121541=DIRECTION('ref_axis',(-0.97166007733449,0.236382516515781,4.99201041585171E-31));
#121542=DIRECTION('center_axis',(0.,0.,-1.));
#121543=DIRECTION('ref_axis',(-0.222520933956319,-0.974927912181823,0.));
#121544=DIRECTION('center_axis',(0.,0.,1.));
#121545=DIRECTION('ref_axis',(0.222520933956319,0.974927912181823,0.));
#121546=DIRECTION('center_axis',(0.,0.,1.));
#121547=DIRECTION('ref_axis',(0.222520933956319,0.974927912181823,0.));
#121548=DIRECTION('center_axis',(0.720140116213513,0.202428074537133,0.663642288932205));
#121549=DIRECTION('ref_axis',(0.692815672802048,-0.158130656272285,-0.703563173472534));
#121550=DIRECTION('center_axis',(0.722211296949797,0.203010273916149,0.661209249211309));
#121551=DIRECTION('ref_axis',(0.690567378811531,-0.157617497840432,-0.705884848750767));
#121552=DIRECTION('center_axis',(-0.562607037873182,0.496261674616308,-0.661209249211308));
#121553=DIRECTION('ref_axis',(-0.690567378811525,0.15761749784045,0.705884848750769));
#121554=DIRECTION('center_axis',(-0.560993575353484,0.494838479458668,-0.663642288932184));
#121555=DIRECTION('ref_axis',(-0.69281567280203,0.158130656272279,0.703563173472553));
#121556=DIRECTION('center_axis',(0.,0.,1.));
#121557=DIRECTION('ref_axis',(0.222520933956319,0.974927912181823,0.));
#121558=DIRECTION('center_axis',(0.,0.,1.));
#121559=DIRECTION('ref_axis',(0.222520933956319,0.974927912181823,0.));
#121560=DIRECTION('center_axis',(0.,0.,1.));
#121561=DIRECTION('ref_axis',(-0.222520933956319,-0.974927912181823,0.));
#121562=DIRECTION('center_axis',(0.,0.,-1.));
#121563=DIRECTION('ref_axis',(0.222520933956311,0.974927912181824,0.));
#121564=DIRECTION('center_axis',(0.612096456134921,0.790783110838282,0.));
#121565=DIRECTION('ref_axis',(-0.790783110838282,0.612096456134921,0.));
#121566=DIRECTION('',(0.,0.,1.));
#121567=DIRECTION('center_axis',(-0.612100330262575,-0.790780112096416,
2.28597549873414E-6));
#121568=DIRECTION('ref_axis',(0.748575529000663,-0.579431101881055,0.322326349457012));
#121569=DIRECTION('',(0.,0.,-1.));
#121570=DIRECTION('center_axis',(0.33173140252029,-0.943373879531292,0.));
#121571=DIRECTION('ref_axis',(0.943373879531292,0.33173140252029,0.));
#121572=DIRECTION('center_axis',(-0.33173140252026,0.943373879531303,-1.39231739104898E-14));
#121573=DIRECTION('ref_axis',(0.942107240145474,0.331285996866079,-0.0518028604029466));
#121574=DIRECTION('',(0.,0.,1.));
#121575=DIRECTION('',(0.,0.,1.));
#121576=DIRECTION('center_axis',(0.,0.,1.));
#121577=DIRECTION('ref_axis',(0.159599895033352,0.987181783414455,0.));
#121578=DIRECTION('center_axis',(0.,0.,-1.));
#121579=DIRECTION('ref_axis',(-0.159599895033352,-0.987181783414455,0.));
#121580=DIRECTION('center_axis',(-0.38355241383127,-0.892890502597183,-0.235868811452375));
#121581=DIRECTION('ref_axis',(-0.604849043571402,0.43587508546863,-0.66646120994284));
#121582=DIRECTION('center_axis',(0.0826554874629293,-0.968263380582128,
0.235868811452328));
#121583=DIRECTION('ref_axis',(0.711383282337372,0.223076850549918,0.666461209943712));
#121584=DIRECTION('center_axis',(0.,0.,-1.));
#121585=DIRECTION('ref_axis',(-0.159599895033376,-0.987181783414451,0.));
#121586=DIRECTION('center_axis',(0.145525051280069,0.989354567104197,-6.76296429840134E-17));
#121587=DIRECTION('ref_axis',(0.989354567104197,-0.145525051280069,1.69481835106077E-31));
#121588=DIRECTION('center_axis',(0.,0.,1.));
#121589=DIRECTION('ref_axis',(0.159599895033376,0.987181783414451,0.));
#121590=DIRECTION('center_axis',(0.173642368382356,0.98480877732815,-1.38914942345546E-16));
#121591=DIRECTION('ref_axis',(-0.98480877732815,0.173642368382356,2.77333911991762E-31));
#121592=DIRECTION('center_axis',(0.,0.,-1.));
#121593=DIRECTION('ref_axis',(-0.159599895033363,-0.987181783414453,0.));
#121594=DIRECTION('center_axis',(0.,0.,1.));
#121595=DIRECTION('ref_axis',(0.159599895033363,0.987181783414453,0.));
#121596=DIRECTION('center_axis',(0.,0.,1.));
#121597=DIRECTION('ref_axis',(0.159599895033363,0.987181783414453,0.));
#121598=DIRECTION('center_axis',(0.705690899844101,0.24815170001039,0.663642288932205));
#121599=DIRECTION('ref_axis',(0.701523674631088,-0.113416907317004,-0.703563173472533));
#121600=DIRECTION('center_axis',(0.707720523475142,0.248865404203735,0.661209249211309));
#121601=DIRECTION('ref_axis',(0.699247121828089,-0.113048851914734,-0.705884848750767));
#121602=DIRECTION('center_axis',(-0.59324669603512,0.459195695102679,-0.661209249211308));
#121603=DIRECTION('ref_axis',(-0.699247121828083,0.113048851914757,0.70588484875077));
#121604=DIRECTION('center_axis',(-0.591545364120386,0.457878798950696,-0.663642288932184));
#121605=DIRECTION('ref_axis',(-0.701523674631068,0.113416907316999,0.703563173472553));
#121606=DIRECTION('center_axis',(0.,0.,1.));
#121607=DIRECTION('ref_axis',(0.159599895033363,0.987181783414453,0.));
#121608=DIRECTION('center_axis',(0.,0.,1.));
#121609=DIRECTION('ref_axis',(0.159599895033363,0.987181783414453,0.));
#121610=DIRECTION('center_axis',(0.,0.,1.));
#121611=DIRECTION('ref_axis',(-0.159599895033363,-0.987181783414453,0.));
#121612=DIRECTION('center_axis',(0.,0.,-1.));
#121613=DIRECTION('ref_axis',(0.159599895033376,0.987181783414451,0.));
#121614=DIRECTION('center_axis',(0.560173190450212,0.828375516719821,0.));
#121615=DIRECTION('ref_axis',(-0.828375516719821,0.560173190450212,0.));
#121616=DIRECTION('',(0.,0.,1.));
#121617=DIRECTION('center_axis',(-0.560177248748139,-0.828372772355381,
2.28597553096324E-6));
#121618=DIRECTION('ref_axis',(0.784161778430318,-0.530279199707863,0.322326349537529));
#121619=DIRECTION('',(0.,0.,-1.));
#121620=DIRECTION('center_axis',(0.39149199676136,-0.920181512785278,0.));
#121621=DIRECTION('ref_axis',(0.920181512785279,0.39149199676136,0.));
#121622=DIRECTION('center_axis',(-0.391491996761343,0.920181512785286,-5.74757724097888E-15));
#121623=DIRECTION('ref_axis',(0.918946013082694,0.390966352376137,-0.0518028604337561));
#121624=DIRECTION('',(0.,0.,1.));
#121625=DIRECTION('',(0.,0.,1.));
#121626=DIRECTION('center_axis',(0.,0.,1.));
#121627=DIRECTION('ref_axis',(0.096023025907694,0.995379112949197,0.));
#121628=DIRECTION('center_axis',(0.,0.,-1.));
#121629=DIRECTION('ref_axis',(-0.096023025907694,-0.995379112949197,0.));
#121630=DIRECTION('center_axis',(-0.325556673341238,-0.915630250825656,
-0.235868811452326));
#121631=DIRECTION('ref_axis',(-0.631532928957046,0.396226722081929,-0.666461209937341));
#121632=DIRECTION('center_axis',(0.144522510692408,-0.960978224356434,0.235868811452296));
#121633=DIRECTION('ref_axis',(-0.695629086210285,-0.268196998624628,-0.666461209934221));
#121634=DIRECTION('center_axis',(0.,0.,-1.));
#121635=DIRECTION('ref_axis',(-0.0960230259076783,-0.995379112949199,0.));
#121636=DIRECTION('center_axis',(0.0818378897014124,0.996645654086356,-6.76296429840134E-17));
#121637=DIRECTION('ref_axis',(0.996645654086356,-0.0818378897014124,-3.620748295448E-32));
#121638=DIRECTION('center_axis',(0.,0.,1.));
#121639=DIRECTION('ref_axis',(0.0960230259076783,0.995379112949198,0.));
#121640=DIRECTION('center_axis',(0.110188686511078,0.993910686814949,-1.38914942345546E-16));
#121641=DIRECTION('ref_axis',(-0.993910686814949,0.110188686511077,1.01689101063646E-31));
#121642=DIRECTION('center_axis',(0.,0.,-1.));
#121643=DIRECTION('ref_axis',(-0.096023025907693,-0.995379112949197,0.));
#121644=DIRECTION('center_axis',(0.,0.,1.));
#121645=DIRECTION('ref_axis',(0.096023025907693,0.995379112949197,0.));
#121646=DIRECTION('center_axis',(0.,0.,1.));
#121647=DIRECTION('ref_axis',(0.096023025907693,0.995379112949197,0.));
#121648=DIRECTION('center_axis',(0.688341848197006,0.292855616919931,0.663642288932205));
#121649=DIRECTION('ref_axis',(0.707348965204713,-0.0682371039617037,-0.703563173472533));
#121650=DIRECTION('center_axis',(0.690321574563952,0.293697893163985,0.661209249211309));
#121651=DIRECTION('ref_axis',(0.705053508433018,-0.0680156640076146,-0.705884848750768));
#121652=DIRECTION('center_axis',(-0.621448576272032,0.420242781980705,-0.661209249211308));
#121653=DIRECTION('ref_axis',(-0.705053508433014,0.0680156640076429,0.70588484875077));
#121654=DIRECTION('center_axis',(-0.619666366100035,0.41903759624314,-0.663642288932184));
#121655=DIRECTION('ref_axis',(-0.707348965204693,0.0682371039617002,0.703563173472553));
#121656=DIRECTION('center_axis',(0.,0.,1.));
#121657=DIRECTION('ref_axis',(0.096023025907693,0.995379112949197,0.));
#121658=DIRECTION('center_axis',(0.,0.,1.));
#121659=DIRECTION('ref_axis',(0.096023025907693,0.995379112949197,0.));
#121660=DIRECTION('center_axis',(0.,0.,1.));
#121661=DIRECTION('ref_axis',(-0.096023025907693,-0.995379112949197,0.));
#121662=DIRECTION('center_axis',(0.,0.,-1.));
#121663=DIRECTION('ref_axis',(0.0960230259076784,0.995379112949199,0.));
#121664=DIRECTION('center_axis',(0.505948052969169,0.862563949917168,0.));
#121665=DIRECTION('ref_axis',(-0.862563949917168,0.505948052969169,0.));
#121666=DIRECTION('',(0.,0.,1.));
#121667=DIRECTION('center_axis',(-0.505952278760923,-0.862561471207359,
2.2859755277705E-6));
#121668=DIRECTION('ref_axis',(0.816525738956301,-0.478948266589601,0.322326349454529));
#121669=DIRECTION('',(0.,0.,-1.));
#121670=DIRECTION('center_axis',(0.449643866412966,-0.893207922824914,0.));
#121671=DIRECTION('ref_axis',(0.893207922824915,0.449643866412966,0.));
#121672=DIRECTION('center_axis',(-0.449643866413041,0.893207922824877,3.75584255351168E-14));
#121673=DIRECTION('ref_axis',(0.892008639742985,0.449040143284211,-0.0518028603762828));
#121674=DIRECTION('',(0.,0.,1.));
#121675=DIRECTION('',(0.,0.,1.));
#121676=DIRECTION('center_axis',(0.,0.,1.));
#121677=DIRECTION('ref_axis',(0.0320515775716322,0.999486216200689,0.));
#121678=DIRECTION('center_axis',(0.,0.,-1.));
#121679=DIRECTION('ref_axis',(-0.0320515775716322,-0.999486216200689,0.));
#121680=DIRECTION('center_axis',(-0.266223150648619,-0.934607477951457,
-0.23586881145234));
#121681=DIRECTION('ref_axis',(-0.655621710048478,0.35495017810224,-0.666461209957712));
#121682=DIRECTION('center_axis',(0.205795659925439,-0.949744202477666,0.235868811452288));
#121683=DIRECTION('ref_axis',(-0.677016400948794,-0.31221506770535,-0.666461209932046));
#121684=DIRECTION('center_axis',(0.,0.,-1.));
#121685=DIRECTION('ref_axis',(-0.0320515775716516,-0.999486216200688,0.));
#121686=DIRECTION('center_axis',(0.0178144386798002,0.999841310296051,-6.76296429840134E-17));
#121687=DIRECTION('ref_axis',(0.999841310296051,-0.0178144386798002,-1.79111484828013E-32));
#121688=DIRECTION('center_axis',(0.,0.,1.));
#121689=DIRECTION('ref_axis',(0.0320515775716516,0.999486216200688,0.));
#121690=DIRECTION('center_axis',(0.0462822156915255,0.998928404096451,-1.38914942345546E-16));
#121691=DIRECTION('ref_axis',(-0.998928404096451,0.0462822156915255,1.84889274661175E-32));
#121692=DIRECTION('center_axis',(0.,0.,-1.));
#121693=DIRECTION('ref_axis',(-0.0320515775716415,-0.999486216200688,0.));
#121694=DIRECTION('center_axis',(0.,0.,1.));
#121695=DIRECTION('ref_axis',(0.0320515775716415,0.999486216200688,0.));
#121696=DIRECTION('center_axis',(0.,0.,1.));
#121697=DIRECTION('ref_axis',(0.0320515775716415,0.999486216200688,0.));
#121698=DIRECTION('center_axis',(0.668164252246806,0.336356127282215,0.663642288932205));
#121699=DIRECTION('ref_axis',(0.710267607154434,-0.0227768997094119,-0.703563173472533));
#121700=DIRECTION('center_axis',(0.670085946229365,0.337323514483224,0.661209249211309));
#121701=DIRECTION('ref_axis',(0.707962678938294,-0.0227029851477806,-0.705884848750767));
#121702=DIRECTION('center_axis',(-0.647096791008741,0.379563001125778,-0.661209249211308));
#121703=DIRECTION('ref_axis',(-0.707962678938293,0.0227029851477993,0.705884848750768));
#121704=DIRECTION('center_axis',(-0.645241026063361,0.378474478169339,-0.663642288932184));
#121705=DIRECTION('ref_axis',(-0.710267607154415,0.022776899709408,0.703563173472553));
#121706=DIRECTION('center_axis',(0.,0.,1.));
#121707=DIRECTION('ref_axis',(0.0320515775716415,0.999486216200688,0.));
#121708=DIRECTION('center_axis',(0.,0.,1.));
#121709=DIRECTION('ref_axis',(0.0320515775716415,0.999486216200688,0.));
#121710=DIRECTION('center_axis',(0.,0.,1.));
#121711=DIRECTION('ref_axis',(-0.0320515775716762,-0.999486216200687,0.));
#121712=DIRECTION('center_axis',(0.,0.,-1.));
#121713=DIRECTION('ref_axis',(0.0320515775716516,0.999486216200688,0.));
#121714=DIRECTION('center_axis',(0.44964386641296,0.893207922824918,0.));
#121715=DIRECTION('ref_axis',(-0.893207922824918,0.44964386641296,0.));
#121716=DIRECTION('',(0.,0.,1.));
#121717=DIRECTION('center_axis',(-0.449648242333896,-0.89320571995527,2.2859755482938E-6));
#121718=DIRECTION('ref_axis',(0.845534420057594,-0.425649232296221,0.322326349440293));
#121719=DIRECTION('',(0.,0.,-1.));
#121720=DIRECTION('center_axis',(0.505948052969176,-0.862563949917164,0.));
#121721=DIRECTION('ref_axis',(0.862563949917164,0.505948052969176,0.));
#121722=DIRECTION('center_axis',(-0.505948052969194,0.862563949917153,-2.04864139282425E-15));
#121723=DIRECTION('ref_axis',(0.861405811563617,0.505268731922799,-0.0518028603993475));
#121724=DIRECTION('',(0.,0.,1.));
#121725=DIRECTION('',(0.,0.,1.));
#121726=DIRECTION('center_axis',(0.,0.,1.));
#121727=DIRECTION('ref_axis',(-0.0320515775716322,0.999486216200689,0.));
#121728=DIRECTION('center_axis',(0.,0.,-1.));
#121729=DIRECTION('ref_axis',(0.0320515775716322,-0.999486216200689,0.));
#121730=DIRECTION('center_axis',(-0.205795659925178,-0.949744202477699,
-0.235868811452383));
#121731=DIRECTION('ref_axis',(-0.677016400935282,0.312215067705664,-0.666461209945624));
#121732=DIRECTION('center_axis',(0.26622315064885,-0.934607477951416,0.235868811452241));
#121733=DIRECTION('ref_axis',(-0.655621710080647,-0.354950178103372,-0.666461209925464));
#121734=DIRECTION('center_axis',(0.,0.,-1.));
#121735=DIRECTION('ref_axis',(0.0320515775716588,-0.999486216200688,0.));
#121736=DIRECTION('center_axis',(-0.0462822156915322,0.998928404096451,
-6.76296429840134E-17));
#121737=DIRECTION('ref_axis',(0.998928404096451,0.0462822156915322,-4.23704587765192E-33));
#121738=DIRECTION('center_axis',(0.,0.,1.));
#121739=DIRECTION('ref_axis',(-0.0320515775716588,0.999486216200688,0.));
#121740=DIRECTION('center_axis',(-0.0178144386798069,0.999841310296051,
-1.38914942345546E-16));
#121741=DIRECTION('ref_axis',(-0.999841310296051,-0.0178144386798069,-7.70371977754894E-33));
#121742=DIRECTION('center_axis',(0.,0.,-1.));
#121743=DIRECTION('ref_axis',(0.0320515775716415,-0.999486216200688,0.));
#121744=DIRECTION('center_axis',(0.,0.,1.));
#121745=DIRECTION('ref_axis',(-0.0320515775716415,0.999486216200688,0.));
#121746=DIRECTION('center_axis',(0.,0.,1.));
#121747=DIRECTION('ref_axis',(-0.0320515775716415,0.999486216200688,0.));
#121748=DIRECTION('center_axis',(0.645241026063342,0.378474478169334,0.663642288932205));
#121749=DIRECTION('ref_axis',(0.710267607154434,0.0227768997094152,-0.703563173472533));
#121750=DIRECTION('center_axis',(0.647096791008737,0.379563001125784,0.661209249211309));
#121751=DIRECTION('ref_axis',(0.707962678938293,0.0227029851478042,-0.705884848750767));
#121752=DIRECTION('center_axis',(-0.670085946229369,0.337323514483218,-0.661209249211308));
#121753=DIRECTION('ref_axis',(-0.707962678938293,-0.0227029851477856,0.705884848750768));
#121754=DIRECTION('center_axis',(-0.668164252246826,0.336356127282219,-0.663642288932184));
#121755=DIRECTION('ref_axis',(-0.710267607154415,-0.0227768997094186,0.703563173472553));
#121756=DIRECTION('center_axis',(0.,0.,1.));
#121757=DIRECTION('ref_axis',(-0.0320515775716415,0.999486216200688,0.));
#121758=DIRECTION('center_axis',(0.,0.,1.));
#121759=DIRECTION('ref_axis',(-0.0320515775716415,0.999486216200688,0.));
#121760=DIRECTION('center_axis',(0.,0.,1.));
#121761=DIRECTION('ref_axis',(0.0320515775716762,-0.999486216200687,0.));
#121762=DIRECTION('center_axis',(0.,0.,-1.));
#121763=DIRECTION('ref_axis',(-0.0320515775716588,0.999486216200688,0.));
#121764=DIRECTION('center_axis',(0.391491996761353,0.920181512785281,0.));
#121765=DIRECTION('ref_axis',(-0.920181512785281,0.391491996761353,0.));
#121766=DIRECTION('',(0.,0.,1.));
#121767=DIRECTION('center_axis',(-0.391496504829856,-0.920179594807873,
2.2859755625072E-6));
#121768=DIRECTION('ref_axis',(0.871068618844222,-0.370601113998325,0.322326349478321));
#121769=DIRECTION('',(0.,0.,-1.));
#121770=DIRECTION('center_axis',(0.560173190450217,-0.828375516719817,0.));
#121771=DIRECTION('ref_axis',(0.828375516719818,0.560173190450217,0.));
#121772=DIRECTION('center_axis',(-0.560173190450193,0.828375516719834,-6.33561319632668E-15));
#121773=DIRECTION('ref_axis',(0.827263282131017,0.559421062960219,-0.0518028604835341));
#121774=DIRECTION('',(0.,0.,1.));
#121775=DIRECTION('',(0.,0.,1.));
#121776=DIRECTION('center_axis',(0.,0.,1.));
#121777=DIRECTION('ref_axis',(-0.096023025907694,0.995379112949197,0.));
#121778=DIRECTION('center_axis',(0.,0.,-1.));
#121779=DIRECTION('ref_axis',(0.096023025907694,-0.995379112949197,0.));
#121780=DIRECTION('center_axis',(-0.144522510692369,-0.960978224356437,
-0.235868811452306));
#121781=DIRECTION('ref_axis',(-0.69562908620194,0.268196998625411,-0.666461209942616));
#121782=DIRECTION('center_axis',(0.325556673341202,-0.915630250825664,0.235868811452345));
#121783=DIRECTION('ref_axis',(-0.631532928959424,-0.396226722082146,-0.666461209934958));
#121784=DIRECTION('center_axis',(0.,0.,-1.));
#121785=DIRECTION('ref_axis',(0.0960230259076855,-0.995379112949198,0.));
#121786=DIRECTION('center_axis',(-0.110188686511084,0.993910686814948,-6.76296429840134E-17));
#121787=DIRECTION('ref_axis',(0.993910686814948,0.110188686511084,-1.14015052707724E-31));
#121788=DIRECTION('center_axis',(0.,0.,1.));
#121789=DIRECTION('ref_axis',(-0.0960230259076855,0.995379112949198,0.));
#121790=DIRECTION('center_axis',(-0.0818378897014191,0.996645654086355,
-1.38914942345546E-16));
#121791=DIRECTION('ref_axis',(-0.996645654086355,-0.0818378897014191,-4.46815747097839E-32));
#121792=DIRECTION('center_axis',(0.,0.,-1.));
#121793=DIRECTION('ref_axis',(0.096023025907693,-0.995379112949197,0.));
#121794=DIRECTION('center_axis',(0.,0.,1.));
#121795=DIRECTION('ref_axis',(-0.096023025907693,0.995379112949197,0.));
#121796=DIRECTION('center_axis',(0.,0.,1.));
#121797=DIRECTION('ref_axis',(-0.096023025907693,0.995379112949197,0.));
#121798=DIRECTION('center_axis',(0.619666366100017,0.419037596243134,0.663642288932205));
#121799=DIRECTION('ref_axis',(0.707348965204713,0.0682371039617049,-0.703563173472533));
#121800=DIRECTION('center_axis',(0.621448576272028,0.42024278198071,0.661209249211309));
#121801=DIRECTION('ref_axis',(0.705053508433015,0.0680156640076478,-0.705884848750769));
#121802=DIRECTION('center_axis',(-0.690321574563955,0.293697893163979,-0.661209249211308));
#121803=DIRECTION('ref_axis',(-0.705053508433017,-0.0680156640076214,0.705884848750769));
#121804=DIRECTION('center_axis',(-0.688341848197026,0.292855616919933,-0.663642288932184));
#121805=DIRECTION('ref_axis',(-0.707348965204693,-0.0682371039617086,0.703563173472553));
#121806=DIRECTION('center_axis',(0.,0.,1.));
#121807=DIRECTION('ref_axis',(-0.0960230259076933,0.995379112949197,0.));
#121808=DIRECTION('center_axis',(0.,0.,1.));
#121809=DIRECTION('ref_axis',(-0.0960230259076933,0.995379112949197,0.));
#121810=DIRECTION('center_axis',(0.,0.,1.));
#121811=DIRECTION('ref_axis',(0.0960230259076933,-0.995379112949197,0.));
#121812=DIRECTION('center_axis',(0.,0.,-1.));
#121813=DIRECTION('ref_axis',(-0.0960230259076855,0.995379112949198,0.));
#121814=DIRECTION('center_axis',(0.331731402520283,0.943373879531295,0.));
#121815=DIRECTION('ref_axis',(-0.943373879531295,0.331731402520284,0.));
#121816=DIRECTION('',(0.,0.,1.));
#121817=DIRECTION('center_axis',(-0.3317360242117,-0.943372254327521,2.28597555787171E-6));
#121818=DIRECTION('ref_axis',(0.893023409830886,-0.314030116230518,0.322326349519031));
#121819=DIRECTION('',(0.,0.,-1.));
#121820=DIRECTION('center_axis',(0.612096456134927,-0.790783110838278,0.));
#121821=DIRECTION('ref_axis',(0.790783110838278,0.612096456134927,0.));
#121822=DIRECTION('center_axis',(-0.612096456134829,0.790783110838353,-6.21041844454129E-14));
#121823=DIRECTION('ref_axis',(0.789721350430635,0.611274612858304,-0.0518028604320807));
#121824=DIRECTION('',(0.,0.,1.));
#121825=DIRECTION('',(0.,0.,1.));
#121826=DIRECTION('center_axis',(0.,0.,1.));
#121827=DIRECTION('ref_axis',(-0.159599895033413,0.987181783414445,0.));
#121828=DIRECTION('center_axis',(0.,0.,-1.));
#121829=DIRECTION('ref_axis',(0.159599895033413,-0.987181783414445,0.));
#121830=DIRECTION('center_axis',(-0.0826554874628396,-0.968263380582128,
-0.235868811452362));
#121831=DIRECTION('ref_axis',(0.71138328233753,-0.223076850549854,0.666461209943565));
#121832=DIRECTION('center_axis',(0.383552413831417,-0.89289050259713,0.235868811452339));
#121833=DIRECTION('ref_axis',(-0.604849043557018,-0.435875085466386,-0.666461209957362));
#121834=DIRECTION('center_axis',(0.,0.,-1.));
#121835=DIRECTION('ref_axis',(0.159599895033383,-0.98718178341445,0.));
#121836=DIRECTION('center_axis',(-0.173642368382363,0.984808777328149,-6.76296429840134E-17));
#121837=DIRECTION('ref_axis',(0.984808777328149,0.173642368382363,-2.77333911991762E-32));
#121838=DIRECTION('center_axis',(0.,0.,1.));
#121839=DIRECTION('ref_axis',(-0.159599895033383,0.98718178341445,0.));
#121840=DIRECTION('center_axis',(-0.145525051280076,0.989354567104196,-1.38914942345546E-16));
#121841=DIRECTION('ref_axis',(-0.989354567104196,-0.145525051280076,8.93631494195677E-32));
#121842=DIRECTION('center_axis',(0.,0.,-1.));
#121843=DIRECTION('ref_axis',(0.159599895033397,-0.987181783414447,0.));
#121844=DIRECTION('center_axis',(0.,0.,1.));
#121845=DIRECTION('ref_axis',(-0.159599895033397,0.987181783414447,0.));
#121846=DIRECTION('center_axis',(0.,0.,1.));
#121847=DIRECTION('ref_axis',(-0.159599895033397,0.987181783414447,0.));
#121848=DIRECTION('center_axis',(0.591545364120368,0.457878798950688,0.663642288932205));
#121849=DIRECTION('ref_axis',(0.701523674631087,0.113416907317007,-0.703563173472533));
#121850=DIRECTION('center_axis',(0.593246696035115,0.459195695102684,0.661209249211309));
#121851=DIRECTION('ref_axis',(0.699247121828084,0.113048851914762,-0.705884848750768));
#121852=DIRECTION('center_axis',(-0.707720523475145,0.248865404203728,-0.661209249211308));
#121853=DIRECTION('ref_axis',(-0.699247121828087,-0.113048851914738,0.705884848750768));
#121854=DIRECTION('center_axis',(-0.705690899844121,0.248151700010391,-0.663642288932184));
#121855=DIRECTION('ref_axis',(-0.701523674631068,-0.113416907317008,0.703563173472553));
#121856=DIRECTION('center_axis',(0.,0.,1.));
#121857=DIRECTION('ref_axis',(-0.159599895033397,0.987181783414447,0.));
#121858=DIRECTION('center_axis',(0.,0.,1.));
#121859=DIRECTION('ref_axis',(-0.159599895033397,0.987181783414447,0.));
#121860=DIRECTION('center_axis',(0.,0.,1.));
#121861=DIRECTION('ref_axis',(0.159599895033398,-0.987181783414447,0.));
#121862=DIRECTION('center_axis',(0.,0.,-1.));
#121863=DIRECTION('ref_axis',(-0.159599895033383,0.98718178341445,0.));
#121864=DIRECTION('center_axis',(0.270607652790095,0.962689720653251,0.));
#121865=DIRECTION('ref_axis',(-0.962689720653251,0.270607652790095,0.));
#121866=DIRECTION('',(0.,0.,1.));
#121867=DIRECTION('center_axis',(-0.270612369112877,-0.962688394901429,
2.28597555201867E-6));
#121868=DIRECTION('ref_axis',(0.911308576098357,-0.256168701364635,0.322326349482542));
#121869=DIRECTION('',(0.,0.,-1.));
#121870=DIRECTION('center_axis',(0.6615044861871,-0.749941207531858,0.));
#121871=DIRECTION('ref_axis',(0.749941207531858,0.6615044861871,0.));
#121872=DIRECTION('center_axis',(-0.661504486187023,0.749941207531925,-4.90156422134779E-14));
#121873=DIRECTION('ref_axis',(0.748934284302182,0.660616304250847,-0.0518028604879182));
#121874=DIRECTION('',(0.,0.,1.));
#121875=DIRECTION('',(0.,0.,1.));
#121876=DIRECTION('center_axis',(0.,0.,1.));
#121877=DIRECTION('ref_axis',(-0.222520933956302,0.974927912181827,0.));
#121878=DIRECTION('center_axis',(0.,0.,-1.));
#121879=DIRECTION('ref_axis',(0.222520933956302,-0.974927912181827,0.));
#121880=DIRECTION('center_axis',(-0.0204488151059326,-0.97156973488516,
-0.23586881145235));
#121881=DIRECTION('ref_axis',(0.724214251965761,-0.177040031847786,0.666461209953744));
#121882=DIRECTION('center_axis',(0.439972055181631,-0.866481675768945,0.235868811452243));
#121883=DIRECTION('ref_axis',(-0.575679703738258,-0.473732344636557,-0.666461209935718));
#121884=DIRECTION('center_axis',(0.,0.,-1.));
#121885=DIRECTION('ref_axis',(0.222520933956318,-0.974927912181823,0.));
#121886=DIRECTION('center_axis',(-0.236382516515787,0.971660077334488,-6.76296429840134E-17));
#121887=DIRECTION('ref_axis',(0.971660077334488,0.236382516515787,6.93889390390725E-14));
#121888=DIRECTION('center_axis',(0.,0.,1.));
#121889=DIRECTION('ref_axis',(-0.222520933956318,0.974927912181823,0.));
#121890=DIRECTION('center_axis',(-0.208614219207997,0.977998009989917,-1.38914942345546E-16));
#121891=DIRECTION('ref_axis',(-0.977998009989917,-0.208614219207997,-3.26637718568075E-31));
#121892=DIRECTION('center_axis',(0.,0.,-1.));
#121893=DIRECTION('ref_axis',(0.222520933956319,-0.974927912181823,0.));
#121894=DIRECTION('center_axis',(0.,0.,1.));
#121895=DIRECTION('ref_axis',(-0.222520933956319,0.974927912181823,0.));
#121896=DIRECTION('center_axis',(0.,0.,1.));
#121897=DIRECTION('ref_axis',(-0.222520933956319,0.974927912181823,0.));
#121898=DIRECTION('center_axis',(0.560993575353466,0.49483847945866,0.663642288932205));
#121899=DIRECTION('ref_axis',(0.69281567280205,0.158130656272286,-0.703563173472532));
#121900=DIRECTION('center_axis',(0.562607037873177,0.496261674616312,0.661209249211309));
#121901=DIRECTION('ref_axis',(0.690567378811527,0.157617497840452,-0.705884848750767));
#121902=DIRECTION('center_axis',(-0.722211296949799,0.203010273916143,-0.661209249211308));
#121903=DIRECTION('ref_axis',(-0.690567378811529,-0.157617497840433,0.705884848750769));
#121904=DIRECTION('center_axis',(-0.720140116213533,0.202428074537133,-0.663642288932184));
#121905=DIRECTION('ref_axis',(-0.692815672802027,-0.15813065627229,0.703563173472553));
#121906=DIRECTION('center_axis',(0.,0.,1.));
#121907=DIRECTION('ref_axis',(-0.222520933956319,0.974927912181823,0.));
#121908=DIRECTION('center_axis',(0.,0.,1.));
#121909=DIRECTION('ref_axis',(-0.222520933956319,0.974927912181823,0.));
#121910=DIRECTION('center_axis',(0.,0.,1.));
#121911=DIRECTION('ref_axis',(0.222520933956321,-0.974927912181822,0.));
#121912=DIRECTION('center_axis',(0.,0.,-1.));
#121913=DIRECTION('ref_axis',(-0.222520933956318,0.974927912181823,0.));
#121914=DIRECTION('center_axis',(0.208371918169433,0.978049663216746,0.));
#121915=DIRECTION('ref_axis',(-0.978049663216746,0.208371918169433,0.));
#121916=DIRECTION('',(0.,0.,1.));
#121917=DIRECTION('center_axis',(-0.208376709743311,-0.978048642364646,
2.28597557508953E-6));
#121918=DIRECTION('ref_axis',(0.925848979922217,-0.197254634349058,0.322326349535389));
#121919=DIRECTION('',(0.,0.,-1.));
#121920=DIRECTION('center_axis',(0.708194252413262,-0.706017634941805,0.));
#121921=DIRECTION('ref_axis',(0.706017634941806,0.708194252413262,0.));
#121922=DIRECTION('center_axis',(-0.708194252413266,0.706017634941802,-2.92121087495308E-15));
#121923=DIRECTION('ref_axis',(0.705069686558799,0.707243381552254,-0.0518028604075977));
#121924=DIRECTION('',(0.,0.,1.));
#121925=DIRECTION('',(0.,0.,1.));
#121926=DIRECTION('center_axis',(0.,0.,1.));
#121927=DIRECTION('ref_axis',(-0.28452758663103,0.958667853036661,0.));
#121928=DIRECTION('center_axis',(0.,0.,-1.));
#121929=DIRECTION('ref_axis',(0.28452758663103,-0.958667853036661,0.));
#121930=DIRECTION('center_axis',(0.0418418858184,-0.97088370074651,-0.235868811452302));
#121931=DIRECTION('ref_axis',(0.734069269914698,-0.130275717673731,0.666461209937605));
#121932=DIRECTION('center_axis',(0.494583756983124,-0.83651228987538,0.23586881145227));
#121933=DIRECTION('ref_axis',(-0.544144772508376,-0.509642935982521,-0.666461209940176));
#121934=DIRECTION('center_axis',(0.,0.,-1.));
#121935=DIRECTION('ref_axis',(0.284527586631037,-0.958667853036659,0.));
#121936=DIRECTION('center_axis',(-0.298151318184958,0.954518617662627,-6.76296429840134E-17));
#121937=DIRECTION('ref_axis',(0.954518617662627,0.298151318184958,6.93889390390724E-14));
#121938=DIRECTION('center_axis',(0.,0.,1.));
#121939=DIRECTION('ref_axis',(-0.284527586631037,0.958667853036659,0.));
#121940=DIRECTION('center_axis',(-0.270846146561583,0.962622649272674,-1.38914942345546E-16));
#121941=DIRECTION('ref_axis',(-0.962622649272674,-0.270846146561583,-3.57452597678271E-31));
#121942=DIRECTION('center_axis',(0.,0.,-1.));
#121943=DIRECTION('ref_axis',(0.284527586631029,-0.958667853036662,0.));
#121944=DIRECTION('center_axis',(0.,0.,1.));
#121945=DIRECTION('ref_axis',(-0.284527586631029,0.958667853036662,0.));
#121946=DIRECTION('center_axis',(0.,0.,1.));
#121947=DIRECTION('ref_axis',(-0.284527586631029,0.958667853036662,0.));
#121948=DIRECTION('center_axis',(0.528136543652692,0.529764762512015,0.663642288932205));
#121949=DIRECTION('ref_axis',(0.681260742764965,0.202194612442036,-0.703563173472534));
#121950=DIRECTION('center_axis',(0.529655506713787,0.531288408461147,0.661209249211309));
#121951=DIRECTION('ref_axis',(0.67904994630919,0.201538459658677,-0.705884848750768));
#121952=DIRECTION('center_axis',(-0.733734349291449,0.156320930867469,-0.661209249211308));
#121953=DIRECTION('ref_axis',(-0.679049946309195,-0.201538459658659,0.705884848750768));
#121954=DIRECTION('center_axis',(-0.731630122375853,0.155872628684916,-0.663642288932184));
#121955=DIRECTION('ref_axis',(-0.681260742764947,-0.202194612442032,0.703563173472552));
#121956=DIRECTION('center_axis',(0.,0.,1.));
#121957=DIRECTION('ref_axis',(-0.284527586631029,0.958667853036662,0.));
#121958=DIRECTION('center_axis',(0.,0.,1.));
#121959=DIRECTION('ref_axis',(-0.284527586631029,0.958667853036662,0.));
#121960=DIRECTION('center_axis',(0.,0.,1.));
#121961=DIRECTION('ref_axis',(0.284527586631029,-0.958667853036662,0.));
#121962=DIRECTION('center_axis',(0.,0.,-1.));
#121963=DIRECTION('ref_axis',(-0.284527586631037,0.958667853036659,0.));
#121964=DIRECTION('center_axis',(0.145279938641377,0.989390589923089,0.));
#121965=DIRECTION('ref_axis',(-0.989390589923089,0.145279938641377,0.));
#121966=DIRECTION('',(0.,0.,1.));
#121967=DIRECTION('center_axis',(-0.145284785776656,-0.989389878165633,
2.28597556942582E-6));
#121968=DIRECTION('ref_axis',(0.936584871683996,-0.137530005730791,0.322326349615356));
#121969=DIRECTION('',(0.,0.,-1.));
#121970=DIRECTION('center_axis',(0.751973896549068,-0.65919288444947,0.));
#121971=DIRECTION('ref_axis',(0.65919288444947,0.751973896549068,0.));
#121972=DIRECTION('center_axis',(-0.751973896549116,0.659192884449415,4.84465751599405E-14));
#121973=DIRECTION('ref_axis',(0.65830780623392,0.750964244093583,-0.0518028603885764));
#121974=DIRECTION('',(0.,0.,1.));
#121975=DIRECTION('',(0.,0.,1.));
#121976=DIRECTION('center_axis',(0.,0.,1.));
#121977=DIRECTION('ref_axis',(-0.345365054421307,0.938468422049761,0.));
#121978=DIRECTION('center_axis',(0.,0.,-1.));
#121979=DIRECTION('ref_axis',(0.345365054421307,-0.938468422049761,0.));
#121980=DIRECTION('center_axis',(0.103960649458841,-0.966208097227613,-0.235868811452239));
#121981=DIRECTION('ref_axis',(0.740907839753173,-0.0829760726379692,0.666461209945384));
#121982=DIRECTION('center_axis',(0.547163108039461,-0.803105495551311,0.235868811452214));
#121983=DIRECTION('ref_axis',(-0.510373833702409,-0.543459295190668,-0.666461209931056));
#121984=DIRECTION('center_axis',(0.,0.,-1.));
#121985=DIRECTION('ref_axis',(0.345365054421312,-0.938468422049759,0.));
#121986=DIRECTION('center_axis',(-0.358694952134449,0.933454836247189,-6.76296429840134E-17));
#121987=DIRECTION('ref_axis',(0.933454836247189,0.358694952134449,-3.75941525144388E-31));
#121988=DIRECTION('center_axis',(0.,0.,1.));
#121989=DIRECTION('ref_axis',(-0.345365054421312,0.938468422049759,0.));
#121990=DIRECTION('center_axis',(-0.331965109002631,0.943291665607659,-1.38914942345546E-16));
#121991=DIRECTION('ref_axis',(-0.943291665607659,-0.331965109002631,-1.04770588974666E-31));
#121992=DIRECTION('center_axis',(0.,0.,-1.));
#121993=DIRECTION('ref_axis',(0.345365054421309,-0.93846842204976,0.));
#121994=DIRECTION('center_axis',(0.,0.,1.));
#121995=DIRECTION('ref_axis',(-0.345365054421309,0.93846842204976,0.));
#121996=DIRECTION('center_axis',(0.,0.,1.));
#121997=DIRECTION('ref_axis',(-0.345365054421309,0.93846842204976,0.));
#121998=DIRECTION('center_axis',(0.493109285609116,0.562514128522023,0.663642288932205));
#121999=DIRECTION('ref_axis',(0.666906366205898,0.245427707578637,-0.703563173472532));
#122000=DIRECTION('center_axis',(0.49452750746656,0.564131964274609,0.661209249211309));
#122001=DIRECTION('ref_axis',(0.664742151921717,0.244631256716292,-0.705884848750766));
#122002=DIRECTION('center_axis',(-0.742242329806336,0.108989231583126,-0.661209249211308));
#122003=DIRECTION('ref_axis',(-0.66474215192172,-0.244631256716279,0.705884848750768));
#122004=DIRECTION('center_axis',(-0.740113703431162,0.108676668766859,-0.663642288932184));
#122005=DIRECTION('ref_axis',(-0.666906366205875,-0.245427707578641,0.703563173472552));
#122006=DIRECTION('center_axis',(0.,0.,1.));
#122007=DIRECTION('ref_axis',(-0.345365054421309,0.93846842204976,0.));
#122008=DIRECTION('center_axis',(0.,0.,1.));
#122009=DIRECTION('ref_axis',(-0.345365054421309,0.93846842204976,0.));
#122010=DIRECTION('center_axis',(0.,0.,1.));
#122011=DIRECTION('ref_axis',(0.345365054421309,-0.93846842204976,0.));
#122012=DIRECTION('center_axis',(0.,0.,-1.));
#122013=DIRECTION('ref_axis',(-0.345365054421312,0.938468422049759,0.));
#122014=DIRECTION('center_axis',(0.0815909726829938,0.996665898471821,0.));
#122015=DIRECTION('ref_axis',(-0.996665898471821,0.0815909726829938,0.));
#122016=DIRECTION('',(0.,0.,1.));
#122017=DIRECTION('center_axis',(-0.0815958554616844,-0.996665498733778,
2.28597552385516E-6));
#122018=DIRECTION('ref_axis',(0.943472135393123,-0.0772402368290282,0.32232634945244));
#122019=DIRECTION('',(0.,0.,-1.));
#122020=DIRECTION('center_axis',(0.792663518646059,-0.6096593689985,0.));
#122021=DIRECTION('ref_axis',(0.6096593689985,0.792663518646059,0.));
#122022=DIRECTION('center_axis',(-0.792663518646146,0.609659368998387,6.460807948113E-14));
#122023=DIRECTION('ref_axis',(0.608840797925512,0.791599233473346,-0.0518028604020782));
#122024=DIRECTION('',(0.,0.,1.));
#122025=DIRECTION('',(0.,0.,1.));
#122026=DIRECTION('center_axis',(0.,0.,1.));
#122027=DIRECTION('ref_axis',(-0.40478334312238,0.914412623015818,0.));
#122028=DIRECTION('center_axis',(0.,0.,-1.));
#122029=DIRECTION('ref_axis',(0.40478334312238,-0.914412623015818,0.));
#122030=DIRECTION('center_axis',(0.165652216491651,-0.957562137386107,-0.235868811452371));
#122031=DIRECTION('ref_axis',(0.744701860353997,-0.0353354611222299,0.666461209953419));
#122032=DIRECTION('center_axis',(0.597494048518655,-0.76639856848047,0.235868811452201));
#122033=DIRECTION('ref_axis',(-0.474505659311357,-0.575042463572249,-0.666461209951677));
#122034=DIRECTION('center_axis',(0.,0.,-1.));
#122035=DIRECTION('ref_axis',(0.404783343122398,-0.914412623015811,0.));
#122036=DIRECTION('center_axis',(-0.417764631585793,0.908555288684176,-6.76296429840134E-17));
#122037=DIRECTION('ref_axis',(0.908555288684176,0.417764631585793,-1.72563323017096E-31));
#122038=DIRECTION('center_axis',(0.,0.,1.));
#122039=DIRECTION('ref_axis',(-0.404783343122398,0.914412623015811,0.));
#122040=DIRECTION('center_axis',(-0.391719955604495,0.920084494153234,-1.38914942345546E-16));
#122041=DIRECTION('ref_axis',(-0.920084494153234,-0.391719955604495,-5.97808654737798E-31));
#122042=DIRECTION('center_axis',(0.,0.,-1.));
#122043=DIRECTION('ref_axis',(0.40478334312241,-0.914412623015806,0.));
#122044=DIRECTION('center_axis',(0.,0.,1.));
#122045=DIRECTION('ref_axis',(-0.40478334312241,0.914412623015806,0.));
#122046=DIRECTION('center_axis',(0.,0.,1.));
#122047=DIRECTION('ref_axis',(-0.40478334312241,0.914412623015806,0.));
#122048=DIRECTION('center_axis',(0.456055735739362,0.592952003319032,0.663642288932205));
#122049=DIRECTION('ref_axis',(0.64981152833712,0.287652287620727,-0.703563173472531));
#122050=DIRECTION('center_axis',(0.457367388615335,0.59465738084094,0.661209249211309));
#122051=DIRECTION('ref_axis',(0.647702789445247,0.286718811466831,-0.705884848750768));
#122052=DIRECTION('center_axis',(-0.747700277377569,0.0612096721680909,
-0.661209249211308));
#122053=DIRECTION('ref_axis',(-0.647702789445254,-0.286718811466814,0.705884848750768));
#122054=DIRECTION('center_axis',(-0.745555998525181,0.0610341331057666,
-0.663642288932184));
#122055=DIRECTION('ref_axis',(-0.649811528337097,-0.287652287620724,0.703563173472554));
#122056=DIRECTION('center_axis',(0.,0.,1.));
#122057=DIRECTION('ref_axis',(-0.40478334312241,0.914412623015806,0.));
#122058=DIRECTION('center_axis',(0.,0.,1.));
#122059=DIRECTION('ref_axis',(-0.40478334312241,0.914412623015806,0.));
#122060=DIRECTION('center_axis',(0.,0.,1.));
#122061=DIRECTION('ref_axis',(0.40478334312241,-0.914412623015806,0.));
#122062=DIRECTION('center_axis',(0.,0.,-1.));
#122063=DIRECTION('ref_axis',(-0.404783343122398,0.914412623015811,0.));
#122064=DIRECTION('center_axis',(0.0175667319166475,0.999845693059568,0.));
#122065=DIRECTION('ref_axis',(-0.999845693059568,0.0175667319166475,0.));
#122066=DIRECTION('',(0.,0.,1.));
#122067=DIRECTION('center_axis',(-0.0175716302745147,-0.999845606983533,
2.28597556281515E-6));
#122068=DIRECTION('ref_axis',(0.94648246962262,-0.0166330712173982,0.322326349588338));
#122069=DIRECTION('',(0.,0.,-1.));
#122070=DIRECTION('center_axis',(0.830095916319141,-0.557620632428791,0.));
#122071=DIRECTION('ref_axis',(0.557620632428791,0.830095916319141,0.));
#122072=DIRECTION('center_axis',(-0.830095916319178,0.557620632428737,3.49407170887273E-14));
#122073=DIRECTION('ref_axis',(0.55687193218257,0.828981371804959,-0.0518028604192842));
#122074=DIRECTION('',(0.,0.,1.));
#122075=DIRECTION('',(0.,0.,1.));
#122076=DIRECTION('center_axis',(0.,0.,1.));
#122077=DIRECTION('ref_axis',(-0.46253829024085,0.886599306372992,0.));
#122078=DIRECTION('center_axis',(0.,0.,-1.));
#122079=DIRECTION('ref_axis',(0.46253829024085,-0.886599306372992,0.));
#122080=DIRECTION('center_axis',(0.226663083033865,-0.944981349325845,-0.235868811452232));
#122081=DIRECTION('ref_axis',(0.745435741288701,0.0124503513895636,0.666461209943716));
#122082=DIRECTION('center_axis',(0.645369757790216,-0.726542345299901,0.235868811452294));
#122083=DIRECTION('ref_axis',(-0.43668763941582,-0.604262659137769,-0.666461209938876));
#122084=DIRECTION('center_axis',(0.,0.,-1.));
#122085=DIRECTION('ref_axis',(0.462538290240839,-0.886599306372998,0.));
#122086=DIRECTION('center_axis',(-0.47511762655572,0.879922292555462,-6.76296429840134E-17));
#122087=DIRECTION('ref_axis',(0.879922292555462,0.47511762655572,0.));
#122088=DIRECTION('center_axis',(0.,0.,1.));
#122089=DIRECTION('ref_axis',(-0.462538290240839,0.886599306372998,0.));
#122090=DIRECTION('center_axis',(-0.449865140885113,0.893096498154828,-1.38914942345546E-16));
#122091=DIRECTION('ref_axis',(-0.893096498154828,-0.449865140885113,-1.09700969632297E-30));
#122092=DIRECTION('center_axis',(0.,0.,-1.));
#122093=DIRECTION('ref_axis',(0.46253829024085,-0.886599306372993,0.));
#122094=DIRECTION('center_axis',(0.,0.,1.));
#122095=DIRECTION('ref_axis',(-0.46253829024085,0.886599306372993,0.));
#122096=DIRECTION('center_axis',(0.,0.,1.));
#122097=DIRECTION('ref_axis',(-0.46253829024085,0.886599306372993,0.));
#122098=DIRECTION('center_axis',(0.417128155027806,0.620953311146597,0.663642288932205));
#122099=DIRECTION('ref_axis',(0.630046475514269,0.32869484271176,-0.703563173472531));
#122100=DIRECTION('center_axis',(0.418327849059292,0.622739222675787,0.661209249211309));
#122101=DIRECTION('ref_axis',(0.628001877275144,0.327628177120047,-0.705884848750765));
#122102=DIRECTION('center_axis',(-0.75008576412785,0.0131785890806838,-0.661209249211308));
#122103=DIRECTION('ref_axis',(-0.628001877275147,-0.327628177120031,0.70588484875077));
#122104=DIRECTION('center_axis',(-0.747934644099999,0.013140795099962,-0.663642288932184));
#122105=DIRECTION('ref_axis',(-0.630046475514242,-0.328694842711771,0.70356317347255));
#122106=DIRECTION('center_axis',(0.,0.,1.));
#122107=DIRECTION('ref_axis',(-0.46253829024085,0.886599306372993,0.));
#122108=DIRECTION('center_axis',(0.,0.,1.));
#122109=DIRECTION('ref_axis',(-0.46253829024085,0.886599306372993,0.));
#122110=DIRECTION('center_axis',(0.,0.,1.));
#122111=DIRECTION('ref_axis',(0.46253829024085,-0.886599306372993,0.));
#122112=DIRECTION('center_axis',(0.,0.,-1.));
#122113=DIRECTION('ref_axis',(-0.462538290240839,0.886599306372998,0.));
#122114=DIRECTION('center_axis',(-0.0465296943191963,0.998916907228305,
0.));
#122115=DIRECTION('ref_axis',(-0.998916907228305,-0.0465296943191963,0.));
#122116=DIRECTION('',(0.,0.,1.));
#122117=DIRECTION('center_axis',(0.0465248005106162,-0.998917135167989,
2.28597555794753E-6));
#122118=DIRECTION('ref_axis',(0.945603504443602,0.0440424432494455,0.322326349491626));
#122119=DIRECTION('',(0.,0.,-1.));
#122120=DIRECTION('center_axis',(0.864117271817053,-0.503290513071182,0.));
#122121=DIRECTION('ref_axis',(0.503290513071182,0.864117271817053,0.));
#122122=DIRECTION('center_axis',(-0.864117271817065,0.503290513071162,2.12451699996577E-15));
#122123=DIRECTION('ref_axis',(0.502614760223245,0.862957047866487,-0.0518028603774638));
#122124=DIRECTION('',(0.,0.,1.));
#122125=DIRECTION('',(0.,0.,1.));
#122126=DIRECTION('center_axis',(0.,0.,1.));
#122127=DIRECTION('ref_axis',(-0.518392568310538,0.855142763005338,0.));
#122128=DIRECTION('center_axis',(0.,0.,-1.));
#122129=DIRECTION('ref_axis',(0.518392568310538,-0.855142763005338,0.));
#122130=DIRECTION('center_axis',(0.286742542349545,-0.928517430203101,-0.235868811452362));
#122131=DIRECTION('ref_axis',(0.743106466856502,0.0601850027323955,0.666461209945596));
#122132=DIRECTION('center_axis',(0.690593504295839,-0.683700603779519,0.235868811452288));
#122133=DIRECTION('ref_axis',(-0.397075176330132,-0.630999809818572,-0.666461209937473));
#122134=DIRECTION('center_axis',(0.,0.,-1.));
#122135=DIRECTION('ref_axis',(0.518392568310529,-0.855142763005344,0.));
#122136=DIRECTION('center_axis',(-0.530518261285717,0.847673506983898,-6.76296429840134E-17));
#122137=DIRECTION('ref_axis',(0.847673506983898,0.530518261285717,7.39557098644698E-32));
#122138=DIRECTION('center_axis',(0.,0.,1.));
#122139=DIRECTION('ref_axis',(-0.518392568310529,0.855142763005344,0.));
#122140=DIRECTION('center_axis',(-0.506161733806064,0.862438577076907,-1.38914942345546E-16));
#122141=DIRECTION('ref_axis',(-0.862438577076907,-0.506161733806063,-1.23259516440783E-30));
#122142=DIRECTION('center_axis',(0.,0.,-1.));
#122143=DIRECTION('ref_axis',(0.518392568310539,-0.855142763005338,0.));
#122144=DIRECTION('center_axis',(0.,0.,1.));
#122145=DIRECTION('ref_axis',(-0.518392568310539,0.855142763005338,0.));
#122146=DIRECTION('center_axis',(0.,0.,1.));
#122147=DIRECTION('ref_axis',(-0.518392568310539,0.855142763005338,0.));
#122148=DIRECTION('center_axis',(0.376486505253533,0.646402988624593,0.663642288932205));
#122149=DIRECTION('ref_axis',(0.607692426578987,0.368386720189267,-0.70356317347253));
#122150=DIRECTION('center_axis',(0.377569310640423,0.648262095467515,0.661209249211309));
#122151=DIRECTION('ref_axis',(0.605720370685325,0.367191248317467,-0.705884848750767));
#122152=DIRECTION('center_axis',(-0.749388987580438,-0.0349066476560543,
-0.661209249211308));
#122153=DIRECTION('ref_axis',(-0.605720370685332,-0.367191248317453,0.705884848750768));
#122154=DIRECTION('center_axis',(-0.747239865790733,-0.0348065412516,-0.663642288932184));
#122155=DIRECTION('ref_axis',(-0.607692426578961,-0.368386720189264,0.703563173472554));
#122156=DIRECTION('center_axis',(0.,0.,1.));
#122157=DIRECTION('ref_axis',(-0.518392568310539,0.855142763005338,0.));
#122158=DIRECTION('center_axis',(0.,0.,1.));
#122159=DIRECTION('ref_axis',(-0.518392568310539,0.855142763005338,0.));
#122160=DIRECTION('center_axis',(0.,0.,1.));
#122161=DIRECTION('ref_axis',(0.51839256831058,-0.855142763005313,0.));
#122162=DIRECTION('center_axis',(0.,0.,-1.));
#122163=DIRECTION('ref_axis',(-0.518392568310529,0.855142763005344,0.));
#122164=DIRECTION('center_axis',(-0.110434920060495,0.993883357558236,0.));
#122165=DIRECTION('ref_axis',(-0.993883357558236,-0.110434920060495,0.));
#122166=DIRECTION('',(0.,0.,1.));
#122167=DIRECTION('center_axis',(0.110430050911002,-0.993883898576976,2.28597551807898E-6));
#122168=DIRECTION('ref_axis',(0.940838851618515,0.10453697787255,0.322326349438621));
#122169=DIRECTION('',(0.,0.,-1.));
#122170=DIRECTION('center_axis',(0.894587784092495,-0.446892265039887,0.));
#122171=DIRECTION('ref_axis',(0.446892265039887,0.894587784092495,0.));
#122172=DIRECTION('center_axis',(-0.894587784092469,0.446892265039938,-2.3976691856752E-14));
#122173=DIRECTION('ref_axis',(0.446292236401057,0.893386648309996,-0.0518028604381615));
#122174=DIRECTION('',(0.,0.,1.));
#122175=DIRECTION('',(0.,0.,1.));
#122176=DIRECTION('center_axis',(0.,0.,1.));
#122177=DIRECTION('ref_axis',(-0.572116660122175,0.820172254596952,0.));
#122178=DIRECTION('center_axis',(0.,0.,-1.));
#122179=DIRECTION('ref_axis',(0.572116660122175,-0.820172254596952,0.));
#122180=DIRECTION('center_axis',(0.345643715052242,-0.908238033793422,-0.235868811452346));
#122181=DIRECTION('ref_axis',(0.737723608554744,0.107672340987873,0.666461209949355));
#122182=DIRECTION('center_axis',(0.73297945396056,-0.638049389824798,0.23586881145222));
#122183=DIRECTION('ref_axis',(-0.35583104616699,-0.655144046928193,-0.666461209942675));
#122184=DIRECTION('center_axis',(0.,0.,-1.));
#122185=DIRECTION('ref_axis',(0.572116660122174,-0.820172254596953,0.));
#122186=DIRECTION('center_axis',(-0.583738882684281,0.811941449146739,-6.76296429840134E-17));
#122187=DIRECTION('ref_axis',(0.811941449146739,0.583738882684281,1.84889274661175E-32));
#122188=DIRECTION('center_axis',(0.,0.,1.));
#122189=DIRECTION('ref_axis',(-0.572116660122174,0.820172254596953,0.));
#122190=DIRECTION('center_axis',(-0.560378399591454,0.828236710893281,-1.38914942345546E-16));
#122191=DIRECTION('ref_axis',(-0.828236710893281,-0.560378399591454,4.19082355898663E-31));
#122192=DIRECTION('center_axis',(0.,0.,-1.));
#122193=DIRECTION('ref_axis',(0.572116660122189,-0.820172254596943,0.));
#122194=DIRECTION('center_axis',(0.,0.,1.));
#122195=DIRECTION('ref_axis',(-0.572116660122189,0.820172254596943,0.));
#122196=DIRECTION('center_axis',(0.,0.,1.));
#122197=DIRECTION('ref_axis',(-0.572116660122189,0.820172254596943,0.));
#122198=DIRECTION('center_axis',(0.33429779167307,0.669196457569324,0.663642288932205));
#122199=DIRECTION('ref_axis',(0.582841239113268,0.406564817614819,-0.703563173472531));
#122200=DIRECTION('center_axis',(0.335259258935769,0.671121120257183,0.661209249211309));
#122201=DIRECTION('ref_axis',(0.580949829165752,0.405245451913269,-0.705884848750767));
#122202=DIRECTION('center_axis',(-0.745612810939625,-0.0828484454901213,
-0.661209249211308));
#122203=DIRECTION('ref_axis',(-0.580949829165763,-0.405245451913251,0.705884848750769));
#122204=DIRECTION('center_axis',(-0.743474518590484,-0.0826108500591795,
-0.663642288932184));
#122205=DIRECTION('ref_axis',(-0.582841239113243,-0.406564817614819,0.703563173472551));
#122206=DIRECTION('center_axis',(0.,0.,1.));
#122207=DIRECTION('ref_axis',(-0.572116660122189,0.820172254596943,0.));
#122208=DIRECTION('center_axis',(0.,0.,1.));
#122209=DIRECTION('ref_axis',(-0.572116660122189,0.820172254596943,0.));
#122210=DIRECTION('center_axis',(0.,0.,1.));
#122211=DIRECTION('ref_axis',(0.572116660122126,-0.820172254596987,0.));
#122212=DIRECTION('center_axis',(0.,0.,-1.));
#122213=DIRECTION('ref_axis',(-0.572116660122174,0.820172254596953,0.));
#122214=DIRECTION('center_axis',(-0.173886345027048,0.984765727984648,0.));
#122215=DIRECTION('ref_axis',(-0.984765727984648,-0.173886345027048,0.));
#122216=DIRECTION('',(0.,0.,1.));
#122217=DIRECTION('center_axis',(0.173881520544841,-0.984766579859303,2.28597557664648E-6));
#122218=DIRECTION('ref_axis',(0.932208090086838,0.164601947622779,0.322326349551875));
#122219=DIRECTION('',(0.,0.,-1.));
#122220=DIRECTION('center_axis',(0.921382243274622,-0.388657640833452,0.));
#122221=DIRECTION('ref_axis',(0.388657640833452,0.921382243274622,0.));
#122222=DIRECTION('center_axis',(-0.921382243274618,0.388657640833462,1.36576092854888E-15));
#122223=DIRECTION('ref_axis',(0.388135802051874,0.92014513138824,-0.0518028604235987));
#122224=DIRECTION('',(0.,0.,1.));
#122225=DIRECTION('',(0.,0.,1.));
#122226=DIRECTION('center_axis',(0.,0.,1.));
#122227=DIRECTION('ref_axis',(-0.623489801858719,0.781831482468041,0.));
#122228=DIRECTION('center_axis',(0.,0.,-1.));
#122229=DIRECTION('ref_axis',(0.623489801858719,-0.781831482468041,0.));
#122230=DIRECTION('center_axis',(0.403124563589518,-0.884226492486404,-0.235868811452366));
#122231=DIRECTION('ref_axis',(0.729309285709624,0.154717230502321,0.666461209946543));
#122232=DIRECTION('center_axis',(0.772353433824904,-0.589776294066584,0.235868811452398));
#122233=DIRECTION('ref_axis',(-0.313124729900363,-0.676596156612425,-0.66646120996058));
#122234=DIRECTION('center_axis',(0.,0.,-1.));
#122235=DIRECTION('ref_axis',(0.623489801858738,-0.781831482468027,0.));
#122236=DIRECTION('center_axis',(-0.634560795802298,0.772872949734142,-6.76296429840134E-17));
#122237=DIRECTION('ref_axis',(0.772872949734142,0.634560795802298,6.93889390390733E-14));
#122238=DIRECTION('center_axis',(0.,0.,1.));
#122239=DIRECTION('ref_axis',(-0.623489801858738,0.781831482468027,0.));
#122240=DIRECTION('center_axis',(-0.612292350332133,0.790631442408378,-1.38914942345546E-16));
#122241=DIRECTION('ref_axis',(-0.790631442408378,-0.612292350332133,1.38050658413677E-30));
#122242=DIRECTION('center_axis',(0.,0.,-1.));
#122243=DIRECTION('ref_axis',(0.623489801858737,-0.781831482468027,0.));
#122244=DIRECTION('center_axis',(0.,0.,1.));
#122245=DIRECTION('ref_axis',(-0.623489801858737,0.781831482468027,0.));
#122246=DIRECTION('center_axis',(0.,0.,1.));
#122247=DIRECTION('ref_axis',(-0.623489801858737,0.781831482468027,0.));
#122248=DIRECTION('center_axis',(0.290735376759972,0.689240054727713,0.663642288932205));
#122249=DIRECTION('ref_axis',(0.555595031976987,0.443072252996905,-0.70356317347253));
#122250=DIRECTION('center_axis',(0.291571555023262,0.691222364408686,0.661209249211309));
#122251=DIRECTION('ref_axis',(0.553792040184796,0.441634415022278,-0.705884848750765));
#122252=DIRECTION('center_axis',(-0.738772751325214,-0.130449801290734,
-0.661209249211308));
#122253=DIRECTION('ref_axis',(-0.553792040184805,-0.441634415022259,0.705884848750771));
#122254=DIRECTION('center_axis',(-0.736654075118562,-0.130075693163894,
-0.663642288932184));
#122255=DIRECTION('ref_axis',(-0.555595031976956,-0.443072252996913,0.70356317347255));
#122256=DIRECTION('center_axis',(0.,0.,1.));
#122257=DIRECTION('ref_axis',(-0.623489801858737,0.781831482468027,0.));
#122258=DIRECTION('center_axis',(0.,0.,1.));
#122259=DIRECTION('ref_axis',(-0.623489801858737,0.781831482468027,0.));
#122260=DIRECTION('center_axis',(0.,0.,1.));
#122261=DIRECTION('ref_axis',(0.623489801858728,-0.781831482468034,0.));
#122262=DIRECTION('center_axis',(0.,0.,-1.));
#122263=DIRECTION('ref_axis',(-0.623489801858737,0.781831482468027,0.));
#122264=DIRECTION('center_axis',(-0.236623233703382,0.971601484803186,0.));
#122265=DIRECTION('ref_axis',(-0.971601484803186,-0.236623233703382,0.));
#122266=DIRECTION('',(0.,0.,1.));
#122267=DIRECTION('center_axis',(0.236618473713326,-0.971602644033223,2.28597559089828E-6));
#122268=DIRECTION('ref_axis',(0.919746685589421,0.223990532666546,0.322326349563655));
#122269=DIRECTION('',(0.,0.,-1.));
#122270=DIRECTION('center_axis',(0.944390545183263,-0.328825939014031,0.));
#122271=DIRECTION('ref_axis',(0.328825939014031,0.944390545183263,0.));
#122272=DIRECTION('center_axis',(-0.944390545183216,0.328825939014167,-4.96985226777598E-14));
#122273=DIRECTION('ref_axis',(0.328384434435842,0.943122540746955,-0.0518028604930213));
#122274=DIRECTION('',(0.,0.,1.));
#122275=DIRECTION('',(0.,0.,1.));
#122276=DIRECTION('center_axis',(0.,0.,1.));
#122277=DIRECTION('ref_axis',(-0.672300890261307,0.740277997075324,0.));
#122278=DIRECTION('center_axis',(0.,0.,-1.));
#122279=DIRECTION('ref_axis',(0.672300890261307,-0.740277997075324,0.));
#122280=DIRECTION('center_axis',(0.458948886824949,-0.856581474855845,-0.235868811452311));
#122281=DIRECTION('ref_axis',(0.717898074564745,0.201126353722678,0.666461209954827));
#122282=DIRECTION('center_axis',(0.808553647760812,-0.539079681008988,0.235868811452327));
#122283=DIRECTION('ref_axis',(-0.269131716982949,-0.69526798758372,-0.666461209940304));
#122284=DIRECTION('center_axis',(0.,0.,-1.));
#122285=DIRECTION('ref_axis',(0.672300890261321,-0.740277997075312,0.));
#122286=DIRECTION('center_axis',(-0.682775162497499,0.73062854959036,-6.76296429840134E-17));
#122287=DIRECTION('ref_axis',(0.73062854959036,0.6827751624975,-2.28030105415449E-31));
#122288=DIRECTION('center_axis',(0.,0.,1.));
#122289=DIRECTION('ref_axis',(-0.672300890261321,0.740277997075312,0.));
#122290=DIRECTION('center_axis',(-0.661690260469,0.749777299736706,-1.38914942345546E-16));
#122291=DIRECTION('ref_axis',(-0.749777299736706,-0.661690260469,1.09700969632297E-30));
#122292=DIRECTION('center_axis',(0.,0.,-1.));
#122293=DIRECTION('ref_axis',(0.672300890261315,-0.740277997075317,0.));
#122294=DIRECTION('center_axis',(0.,0.,1.));
#122295=DIRECTION('ref_axis',(-0.672300890261315,0.740277997075317,0.));
#122296=DIRECTION('center_axis',(0.,0.,1.));
#122297=DIRECTION('ref_axis',(-0.672300890261315,0.740277997075317,0.));
#122298=DIRECTION('center_axis',(0.245978267821224,0.706451416659698,0.663642288932205));
#122299=DIRECTION('ref_axis',(0.526065765679537,0.477759009452737,-0.703563173472534));
#122300=DIRECTION('center_axis',(0.246685721049263,0.708483227598101,0.661209249211309));
#122301=DIRECTION('ref_axis',(0.524358600922691,0.476208607589683,-0.705884848750767));
#122302=DIRECTION('center_axis',(-0.728896916009349,-0.177515110876448,
-0.661209249211308));
#122303=DIRECTION('ref_axis',(-0.5243586009227,-0.476208607589672,0.705884848750767));
#122304=DIRECTION('center_axis',(-0.726806562040175,-0.17700602734425,-0.663642288932184));
#122305=DIRECTION('ref_axis',(-0.526065765679519,-0.47775900945273,0.703563173472551));
#122306=DIRECTION('center_axis',(0.,0.,1.));
#122307=DIRECTION('ref_axis',(-0.672300890261315,0.740277997075317,0.));
#122308=DIRECTION('center_axis',(0.,0.,1.));
#122309=DIRECTION('ref_axis',(-0.672300890261315,0.740277997075317,0.));
#122310=DIRECTION('center_axis',(0.,0.,1.));
#122311=DIRECTION('ref_axis',(0.672300890261315,-0.740277997075317,0.));
#122312=DIRECTION('center_axis',(0.,0.,-1.));
#122313=DIRECTION('ref_axis',(-0.672300890261321,0.740277997075312,0.));
#122314=DIRECTION('center_axis',(-0.298387786756903,0.954444722712802,0.));
#122315=DIRECTION('ref_axis',(-0.954444722712802,-0.298387786756903,0.));
#122316=DIRECTION('',(0.,0.,1.));
#122317=DIRECTION('center_axis',(0.298383110819051,-0.954446184534634,2.28597552936751E-6));
#122318=DIRECTION('ref_axis',(0.903505844692068,0.282458692570506,0.322326349525809));
#122319=DIRECTION('',(0.,0.,-1.));
#122320=DIRECTION('center_axis',(0.963518143770609,-0.267643020878258,0.));
#122321=DIRECTION('ref_axis',(0.267643020878258,0.963518143770609,0.));
#122322=DIRECTION('center_axis',(-0.963518143770608,0.267643020878261,9.48445089270243E-17));
#122323=DIRECTION('ref_axis',(0.267283664742203,0.962224457292137,-0.0518028604502678));
#122324=DIRECTION('',(0.,0.,1.));
#122325=DIRECTION('',(0.,0.,1.));
#122326=DIRECTION('center_axis',(0.,0.,1.));
#122327=DIRECTION('ref_axis',(-0.71834935009773,0.695682550603484,0.));
#122328=DIRECTION('center_axis',(0.,0.,-1.));
#122329=DIRECTION('ref_axis',(0.71834935009773,-0.695682550603484,0.));
#122330=DIRECTION('center_axis',(0.512887290640217,-0.825416580208937,-0.235868811452301));
#122331=DIRECTION('ref_axis',(0.703536866252696,0.246709005622772,0.666461209949955));
#122332=DIRECTION('center_axis',(0.84143134132397,-0.48616787390969,0.235868811452204));
#122333=DIRECTION('ref_axis',(-0.224032784092084,-0.711082813242973,-0.666461209945791));
#122334=DIRECTION('center_axis',(0.,0.,-1.));
#122335=DIRECTION('ref_axis',(0.718349350097732,-0.695682550603482,0.));
#122336=DIRECTION('center_axis',(-0.728183859595186,0.685381840016978,-6.76296429840134E-17));
#122337=DIRECTION('ref_axis',(0.685381840016978,0.728183859595186,8.81305542551599E-31));
#122338=DIRECTION('center_axis',(0.,0.,1.));
#122339=DIRECTION('ref_axis',(-0.718349350097731,0.695682550603482,0.));
#122340=DIRECTION('center_axis',(-0.708369143393485,0.705842161313689,-1.38914942345546E-16));
#122341=DIRECTION('ref_axis',(-0.705842161313689,-0.708369143393485,-6.5327543713615E-31));
#122342=DIRECTION('center_axis',(0.,0.,-1.));
#122343=DIRECTION('ref_axis',(0.718349350097735,-0.695682550603479,0.));
#122344=DIRECTION('center_axis',(0.,0.,1.));
#122345=DIRECTION('ref_axis',(-0.718349350097735,0.695682550603479,0.));
#122346=DIRECTION('center_axis',(0.,0.,1.));
#122347=DIRECTION('ref_axis',(-0.718349350097735,0.695682550603479,0.));
#122348=DIRECTION('center_axis',(0.200210381417825,0.720759818187274,0.663642288932205));
#122349=DIRECTION('ref_axis',(0.494374782310168,0.510482551659733,-0.703563173472533));
#122350=DIRECTION('center_axis',(0.20078620253355,0.72283278123614,0.661209249211309));
#122351=DIRECTION('ref_axis',(0.492770459694828,0.508825956842076,-0.705884848750768));
#122352=DIRECTION('center_axis',(-0.716025886917704,-0.223850972794698,
-0.661209249211308));
#122353=DIRECTION('ref_axis',(-0.492770459694842,-0.508825956842062,0.705884848750768));
#122354=DIRECTION('center_axis',(-0.713972444898846,-0.223209005790574,
-0.663642288932184));
#122355=DIRECTION('ref_axis',(-0.494374782310152,-0.510482551659722,0.703563173472552));
#122356=DIRECTION('center_axis',(0.,0.,1.));
#122357=DIRECTION('ref_axis',(-0.718349350097727,0.695682550603487,0.));
#122358=DIRECTION('center_axis',(0.,0.,1.));
#122359=DIRECTION('ref_axis',(-0.718349350097727,0.695682550603487,0.));
#122360=DIRECTION('center_axis',(0.,0.,1.));
#122361=DIRECTION('ref_axis',(0.718349350097761,-0.695682550603452,0.));
#122362=DIRECTION('center_axis',(0.,0.,-1.));
#122363=DIRECTION('ref_axis',(-0.718349350097731,0.695682550603482,0.));
#122364=DIRECTION('center_axis',(-0.358926200390661,0.93336594252904,0.));
#122365=DIRECTION('ref_axis',(-0.93336594252904,-0.358926200390661,0.));
#122366=DIRECTION('',(0.,0.,1.));
#122367=DIRECTION('center_axis',(0.358921627719158,-0.933367700935813,2.28597556646122E-6));
#122368=DIRECTION('ref_axis',(0.883552304442921,0.339766169107703,0.322326349595374));
#122369=DIRECTION('',(0.,0.,-1.));
#122370=DIRECTION('center_axis',(0.978686439631208,-0.205360300160449,0.));
#122371=DIRECTION('ref_axis',(0.205360300160449,0.978686439631208,0.));
#122372=DIRECTION('center_axis',(-0.978686439631198,0.205360300160498,-2.97053001959438E-14));
#122373=DIRECTION('ref_axis',(0.205084569137578,0.977372387144383,-0.0518028604359201));
#122374=DIRECTION('',(0.,0.,1.));
#122375=DIRECTION('',(0.,0.,1.));
#122376=DIRECTION('center_axis',(0.,0.,1.));
#122377=DIRECTION('ref_axis',(-0.761445958369139,0.648228395307783,0.));
#122378=DIRECTION('center_axis',(0.,0.,-1.));
#122379=DIRECTION('ref_axis',(0.761445958369139,-0.648228395307783,0.));
#122380=DIRECTION('center_axis',(0.564718130564305,-0.790859871782637,-0.235868811452275));
#122381=DIRECTION('ref_axis',(0.686284674053918,0.291277877306599,0.666461209936834));
#122382=DIRECTION('center_axis',(0.870851413018679,-0.431258298734532,0.2358688114524));
#122383=DIRECTION('ref_axis',(-0.178013252433613,-0.723975647090741,-0.666461209957151));
#122384=DIRECTION('center_axis',(0.,0.,-1.));
#122385=DIRECTION('ref_axis',(0.761445958369138,-0.648228395307784,0.));
#122386=DIRECTION('center_axis',(-0.770600293018847,0.637318749449024,-6.76296429840134E-17));
#122387=DIRECTION('ref_axis',(0.637318749449024,0.770600293018847,-9.86076131526264E-32));
#122388=DIRECTION('center_axis',(0.,0.,1.));
#122389=DIRECTION('ref_axis',(-0.761445958369138,0.648228395307784,0.));
#122390=DIRECTION('center_axis',(-0.75213718556306,0.659006566047167,-1.38914942345546E-16));
#122391=DIRECTION('ref_axis',(-0.659006566047166,-0.75213718556306,1.06003184139073E-30));
#122392=DIRECTION('center_axis',(0.,0.,-1.));
#122393=DIRECTION('ref_axis',(0.76144595836914,-0.648228395307782,0.));
#122394=DIRECTION('center_axis',(0.,0.,1.));
#122395=DIRECTION('ref_axis',(-0.76144595836914,0.648228395307782,0.));
#122396=DIRECTION('center_axis',(0.,0.,1.));
#122397=DIRECTION('ref_axis',(-0.76144595836914,0.648228395307782,0.));
#122398=DIRECTION('center_axis',(0.153619787612189,0.732106463019423,0.663642288932205));
#122399=DIRECTION('ref_axis',(0.460652306917222,0.541108411563798,-0.703563173472535));
#122400=DIRECTION('center_axis',(0.154061610443123,0.734212059928934,0.661209249211309));
#122401=DIRECTION('ref_axis',(0.459157418949153,0.539352431094974,-0.705884848750767));
#122402=DIRECTION('center_axis',(-0.700212553869644,-0.269266983049852,
-0.661209249211308));
#122403=DIRECTION('ref_axis',(-0.459157418949171,-0.539352431094955,0.70588484875077));
#122404=DIRECTION('center_axis',(-0.698204461834818,-0.268494770553923,
-0.663642288932184));
#122405=DIRECTION('ref_axis',(-0.46065230691722,-0.541108411563773,0.703563173472556));
#122406=DIRECTION('center_axis',(0.,0.,1.));
#122407=DIRECTION('ref_axis',(-0.76144595836914,0.648228395307782,0.));
#122408=DIRECTION('center_axis',(0.,0.,1.));
#122409=DIRECTION('ref_axis',(-0.76144595836914,0.648228395307782,0.));
#122410=DIRECTION('center_axis',(0.,0.,1.));
#122411=DIRECTION('ref_axis',(0.761445958369091,-0.648228395307839,0.));
#122412=DIRECTION('center_axis',(0.,0.,-1.));
#122413=DIRECTION('ref_axis',(-0.761445958369138,0.648228395307784,0.));
#122414=DIRECTION('center_axis',(-0.417989709277585,0.908451761481059,0.));
#122415=DIRECTION('ref_axis',(-0.908451761481059,-0.417989709277585,0.));
#122416=DIRECTION('',(0.,0.,1.));
#122417=DIRECTION('center_axis',(0.417985258662655,-0.908453809247057,2.28597556699346E-6));
#122418=DIRECTION('ref_axis',(0.859968058324844,0.395677473606074,0.322326349437511));
#122419=DIRECTION('',(0.,0.,-1.));
#122420=DIRECTION('center_axis',(0.98983310298378,-0.142233709919634,0.));
#122421=DIRECTION('ref_axis',(0.142233709919634,0.98983310298378,0.));
#122422=DIRECTION('center_axis',(-0.989833102983781,0.142233709919624,4.45769191956972E-15));
#122423=DIRECTION('ref_axis',(0.14204273704737,0.988504084210138,-0.0518028604612583));
#122424=DIRECTION('',(0.,0.,1.));
#122425=DIRECTION('',(0.,0.,1.));
#122426=DIRECTION('center_axis',(0.,0.,1.));
#122427=DIRECTION('ref_axis',(-0.801413621867962,0.59811053049121,0.));
#122428=DIRECTION('center_axis',(0.,0.,-1.));
#122429=DIRECTION('ref_axis',(0.801413621867962,-0.59811053049121,0.));
#122430=DIRECTION('center_axis',(0.614228422558437,-0.753053350504075,-0.235868811452385));
#122431=DIRECTION('ref_axis',(0.666212390911907,0.334649825703311,0.666461209938121));
#122432=DIRECTION('center_axis',(0.896692969460538,-0.374576590704866,0.235868811452388));
#122433=DIRECTION('ref_axis',(-0.131262226148597,-0.733893509725554,-0.666461209950904));
#122434=DIRECTION('center_axis',(0.,0.,-1.));
#122435=DIRECTION('ref_axis',(0.80141362186796,-0.598110530491212,0.));
#122436=DIRECTION('center_axis',(-0.809850164545249,0.58663677943514,-6.76296429840134E-17));
#122437=DIRECTION('ref_axis',(0.58663677943514,0.809850164545249,-5.66993775627602E-31));
#122438=DIRECTION('center_axis',(0.,0.,1.));
#122439=DIRECTION('ref_axis',(-0.80141362186796,0.598110530491212,0.));
#122440=DIRECTION('center_axis',(-0.792814534704237,0.60946297144429,-1.38914942345546E-16));
#122441=DIRECTION('ref_axis',(-0.60946297144429,-0.792814534704237,-1.23259516440783E-31));
#122442=DIRECTION('center_axis',(0.,0.,-1.));
#122443=DIRECTION('ref_axis',(0.801413621867966,-0.598110530491204,0.));
#122444=DIRECTION('center_axis',(0.,0.,1.));
#122445=DIRECTION('ref_axis',(-0.801413621867966,0.598110530491204,0.));
#122446=DIRECTION('center_axis',(0.,0.,1.));
#122447=DIRECTION('ref_axis',(-0.801413621867966,0.598110530491204,0.));
#122448=DIRECTION('center_axis',(0.106397937147913,0.740444725358681,0.663642288932205));
#122449=DIRECTION('ref_axis',(0.425036912385557,0.569510740937352,-0.703563173472533));
#122450=DIRECTION('center_axis',(0.106703946149272,0.742574303779487,0.661209249211309));
#122451=DIRECTION('ref_axis',(0.423657601880061,0.567662590517769,-0.705884848750766));
#122452=DIRECTION('center_axis',(-0.681521897242611,-0.313576517514068,
-0.661209249211308));
#122453=DIRECTION('ref_axis',(-0.423657601880075,-0.567662590517753,0.70588484875077));
#122454=DIRECTION('center_axis',(-0.679567406872724,-0.312677232713118,
-0.663642288932184));
#122455=DIRECTION('ref_axis',(-0.425036912385535,-0.569510740937347,0.70356317347255));
#122456=DIRECTION('center_axis',(0.,0.,1.));
#122457=DIRECTION('ref_axis',(-0.801413621867966,0.598110530491204,0.));
#122458=DIRECTION('center_axis',(0.,0.,1.));
#122459=DIRECTION('ref_axis',(-0.801413621867966,0.598110530491204,0.));
#122460=DIRECTION('center_axis',(0.,0.,1.));
#122461=DIRECTION('ref_axis',(0.801413621867988,-0.598110530491173,0.));
#122462=DIRECTION('center_axis',(0.,0.,-1.));
#122463=DIRECTION('ref_axis',(-0.80141362186796,0.598110530491212,0.));
#122464=DIRECTION('center_axis',(-0.475335608790577,0.879804557282861,0.));
#122465=DIRECTION('ref_axis',(-0.879804557282862,-0.475335608790577,0.));
#122466=DIRECTION('',(0.,0.,1.));
#122467=DIRECTION('center_axis',(0.475331298520703,-0.879806885993396,2.28597555931563E-6));
#122468=DIRECTION('ref_axis',(0.832850018919391,0.449962854461081,0.322326349514286));
#122469=DIRECTION('',(0.,0.,-1.));
#122470=DIRECTION('center_axis',(0.996912329797656,-0.0785226508557234,
0.));
#122471=DIRECTION('ref_axis',(0.0785226508557234,0.996912329797656,0.));
#122472=DIRECTION('center_axis',(-0.996912329797664,0.0785226508556254,
4.36901230372518E-14));
#122473=DIRECTION('ref_axis',(0.0784172208831005,0.995573805965461,-0.051802860388376));
#122474=DIRECTION('',(0.,0.,1.));
#122475=DIRECTION('',(0.,0.,1.));
#122476=DIRECTION('center_axis',(0.,0.,1.));
#122477=DIRECTION('ref_axis',(-0.83808810489185,0.545534901210534,0.));
#122478=DIRECTION('center_axis',(0.,0.,-1.));
#122479=DIRECTION('ref_axis',(0.83808810489185,-0.545534901210534,0.));
#122480=DIRECTION('center_axis',(0.661214718212524,-0.712152371479,-0.235868811452401));
#122481=DIRECTION('ref_axis',(0.643402498150284,0.376646626178607,0.66646120994567));
#122482=DIRECTION('center_axis',(0.918849822150862,-0.316355667117517,0.235868811452384));
#122483=DIRECTION('ref_axis',(-0.0839718152178504,-0.740795646506438,-0.666461209948582));
#122484=DIRECTION('center_axis',(0.,0.,-1.));
#122485=DIRECTION('ref_axis',(0.838088104891844,-0.545534901210544,0.));
#122486=DIRECTION('center_axis',(-0.84577218803322,0.533544193061362,-6.76296429840134E-17));
#122487=DIRECTION('ref_axis',(0.533544193061362,0.84577218803322,-5.54667823983524E-31));
#122488=DIRECTION('center_axis',(0.,0.,1.));
#122489=DIRECTION('ref_axis',(-0.838088104891844,0.545534901210544,0.));
#122490=DIRECTION('center_axis',(-0.83023403886413,0.557414962762352,-1.38914942345546E-16));
#122491=DIRECTION('ref_axis',(-0.557414962762352,-0.83023403886413,7.64209001932855E-31));
#122492=DIRECTION('center_axis',(0.,0.,-1.));
#122493=DIRECTION('ref_axis',(0.838088104891845,-0.545534901210541,0.));
#122494=DIRECTION('center_axis',(0.,0.,1.));
#122495=DIRECTION('ref_axis',(-0.838088104891845,0.545534901210541,0.));
#122496=DIRECTION('center_axis',(0.,0.,1.));
#122497=DIRECTION('ref_axis',(-0.838088104891845,0.545534901210541,0.));
#122498=DIRECTION('center_axis',(0.0587388747376102,0.745740341496545,0.663642288932205));
#122499=DIRECTION('ref_axis',(0.387674950010748,0.59557282851673,-0.703563173472536));
#122500=DIRECTION('center_axis',(0.0589078124527693,0.747885150534122,0.661209249211309));
#122501=DIRECTION('ref_axis',(0.386416884850565,0.593640102592886,-0.705884848750767));
#122502=DIRECTION('center_axis',(-0.660030720953819,-0.356597498805866,
-0.661209249211308));
#122503=DIRECTION('ref_axis',(-0.386416884850578,-0.593640102592876,0.705884848750768));
#122504=DIRECTION('center_axis',(-0.658137863669038,-0.355574837054039,
-0.663642288932184));
#122505=DIRECTION('ref_axis',(-0.387674950010746,-0.595572828516711,0.703563173472553));
#122506=DIRECTION('center_axis',(0.,0.,1.));
#122507=DIRECTION('ref_axis',(-0.838088104891845,0.545534901210541,0.));
#122508=DIRECTION('center_axis',(0.,0.,1.));
#122509=DIRECTION('ref_axis',(-0.838088104891845,0.545534901210541,0.));
#122510=DIRECTION('center_axis',(0.,0.,1.));
#122511=DIRECTION('ref_axis',(0.83808810489183,-0.545534901210566,0.));
#122512=DIRECTION('center_axis',(0.,0.,-1.));
#122513=DIRECTION('ref_axis',(-0.838088104891844,0.545534901210544,0.));
#122514=DIRECTION('center_axis',(-0.530728252327879,0.847542047441303,0.));
#122515=DIRECTION('ref_axis',(-0.847542047441303,-0.530728252327879,0.));
#122516=DIRECTION('',(0.,0.,1.));
#122517=DIRECTION('center_axis',(0.530724100115005,-0.847544647527133,2.28597551887765E-6));
#122518=DIRECTION('ref_axis',(0.802309620147107,0.502399241430756,0.322326349573232));
#122519=DIRECTION('',(0.,0.,-1.));
#122520=DIRECTION('center_axis',(0.999895030011369,-0.0144889253763915,
0.));
#122521=DIRECTION('ref_axis',(0.0144889253763915,0.99989503001137,0.));
#122522=DIRECTION('center_axis',(-0.999895030011369,0.0144889253764111,
-1.28134931560421E-14));
#122523=DIRECTION('ref_axis',(0.0144694715374454,0.998552501397843,-0.0518028603991841));
#122524=DIRECTION('',(0.,0.,1.));
#122525=DIRECTION('',(0.,0.,1.));
#122526=DIRECTION('center_axis',(0.,0.,1.));
#122527=DIRECTION('ref_axis',(-0.871318704123387,0.490717552003943,0.));
#122528=DIRECTION('center_axis',(0.,0.,-1.));
#122529=DIRECTION('ref_axis',(0.871318704123387,-0.490717552003943,0.));
#122530=DIRECTION('center_axis',(0.705483940759275,-0.66832500560343,-0.235868811452342));
#122531=DIRECTION('ref_axis',(0.617948726513988,0.417095704873767,0.666461209955685));
#122532=DIRECTION('center_axis',(0.93723092382929,-0.256834770235915,0.235868811452386));
#122533=DIRECTION('ref_axis',(-0.0363363460880332,-0.744653695079018,-0.666461209942586));
#122534=DIRECTION('center_axis',(0.,0.,-1.));
#122535=DIRECTION('ref_axis',(0.871318704123392,-0.490717552003933,0.));
#122536=DIRECTION('center_axis',(-0.878218752182996,0.478259159153425,-6.76296429840134E-17));
#122537=DIRECTION('ref_axis',(0.478259159153425,0.878218752182996,6.93889390390724E-14));
#122538=DIRECTION('center_axis',(0.,0.,1.));
#122539=DIRECTION('ref_axis',(-0.871318704123392,0.490717552003933,0.));
#122540=DIRECTION('center_axis',(-0.864241933273687,0.503076416433289,-1.38914942345546E-16));
#122541=DIRECTION('ref_axis',(-0.503076416433289,-0.864241933273687,-1.46678824564532E-30));
#122542=DIRECTION('center_axis',(0.,0.,-1.));
#122543=DIRECTION('ref_axis',(0.871318704123391,-0.490717552003934,0.));
#122544=DIRECTION('center_axis',(0.,0.,1.));
#122545=DIRECTION('ref_axis',(-0.871318704123391,0.490717552003934,0.));
#122546=DIRECTION('center_axis',(0.,0.,1.));
#122547=DIRECTION('ref_axis',(-0.871318704123391,0.490717552003934,0.));
#122548=DIRECTION('center_axis',(0.0108384416915616,0.747971550610398,0.663642288932205));
#122549=DIRECTION('ref_axis',(0.348719948110342,0.619187579593757,-0.703563173472536));
#122550=DIRECTION('center_axis',(0.0108696139192121,0.75012277678435,0.661209249211309));
#122551=DIRECTION('ref_axis',(0.347588297955049,0.617178220151048,-0.70588484875077));
#122552=DIRECTION('center_axis',(-0.635827336856483,-0.398153144485148,
-0.661209249211308));
#122553=DIRECTION('ref_axis',(-0.347588297955069,-0.61717822015104,0.705884848750767));
#122554=DIRECTION('center_axis',(-0.634003890813407,-0.397011308118942,
-0.663642288932184));
#122555=DIRECTION('ref_axis',(-0.34871994811034,-0.619187579593738,0.703563173472553));
#122556=DIRECTION('center_axis',(0.,0.,1.));
#122557=DIRECTION('ref_axis',(-0.871318704123391,0.490717552003934,0.));
#122558=DIRECTION('center_axis',(0.,0.,1.));
#122559=DIRECTION('ref_axis',(-0.871318704123391,0.490717552003934,0.));
#122560=DIRECTION('center_axis',(0.,0.,1.));
#122561=DIRECTION('ref_axis',(0.871318704123372,-0.490717552003968,0.));
#122562=DIRECTION('center_axis',(0.,0.,-1.));
#122563=DIRECTION('ref_axis',(-0.871318704123392,0.490717552003933,0.));
#122564=DIRECTION('center_axis',(-0.583940019635513,0.811796805529608,0.));
#122565=DIRECTION('ref_axis',(-0.811796805529608,-0.583940019635513,0.));
#122566=DIRECTION('',(0.,0.,1.));
#122567=DIRECTION('center_axis',(0.583936042541839,-0.811799666306503,2.28597554981395E-6));
#122568=DIRECTION('ref_axis',(0.768472359086984,0.552771162175832,0.322326349506313));
#122569=DIRECTION('',(0.,0.,-1.));
#122570=DIRECTION('center_axis',(0.998768947069955,0.0496043382051768,0.));
#122571=DIRECTION('ref_axis',(-0.0496043382051768,0.998768947069955,0.));
#122572=DIRECTION('center_axis',(-0.998768947069955,-0.0496043382051805,
5.96571961151145E-15));
#122573=DIRECTION('ref_axis',(0.0495377359705003,-0.997427930412718,0.0518028604183216));
#122574=DIRECTION('',(0.,0.,1.));
#122575=DIRECTION('',(0.,0.,1.));
#122576=DIRECTION('center_axis',(0.,0.,1.));
#122577=DIRECTION('ref_axis',(-0.900968867902423,0.433883739117549,0.));
#122578=DIRECTION('center_axis',(0.,0.,-1.));
#122579=DIRECTION('ref_axis',(0.900968867902423,-0.433883739117549,0.));
#122580=DIRECTION('center_axis',(0.74685417846772,-0.621751348924435,-0.235868811452366));
#122581=DIRECTION('ref_axis',(0.589955671017639,0.455830847862106,0.666461209952569));
#122582=DIRECTION('center_axis',(0.951760742606324,-0.196258484192456,0.235868811452338));
#122583=DIRECTION('ref_axis',(0.0114484368873645,-0.745451801881426,-0.666461209947415));
#122584=DIRECTION('center_axis',(0.,0.,-1.));
#122585=DIRECTION('ref_axis',(0.900968867902422,-0.433883739117553,0.));
#122586=DIRECTION('center_axis',(-0.907056527102721,0.421008855774258,-6.76296429840134E-17));
#122587=DIRECTION('ref_axis',(0.421008855774258,0.907056527102721,6.9388939039073E-14));
#122588=DIRECTION('center_axis',(0.,0.,1.));
#122589=DIRECTION('ref_axis',(-0.900968867902422,0.433883739117553,0.));
#122590=DIRECTION('center_axis',(-0.894698472200109,0.446670621199548,-1.38914942345546E-16));
#122591=DIRECTION('ref_axis',(-0.446670621199548,-0.894698472200109,3.69778549322349E-32));
#122592=DIRECTION('center_axis',(0.,0.,-1.));
#122593=DIRECTION('ref_axis',(0.900968867902425,-0.433883739117546,0.));
#122594=DIRECTION('center_axis',(0.,0.,1.));
#122595=DIRECTION('ref_axis',(-0.900968867902425,0.433883739117546,0.));
#122596=DIRECTION('center_axis',(0.,0.,1.));
#122597=DIRECTION('ref_axis',(-0.900968867902425,0.433883739117546,0.));
#122598=DIRECTION('center_axis',(-0.0371065288362363,0.747129184183398,
0.663642288932205));
#122599=DIRECTION('ref_axis',(0.308331981142967,0.640257956090912,-0.703563173472532));
#122600=DIRECTION('center_axis',(-0.037213250189464,0.749277987643941,0.661209249211309));
#122601=DIRECTION('ref_axis',(0.307331396185796,0.638180220018292,-0.705884848750768));
#122602=DIRECTION('center_axis',(-0.609011201847467,-0.438072693490158,
-0.661209249211308));
#122603=DIRECTION('ref_axis',(-0.307331396185819,-0.638180220018278,0.70588484875077));
#122604=DIRECTION('center_axis',(-0.607264659977016,-0.436816374560125,
-0.663642288932184));
#122605=DIRECTION('ref_axis',(-0.308331981142956,-0.640257956090894,0.703563173472554));
#122606=DIRECTION('center_axis',(0.,0.,1.));
#122607=DIRECTION('ref_axis',(-0.900968867902425,0.433883739117546,0.));
#122608=DIRECTION('center_axis',(0.,0.,1.));
#122609=DIRECTION('ref_axis',(-0.900968867902425,0.433883739117546,0.));
#122610=DIRECTION('center_axis',(0.,0.,1.));
#122611=DIRECTION('ref_axis',(0.900968867902412,-0.433883739117574,0.));
#122612=DIRECTION('center_axis',(0.,0.,-1.));
#122613=DIRECTION('ref_axis',(-0.900968867902422,0.433883739117553,0.));
#122614=DIRECTION('center_axis',(-0.634752252147723,0.772715716414124,0.));
#122615=DIRECTION('ref_axis',(-0.772715716414124,-0.634752252147723,0.));
#122616=DIRECTION('',(0.,0.,1.));
#122617=DIRECTION('center_axis',(0.634748466515921,-0.772718826126594,2.28597560005782E-6));
#122618=DIRECTION('ref_axis',(0.731477280229487,0.600871627619704,0.322326349574031));
#122619=DIRECTION('',(0.,0.,-1.));
#122620=DIRECTION('center_axis',(0.993538708289763,0.113493766920963,0.));
#122621=DIRECTION('ref_axis',(-0.113493766920963,0.993538708289763,0.));
#122622=DIRECTION('center_axis',(-0.993538708289748,-0.113493766921094,
5.7807728191039E-14));
#122623=DIRECTION('ref_axis',(0.113341382295553,-0.992204714114264,0.0518028604303367));
#122624=DIRECTION('',(0.,0.,1.));
#122625=DIRECTION('',(0.,0.,1.));
#122626=DIRECTION('center_axis',(0.,0.,1.));
#122627=DIRECTION('ref_axis',(-0.926916757346023,0.375267004879372,0.));
#122628=DIRECTION('center_axis',(0.,0.,-1.));
#122629=DIRECTION('ref_axis',(0.926916757346023,-0.375267004879372,0.));
#122630=DIRECTION('center_axis',(0.785155432157007,-0.572622782587642,-0.235868811452318));
#122631=DIRECTION('ref_axis',(0.559538361127005,0.492692884129434,0.666461209940628));
#122632=DIRECTION('center_axis',(0.962379572339946,-0.134875729940102,0.235868811452272));
#122633=DIRECTION('ref_axis',(0.059186175773507,-0.743186687345194,-0.666461209936621));
#122634=DIRECTION('center_axis',(0.,0.,-1.));
#122635=DIRECTION('ref_axis',(0.926916757346024,-0.375267004879368,0.));
#122636=DIRECTION('center_axis',(-0.932167012189566,0.362028536700599,-6.76296429840134E-17));
#122637=DIRECTION('ref_axis',(0.362028536700599,0.932167012189566,8.65898102996501E-31));
#122638=DIRECTION('center_axis',(0.,0.,1.));
#122639=DIRECTION('ref_axis',(-0.926916757346024,0.375267004879368,0.));
#122640=DIRECTION('center_axis',(-0.921478503192041,0.388429360572751,-1.38914942345546E-16));
#122641=DIRECTION('ref_axis',(-0.388429360572751,-0.921478503192041,5.97808654737798E-31));
#122642=DIRECTION('center_axis',(0.,0.,-1.));
#122643=DIRECTION('ref_axis',(0.92691675734602,-0.375267004879378,0.));
#122644=DIRECTION('center_axis',(0.,0.,1.));
#122645=DIRECTION('ref_axis',(-0.926916757346019,0.375267004879381,0.));
#122646=DIRECTION('center_axis',(0.,0.,1.));
#122647=DIRECTION('ref_axis',(-0.926916757346019,0.375267004879381,0.));
#122648=DIRECTION('center_axis',(-0.0848990206777204,0.743216703679881,
0.663642288932205));
#122649=DIRECTION('ref_axis',(0.266677011928053,0.658697375311593,-0.703563173472535));
#122650=DIRECTION('center_axis',(-0.0851431970708945,0.745354254532678,
0.661209249211309));
#122651=DIRECTION('ref_axis',(0.265811603787226,0.656559800472254,-0.705884848750769));
#122652=DIRECTION('center_axis',(-0.579692509177567,-0.476192107831319,
-0.661209249211308));
#122653=DIRECTION('ref_axis',(-0.265811603787247,-0.656559800472248,0.705884848750767));
#122654=DIRECTION('center_axis',(-0.578030048394918,-0.474826468821422,
-0.663642288932184));
#122655=DIRECTION('ref_axis',(-0.266677011928043,-0.658697375311579,0.703563173472551));
#122656=DIRECTION('center_axis',(0.,0.,1.));
#122657=DIRECTION('ref_axis',(-0.92691675734602,0.375267004879378,0.));
#122658=DIRECTION('center_axis',(0.,0.,1.));
#122659=DIRECTION('ref_axis',(-0.92691675734602,0.375267004879378,0.));
#122660=DIRECTION('center_axis',(0.,0.,1.));
#122661=DIRECTION('ref_axis',(0.926916757346018,-0.375267004879384,0.));
#122662=DIRECTION('center_axis',(0.,0.,-1.));
#122663=DIRECTION('ref_axis',(-0.926916757346024,0.375267004879368,0.));
#122664=DIRECTION('center_axis',(-0.682956151501928,0.730459372672893,0.));
#122665=DIRECTION('ref_axis',(-0.730459372672893,-0.682956151501928,0.));
#122666=DIRECTION('',(0.,0.,1.));
#122667=DIRECTION('center_axis',(0.682952572888172,-0.730462718542295,2.28597554966162E-6));
#122668=DIRECTION('ref_axis',(0.691476404378248,0.646502982704101,0.322326349439246));
#122669=DIRECTION('',(0.,0.,-1.));
#122670=DIRECTION('center_axis',(0.984225805843823,0.176916825404134,0.));
#122671=DIRECTION('ref_axis',(-0.176916825404134,0.984225805843823,0.));
#122672=DIRECTION('center_axis',(-0.984225805843822,-0.176916825404143,
4.89397666063556E-15));
#122673=DIRECTION('ref_axis',(0.176679284569536,-0.982904315822576,0.0518028603587719));
#122674=DIRECTION('',(0.,0.,1.));
#122675=DIRECTION('',(0.,0.,1.));
#122676=DIRECTION('center_axis',(0.,0.,1.));
#122677=DIRECTION('ref_axis',(-0.949055747010676,0.315108218023599,0.));
#122678=DIRECTION('center_axis',(0.,0.,-1.));
#122679=DIRECTION('ref_axis',(0.949055747010676,-0.315108218023599,0.));
#122680=DIRECTION('center_axis',(0.820230313760376,-0.521141186409809,-0.235868811452324));
#122681=DIRECTION('ref_axis',(0.526821788080383,0.527530339630141,0.66646120995411));
#122682=DIRECTION('center_axis',(0.969043777980972,-0.0729387423830074,
0.235868811452363));
#122683=DIRECTION('ref_axis',(0.106680705974441,-0.73786765928216,-0.66646120994268));
#122684=DIRECTION('center_axis',(0.,0.,-1.));
#122685=DIRECTION('ref_axis',(0.949055747010671,-0.315108218023615,0.));
#122686=DIRECTION('center_axis',(-0.953447023074127,0.301560564714759,-6.76296429840134E-17));
#122687=DIRECTION('ref_axis',(0.301560564714759,0.953447023074127,6.93889390390713E-14));
#122688=DIRECTION('center_axis',(0.,0.,1.));
#122689=DIRECTION('ref_axis',(-0.949055747010671,0.315108218023615,0.));
#122690=DIRECTION('center_axis',(-0.944471981357837,0.328591960385524,-1.38914942345546E-16));
#122691=DIRECTION('ref_axis',(-0.328591960385524,-0.944471981357837,1.17096540618744E-31));
#122692=DIRECTION('center_axis',(0.,0.,-1.));
#122693=DIRECTION('ref_axis',(0.949055747010673,-0.315108218023608,0.));
#122694=DIRECTION('center_axis',(0.,0.,1.));
#122695=DIRECTION('ref_axis',(-0.949055747010673,0.315108218023608,0.));
#122696=DIRECTION('center_axis',(0.,0.,1.));
#122697=DIRECTION('ref_axis',(-0.949055747010673,0.315108218023608,0.));
#122698=DIRECTION('center_axis',(-0.132342644232457,0.73625018632146,0.663642288932205));
#122699=DIRECTION('ref_axis',(0.223926209669102,0.674430065726972,-0.703563173472533));
#122700=DIRECTION('center_axis',(-0.132723272292402,0.738367700911554,0.661209249211309));
#122701=DIRECTION('ref_axis',(0.223199534492297,0.67224143587444,-0.705884848750767));
#122702=DIRECTION('center_axis',(-0.547991735643803,-0.512354746658515,
-0.661209249211308));
#122703=DIRECTION('ref_axis',(-0.223199534492311,-0.672241435874435,0.705884848750767));
#122704=DIRECTION('center_axis',(-0.546420187356908,-0.510885399272374,
-0.663642288932184));
#122705=DIRECTION('ref_axis',(-0.223926209669094,-0.674430065726953,0.703563173472554));
#122706=DIRECTION('center_axis',(0.,0.,1.));
#122707=DIRECTION('ref_axis',(-0.949055747010673,0.315108218023608,0.));
#122708=DIRECTION('center_axis',(0.,0.,1.));
#122709=DIRECTION('ref_axis',(-0.949055747010673,0.315108218023608,0.));
#122710=DIRECTION('center_axis',(0.,0.,1.));
#122711=DIRECTION('ref_axis',(0.949055747010662,-0.315108218023641,0.));
#122712=DIRECTION('center_axis',(0.,0.,-1.));
#122713=DIRECTION('ref_axis',(-0.949055747010671,0.315108218023615,0.));
#122714=DIRECTION('center_axis',(-0.728353637535975,0.685201414686305,0.));
#122715=DIRECTION('ref_axis',(-0.685201414686304,-0.728353637535975,0.));
#122716=DIRECTION('',(0.,0.,1.));
#122717=DIRECTION('center_axis',(0.728350280645412,-0.685204982963875,2.28597554837052E-6));
#122718=DIRECTION('ref_axis',(0.648634103605699,0.689477718308503,0.322326349521306));
#122719=DIRECTION('',(0.,0.,-1.));
#122720=DIRECTION('center_axis',(0.970868508445898,0.23961289470318,0.));
#122721=DIRECTION('ref_axis',(-0.23961289470318,0.970868508445898,0.));
#122722=DIRECTION('center_axis',(-0.97086850844591,-0.239612894703131,-1.78307676782824E-14));
#122723=DIRECTION('ref_axis',(0.239291173764342,-0.969564952857368,0.0518028604342702));
#122724=DIRECTION('',(0.,0.,1.));
#122725=DIRECTION('',(0.,0.,1.));
#122726=DIRECTION('center_axis',(0.,0.,1.));
#122727=DIRECTION('ref_axis',(-0.967294863039036,0.253654583909484,0.));
#122728=DIRECTION('center_axis',(0.,0.,-1.));
#122729=DIRECTION('ref_axis',(0.967294863039036,-0.253654583909484,0.));
#122730=DIRECTION('center_axis',(0.851934693065737,-0.467518109312347,-0.235868811452463));
#122731=DIRECTION('ref_axis',(0.491940391306886,0.560200059816394,0.666461209960892));
#122732=DIRECTION('center_axis',(0.971725974879099,-0.0107020338878288,
0.235868811452317));
#122733=DIRECTION('ref_axis',(0.153736862271372,-0.729516574733322,-0.666461209950222));
#122734=DIRECTION('center_axis',(0.,0.,-1.));
#122735=DIRECTION('ref_axis',(0.967294863039031,-0.253654583909501,0.));
#122736=DIRECTION('center_axis',(-0.970809115627132,0.239853415683968,-6.76296429840134E-17));
#122737=DIRECTION('ref_axis',(0.239853415683968,0.970809115627132,1.81807786750155E-31));
#122738=DIRECTION('center_axis',(0.,0.,1.));
#122739=DIRECTION('ref_axis',(-0.967294863039031,0.253654583909501,0.));
#122740=DIRECTION('center_axis',(-0.963584421563629,0.267404305350318,-1.38914942345546E-16));
#122741=DIRECTION('ref_axis',(-0.267404305350318,-0.963584421563629,9.05957445839756E-31));
#122742=DIRECTION('center_axis',(0.,0.,-1.));
#122743=DIRECTION('ref_axis',(0.967294863039032,-0.253654583909497,0.));
#122744=DIRECTION('center_axis',(0.,0.,1.));
#122745=DIRECTION('ref_axis',(-0.967294863039032,0.253654583909497,0.));
#122746=DIRECTION('center_axis',(0.,0.,1.));
#122747=DIRECTION('ref_axis',(-0.967294863039032,0.253654583909497,0.));
#122748=DIRECTION('center_axis',(-0.179242443474634,0.726258259022275,0.663642288932205));
#122749=DIRECTION('ref_axis',(0.180255246582592,0.687391378337485,-0.703563173472533));
#122750=DIRECTION('center_axis',(-0.179757959119008,0.728347036028009,0.661209249211309));
#122751=DIRECTION('ref_axis',(0.179670290433983,0.685160687021282,-0.705884848750767));
#122752=DIRECTION('center_axis',(-0.51403914652442,-0.546412009931942,-0.661209249211308));
#122753=DIRECTION('ref_axis',(-0.179670290434002,-0.685160687021275,0.705884848750769));
#122754=DIRECTION('center_axis',(-0.512564968562287,-0.544844992033141,
-0.663642288932184));
#122755=DIRECTION('ref_axis',(-0.180255246582581,-0.687391378337468,0.703563173472552));
#122756=DIRECTION('center_axis',(0.,0.,1.));
#122757=DIRECTION('ref_axis',(-0.967294863039032,0.253654583909497,0.));
#122758=DIRECTION('center_axis',(0.,0.,1.));
#122759=DIRECTION('ref_axis',(-0.967294863039032,0.253654583909497,0.));
#122760=DIRECTION('center_axis',(0.,0.,1.));
#122761=DIRECTION('ref_axis',(0.967294863039023,-0.253654583909532,0.));
#122762=DIRECTION('center_axis',(0.,0.,-1.));
#122763=DIRECTION('ref_axis',(-0.967294863039031,0.253654583909501,0.));
#122764=DIRECTION('center_axis',(-0.770758162242022,0.637127817111528,0.));
#122765=DIRECTION('ref_axis',(-0.637127817111528,-0.770758162242022,0.));
#122766=DIRECTION('',(0.,0.,1.));
#122767=DIRECTION('center_axis',(0.770755040868896,-0.637131593134385,2.28597555422295E-6));
#122768=DIRECTION('ref_axis',(0.603126426175686,0.729619242077449,0.322326349588231));
#122769=DIRECTION('',(0.,0.,-1.));
#122770=DIRECTION('center_axis',(0.953521704096127,0.301324343221085,0.));
#122771=DIRECTION('ref_axis',(-0.301324343221085,0.953521704096127,0.));
#122772=DIRECTION('center_axis',(-0.953521704096134,-0.301324343221062,
-1.04139270801893E-14));
#122773=DIRECTION('ref_axis',(0.300919764198671,-0.952241439532216,0.0518028604637758));
#122774=DIRECTION('',(0.,0.,1.));
#122775=DIRECTION('',(0.,0.,1.));
#122776=DIRECTION('center_axis',(0.,0.,1.));
#122777=DIRECTION('ref_axis',(-0.981559156991069,0.191158628701354,0.));
#122778=DIRECTION('center_axis',(0.,0.,-1.));
#122779=DIRECTION('ref_axis',(0.981559156991069,-0.191158628701354,0.));
#122780=DIRECTION('center_axis',(0.880138289977623,-0.411973900021994,-0.235868811452329));
#122781=DIRECTION('ref_axis',(0.455037505950061,0.59056779781637,0.666461209944789));
#122782=DIRECTION('center_axis',(0.970415141311856,0.0515786515599078,0.235868811452368));
#122783=DIRECTION('ref_axis',(0.200161280821526,-0.718167750109119,-0.666461209946305));
#122784=DIRECTION('center_axis',(0.,0.,-1.));
#122785=DIRECTION('ref_axis',(0.981559156991067,-0.191158628701366,0.));
#122786=DIRECTION('center_axis',(-0.984181945286122,0.177160657519735,-6.76296429840134E-17));
#122787=DIRECTION('ref_axis',(0.177160657519735,0.984181945286122,6.93889390390728E-14));
#122788=DIRECTION('center_axis',(0.,0.,1.));
#122789=DIRECTION('ref_axis',(-0.981559156991067,0.191158628701366,0.));
#122790=DIRECTION('center_axis',(-0.978737286693006,0.205117828666384,-1.38914942345546E-16));
#122791=DIRECTION('ref_axis',(-0.205117828666384,-0.978737286693006,4.74549138297015E-31));
#122792=DIRECTION('center_axis',(0.,0.,-1.));
#122793=DIRECTION('ref_axis',(0.981559156991067,-0.191158628701365,0.));
#122794=DIRECTION('center_axis',(0.,0.,1.));
#122795=DIRECTION('ref_axis',(-0.981559156991067,0.191158628701365,0.));
#122796=DIRECTION('center_axis',(0.,0.,1.));
#122797=DIRECTION('ref_axis',(-0.981559156991067,0.191158628701365,0.));
#122798=DIRECTION('center_axis',(-0.225405697069191,0.71328198075486,0.663642288932205));
#122799=DIRECTION('ref_axis',(0.135843576023242,0.697528052329421,-0.703563173472534));
#122800=DIRECTION('center_axis',(-0.226053981933632,0.715333436943476,0.661209249211309));
#122801=DIRECTION('ref_axis',(0.135402742613117,0.695264465938647,-0.705884848750767));
#122802=DIRECTION('center_axis',(-0.477974260290917,-0.57822394905155,-0.661209249211308));
#122803=DIRECTION('ref_axis',(-0.13540274261313,-0.695264465938645,0.705884848750767));
#122804=DIRECTION('center_axis',(-0.476603510367002,-0.57656569985276,-0.663642288932184));
#122805=DIRECTION('ref_axis',(-0.135843576023242,-0.6975280523294,0.703563173472554));
#122806=DIRECTION('center_axis',(0.,0.,1.));
#122807=DIRECTION('ref_axis',(-0.981559156991067,0.191158628701365,0.));
#122808=DIRECTION('center_axis',(0.,0.,1.));
#122809=DIRECTION('ref_axis',(-0.981559156991067,0.191158628701365,0.));
#122810=DIRECTION('center_axis',(0.,0.,1.));
#122811=DIRECTION('ref_axis',(0.981559156991053,-0.191158628701434,0.));
#122812=DIRECTION('center_axis',(0.,0.,-1.));
#122813=DIRECTION('ref_axis',(-0.981559156991067,0.191158628701366,0.));
#122814=DIRECTION('center_axis',(-0.80999547633231,0.586436124672751,0.));
#122815=DIRECTION('ref_axis',(-0.586436124672751,-0.80999547633231,0.));
#122816=DIRECTION('',(0.,0.,1.));
#122817=DIRECTION('center_axis',(0.80999260330302,-0.586440092924393,2.28597554479797E-6));
#122818=DIRECTION('ref_axis',(0.55514037291836,0.766762603911661,0.322326349525871));
#122819=DIRECTION('',(0.,0.,-1.));
#122820=DIRECTION('center_axis',(0.93225667453446,0.361797585378826,0.));
#122821=DIRECTION('ref_axis',(-0.361797585378826,0.932256674534461,0.));
#122822=DIRECTION('center_axis',(-0.93225667453447,-0.361797585378803,-6.98055585703023E-15));
#122823=DIRECTION('ref_axis',(0.361311810775726,-0.931004961879828,0.0518028604336393));
#122824=DIRECTION('',(0.,0.,1.));
#122825=DIRECTION('',(0.,0.,1.));
#122826=DIRECTION('center_axis',(0.,0.,1.));
#122827=DIRECTION('ref_axis',(-0.991790013823251,0.127877161684469,0.));
#122828=DIRECTION('center_axis',(0.,0.,-1.));
#122829=DIRECTION('ref_axis',(0.991790013823251,-0.127877161684469,0.));
#122830=DIRECTION('center_axis',(0.904725209867041,-0.354736801608044,-0.235868811452327));
#122831=DIRECTION('ref_axis',(0.416264773868949,0.618508766020696,0.666461209967533));
#122832=DIRECTION('center_axis',(0.965116663775578,0.113647389264953,0.235868811452381));
#122833=DIRECTION('ref_axis',(0.245763193733702,-0.703867820162628,-0.666461209932972));
#122834=DIRECTION('center_axis',(0.,0.,-1.));
#122835=DIRECTION('ref_axis',(0.991790013823247,-0.127877161684499,0.));
#122836=DIRECTION('center_axis',(-0.993510560225566,0.113739908212912,-6.76296429840134E-17));
#122837=DIRECTION('ref_axis',(0.113739908212912,0.993510560225566,-5.39260384428426E-32));
#122838=DIRECTION('center_axis',(0.,0.,1.));
#122839=DIRECTION('ref_axis',(-0.991790013823247,0.127877161684499,0.));
#122840=DIRECTION('center_axis',(-0.989868310372872,0.141988478826823,-1.38914942345546E-16));
#122841=DIRECTION('ref_axis',(-0.141988478826823,-0.989868310372872,3.05067303190938E-31));
#122842=DIRECTION('center_axis',(0.,0.,-1.));
#122843=DIRECTION('ref_axis',(0.991790013823245,-0.127877161684511,0.));
#122844=DIRECTION('center_axis',(0.,0.,1.));
#122845=DIRECTION('ref_axis',(-0.991790013823245,0.127877161684511,0.));
#122846=DIRECTION('center_axis',(0.,0.,1.));
#122847=DIRECTION('ref_axis',(-0.991790013823245,0.127877161684511,0.));
#122848=DIRECTION('center_axis',(-0.27064271030512,0.697374673830017,0.663642288932205));
#122849=DIRECTION('ref_axis',(0.0908736950716613,0.704798433935037,-0.703563173472533));
#122850=DIRECTION('center_axis',(-0.271421100448064,0.699380379328001,0.661209249211309));
#122851=DIRECTION('ref_axis',(0.0905787958790554,0.70251125403171,-0.705884848750768));
#122852=DIRECTION('center_axis',(-0.439945275296721,-0.607659841935857,
-0.661209249211308));
#122853=DIRECTION('ref_axis',(-0.0905787958790776,-0.702511254031706,0.705884848750769));
#122854=DIRECTION('center_axis',(-0.438683586116486,-0.605917175538729,
-0.663642288932184));
#122855=DIRECTION('ref_axis',(-0.0908736950716505,-0.704798433935021,0.703563173472551));
#122856=DIRECTION('center_axis',(0.,0.,1.));
#122857=DIRECTION('ref_axis',(-0.991790013823245,0.127877161684511,0.));
#122858=DIRECTION('center_axis',(0.,0.,1.));
#122859=DIRECTION('ref_axis',(-0.991790013823245,0.127877161684511,0.));
#122860=DIRECTION('center_axis',(0.,0.,1.));
#122861=DIRECTION('ref_axis',(0.991790013823245,-0.127877161684511,0.));
#122862=DIRECTION('center_axis',(0.,0.,-1.));
#122863=DIRECTION('ref_axis',(-0.991790013823247,0.127877161684499,0.));
#122864=DIRECTION('center_axis',(-0.845904345266863,0.533334640407541,0.));
#122865=DIRECTION('ref_axis',(-0.533334640407541,-0.845904345266863,0.));
#122866=DIRECTION('',(0.,0.,1.));
#122867=DIRECTION('center_axis',(0.845901732387273,-0.533338784581606,2.28597554008475E-6));
#122868=DIRECTION('ref_axis',(0.504873128786085,0.800755173732798,0.322326349481245));
#122869=DIRECTION('',(0.,0.,-1.));
#122870=DIRECTION('center_axis',(0.907160802328702,0.420784123652907,0.));
#122871=DIRECTION('ref_axis',(-0.420784123652907,0.907160802328703,0.));
#122872=DIRECTION('center_axis',(-0.907160802328718,-0.420784123652873,
-1.98035334639662E-14));
#122873=DIRECTION('ref_axis',(0.420219149621948,-0.905942785140381,0.0518028603756245));
#122874=DIRECTION('',(0.,0.,1.));
#122875=DIRECTION('',(0.,0.,1.));
#122876=DIRECTION('center_axis',(0.,0.,1.));
#122877=DIRECTION('ref_axis',(-0.997945392750336,0.0640702199807125,0.));
#122878=DIRECTION('center_axis',(0.,0.,-1.));
#122879=DIRECTION('ref_axis',(0.997945392750336,-0.0640702199807125,0.));
#122880=DIRECTION('center_axis',(0.925594419806154,-0.296042013585577,-0.235868811452269));
#122881=DIRECTION('ref_axis',(0.375781520549068,0.643908149076571,0.666461209948947));
#122882=DIRECTION('center_axis',(0.955852314850975,0.175249125470216,0.235868811452378));
#122883=DIRECTION('ref_axis',(0.290355212969804,-0.686675546343255,-0.666461209940573));
#122884=DIRECTION('center_axis',(0.,0.,-1.));
#122885=DIRECTION('ref_axis',(0.997945392750337,-0.0640702199807057,0.));
#122886=DIRECTION('center_axis',(-0.998756627165697,0.0498517772261083,
-6.76296429840134E-17));
#122887=DIRECTION('ref_axis',(0.0498517772261083,0.998756627165697,-3.73630409211124E-32));
#122888=DIRECTION('center_axis',(0.,0.,1.));
#122889=DIRECTION('ref_axis',(-0.997945392750337,0.0640702199807057,0.));
#122890=DIRECTION('center_axis',(-0.996931752839329,0.0782756678713304,
-1.38914942345546E-16));
#122891=DIRECTION('ref_axis',(-0.0782756678713304,-0.996931752839329,-1.95674482349743E-31));
#122892=DIRECTION('center_axis',(0.,0.,-1.));
#122893=DIRECTION('ref_axis',(0.997945392750337,-0.0640702199806998,0.));
#122894=DIRECTION('center_axis',(0.,0.,1.));
#122895=DIRECTION('ref_axis',(-0.997945392750337,0.0640702199806998,0.));
#122896=DIRECTION('center_axis',(0.,0.,1.));
#122897=DIRECTION('ref_axis',(-0.997945392750337,0.0640702199806997,0.));
#122898=DIRECTION('center_axis',(-0.314767594591725,0.678601704784009,0.663642288932205));
#122899=DIRECTION('ref_axis',(0.0455303946146855,0.709172647596824,-0.703563173472533));
#122900=DIRECTION('center_axis',(-0.315672891441111,0.680553417717247,0.661209249211309));
#122901=DIRECTION('ref_axis',(0.0453826414436359,0.706871272693765,-0.705884848750768));
#122902=DIRECTION('center_axis',(-0.400108460798365,-0.634598730187022,
-0.661209249211308));
#122903=DIRECTION('ref_axis',(-0.0453826414436631,-0.706871272693762,0.705884848750769));
#122904=DIRECTION('center_axis',(-0.398961016913284,-0.632778807581583,
-0.663642288932184));
#122905=DIRECTION('ref_axis',(-0.0455303946146791,-0.709172647596805,0.703563173472553));
#122906=DIRECTION('center_axis',(0.,0.,1.));
#122907=DIRECTION('ref_axis',(-0.997945392750337,0.0640702199806997,0.));
#122908=DIRECTION('center_axis',(0.,0.,1.));
#122909=DIRECTION('ref_axis',(-0.997945392750337,0.0640702199806997,0.));
#122910=DIRECTION('center_axis',(0.,0.,1.));
#122911=DIRECTION('ref_axis',(0.997945392750337,-0.0640702199806997,0.));
#122912=DIRECTION('center_axis',(0.,0.,-1.));
#122913=DIRECTION('ref_axis',(-0.997945392750337,0.0640702199807057,0.));
#122914=DIRECTION('center_axis',(-0.878337211800797,0.47804156970498,0.));
#122915=DIRECTION('ref_axis',(-0.47804156970498,-0.878337211800797,0.));
#122916=DIRECTION('',(0.,0.,1.));
#122917=DIRECTION('center_axis',(0.878334869807783,-0.478045872772184,2.28597554380844E-6));
#122918=DIRECTION('ref_axis',(0.452531252665384,0.831457268774235,0.322326349471446));
#122919=DIRECTION('',(0.,0.,-1.));
#122920=DIRECTION('center_axis',(0.878337211800797,0.47804156970498,0.));
#122921=DIRECTION('ref_axis',(-0.47804156970498,0.878337211800797,0.));
#122922=DIRECTION('center_axis',(-0.878337211800815,-0.478041569704948,
-1.94241554282581E-14));
#122923=DIRECTION('ref_axis',(0.477399717843322,-0.877157895167585,0.0518028604257383));
#122924=DIRECTION('',(0.,0.,1.));
#122925=DIRECTION('',(0.,0.,1.));
#122926=DIRECTION('center_axis',(0.,0.,1.));
#122927=DIRECTION('ref_axis',(-1.,0.,0.));
#122928=DIRECTION('center_axis',(0.,0.,-1.));
#122929=DIRECTION('ref_axis',(1.,0.,0.));
#122930=DIRECTION('center_axis',(0.942660163734981,-0.236130725428042,-0.235868811452395));
#122931=DIRECTION('ref_axis',(0.333754100353815,0.666661575414249,0.666461209946391));
#122932=DIRECTION('center_axis',(0.942660163734932,0.236130725428364,0.235868811452266));
#122933=DIRECTION('ref_axis',(0.333754100353955,-0.666661575429315,-0.66646120993125));
#122934=DIRECTION('center_axis',(0.,0.,-1.));
#122935=DIRECTION('ref_axis',(1.,0.,0.));
#122936=DIRECTION('center_axis',(-0.999898588892179,-0.0142412054064829,
-6.76296429840134E-17));
#122937=DIRECTION('ref_axis',(-0.0142412054064829,0.999898588892179,-3.2740809054583E-33));
#122938=DIRECTION('center_axis',(0.,0.,1.));
#122939=DIRECTION('ref_axis',(-1.,0.,0.));
#122940=DIRECTION('center_axis',(-0.999898588892179,0.0142412054064834,
-1.38914942345546E-16));
#122941=DIRECTION('ref_axis',(-0.0142412054064834,-0.999898588892179,3.85185988877447E-34));
#122942=DIRECTION('center_axis',(0.,0.,-1.));
#122943=DIRECTION('ref_axis',(1.,0.,0.));
#122944=DIRECTION('center_axis',(0.,0.,1.));
#122945=DIRECTION('ref_axis',(-1.,0.,0.));
#122946=DIRECTION('center_axis',(0.,0.,1.));
#122947=DIRECTION('ref_axis',(-1.,0.,0.));
#122948=DIRECTION('center_axis',(-0.357599031314712,0.657040215773436,0.663642288932205));
#122949=DIRECTION('ref_axis',(4.21884749357559E-15,0.710632718732581,-0.703563173472532));
#122950=DIRECTION('center_axis',(-0.358627514811599,0.658929916134845,0.661209249211309));
#122951=DIRECTION('ref_axis',(-9.74220704108575E-15,0.70832660567291,-0.705884848750767));
#122952=DIRECTION('center_axis',(-0.358627514811598,-0.658929916134846,
-0.661209249211308));
#122953=DIRECTION('ref_axis',(-9.24260668000443E-15,-0.708326605672909,
0.705884848750768));
#122954=DIRECTION('center_axis',(-0.35759903131472,-0.657040215773453,-0.663642288932184));
#122955=DIRECTION('ref_axis',(5.60662627435704E-15,-0.710632718732561,0.703563173472552));
#122956=DIRECTION('center_axis',(0.,0.,1.));
#122957=DIRECTION('ref_axis',(-1.,0.,0.));
#122958=DIRECTION('center_axis',(0.,0.,1.));
#122959=DIRECTION('ref_axis',(-1.,0.,0.));
#122960=DIRECTION('center_axis',(0.,0.,1.));
#122961=DIRECTION('ref_axis',(1.,0.,0.));
#122962=DIRECTION('center_axis',(0.,0.,-1.));
#122963=DIRECTION('ref_axis',(-1.,0.,0.));
#122964=DIRECTION('center_axis',(-0.907160802328708,0.420784123652894,0.));
#122965=DIRECTION('ref_axis',(-0.420784123652894,-0.907160802328709,0.));
#122966=DIRECTION('',(0.,0.,1.));
#122967=DIRECTION('center_axis',(0.907158740846047,-0.42078856793096,2.28597552685862E-6));
#122968=DIRECTION('ref_axis',(0.398329828560756,0.858742727554402,0.322326349452206));
#122969=DIRECTION('',(0.,0.,-1.));
#122970=DIRECTION('center_axis',(0.845904345266855,0.533334640407553,0.));
#122971=DIRECTION('ref_axis',(-0.533334640407553,0.845904345266855,0.));
#122972=DIRECTION('center_axis',(-0.845904345266892,-0.533334640407494,
-3.18298171959134E-14));
#122973=DIRECTION('ref_axis',(0.532618548224074,-0.844768575257462,0.0518028603955189));
#122974=DIRECTION('',(0.,0.,1.));
#122975=DIRECTION('',(0.,0.,1.));
#122976=DIRECTION('center_axis',(0.,0.,1.));
#122977=DIRECTION('ref_axis',(-0.997945392750336,-0.0640702199807127,0.));
#122978=DIRECTION('center_axis',(0.,0.,-1.));
#122979=DIRECTION('ref_axis',(0.997945392750336,0.0640702199807127,0.));
#122980=DIRECTION('center_axis',(0.955852314850978,-0.175249125470207,-0.235868811452373));
#122981=DIRECTION('ref_axis',(0.290355212971756,0.686675546312613,0.666461209971294));
#122982=DIRECTION('center_axis',(0.925594419806159,0.296042013585558,0.235868811452273));
#122983=DIRECTION('ref_axis',(0.375781520550134,-0.643908149093292,-0.66646120993219));
#122984=DIRECTION('center_axis',(0.,0.,-1.));
#122985=DIRECTION('ref_axis',(0.997945392750336,0.0640702199807201,0.));
#122986=DIRECTION('center_axis',(-0.996931752839328,-0.0782756678713443,
-6.76296429840134E-17));
#122987=DIRECTION('ref_axis',(-0.0782756678713443,0.996931752839328,2.54222752659115E-32));
#122988=DIRECTION('center_axis',(0.,0.,1.));
#122989=DIRECTION('ref_axis',(-0.997945392750336,-0.0640702199807201,0.));
#122990=DIRECTION('center_axis',(-0.998756627165696,-0.0498517772261222,
-1.38914942345546E-16));
#122991=DIRECTION('ref_axis',(0.0498517772261222,-0.998756627165696,5.39260384428426E-32));
#122992=DIRECTION('center_axis',(0.,0.,-1.));
#122993=DIRECTION('ref_axis',(0.997945392750335,0.0640702199807342,0.));
#122994=DIRECTION('center_axis',(0.,0.,1.));
#122995=DIRECTION('ref_axis',(-0.997945392750335,-0.0640702199807344,0.));
#122996=DIRECTION('center_axis',(0.,0.,1.));
#122997=DIRECTION('ref_axis',(-0.997945392750335,-0.0640702199807344,0.));
#122998=DIRECTION('center_axis',(-0.398961016913283,0.632778807581561,0.663642288932205));
#122999=DIRECTION('ref_axis',(-0.0455303946146904,0.709172647596825,-0.703563173472532));
#123000=DIRECTION('center_axis',(-0.400108460798375,0.634598730187015,0.661209249211309));
#123001=DIRECTION('ref_axis',(-0.0453826414436742,0.706871272693762,-0.705884848750769));
#123002=DIRECTION('center_axis',(-0.3156728914411,-0.680553417717253,-0.661209249211308));
#123003=DIRECTION('ref_axis',(0.0453826414436472,-0.706871272693764,0.705884848750769));
#123004=DIRECTION('center_axis',(-0.314767594591723,-0.67860170478403,-0.663642288932184));
#123005=DIRECTION('ref_axis',(0.0455303946146966,-0.709172647596804,0.703563173472552));
#123006=DIRECTION('center_axis',(0.,0.,1.));
#123007=DIRECTION('ref_axis',(-0.997945392750335,-0.0640702199807344,0.));
#123008=DIRECTION('center_axis',(0.,0.,1.));
#123009=DIRECTION('ref_axis',(-0.997945392750335,-0.0640702199807344,0.));
#123010=DIRECTION('center_axis',(0.,0.,1.));
#123011=DIRECTION('ref_axis',(0.997945392750335,0.0640702199807343,0.));
#123012=DIRECTION('center_axis',(0.,0.,-1.));
#123013=DIRECTION('ref_axis',(-0.997945392750336,-0.0640702199807201,0.));
#123014=DIRECTION('center_axis',(-0.932256674534466,0.361797585378813,0.));
#123015=DIRECTION('ref_axis',(-0.361797585378813,-0.932256674534466,0.));
#123016=DIRECTION('',(0.,0.,1.));
#123017=DIRECTION('center_axis',(0.93225490203322,-0.361802152605269,2.28597552739037E-6));
#123018=DIRECTION('ref_axis',(0.342491581739211,0.882499428244109,0.322326349507133));
#123019=DIRECTION('',(0.,0.,-1.));
#123020=DIRECTION('center_axis',(0.809995476332301,0.586436124672763,0.));
#123021=DIRECTION('ref_axis',(-0.586436124672763,0.809995476332301,0.));
#123022=DIRECTION('center_axis',(-0.809995476332275,-0.586436124672799,
3.11089989280751E-14));
#123023=DIRECTION('ref_axis',(0.585648734744481,-0.808907920069597,0.0518028603541021));
#123024=DIRECTION('',(0.,0.,1.));
#123025=DIRECTION('',(0.,0.,1.));
#123026=DIRECTION('center_axis',(0.,0.,1.));
#123027=DIRECTION('ref_axis',(-0.991790013823243,-0.127877161684531,0.));
#123028=DIRECTION('center_axis',(0.,0.,-1.));
#123029=DIRECTION('ref_axis',(0.991790013823243,0.127877161684531,0.));
#123030=DIRECTION('center_axis',(0.965116663775579,-0.113647389264971,-0.235868811452367));
#123031=DIRECTION('ref_axis',(0.245763193736745,0.703867820139019,0.666461209956784));
#123032=DIRECTION('center_axis',(0.904725209867048,0.354736801608014,0.235868811452345));
#123033=DIRECTION('ref_axis',(0.416264773870607,-0.618508766033597,-0.666461209954525));
#123034=DIRECTION('center_axis',(0.,0.,-1.));
#123035=DIRECTION('ref_axis',(0.991790013823245,0.127877161684513,0.));
#123036=DIRECTION('center_axis',(-0.98986831037287,-0.141988478826837,-6.76296429840134E-17));
#123037=DIRECTION('ref_axis',(-0.141988478826837,0.98986831037287,8.0118685686509E-32));
#123038=DIRECTION('center_axis',(0.,0.,1.));
#123039=DIRECTION('ref_axis',(-0.991790013823245,-0.127877161684513,0.));
#123040=DIRECTION('center_axis',(-0.993510560225565,-0.113739908212926,
-1.38914942345546E-16));
#123041=DIRECTION('ref_axis',(0.113739908212926,-0.993510560225564,3.08148791101958E-32));
#123042=DIRECTION('center_axis',(0.,0.,-1.));
#123043=DIRECTION('ref_axis',(0.991790013823245,0.127877161684512,0.));
#123044=DIRECTION('center_axis',(0.,0.,1.));
#123045=DIRECTION('ref_axis',(-0.991790013823245,-0.127877161684512,0.));
#123046=DIRECTION('center_axis',(0.,0.,1.));
#123047=DIRECTION('ref_axis',(-0.991790013823245,-0.127877161684512,0.));
#123048=DIRECTION('center_axis',(-0.438683586116484,0.605917175538708,0.663642288932205));
#123049=DIRECTION('ref_axis',(-0.0908736950716741,0.704798433935035,-0.703563173472534));
#123050=DIRECTION('center_axis',(-0.43994527529673,0.607659841935849,0.661209249211309));
#123051=DIRECTION('ref_axis',(-0.0905787958790902,0.702511254031705,-0.705884848750768));
#123052=DIRECTION('center_axis',(-0.271421100448053,-0.699380379328006,
-0.661209249211308));
#123053=DIRECTION('ref_axis',(0.0905787958790646,-0.702511254031708,0.705884848750769));
#123054=DIRECTION('center_axis',(-0.270642710305116,-0.697374673830039,
-0.663642288932184));
#123055=DIRECTION('ref_axis',(0.0908736950716735,-0.704798433935017,0.703563173472552));
#123056=DIRECTION('center_axis',(0.,0.,1.));
#123057=DIRECTION('ref_axis',(-0.991790013823245,-0.127877161684512,0.));
#123058=DIRECTION('center_axis',(0.,0.,1.));
#123059=DIRECTION('ref_axis',(-0.991790013823245,-0.127877161684512,0.));
#123060=DIRECTION('center_axis',(0.,0.,1.));
#123061=DIRECTION('ref_axis',(0.991790013823245,0.127877161684511,0.));
#123062=DIRECTION('center_axis',(0.,0.,-1.));
#123063=DIRECTION('ref_axis',(-0.991790013823245,-0.127877161684513,0.));
#123064=DIRECTION('center_axis',(-0.953521704096131,0.301324343221071,0.));
#123065=DIRECTION('ref_axis',(-0.301324343221071,-0.953521704096131,0.));
#123066=DIRECTION('',(0.,0.,1.));
#123067=DIRECTION('center_axis',(0.953520227859841,-0.301329014628347,2.28597558455223E-6));
#123068=DIRECTION('ref_axis',(0.285245963537521,0.902629749458501,0.322326349648977));
#123069=DIRECTION('',(0.,0.,-1.));
#123070=DIRECTION('center_axis',(0.770758162242013,0.637127817111539,0.));
#123071=DIRECTION('ref_axis',(-0.637127817111539,0.770758162242013,0.));
#123072=DIRECTION('center_axis',(-0.770758162242,-0.637127817111555,-4.55253642849831E-16));
#123073=DIRECTION('ref_axis',(0.636272364988702,-0.769723288723081,0.0518028604326862));
#123074=DIRECTION('',(0.,0.,1.));
#123075=DIRECTION('',(0.,0.,1.));
#123076=DIRECTION('center_axis',(0.,0.,1.));
#123077=DIRECTION('ref_axis',(-0.981559156991069,-0.191158628701354,0.));
#123078=DIRECTION('center_axis',(0.,0.,-1.));
#123079=DIRECTION('ref_axis',(0.981559156991069,0.191158628701354,0.));
#123080=DIRECTION('center_axis',(0.970415141311862,-0.0515786515600848,
-0.235868811452304));
#123081=DIRECTION('ref_axis',(0.200161280820835,0.718167750113079,0.666461209942244));
#123082=DIRECTION('center_axis',(0.880138289977647,0.411973900021917,0.235868811452373));
#123083=DIRECTION('ref_axis',(0.4550375059517,-0.590567797824916,-0.666461209936097));
#123084=DIRECTION('center_axis',(0.,0.,-1.));
#123085=DIRECTION('ref_axis',(0.981559156991064,0.19115862870138,0.));
#123086=DIRECTION('center_axis',(-0.978737286693004,-0.205117828666397,
-6.76296429840134E-17));
#123087=DIRECTION('ref_axis',(-0.205117828666397,0.978737286693004,-1.34044724129352E-31));
#123088=DIRECTION('center_axis',(0.,0.,1.));
#123089=DIRECTION('ref_axis',(-0.981559156991064,-0.19115862870138,0.));
#123090=DIRECTION('center_axis',(-0.98418194528612,-0.177160657519749,-1.38914942345546E-16));
#123091=DIRECTION('ref_axis',(0.177160657519749,-0.984181945286119,1.54074395550979E-31));
#123092=DIRECTION('center_axis',(0.,0.,-1.));
#123093=DIRECTION('ref_axis',(0.981559156991067,0.191158628701365,0.));
#123094=DIRECTION('center_axis',(0.,0.,1.));
#123095=DIRECTION('ref_axis',(-0.981559156991067,-0.191158628701365,0.));
#123096=DIRECTION('center_axis',(0.,0.,1.));
#123097=DIRECTION('ref_axis',(-0.981559156991067,-0.191158628701365,0.));
#123098=DIRECTION('center_axis',(-0.476603510366998,0.576565699852739,0.663642288932205));
#123099=DIRECTION('ref_axis',(-0.13584357602325,0.697528052329421,-0.703563173472532));
#123100=DIRECTION('center_axis',(-0.477974260290926,0.578223949051541,0.661209249211309));
#123101=DIRECTION('ref_axis',(-0.135402742613152,0.695264465938639,-0.705884848750769));
#123102=DIRECTION('center_axis',(-0.22605398193362,-0.715333436943481,-0.661209249211308));
#123103=DIRECTION('ref_axis',(0.135402742613124,-0.695264465938644,0.705884848750769));
#123104=DIRECTION('center_axis',(-0.225405697069186,-0.713281980754881,
-0.663642288932184));
#123105=DIRECTION('ref_axis',(0.135843576023254,-0.6975280523294,0.703563173472552));
#123106=DIRECTION('center_axis',(0.,0.,1.));
#123107=DIRECTION('ref_axis',(-0.981559156991067,-0.191158628701366,0.));
#123108=DIRECTION('center_axis',(0.,0.,1.));
#123109=DIRECTION('ref_axis',(-0.981559156991067,-0.191158628701366,0.));
#123110=DIRECTION('center_axis',(0.,0.,1.));
#123111=DIRECTION('ref_axis',(0.981559156991053,0.191158628701435,0.));
#123112=DIRECTION('center_axis',(0.,0.,-1.));
#123113=DIRECTION('ref_axis',(-0.981559156991064,-0.19115862870138,0.));
#123114=DIRECTION('center_axis',(-0.970868508445902,0.239612894703166,0.));
#123115=DIRECTION('ref_axis',(-0.239612894703166,-0.970868508445902,0.));
#123116=DIRECTION('',(0.,0.,1.));
#123117=DIRECTION('center_axis',(0.970867334540797,-0.239617651095285,2.28597557668383E-6));
#123118=DIRECTION('ref_axis',(0.226828208517194,0.919050971517716,0.322326349486391));
#123119=DIRECTION('',(0.,0.,-1.));
#123120=DIRECTION('center_axis',(0.728353637535965,0.685201414686315,0.));
#123121=DIRECTION('ref_axis',(-0.685201414686315,0.728353637535965,0.));
#123122=DIRECTION('center_axis',(-0.72835363753595,-0.685201414686332,1.04328959819753E-14));
#123123=DIRECTION('ref_axis',(0.684281415609948,-0.72737569928385,0.051802860366741));
#123124=DIRECTION('',(0.,0.,1.));
#123125=DIRECTION('',(0.,0.,1.));
#123126=DIRECTION('center_axis',(0.,0.,1.));
#123127=DIRECTION('ref_axis',(-0.967294863039035,-0.253654583909488,0.));
#123128=DIRECTION('center_axis',(0.,0.,-1.));
#123129=DIRECTION('ref_axis',(0.967294863039035,0.253654583909488,0.));
#123130=DIRECTION('center_axis',(0.971725974879087,0.0107020338879415,-0.235868811452361));
#123131=DIRECTION('ref_axis',(0.153736862271298,0.729516574733416,0.666461209950137));
#123132=DIRECTION('center_axis',(0.851934693065624,0.467518109312609,0.235868811452351));
#123133=DIRECTION('ref_axis',(0.49194039131042,-0.560200059829388,-0.666461209947361));
#123134=DIRECTION('center_axis',(0.,0.,-1.));
#123135=DIRECTION('ref_axis',(0.967294863039027,0.253654583909515,0.));
#123136=DIRECTION('center_axis',(-0.963584421563626,-0.267404305350331,
-6.76296429840134E-17));
#123137=DIRECTION('ref_axis',(-0.267404305350331,0.963584421563625,6.93889390390731E-14));
#123138=DIRECTION('center_axis',(0.,0.,1.));
#123139=DIRECTION('ref_axis',(-0.967294863039027,-0.253654583909515,0.));
#123140=DIRECTION('center_axis',(-0.970809115627128,-0.239853415683982,
-1.38914942345546E-16));
#123141=DIRECTION('ref_axis',(0.239853415683982,-0.970809115627128,-2.46519032881566E-32));
#123142=DIRECTION('center_axis',(0.,0.,-1.));
#123143=DIRECTION('ref_axis',(0.967294863039023,0.25365458390953,0.));
#123144=DIRECTION('center_axis',(0.,0.,1.));
#123145=DIRECTION('ref_axis',(-0.967294863039023,-0.25365458390953,0.));
#123146=DIRECTION('center_axis',(0.,0.,1.));
#123147=DIRECTION('ref_axis',(-0.967294863039023,-0.25365458390953,0.));
#123148=DIRECTION('center_axis',(-0.512564968562282,0.54484499203312,0.663642288932205));
#123149=DIRECTION('ref_axis',(-0.180255246582595,0.687391378337486,-0.703563173472532));
#123150=DIRECTION('center_axis',(-0.514039146524428,0.546412009931933,0.661209249211309));
#123151=DIRECTION('ref_axis',(-0.17967029043401,0.685160687021275,-0.705884848750767));
#123152=DIRECTION('center_axis',(-0.179757959118996,-0.728347036028013,
-0.661209249211308));
#123153=DIRECTION('ref_axis',(0.179670290433992,-0.685160687021278,0.705884848750768));
#123154=DIRECTION('center_axis',(-0.179242443474628,-0.726258259022296,
-0.663642288932184));
#123155=DIRECTION('ref_axis',(0.180255246582597,-0.687391378337463,0.703563173472553));
#123156=DIRECTION('center_axis',(0.,0.,1.));
#123157=DIRECTION('ref_axis',(-0.967294863039023,-0.25365458390953,0.));
#123158=DIRECTION('center_axis',(0.,0.,1.));
#123159=DIRECTION('ref_axis',(-0.967294863039023,-0.25365458390953,0.));
#123160=DIRECTION('center_axis',(0.,0.,1.));
#123161=DIRECTION('ref_axis',(0.967294863039023,0.25365458390953,0.));
#123162=DIRECTION('center_axis',(0.,0.,-1.));
#123163=DIRECTION('ref_axis',(-0.967294863039028,-0.253654583909515,0.));
#123164=DIRECTION('center_axis',(-0.984225805843826,0.17691682540412,0.));
#123165=DIRECTION('ref_axis',(-0.17691682540412,-0.984225805843826,0.));
#123166=DIRECTION('',(0.,0.,1.));
#123167=DIRECTION('center_axis',(0.984224939093727,-0.176921647236071,2.28597557197196E-6));
#123168=DIRECTION('ref_axis',(0.16747836771619,0.931695615942342,0.322326349498364));
#123169=DIRECTION('',(0.,0.,-1.));
#123170=DIRECTION('center_axis',(0.682956151501917,0.730459372672903,0.));
#123171=DIRECTION('ref_axis',(-0.730459372672903,0.682956151501917,0.));
#123172=DIRECTION('center_axis',(-0.682956151501931,-0.73045937267289,-5.27335469634203E-15));
#123173=DIRECTION('ref_axis',(0.729478607109897,-0.682039167067909,0.0518028604839242));
#123174=DIRECTION('',(0.,0.,1.));
#123175=DIRECTION('',(0.,0.,1.));
#123176=DIRECTION('center_axis',(0.,0.,1.));
#123177=DIRECTION('ref_axis',(-0.949055747010657,-0.315108218023656,0.));
#123178=DIRECTION('center_axis',(0.,0.,-1.));
#123179=DIRECTION('ref_axis',(0.949055747010657,0.315108218023656,0.));
#123180=DIRECTION('center_axis',(0.969043777980998,0.0729387423828591,-0.235868811452303));
#123181=DIRECTION('ref_axis',(0.106680705979194,0.737867659268036,0.666461209957557));
#123182=DIRECTION('center_axis',(0.820230313760368,0.521141186409817,0.235868811452335));
#123183=DIRECTION('ref_axis',(0.526821788084768,-0.527530339643292,-0.666461209940235));
#123184=DIRECTION('center_axis',(0.,0.,-1.));
#123185=DIRECTION('ref_axis',(0.949055747010666,0.315108218023628,0.));
#123186=DIRECTION('center_axis',(-0.944471981357833,-0.328591960385537,
-6.76296429840134E-17));
#123187=DIRECTION('ref_axis',(-0.328591960385537,0.944471981357833,6.93889390390723E-14));
#123188=DIRECTION('center_axis',(0.,0.,1.));
#123189=DIRECTION('ref_axis',(-0.949055747010666,-0.315108218023628,0.));
#123190=DIRECTION('center_axis',(-0.953447023074123,-0.301560564714772,
-1.38914942345546E-16));
#123191=DIRECTION('ref_axis',(0.301560564714772,-0.953447023074123,-1.10317267214501E-30));
#123192=DIRECTION('center_axis',(0.,0.,-1.));
#123193=DIRECTION('ref_axis',(0.949055747010662,0.315108218023641,0.));
#123194=DIRECTION('center_axis',(0.,0.,1.));
#123195=DIRECTION('ref_axis',(-0.949055747010662,-0.315108218023641,0.));
#123196=DIRECTION('center_axis',(0.,0.,1.));
#123197=DIRECTION('ref_axis',(-0.949055747010662,-0.315108218023641,0.));
#123198=DIRECTION('center_axis',(-0.546420187356902,0.510885399272354,0.663642288932205));
#123199=DIRECTION('ref_axis',(-0.223926209669107,0.674430065726971,-0.703563173472533));
#123200=DIRECTION('center_axis',(-0.547991735643811,0.512354746658505,0.661209249211309));
#123201=DIRECTION('ref_axis',(-0.223199534492319,0.672241435874434,-0.705884848750766));
#123202=DIRECTION('center_axis',(-0.13272327229239,-0.738367700911557,-0.661209249211308));
#123203=DIRECTION('ref_axis',(0.223199534492305,-0.672241435874436,0.705884848750769));
#123204=DIRECTION('center_axis',(-0.13234264423245,-0.736250186321481,-0.663642288932184));
#123205=DIRECTION('ref_axis',(0.223926209669108,-0.67443006572695,0.703563173472552));
#123206=DIRECTION('center_axis',(0.,0.,1.));
#123207=DIRECTION('ref_axis',(-0.949055747010662,-0.315108218023641,0.));
#123208=DIRECTION('center_axis',(0.,0.,1.));
#123209=DIRECTION('ref_axis',(-0.949055747010662,-0.315108218023641,0.));
#123210=DIRECTION('center_axis',(0.,0.,1.));
#123211=DIRECTION('ref_axis',(0.94905574701065,0.315108218023678,0.));
#123212=DIRECTION('center_axis',(0.,0.,-1.));
#123213=DIRECTION('ref_axis',(-0.949055747010666,-0.315108218023628,0.));
#123214=DIRECTION('center_axis',(-0.993538708289764,0.113493766920949,0.));
#123215=DIRECTION('ref_axis',(-0.113493766920949,-0.993538708289764,0.));
#123216=DIRECTION('',(0.,0.,1.));
#123217=DIRECTION('center_axis',(0.993538152256336,-0.113498634378743,2.28597554183348E-6));
#123218=DIRECTION('ref_axis',(0.107440322381736,0.940511723259278,0.32232634943233));
#123219=DIRECTION('',(0.,0.,-1.));
#123220=DIRECTION('center_axis',(0.634752252147712,0.772715716414133,0.));
#123221=DIRECTION('ref_axis',(-0.772715716414133,0.634752252147712,0.));
#123222=DIRECTION('center_axis',(-0.634752252147764,-0.772715716414091,
-4.12383924814779E-14));
#123223=DIRECTION('ref_axis',(0.771678214548363,-0.633899989624967,0.0518028603931937));
#123224=DIRECTION('',(0.,0.,1.));
#123225=DIRECTION('',(0.,0.,1.));
#123226=DIRECTION('center_axis',(0.,0.,1.));
#123227=DIRECTION('ref_axis',(-0.926916757346018,-0.375267004879383,0.));
#123228=DIRECTION('center_axis',(0.,0.,-1.));
#123229=DIRECTION('ref_axis',(0.926916757346018,0.375267004879383,0.));
#123230=DIRECTION('center_axis',(0.962379572339892,0.134875729940326,-0.235868811452366));
#123231=DIRECTION('ref_axis',(0.0591861757799709,0.743186687328967,0.666461209954142));
#123232=DIRECTION('center_axis',(0.785155432156967,0.572622782587701,0.235868811452306));
#123233=DIRECTION('ref_axis',(0.559538361127139,-0.492692884129657,-0.66646120994035));
#123234=DIRECTION('center_axis',(0.,0.,-1.));
#123235=DIRECTION('ref_axis',(0.926916757346019,0.375267004879382,0.));
#123236=DIRECTION('center_axis',(-0.921478503192035,-0.388429360572764,
-6.76296429840134E-17));
#123237=DIRECTION('ref_axis',(-0.388429360572764,0.921478503192035,-6.44030973403092E-31));
#123238=DIRECTION('center_axis',(0.,0.,1.));
#123239=DIRECTION('ref_axis',(-0.926916757346019,-0.375267004879382,0.));
#123240=DIRECTION('center_axis',(-0.932167012189561,-0.362028536700612,
-1.38914942345546E-16));
#123241=DIRECTION('ref_axis',(0.362028536700612,-0.932167012189561,-2.83496887813801E-31));
#123242=DIRECTION('center_axis',(0.,0.,-1.));
#123243=DIRECTION('ref_axis',(0.92691675734602,0.375267004879378,0.));
#123244=DIRECTION('center_axis',(0.,0.,1.));
#123245=DIRECTION('ref_axis',(-0.92691675734602,-0.375267004879378,0.));
#123246=DIRECTION('center_axis',(0.,0.,1.));
#123247=DIRECTION('ref_axis',(-0.92691675734602,-0.375267004879378,0.));
#123248=DIRECTION('center_axis',(-0.57803004839491,0.474826468821402,0.663642288932205));
#123249=DIRECTION('ref_axis',(-0.266677011928071,0.658697375311585,-0.703563173472535));
#123250=DIRECTION('center_axis',(-0.579692509177574,0.476192107831309,0.661209249211309));
#123251=DIRECTION('ref_axis',(-0.265811603787261,0.656559800472242,-0.705884848750767));
#123252=DIRECTION('center_axis',(-0.0851431970708823,-0.74535425453268,
-0.661209249211308));
#123253=DIRECTION('ref_axis',(0.265811603787243,-0.656559800472249,0.705884848750768));
#123254=DIRECTION('center_axis',(-0.0848990206777118,-0.743216703679901,
-0.663642288932184));
#123255=DIRECTION('ref_axis',(0.266677011928059,-0.65869737531157,0.703563173472554));
#123256=DIRECTION('center_axis',(0.,0.,1.));
#123257=DIRECTION('ref_axis',(-0.926916757346019,-0.375267004879381,0.));
#123258=DIRECTION('center_axis',(0.,0.,1.));
#123259=DIRECTION('ref_axis',(-0.926916757346019,-0.375267004879381,0.));
#123260=DIRECTION('center_axis',(0.,0.,1.));
#123261=DIRECTION('ref_axis',(0.926916757346035,0.375267004879342,0.));
#123262=DIRECTION('center_axis',(0.,0.,-1.));
#123263=DIRECTION('ref_axis',(-0.926916757346019,-0.375267004879382,0.));
#123264=DIRECTION('center_axis',(-0.998768947069956,0.0496043382051624,
0.));
#123265=DIRECTION('ref_axis',(-0.0496043382051624,-0.998768947069956,0.));
#123266=DIRECTION('',(0.,0.,1.));
#123267=DIRECTION('center_axis',(0.998768704038046,-0.0496092312874968,
2.28597557253148E-6));
#123268=DIRECTION('ref_axis',(0.0469607817114965,0.94546306611664,0.322326349512986));
#123269=DIRECTION('',(0.,0.,-1.));
#123270=DIRECTION('center_axis',(0.583940019635501,0.811796805529617,0.));
#123271=DIRECTION('ref_axis',(-0.811796805529617,0.583940019635501,0.));
#123272=DIRECTION('center_axis',(-0.583940019635481,-0.811796805529632,
5.69067053562094E-16));
#123273=DIRECTION('ref_axis',(0.810706830675423,-0.583155981150193,0.0518028603936798));
#123274=DIRECTION('',(0.,0.,1.));
#123275=DIRECTION('',(0.,0.,1.));
#123276=DIRECTION('center_axis',(0.,0.,1.));
#123277=DIRECTION('ref_axis',(-0.900968867902417,-0.433883739117562,0.));
#123278=DIRECTION('center_axis',(0.,0.,-1.));
#123279=DIRECTION('ref_axis',(0.900968867902417,0.433883739117562,0.));
#123280=DIRECTION('center_axis',(0.951760742606333,0.196258484192423,-0.235868811452327));
#123281=DIRECTION('ref_axis',(0.0114484368867947,0.745451801882648,0.666461209946058));
#123282=DIRECTION('center_axis',(0.746854178467675,0.621751348924495,0.235868811452354));
#123283=DIRECTION('ref_axis',(0.589955671020197,-0.455830847867314,-0.666461209946742));
#123284=DIRECTION('center_axis',(0.,0.,-1.));
#123285=DIRECTION('ref_axis',(0.900968867902415,0.433883739117566,0.));
#123286=DIRECTION('center_axis',(-0.894698472200103,-0.446670621199561,
-6.76296429840134E-17));
#123287=DIRECTION('ref_axis',(-0.446670621199561,0.894698472200103,1.23259516440783E-31));
#123288=DIRECTION('center_axis',(0.,0.,1.));
#123289=DIRECTION('ref_axis',(-0.900968867902415,-0.433883739117566,0.));
#123290=DIRECTION('center_axis',(-0.907056527102715,-0.421008855774271,
-1.38914942345546E-16));
#123291=DIRECTION('ref_axis',(0.421008855774271,-0.907056527102715,-2.58844984525645E-31));
#123292=DIRECTION('center_axis',(0.,0.,-1.));
#123293=DIRECTION('ref_axis',(0.900968867902412,0.433883739117574,0.));
#123294=DIRECTION('center_axis',(0.,0.,1.));
#123295=DIRECTION('ref_axis',(-0.900968867902412,-0.433883739117574,0.));
#123296=DIRECTION('center_axis',(0.,0.,1.));
#123297=DIRECTION('ref_axis',(-0.900968867902412,-0.433883739117574,0.));
#123298=DIRECTION('center_axis',(-0.607264659977007,0.436816374560105,0.663642288932205));
#123299=DIRECTION('ref_axis',(-0.308331981142968,0.640257956090913,-0.703563173472532));
#123300=DIRECTION('center_axis',(-0.609011201847474,0.438072693490148,0.661209249211309));
#123301=DIRECTION('ref_axis',(-0.307331396185831,0.638180220018272,-0.70588484875077));
#123302=DIRECTION('center_axis',(-0.0372132501894517,-0.749277987643942,
-0.661209249211308));
#123303=DIRECTION('ref_axis',(0.307331396185812,-0.638180220018285,0.705884848750767));
#123304=DIRECTION('center_axis',(-0.0371065288362263,-0.747129184183417,
-0.663642288932184));
#123305=DIRECTION('ref_axis',(0.308331981142974,-0.640257956090888,0.703563173472551));
#123306=DIRECTION('center_axis',(0.,0.,1.));
#123307=DIRECTION('ref_axis',(-0.900968867902412,-0.433883739117574,0.));
#123308=DIRECTION('center_axis',(0.,0.,1.));
#123309=DIRECTION('ref_axis',(-0.900968867902412,-0.433883739117574,0.));
#123310=DIRECTION('center_axis',(0.,0.,1.));
#123311=DIRECTION('ref_axis',(0.900968867902445,0.433883739117504,0.));
#123312=DIRECTION('center_axis',(0.,0.,-1.));
#123313=DIRECTION('ref_axis',(-0.900968867902415,-0.433883739117566,0.));
#123314=DIRECTION('center_axis',(-0.999895030011369,-0.0144889253764059,
0.));
#123315=DIRECTION('ref_axis',(0.0144889253764059,-0.999895030011369,0.));
#123316=DIRECTION('',(0.,0.,1.));
#123317=DIRECTION('center_axis',(0.999895100979656,0.0144840267763789,2.28597555049375E-6));
#123318=DIRECTION('ref_axis',(0.0137117308809598,-0.946529298470156,-0.322326349487352));
#123319=DIRECTION('',(0.,0.,-1.));
#123320=DIRECTION('center_axis',(0.530728252327867,0.84754204744131,0.));
#123321=DIRECTION('ref_axis',(-0.84754204744131,0.530728252327867,0.));
#123322=DIRECTION('center_axis',(-0.530728252327927,-0.847542047441273,
-2.31041223746203E-14));
#123323=DIRECTION('ref_axis',(0.846404078535633,-0.530015659660323,0.0518028604719626));
#123324=DIRECTION('',(0.,0.,1.));
#123325=DIRECTION('',(0.,0.,1.));
#123326=DIRECTION('center_axis',(0.,0.,1.));
#123327=DIRECTION('ref_axis',(-0.871318704123379,-0.490717552003956,0.));
#123328=DIRECTION('center_axis',(0.,0.,-1.));
#123329=DIRECTION('ref_axis',(0.871318704123379,0.490717552003956,0.));
#123330=DIRECTION('center_axis',(0.937230923829337,0.256834770235804,-0.235868811452317));
#123331=DIRECTION('ref_axis',(-0.0363363460864612,0.7446536950763,0.666461209945708));
#123332=DIRECTION('center_axis',(0.705483940759196,0.668325005603523,0.235868811452313));
#123333=DIRECTION('ref_axis',(0.61794872652725,-0.417095704897173,-0.666461209928741));
#123334=DIRECTION('center_axis',(0.,0.,-1.));
#123335=DIRECTION('ref_axis',(0.871318704123385,0.490717552003945,0.));
#123336=DIRECTION('center_axis',(-0.86424193327368,-0.503076416433301,-6.76296429840134E-17));
#123337=DIRECTION('ref_axis',(-0.503076416433301,0.86424193327368,6.93889390390714E-14));
#123338=DIRECTION('center_axis',(0.,0.,1.));
#123339=DIRECTION('ref_axis',(-0.871318704123385,-0.490717552003945,0.));
#123340=DIRECTION('center_axis',(-0.87821875218299,-0.478259159153437,-1.38914942345546E-16));
#123341=DIRECTION('ref_axis',(0.478259159153437,-0.87821875218299,6.5327543713615E-31));
#123342=DIRECTION('center_axis',(0.,0.,-1.));
#123343=DIRECTION('ref_axis',(0.871318704123391,0.490717552003934,0.));
#123344=DIRECTION('center_axis',(0.,0.,1.));
#123345=DIRECTION('ref_axis',(-0.871318704123391,-0.490717552003934,0.));
#123346=DIRECTION('center_axis',(0.,0.,1.));
#123347=DIRECTION('ref_axis',(-0.871318704123391,-0.490717552003934,0.));
#123348=DIRECTION('center_axis',(-0.634003890813397,0.397011308118922,0.663642288932205));
#123349=DIRECTION('ref_axis',(-0.348719948110368,0.619187579593742,-0.703563173472536));
#123350=DIRECTION('center_axis',(-0.635827336856489,0.398153144485137,0.661209249211309));
#123351=DIRECTION('ref_axis',(-0.34758829795508,0.617178220151034,-0.705884848750766));
#123352=DIRECTION('center_axis',(0.0108696139192246,-0.750122776784351,
-0.661209249211308));
#123353=DIRECTION('ref_axis',(0.347588297955064,-0.61717822015104,0.705884848750769));
#123354=DIRECTION('center_axis',(0.0108384416915727,-0.747971550610416,
-0.663642288932184));
#123355=DIRECTION('ref_axis',(0.34871994811035,-0.619187579593732,0.703563173472553));
#123356=DIRECTION('center_axis',(0.,0.,1.));
#123357=DIRECTION('ref_axis',(-0.871318704123391,-0.490717552003934,0.));
#123358=DIRECTION('center_axis',(0.,0.,1.));
#123359=DIRECTION('ref_axis',(-0.871318704123391,-0.490717552003934,0.));
#123360=DIRECTION('center_axis',(0.,0.,1.));
#123361=DIRECTION('ref_axis',(0.871318704123396,0.490717552003927,0.));
#123362=DIRECTION('center_axis',(0.,0.,-1.));
#123363=DIRECTION('ref_axis',(-0.871318704123385,-0.490717552003945,0.));
#123364=DIRECTION('center_axis',(-0.996912329797655,-0.0785226508557379,
0.));
#123365=DIRECTION('ref_axis',(0.0785226508557379,-0.996912329797655,0.));
#123366=DIRECTION('',(0.,0.,1.));
#123367=DIRECTION('center_axis',(0.996912714474511,0.0785177668673503,2.28597555777743E-6));
#123368=DIRECTION('ref_axis',(0.0743278990288261,-0.943706038877036,-0.322326349548056));
#123369=DIRECTION('',(0.,0.,-1.));
#123370=DIRECTION('center_axis',(0.475335608790564,0.879804557282868,0.));
#123371=DIRECTION('ref_axis',(-0.879804557282868,0.475335608790564,0.));
#123372=DIRECTION('center_axis',(-0.475335608790582,-0.879804557282858,
-1.09640252319663E-14));
#123373=DIRECTION('ref_axis',(0.878623270489444,-0.474697390140252,0.0518028604274629));
#123374=DIRECTION('',(0.,0.,1.));
#123375=DIRECTION('',(0.,0.,1.));
#123376=DIRECTION('center_axis',(0.,0.,1.));
#123377=DIRECTION('ref_axis',(-0.838088104891841,-0.545534901210548,0.));
#123378=DIRECTION('center_axis',(0.,0.,-1.));
#123379=DIRECTION('ref_axis',(0.838088104891841,0.545534901210548,0.));
#123380=DIRECTION('center_axis',(0.918849822150947,0.316355667117322,-0.235868811452313));
#123381=DIRECTION('ref_axis',(-0.0839718152198296,0.740795646509661,0.66646120994475));
#123382=DIRECTION('center_axis',(0.661214718212255,0.712152371479303,0.235868811452242));
#123383=DIRECTION('ref_axis',(0.643402498157302,-0.376646626189073,-0.66646120993298));
#123384=DIRECTION('center_axis',(0.,0.,-1.));
#123385=DIRECTION('ref_axis',(0.838088104891836,0.545534901210556,0.));
#123386=DIRECTION('center_axis',(-0.830234038864122,-0.557414962762364,
-6.76296429840134E-17));
#123387=DIRECTION('ref_axis',(-0.557414962762364,0.830234038864122,4.00593428432545E-31));
#123388=DIRECTION('center_axis',(0.,0.,1.));
#123389=DIRECTION('ref_axis',(-0.838088104891836,-0.545534901210556,0.));
#123390=DIRECTION('center_axis',(-0.845772188033212,-0.533544193061374,
-1.38914942345546E-16));
#123391=DIRECTION('ref_axis',(0.533544193061374,-0.845772188033212,7.88860905221012E-31));
#123392=DIRECTION('center_axis',(0.,0.,-1.));
#123393=DIRECTION('ref_axis',(0.83808810489183,0.545534901210566,0.));
#123394=DIRECTION('center_axis',(0.,0.,1.));
#123395=DIRECTION('ref_axis',(-0.83808810489183,-0.545534901210566,0.));
#123396=DIRECTION('center_axis',(0.,0.,1.));
#123397=DIRECTION('ref_axis',(-0.83808810489183,-0.545534901210566,0.));
#123398=DIRECTION('center_axis',(-0.658137863669027,0.355574837054021,0.663642288932205));
#123399=DIRECTION('ref_axis',(-0.387674950010773,0.595572828516714,-0.703563173472536));
#123400=DIRECTION('center_axis',(-0.660030720953824,0.356597498805855,0.661209249211309));
#123401=DIRECTION('ref_axis',(-0.386416884850581,0.593640102592878,-0.705884848750765));
#123402=DIRECTION('center_axis',(0.0589078124527818,-0.747885150534122,
-0.661209249211308));
#123403=DIRECTION('ref_axis',(0.386416884850565,-0.593640102592882,0.70588484875077));
#123404=DIRECTION('center_axis',(0.0587388747376226,-0.745740341496563,
-0.663642288932184));
#123405=DIRECTION('ref_axis',(0.387674950010756,-0.595572828516704,0.703563173472553));
#123406=DIRECTION('center_axis',(0.,0.,1.));
#123407=DIRECTION('ref_axis',(-0.83808810489183,-0.545534901210566,0.));
#123408=DIRECTION('center_axis',(0.,0.,1.));
#123409=DIRECTION('ref_axis',(-0.83808810489183,-0.545534901210566,0.));
#123410=DIRECTION('center_axis',(0.,0.,1.));
#123411=DIRECTION('ref_axis',(0.838088104891825,0.545534901210574,0.));
#123412=DIRECTION('center_axis',(0.,0.,-1.));
#123413=DIRECTION('ref_axis',(-0.838088104891836,-0.545534901210556,0.));
#123414=DIRECTION('center_axis',(-0.989833102983778,-0.142233709919647,
0.));
#123415=DIRECTION('ref_axis',(0.142233709919647,-0.989833102983778,0.));
#123416=DIRECTION('',(0.,0.,1.));
#123417=DIRECTION('center_axis',(0.989833799788485,0.14222886061227,2.28597555000455E-6));
#123418=DIRECTION('ref_axis',(0.134638637897654,-0.937004888773812,-0.32232634952644));
#123419=DIRECTION('',(0.,0.,-1.));
#123420=DIRECTION('center_axis',(0.417989709277573,0.908451761481065,0.));
#123421=DIRECTION('ref_axis',(-0.908451761481065,0.417989709277573,0.));
#123422=DIRECTION('center_axis',(-0.41798970927758,-0.908451761481062,-2.56269863120773E-14));
#123423=DIRECTION('ref_axis',(0.907232010956192,-0.417428487219462,0.0518028604814085));
#123424=DIRECTION('',(0.,0.,1.));
#123425=DIRECTION('',(0.,0.,1.));
#123426=DIRECTION('center_axis',(0.,0.,1.));
#123427=DIRECTION('ref_axis',(-0.80141362186795,-0.598110530491225,0.));
#123428=DIRECTION('center_axis',(0.,0.,-1.));
#123429=DIRECTION('ref_axis',(0.80141362186795,0.598110530491225,0.));
#123430=DIRECTION('center_axis',(0.896692969460527,0.374576590704891,-0.235868811452391));
#123431=DIRECTION('ref_axis',(-0.13126222615057,0.73389350972817,0.666461209947634));
#123432=DIRECTION('center_axis',(0.614228422558169,0.75305335050433,0.23586881145227));
#123433=DIRECTION('ref_axis',(0.666212390916414,-0.334649825709052,-0.666461209930733));
#123434=DIRECTION('center_axis',(0.,0.,-1.));
#123435=DIRECTION('ref_axis',(0.801413621867952,0.598110530491223,0.));
#123436=DIRECTION('center_axis',(-0.792814534704229,-0.609462971444301,
-6.76296429840134E-17));
#123437=DIRECTION('ref_axis',(-0.609462971444301,0.792814534704229,4.62223186652937E-31));
#123438=DIRECTION('center_axis',(0.,0.,1.));
#123439=DIRECTION('ref_axis',(-0.801413621867952,-0.598110530491223,0.));
#123440=DIRECTION('center_axis',(-0.809850164545241,-0.586636779435151,
-1.38914942345546E-16));
#123441=DIRECTION('ref_axis',(0.586636779435151,-0.809850164545241,7.02579243712464E-31));
#123442=DIRECTION('center_axis',(0.,0.,-1.));
#123443=DIRECTION('ref_axis',(0.801413621867943,0.598110530491235,0.));
#123444=DIRECTION('center_axis',(0.,0.,1.));
#123445=DIRECTION('ref_axis',(-0.801413621867943,-0.598110530491235,0.));
#123446=DIRECTION('center_axis',(0.,0.,1.));
#123447=DIRECTION('ref_axis',(-0.801413621867943,-0.598110530491235,0.));
#123448=DIRECTION('center_axis',(-0.679567406872712,0.312677232713101,0.663642288932205));
#123449=DIRECTION('ref_axis',(-0.425036912385568,0.569510740937341,-0.703563173472535));
#123450=DIRECTION('center_axis',(-0.681521897242615,0.313576517514057,0.661209249211309));
#123451=DIRECTION('ref_axis',(-0.423657601880078,0.567662590517755,-0.705884848750767));
#123452=DIRECTION('center_axis',(0.106703946149284,-0.742574303779486,-0.661209249211308));
#123453=DIRECTION('ref_axis',(0.42365760188006,-0.567662590517765,0.705884848750769));
#123454=DIRECTION('center_axis',(0.106397937147926,-0.740444725358698,-0.663642288932184));
#123455=DIRECTION('ref_axis',(0.425036912385554,-0.569510740937329,0.703563173472553));
#123456=DIRECTION('center_axis',(0.,0.,1.));
#123457=DIRECTION('ref_axis',(-0.801413621867943,-0.598110530491235,0.));
#123458=DIRECTION('center_axis',(0.,0.,1.));
#123459=DIRECTION('ref_axis',(-0.801413621867943,-0.598110530491235,0.));
#123460=DIRECTION('center_axis',(0.,0.,1.));
#123461=DIRECTION('ref_axis',(0.801413621867959,0.598110530491212,0.));
#123462=DIRECTION('center_axis',(0.,0.,-1.));
#123463=DIRECTION('ref_axis',(-0.801413621867952,-0.598110530491223,0.));
#123464=DIRECTION('center_axis',(-0.978686439631205,-0.205360300160462,
0.));
#123465=DIRECTION('ref_axis',(0.205360300160462,-0.978686439631205,0.));
#123466=DIRECTION('',(0.,0.,1.));
#123467=DIRECTION('center_axis',(0.97868744570043,0.205355505460999,2.28597553472572E-6));
#123468=DIRECTION('ref_axis',(0.194396117719157,-0.926453384570327,-0.322326349580523));
#123469=DIRECTION('',(0.,0.,-1.));
#123470=DIRECTION('center_axis',(0.358926200390648,0.933365942529045,0.));
#123471=DIRECTION('ref_axis',(-0.933365942529045,0.358926200390648,0.));
#123472=DIRECTION('center_axis',(-0.358926200390652,-0.933365942529043,
-2.20798016782112E-14));
#123473=DIRECTION('ref_axis',(0.93211274049379,-0.358444281108687,0.0518028604387188));
#123474=DIRECTION('',(0.,0.,1.));
#123475=DIRECTION('',(0.,0.,1.));
#123476=DIRECTION('center_axis',(0.,0.,1.));
#123477=DIRECTION('ref_axis',(-0.761445958369139,-0.648228395307783,0.));
#123478=DIRECTION('center_axis',(0.,0.,-1.));
#123479=DIRECTION('ref_axis',(0.761445958369139,0.648228395307783,0.));
#123480=DIRECTION('center_axis',(0.870851413018736,0.431258298734448,-0.235868811452342));
#123481=DIRECTION('ref_axis',(-0.178013252430194,0.723975647086769,0.666461209962379));
#123482=DIRECTION('center_axis',(0.564718130564361,0.790859871782578,0.235868811452335));
#123483=DIRECTION('ref_axis',(0.686284674057369,-0.291277877310675,-0.6664612099315));
#123484=DIRECTION('center_axis',(0.,0.,-1.));
#123485=DIRECTION('ref_axis',(0.761445958369129,0.648228395307795,0.));
#123486=DIRECTION('center_axis',(-0.752137185563052,-0.659006566047177,
-6.76296429840134E-17));
#123487=DIRECTION('ref_axis',(-0.659006566047177,0.752137185563051,-3.88267476788467E-31));
#123488=DIRECTION('center_axis',(0.,0.,1.));
#123489=DIRECTION('ref_axis',(-0.761445958369129,-0.648228395307795,0.));
#123490=DIRECTION('center_axis',(-0.770600293018838,-0.637318749449034,
-1.38914942345546E-16));
#123491=DIRECTION('ref_axis',(0.637318749449034,-0.770600293018838,-1.84889274661175E-31));
#123492=DIRECTION('center_axis',(0.,0.,-1.));
#123493=DIRECTION('ref_axis',(0.761445958369123,0.648228395307802,0.));
#123494=DIRECTION('center_axis',(0.,0.,1.));
#123495=DIRECTION('ref_axis',(-0.761445958369123,-0.648228395307802,0.));
#123496=DIRECTION('center_axis',(0.,0.,1.));
#123497=DIRECTION('ref_axis',(-0.761445958369123,-0.648228395307802,0.));
#123498=DIRECTION('center_axis',(-0.698204461834805,0.268494770553906,0.663642288932205));
#123499=DIRECTION('ref_axis',(-0.460652306917231,0.541108411563796,-0.703563173472531));
#123500=DIRECTION('center_axis',(-0.700212553869647,0.269266983049841,0.661209249211309));
#123501=DIRECTION('ref_axis',(-0.45915741894918,0.539352431094948,-0.705884848750769));
#123502=DIRECTION('center_axis',(0.154061610443135,-0.734212059928932,-0.661209249211308));
#123503=DIRECTION('ref_axis',(0.459157418949166,-0.539352431094964,0.705884848750767));
#123504=DIRECTION('center_axis',(0.153619787612203,-0.732106463019439,-0.663642288932184));
#123505=DIRECTION('ref_axis',(0.46065230691723,-0.54110841156377,0.703563173472551));
#123506=DIRECTION('center_axis',(0.,0.,1.));
#123507=DIRECTION('ref_axis',(-0.761445958369123,-0.648228395307802,0.));
#123508=DIRECTION('center_axis',(0.,0.,1.));
#123509=DIRECTION('ref_axis',(-0.761445958369123,-0.648228395307802,0.));
#123510=DIRECTION('center_axis',(0.,0.,1.));
#123511=DIRECTION('ref_axis',(0.761445958369147,0.648228395307773,0.));
#123512=DIRECTION('center_axis',(0.,0.,-1.));
#123513=DIRECTION('ref_axis',(-0.761445958369129,-0.648228395307795,0.));
#123514=DIRECTION('center_axis',(-0.963518143770605,-0.267643020878272,
0.));
#123515=DIRECTION('ref_axis',(0.267643020878272,-0.963518143770605,0.));
#123516=DIRECTION('',(0.,0.,1.));
#123517=DIRECTION('center_axis',(0.963519454970197,0.267638300489127,2.28597552263965E-6));
#123518=DIRECTION('ref_axis',(0.253354782218402,-0.912094884778792,-0.322326349353304));
#123519=DIRECTION('',(0.,0.,-1.));
#123520=DIRECTION('center_axis',(0.29838778675689,0.954444722712806,0.));
#123521=DIRECTION('ref_axis',(-0.954444722712806,0.29838778675689,0.));
#123522=DIRECTION('center_axis',(-0.298387786756925,-0.954444722712795,
-1.55544994640349E-14));
#123523=DIRECTION('ref_axis',(0.953163218842664,-0.297987150560371,0.051802860407533));
#123524=DIRECTION('',(0.,0.,1.));
#123525=DIRECTION('',(0.,0.,1.));
#123526=DIRECTION('center_axis',(0.,0.,1.));
#123527=DIRECTION('ref_axis',(-0.718349350097714,-0.6956825506035,0.));
#123528=DIRECTION('center_axis',(0.,0.,-1.));
#123529=DIRECTION('ref_axis',(0.718349350097714,0.6956825506035,0.));
#123530=DIRECTION('center_axis',(0.841431341323684,0.486167873910092,-0.235868811452398));
#123531=DIRECTION('ref_axis',(-0.224032784086759,0.711082813237174,0.66646120995377));
#123532=DIRECTION('center_axis',(0.512887290640309,0.825416580208867,0.235868811452346));
#123533=DIRECTION('ref_axis',(0.703536866256326,-0.246709005626589,-0.666461209944711));
#123534=DIRECTION('center_axis',(0.,0.,-1.));
#123535=DIRECTION('ref_axis',(0.718349350097721,0.695682550603493,0.));
#123536=DIRECTION('center_axis',(-0.708369143393475,-0.705842161313699,
-6.76296429840134E-17));
#123537=DIRECTION('ref_axis',(-0.705842161313699,0.708369143393475,4.00593428432545E-31));
#123538=DIRECTION('center_axis',(0.,0.,1.));
#123539=DIRECTION('ref_axis',(-0.718349350097721,-0.695682550603493,0.));
#123540=DIRECTION('center_axis',(-0.728183859595176,-0.685381840016989,
-1.38914942345546E-16));
#123541=DIRECTION('ref_axis',(0.685381840016988,-0.728183859595176,-1.3065508742723E-30));
#123542=DIRECTION('center_axis',(0.,0.,-1.));
#123543=DIRECTION('ref_axis',(0.718349350097727,0.695682550603487,0.));
#123544=DIRECTION('center_axis',(0.,0.,1.));
#123545=DIRECTION('ref_axis',(-0.718349350097727,-0.695682550603487,0.));
#123546=DIRECTION('center_axis',(0.,0.,1.));
#123547=DIRECTION('ref_axis',(-0.718349350097727,-0.695682550603487,0.));
#123548=DIRECTION('center_axis',(-0.713972444898831,0.223209005790558,0.663642288932205));
#123549=DIRECTION('ref_axis',(-0.494374782310175,0.510482551659726,-0.703563173472533));
#123550=DIRECTION('center_axis',(-0.716025886917708,0.223850972794686,0.661209249211309));
#123551=DIRECTION('ref_axis',(-0.492770459694853,0.508825956842051,-0.705884848750768));
#123552=DIRECTION('center_axis',(0.200786202533562,-0.722832781236137,-0.661209249211308));
#123553=DIRECTION('ref_axis',(0.492770459694833,-0.508825956842068,0.705884848750769));
#123554=DIRECTION('center_axis',(0.200210381417841,-0.72075981818729,-0.663642288932184));
#123555=DIRECTION('ref_axis',(0.494374782310176,-0.510482551659703,0.703563173472549));
#123556=DIRECTION('center_axis',(0.,0.,1.));
#123557=DIRECTION('ref_axis',(-0.718349350097718,-0.695682550603496,0.));
#123558=DIRECTION('center_axis',(0.,0.,1.));
#123559=DIRECTION('ref_axis',(-0.718349350097718,-0.695682550603496,0.));
#123560=DIRECTION('center_axis',(0.,0.,1.));
#123561=DIRECTION('ref_axis',(0.718349350097718,0.695682550603496,0.));
#123562=DIRECTION('center_axis',(0.,0.,-1.));
#123563=DIRECTION('ref_axis',(-0.718349350097721,-0.695682550603493,0.));
#123564=DIRECTION('center_axis',(-0.944390545183258,-0.328825939014045,
0.));
#123565=DIRECTION('ref_axis',(0.328825939014045,-0.944390545183258,0.));
#123566=DIRECTION('',(0.,0.,1.));
#123567=DIRECTION('center_axis',(0.944392156125255,0.328821312332193,2.28597556106335E-6));
#123568=DIRECTION('ref_axis',(0.311272357528953,-0.89398839130544,-0.322326349604682));
#123569=DIRECTION('',(0.,0.,-1.));
#123570=DIRECTION('center_axis',(0.236623233703368,0.971601484803189,0.));
#123571=DIRECTION('ref_axis',(-0.971601484803189,0.236623233703368,0.));
#123572=DIRECTION('center_axis',(-0.236623233703389,-0.971601484803184,
-6.58220891953721E-15));
#123573=DIRECTION('ref_axis',(0.970296945073439,-0.236305526892341,0.0518028603581309));
#123574=DIRECTION('',(0.,0.,1.));
#123575=DIRECTION('',(0.,0.,1.));
#123576=DIRECTION('center_axis',(0.,0.,1.));
#123577=DIRECTION('ref_axis',(-0.672300890261307,-0.740277997075324,0.));
#123578=DIRECTION('center_axis',(0.,0.,-1.));
#123579=DIRECTION('ref_axis',(0.672300890261307,0.740277997075324,0.));
#123580=DIRECTION('center_axis',(0.808553647760917,0.539079681008855,-0.235868811452268));
#123581=DIRECTION('ref_axis',(-0.269131716983368,0.695267987584204,0.66646120993963));
#123582=DIRECTION('center_axis',(0.458948886824981,0.85658147485582,0.235868811452339));
#123583=DIRECTION('ref_axis',(0.717898074571082,-0.201126353728443,-0.666461209946261));
#123584=DIRECTION('center_axis',(0.,0.,-1.));
#123585=DIRECTION('ref_axis',(0.67230089026131,0.740277997075322,0.));
#123586=DIRECTION('center_axis',(-0.66169026046899,-0.749777299736715,-6.76296429840134E-17));
#123587=DIRECTION('ref_axis',(-0.749777299736715,0.66169026046899,4.93038065763132E-31));
#123588=DIRECTION('center_axis',(0.,0.,1.));
#123589=DIRECTION('ref_axis',(-0.67230089026131,-0.740277997075321,0.));
#123590=DIRECTION('center_axis',(-0.682775162497489,-0.73062854959037,-1.38914942345546E-16));
#123591=DIRECTION('ref_axis',(0.73062854959037,-0.682775162497489,-2.71170936169723E-31));
#123592=DIRECTION('center_axis',(0.,0.,-1.));
#123593=DIRECTION('ref_axis',(0.672300890261315,0.740277997075317,0.));
#123594=DIRECTION('center_axis',(0.,0.,1.));
#123595=DIRECTION('ref_axis',(-0.672300890261315,-0.740277997075317,0.));
#123596=DIRECTION('center_axis',(0.,0.,1.));
#123597=DIRECTION('ref_axis',(-0.672300890261315,-0.740277997075317,0.));
#123598=DIRECTION('center_axis',(-0.726806562040159,0.177006027344235,0.663642288932205));
#123599=DIRECTION('ref_axis',(-0.526065765679541,0.477759009452735,-0.703563173472531));
#123600=DIRECTION('center_axis',(-0.728896916009352,0.177515110876435,0.661209249211309));
#123601=DIRECTION('ref_axis',(-0.524358600922711,0.47620860758966,-0.705884848750768));
#123602=DIRECTION('center_axis',(0.246685721049275,-0.708483227598097,-0.661209249211308));
#123603=DIRECTION('ref_axis',(0.524358600922702,-0.476208607589672,0.705884848750766));
#123604=DIRECTION('center_axis',(0.24597826782124,-0.706451416659712,-0.663642288932184));
#123605=DIRECTION('ref_axis',(0.526065765679537,-0.477759009452711,0.703563173472551));
#123606=DIRECTION('center_axis',(0.,0.,1.));
#123607=DIRECTION('ref_axis',(-0.672300890261315,-0.740277997075317,0.));
#123608=DIRECTION('center_axis',(0.,0.,1.));
#123609=DIRECTION('ref_axis',(-0.672300890261315,-0.740277997075317,0.));
#123610=DIRECTION('center_axis',(0.,0.,1.));
#123611=DIRECTION('ref_axis',(0.67230089026136,0.740277997075276,0.));
#123612=DIRECTION('center_axis',(0.,0.,-1.));
#123613=DIRECTION('ref_axis',(-0.67230089026131,-0.740277997075322,0.));
#123614=DIRECTION('center_axis',(-0.921382243274616,-0.388657640833466,
0.));
#123615=DIRECTION('ref_axis',(0.388657640833466,-0.921382243274617,0.));
#123616=DIRECTION('',(0.,0.,1.));
#123617=DIRECTION('center_axis',(0.921384147339249,0.38865312687112,2.28597552009451E-6));
#123618=DIRECTION('ref_axis',(0.367910847977183,-0.872208307853349,-0.322326349609068));
#123619=DIRECTION('',(0.,0.,-1.));
#123620=DIRECTION('center_axis',(0.173886345027034,0.984765727984651,0.));
#123621=DIRECTION('ref_axis',(-0.984765727984651,0.173886345027034,0.));
#123622=DIRECTION('center_axis',(-0.173886345027096,-0.98476572798464,-3.60124600396073E-14));
#123623=DIRECTION('ref_axis',(0.983443513025211,-0.173652873126014,0.0518028603815676));
#123624=DIRECTION('',(0.,0.,1.));
#123625=DIRECTION('',(0.,0.,1.));
#123626=DIRECTION('center_axis',(0.,0.,1.));
#123627=DIRECTION('ref_axis',(-0.623489801858719,-0.781831482468041,0.));
#123628=DIRECTION('center_axis',(0.,0.,-1.));
#123629=DIRECTION('ref_axis',(0.623489801858719,0.781831482468041,0.));
#123630=DIRECTION('center_axis',(0.772353433824751,0.589776294066747,-0.235868811452489));
#123631=DIRECTION('ref_axis',(-0.313124729911562,0.676596156621241,0.666461209946368));
#123632=DIRECTION('center_axis',(0.403124563589422,0.884226492486458,0.23586881145233));
#123633=DIRECTION('ref_axis',(0.729309285718661,-0.15471723050946,-0.666461209934996));
#123634=DIRECTION('center_axis',(0.,0.,-1.));
#123635=DIRECTION('ref_axis',(0.623489801858726,0.781831482468036,0.));
#123636=DIRECTION('center_axis',(-0.612292350332122,-0.790631442408387,
-6.76296429840134E-17));
#123637=DIRECTION('ref_axis',(-0.790631442408387,0.612292350332122,-3.01985815279918E-31));
#123638=DIRECTION('center_axis',(0.,0.,1.));
#123639=DIRECTION('ref_axis',(-0.623489801858726,-0.781831482468036,0.));
#123640=DIRECTION('center_axis',(-0.634560795802287,-0.772872949734151,
-1.38914942345546E-16));
#123641=DIRECTION('ref_axis',(0.772872949734151,-0.634560795802287,7.39557098644698E-32));
#123642=DIRECTION('center_axis',(0.,0.,-1.));
#123643=DIRECTION('ref_axis',(0.623489801858737,0.781831482468027,0.));
#123644=DIRECTION('center_axis',(0.,0.,1.));
#123645=DIRECTION('ref_axis',(-0.623489801858737,-0.781831482468027,0.));
#123646=DIRECTION('center_axis',(0.,0.,1.));
#123647=DIRECTION('ref_axis',(-0.623489801858737,-0.781831482468027,0.));
#123648=DIRECTION('center_axis',(-0.736654075118546,0.13007569316388,0.663642288932205));
#123649=DIRECTION('ref_axis',(-0.555595031976983,0.443072252996905,-0.703563173472533));
#123650=DIRECTION('center_axis',(-0.738772751325215,0.130449801290721,0.661209249211309));
#123651=DIRECTION('ref_axis',(-0.553792040184809,0.44163441502226,-0.705884848750767));
#123652=DIRECTION('center_axis',(0.291571555023274,-0.691222364408681,-0.661209249211308));
#123653=DIRECTION('ref_axis',(0.553792040184795,-0.441634415022275,0.705884848750769));
#123654=DIRECTION('center_axis',(0.290735376759989,-0.689240054727726,-0.663642288932184));
#123655=DIRECTION('ref_axis',(0.555595031976965,-0.443072252996894,0.703563173472555));
#123656=DIRECTION('center_axis',(0.,0.,1.));
#123657=DIRECTION('ref_axis',(-0.623489801858737,-0.781831482468027,0.));
#123658=DIRECTION('center_axis',(0.,0.,1.));
#123659=DIRECTION('ref_axis',(-0.623489801858737,-0.781831482468027,0.));
#123660=DIRECTION('center_axis',(0.,0.,1.));
#123661=DIRECTION('ref_axis',(0.623489801858737,0.781831482468027,0.));
#123662=DIRECTION('center_axis',(0.,0.,-1.));
#123663=DIRECTION('ref_axis',(-0.623489801858726,-0.781831482468036,0.));
#123664=DIRECTION('center_axis',(-0.894587784092488,-0.4468922650399,0.));
#123665=DIRECTION('ref_axis',(0.4468922650399,-0.894587784092488,0.));
#123666=DIRECTION('',(0.,0.,1.));
#123667=DIRECTION('center_axis',(0.894589973455606,0.446887882345754,2.28597555658038E-6));
#123668=DIRECTION('ref_axis',(0.423037513841325,-0.846844133390666,-0.322326349566341));
#123669=DIRECTION('',(0.,0.,-1.));
#123670=DIRECTION('center_axis',(0.11043492006048,0.993883357558238,0.));
#123671=DIRECTION('ref_axis',(-0.993883357558238,0.11043492006048,0.));
#123672=DIRECTION('center_axis',(-0.110434920060485,-0.993883357558237,
5.17851018741787E-15));
#123673=DIRECTION('ref_axis',(0.992548900635969,-0.11028664245586,0.0518028603664164));
#123674=DIRECTION('',(0.,0.,1.));
#123675=DIRECTION('',(0.,0.,1.));
#123676=DIRECTION('center_axis',(0.,0.,1.));
#123677=DIRECTION('ref_axis',(-0.572116660122161,-0.820172254596962,0.));
#123678=DIRECTION('center_axis',(0.,0.,-1.));
#123679=DIRECTION('ref_axis',(0.572116660122161,0.820172254596962,0.));
#123680=DIRECTION('center_axis',(0.732979453960397,0.638049389824958,-0.235868811452291));
#123681=DIRECTION('ref_axis',(-0.355831046164631,0.655144046926414,0.666461209945684));
#123682=DIRECTION('center_axis',(0.345643715051997,0.90823803379354,0.235868811452253));
#123683=DIRECTION('ref_axis',(0.737723608566232,-0.107672340995733,-0.666461209935369));
#123684=DIRECTION('center_axis',(0.,0.,-1.));
#123685=DIRECTION('ref_axis',(0.572116660122162,0.820172254596961,0.));
#123686=DIRECTION('center_axis',(-0.560378399591443,-0.828236710893289,
-6.76296429840134E-17));
#123687=DIRECTION('ref_axis',(-0.828236710893289,0.560378399591443,2.46519032881566E-31));
#123688=DIRECTION('center_axis',(0.,0.,1.));
#123689=DIRECTION('ref_axis',(-0.572116660122162,-0.820172254596961,0.));
#123690=DIRECTION('center_axis',(-0.58373888268427,-0.811941449146747,-1.38914942345546E-16));
#123691=DIRECTION('ref_axis',(0.811941449146747,-0.58373888268427,2.46519032881566E-32));
#123692=DIRECTION('center_axis',(0.,0.,-1.));
#123693=DIRECTION('ref_axis',(0.572116660122157,0.820172254596965,0.));
#123694=DIRECTION('center_axis',(0.,0.,1.));
#123695=DIRECTION('ref_axis',(-0.572116660122157,-0.820172254596965,0.));
#123696=DIRECTION('center_axis',(0.,0.,1.));
#123697=DIRECTION('ref_axis',(-0.572116660122157,-0.820172254596965,0.));
#123698=DIRECTION('center_axis',(-0.743474518590466,0.0826108500591668,
0.663642288932205));
#123699=DIRECTION('ref_axis',(-0.58284123911327,0.406564817614812,-0.703563173472534));
#123700=DIRECTION('center_axis',(-0.745612810939625,0.082848445490109,0.661209249211309));
#123701=DIRECTION('ref_axis',(-0.580949829165767,0.405245451913252,-0.705884848750765));
#123702=DIRECTION('center_axis',(0.33525925893578,-0.671121120257178,-0.661209249211308));
#123703=DIRECTION('ref_axis',(0.580949829165751,-0.405245451913266,0.70588484875077));
#123704=DIRECTION('center_axis',(0.334297791673088,-0.669196457569336,-0.663642288932184));
#123705=DIRECTION('ref_axis',(0.582841239113255,-0.406564817614802,0.703563173472553));
#123706=DIRECTION('center_axis',(0.,0.,1.));
#123707=DIRECTION('ref_axis',(-0.572116660122157,-0.820172254596965,0.));
#123708=DIRECTION('center_axis',(0.,0.,1.));
#123709=DIRECTION('ref_axis',(-0.572116660122157,-0.820172254596965,0.));
#123710=DIRECTION('center_axis',(0.,0.,1.));
#123711=DIRECTION('ref_axis',(0.572116660122157,0.820172254596965,0.));
#123712=DIRECTION('center_axis',(0.,0.,-1.));
#123713=DIRECTION('ref_axis',(-0.572116660122162,-0.820172254596961,0.));
#123714=DIRECTION('center_axis',(-0.864117271817046,-0.503290513071194,
0.));
#123715=DIRECTION('ref_axis',(0.503290513071194,-0.864117271817046,0.));
#123716=DIRECTION('',(0.,0.,1.));
#123717=DIRECTION('center_axis',(0.864119737482042,0.503286279654772,2.28597554434033E-6));
#123718=DIRECTION('ref_axis',(0.476425827832821,-0.81800009475483,-0.32232634945797));
#123719=DIRECTION('',(0.,0.,-1.));
#123720=DIRECTION('center_axis',(0.0465296943191825,0.998916907228306,0.));
#123721=DIRECTION('ref_axis',(-0.998916907228306,0.0465296943191825,0.));
#123722=DIRECTION('center_axis',(-0.0465296943192999,-0.9989169072283,-5.01419207570033E-14));
#123723=DIRECTION('ref_axis',(0.99757569190683,-0.0464672203152359,0.0518028604691345));
#123724=DIRECTION('',(0.,0.,1.));
#123725=DIRECTION('',(0.,0.,1.));
#123726=DIRECTION('center_axis',(0.,0.,1.));
#123727=DIRECTION('ref_axis',(-0.518392568310538,-0.855142763005338,0.));
#123728=DIRECTION('center_axis',(0.,0.,-1.));
#123729=DIRECTION('ref_axis',(0.518392568310538,0.855142763005338,0.));
#123730=DIRECTION('center_axis',(0.690593504295649,0.683700603779683,-0.235868811452367));
#123731=DIRECTION('ref_axis',(-0.397075176320611,0.630999809812658,0.666461209948745));
#123732=DIRECTION('center_axis',(0.28674254234956,0.928517430203087,0.235868811452396));
#123733=DIRECTION('ref_axis',(0.743106466862043,-0.0601850027357412,-0.666461209939115));
#123734=DIRECTION('center_axis',(0.,0.,-1.));
#123735=DIRECTION('ref_axis',(0.518392568310517,0.855142763005351,0.));
#123736=DIRECTION('center_axis',(-0.506161733806052,-0.862438577076914,
-6.76296429840134E-17));
#123737=DIRECTION('ref_axis',(-0.862438577076914,0.506161733806052,6.90253292068385E-31));
#123738=DIRECTION('center_axis',(0.,0.,1.));
#123739=DIRECTION('ref_axis',(-0.518392568310517,-0.855142763005351,0.));
#123740=DIRECTION('center_axis',(-0.530518261285706,-0.847673506983905,
-1.38914942345546E-16));
#123741=DIRECTION('ref_axis',(0.847673506983905,-0.530518261285706,-3.69778549322349E-32));
#123742=DIRECTION('center_axis',(0.,0.,-1.));
#123743=DIRECTION('ref_axis',(0.518392568310514,0.855142763005353,0.));
#123744=DIRECTION('center_axis',(0.,0.,1.));
#123745=DIRECTION('ref_axis',(-0.518392568310514,-0.855142763005353,0.));
#123746=DIRECTION('center_axis',(0.,0.,1.));
#123747=DIRECTION('ref_axis',(-0.518392568310514,-0.855142763005353,0.));
#123748=DIRECTION('center_axis',(-0.747239865790715,0.0348065412515887,
0.663642288932205));
#123749=DIRECTION('ref_axis',(-0.607692426578982,0.368386720189271,-0.703563173472532));
#123750=DIRECTION('center_axis',(-0.749388987580438,0.0349066476560422,
0.661209249211309));
#123751=DIRECTION('ref_axis',(-0.60572037068534,0.367191248317438,-0.705884848750768));
#123752=DIRECTION('center_axis',(0.377569310640434,-0.648262095467509,-0.661209249211308));
#123753=DIRECTION('ref_axis',(0.605720370685331,-0.367191248317456,0.705884848750767));
#123754=DIRECTION('center_axis',(0.376486505253551,-0.646402988624604,-0.663642288932184));
#123755=DIRECTION('ref_axis',(0.607692426578966,-0.368386720189256,0.703563173472553));
#123756=DIRECTION('center_axis',(0.,0.,1.));
#123757=DIRECTION('ref_axis',(-0.518392568310514,-0.855142763005353,0.));
#123758=DIRECTION('center_axis',(0.,0.,1.));
#123759=DIRECTION('ref_axis',(-0.518392568310514,-0.855142763005353,0.));
#123760=DIRECTION('center_axis',(0.,0.,1.));
#123761=DIRECTION('ref_axis',(0.51839256831062,0.855142763005288,0.));
#123762=DIRECTION('center_axis',(0.,0.,-1.));
#123763=DIRECTION('ref_axis',(-0.518392568310517,-0.855142763005351,0.));
#123764=DIRECTION('axis',(0.,0.,1.));
#123765=DIRECTION('refdir',(1.,0.,0.));
#123766=DIRECTION('center_axis',(0.,0.,1.));
#123767=DIRECTION('ref_axis',(0.,1.,0.));
#123768=DIRECTION('',(0.,0.,-1.));
#123769=DIRECTION('center_axis',(0.,-4.12699273797265E-32,1.));
#123770=DIRECTION('ref_axis',(0.,-1.,-4.12699273797265E-32));
#123771=DIRECTION('center_axis',(0.,0.,1.));
#123772=DIRECTION('ref_axis',(0.,1.,0.));
#123773=DIRECTION('',(0.,0.,-1.));
#123774=DIRECTION('center_axis',(0.,0.,1.));
#123775=DIRECTION('ref_axis',(0.,1.,0.));
#123776=DIRECTION('',(0.,0.,-1.));
#123777=DIRECTION('center_axis',(0.,0.,1.));
#123778=DIRECTION('ref_axis',(0.,1.,0.));
#123779=DIRECTION('',(0.,0.,-1.));
#123780=DIRECTION('center_axis',(0.,0.,1.));
#123781=DIRECTION('ref_axis',(0.,1.,0.));
#123782=DIRECTION('',(0.,0.,-1.));
#123783=DIRECTION('center_axis',(0.,0.,1.));
#123784=DIRECTION('ref_axis',(0.,1.,0.));
#123785=DIRECTION('',(0.,0.,-1.));
#123786=DIRECTION('center_axis',(0.,0.,1.));
#123787=DIRECTION('ref_axis',(0.,1.,0.));
#123788=DIRECTION('',(0.,0.,-1.));
#123789=DIRECTION('center_axis',(0.,0.,1.));
#123790=DIRECTION('ref_axis',(0.,1.,0.));
#123791=DIRECTION('',(0.,0.,-1.));
#123792=DIRECTION('center_axis',(0.,0.,1.));
#123793=DIRECTION('ref_axis',(0.,1.,0.));
#123794=DIRECTION('',(0.,0.,-1.));
#123795=DIRECTION('center_axis',(0.,0.,1.));
#123796=DIRECTION('ref_axis',(0.,1.,0.));
#123797=DIRECTION('',(0.,0.,-1.));
#123798=DIRECTION('center_axis',(0.,0.,1.));
#123799=DIRECTION('ref_axis',(0.,1.,0.));
#123800=DIRECTION('',(0.,0.,-1.));
#123801=DIRECTION('center_axis',(0.,0.,1.));
#123802=DIRECTION('ref_axis',(0.,1.,0.));
#123803=DIRECTION('',(0.,0.,-1.));
#123804=DIRECTION('center_axis',(0.,0.,1.));
#123805=DIRECTION('ref_axis',(0.,1.,0.));
#123806=DIRECTION('',(0.,0.,-1.));
#123807=DIRECTION('center_axis',(0.,0.,1.));
#123808=DIRECTION('ref_axis',(0.,1.,0.));
#123809=DIRECTION('',(0.,0.,-1.));
#123810=DIRECTION('center_axis',(0.,0.,1.));
#123811=DIRECTION('ref_axis',(0.,1.,0.));
#123812=DIRECTION('',(0.,0.,-1.));
#123813=DIRECTION('center_axis',(0.,0.,1.));
#123814=DIRECTION('ref_axis',(0.,1.,0.));
#123815=DIRECTION('',(0.,0.,-1.));
#123816=DIRECTION('center_axis',(0.,0.,1.));
#123817=DIRECTION('ref_axis',(0.,1.,0.));
#123818=DIRECTION('',(0.,0.,-1.));
#123819=DIRECTION('center_axis',(0.,0.,1.));
#123820=DIRECTION('ref_axis',(0.,1.,0.));
#123821=DIRECTION('',(0.,0.,-1.));
#123822=DIRECTION('center_axis',(0.,0.,1.));
#123823=DIRECTION('ref_axis',(0.,1.,0.));
#123824=DIRECTION('',(0.,0.,-1.));
#123825=DIRECTION('center_axis',(0.,0.,1.));
#123826=DIRECTION('ref_axis',(0.,1.,0.));
#123827=DIRECTION('',(0.,0.,-1.));
#123828=DIRECTION('center_axis',(0.,0.,1.));
#123829=DIRECTION('ref_axis',(0.,1.,0.));
#123830=DIRECTION('',(0.,0.,-1.));
#123831=DIRECTION('center_axis',(0.,0.,1.));
#123832=DIRECTION('ref_axis',(0.,1.,0.));
#123833=DIRECTION('',(0.,0.,-1.));
#123834=DIRECTION('center_axis',(0.,0.,1.));
#123835=DIRECTION('ref_axis',(0.,1.,0.));
#123836=DIRECTION('',(0.,0.,-1.));
#123837=DIRECTION('center_axis',(0.,0.,1.));
#123838=DIRECTION('ref_axis',(0.,1.,0.));
#123839=DIRECTION('',(0.,0.,-1.));
#123840=DIRECTION('center_axis',(0.,0.,1.));
#123841=DIRECTION('ref_axis',(0.,1.,0.));
#123842=DIRECTION('',(0.,0.,-1.));
#123843=DIRECTION('center_axis',(0.,0.,1.));
#123844=DIRECTION('ref_axis',(0.,1.,0.));
#123845=DIRECTION('',(0.,0.,-1.));
#123846=DIRECTION('center_axis',(0.,0.,1.));
#123847=DIRECTION('ref_axis',(0.,1.,0.));
#123848=DIRECTION('',(0.,0.,-1.));
#123849=DIRECTION('center_axis',(0.,0.,1.));
#123850=DIRECTION('ref_axis',(0.,1.,0.));
#123851=DIRECTION('',(0.,0.,-1.));
#123852=DIRECTION('center_axis',(0.,0.,1.));
#123853=DIRECTION('ref_axis',(0.,1.,0.));
#123854=DIRECTION('',(0.,0.,-1.));
#123855=DIRECTION('center_axis',(0.,0.,1.));
#123856=DIRECTION('ref_axis',(0.,1.,0.));
#123857=DIRECTION('',(0.,0.,-1.));
#123858=DIRECTION('center_axis',(0.,0.,1.));
#123859=DIRECTION('ref_axis',(0.,1.,0.));
#123860=DIRECTION('',(0.,0.,-1.));
#123861=DIRECTION('center_axis',(0.,0.,1.));
#123862=DIRECTION('ref_axis',(0.,1.,0.));
#123863=DIRECTION('',(0.,0.,-1.));
#123864=DIRECTION('center_axis',(0.,0.,1.));
#123865=DIRECTION('ref_axis',(0.,1.,0.));
#123866=DIRECTION('',(0.,0.,-1.));
#123867=DIRECTION('center_axis',(0.,0.,1.));
#123868=DIRECTION('ref_axis',(0.,1.,0.));
#123869=DIRECTION('',(0.,0.,-1.));
#123870=DIRECTION('center_axis',(0.,0.,1.));
#123871=DIRECTION('ref_axis',(0.,1.,0.));
#123872=DIRECTION('',(0.,0.,-1.));
#123873=DIRECTION('center_axis',(0.,0.,1.));
#123874=DIRECTION('ref_axis',(0.,1.,0.));
#123875=DIRECTION('',(0.,0.,-1.));
#123876=DIRECTION('center_axis',(0.,-1.22464679914735E-16,1.));
#123877=DIRECTION('ref_axis',(0.,-1.,-1.22464679914735E-16));
#123878=DIRECTION('',(8.65956056235489E-17,-0.707106781186543,-0.707106781186552));
#123879=DIRECTION('center_axis',(0.,0.,1.));
#123880=DIRECTION('ref_axis',(0.802795663530306,0.596254243269543,0.));
#123881=DIRECTION('center_axis',(0.,-4.12699273797265E-32,1.));
#123882=DIRECTION('ref_axis',(0.,-1.,-4.12699273797265E-32));
#123883=DIRECTION('',(8.65956056235498E-17,-0.707106781186552,-0.707106781186544));
#123884=DIRECTION('center_axis',(0.,-4.12699273797265E-32,1.));
#123885=DIRECTION('ref_axis',(0.,-1.,-4.12699273797265E-32));
#123886=DIRECTION('center_axis',(0.,-4.12699273797265E-32,1.));
#123887=DIRECTION('ref_axis',(0.,-1.,-4.12699273797265E-32));
#123888=DIRECTION('',(0.,4.12699273797265E-32,-1.));
#123889=DIRECTION('center_axis',(0.,-4.12699273797265E-32,1.));
#123890=DIRECTION('ref_axis',(0.,-1.,-4.12699273797265E-32));
#123891=DIRECTION('center_axis',(0.,-4.12699273797265E-32,1.));
#123892=DIRECTION('ref_axis',(0.,-1.,-4.12699273797265E-32));
#123893=DIRECTION('',(0.,4.12699273797265E-32,-1.));
#123894=DIRECTION('center_axis',(0.,-4.12699273797265E-32,1.));
#123895=DIRECTION('ref_axis',(0.,-1.,-4.12699273797265E-32));
#123896=DIRECTION('',(0.,4.12699273797265E-32,-1.));
#123897=DIRECTION('center_axis',(0.,-4.12699273797265E-32,1.));
#123898=DIRECTION('ref_axis',(0.,-1.,-4.12699273797265E-32));
#123899=DIRECTION('',(0.,4.12699273797265E-32,-1.));
#123900=DIRECTION('center_axis',(0.,-4.12699273797265E-32,1.));
#123901=DIRECTION('ref_axis',(0.,-1.,-4.12699273797265E-32));
#123902=DIRECTION('',(0.,4.12699273797265E-32,-1.));
#123903=DIRECTION('center_axis',(0.,-4.12699273797265E-32,1.));
#123904=DIRECTION('ref_axis',(0.,-1.,-4.12699273797265E-32));
#123905=DIRECTION('',(0.,4.12699273797265E-32,-1.));
#123906=DIRECTION('center_axis',(0.,-4.12699273797265E-32,1.));
#123907=DIRECTION('ref_axis',(0.,-1.,-4.12699273797265E-32));
#123908=DIRECTION('',(0.,4.12699273797265E-32,-1.));
#123909=DIRECTION('center_axis',(0.,-4.12699273797265E-32,1.));
#123910=DIRECTION('ref_axis',(0.,-1.,-4.12699273797265E-32));
#123911=DIRECTION('',(0.,4.12699273797265E-32,-1.));
#123912=DIRECTION('center_axis',(0.,-4.12699273797265E-32,1.));
#123913=DIRECTION('ref_axis',(0.,-1.,-4.12699273797265E-32));
#123914=DIRECTION('',(0.,4.12699273797265E-32,-1.));
#123915=DIRECTION('center_axis',(0.,-4.12699273797265E-32,1.));
#123916=DIRECTION('ref_axis',(0.,-1.,-4.12699273797265E-32));
#123917=DIRECTION('',(0.,4.12699273797265E-32,-1.));
#123918=DIRECTION('center_axis',(0.,-4.12699273797265E-32,1.));
#123919=DIRECTION('ref_axis',(0.,-1.,-4.12699273797265E-32));
#123920=DIRECTION('',(0.,4.12699273797265E-32,-1.));
#123921=DIRECTION('center_axis',(0.,-4.12699273797265E-32,1.));
#123922=DIRECTION('ref_axis',(0.,-1.,-4.12699273797265E-32));
#123923=DIRECTION('',(0.,4.12699273797265E-32,-1.));
#123924=DIRECTION('center_axis',(0.,-4.12699273797265E-32,1.));
#123925=DIRECTION('ref_axis',(0.,-1.,-4.12699273797265E-32));
#123926=DIRECTION('',(0.,4.12699273797265E-32,-1.));
#123927=DIRECTION('center_axis',(0.,-4.12699273797265E-32,1.));
#123928=DIRECTION('ref_axis',(0.,-1.,-4.12699273797265E-32));
#123929=DIRECTION('',(0.,4.12699273797265E-32,-1.));
#123930=DIRECTION('center_axis',(0.,-4.12699273797265E-32,1.));
#123931=DIRECTION('ref_axis',(0.,-1.,-4.12699273797265E-32));
#123932=DIRECTION('',(0.,4.12699273797265E-32,-1.));
#123933=DIRECTION('center_axis',(0.,-4.12699273797265E-32,1.));
#123934=DIRECTION('ref_axis',(0.,-1.,-4.12699273797265E-32));
#123935=DIRECTION('',(0.,4.12699273797265E-32,-1.));
#123936=DIRECTION('center_axis',(0.,-4.12699273797265E-32,1.));
#123937=DIRECTION('ref_axis',(0.,-1.,-4.12699273797265E-32));
#123938=DIRECTION('',(0.,4.12699273797265E-32,-1.));
#123939=DIRECTION('center_axis',(0.,-4.12699273797265E-32,1.));
#123940=DIRECTION('ref_axis',(0.,-1.,-4.12699273797265E-32));
#123941=DIRECTION('',(0.,4.12699273797265E-32,-1.));
#123942=DIRECTION('center_axis',(0.,-4.12699273797265E-32,1.));
#123943=DIRECTION('ref_axis',(0.,-1.,-4.12699273797265E-32));
#123944=DIRECTION('',(0.,4.12699273797265E-32,-1.));
#123945=DIRECTION('center_axis',(0.,-4.12699273797265E-32,1.));
#123946=DIRECTION('ref_axis',(0.,-1.,-4.12699273797265E-32));
#123947=DIRECTION('',(0.,4.12699273797265E-32,-1.));
#123948=DIRECTION('center_axis',(0.,-4.12699273797265E-32,1.));
#123949=DIRECTION('ref_axis',(0.,-1.,-4.12699273797265E-32));
#123950=DIRECTION('',(0.,4.12699273797265E-32,-1.));
#123951=DIRECTION('center_axis',(0.,-4.12699273797265E-32,1.));
#123952=DIRECTION('ref_axis',(0.,-1.,-4.12699273797265E-32));
#123953=DIRECTION('',(0.,4.12699273797265E-32,-1.));
#123954=DIRECTION('center_axis',(0.,-4.12699273797265E-32,1.));
#123955=DIRECTION('ref_axis',(0.,-1.,-4.12699273797265E-32));
#123956=DIRECTION('',(0.,4.12699273797265E-32,-1.));
#123957=DIRECTION('center_axis',(0.,-4.12699273797265E-32,1.));
#123958=DIRECTION('ref_axis',(0.,-1.,-4.12699273797265E-32));
#123959=DIRECTION('',(0.,4.12699273797265E-32,-1.));
#123960=DIRECTION('center_axis',(0.,-4.12699273797265E-32,1.));
#123961=DIRECTION('ref_axis',(0.,-1.,-4.12699273797265E-32));
#123962=DIRECTION('',(0.,4.12699273797265E-32,-1.));
#123963=DIRECTION('center_axis',(0.,-4.12699273797265E-32,1.));
#123964=DIRECTION('ref_axis',(0.,-1.,-4.12699273797265E-32));
#123965=DIRECTION('',(0.,4.12699273797265E-32,-1.));
#123966=DIRECTION('center_axis',(0.,-4.12699273797265E-32,1.));
#123967=DIRECTION('ref_axis',(0.,-1.,-4.12699273797265E-32));
#123968=DIRECTION('',(0.,4.12699273797265E-32,-1.));
#123969=DIRECTION('center_axis',(0.,-4.12699273797265E-32,1.));
#123970=DIRECTION('ref_axis',(0.,-1.,-4.12699273797265E-32));
#123971=DIRECTION('',(0.,4.12699273797265E-32,-1.));
#123972=DIRECTION('center_axis',(0.,-4.12699273797265E-32,1.));
#123973=DIRECTION('ref_axis',(0.,-1.,-4.12699273797265E-32));
#123974=DIRECTION('',(0.,4.12699273797265E-32,-1.));
#123975=DIRECTION('center_axis',(0.,-4.12699273797265E-32,1.));
#123976=DIRECTION('ref_axis',(0.,-1.,-4.12699273797265E-32));
#123977=DIRECTION('',(0.,4.12699273797265E-32,-1.));
#123978=DIRECTION('center_axis',(0.,-4.12699273797265E-32,1.));
#123979=DIRECTION('ref_axis',(0.,-1.,-4.12699273797265E-32));
#123980=DIRECTION('',(0.,4.12699273797265E-32,-1.));
#123981=DIRECTION('center_axis',(0.,-4.12699273797265E-32,1.));
#123982=DIRECTION('ref_axis',(0.,-1.,-4.12699273797265E-32));
#123983=DIRECTION('',(0.,4.12699273797265E-32,-1.));
#123984=DIRECTION('center_axis',(0.,-4.12699273797265E-32,1.));
#123985=DIRECTION('ref_axis',(0.,-1.,-4.12699273797265E-32));
#123986=DIRECTION('',(0.,4.12699273797265E-32,-1.));
#123987=DIRECTION('center_axis',(0.,-4.12699273797265E-32,1.));
#123988=DIRECTION('ref_axis',(0.,-1.,-4.12699273797265E-32));
#123989=DIRECTION('',(0.,4.12699273797265E-32,-1.));
#123990=DIRECTION('center_axis',(0.,-4.12699273797265E-32,1.));
#123991=DIRECTION('ref_axis',(0.,-1.,-4.12699273797265E-32));
#123992=DIRECTION('center_axis',(0.,1.22464679914735E-16,-1.));
#123993=DIRECTION('ref_axis',(0.,1.,1.22464679914735E-16));
#123994=DIRECTION('',(0.,4.12699273797265E-32,-1.));
#123995=DIRECTION('center_axis',(0.,1.22464679914735E-16,-1.));
#123996=DIRECTION('ref_axis',(0.,1.,1.22464679914735E-16));
#123997=DIRECTION('',(0.,4.12699273797265E-32,-1.));
#123998=DIRECTION('center_axis',(-1.70823811232218E-32,2.97377031107479E-32,
-1.));
#123999=DIRECTION('ref_axis',(0.830050209755074,0.557688666986839,0.));
#124000=DIRECTION('center_axis',(1.70823811232218E-32,-2.97377031107479E-32,
1.));
#124001=DIRECTION('ref_axis',(-0.830050209755074,-0.557688666986839,-2.40514597263697E-33));
#124002=DIRECTION('center_axis',(0.545790114644076,-0.837921924022045,6.13681984861663E-17));
#124003=DIRECTION('ref_axis',(0.837921924022045,0.545790114644076,-3.6361557350031E-31));
#124004=DIRECTION('center_axis',(-1.70823811232218E-32,2.97377031107479E-32,
-1.));
#124005=DIRECTION('ref_axis',(0.830050209755074,0.557688666986839,2.40514597263697E-33));
#124006=DIRECTION('center_axis',(0.569473707694335,-0.822009547538754,-3.46966352979465E-16));
#124007=DIRECTION('ref_axis',(-0.822009547538754,-0.569473707694335,7.88510670898553E-14));
#124008=DIRECTION('center_axis',(-1.79610390708164E-32,3.11682651859213E-32,
-1.));
#124009=DIRECTION('ref_axis',(0.872745089844851,0.488176206048291,0.));
#124010=DIRECTION('center_axis',(1.79610390708164E-32,-3.11682651859213E-32,
1.));
#124011=DIRECTION('ref_axis',(-0.872745089844851,-0.488176206048291,4.59803209996414E-34));
#124012=DIRECTION('center_axis',(0.4756756273667,-0.879620769155263,6.13681984861663E-17));
#124013=DIRECTION('ref_axis',(0.879620769155263,0.4756756273667,1.87970762572194E-31));
#124014=DIRECTION('center_axis',(-1.79610390708164E-32,3.11682651859213E-32,
-1.));
#124015=DIRECTION('ref_axis',(0.872745089844851,0.488176206048291,-4.59803209996414E-34));
#124016=DIRECTION('center_axis',(0.500577421621527,-0.865691772493388,-3.46966352979465E-16));
#124017=DIRECTION('ref_axis',(-0.865691772493388,-0.500577421621527,7.88510670898553E-14));
#124018=DIRECTION('center_axis',(-1.87201692667575E-32,3.2665685963594E-32,
-1.));
#124019=DIRECTION('ref_axis',(0.909631995354514,0.415415013001897,0.));
#124020=DIRECTION('center_axis',(1.87201692667575E-32,-3.2665685963594E-32,
1.));
#124021=DIRECTION('ref_axis',(-0.909631995354514,-0.415415013001896,3.45864856421259E-33));
#124022=DIRECTION('center_axis',(0.402395597270152,-0.915465883196964,6.13681984861663E-17));
#124023=DIRECTION('ref_axis',(0.915465883196964,0.402395597270152,-6.16297582203915E-33));
#124024=DIRECTION('center_axis',(-1.87201692667575E-32,3.2665685963594E-32,
-1.));
#124025=DIRECTION('ref_axis',(0.909631995354514,0.415415013001897,-3.45864856421259E-33));
#124026=DIRECTION('center_axis',(0.428349875397288,-0.903612961531168,-3.46966352979465E-16));
#124027=DIRECTION('ref_axis',(-0.903612961531168,-0.428349875397288,7.88510670898543E-14));
#124028=DIRECTION('center_axis',(-1.93547198248389E-32,3.42200003555476E-32,
-1.));
#124029=DIRECTION('ref_axis',(0.940465450013808,0.339889301582627,0.));
#124030=DIRECTION('center_axis',(1.93547198248389E-32,-3.42200003555476E-32,
1.));
#124031=DIRECTION('ref_axis',(-0.940465450013808,-0.339889301582627,6.57143326895392E-33));
#124032=DIRECTION('center_axis',(0.326437690864372,-0.945218722827229,6.13681984861663E-17));
#124033=DIRECTION('ref_axis',(0.945218722827228,0.326437690864372,2.65007960347684E-31));
#124034=DIRECTION('center_axis',(-1.93547198248389E-32,3.42200003555476E-32,
-1.));
#124035=DIRECTION('ref_axis',(0.940465450013808,0.339889301582627,-6.57143326895392E-33));
#124036=DIRECTION('center_axis',(0.353271731425036,-0.935520755395602,-3.46966352979465E-16));
#124037=DIRECTION('ref_axis',(-0.935520755395602,-0.353271731425036,7.88510670898545E-14));
#124038=DIRECTION('center_axis',(-1.98604679157899E-32,3.58208646559475E-32,
-1.));
#124039=DIRECTION('ref_axis',(0.965040262269137,0.262101682939113,0.));
#124040=DIRECTION('center_axis',(1.98604679157899E-32,-3.58208646559475E-32,
1.));
#124041=DIRECTION('ref_axis',(-0.965040262269137,-0.262101682939113,9.77744225558367E-33));
#124042=DIRECTION('center_axis',(0.248307395484317,-0.96868128780719,6.13681984861663E-17));
#124043=DIRECTION('ref_axis',(0.968681287807189,0.248307395484317,-4.00593428432545E-32));
#124044=DIRECTION('center_axis',(-1.98604679157899E-32,3.58208646559475E-32,
-1.));
#124045=DIRECTION('ref_axis',(0.965040262269137,0.262101682939113,-9.77744225558366E-33));
#124046=DIRECTION('center_axis',(0.275842622365882,-0.961202812982938,-3.46966352979465E-16));
#124047=DIRECTION('ref_axis',(-0.961202812982938,-0.275842622365882,7.88510670898555E-14));
#124048=DIRECTION('center_axis',(-2.0234047869508E-32,3.74576253769986E-32,
-1.));
#124049=DIRECTION('ref_axis',(0.983192890799501,0.182569820839372,0.));
#124050=DIRECTION('center_axis',(2.0234047869508E-32,-3.74576253769986E-32,
1.));
#124051=DIRECTION('ref_axis',(-0.983192890799501,-0.182569820839372,1.30553400632501E-32));
#124052=DIRECTION('center_axis',(0.16852465535515,-0.985697438637956,6.13681984861663E-17));
#124053=DIRECTION('ref_axis',(0.985697438637956,0.16852465535515,-9.24446373305873E-32));
#124054=DIRECTION('center_axis',(-2.0234047869508E-32,3.74576253769986E-32,
-1.));
#124055=DIRECTION('ref_axis',(0.983192890799501,0.182569820839372,-1.30553400632501E-32));
#124056=DIRECTION('center_axis',(0.196577826165713,-0.980488224437174,-3.46966352979465E-16));
#124057=DIRECTION('ref_axis',(-0.980488224437174,-0.196577826165713,7.88510670898544E-14));
#124058=DIRECTION('center_axis',(-2.04729735730373E-32,3.91193901461487E-32,
-1.));
#124059=DIRECTION('ref_axis',(0.994802532857003,0.101822986703845,0.));
#124060=DIRECTION('center_axis',(2.04729735730373E-32,-3.91193901461487E-32,
1.));
#124061=DIRECTION('ref_axis',(-0.994802532857003,-0.101822986703845,1.63833128228582E-32));
#124062=DIRECTION('center_axis',(0.0876204114492056,-0.996153935643218,
6.13681984861663E-17));
#124063=DIRECTION('ref_axis',(0.996153935643218,0.0876204114492056,7.70371977754894E-34));
#124064=DIRECTION('center_axis',(-2.04729735730373E-32,3.91193901461487E-32,
-1.));
#124065=DIRECTION('ref_axis',(0.994802532857003,0.101822986703845,-1.63833128228582E-32));
#124066=DIRECTION('center_axis',(0.116004836965469,-0.993248648526951,-3.46966352979465E-16));
#124067=DIRECTION('ref_axis',(-0.993248648526951,-0.116004836965469,7.88510670898549E-14));
#124068=DIRECTION('center_axis',(-2.0575655015241E-32,4.07951001930311E-32,
-1.));
#124069=DIRECTION('ref_axis',(0.999791928189206,0.0203985373914152,0.));
#124070=DIRECTION('center_axis',(2.0575655015241E-32,-4.07951001930311E-32,
1.));
#124071=DIRECTION('ref_axis',(-0.999791928189206,-0.0203985373914152,1.97392134247697E-32));
#124072=DIRECTION('center_axis',(0.00613306816141749,-0.999981192560604,
6.13681984861663E-17));
#124073=DIRECTION('ref_axis',(0.999981192560604,0.0061330681614175,-3.37037740267766E-33));
#124074=DIRECTION('center_axis',(-2.0575655015241E-32,4.07951001930311E-32,
-1.));
#124075=DIRECTION('ref_axis',(0.999791928189206,0.0203985373914152,-1.97392134247697E-32));
#124076=DIRECTION('center_axis',(0.0346598547146713,-0.999399166735273,
-3.46966352979465E-16));
#124077=DIRECTION('ref_axis',(-0.999399166735273,-0.0346598547146713,7.88510670898555E-14));
#124078=DIRECTION('center_axis',(-2.05414088680624E-32,4.24736039437564E-32,
-1.));
#124079=DIRECTION('ref_axis',(0.998127873193367,-0.061161660821833,0.));
#124080=DIRECTION('center_axis',(2.05414088680624E-32,-4.24736039437564E-32,
1.));
#124081=DIRECTION('ref_axis',(-0.998127873193367,0.061161660821833,2.31007089041634E-32));
#124082=DIRECTION('center_axis',(-0.0753950896830998,-0.997153739626783,
6.13681984861663E-17));
#124083=DIRECTION('ref_axis',(0.997153739626783,-0.0753950896830998,3.38963670212153E-32));
#124084=DIRECTION('center_axis',(-2.05414088680624E-32,4.24736039437564E-32,
-1.));
#124085=DIRECTION('ref_axis',(0.998127873193367,-0.061161660821833,-2.31007089041634E-32));
#124086=DIRECTION('center_axis',(-0.0469157831507791,-0.998898848378228,
-3.46966352979465E-16));
#124087=DIRECTION('ref_axis',(-0.998898848378228,0.0469157831507791,7.88510670898549E-14));
#124088=DIRECTION('center_axis',(-2.03704630339607E-32,4.41437312327972E-32,
-1.));
#124089=DIRECTION('ref_axis',(0.989821441880934,-0.142314838273276,0.));
#124090=DIRECTION('center_axis',(2.03704630339607E-32,-4.41437312327972E-32,
1.));
#124091=DIRECTION('ref_axis',(-0.989821441880934,0.142314838273276,2.64454290632317E-32));
#124092=DIRECTION('center_axis',(-0.15642150564509,-0.987690393074532,6.13681984861663E-17));
#124093=DIRECTION('ref_axis',(0.987690393074532,-0.15642150564509,1.55615139506489E-31));
#124094=DIRECTION('center_axis',(-2.03704630339607E-32,4.41437312327972E-32,
-1.));
#124095=DIRECTION('ref_axis',(0.989821441880934,-0.142314838273276,-2.64454290632317E-32));
#124096=DIRECTION('center_axis',(-0.12817920421992,-0.991751022991934,-3.46966352979465E-16));
#124097=DIRECTION('ref_axis',(-0.991751022991934,0.12817920421992,7.88510670898542E-14));
#124098=DIRECTION('center_axis',(-2.00639551292579E-32,4.57943676385965E-32,
-1.));
#124099=DIRECTION('ref_axis',(0.974927912181826,-0.222520933956305,0.));
#124100=DIRECTION('center_axis',(2.00639551292579E-32,-4.57943676385965E-32,
1.));
#124101=DIRECTION('ref_axis',(-0.974927912181826,0.222520933956305,2.97511153411561E-32));
#124102=DIRECTION('center_axis',(-0.236406962294745,-0.971654129913814,
6.13681984861663E-17));
#124103=DIRECTION('ref_axis',(0.971654129913814,-0.236406962294745,-1.72563323017096E-31));
#124104=DIRECTION('center_axis',(-2.00639551292579E-32,4.57943676385965E-32,
-1.));
#124105=DIRECTION('ref_axis',(0.974927912181826,-0.222520933956305,-2.97511153411561E-32));
#124106=DIRECTION('center_axis',(-0.208589613833058,-0.978003258175031,
-3.46966352979465E-16));
#124107=DIRECTION('ref_axis',(-0.978003258175031,0.208589613833058,7.88510670898555E-14));
#124108=DIRECTION('center_axis',(-1.96239249134894E-32,4.74145284482097E-32,
-1.));
#124109=DIRECTION('ref_axis',(0.953546398078931,-0.301246189537225,0.));
#124110=DIRECTION('center_axis',(1.96239249134894E-32,-4.74145284482097E-32,
1.));
#124111=DIRECTION('ref_axis',(-0.95354639807893,0.301246189537225,3.29957689411567E-32));
#124112=DIRECTION('center_axis',(-0.31481916961473,-0.949151668830167,6.13681984861663E-17));
#124113=DIRECTION('ref_axis',(0.949151668830167,-0.31481916961473,-1.72563323017096E-31));
#124114=DIRECTION('center_axis',(-1.96239249134894E-32,4.74145284482097E-32,
-1.));
#124115=DIRECTION('ref_axis',(0.953546398078931,-0.301246189537225,-3.29957689411567E-32));
#124116=DIRECTION('center_axis',(-0.287611893981001,-0.957747043034152,
-3.46966352979465E-16));
#124117=DIRECTION('ref_axis',(-0.957747043034152,0.287611893981001,7.88510670898555E-14));
#124118=DIRECTION('center_axis',(-1.90533007151413E-32,4.89934317587563E-32,
-1.));
#124119=DIRECTION('ref_axis',(0.925819190020902,-0.377966701428898,0.));
#124120=DIRECTION('center_axis',(1.90533007151413E-32,-4.89934317587563E-32,
1.));
#124121=DIRECTION('ref_axis',(-0.925819190020902,0.377966701428898,3.61577972288558E-32));
#124122=DIRECTION('center_axis',(-0.391136307302437,-0.920332759989458,
6.13681984861663E-17));
#124123=DIRECTION('ref_axis',(0.920332759989458,-0.391136307302437,2.61926472436664E-31));
#124124=DIRECTION('center_axis',(-1.90533007151413E-32,4.89934317587563E-32,
-1.));
#124125=DIRECTION('ref_axis',(0.925819190020902,-0.377966701428898,-3.61577972288558E-32));
#124126=DIRECTION('center_axis',(-0.364720164427122,-0.93111717933902,-3.46966352979465E-16));
#124127=DIRECTION('ref_axis',(-0.93111717933902,0.364720164427122,7.88510670898555E-14));
#124128=DIRECTION('center_axis',(-1.83558799441074E-32,5.05205702292055E-32,
-1.));
#124129=DIRECTION('ref_axis',(0.891930808002698,-0.452171907282677,0.));
#124130=DIRECTION('center_axis',(1.83558799441074E-32,-5.05205702292055E-32,
1.));
#124131=DIRECTION('ref_axis',(-0.891930808002698,0.452171907282677,3.92161574276965E-32));
#124132=DIRECTION('center_axis',(-0.464850497397995,-0.885389188475236,
6.13681984861663E-17));
#124133=DIRECTION('ref_axis',(0.885389188475236,-0.464850497397995,-2.8965986363584E-31));
#124134=DIRECTION('center_axis',(-1.83558799441074E-32,5.05205702292055E-32,
-1.));
#124135=DIRECTION('ref_axis',(0.891930808002698,-0.452171907282677,-3.92161574276965E-32));
#124136=DIRECTION('center_axis',(-0.439401282353573,-0.898290884438908,
-3.46966352979465E-16));
#124137=DIRECTION('ref_axis',(-0.898290884438908,0.439401282353573,1.57702134179708E-13));
#124138=DIRECTION('center_axis',(-1.75363038205524E-32,5.19857810049965E-32,
-1.));
#124139=DIRECTION('ref_axis',(0.852106773615461,-0.523367983696604,0.));
#124140=DIRECTION('center_axis',(1.75363038205524E-32,-5.19857810049965E-32,
1.));
#124141=DIRECTION('ref_axis',(-0.852106773615461,0.523367983696604,4.21504966551496E-32));
#124142=DIRECTION('center_axis',(-0.535471184128302,-0.844553497990645,
6.13681984861663E-17));
#124143=DIRECTION('ref_axis',(0.844553497990645,-0.535471184128302,-4.93038065763132E-32));
#124144=DIRECTION('center_axis',(-1.75363038205524E-32,5.19857810049965E-32,
-1.));
#124145=DIRECTION('ref_axis',(0.852106773615461,-0.523367983696604,-4.21504966551496E-32));
#124146=DIRECTION('center_axis',(-0.511158257242069,-0.859486611910419,
-3.46966352979465E-16));
#124147=DIRECTION('ref_axis',(-0.859486611910419,0.511158257242069,7.88510670898547E-14));
#124148=DIRECTION('center_axis',(-1.66000264883581E-32,5.33793133501592E-32,
-1.));
#124149=DIRECTION('ref_axis',(0.806612109237535,-0.59108113252867,0.));
#124150=DIRECTION('center_axis',(1.66000264883581E-32,-5.33793133501592E-32,
1.));
#124151=DIRECTION('ref_axis',(-0.806612109237535,0.59108113252867,4.49412873677883E-32));
#124152=DIRECTION('center_axis',(-0.602528398474762,-0.798097443318445,
6.13681984861663E-17));
#124153=DIRECTION('ref_axis',(0.798097443318445,-0.602528398474762,-2.65007960347684E-31));
#124154=DIRECTION('center_axis',(-1.66000264883581E-32,5.33793133501592E-32,
-1.));
#124155=DIRECTION('ref_axis',(0.806612109237535,-0.59108113252867,-4.49412873677883E-32));
#124156=DIRECTION('center_axis',(-0.579513558263796,-0.814962597784975,
-3.46966352979465E-16));
#124157=DIRECTION('ref_axis',(-0.814962597784975,0.579513558263796,7.88510670898541E-14));
#124158=DIRECTION('center_axis',(-1.55532787186954E-32,5.46918935368532E-32,
-1.));
#124159=DIRECTION('ref_axis',(0.755749574354264,-0.654860733945279,0.));
#124160=DIRECTION('center_axis',(1.55532787186954E-32,-5.46918935368532E-32,
1.));
#124161=DIRECTION('ref_axis',(-0.755749574354264,0.654860733945279,4.7569957313868E-32));
#124162=DIRECTION('center_axis',(-0.665575885739561,-0.74633018183777,6.13681984861663E-17));
#124163=DIRECTION('ref_axis',(0.74633018183777,-0.665575885739561,3.14311766923997E-31));
#124164=DIRECTION('center_axis',(-1.55532787186954E-32,5.46918935368532E-32,
-1.));
#124165=DIRECTION('ref_axis',(0.755749574354264,-0.654860733945279,-4.7569957313868E-32));
#124166=DIRECTION('center_axis',(-0.644012292168283,-0.765015142030636,
-3.46966352979465E-16));
#124167=DIRECTION('ref_axis',(-0.765015142030636,0.644012292168283,7.88510670898549E-14));
#124168=DIRECTION('center_axis',(-1.44030264452701E-32,5.59147865604965E-32,
-1.));
#124169=DIRECTION('ref_axis',(0.699857650743568,-0.714282345221898,0.));
#124170=DIRECTION('center_axis',(1.44030264452701E-32,-5.59147865604965E-32,
1.));
#124171=DIRECTION('ref_axis',(-0.699857650743568,0.714282345221898,5.00190131285975E-32));
#124172=DIRECTION('center_axis',(-0.724194075297055,-0.689596216132777,
6.13681984861663E-17));
#124173=DIRECTION('ref_axis',(0.689596216132777,-0.724194075297054,7.39557098644698E-32));
#124174=DIRECTION('center_axis',(-1.44030264452701E-32,5.59147865604965E-32,
-1.));
#124175=DIRECTION('ref_axis',(0.699857650743568,-0.714282345221898,-5.00190131285975E-32));
#124176=DIRECTION('center_axis',(-0.70422523052294,-0.709976636724697,-3.46966352979465E-16));
#124177=DIRECTION('ref_axis',(-0.709976636724697,0.704225230522939,7.88510670898545E-14));
#124178=DIRECTION('center_axis',(-1.31569244071836E-32,5.70398542697799E-32,
-1.));
#124179=DIRECTION('ref_axis',(0.639308289935558,-0.768950525339357,0.));
#124180=DIRECTION('center_axis',(1.31569244071836E-32,-5.70398542697799E-32,
1.));
#124181=DIRECTION('ref_axis',(-0.639308289935558,0.768950525339357,5.22721567495956E-32));
#124182=DIRECTION('center_axis',(-0.777992872767058,-0.628273101384788,
6.13681984861663E-17));
#124183=DIRECTION('ref_axis',(0.628273101384788,-0.777992872767058,-1.41748443906901E-31));
#124184=DIRECTION('center_axis',(-1.31569244071836E-32,5.70398542697799E-32,
-1.));
#124185=DIRECTION('ref_axis',(0.639308289935558,-0.768950525339357,-5.22721567495956E-32));
#124186=DIRECTION('center_axis',(-0.75975166615745,-0.650213354039255,-3.46966352979465E-16));
#124187=DIRECTION('ref_axis',(-0.650213354039255,0.75975166615745,7.88510670898545E-14));
#124188=DIRECTION('center_axis',(-1.18232652079071E-32,5.80596095247213E-32,
-1.));
#124189=DIRECTION('ref_axis',(0.57450443793647,-0.818501466578589,0.));
#124190=DIRECTION('center_axis',(1.18232652079071E-32,-5.80596095247213E-32,
1.));
#124191=DIRECTION('ref_axis',(-0.57450443793647,0.818501466578589,5.43143938778071E-32));
#124192=DIRECTION('center_axis',(-0.826614256028586,-0.562768932804849,
6.13681984861663E-17));
#124193=DIRECTION('ref_axis',(0.562768932804848,-0.826614256028586,-3.82104500966428E-31));
#124194=DIRECTION('center_axis',(-1.18232652079071E-32,5.80596095247213E-32,
-1.));
#124195=DIRECTION('ref_axis',(0.57450443793647,-0.818501466578589,-5.43143938778071E-32));
#124196=DIRECTION('center_axis',(-0.810222079803885,-0.586123008760335,
-3.46966352979465E-16));
#124197=DIRECTION('ref_axis',(-0.586123008760335,0.810222079803885,1.5770213417971E-13));
#124198=DIRECTION('center_axis',(-1.04109241293733E-32,5.89672660223468E-32,
-1.));
#124199=DIRECTION('ref_axis',(0.505877353689475,-0.862605415600977,0.));
#124200=DIRECTION('center_axis',(1.04109241293733E-32,-5.89672660223468E-32,
1.));
#124201=DIRECTION('ref_axis',(-0.505877353689475,0.862605415600977,5.61321337620891E-32));
#124202=DIRECTION('center_axis',(-0.869734657797995,-0.493519629827431,
6.13681984861663E-17));
#124203=DIRECTION('ref_axis',(0.493519629827431,-0.869734657797995,2.65007960347684E-31));
#124204=DIRECTION('center_axis',(-1.04109241293733E-32,5.89672660223468E-32,
-1.));
#124205=DIRECTION('ref_axis',(0.505877353689475,-0.862605415600977,-5.61321337620891E-32));
#124206=DIRECTION('center_axis',(-0.855300599186458,-0.518132111561603,
-3.46966352979465E-16));
#124207=DIRECTION('ref_axis',(-0.518132111561603,0.855300599186458,7.88510670898553E-14));
#124208=DIRECTION('center_axis',(-8.92930006844022E-33,5.97567834584174E-32,
-1.));
#124209=DIRECTION('ref_axis',(0.433883739117565,-0.900968867902416,0.));
#124210=DIRECTION('center_axis',(8.92930006844022E-33,-5.97567834584174E-32,
1.));
#124211=DIRECTION('ref_axis',(-0.433883739117565,0.900968867902416,5.77132796434177E-32));
#124212=DIRECTION('center_axis',(-0.907067118915877,-0.420986035138519,
6.13681984861663E-17));
#124213=DIRECTION('ref_axis',(0.420986035138519,-0.907067118915877,2.40356057059527E-31));
#124214=DIRECTION('center_axis',(-8.92930006844022E-33,5.97567834584174E-32,
-1.));
#124215=DIRECTION('ref_axis',(0.433883739117565,-0.900968867902416,-5.77132796434177E-32));
#124216=DIRECTION('center_axis',(-0.894687234196112,-0.44669313064621,-3.46966352979465E-16));
#124217=DIRECTION('ref_axis',(-0.44669313064621,0.894687234196112,7.88510670898555E-14));
#124218=DIRECTION('center_axis',(-7.38825298878243E-33,6.04229077246574E-32,
-1.));
#124219=DIRECTION('ref_axis',(0.359002699847606,-0.933336521037364,0.));
#124220=DIRECTION('center_axis',(7.38825298878243E-33,-6.04229077246574E-32,
1.));
#124221=DIRECTION('ref_axis',(-0.359002699847605,0.933336521037364,5.90473092568234E-32));
#124222=DIRECTION('center_axis',(-0.938363198012914,-0.345650847843566,
6.13681984861663E-17));
#124223=DIRECTION('ref_axis',(0.345650847843566,-0.938363198012914,-1.14015052707724E-31));
#124224=DIRECTION('center_axis',(-7.38825298878243E-33,6.04229077246574E-32,
-1.));
#124225=DIRECTION('ref_axis',(0.359002699847606,-0.933336521037364,-5.90473092568234E-32));
#124226=DIRECTION('center_axis',(-0.928119873275193,-0.372281480645545,
-3.46966352979465E-16));
#124227=DIRECTION('ref_axis',(-0.372281480645545,0.928119873275193,7.88510670898547E-14));
#124228=DIRECTION('center_axis',(-5.79803830446025E-33,6.09612058739776E-32,
-1.));
#124229=DIRECTION('ref_axis',(0.281732556841437,-0.959492973614495,0.));
#124230=DIRECTION('center_axis',(5.79803830446025E-33,-6.09612058739776E-32,
1.));
#124231=DIRECTION('ref_axis',(-0.281732556841437,0.959492973614495,6.01253448553284E-32));
#124232=DIRECTION('center_axis',(-0.963414624846205,-0.268015411184591,
6.13681984861663E-17));
#124233=DIRECTION('ref_axis',(0.268015411184591,-0.963414624846205,-6.16297582203915E-32));
#124234=DIRECTION('center_axis',(-5.79803830446025E-33,6.09612058739776E-32,
-1.));
#124235=DIRECTION('ref_axis',(0.281732556841437,-0.959492973614495,-6.01253448553284E-32));
#124236=DIRECTION('center_axis',(-0.955376027726628,-0.295392358813306,
-3.46966352979465E-16));
#124237=DIRECTION('ref_axis',(-0.295392358813306,0.955376027726628,1.35585468084861E-30));
#124238=DIRECTION('center_axis',(-4.16923863183086E-33,6.13680956210074E-32,
-1.));
#124239=DIRECTION('ref_axis',(0.202587530152088,-0.97926415875742,0.));
#124240=DIRECTION('center_axis',(4.16923863183086E-33,-6.13680956210074E-32,
1.));
#124241=DIRECTION('ref_axis',(-0.202587530152088,0.97926415875742,6.0940212289888E-32));
#124242=DIRECTION('center_axis',(-0.982054686303369,-0.188596376183613,
6.13681984861663E-17));
#124243=DIRECTION('ref_axis',(0.188596376183613,-0.982054686303369,4.62223186652937E-32));
#124244=DIRECTION('center_axis',(-4.16923863183086E-33,6.13680956210074E-32,
-1.));
#124245=DIRECTION('ref_axis',(0.202587530152088,-0.97926415875742,-6.0940212289888E-32));
#124246=DIRECTION('center_axis',(-0.976274312339492,-0.216537449569472,
-3.46966352979465E-16));
#124247=DIRECTION('ref_axis',(-0.216537449569472,0.976274312339492,7.88510670898554E-14));
#124248=DIRECTION('center_axis',(-2.51269336398259E-33,6.16408691816122E-32,
-1.));
#124249=DIRECTION('ref_axis',(0.122094316874167,-0.992518502491027,0.));
#124250=DIRECTION('center_axis',(2.51269336398259E-33,-6.16408691816122E-32,
1.));
#124251=DIRECTION('ref_axis',(-0.122094316874167,0.992518502491027,6.14864887521687E-32));
#124252=DIRECTION('center_axis',(-0.994159335850803,-0.107922263415344,
6.13681984861663E-17));
#124253=DIRECTION('ref_axis',(0.107922263415344,-0.994159335850803,4.16000867987643E-32));
#124254=DIRECTION('center_axis',(-2.51269336398259E-33,6.16408691816122E-32,
-1.));
#124255=DIRECTION('ref_axis',(0.122094316874167,-0.992518502491027,-6.14864887521687E-32));
#124256=DIRECTION('center_axis',(-0.99067565247766,-0.136241519324918,-3.46966352979465E-16));
#124257=DIRECTION('ref_axis',(-0.136241519324918,0.99067565247766,1.5770213417971E-13));
#124258=DIRECTION('center_axis',(-8.39426536362247E-34,6.17777112927507E-32,
-1.));
#124259=DIRECTION('ref_axis',(0.0407885860615926,-0.999167799344583,0.));
#124260=DIRECTION('center_axis',(8.39426536362247E-34,-6.17777112927507E-32,
1.));
#124261=DIRECTION('ref_axis',(-0.0407885860615926,0.999167799344583,6.17605388624435E-32));
#124262=DIRECTION('center_axis',(-0.999648019042894,-0.0265299457899662,
6.13681984861663E-17));
#124263=DIRECTION('ref_axis',(0.0265299457899662,-0.999648019042894,1.63704045272915E-32));
#124264=DIRECTION('center_axis',(-8.39426536362247E-34,6.17777112927507E-32,
-1.));
#124265=DIRECTION('ref_axis',(0.0407885860615926,-0.999167799344583,-6.17605388624435E-32));
#124266=DIRECTION('center_axis',(-0.998484209598567,-0.055038924247525,
-3.46966352979465E-16));
#124267=DIRECTION('ref_axis',(-0.055038924247525,0.998484209598567,7.88510670898542E-14));
#124268=DIRECTION('center_axis',(8.39426536361969E-34,6.17777112927507E-32,
-1.));
#124269=DIRECTION('ref_axis',(-0.0407885860615791,-0.999167799344583,0.));
#124270=DIRECTION('center_axis',(-8.39426536361969E-34,-6.17777112927507E-32,
1.));
#124271=DIRECTION('ref_axis',(0.0407885860615791,0.999167799344583,6.17605388624435E-32));
#124272=DIRECTION('center_axis',(-0.998484209598568,0.0550389242475112,
6.13681984861663E-17));
#124273=DIRECTION('ref_axis',(-0.0550389242475112,-0.998484209598568,-1.00148357108136E-32));
#124274=DIRECTION('center_axis',(8.39426536361969E-34,6.17777112927507E-32,
-1.));
#124275=DIRECTION('ref_axis',(-0.0407885860615791,-0.999167799344583,-6.17605388624435E-32));
#124276=DIRECTION('center_axis',(-0.999648019042894,0.0265299457899523,
-3.46966352979465E-16));
#124277=DIRECTION('ref_axis',(0.0265299457899523,0.999648019042894,7.88510670898553E-14));
#124278=DIRECTION('center_axis',(2.51269336398232E-33,6.16408691816122E-32,
-1.));
#124279=DIRECTION('ref_axis',(-0.122094316874153,-0.992518502491029,0.));
#124280=DIRECTION('center_axis',(-2.51269336398232E-33,-6.16408691816122E-32,
1.));
#124281=DIRECTION('ref_axis',(0.122094316874153,0.992518502491029,6.14864887521688E-32));
#124282=DIRECTION('center_axis',(-0.990675652477662,0.136241519324904,6.13681984861664E-17));
#124283=DIRECTION('ref_axis',(-0.136241519324904,-0.990675652477662,-5.54667823983524E-32));
#124284=DIRECTION('center_axis',(2.51269336398232E-33,6.16408691816122E-32,
-1.));
#124285=DIRECTION('ref_axis',(-0.122094316874153,-0.992518502491028,-6.14864887521688E-32));
#124286=DIRECTION('center_axis',(-0.994159335850804,0.10792226341533,-3.46966352979465E-16));
#124287=DIRECTION('ref_axis',(0.10792226341533,0.994159335850804,7.88510670898554E-14));
#124288=DIRECTION('center_axis',(4.16923863183059E-33,6.13680956210074E-32,
-1.));
#124289=DIRECTION('ref_axis',(-0.202587530152075,-0.979264158757422,0.));
#124290=DIRECTION('center_axis',(-4.16923863183059E-33,-6.13680956210074E-32,
1.));
#124291=DIRECTION('ref_axis',(0.202587530152075,0.979264158757422,6.09402122898881E-32));
#124292=DIRECTION('center_axis',(-0.976274312339495,0.216537449569458,6.13681984861664E-17));
#124293=DIRECTION('ref_axis',(-0.216537449569458,-0.976274312339495,1.38666955995881E-32));
#124294=DIRECTION('center_axis',(4.16923863183059E-33,6.13680956210074E-32,
-1.));
#124295=DIRECTION('ref_axis',(-0.202587530152075,-0.979264158757422,-6.09402122898881E-32));
#124296=DIRECTION('center_axis',(-0.982054686303372,0.188596376183599,-3.46966352979465E-16));
#124297=DIRECTION('ref_axis',(0.188596376183599,0.982054686303372,7.88510670898547E-14));
#124298=DIRECTION('center_axis',(5.79803830445998E-33,6.09612058739777E-32,
-1.));
#124299=DIRECTION('ref_axis',(-0.281732556841424,-0.959492973614499,0.));
#124300=DIRECTION('center_axis',(-5.79803830445998E-33,-6.09612058739777E-32,
1.));
#124301=DIRECTION('ref_axis',(0.281732556841424,0.959492973614499,6.01253448553286E-32));
#124302=DIRECTION('center_axis',(-0.955376027726632,0.295392358813292,6.13681984861664E-17));
#124303=DIRECTION('ref_axis',(-0.295392358813292,-0.955376027726632,1.32503980173842E-31));
#124304=DIRECTION('center_axis',(5.79803830445998E-33,6.09612058739777E-32,
-1.));
#124305=DIRECTION('ref_axis',(-0.281732556841424,-0.959492973614499,-6.01253448553286E-32));
#124306=DIRECTION('center_axis',(-0.963414624846209,0.268015411184578,-3.46966352979465E-16));
#124307=DIRECTION('ref_axis',(0.268015411184578,0.963414624846209,7.88510670898549E-14));
#124308=DIRECTION('center_axis',(7.38825298878218E-33,6.04229077246575E-32,
-1.));
#124309=DIRECTION('ref_axis',(-0.359002699847593,-0.933336521037369,0.));
#124310=DIRECTION('center_axis',(-7.38825298878218E-33,-6.04229077246575E-32,
1.));
#124311=DIRECTION('ref_axis',(0.359002699847593,0.933336521037369,5.90473092568236E-32));
#124312=DIRECTION('center_axis',(-0.928119873275198,0.372281480645533,6.13681984861664E-17));
#124313=DIRECTION('ref_axis',(-0.372281480645533,-0.928119873275198,-1.14015052707724E-31));
#124314=DIRECTION('center_axis',(7.38825298878218E-33,6.04229077246575E-32,
-1.));
#124315=DIRECTION('ref_axis',(-0.359002699847593,-0.933336521037369,-5.90473092568236E-32));
#124316=DIRECTION('center_axis',(-0.938363198012919,0.345650847843554,-3.46966352979465E-16));
#124317=DIRECTION('ref_axis',(0.345650847843554,0.938363198012919,7.88510670898547E-14));
#124318=DIRECTION('center_axis',(8.92930006843997E-33,5.97567834584175E-32,
-1.));
#124319=DIRECTION('ref_axis',(-0.433883739117553,-0.900968867902422,0.));
#124320=DIRECTION('center_axis',(-8.92930006843997E-33,-5.97567834584175E-32,
1.));
#124321=DIRECTION('ref_axis',(0.433883739117553,0.900968867902422,5.7713279643418E-32));
#124322=DIRECTION('center_axis',(-0.894687234196118,0.446693130646198,6.13681984861664E-17));
#124323=DIRECTION('ref_axis',(-0.446693130646198,-0.894687234196118,4.00593428432545E-32));
#124324=DIRECTION('center_axis',(8.92930006843997E-33,5.97567834584175E-32,
-1.));
#124325=DIRECTION('ref_axis',(-0.433883739117553,-0.900968867902422,-5.7713279643418E-32));
#124326=DIRECTION('center_axis',(-0.907067118915883,0.420986035138506,-3.46966352979465E-16));
#124327=DIRECTION('ref_axis',(0.420986035138506,0.907067118915883,7.88510670898557E-14));
#124328=DIRECTION('center_axis',(1.04109241293731E-32,5.89672660223469E-32,
-1.));
#124329=DIRECTION('ref_axis',(-0.505877353689464,-0.862605415600984,0.));
#124330=DIRECTION('center_axis',(-1.04109241293731E-32,-5.89672660223469E-32,
1.));
#124331=DIRECTION('ref_axis',(0.505877353689463,0.862605415600983,5.61321337620894E-32));
#124332=DIRECTION('center_axis',(-0.855300599186466,0.518132111561591,6.13681984861664E-17));
#124333=DIRECTION('ref_axis',(-0.518132111561591,-0.855300599186465,4.00593428432545E-32));
#124334=DIRECTION('center_axis',(1.04109241293731E-32,5.89672660223469E-32,
-1.));
#124335=DIRECTION('ref_axis',(-0.505877353689463,-0.862605415600984,-5.61321337620894E-32));
#124336=DIRECTION('center_axis',(-0.869734657798002,0.493519629827419,-3.46966352979465E-16));
#124337=DIRECTION('ref_axis',(0.493519629827419,0.869734657798002,2.95822839457879E-30));
#124338=DIRECTION('center_axis',(1.18232652079068E-32,5.80596095247215E-32,
-1.));
#124339=DIRECTION('ref_axis',(-0.574504437936459,-0.818501466578597,0.));
#124340=DIRECTION('center_axis',(-1.18232652079068E-32,-5.80596095247215E-32,
1.));
#124341=DIRECTION('ref_axis',(0.574504437936459,0.818501466578597,5.43143938778074E-32));
#124342=DIRECTION('center_axis',(-0.810222079803893,0.586123008760323,6.13681984861664E-17));
#124343=DIRECTION('ref_axis',(-0.586123008760323,-0.810222079803893,1.91052250483214E-31));
#124344=DIRECTION('center_axis',(1.18232652079068E-32,5.80596095247215E-32,
-1.));
#124345=DIRECTION('ref_axis',(-0.574504437936459,-0.818501466578597,-5.43143938778074E-32));
#124346=DIRECTION('center_axis',(-0.826614256028593,0.562768932804837,-3.46966352979465E-16));
#124347=DIRECTION('ref_axis',(0.562768932804837,0.826614256028593,7.8851067089855E-14));
#124348=DIRECTION('center_axis',(1.31569244071834E-32,5.70398542697801E-32,
-1.));
#124349=DIRECTION('ref_axis',(-0.639308289935547,-0.768950525339365,0.));
#124350=DIRECTION('center_axis',(-1.31569244071834E-32,-5.70398542697801E-32,
1.));
#124351=DIRECTION('ref_axis',(0.639308289935547,0.768950525339365,5.22721567495959E-32));
#124352=DIRECTION('center_axis',(-0.759751666157459,0.650213354039245,6.13681984861664E-17));
#124353=DIRECTION('ref_axis',(-0.650213354039245,-0.759751666157459,2.1570415377137E-31));
#124354=DIRECTION('center_axis',(1.31569244071834E-32,5.70398542697801E-32,
-1.));
#124355=DIRECTION('ref_axis',(-0.639308289935547,-0.768950525339365,-5.22721567495959E-32));
#124356=DIRECTION('center_axis',(-0.777992872767067,0.628273101384777,-3.46966352979465E-16));
#124357=DIRECTION('ref_axis',(0.628273101384777,0.777992872767067,7.88510670898555E-14));
#124358=DIRECTION('center_axis',(1.44030264452699E-32,5.59147865604967E-32,
-1.));
#124359=DIRECTION('ref_axis',(-0.699857650743558,-0.714282345221907,0.));
#124360=DIRECTION('center_axis',(-1.44030264452699E-32,-5.59147865604967E-32,
1.));
#124361=DIRECTION('ref_axis',(0.699857650743558,0.714282345221907,5.00190131285979E-32));
#124362=DIRECTION('center_axis',(-0.704225230522949,0.709976636724688,6.13681984861664E-17));
#124363=DIRECTION('ref_axis',(-0.709976636724688,-0.704225230522949,-8.0118685686509E-32));
#124364=DIRECTION('center_axis',(1.44030264452699E-32,5.59147865604967E-32,
-1.));
#124365=DIRECTION('ref_axis',(-0.699857650743558,-0.714282345221907,-5.00190131285979E-32));
#124366=DIRECTION('center_axis',(-0.724194075297064,0.689596216132768,-3.46966352979465E-16));
#124367=DIRECTION('ref_axis',(0.689596216132768,0.724194075297064,2.12006368278147E-30));
#124368=DIRECTION('center_axis',(1.55532787186952E-32,5.46918935368534E-32,
-1.));
#124369=DIRECTION('ref_axis',(-0.755749574354255,-0.654860733945289,0.));
#124370=DIRECTION('center_axis',(-1.55532787186952E-32,-5.46918935368534E-32,
1.));
#124371=DIRECTION('ref_axis',(0.755749574354255,0.654860733945289,4.75699573138684E-32));
#124372=DIRECTION('center_axis',(-0.644012292168293,0.765015142030627,6.13681984861664E-17));
#124373=DIRECTION('ref_axis',(-0.765015142030627,-0.644012292168293,-2.46519032881566E-32));
#124374=DIRECTION('center_axis',(1.55532787186952E-32,5.46918935368534E-32,
-1.));
#124375=DIRECTION('ref_axis',(-0.755749574354255,-0.654860733945289,-4.75699573138684E-32));
#124376=DIRECTION('center_axis',(-0.665575885739571,0.746330181837761,-3.46966352979465E-16));
#124377=DIRECTION('ref_axis',(0.746330181837761,0.665575885739571,7.88510670898554E-14));
#124378=DIRECTION('center_axis',(1.66000264883579E-32,5.33793133501594E-32,
-1.));
#124379=DIRECTION('ref_axis',(-0.806612109237527,-0.59108113252868,0.));
#124380=DIRECTION('center_axis',(-1.66000264883579E-32,-5.33793133501594E-32,
1.));
#124381=DIRECTION('ref_axis',(0.806612109237527,0.59108113252868,4.49412873677887E-32));
#124382=DIRECTION('center_axis',(-0.579513558263807,0.814962597784967,6.13681984861664E-17));
#124383=DIRECTION('ref_axis',(-0.814962597784967,-0.579513558263806,2.77333911991762E-31));
#124384=DIRECTION('center_axis',(1.66000264883579E-32,5.33793133501594E-32,
-1.));
#124385=DIRECTION('ref_axis',(-0.806612109237527,-0.59108113252868,-4.49412873677888E-32));
#124386=DIRECTION('center_axis',(-0.602528398474773,0.798097443318436,-3.46966352979465E-16));
#124387=DIRECTION('ref_axis',(0.798097443318437,0.602528398474773,7.88510670898551E-14));
#124388=DIRECTION('center_axis',(1.75363038205522E-32,5.19857810049967E-32,
-1.));
#124389=DIRECTION('ref_axis',(-0.852106773615454,-0.523367983696616,0.));
#124390=DIRECTION('center_axis',(-1.75363038205522E-32,-5.19857810049967E-32,
1.));
#124391=DIRECTION('ref_axis',(0.852106773615454,0.523367983696616,4.21504966551501E-32));
#124392=DIRECTION('center_axis',(-0.511158257242081,0.859486611910412,6.13681984861664E-17));
#124393=DIRECTION('ref_axis',(-0.859486611910412,-0.511158257242081,1.26341004351803E-31));
#124394=DIRECTION('center_axis',(1.75363038205522E-32,5.19857810049967E-32,
-1.));
#124395=DIRECTION('ref_axis',(-0.852106773615454,-0.523367983696616,-4.21504966551501E-32));
#124396=DIRECTION('center_axis',(-0.535471184128314,0.844553497990637,-3.46966352979465E-16));
#124397=DIRECTION('ref_axis',(0.844553497990637,0.535471184128314,7.88510670898547E-14));
#124398=DIRECTION('center_axis',(1.83558799441073E-32,5.05205702292057E-32,
-1.));
#124399=DIRECTION('ref_axis',(-0.891930808002692,-0.452171907282689,0.));
#124400=DIRECTION('center_axis',(-1.83558799441073E-32,-5.05205702292057E-32,
1.));
#124401=DIRECTION('ref_axis',(0.891930808002692,0.452171907282689,3.9216157427697E-32));
#124402=DIRECTION('center_axis',(-0.439401282353585,0.898290884438902,6.13681984861664E-17));
#124403=DIRECTION('ref_axis',(-0.898290884438902,-0.439401282353585,8.32001735975286E-32));
#124404=DIRECTION('center_axis',(1.83558799441073E-32,5.05205702292057E-32,
-1.));
#124405=DIRECTION('ref_axis',(-0.891930808002692,-0.452171907282689,-3.9216157427697E-32));
#124406=DIRECTION('center_axis',(-0.464850497398007,0.88538918847523,-3.46966352979465E-16));
#124407=DIRECTION('ref_axis',(0.88538918847523,0.464850497398007,-1.97215226305253E-31));
#124408=DIRECTION('center_axis',(1.90533007151412E-32,4.89934317587566E-32,
-1.));
#124409=DIRECTION('ref_axis',(-0.925819190020897,-0.37796670142891,0.));
#124410=DIRECTION('center_axis',(-1.90533007151412E-32,-4.89934317587566E-32,
1.));
#124411=DIRECTION('ref_axis',(0.925819190020897,0.37796670142891,3.61577972288563E-32));
#124412=DIRECTION('center_axis',(-0.364720164427135,0.931117179339015,6.13681984861664E-17));
#124413=DIRECTION('ref_axis',(-0.931117179339015,-0.364720164427135,-2.24948617504429E-31));
#124414=DIRECTION('center_axis',(1.90533007151412E-32,4.89934317587566E-32,
-1.));
#124415=DIRECTION('ref_axis',(-0.925819190020897,-0.37796670142891,-3.61577972288563E-32));
#124416=DIRECTION('center_axis',(-0.39113630730245,0.920332759989453,-3.46966352979465E-16));
#124417=DIRECTION('ref_axis',(0.920332759989453,0.39113630730245,7.8851067089854E-14));
#124418=DIRECTION('center_axis',(1.96239249134893E-32,4.74145284482099E-32,
-1.));
#124419=DIRECTION('ref_axis',(-0.953546398078926,-0.301246189537238,0.));
#124420=DIRECTION('center_axis',(-1.96239249134893E-32,-4.74145284482099E-32,
1.));
#124421=DIRECTION('ref_axis',(0.953546398078926,0.301246189537238,3.29957689411572E-32));
#124422=DIRECTION('center_axis',(-0.287611893981014,0.957747043034148,6.13681984861664E-17));
#124423=DIRECTION('ref_axis',(-0.957747043034148,-0.287611893981014,3.69778549322349E-32));
#124424=DIRECTION('center_axis',(1.96239249134893E-32,4.74145284482099E-32,
-1.));
#124425=DIRECTION('ref_axis',(-0.953546398078926,-0.301246189537238,-3.29957689411572E-32));
#124426=DIRECTION('center_axis',(-0.314819169614744,0.949151668830163,-3.46966352979465E-16));
#124427=DIRECTION('ref_axis',(0.949151668830163,0.314819169614744,7.88510670898548E-14));
#124428=DIRECTION('center_axis',(2.00639551292578E-32,4.57943676385968E-32,
-1.));
#124429=DIRECTION('ref_axis',(-0.974927912181823,-0.222520933956318,0.));
#124430=DIRECTION('center_axis',(-2.00639551292578E-32,-4.57943676385968E-32,
1.));
#124431=DIRECTION('ref_axis',(0.974927912181823,0.222520933956318,2.97511153411567E-32));
#124432=DIRECTION('center_axis',(-0.208589613833072,0.978003258175028,6.13681984861664E-17));
#124433=DIRECTION('ref_axis',(-0.978003258175028,-0.208589613833072,-5.0844550531823E-32));
#124434=DIRECTION('center_axis',(2.00639551292578E-32,4.57943676385968E-32,
-1.));
#124435=DIRECTION('ref_axis',(-0.974927912181823,-0.222520933956318,-2.97511153411566E-32));
#124436=DIRECTION('center_axis',(-0.236406962294758,0.971654129913811,-3.46966352979465E-16));
#124437=DIRECTION('ref_axis',(0.971654129913811,0.236406962294758,1.5770213417971E-13));
#124438=DIRECTION('center_axis',(2.03704630339607E-32,4.41437312327975E-32,
-1.));
#124439=DIRECTION('ref_axis',(-0.989821441880932,-0.142314838273289,0.));
#124440=DIRECTION('center_axis',(-2.03704630339607E-32,-4.41437312327975E-32,
1.));
#124441=DIRECTION('ref_axis',(0.989821441880932,0.142314838273289,2.64454290632323E-32));
#124442=DIRECTION('center_axis',(-0.128179204219934,0.991751022991933,6.13681984861664E-17));
#124443=DIRECTION('ref_axis',(-0.991751022991932,-0.128179204219934,4.16000867987643E-32));
#124444=DIRECTION('center_axis',(2.03704630339607E-32,4.41437312327975E-32,
-1.));
#124445=DIRECTION('ref_axis',(-0.989821441880932,-0.142314838273289,-2.64454290632323E-32));
#124446=DIRECTION('center_axis',(-0.156421505645104,0.98769039307453,-3.46966352979465E-16));
#124447=DIRECTION('ref_axis',(0.98769039307453,0.156421505645104,7.88510670898555E-14));
#124448=DIRECTION('center_axis',(2.05414088680624E-32,4.24736039437567E-32,
-1.));
#124449=DIRECTION('ref_axis',(-0.998127873193367,-0.0611616608218463,0.));
#124450=DIRECTION('center_axis',(-2.05414088680624E-32,-4.24736039437567E-32,
1.));
#124451=DIRECTION('ref_axis',(0.998127873193367,0.0611616608218462,2.3100708904164E-32));
#124452=DIRECTION('center_axis',(-0.0469157831507927,0.998898848378227,
6.13681984861664E-17));
#124453=DIRECTION('ref_axis',(-0.998898848378227,-0.0469157831507927,-3.58222969656026E-32));
#124454=DIRECTION('center_axis',(2.05414088680624E-32,4.24736039437567E-32,
-1.));
#124455=DIRECTION('ref_axis',(-0.998127873193367,-0.0611616608218463,-2.3100708904164E-32));
#124456=DIRECTION('center_axis',(-0.0753950896831134,0.997153739626782,
-3.46966352979465E-16));
#124457=DIRECTION('ref_axis',(0.997153739626782,0.0753950896831134,7.88510670898542E-14));
#124458=DIRECTION('center_axis',(2.0575655015241E-32,4.07951001930313E-32,
-1.));
#124459=DIRECTION('ref_axis',(-0.999791928189207,0.0203985373914021,0.));
#124460=DIRECTION('center_axis',(-2.0575655015241E-32,-4.07951001930313E-32,
1.));
#124461=DIRECTION('ref_axis',(0.999791928189207,-0.0203985373914021,1.97392134247702E-32));
#124462=DIRECTION('center_axis',(0.0346598547146579,0.999399166735274,6.13681984861664E-17));
#124463=DIRECTION('ref_axis',(-0.999399166735273,0.0346598547146579,-2.1570415377137E-32));
#124464=DIRECTION('center_axis',(2.0575655015241E-32,4.07951001930313E-32,
-1.));
#124465=DIRECTION('ref_axis',(-0.999791928189207,0.0203985373914021,-1.97392134247702E-32));
#124466=DIRECTION('center_axis',(0.00613306816140406,0.999981192560604,
-3.46966352979465E-16));
#124467=DIRECTION('ref_axis',(0.999981192560604,-0.00613306816140406,7.88510670898547E-14));
#124468=DIRECTION('center_axis',(2.04729735730374E-32,3.9119390146149E-32,
-1.));
#124469=DIRECTION('ref_axis',(-0.994802532857004,0.101822986703832,0.));
#124470=DIRECTION('center_axis',(-2.04729735730374E-32,-3.9119390146149E-32,
1.));
#124471=DIRECTION('ref_axis',(0.994802532857004,-0.101822986703832,1.63833128228587E-32));
#124472=DIRECTION('center_axis',(0.116004836965456,0.993248648526953,6.13681984861664E-17));
#124473=DIRECTION('ref_axis',(-0.993248648526953,0.116004836965456,-7.39557098644699E-32));
#124474=DIRECTION('center_axis',(2.04729735730374E-32,3.9119390146149E-32,
-1.));
#124475=DIRECTION('ref_axis',(-0.994802532857004,0.101822986703832,-1.63833128228587E-32));
#124476=DIRECTION('center_axis',(0.0876204114491922,0.996153935643219,-3.46966352979465E-16));
#124477=DIRECTION('ref_axis',(0.996153935643219,-0.0876204114491922,7.88510670898545E-14));
#124478=DIRECTION('center_axis',(2.0234047869508E-32,3.74576253769989E-32,
-1.));
#124479=DIRECTION('ref_axis',(-0.983192890799504,0.182569820839359,0.));
#124480=DIRECTION('center_axis',(-2.0234047869508E-32,-3.74576253769989E-32,
1.));
#124481=DIRECTION('ref_axis',(0.983192890799504,-0.182569820839359,1.30553400632506E-32));
#124482=DIRECTION('center_axis',(0.1965778261657,0.980488224437177,6.13681984861664E-17));
#124483=DIRECTION('ref_axis',(-0.980488224437177,0.1965778261657,5.54667823983524E-32));
#124484=DIRECTION('center_axis',(2.0234047869508E-32,3.74576253769989E-32,
-1.));
#124485=DIRECTION('ref_axis',(-0.983192890799503,0.182569820839359,-1.30553400632506E-32));
#124486=DIRECTION('center_axis',(0.168524655355137,0.985697438637959,-3.46966352979465E-16));
#124487=DIRECTION('ref_axis',(0.985697438637959,-0.168524655355137,7.88510670898548E-14));
#124488=DIRECTION('center_axis',(1.986046791579E-32,3.58208646559478E-32,
-1.));
#124489=DIRECTION('ref_axis',(-0.965040262269141,0.262101682939099,0.));
#124490=DIRECTION('center_axis',(-1.986046791579E-32,-3.58208646559478E-32,
1.));
#124491=DIRECTION('ref_axis',(0.965040262269141,-0.262101682939099,9.77744225558421E-33));
#124492=DIRECTION('center_axis',(0.275842622365869,0.961202812982942,6.13681984861664E-17));
#124493=DIRECTION('ref_axis',(-0.961202812982942,0.275842622365869,1.41748443906901E-31));
#124494=DIRECTION('center_axis',(1.986046791579E-32,3.58208646559478E-32,
-1.));
#124495=DIRECTION('ref_axis',(-0.965040262269141,0.2621016829391,-9.77744225558421E-33));
#124496=DIRECTION('center_axis',(0.248307395484303,0.968681287807193,-3.46966352979465E-16));
#124497=DIRECTION('ref_axis',(0.968681287807193,-0.248307395484303,1.57702134179711E-13));
#124498=DIRECTION('center_axis',(1.9354719824839E-32,3.42200003555479E-32,
-1.));
#124499=DIRECTION('ref_axis',(-0.940465450013813,0.339889301582614,0.));
#124500=DIRECTION('center_axis',(-1.9354719824839E-32,-3.42200003555479E-32,
1.));
#124501=DIRECTION('ref_axis',(0.940465450013812,-0.339889301582614,6.57143326895444E-33));
#124502=DIRECTION('center_axis',(0.353271731425022,0.935520755395607,6.13681984861664E-17));
#124503=DIRECTION('ref_axis',(-0.935520755395607,0.353271731425022,9.24446373305873E-33));
#124504=DIRECTION('center_axis',(1.9354719824839E-32,3.42200003555479E-32,
-1.));
#124505=DIRECTION('ref_axis',(-0.940465450013812,0.339889301582614,-6.57143326895444E-33));
#124506=DIRECTION('center_axis',(0.326437690864358,0.945218722827233,-3.46966352979465E-16));
#124507=DIRECTION('ref_axis',(0.945218722827233,-0.326437690864358,7.88510670898542E-14));
#124508=DIRECTION('center_axis',(1.87201692667576E-32,3.26656859635943E-32,
-1.));
#124509=DIRECTION('ref_axis',(-0.909631995354519,0.415415013001884,0.));
#124510=DIRECTION('center_axis',(-1.87201692667576E-32,-3.26656859635943E-32,
1.));
#124511=DIRECTION('ref_axis',(0.909631995354519,-0.415415013001884,3.45864856421308E-33));
#124512=DIRECTION('center_axis',(0.428349875397276,0.903612961531174,6.13681984861664E-17));
#124513=DIRECTION('ref_axis',(-0.903612961531174,0.428349875397276,9.55261252416069E-32));
#124514=DIRECTION('center_axis',(1.87201692667576E-32,3.26656859635943E-32,
-1.));
#124515=DIRECTION('ref_axis',(-0.909631995354519,0.415415013001884,-3.45864856421309E-33));
#124516=DIRECTION('center_axis',(0.402395597270139,0.91546588319697,-3.46966352979465E-16));
#124517=DIRECTION('ref_axis',(0.91546588319697,-0.402395597270139,7.88510670898551E-14));
#124518=DIRECTION('center_axis',(1.79610390708165E-32,3.11682651859216E-32,
-1.));
#124519=DIRECTION('ref_axis',(-0.872745089844857,0.488176206048279,0.));
#124520=DIRECTION('center_axis',(-1.79610390708165E-32,-3.11682651859216E-32,
1.));
#124521=DIRECTION('ref_axis',(0.872745089844857,-0.488176206048279,4.59803209996904E-34));
#124522=DIRECTION('center_axis',(0.500577421621515,0.865691772493395,6.13681984861664E-17));
#124523=DIRECTION('ref_axis',(-0.865691772493395,0.500577421621515,3.57452597678271E-31));
#124524=DIRECTION('center_axis',(1.79610390708165E-32,3.11682651859216E-32,
-1.));
#124525=DIRECTION('ref_axis',(-0.872745089844857,0.488176206048279,-4.59803209996901E-34));
#124526=DIRECTION('center_axis',(0.475675627366687,0.87962076915527,-3.46966352979465E-16));
#124527=DIRECTION('ref_axis',(0.87962076915527,-0.475675627366688,1.57702134179709E-13));
#124528=DIRECTION('center_axis',(1.7082381123222E-32,2.97377031107481E-32,
-1.));
#124529=DIRECTION('ref_axis',(-0.830050209755082,0.557688666986828,0.));
#124530=DIRECTION('center_axis',(-1.7082381123222E-32,-2.97377031107481E-32,
1.));
#124531=DIRECTION('ref_axis',(0.830050209755082,-0.557688666986828,-2.40514597263651E-33));
#124532=DIRECTION('center_axis',(0.569473707694324,0.822009547538762,6.13681984861664E-17));
#124533=DIRECTION('ref_axis',(-0.822009547538762,0.569473707694324,3.38963670212154E-31));
#124534=DIRECTION('center_axis',(1.7082381123222E-32,2.97377031107481E-32,
-1.));
#124535=DIRECTION('ref_axis',(-0.830050209755082,0.557688666986828,2.40514597263651E-33));
#124536=DIRECTION('center_axis',(0.545790114644065,0.837921924022053,-3.46966352979465E-16));
#124537=DIRECTION('ref_axis',(0.837921924022053,-0.545790114644065,7.8851067089855E-14));
#124538=DIRECTION('center_axis',(1.60900427476469E-32,2.83835198926582E-32,
-1.));
#124539=DIRECTION('ref_axis',(-0.781831482468031,0.623489801858732,0.));
#124540=DIRECTION('center_axis',(-1.60900427476469E-32,-2.83835198926582E-32,
1.));
#124541=DIRECTION('ref_axis',(0.781831482468031,-0.623489801858732,-5.11713321956004E-33));
#124542=DIRECTION('center_axis',(0.634580240198975,0.772856984667287,6.13681984861664E-17));
#124543=DIRECTION('ref_axis',(-0.772856984667287,0.634580240198975,9.24446373305873E-32));
#124544=DIRECTION('center_axis',(1.60900427476469E-32,2.83835198926582E-32,
-1.));
#124545=DIRECTION('ref_axis',(-0.781831482468031,0.623489801858732,5.11713321956004E-33));
#124546=DIRECTION('center_axis',(0.612272458757516,0.790646846731855,-3.46966352979465E-16));
#124547=DIRECTION('ref_axis',(0.790646846731855,-0.612272458757516,7.8851067089855E-14));
#124548=DIRECTION('center_axis',(1.49906277922564E-32,2.71147273975435E-32,
-1.));
#124549=DIRECTION('ref_axis',(-0.72840979565827,0.685141714967843,0.));
#124550=DIRECTION('center_axis',(-1.49906277922564E-32,-2.71147273975435E-32,
1.));
#124551=DIRECTION('ref_axis',(0.72840979565827,-0.685141714967843,-7.6581107030918E-33));
#124552=DIRECTION('center_axis',(0.695463745903472,0.718561186075278,6.13681984861664E-17));
#124553=DIRECTION('ref_axis',(-0.718561186075278,0.695463745903472,3.45126646034192E-31));
#124554=DIRECTION('center_axis',(1.49906277922564E-32,2.71147273975435E-32,
-1.));
#124555=DIRECTION('ref_axis',(-0.72840979565827,0.685141714967843,7.6581107030918E-33));
#124556=DIRECTION('center_axis',(0.674680230675781,0.738110145124205,-3.46966352979465E-16));
#124557=DIRECTION('ref_axis',(0.738110145124205,-0.674680230675781,7.88510670898546E-14));
#124558=DIRECTION('center_axis',(1.3791452682188E-32,2.59397692301231E-32,
-1.));
#124559=DIRECTION('ref_axis',(-0.670140661837561,0.742234123004269,0.));
#124560=DIRECTION('center_axis',(-1.3791452682188E-32,-2.59397692301231E-32,
1.));
#124561=DIRECTION('ref_axis',(0.670140661837561,-0.742234123004269,-1.00111686373107E-32));
#124562=DIRECTION('center_axis',(0.751719055122423,0.659483481344189,6.13681984861664E-17));
#124563=DIRECTION('ref_axis',(-0.659483481344189,0.751719055122423,-1.66400347195057E-31));
#124564=DIRECTION('center_axis',(1.3791452682188E-32,2.59397692301231E-32,
-1.));
#124565=DIRECTION('ref_axis',(-0.670140661837561,0.742234123004269,1.00111686373107E-32));
#124566=DIRECTION('center_axis',(0.732598116973302,0.680661442280354,-3.46966352979465E-16));
#124567=DIRECTION('ref_axis',(0.680661442280354,-0.732598116973302,-7.64209001932855E-31));
#124568=DIRECTION('center_axis',(1.25004977299491E-32,2.48664645431468E-32,
-1.));
#124569=DIRECTION('ref_axis',(-0.607411852477749,0.794387085412112,0.));
#124570=DIRECTION('center_axis',(-1.25004977299491E-32,-2.48664645431468E-32,
1.));
#124571=DIRECTION('ref_axis',(0.607411852477749,-0.794387085412112,-1.21606478098917E-32));
#124572=DIRECTION('center_axis',(0.802971798054448,0.59601702285187,6.13681984861664E-17));
#124573=DIRECTION('ref_axis',(-0.59601702285187,0.802971798054448,8.0118685686509E-32));
#124574=DIRECTION('center_axis',(1.25004977299491E-32,2.48664645431468E-32,
-1.));
#124575=DIRECTION('ref_axis',(-0.607411852477749,0.794387085412112,1.21606478098917E-32));
#124576=DIRECTION('center_axis',(0.785640683672546,0.618683049839362,-3.46966352979465E-16));
#124577=DIRECTION('ref_axis',(0.618683049839362,-0.785640683672546,7.88510670898545E-14));
#124578=DIRECTION('center_axis',(1.11263540277544E-32,2.39019560022234E-32,
-1.));
#124579=DIRECTION('ref_axis',(-0.540640817455599,0.841253532831181,0.));
#124580=DIRECTION('center_axis',(-1.11263540277544E-32,-2.39019560022234E-32,
1.));
#124581=DIRECTION('ref_axis',(0.540640817455599,-0.841253532831181,-1.40922437915804E-32));
#124582=DIRECTION('center_axis',(0.848880896151442,0.528584169408359,6.13681984861664E-17));
#124583=DIRECTION('ref_axis',(-0.528584169408359,0.848880896151442,4.62223186652936E-32));
#124584=DIRECTION('center_axis',(1.11263540277544E-32,2.39019560022234E-32,
-1.));
#124585=DIRECTION('ref_axis',(-0.540640817455599,0.841253532831181,1.40922437915804E-32));
#124586=DIRECTION('center_axis',(0.833454941243539,0.552587423777206,-3.46966352979465E-16));
#124587=DIRECTION('ref_axis',(0.552587423777206,-0.833454941243539,1.57702134179709E-13));
#124588=DIRECTION('center_axis',(9.67816627522413E-33,2.30526622525603E-32,
-1.));
#124589=DIRECTION('ref_axis',(-0.470271906992738,0.882521576786321,0.));
#124590=DIRECTION('center_axis',(-9.67816627522413E-33,-2.30526622525603E-32,
1.));
#124591=DIRECTION('ref_axis',(0.470271906992738,-0.882521576786321,-1.57931021298095E-32));
#124592=DIRECTION('center_axis',(0.889140831940038,0.457633675527684,6.13681984861664E-17));
#124593=DIRECTION('ref_axis',(-0.457633675527684,0.889140831940038,1.4791141972894E-31));
#124594=DIRECTION('center_axis',(9.67816627522413E-33,2.30526622525603E-32,
-1.));
#124595=DIRECTION('ref_axis',(-0.470271906992738,0.882521576786321,1.57931021298095E-32));
#124596=DIRECTION('center_axis',(0.875722693690941,0.48281441958032,-3.46966352979465E-16));
#124597=DIRECTION('ref_axis',(0.48281441958032,-0.875722693690941,7.88510670898549E-14));
#124598=DIRECTION('center_axis',(8.1655719229173E-33,2.23242352039377E-32,
-1.));
#124599=DIRECTION('ref_axis',(-0.396773414578243,0.917916585253759,0.));
#124600=DIRECTION('center_axis',(-8.1655719229173E-33,-2.23242352039377E-32,
1.));
#124601=DIRECTION('ref_axis',(0.396773414578243,-0.917916585253759,-1.72519038929601E-32));
#124602=DIRECTION('center_axis',(0.923483682189984,0.383637705040614,6.13681984861663E-17));
#124603=DIRECTION('ref_axis',(-0.383637705040614,0.923483682189984,5.54667823983524E-32));
#124604=DIRECTION('center_axis',(8.1655719229173E-33,2.23242352039377E-32,
-1.));
#124605=DIRECTION('ref_axis',(-0.396773414578243,0.917916585253759,1.72519038929601E-32));
#124606=DIRECTION('center_axis',(0.912162656095905,0.4098283650799,-3.46966352979465E-16));
#124607=DIRECTION('ref_axis',(0.4098283650799,-0.912162656095905,7.88510670898547E-14));
#124608=DIRECTION('center_axis',(6.598637036688E-33,2.17215224181823E-32,
-1.));
#124609=DIRECTION('ref_axis',(-0.320634460552736,0.94720301029191,0.));
#124610=DIRECTION('center_axis',(-6.598637036688E-33,-2.17215224181823E-32,
1.));
#124611=DIRECTION('ref_axis',(0.320634460552736,-0.94720301029191,-1.84589409959837E-32));
#124612=DIRECTION('center_axis',(0.951680900899038,0.307088688922265,6.13681984861664E-17));
#124613=DIRECTION('ref_axis',(-0.307088688922265,0.951680900899038,9.24446373305873E-33));
#124614=DIRECTION('center_axis',(6.598637036688E-33,2.17215224181823E-32,
-1.));
#124615=DIRECTION('ref_axis',(-0.320634460552736,0.94720301029191,1.84589409959837E-32));
#124616=DIRECTION('center_axis',(0.942532326520795,0.334114970426793,-3.46966352979465E-16));
#124617=DIRECTION('ref_axis',(0.334114970426793,-0.942532326520795,7.88510670898544E-14));
#124618=DIRECTION('center_axis',(4.98778930967801E-33,2.12485348494426E-32,
-1.));
#124619=DIRECTION('ref_axis',(-0.242361737093213,0.970185955574064,0.));
#124620=DIRECTION('center_axis',(-4.98778930967801E-33,-2.12485348494426E-32,
1.));
#124621=DIRECTION('ref_axis',(0.242361737093213,-0.970185955574064,-1.94061808061067E-32));
#124622=DIRECTION('center_axis',(0.973544840228905,0.228496048245205,6.13681984861664E-17));
#124623=DIRECTION('ref_axis',(-0.228496048245205,0.973544840228905,7.08742219534502E-32));
#124624=DIRECTION('center_axis',(4.98778930967801E-33,2.12485348494426E-32,
-1.));
#124625=DIRECTION('ref_axis',(-0.242361737093213,0.970185955574064,1.94061808061067E-32));
#124626=DIRECTION('center_axis',(0.966629599819577,0.256178095770586,-3.46966352979465E-16));
#124627=DIRECTION('ref_axis',(0.256178095770586,-0.966629599819577,7.88510670898549E-14));
#124628=DIRECTION('center_axis',(3.34374866773943E-33,2.09084201519512E-32,
-1.));
#124629=DIRECTION('ref_axis',(-0.162476136260206,0.986712473391289,0.));
#124630=DIRECTION('center_axis',(-3.34374866773943E-33,-2.09084201519512E-32,
1.));
#124631=DIRECTION('ref_axis',(0.162476136260206,-0.986712473391289,-2.00873195986765E-32));
#124632=DIRECTION('center_axis',(0.988929999270642,0.148382804066268,6.13681984861664E-17));
#124633=DIRECTION('ref_axis',(-0.148382804066268,0.988929999270642,-4.46815747097839E-32));
#124634=DIRECTION('center_axis',(3.34374866773943E-33,2.09084201519512E-32,
-1.));
#124635=DIRECTION('ref_axis',(-0.162476136260206,0.986712473391289,2.00873195986765E-32));
#124636=DIRECTION('center_axis',(0.984294112614218,0.176536398153437,-3.46966352979465E-16));
#124637=DIRECTION('ref_axis',(0.176536398153437,-0.984294112614218,7.88510670898552E-14));
#124638=DIRECTION('center_axis',(-1.60900427476467E-32,2.8383519892658E-32,
-1.));
#124639=DIRECTION('ref_axis',(0.781831482468023,0.623489801858742,0.));
#124640=DIRECTION('center_axis',(1.60900427476467E-32,-2.8383519892658E-32,
1.));
#124641=DIRECTION('ref_axis',(-0.781831482468023,-0.623489801858742,-5.11713321956047E-33));
#124642=DIRECTION('center_axis',(0.612272458757527,-0.790646846731847,6.13681984861663E-17));
#124643=DIRECTION('ref_axis',(0.790646846731847,0.612272458757527,-5.23852944873328E-31));
#124644=DIRECTION('center_axis',(-1.60900427476467E-32,2.8383519892658E-32,
-1.));
#124645=DIRECTION('ref_axis',(0.781831482468023,0.623489801858742,5.11713321956047E-33));
#124646=DIRECTION('center_axis',(0.634580240198986,-0.772856984667278,-3.46966352979465E-16));
#124647=DIRECTION('ref_axis',(-0.772856984667278,-0.634580240198986,7.88510670898554E-14));
#124648=DIRECTION('center_axis',(-1.49906277922563E-32,2.71147273975433E-32,
-1.));
#124649=DIRECTION('ref_axis',(0.728409795658261,0.685141714967852,0.));
#124650=DIRECTION('center_axis',(1.49906277922563E-32,-2.71147273975433E-32,
1.));
#124651=DIRECTION('ref_axis',(-0.728409795658261,-0.685141714967852,-7.6581107030922E-33));
#124652=DIRECTION('center_axis',(0.674680230675791,-0.738110145124195,6.13681984861663E-17));
#124653=DIRECTION('ref_axis',(0.738110145124195,0.674680230675791,2.09541177949331E-31));
#124654=DIRECTION('center_axis',(-1.49906277922563E-32,2.71147273975433E-32,
-1.));
#124655=DIRECTION('ref_axis',(0.728409795658261,0.685141714967853,7.65811070309221E-33));
#124656=DIRECTION('center_axis',(0.695463745903482,-0.718561186075269,-3.46966352979465E-16));
#124657=DIRECTION('ref_axis',(-0.718561186075269,-0.695463745903482,7.8851067089855E-14));
#124658=DIRECTION('center_axis',(-1.37914526821878E-32,2.59397692301229E-32,
-1.));
#124659=DIRECTION('ref_axis',(0.670140661837551,0.742234123004278,0.));
#124660=DIRECTION('center_axis',(1.37914526821878E-32,-2.59397692301229E-32,
1.));
#124661=DIRECTION('ref_axis',(-0.670140661837551,-0.742234123004278,-1.0011168637311E-32));
#124662=DIRECTION('center_axis',(0.732598116973311,-0.680661442280345,6.13681984861663E-17));
#124663=DIRECTION('ref_axis',(0.680661442280345,0.732598116973311,5.79319727271681E-31));
#124664=DIRECTION('center_axis',(-1.37914526821878E-32,2.59397692301229E-32,
-1.));
#124665=DIRECTION('ref_axis',(0.670140661837551,0.742234123004278,1.00111686373111E-32));
#124666=DIRECTION('center_axis',(0.751719055122432,-0.659483481344179,-3.46966352979465E-16));
#124667=DIRECTION('ref_axis',(-0.659483481344179,-0.751719055122432,7.88510670898551E-14));
#124668=DIRECTION('center_axis',(-1.25004977299489E-32,2.48664645431466E-32,
-1.));
#124669=DIRECTION('ref_axis',(0.607411852477738,0.79438708541212,0.));
#124670=DIRECTION('center_axis',(1.25004977299489E-32,-2.48664645431466E-32,
1.));
#124671=DIRECTION('ref_axis',(-0.607411852477738,-0.79438708541212,-1.2160647809892E-32));
#124672=DIRECTION('center_axis',(0.785640683672555,-0.61868304983935,6.13681984861663E-17));
#124673=DIRECTION('ref_axis',(0.61868304983935,0.785640683672555,9.24446373305873E-32));
#124674=DIRECTION('center_axis',(-1.25004977299489E-32,2.48664645431466E-32,
-1.));
#124675=DIRECTION('ref_axis',(0.607411852477738,0.79438708541212,1.2160647809892E-32));
#124676=DIRECTION('center_axis',(0.802971798054457,-0.596017022851859,-3.46966352979465E-16));
#124677=DIRECTION('ref_axis',(-0.596017022851859,-0.802971798054457,7.88510670898544E-14));
#124678=DIRECTION('center_axis',(-1.11263540277541E-32,2.39019560022233E-32,
-1.));
#124679=DIRECTION('ref_axis',(0.540640817455587,0.841253532831188,0.));
#124680=DIRECTION('center_axis',(1.11263540277541E-32,-2.39019560022233E-32,
1.));
#124681=DIRECTION('ref_axis',(-0.540640817455587,-0.841253532831188,-1.40922437915807E-32));
#124682=DIRECTION('center_axis',(0.833454941243547,-0.552587423777194,6.13681984861663E-17));
#124683=DIRECTION('ref_axis',(0.552587423777194,0.833454941243547,9.86076131526265E-32));
#124684=DIRECTION('center_axis',(-1.11263540277541E-32,2.39019560022233E-32,
-1.));
#124685=DIRECTION('ref_axis',(0.540640817455587,0.841253532831188,1.40922437915807E-32));
#124686=DIRECTION('center_axis',(0.84888089615145,-0.528584169408347,-3.46966352979465E-16));
#124687=DIRECTION('ref_axis',(-0.528584169408346,-0.84888089615145,7.8851067089855E-14));
#124688=DIRECTION('center_axis',(-9.67816627522388E-33,2.30526622525602E-32,
-1.));
#124689=DIRECTION('ref_axis',(0.470271906992726,0.882521576786327,0.));
#124690=DIRECTION('center_axis',(9.67816627522388E-33,-2.30526622525602E-32,
1.));
#124691=DIRECTION('ref_axis',(-0.470271906992726,-0.882521576786327,-1.57931021298098E-32));
#124692=DIRECTION('center_axis',(0.875722693690948,-0.482814419580308,6.13681984861663E-17));
#124693=DIRECTION('ref_axis',(0.482814419580308,0.875722693690948,-1.07852076885685E-31));
#124694=DIRECTION('center_axis',(-9.67816627522388E-33,2.30526622525602E-32,
-1.));
#124695=DIRECTION('ref_axis',(0.470271906992726,0.882521576786327,1.57931021298098E-32));
#124696=DIRECTION('center_axis',(0.889140831940044,-0.457633675527671,-3.46966352979465E-16));
#124697=DIRECTION('ref_axis',(-0.457633675527671,-0.889140831940044,7.88510670898546E-14));
#124698=DIRECTION('center_axis',(-8.16557192291705E-33,2.23242352039376E-32,
-1.));
#124699=DIRECTION('ref_axis',(0.396773414578231,0.917916585253765,0.));
#124700=DIRECTION('center_axis',(8.16557192291705E-33,-2.23242352039376E-32,
1.));
#124701=DIRECTION('ref_axis',(-0.396773414578231,-0.917916585253764,-1.72519038929603E-32));
#124702=DIRECTION('center_axis',(0.912162656095911,-0.409828365079887,6.13681984861663E-17));
#124703=DIRECTION('ref_axis',(0.409828365079887,0.912162656095911,2.46519032881566E-32));
#124704=DIRECTION('center_axis',(-8.16557192291705E-33,2.23242352039376E-32,
-1.));
#124705=DIRECTION('ref_axis',(0.396773414578231,0.917916585253764,1.72519038929603E-32));
#124706=DIRECTION('center_axis',(0.923483682189989,-0.383637705040601,-3.46966352979465E-16));
#124707=DIRECTION('ref_axis',(-0.383637705040601,-0.923483682189989,7.88510670898542E-14));
#124708=DIRECTION('center_axis',(-6.59863703668774E-33,2.17215224181822E-32,
-1.));
#124709=DIRECTION('ref_axis',(0.320634460552723,0.947203010291914,0.));
#124710=DIRECTION('center_axis',(6.59863703668774E-33,-2.17215224181822E-32,
1.));
#124711=DIRECTION('ref_axis',(-0.320634460552723,-0.947203010291914,-1.84589409959839E-32));
#124712=DIRECTION('center_axis',(0.9425323265208,-0.33411497042678,6.13681984861663E-17));
#124713=DIRECTION('ref_axis',(0.33411497042678,0.9425323265208,1.29422492262822E-31));
#124714=DIRECTION('center_axis',(-6.59863703668774E-33,2.17215224181822E-32,
-1.));
#124715=DIRECTION('ref_axis',(0.320634460552723,0.947203010291914,1.84589409959839E-32));
#124716=DIRECTION('center_axis',(0.951680900899042,-0.307088688922252,-3.46966352979465E-16));
#124717=DIRECTION('ref_axis',(-0.307088688922252,-0.951680900899042,1.57702134179711E-13));
#124718=DIRECTION('center_axis',(-4.98778930967775E-33,2.12485348494425E-32,
-1.));
#124719=DIRECTION('ref_axis',(0.2423617370932,0.970185955574068,0.));
#124720=DIRECTION('center_axis',(4.98778930967775E-33,-2.12485348494425E-32,
1.));
#124721=DIRECTION('ref_axis',(-0.2423617370932,-0.970185955574068,-1.94061808061069E-32));
#124722=DIRECTION('center_axis',(0.966629599819581,-0.256178095770573,6.13681984861663E-17));
#124723=DIRECTION('ref_axis',(0.256178095770573,0.966629599819581,-3.08148791101958E-32));
#124724=DIRECTION('center_axis',(-4.98778930967775E-33,2.12485348494425E-32,
-1.));
#124725=DIRECTION('ref_axis',(0.2423617370932,0.970185955574068,1.94061808061069E-32));
#124726=DIRECTION('center_axis',(0.973544840228909,-0.228496048245192,-3.46966352979465E-16));
#124727=DIRECTION('ref_axis',(-0.228496048245192,-0.973544840228909,1.57702134179709E-13));
#124728=DIRECTION('center_axis',(-3.34374866773916E-33,2.09084201519511E-32,
-1.));
#124729=DIRECTION('ref_axis',(0.162476136260193,0.986712473391291,0.));
#124730=DIRECTION('center_axis',(3.34374866773916E-33,-2.09084201519511E-32,
1.));
#124731=DIRECTION('ref_axis',(-0.162476136260193,-0.986712473391291,-2.00873195986766E-32));
#124732=DIRECTION('center_axis',(0.984294112614221,-0.176536398153423,6.13681984861663E-17));
#124733=DIRECTION('ref_axis',(0.176536398153423,0.984294112614221,-4.93038065763132E-32));
#124734=DIRECTION('center_axis',(-3.34374866773916E-33,2.09084201519511E-32,
-1.));
#124735=DIRECTION('ref_axis',(0.162476136260193,0.986712473391291,2.00873195986766E-32));
#124736=DIRECTION('center_axis',(0.988929999270644,-0.148382804066255,-3.46966352979465E-16));
#124737=DIRECTION('ref_axis',(-0.148382804066255,-0.988929999270644,7.88510670898552E-14));
#124738=DIRECTION('center_axis',(-1.67745593009647E-33,2.07034417329048E-32,
-1.));
#124739=DIRECTION('ref_axis',(0.0815092835470502,0.996672582494194,0.));
#124740=DIRECTION('center_axis',(1.67745593009647E-33,-2.07034417329048E-32,
1.));
#124741=DIRECTION('ref_axis',(-0.0815092835470502,-0.996672582494194,-2.04978245074084E-32));
#124742=DIRECTION('center_axis',(0.99540831048651,-0.0957198799330179,6.13681984861663E-17));
#124743=DIRECTION('ref_axis',(0.0957198799330179,0.99540831048651,1.92592994438724E-32));
#124744=DIRECTION('center_axis',(-1.67745593009647E-33,2.07034417329048E-32,
-1.));
#124745=DIRECTION('ref_axis',(0.0815092835470502,0.996672582494194,2.04978245074084E-32));
#124746=DIRECTION('center_axis',(0.997733992329198,-0.0672820968076959,
-3.46966352979465E-16));
#124747=DIRECTION('ref_axis',(-0.0672820968076959,-0.997733992329198,7.88510670898553E-14));
#124748=DIRECTION('center_axis',(1.67745593009674E-33,2.07034417329048E-32,
-1.));
#124749=DIRECTION('ref_axis',(-0.0815092835470633,0.996672582494193,0.));
#124750=DIRECTION('center_axis',(-1.67745593009674E-33,-2.07034417329048E-32,
1.));
#124751=DIRECTION('ref_axis',(0.0815092835470634,-0.996672582494193,-2.04978245074083E-32));
#124752=DIRECTION('center_axis',(0.997733992329197,0.0672820968077094,6.13681984861663E-17));
#124753=DIRECTION('ref_axis',(-0.0672820968077094,0.997733992329197,1.4637067577343E-32));
#124754=DIRECTION('center_axis',(1.67745593009674E-33,2.07034417329048E-32,
-1.));
#124755=DIRECTION('ref_axis',(-0.0815092835470634,0.996672582494193,2.04978245074083E-32));
#124756=DIRECTION('center_axis',(0.995408310486509,0.0957198799330314,-3.46966352979465E-16));
#124757=DIRECTION('ref_axis',(0.0957198799330314,-0.995408310486509,7.88510670898544E-14));
#124758=DIRECTION('center_axis',(0.,2.06349636898632E-32,-1.));
#124759=DIRECTION('ref_axis',(0.,1.,0.));
#124760=DIRECTION('center_axis',(0.,-2.06349636898632E-32,1.));
#124761=DIRECTION('ref_axis',(0.,-1.,-2.06349636898632E-32));
#124762=DIRECTION('center_axis',(0.999898230283323,-0.01426636170434,6.13681984861663E-17));
#124763=DIRECTION('ref_axis',(0.01426636170434,0.999898230283323,0.));
#124764=DIRECTION('center_axis',(0.,2.06349636898632E-32,-1.));
#124765=DIRECTION('ref_axis',(0.,1.,2.06349636898632E-32));
#124766=DIRECTION('center_axis',(0.,2.06349636898632E-32,-1.));
#124767=DIRECTION('ref_axis',(0.,1.,2.06349636898632E-32));
#124768=DIRECTION('center_axis',(0.999898230283323,0.0142663617043404,-3.46966352979465E-16));
#124769=DIRECTION('ref_axis',(0.0142663617043404,-0.999898230283323,7.88510670898545E-14));
#124770=DIRECTION('center_axis',(0.,-4.12699273797265E-32,1.));
#124771=DIRECTION('ref_axis',(0.,-1.,-4.12699273797265E-32));
#124772=DIRECTION('center_axis',(0.,-4.12699273797265E-32,1.));
#124773=DIRECTION('ref_axis',(0.,-1.,-4.12699273797265E-32));
#124774=DIRECTION('center_axis',(0.,-4.12699273797265E-32,1.));
#124775=DIRECTION('ref_axis',(0.,-1.,-4.12699273797265E-32));
#124776=DIRECTION('center_axis',(0.,-1.22464679914735E-16,1.));
#124777=DIRECTION('ref_axis',(0.,-1.,-1.22464679914735E-16));
#124778=DIRECTION('center_axis',(0.,1.22464679914735E-16,-1.));
#124779=DIRECTION('ref_axis',(0.,1.,1.22464679914735E-16));
#124780=DIRECTION('',(8.65956056235493E-17,-0.707106781186547,-0.707106781186548));
#124781=DIRECTION('center_axis',(0.,-1.22464679914735E-16,1.));
#124782=DIRECTION('ref_axis',(0.,-1.,-1.22464679914735E-16));
#124783=DIRECTION('center_axis',(0.,0.,1.));
#124784=DIRECTION('ref_axis',(1.,0.,0.));
#124785=DIRECTION('',(-0.86602540378444,-1.06057523872491E-16,0.499999999999998));
#124786=DIRECTION('center_axis',(0.,4.12699273797265E-32,-1.));
#124787=DIRECTION('ref_axis',(0.,1.,4.12699273797265E-32));
#124788=DIRECTION('center_axis',(0.,4.12699273797265E-32,-1.));
#124789=DIRECTION('ref_axis',(0.,1.,4.12699273797265E-32));
#124790=DIRECTION('center_axis',(0.,4.12699273797265E-32,-1.));
#124791=DIRECTION('ref_axis',(0.,1.,4.12699273797265E-32));
#124792=DIRECTION('center_axis',(0.,0.,1.));
#124793=DIRECTION('ref_axis',(1.,0.,0.));
#124794=DIRECTION('center_axis',(0.,4.12699273797265E-32,-1.));
#124795=DIRECTION('ref_axis',(0.,1.,4.12699273797265E-32));
#124796=DIRECTION('center_axis',(0.,4.12699273797265E-32,-1.));
#124797=DIRECTION('ref_axis',(0.,1.,4.12699273797265E-32));
#124798=DIRECTION('center_axis',(0.,0.,1.));
#124799=DIRECTION('ref_axis',(1.,0.,0.));
#124800=DIRECTION('center_axis',(0.,0.,1.));
#124801=DIRECTION('ref_axis',(1.,0.,0.));
#124802=DIRECTION('center_axis',(0.,-4.12699273797265E-32,1.));
#124803=DIRECTION('ref_axis',(0.,-1.,0.));
#124804=DIRECTION('center_axis',(0.,-4.12699273797265E-32,1.));
#124805=DIRECTION('ref_axis',(0.,-1.,-4.12699273797265E-32));
#124806=DIRECTION('center_axis',(-1.,-1.22464679914735E-16,-5.05410844666257E-48));
#124807=DIRECTION('ref_axis',(-1.22464679914735E-16,1.,0.));
#124808=DIRECTION('center_axis',(0.,-4.12699273797265E-32,1.));
#124809=DIRECTION('ref_axis',(0.,-1.,-4.12699273797265E-32));
#124810=DIRECTION('center_axis',(0.,-4.12699273797265E-32,1.));
#124811=DIRECTION('ref_axis',(0.,-1.,-4.12699273797265E-32));
#124812=DIRECTION('center_axis',(0.,-4.12699273797265E-32,1.));
#124813=DIRECTION('ref_axis',(0.,-1.,-4.12699273797265E-32));
#124814=DIRECTION('',(8.6595605623543E-17,-0.707106781186496,-0.707106781186599));
#124815=DIRECTION('center_axis',(0.,-4.12699273797265E-32,1.));
#124816=DIRECTION('ref_axis',(0.,-1.,0.));
#124817=DIRECTION('center_axis',(0.,-4.12699273797265E-32,1.));
#124818=DIRECTION('ref_axis',(0.,-1.,-4.12699273797265E-32));
#124819=DIRECTION('center_axis',(-1.,-1.22464679914735E-16,-5.05410844666257E-48));
#124820=DIRECTION('ref_axis',(-1.22464679914735E-16,1.,0.));
#124821=DIRECTION('center_axis',(0.,4.12699273797265E-32,-1.));
#124822=DIRECTION('ref_axis',(0.,1.,4.12699273797265E-32));
#124823=DIRECTION('',(-0.282888365662603,0.675203035852198,-0.681230528491433));
#124824=DIRECTION('center_axis',(0.,-4.12699273797265E-32,1.));
#124825=DIRECTION('ref_axis',(0.,-1.,-4.12699273797265E-32));
#124826=DIRECTION('',(-0.226911762261394,-0.696014381459685,0.681230528491435));
#124827=DIRECTION('',(-0.336982393663624,0.649898325441773,-0.681230528491431));
#124828=DIRECTION('center_axis',(0.,-4.12699273797265E-32,1.));
#124829=DIRECTION('ref_axis',(0.,-1.,-4.12699273797265E-32));
#124830=DIRECTION('',(-0.169425098520137,-0.712193866192861,0.681230528491426));
#124831=DIRECTION('',(-0.388833859432995,0.620268648901205,-0.681230528491432));
#124832=DIRECTION('center_axis',(0.,-4.12699273797265E-32,1.));
#124833=DIRECTION('ref_axis',(0.,-1.,-4.12699273797265E-32));
#124834=DIRECTION('',(-0.110810938701405,-0.723633818250228,0.681230528491427));
#124835=DIRECTION('',(-0.438097700020906,0.586511186839332,-0.681230528491428));
#124836=DIRECTION('center_axis',(0.,-4.12699273797265E-32,1.));
#124837=DIRECTION('ref_axis',(0.,-1.,-4.12699273797265E-32));
#124838=DIRECTION('',(-0.0514593503681312,-0.730258106638318,0.681230528491426));
#124839=DIRECTION('',(-0.484446072696218,0.548850589596559,-0.681230528491436));
#124840=DIRECTION('center_axis',(0.,-4.12699273797265E-32,1.));
#124841=DIRECTION('ref_axis',(0.,-1.,-4.12699273797265E-32));
#124842=DIRECTION('',(0.00823469145164575,-0.73202264781083,0.681230528491434));
#124843=DIRECTION('',(-0.527570536685703,0.507537482234015,-0.681230528491432));
#124844=DIRECTION('center_axis',(0.,-4.12699273797265E-32,1.));
#124845=DIRECTION('ref_axis',(0.,-1.,-4.12699273797265E-32));
#124846=DIRECTION('',(0.0678739327584426,-0.728915699037407,0.681230528491429));
#124847=DIRECTION('',(-0.567184105796568,0.462846796664981,-0.68123052849143));
#124848=DIRECTION('center_axis',(0.,-4.12699273797265E-32,1.));
#124849=DIRECTION('ref_axis',(0.,-1.,-4.12699273797265E-32));
#124850=DIRECTION('',(0.127061484241137,-0.720957936549514,0.681230528491425));
#124851=DIRECTION('',(-0.603023158262138,0.415075942028502,-0.681230528491426));
#124852=DIRECTION('center_axis',(0.,-4.12699273797265E-32,1.));
#124853=DIRECTION('ref_axis',(0.,-1.,-4.12699273797265E-32));
#124854=DIRECTION('',(0.185403462509881,-0.708202317943565,0.681230528491427));
#124855=DIRECTION('',(-0.634849191101295,0.364542825480514,-0.681230528491432));
#124856=DIRECTION('center_axis',(0.,-4.12699273797265E-32,1.));
#124857=DIRECTION('ref_axis',(0.,-1.,-4.12699273797265E-32));
#124858=DIRECTION('',(0.242511611325033,-0.690733729756857,0.681230528491433));
#124859=DIRECTION('',(-0.662450407316416,0.311583736574296,-0.681230528491431));
#124860=DIRECTION('center_axis',(0.,-4.12699273797265E-32,1.));
#124861=DIRECTION('ref_axis',(0.,-1.,-4.12699273797265E-32));
#124862=DIRECTION('',(0.298005885378429,-0.668668422561666,0.681230528491429));
#124863=DIRECTION('',(-0.685643125367474,0.256551109308882,-0.681230528491424));
#124864=DIRECTION('center_axis',(0.,-4.12699273797265E-32,1.));
#124865=DIRECTION('ref_axis',(0.,-1.,-4.12699273797265E-32));
#124866=DIRECTION('',(0.351516979432132,-0.642153237336854,0.681230528491427));
#124867=DIRECTION('',(-0.704273001542363,0.199811176738953,-0.681230528491424));
#124868=DIRECTION('center_axis',(0.,-4.12699273797265E-32,1.));
#124869=DIRECTION('ref_axis',(0.,-1.,-4.12699273797265E-32));
#124870=DIRECTION('',(0.402688785983932,-0.611364628265391,0.681230528491425));
#124871=DIRECTION('',(-0.718216057088846,0.14174153375436,-0.68123052849143));
#124872=DIRECTION('center_axis',(0.,-4.12699273797265E-32,1.));
#124873=DIRECTION('ref_axis',(0.,-1.,-4.12699273797265E-32));
#124874=DIRECTION('',(0.451180765103993,-0.57650748846088,0.681230528491423));
#124875=DIRECTION('',(-0.72737950327272,0.0827286242483378,-0.681230528491427));
#124876=DIRECTION('center_axis',(0.,-4.12699273797265E-32,1.));
#124877=DIRECTION('ref_axis',(0.,-1.,-4.12699273797265E-32));
#124878=DIRECTION('',(0.496670210671858,-0.537813786437704,0.681230528491429));
#124879=DIRECTION('',(-0.731702358871481,0.023165169397201,-0.681230528491428));
#124880=DIRECTION('center_axis',(0.,-4.12699273797265E-32,1.));
#124881=DIRECTION('ref_axis',(0.,-1.,-4.12699273797265E-32));
#124882=DIRECTION('',(0.538854397932528,-0.495541022398817,0.681230528491426));
#124883=DIRECTION('',(-0.731155855994348,-0.0365524458342823,-0.681230528491423));
#124884=DIRECTION('center_axis',(0.,-4.12699273797265E-32,1.));
#124885=DIRECTION('ref_axis',(0.,-1.,-4.12699273797265E-32));
#124886=DIRECTION('',(0.577452598079667,-0.449970514614377,0.681230528491431));
#124887=DIRECTION('',(-0.725743631527792,-0.0960268105694711,-0.681230528491426));
#124888=DIRECTION('center_axis',(0.,-4.12699273797265E-32,1.));
#124889=DIRECTION('ref_axis',(0.,-1.,-4.12699273797265E-32));
#124890=DIRECTION('',(0.612207946459573,-0.401405527295087,0.681230528491425));
#124891=DIRECTION('',(-0.715501702932691,-0.154862132723631,-0.681230528491426));
#124892=DIRECTION('center_axis',(0.,-4.12699273797265E-32,1.));
#124893=DIRECTION('ref_axis',(0.,-1.,-4.12699273797265E-32));
#124894=DIRECTION('',(0.642889151962973,-0.350169252418901,0.681230528491433));
#124895=DIRECTION('',(-0.700498228554037,-0.212666872934969,-0.681230528491433));
#124896=DIRECTION('center_axis',(0.,-4.12699273797265E-32,1.));
#124897=DIRECTION('ref_axis',(0.,-1.,-4.12699273797265E-32));
#124898=DIRECTION('',(0.669292036229316,-0.296602658941726,0.681230528491431));
#124899=DIRECTION('',(-0.680833054038443,-0.269056350194485,-0.681230528491427));
#124900=DIRECTION('center_axis',(0.,-4.12699273797265E-32,1.));
#124901=DIRECTION('ref_axis',(0.,-1.,-4.12699273797265E-32));
#124902=DIRECTION('',(0.691240892419964,-0.241062223705287,0.68123052849143));
#124903=DIRECTION('',(-0.656637047877763,-0.323655301834632,-0.681230528491428));
#124904=DIRECTION('center_axis',(0.,-4.12699273797265E-32,1.));
#124905=DIRECTION('ref_axis',(0.,-1.,-4.12699273797265E-32));
#124906=DIRECTION('',(0.708589654518281,-0.183917559142556,0.681230528491427));
#124907=DIRECTION('',(-0.628071230500937,-0.376100380840438,-0.681230528491432));
#124908=DIRECTION('center_axis',(0.,-4.12699273797265E-32,1.));
#124909=DIRECTION('ref_axis',(0.,-1.,-4.12699273797265E-32));
#124910=DIRECTION('',(0.721222869374837,-0.125548953567995,0.681230528491427));
#124911=DIRECTION('',(-0.595325702709604,-0.426042573863937,-0.681230528491426));
#124912=DIRECTION('center_axis',(0.,-4.12699273797265E-32,1.));
#124913=DIRECTION('ref_axis',(0.,-1.,-4.12699273797265E-32));
#124914=DIRECTION('',(0.7290564650291,-0.0663448404215596,0.681230528491428));
#124915=DIRECTION('',(-0.558618380588551,-0.473149523850459,-0.681230528491427));
#124916=DIRECTION('center_axis',(0.,-4.12699273797265E-32,1.));
#124917=DIRECTION('ref_axis',(0.,-1.,-4.12699273797265E-32));
#124918=DIRECTION('',(0.732038310194444,-0.00669921330824207,0.68123052849143));
#124919=DIRECTION('',(-0.518193545310225,-0.517107741819927,-0.681230528491432));
#124920=DIRECTION('center_axis',(0.,-4.12699273797265E-32,1.));
#124921=DIRECTION('ref_axis',(0.,-1.,-4.12699273797265E-32));
#124922=DIRECTION('',(0.730148561183267,0.052990995964345,0.681230528491429));
#124923=DIRECTION('',(-0.474320217483789,-0.557624693084355,-0.681230528491428));
#124924=DIRECTION('center_axis',(0.,-4.12699273797265E-32,1.));
#124925=DIRECTION('ref_axis',(0.,-1.,-4.12699273797265E-32));
#124926=DIRECTION('',(0.72339979396345,0.112328558901694,0.681230528491425));
#124927=DIRECTION('',(-0.427290366867324,-0.594430744017905,-0.681230528491426));
#124928=DIRECTION('center_axis',(0.,-4.12699273797265E-32,1.));
#124929=DIRECTION('ref_axis',(0.,-1.,-4.12699273797265E-32));
#124930=DIRECTION('',(0.711836920467365,0.170918593812461,0.681230528491427));
#124931=DIRECTION('',(-0.377416969357283,-0.627280956424197,-0.681230528491426));
#124932=DIRECTION('center_axis',(0.,-4.12699273797265E-32,1.));
#124933=DIRECTION('ref_axis',(0.,-1.,-4.12699273797265E-32));
#124934=DIRECTION('',(0.695536889710404,0.228371193680976,0.681230528491423));
#124935=DIRECTION('',(-0.325031924185611,-0.655956717559541,-0.681230528491429));
#124936=DIRECTION('center_axis',(0.,-4.12699273797265E-32,1.));
#124937=DIRECTION('ref_axis',(0.,-1.,-4.12699273797265E-32));
#124938=DIRECTION('',(0.67460817570792,0.284304020934146,0.681230528491427));
#124939=DIRECTION('',(-0.27048384518497,-0.680267194964773,-0.68123052849143));
#124940=DIRECTION('center_axis',(0.,-4.12699273797265E-32,1.));
#124941=DIRECTION('ref_axis',(0.,-1.,-4.12699273797265E-32));
#124942=DIRECTION('',(0.649190055598613,0.338344851834863,0.681230528491431));
#124943=DIRECTION('',(-0.21413574082131,-0.700050606423701,-0.681230528491433));
#124944=DIRECTION('center_axis',(0.,-4.12699273797265E-32,1.));
#124945=DIRECTION('ref_axis',(0.,-1.,-4.12699273797265E-32));
#124946=DIRECTION('',(0.619451682778123,0.39013405356959,0.681230528491429));
#124947=DIRECTION('',(-0.156362598432402,-0.715175296597104,-0.681230528491429));
#124948=DIRECTION('center_axis',(0.,-4.12699273797265E-32,1.));
#124949=DIRECTION('ref_axis',(0.,-1.,-4.12699273797265E-32));
#124950=DIRECTION('',(0.585590961211076,0.439326977545395,0.681230528491432));
#124951=DIRECTION('',(-0.0975488887489323,-0.725540613167269,-0.681230528491429));
#124952=DIRECTION('center_axis',(0.,-4.12699273797265E-32,1.));
#124953=DIRECTION('ref_axis',(0.,-1.,-4.12699273797265E-32));
#124954=DIRECTION('',(0.547833228412878,0.485596252969493,0.681230528491429));
#124955=DIRECTION('',(-0.0380860073052719,-0.731077576662577,-0.681230528491432));
#124956=DIRECTION('center_axis',(0.,-4.12699273797265E-32,1.));
#124957=DIRECTION('ref_axis',(0.,-1.,-4.12699273797265E-32));
#124958=DIRECTION('',(0.506429755865707,0.528633965447829,0.681230528491423));
#124959=DIRECTION('',(0.0216303302332448,-0.731749339504516,-0.681230528491425));
#124960=DIRECTION('center_axis',(0.,-4.12699273797265E-32,1.));
#124961=DIRECTION('ref_axis',(0.,-1.,-4.12699273797265E-32));
#124962=DIRECTION('',(0.461656076848288,0.568153706104551,0.681230528491429));
#124963=DIRECTION('',(0.0812027214928242,-0.727551431222185,-0.681230528491427));
#124964=DIRECTION('center_axis',(0.,-4.12699273797265E-32,1.));
#124965=DIRECTION('ref_axis',(0.,-1.,-4.12699273797265E-32));
#124966=DIRECTION('',(0.413810152807329,0.603892477585927,0.681230528491425));
#124967=DIRECTION('',(0.140234722038368,-0.718511788202607,-0.68123052849143));
#124968=DIRECTION('center_axis',(0.,-4.12699273797265E-32,1.));
#124969=DIRECTION('ref_axis',(0.,-1.,-4.12699273797265E-32));
#124970=DIRECTION('',(0.363210390473304,0.635612444264213,0.681230528491422));
#124971=DIRECTION('',(0.19833348364585,-0.704690567778647,-0.681230528491427));
#124972=DIRECTION('center_axis',(0.,-4.12699273797265E-32,1.));
#124973=DIRECTION('ref_axis',(0.,-1.,-4.12699273797265E-32));
#124974=DIRECTION('',(0.310193522916185,0.663102514994576,0.681230528491431));
#124975=DIRECTION('',(0.25511236864239,-0.686179747891876,-0.681230528491428));
#124976=DIRECTION('center_axis',(0.,-4.12699273797265E-32,1.));
#124977=DIRECTION('ref_axis',(0.,-1.,-4.12699273797265E-32));
#124978=DIRECTION('',(8.65956056235492E-17,0.707106781186547,0.707106781186548));
#124979=DIRECTION('center_axis',(0.,-4.12699273797265E-32,1.));
#124980=DIRECTION('ref_axis',(0.,-1.,-4.12699273797265E-32));
#124981=DIRECTION('center_axis',(0.,-4.12699273797265E-32,1.));
#124982=DIRECTION('ref_axis',(0.,-1.,-4.12699273797265E-32));
#124983=DIRECTION('center_axis',(0.,-4.12699273797265E-32,1.));
#124984=DIRECTION('ref_axis',(0.,-1.,-4.12699273797265E-32));
#124985=DIRECTION('',(0.255112368642381,0.686179747891878,0.68123052849143));
#124986=DIRECTION('',(0.310193522916193,-0.663102514994574,-0.68123052849143));
#124987=DIRECTION('center_axis',(0.,-4.12699273797265E-32,1.));
#124988=DIRECTION('ref_axis',(0.,-1.,-4.12699273797265E-32));
#124989=DIRECTION('',(0.198333483645841,0.704690567778648,0.681230528491429));
#124990=DIRECTION('',(0.363210390473318,-0.635612444264197,-0.68123052849143));
#124991=DIRECTION('center_axis',(0.,-4.12699273797265E-32,1.));
#124992=DIRECTION('ref_axis',(0.,-1.,-4.12699273797265E-32));
#124993=DIRECTION('',(0.140234722038358,0.718511788202608,0.681230528491431));
#124994=DIRECTION('',(0.413810152807337,-0.603892477585918,-0.681230528491428));
#124995=DIRECTION('center_axis',(0.,-4.12699273797265E-32,1.));
#124996=DIRECTION('ref_axis',(0.,-1.,-4.12699273797265E-32));
#124997=DIRECTION('',(0.0812027214928108,0.727551431222181,0.681230528491433));
#124998=DIRECTION('',(0.461656076848292,-0.568153706104549,-0.681230528491427));
#124999=DIRECTION('center_axis',(0.,-4.12699273797265E-32,1.));
#125000=DIRECTION('ref_axis',(0.,-1.,-4.12699273797265E-32));
#125001=DIRECTION('',(0.0216303302332394,0.731749339504505,0.681230528491436));
#125002=DIRECTION('',(0.506429755865719,-0.528633965447818,-0.681230528491424));
#125003=DIRECTION('center_axis',(0.,-4.12699273797265E-32,1.));
#125004=DIRECTION('ref_axis',(0.,-1.,-4.12699273797265E-32));
#125005=DIRECTION('',(-0.0380860073052859,0.73107757666258,0.681230528491429));
#125006=DIRECTION('',(0.547833228412883,-0.485596252969484,-0.681230528491432));
#125007=DIRECTION('center_axis',(0.,-4.12699273797265E-32,1.));
#125008=DIRECTION('ref_axis',(0.,-1.,-4.12699273797265E-32));
#125009=DIRECTION('',(-0.0975488887489436,0.725540613167269,0.681230528491428));
#125010=DIRECTION('',(0.585590961211085,-0.439326977545388,-0.681230528491429));
#125011=DIRECTION('center_axis',(0.,-4.12699273797265E-32,1.));
#125012=DIRECTION('ref_axis',(0.,-1.,-4.12699273797265E-32));
#125013=DIRECTION('',(-0.156362598432407,0.715175296597106,0.681230528491426));
#125014=DIRECTION('',(0.619451682778131,-0.390134053569583,-0.681230528491426));
#125015=DIRECTION('center_axis',(0.,-4.12699273797265E-32,1.));
#125016=DIRECTION('ref_axis',(0.,-1.,-4.12699273797265E-32));
#125017=DIRECTION('',(-0.214135740821315,0.7000506064237,0.681230528491432));
#125018=DIRECTION('',(0.649190055598621,-0.338344851834856,-0.681230528491427));
#125019=DIRECTION('center_axis',(0.,-4.12699273797265E-32,1.));
#125020=DIRECTION('ref_axis',(0.,-1.,-4.12699273797265E-32));
#125021=DIRECTION('',(-0.270483845184975,0.680267194964772,0.681230528491429));
#125022=DIRECTION('',(0.674608175707922,-0.284304020934136,-0.681230528491429));
#125023=DIRECTION('center_axis',(0.,-4.12699273797265E-32,1.));
#125024=DIRECTION('ref_axis',(0.,-1.,-4.12699273797265E-32));
#125025=DIRECTION('',(-0.325031924185617,0.65595671755954,0.681230528491428));
#125026=DIRECTION('',(0.695536889710403,-0.228371193680966,-0.681230528491428));
#125027=DIRECTION('center_axis',(0.,-4.12699273797265E-32,1.));
#125028=DIRECTION('ref_axis',(0.,-1.,-4.12699273797265E-32));
#125029=DIRECTION('',(-0.377416969357297,0.627280956424184,0.681230528491431));
#125030=DIRECTION('',(0.711836920467366,-0.17091859381245,-0.681230528491429));
#125031=DIRECTION('center_axis',(0.,-4.12699273797265E-32,1.));
#125032=DIRECTION('ref_axis',(0.,-1.,-4.12699273797265E-32));
#125033=DIRECTION('',(-0.427290366867324,0.594430744017905,0.681230528491426));
#125034=DIRECTION('',(0.723399793963449,-0.112328558901684,-0.681230528491429));
#125035=DIRECTION('center_axis',(0.,-4.12699273797265E-32,1.));
#125036=DIRECTION('ref_axis',(0.,-1.,-4.12699273797265E-32));
#125037=DIRECTION('',(-0.474320217483799,0.557624693084348,0.681230528491426));
#125038=DIRECTION('',(0.730148561183259,-0.0529909959643429,-0.681230528491438));
#125039=DIRECTION('center_axis',(0.,-4.12699273797265E-32,1.));
#125040=DIRECTION('ref_axis',(0.,-1.,-4.12699273797265E-32));
#125041=DIRECTION('',(-0.518193545310239,0.517107741819918,0.681230528491428));
#125042=DIRECTION('',(0.732038310194444,0.00669921330825058,-0.68123052849143));
#125043=DIRECTION('center_axis',(0.,-4.12699273797265E-32,1.));
#125044=DIRECTION('ref_axis',(0.,-1.,-4.12699273797265E-32));
#125045=DIRECTION('',(-0.558618380588554,0.47314952385045,0.681230528491431));
#125046=DIRECTION('',(0.729056465029095,0.0663448404215658,-0.681230528491433));
#125047=DIRECTION('center_axis',(0.,-4.12699273797265E-32,1.));
#125048=DIRECTION('ref_axis',(0.,-1.,-4.12699273797265E-32));
#125049=DIRECTION('',(-0.595325702709605,0.426042573863934,0.681230528491427));
#125050=DIRECTION('',(0.72122286937483,0.125548953568005,-0.681230528491432));
#125051=DIRECTION('center_axis',(0.,-4.12699273797265E-32,1.));
#125052=DIRECTION('ref_axis',(0.,-1.,-4.12699273797265E-32));
#125053=DIRECTION('',(-0.628071230500946,0.376100380840428,0.681230528491429));
#125054=DIRECTION('',(0.70858965451828,0.183917559142564,-0.681230528491425));
#125055=DIRECTION('center_axis',(0.,-4.12699273797265E-32,1.));
#125056=DIRECTION('ref_axis',(0.,-1.,-4.12699273797265E-32));
#125057=DIRECTION('',(-0.656637047877765,0.323655301834624,0.681230528491429));
#125058=DIRECTION('',(0.691240892419969,0.241062223705293,-0.681230528491424));
#125059=DIRECTION('center_axis',(0.,-4.12699273797265E-32,1.));
#125060=DIRECTION('ref_axis',(0.,-1.,-4.12699273797265E-32));
#125061=DIRECTION('',(-0.680833054038444,0.269056350194477,0.681230528491429));
#125062=DIRECTION('',(0.669292036229309,0.296602658941735,-0.681230528491434));
#125063=DIRECTION('center_axis',(0.,-4.12699273797265E-32,1.));
#125064=DIRECTION('ref_axis',(0.,-1.,-4.12699273797265E-32));
#125065=DIRECTION('',(-0.700498228554044,0.212666872934959,0.681230528491429));
#125066=DIRECTION('',(0.642889151962971,0.350169252418909,-0.681230528491431));
#125067=DIRECTION('center_axis',(0.,-4.12699273797265E-32,1.));
#125068=DIRECTION('ref_axis',(0.,-1.,-4.12699273797265E-32));
#125069=DIRECTION('',(-0.715501702932687,0.154862132723623,0.681230528491433));
#125070=DIRECTION('',(0.612207946459557,0.401405527295097,-0.681230528491433));
#125071=DIRECTION('center_axis',(0.,-4.12699273797265E-32,1.));
#125072=DIRECTION('ref_axis',(0.,-1.,-4.12699273797265E-32));
#125073=DIRECTION('',(-0.725743631527792,0.0960268105694655,0.681230528491427));
#125074=DIRECTION('',(0.577452598079657,0.449970514614387,-0.681230528491433));
#125075=DIRECTION('center_axis',(0.,-4.12699273797265E-32,1.));
#125076=DIRECTION('ref_axis',(0.,-1.,-4.12699273797265E-32));
#125077=DIRECTION('',(-0.731155855994343,0.0365524458342741,0.681230528491429));
#125078=DIRECTION('',(0.538854397932528,0.495541022398819,-0.681230528491425));
#125079=DIRECTION('center_axis',(0.,-4.12699273797265E-32,1.));
#125080=DIRECTION('ref_axis',(0.,-1.,-4.12699273797265E-32));
#125081=DIRECTION('',(-0.731702358871478,-0.0231651693972153,0.68123052849143));
#125082=DIRECTION('',(0.496670210671855,0.53781378643771,-0.681230528491426));
#125083=DIRECTION('center_axis',(0.,-4.12699273797265E-32,1.));
#125084=DIRECTION('ref_axis',(0.,-1.,-4.12699273797265E-32));
#125085=DIRECTION('',(-0.72737950327272,-0.0827286242483435,0.681230528491426));
#125086=DIRECTION('',(0.451180765103981,0.576507488460881,-0.681230528491431));
#125087=DIRECTION('center_axis',(0.,-4.12699273797265E-32,1.));
#125088=DIRECTION('ref_axis',(0.,-1.,-4.12699273797265E-32));
#125089=DIRECTION('',(-0.718216057088845,-0.141741533754371,0.681230528491429));
#125090=DIRECTION('',(0.402688785983913,0.611364628265397,-0.681230528491432));
#125091=DIRECTION('center_axis',(0.,-4.12699273797265E-32,1.));
#125092=DIRECTION('ref_axis',(0.,-1.,-4.12699273797265E-32));
#125093=DIRECTION('',(-0.70427300154235,-0.199811176738967,0.681230528491434));
#125094=DIRECTION('',(0.351516979432122,0.642153237336857,-0.681230528491429));
#125095=DIRECTION('center_axis',(0.,-4.12699273797265E-32,1.));
#125096=DIRECTION('ref_axis',(0.,-1.,-4.12699273797265E-32));
#125097=DIRECTION('',(-0.685643125367468,-0.256551109308884,0.68123052849143));
#125098=DIRECTION('',(0.298005885378418,0.668668422561672,-0.681230528491428));
#125099=DIRECTION('center_axis',(0.,-4.12699273797265E-32,1.));
#125100=DIRECTION('ref_axis',(0.,-1.,-4.12699273797265E-32));
#125101=DIRECTION('',(-0.662450407316412,-0.311583736574311,0.681230528491427));
#125102=DIRECTION('',(0.242511611325018,0.690733729756874,-0.681230528491421));
#125103=DIRECTION('center_axis',(0.,-4.12699273797265E-32,1.));
#125104=DIRECTION('ref_axis',(0.,-1.,-4.12699273797265E-32));
#125105=DIRECTION('',(-0.634849191101292,-0.364542825480524,0.681230528491429));
#125106=DIRECTION('',(0.185403462509872,0.708202317943561,-0.681230528491434));
#125107=DIRECTION('center_axis',(0.,-4.12699273797265E-32,1.));
#125108=DIRECTION('ref_axis',(0.,-1.,-4.12699273797265E-32));
#125109=DIRECTION('',(-0.603023158262138,-0.415075942028502,0.681230528491426));
#125110=DIRECTION('',(0.127061484241121,0.720957936549513,-0.681230528491429));
#125111=DIRECTION('center_axis',(0.,-4.12699273797265E-32,1.));
#125112=DIRECTION('ref_axis',(0.,-1.,-4.12699273797265E-32));
#125113=DIRECTION('',(-0.567184105796557,-0.462846796664993,0.681230528491431));
#125114=DIRECTION('',(0.0678739327584265,0.728915699037399,-0.681230528491438));
#125115=DIRECTION('center_axis',(0.,-4.12699273797265E-32,1.));
#125116=DIRECTION('ref_axis',(0.,-1.,-4.12699273797265E-32));
#125117=DIRECTION('',(-0.527570536685702,-0.507537482234019,0.68123052849143));
#125118=DIRECTION('',(0.00823469145162862,0.732022647810838,-0.681230528491425));
#125119=DIRECTION('center_axis',(0.,-4.12699273797265E-32,1.));
#125120=DIRECTION('ref_axis',(0.,-1.,-4.12699273797265E-32));
#125121=DIRECTION('',(-0.48444607269621,-0.548850589596576,0.681230528491428));
#125122=DIRECTION('',(-0.0514593503681429,0.730258106638313,-0.681230528491432));
#125123=DIRECTION('center_axis',(0.,-4.12699273797265E-32,1.));
#125124=DIRECTION('ref_axis',(0.,-1.,-4.12699273797265E-32));
#125125=DIRECTION('',(-0.438097700020894,-0.586511186839349,0.681230528491422));
#125126=DIRECTION('',(-0.110810938701414,0.723633818250228,-0.681230528491426));
#125127=DIRECTION('center_axis',(0.,-4.12699273797265E-32,1.));
#125128=DIRECTION('ref_axis',(0.,-1.,-4.12699273797265E-32));
#125129=DIRECTION('',(-0.388833859432984,-0.620268648901214,0.68123052849143));
#125130=DIRECTION('',(-0.16942509852015,0.712193866192848,-0.681230528491436));
#125131=DIRECTION('center_axis',(0.,-4.12699273797265E-32,1.));
#125132=DIRECTION('ref_axis',(0.,-1.,-4.12699273797265E-32));
#125133=DIRECTION('',(-0.336982393663615,-0.649898325441775,0.681230528491433));
#125134=DIRECTION('',(-0.226911762261403,0.696014381459684,-0.681230528491434));
#125135=DIRECTION('center_axis',(0.,-4.12699273797265E-32,1.));
#125136=DIRECTION('ref_axis',(0.,-1.,-4.12699273797265E-32));
#125137=DIRECTION('',(-0.282888365662603,-0.675203035852198,0.681230528491433));
#125138=DIRECTION('center_axis',(0.,-4.12699273797265E-32,1.));
#125139=DIRECTION('ref_axis',(0.,-1.,0.));
#125140=DIRECTION('center_axis',(0.,-4.12699273797265E-32,1.));
#125141=DIRECTION('ref_axis',(0.,-1.,-4.12699273797265E-32));
#125142=DIRECTION('center_axis',(-1.,-1.22464679914735E-16,-5.05410844666257E-48));
#125143=DIRECTION('ref_axis',(-1.22464679914735E-16,1.,0.));
#125144=DIRECTION('center_axis',(0.,-4.12699273797265E-32,1.));
#125145=DIRECTION('ref_axis',(0.,-1.,-4.12699273797265E-32));
#125146=DIRECTION('center_axis',(0.,-4.12699273797265E-32,1.));
#125147=DIRECTION('ref_axis',(0.,-1.,-4.12699273797265E-32));
#125148=DIRECTION('',(-2.24445597957705E-36,4.11599200331947E-32,-1.));
#125149=DIRECTION('',(2.24445597957705E-36,-4.11599200331947E-32,1.));
#125150=DIRECTION('center_axis',(0.,-4.12699273797265E-32,1.));
#125151=DIRECTION('ref_axis',(0.,-1.,-4.12699273797265E-32));
#125152=DIRECTION('',(-6.71843145449713E-36,4.11602859211924E-32,-1.));
#125153=DIRECTION('',(6.71843145449713E-36,-4.11602859211924E-32,1.));
#125154=DIRECTION('center_axis',(0.,-4.12699273797265E-32,1.));
#125155=DIRECTION('ref_axis',(0.,-1.,-4.12699273797265E-32));
#125156=DIRECTION('',(-1.11476968765511E-35,4.11610152622635E-32,-1.));
#125157=DIRECTION('',(1.11476968765511E-35,-4.11610152622635E-32,1.));
#125158=DIRECTION('center_axis',(0.,-4.12699273797265E-32,1.));
#125159=DIRECTION('ref_axis',(0.,-1.,-4.12699273797265E-32));
#125160=DIRECTION('',(-1.5502776215132E-35,4.11621032027636E-32,-1.));
#125161=DIRECTION('',(1.5502776215132E-35,-4.11621032027636E-32,1.));
#125162=DIRECTION('center_axis',(0.,-4.12699273797265E-32,1.));
#125163=DIRECTION('ref_axis',(0.,-1.,-4.12699273797265E-32));
#125164=DIRECTION('',(-1.97546871357812E-35,4.11635425026281E-32,-1.));
#125165=DIRECTION('',(1.97546871357812E-35,-4.11635425026281E-32,1.));
#125166=DIRECTION('center_axis',(0.,-4.12699273797265E-32,1.));
#125167=DIRECTION('ref_axis',(0.,-1.,-4.12699273797265E-32));
#125168=DIRECTION('',(-2.3875133872833E-35,4.11653235835539E-32,-1.));
#125169=DIRECTION('',(2.3875133872833E-35,-4.11653235835539E-32,1.));
#125170=DIRECTION('center_axis',(0.,-4.12699273797265E-32,1.));
#125171=DIRECTION('ref_axis',(0.,-1.,-4.12699273797265E-32));
#125172=DIRECTION('',(-2.78366955330785E-35,4.11674345927413E-32,-1.));
#125173=DIRECTION('',(2.78366955330785E-35,-4.11674345927413E-32,1.));
#125174=DIRECTION('center_axis',(0.,-4.12699273797265E-32,1.));
#125175=DIRECTION('ref_axis',(0.,-1.,-4.12699273797265E-32));
#125176=DIRECTION('',(-3.1613008577281E-35,4.11698614817723E-32,-1.));
#125177=DIRECTION('',(3.1613008577281E-35,-4.11698614817723E-32,1.));
#125178=DIRECTION('center_axis',(0.,-4.12699273797265E-32,1.));
#125179=DIRECTION('ref_axis',(0.,-1.,-4.12699273797265E-32));
#125180=DIRECTION('',(-3.51789422651897E-35,4.1172588100101E-32,-1.));
#125181=DIRECTION('',(3.51789422651897E-35,-4.1172588100101E-32,1.));
#125182=DIRECTION('center_axis',(0.,-4.12699273797265E-32,1.));
#125183=DIRECTION('ref_axis',(0.,-1.,-4.12699273797265E-32));
#125184=DIRECTION('',(-3.85107658964331E-35,4.11755963025323E-32,-1.));
#125185=DIRECTION('',(3.85107658964331E-35,-4.11755963025323E-32,1.));
#125186=DIRECTION('center_axis',(0.,-4.12699273797265E-32,1.));
#125187=DIRECTION('ref_axis',(0.,-1.,-4.12699273797265E-32));
#125188=DIRECTION('',(-4.1586306734472E-35,4.11788660699752E-32,-1.));
#125189=DIRECTION('',(4.1586306734472E-35,-4.11788660699752E-32,1.));
#125190=DIRECTION('center_axis',(0.,-4.12699273797265E-32,1.));
#125191=DIRECTION('ref_axis',(0.,-1.,-4.12699273797265E-32));
#125192=DIRECTION('',(-4.43850975624469E-35,4.11823756426669E-32,-1.));
#125193=DIRECTION('',(4.43850975624469E-35,-4.11823756426669E-32,1.));
#125194=DIRECTION('center_axis',(0.,-4.12699273797265E-32,1.));
#125195=DIRECTION('ref_axis',(0.,-1.,-4.12699273797265E-32));
#125196=DIRECTION('',(-4.6888512889172E-35,4.11861016649801E-32,-1.));
#125197=DIRECTION('',(4.6888512889172E-35,-4.11861016649801E-32,1.));
#125198=DIRECTION('center_axis',(0.,-4.12699273797265E-32,1.));
#125199=DIRECTION('ref_axis',(0.,-1.,-4.12699273797265E-32));
#125200=DIRECTION('',(-4.90798928986703E-35,4.11900193408512E-32,-1.));
#125201=DIRECTION('',(4.90798928986703E-35,-4.11900193408512E-32,1.));
#125202=DIRECTION('center_axis',(0.,-4.12699273797265E-32,1.));
#125203=DIRECTION('ref_axis',(0.,-1.,-4.12699273797265E-32));
#125204=DIRECTION('',(-5.09446543185543E-35,4.11941025987936E-32,-1.));
#125205=DIRECTION('',(5.09446543185543E-35,-4.11941025987936E-32,1.));
#125206=DIRECTION('center_axis',(0.,-4.12699273797265E-32,1.));
#125207=DIRECTION('ref_axis',(0.,-1.,-4.12699273797265E-32));
#125208=DIRECTION('',(-5.24703874692283E-35,4.11983242653994E-32,-1.));
#125209=DIRECTION('',(5.24703874692283E-35,-4.11983242653994E-32,1.));
#125210=DIRECTION('center_axis',(0.,-4.12699273797265E-32,1.));
#125211=DIRECTION('ref_axis',(0.,-1.,-4.12699273797265E-32));
#125212=DIRECTION('',(-5.36469388482745E-35,4.12026562461737E-32,-1.));
#125213=DIRECTION('',(5.36469388482745E-35,-4.12026562461737E-32,1.));
#125214=DIRECTION('center_axis',(0.,-4.12699273797265E-32,1.));
#125215=DIRECTION('ref_axis',(0.,-1.,-4.12699273797265E-32));
#125216=DIRECTION('',(-5.44664787004251E-35,4.12070697124994E-32,-1.));
#125217=DIRECTION('',(5.44664787004251E-35,-4.12070697124994E-32,1.));
#125218=DIRECTION('center_axis',(0.,-4.12699273797265E-32,1.));
#125219=DIRECTION('ref_axis',(0.,-1.,-4.12699273797265E-32));
#125220=DIRECTION('',(-5.49235531231428E-35,4.12115352934861E-32,-1.));
#125221=DIRECTION('',(5.49235531231428E-35,-4.12115352934861E-32,1.));
#125222=DIRECTION('center_axis',(0.,-4.12699273797265E-32,1.));
#125223=DIRECTION('ref_axis',(0.,-1.,-4.12699273797265E-32));
#125224=DIRECTION('',(-5.50151203616034E-35,4.12160232714293E-32,-1.));
#125225=DIRECTION('',(5.50151203616034E-35,-4.12160232714293E-32,1.));
#125226=DIRECTION('center_axis',(0.,-4.12699273797265E-32,1.));
#125227=DIRECTION('ref_axis',(0.,-1.,-4.12699273797265E-32));
#125228=DIRECTION('',(-5.47405710508952E-35,4.1220503779576E-32,-1.));
#125229=DIRECTION('',(5.47405710508952E-35,-4.1220503779576E-32,1.));
#125230=DIRECTION('center_axis',(0.,-4.12699273797265E-32,1.));
#125231=DIRECTION('ref_axis',(0.,-1.,-4.12699273797265E-32));
#125232=DIRECTION('',(-5.41017322714156E-35,4.12249470008839E-32,-1.));
#125233=DIRECTION('',(5.41017322714156E-35,-4.12249470008839E-32,1.));
#125234=DIRECTION('center_axis',(0.,-4.12699273797265E-32,1.));
#125235=DIRECTION('ref_axis',(0.,-1.,-4.12699273797265E-32));
#125236=DIRECTION('',(-5.3102855389809E-35,4.12293233664482E-32,-1.));
#125237=DIRECTION('',(5.3102855389809E-35,-4.12293233664482E-32,1.));
#125238=DIRECTION('center_axis',(0.,-4.12699273797265E-32,1.));
#125239=DIRECTION('ref_axis',(0.,-1.,-4.12699273797265E-32));
#125240=DIRECTION('',(-5.17505877669541E-35,4.12336037522781E-32,-1.));
#125241=DIRECTION('',(5.17505877669541E-35,-4.12336037522781E-32,1.));
#125242=DIRECTION('center_axis',(0.,-4.12699273797265E-32,1.));
#125243=DIRECTION('ref_axis',(0.,-1.,-4.12699273797265E-32));
#125244=DIRECTION('',(-5.00539285207499E-35,4.12377596731122E-32,-1.));
#125245=DIRECTION('',(5.00539285207499E-35,-4.12377596731122E-32,1.));
#125246=DIRECTION('center_axis',(0.,-4.12699273797265E-32,1.));
#125247=DIRECTION('ref_axis',(0.,-1.,-4.12699273797265E-32));
#125248=DIRECTION('',(-4.80241686385389E-35,4.1241763471983E-32,-1.));
#125249=DIRECTION('',(4.80241686385389E-35,-4.1241763471983E-32,1.));
#125250=DIRECTION('center_axis',(0.,-4.12699273797265E-32,1.));
#125251=DIRECTION('ref_axis',(0.,-1.,-4.12699273797265E-32));
#125252=DIRECTION('',(-4.56748158374851E-35,4.12455885042696E-32,-1.));
#125253=DIRECTION('',(4.56748158374851E-35,-4.12455885042696E-32,1.));
#125254=DIRECTION('center_axis',(0.,-4.12699273797265E-32,1.));
#125255=DIRECTION('ref_axis',(0.,-1.,-4.12699273797265E-32));
#125256=DIRECTION('',(-4.30215046728491E-35,4.12492093150131E-32,-1.));
#125257=DIRECTION('',(4.30215046728491E-35,-4.12492093150131E-32,1.));
#125258=DIRECTION('center_axis',(0.,-4.12699273797265E-32,1.));
#125259=DIRECTION('ref_axis',(0.,-1.,-4.12699273797265E-32));
#125260=DIRECTION('',(-4.00818924926601E-35,4.12526018083156E-32,-1.));
#125261=DIRECTION('',(4.00818924926601E-35,-4.12526018083156E-32,1.));
#125262=DIRECTION('center_axis',(0.,-4.12699273797265E-32,1.));
#125263=DIRECTION('ref_axis',(0.,-1.,-4.12699273797265E-32));
#125264=DIRECTION('',(-3.68755419309802E-35,4.12557434076937E-32,-1.));
#125265=DIRECTION('',(3.68755419309802E-35,-4.12557434076937E-32,1.));
#125266=DIRECTION('center_axis',(0.,-4.12699273797265E-32,1.));
#125267=DIRECTION('ref_axis',(0.,-1.,-4.12699273797265E-32));
#125268=DIRECTION('',(-3.34237907217807E-35,4.1258613206322E-32,-1.));
#125269=DIRECTION('',(3.34237907217807E-35,-4.1258613206322E-32,1.));
#125270=DIRECTION('center_axis',(0.,-4.12699273797265E-32,1.));
#125271=DIRECTION('ref_axis',(0.,-1.,-4.12699273797265E-32));
#125272=DIRECTION('',(-2.97496096998759E-35,4.1261192106164E-32,-1.));
#125273=DIRECTION('',(2.97496096998759E-35,-4.1261192106164E-32,1.));
#125274=DIRECTION('center_axis',(0.,-4.12699273797265E-32,1.));
#125275=DIRECTION('ref_axis',(0.,-1.,-4.12699273797265E-32));
#125276=DIRECTION('',(-2.58774499337527E-35,4.12634629450669E-32,-1.));
#125277=DIRECTION('',(2.58774499337527E-35,-4.12634629450669E-32,1.));
#125278=DIRECTION('center_axis',(0.,-4.12699273797265E-32,1.));
#125279=DIRECTION('ref_axis',(0.,-1.,-4.12699273797265E-32));
#125280=DIRECTION('',(-2.18330800078025E-35,4.12654106109723E-32,-1.));
#125281=DIRECTION('',(2.18330800078025E-35,-4.12654106109723E-32,1.));
#125282=DIRECTION('center_axis',(0.,-4.12699273797265E-32,1.));
#125283=DIRECTION('ref_axis',(0.,-1.,-4.12699273797265E-32));
#125284=DIRECTION('',(-1.76434145365967E-35,4.1267022142485E-32,-1.));
#125285=DIRECTION('',(1.76434145365967E-35,-4.1267022142485E-32,1.));
#125286=DIRECTION('center_axis',(0.,-4.12699273797265E-32,1.));
#125287=DIRECTION('ref_axis',(0.,-1.,-4.12699273797265E-32));
#125288=DIRECTION('',(-1.3336335052612E-35,4.12682868151287E-32,-1.));
#125289=DIRECTION('',(1.3336335052612E-35,-4.12682868151287E-32,1.));
#125290=DIRECTION('center_axis',(0.,-4.12699273797265E-32,1.));
#125291=DIRECTION('ref_axis',(0.,-1.,-4.12699273797265E-32));
#125292=DIRECTION('',(-8.94050445919518E-36,4.12691962127155E-32,-1.));
#125293=DIRECTION('',(8.94050445919518E-36,-4.12691962127155E-32,1.));
#125294=DIRECTION('center_axis',(0.,-4.12699273797265E-32,1.));
#125295=DIRECTION('ref_axis',(0.,-1.,-4.12699273797265E-32));
#125296=DIRECTION('',(-4.48517628368065E-36,4.12697442833547E-32,-1.));
#125297=DIRECTION('',(4.48517628368065E-36,-4.12697442833547E-32,1.));
#125298=DIRECTION('center_axis',(0.,-4.12699273797265E-32,1.));
#125299=DIRECTION('ref_axis',(0.,-1.,-4.12699273797265E-32));
#125300=DIRECTION('',(0.,4.12699273797265E-32,-1.));
#125301=DIRECTION('',(0.,4.12699273797265E-32,-1.));
#125302=DIRECTION('',(0.,-4.12699273797265E-32,1.));
#125303=DIRECTION('center_axis',(0.,-4.12699273797265E-32,1.));
#125304=DIRECTION('ref_axis',(0.,-1.,-4.12699273797265E-32));
#125305=DIRECTION('',(4.48517628367996E-36,4.12697442833547E-32,-1.));
#125306=DIRECTION('',(-4.48517628367996E-36,-4.12697442833547E-32,1.));
#125307=DIRECTION('center_axis',(0.,-4.12699273797265E-32,1.));
#125308=DIRECTION('ref_axis',(0.,-1.,-4.12699273797265E-32));
#125309=DIRECTION('',(8.94050445919518E-36,4.12691962127156E-32,-1.));
#125310=DIRECTION('',(-8.94050445919518E-36,-4.12691962127156E-32,1.));
#125311=DIRECTION('center_axis',(0.,-4.12699273797265E-32,1.));
#125312=DIRECTION('ref_axis',(0.,-1.,-4.12699273797265E-32));
#125313=DIRECTION('',(1.3336335052612E-35,4.12682868151287E-32,-1.));
#125314=DIRECTION('',(-1.3336335052612E-35,-4.12682868151287E-32,1.));
#125315=DIRECTION('center_axis',(0.,-4.12699273797265E-32,1.));
#125316=DIRECTION('ref_axis',(0.,-1.,-4.12699273797265E-32));
#125317=DIRECTION('',(1.76434145365967E-35,4.1267022142485E-32,-1.));
#125318=DIRECTION('',(-1.76434145365967E-35,-4.1267022142485E-32,1.));
#125319=DIRECTION('center_axis',(0.,-4.12699273797265E-32,1.));
#125320=DIRECTION('ref_axis',(0.,-1.,-4.12699273797265E-32));
#125321=DIRECTION('',(2.18330800077971E-35,4.12654106109723E-32,-1.));
#125322=DIRECTION('',(-2.18330800077971E-35,-4.12654106109723E-32,1.));
#125323=DIRECTION('center_axis',(0.,-4.12699273797265E-32,1.));
#125324=DIRECTION('ref_axis',(0.,-1.,-4.12699273797265E-32));
#125325=DIRECTION('',(2.58774499337554E-35,4.12634629450669E-32,-1.));
#125326=DIRECTION('',(-2.58774499337554E-35,-4.12634629450669E-32,1.));
#125327=DIRECTION('center_axis',(0.,-4.12699273797265E-32,1.));
#125328=DIRECTION('ref_axis',(0.,-1.,-4.12699273797265E-32));
#125329=DIRECTION('',(2.97496096998732E-35,4.1261192106164E-32,-1.));
#125330=DIRECTION('',(-2.97496096998732E-35,-4.1261192106164E-32,1.));
#125331=DIRECTION('center_axis',(0.,-4.12699273797265E-32,1.));
#125332=DIRECTION('ref_axis',(0.,-1.,-4.12699273797265E-32));
#125333=DIRECTION('',(3.34237907217862E-35,4.1258613206322E-32,-1.));
#125334=DIRECTION('',(-3.34237907217862E-35,-4.1258613206322E-32,1.));
#125335=DIRECTION('center_axis',(0.,-4.12699273797265E-32,1.));
#125336=DIRECTION('ref_axis',(0.,-1.,-4.12699273797265E-32));
#125337=DIRECTION('',(3.68755419309748E-35,4.12557434076937E-32,-1.));
#125338=DIRECTION('',(-3.68755419309748E-35,-4.12557434076937E-32,1.));
#125339=DIRECTION('center_axis',(0.,-4.12699273797265E-32,1.));
#125340=DIRECTION('ref_axis',(0.,-1.,-4.12699273797265E-32));
#125341=DIRECTION('',(4.00818924926656E-35,4.12526018083156E-32,-1.));
#125342=DIRECTION('',(-4.00818924926656E-35,-4.12526018083156E-32,1.));
#125343=DIRECTION('center_axis',(0.,-4.12699273797265E-32,1.));
#125344=DIRECTION('ref_axis',(0.,-1.,-4.12699273797265E-32));
#125345=DIRECTION('',(4.30215046728545E-35,4.12492093150131E-32,-1.));
#125346=DIRECTION('',(-4.30215046728545E-35,-4.12492093150131E-32,1.));
#125347=DIRECTION('center_axis',(0.,-4.12699273797265E-32,1.));
#125348=DIRECTION('ref_axis',(0.,-1.,-4.12699273797265E-32));
#125349=DIRECTION('',(4.56748158374851E-35,4.12455885042696E-32,-1.));
#125350=DIRECTION('',(-4.56748158374851E-35,-4.12455885042696E-32,1.));
#125351=DIRECTION('center_axis',(0.,-4.12699273797265E-32,1.));
#125352=DIRECTION('ref_axis',(0.,-1.,-4.12699273797265E-32));
#125353=DIRECTION('',(4.80241686385389E-35,4.1241763471983E-32,-1.));
#125354=DIRECTION('',(-4.80241686385389E-35,-4.1241763471983E-32,1.));
#125355=DIRECTION('center_axis',(0.,-4.12699273797265E-32,1.));
#125356=DIRECTION('ref_axis',(0.,-1.,-4.12699273797265E-32));
#125357=DIRECTION('',(5.00539285207335E-35,4.12377596731122E-32,-1.));
#125358=DIRECTION('',(-5.00539285207335E-35,-4.12377596731122E-32,1.));
#125359=DIRECTION('center_axis',(0.,-4.12699273797265E-32,1.));
#125360=DIRECTION('ref_axis',(0.,-1.,-4.12699273797265E-32));
#125361=DIRECTION('',(5.17505877669431E-35,4.12336037522781E-32,-1.));
#125362=DIRECTION('',(-5.17505877669431E-35,-4.12336037522781E-32,1.));
#125363=DIRECTION('center_axis',(0.,-4.12699273797265E-32,1.));
#125364=DIRECTION('ref_axis',(0.,-1.,-4.12699273797265E-32));
#125365=DIRECTION('',(5.31028553898035E-35,4.12293233664482E-32,-1.));
#125366=DIRECTION('',(-5.31028553898035E-35,-4.12293233664482E-32,1.));
#125367=DIRECTION('center_axis',(0.,-4.12699273797265E-32,1.));
#125368=DIRECTION('ref_axis',(0.,-1.,-4.12699273797265E-32));
#125369=DIRECTION('',(5.41017322714046E-35,4.12249470008839E-32,-1.));
#125370=DIRECTION('',(-5.41017322714046E-35,-4.12249470008839E-32,1.));
#125371=DIRECTION('center_axis',(0.,-4.12699273797265E-32,1.));
#125372=DIRECTION('ref_axis',(0.,-1.,-4.12699273797265E-32));
#125373=DIRECTION('',(5.47405710508952E-35,4.1220503779576E-32,-1.));
#125374=DIRECTION('',(-5.47405710508952E-35,-4.1220503779576E-32,1.));
#125375=DIRECTION('center_axis',(0.,-4.12699273797265E-32,1.));
#125376=DIRECTION('ref_axis',(0.,-1.,-4.12699273797265E-32));
#125377=DIRECTION('',(5.50151203615979E-35,4.12160232714292E-32,-1.));
#125378=DIRECTION('',(-5.50151203615979E-35,-4.12160232714292E-32,1.));
#125379=DIRECTION('center_axis',(0.,-4.12699273797265E-32,1.));
#125380=DIRECTION('ref_axis',(0.,-1.,-4.12699273797265E-32));
#125381=DIRECTION('',(5.49235531231592E-35,4.12115352934861E-32,-1.));
#125382=DIRECTION('',(-5.49235531231592E-35,-4.12115352934861E-32,1.));
#125383=DIRECTION('center_axis',(0.,-4.12699273797265E-32,1.));
#125384=DIRECTION('ref_axis',(0.,-1.,-4.12699273797265E-32));
#125385=DIRECTION('',(5.44664787004196E-35,4.12070697124994E-32,-1.));
#125386=DIRECTION('',(-5.44664787004196E-35,-4.12070697124994E-32,1.));
#125387=DIRECTION('center_axis',(0.,-4.12699273797265E-32,1.));
#125388=DIRECTION('ref_axis',(0.,-1.,-4.12699273797265E-32));
#125389=DIRECTION('',(5.36469388482745E-35,4.12026562461737E-32,-1.));
#125390=DIRECTION('',(-5.36469388482745E-35,-4.12026562461737E-32,1.));
#125391=DIRECTION('center_axis',(0.,-4.12699273797265E-32,1.));
#125392=DIRECTION('ref_axis',(0.,-1.,-4.12699273797265E-32));
#125393=DIRECTION('',(5.24703874692173E-35,4.11983242653994E-32,-1.));
#125394=DIRECTION('',(-5.24703874692173E-35,-4.11983242653994E-32,1.));
#125395=DIRECTION('center_axis',(0.,-4.12699273797265E-32,1.));
#125396=DIRECTION('ref_axis',(0.,-1.,-4.12699273797265E-32));
#125397=DIRECTION('',(5.09446543185489E-35,4.11941025987936E-32,-1.));
#125398=DIRECTION('',(-5.09446543185489E-35,-4.11941025987936E-32,1.));
#125399=DIRECTION('center_axis',(0.,-4.12699273797265E-32,1.));
#125400=DIRECTION('ref_axis',(0.,-1.,-4.12699273797265E-32));
#125401=DIRECTION('',(4.90798928986758E-35,4.11900193408512E-32,-1.));
#125402=DIRECTION('',(-4.90798928986758E-35,-4.11900193408512E-32,1.));
#125403=DIRECTION('center_axis',(0.,-4.12699273797265E-32,1.));
#125404=DIRECTION('ref_axis',(0.,-1.,-4.12699273797265E-32));
#125405=DIRECTION('',(4.6888512889172E-35,4.11861016649801E-32,-1.));
#125406=DIRECTION('',(-4.6888512889172E-35,-4.11861016649801E-32,1.));
#125407=DIRECTION('center_axis',(0.,-4.12699273797265E-32,1.));
#125408=DIRECTION('ref_axis',(0.,-1.,-4.12699273797265E-32));
#125409=DIRECTION('',(4.43850975624469E-35,4.11823756426669E-32,-1.));
#125410=DIRECTION('',(-4.43850975624469E-35,-4.11823756426669E-32,1.));
#125411=DIRECTION('center_axis',(0.,-4.12699273797265E-32,1.));
#125412=DIRECTION('ref_axis',(0.,-1.,-4.12699273797265E-32));
#125413=DIRECTION('',(4.15863067344775E-35,4.11788660699752E-32,-1.));
#125414=DIRECTION('',(-4.15863067344775E-35,-4.11788660699752E-32,1.));
#125415=DIRECTION('center_axis',(0.,-4.12699273797265E-32,1.));
#125416=DIRECTION('ref_axis',(0.,-1.,-4.12699273797265E-32));
#125417=DIRECTION('',(3.85107658964385E-35,4.11755963025323E-32,-1.));
#125418=DIRECTION('',(-3.85107658964385E-35,-4.11755963025323E-32,1.));
#125419=DIRECTION('center_axis',(0.,-4.12699273797265E-32,1.));
#125420=DIRECTION('ref_axis',(0.,-1.,-4.12699273797265E-32));
#125421=DIRECTION('',(3.51789422651897E-35,4.1172588100101E-32,-1.));
#125422=DIRECTION('',(-3.51789422651897E-35,-4.1172588100101E-32,1.));
#125423=DIRECTION('center_axis',(0.,-4.12699273797265E-32,1.));
#125424=DIRECTION('ref_axis',(0.,-1.,-4.12699273797265E-32));
#125425=DIRECTION('',(3.16130085772864E-35,4.11698614817723E-32,-1.));
#125426=DIRECTION('',(-3.16130085772864E-35,-4.11698614817723E-32,1.));
#125427=DIRECTION('center_axis',(0.,-4.12699273797265E-32,1.));
#125428=DIRECTION('ref_axis',(0.,-1.,-4.12699273797265E-32));
#125429=DIRECTION('',(2.7836695533073E-35,4.11674345927413E-32,-1.));
#125430=DIRECTION('',(-2.7836695533073E-35,-4.11674345927413E-32,1.));
#125431=DIRECTION('center_axis',(0.,-4.12699273797265E-32,1.));
#125432=DIRECTION('ref_axis',(0.,-1.,-4.12699273797265E-32));
#125433=DIRECTION('',(2.38751338728303E-35,4.11653235835539E-32,-1.));
#125434=DIRECTION('',(-2.38751338728303E-35,-4.11653235835539E-32,1.));
#125435=DIRECTION('center_axis',(0.,-4.12699273797265E-32,1.));
#125436=DIRECTION('ref_axis',(0.,-1.,-4.12699273797265E-32));
#125437=DIRECTION('',(1.9754687135784E-35,4.11635425026281E-32,-1.));
#125438=DIRECTION('',(-1.9754687135784E-35,-4.11635425026281E-32,1.));
#125439=DIRECTION('center_axis',(0.,-4.12699273797265E-32,1.));
#125440=DIRECTION('ref_axis',(0.,-1.,-4.12699273797265E-32));
#125441=DIRECTION('',(1.55027762151293E-35,4.11621032027636E-32,-1.));
#125442=DIRECTION('',(-1.55027762151293E-35,-4.11621032027636E-32,1.));
#125443=DIRECTION('center_axis',(0.,-4.12699273797265E-32,1.));
#125444=DIRECTION('ref_axis',(0.,-1.,-4.12699273797265E-32));
#125445=DIRECTION('',(1.11476968765511E-35,4.11610152622635E-32,-1.));
#125446=DIRECTION('',(-1.11476968765511E-35,-4.11610152622635E-32,1.));
#125447=DIRECTION('center_axis',(0.,-4.12699273797265E-32,1.));
#125448=DIRECTION('ref_axis',(0.,-1.,-4.12699273797265E-32));
#125449=DIRECTION('',(6.7184314544985E-36,4.11602859211924E-32,-1.));
#125450=DIRECTION('',(-6.7184314544985E-36,-4.11602859211924E-32,1.));
#125451=DIRECTION('center_axis',(0.,-4.12699273797265E-32,1.));
#125452=DIRECTION('ref_axis',(0.,-1.,-4.12699273797265E-32));
#125453=DIRECTION('',(2.24445597957774E-36,4.11599200331947E-32,-1.));
#125454=DIRECTION('',(-2.24445597957774E-36,-4.11599200331947E-32,1.));
#125455=DIRECTION('center_axis',(0.,-4.12699273797265E-32,1.));
#125456=DIRECTION('ref_axis',(0.,-1.,0.));
#125457=DIRECTION('center_axis',(-0.964116593759479,0.265479120587077,0.000173694938042578));
#125458=DIRECTION('ref_axis',(0.262650981856607,0.953940735958569,-0.14495355810943));
#125459=DIRECTION('center_axis',(0.964117203276892,0.265476906397448,0.000174685963057186));
#125460=DIRECTION('ref_axis',(0.261983001398329,-0.951534581673234,0.161080249746099));
#125461=DIRECTION('center_axis',(0.,-4.12699273797265E-32,1.));
#125462=DIRECTION('ref_axis',(0.,-1.,0.));
#125463=DIRECTION('center_axis',(-0.784008375826398,0.620750220393733,0.000174685963051847));
#125464=DIRECTION('ref_axis',(0.612666106769434,0.77375279952214,0.161080249713102));
#125465=DIRECTION('center_axis',(0.355732454713716,-0.934587818502586,0.000173694938015866));
#125466=DIRECTION('ref_axis',(0.924708188924584,0.351998908103049,0.14495355818357));
#125467=DIRECTION('center_axis',(0.,-4.12699273797265E-32,1.));
#125468=DIRECTION('ref_axis',(0.,-1.,0.));
#125469=DIRECTION('center_axis',(0.278371200818614,-0.960473552152724,0.000173694938036704));
#125470=DIRECTION('ref_axis',(0.950322477522101,0.275455358806153,0.144953558153051));
#125471=DIRECTION('center_axis',(-0.730802746906005,0.682588686252162,0.000174685963045779));
#125472=DIRECTION('ref_axis',(0.67369554717971,0.721240225503635,0.161080249645006));
#125473=DIRECTION('center_axis',(0.,-4.12699273797265E-32,1.));
#125474=DIRECTION('ref_axis',(0.,-1.,0.));
#125475=DIRECTION('center_axis',(0.199157432510043,-0.979967492780284,0.000173694938040826));
#125476=DIRECTION('ref_axis',(0.969612526830206,0.197078699543833,0.144953558080011));
#125477=DIRECTION('center_axis',(-0.672733746278912,0.739884637022796,0.000174685963050579));
#125478=DIRECTION('ref_axis',(0.730241654858009,0.663927916762316,0.161080249732511));
#125479=DIRECTION('center_axis',(0.,-4.12699273797265E-32,1.));
#125480=DIRECTION('ref_axis',(0.,-1.,0.));
#125481=DIRECTION('center_axis',(0.118618304346775,-0.992939911426651,0.00017369493805128));
#125482=DIRECTION('ref_axis',(0.98244996474591,0.117390514049851,0.14495355801729));
#125483=DIRECTION('center_axis',(-0.610187813563555,0.792256777606442,0.000174685963065682));
#125484=DIRECTION('ref_axis',(0.781928124821259,0.602197277291061,0.161080249679293));
#125485=DIRECTION('center_axis',(0.,-4.12699273797265E-32,1.));
#125486=DIRECTION('ref_axis',(0.,-1.,0.));
#125487=DIRECTION('center_axis',(0.0372897909386947,-0.999304478786029,
0.000173694938041732));
#125488=DIRECTION('ref_axis',(0.988749360215715,0.0369211140505736,0.144953558115277));
#125489=DIRECTION('center_axis',(-0.54358118162286,0.83935658004826,0.000174685963067228));
#125490=DIRECTION('ref_axis',(0.828410992105546,0.536459114282095,0.161080249758856));
#125491=DIRECTION('center_axis',(0.,-4.12699273797265E-32,1.));
#125492=DIRECTION('ref_axis',(0.,-1.,0.));
#125493=DIRECTION('center_axis',(-0.0442868798756908,-0.999018839712718,
0.000173694938034547));
#125494=DIRECTION('ref_axis',(0.988468791846664,-0.0437939898697778,0.144953558067689));
#125495=DIRECTION('center_axis',(-0.473357106603132,0.880870602933896,0.000174685963033159));
#125496=DIRECTION('ref_axis',(0.869380920935805,0.467150904390525,0.161080249689174));
#125497=DIRECTION('center_axis',(0.,-4.12699273797265E-32,1.));
#125498=DIRECTION('ref_axis',(0.,-1.,0.));
#125499=DIRECTION('center_axis',(-0.125568828811331,-0.992084895087623,
0.000173694938030051));
#125500=DIRECTION('ref_axis',(0.981610126752954,-0.124217652014093,0.144953558025165));
#125501=DIRECTION('center_axis',(-0.399982918137251,0.916522577290502,0.000174685963062819));
#125502=DIRECTION('ref_axis',(0.904565263167025,0.394733882299028,0.161080249679181));
#125503=DIRECTION('center_axis',(0.,-4.12699273797265E-32,1.));
#125504=DIRECTION('ref_axis',(0.,-1.,0.));
#125505=DIRECTION('center_axis',(-0.206015137908635,-0.978548789168202,
0.000173694938025831));
#125506=DIRECTION('ref_axis',(0.968219008221905,-0.203814666180172,0.144953557968256));
#125507=DIRECTION('center_axis',(-0.323946909343764,0.946075245110788,0.000174685963058239));
#125508=DIRECTION('ref_axis',(0.933729872804219,0.319689971343558,0.16108024973712));
#125509=DIRECTION('center_axis',(0.,-4.12699273797265E-32,1.));
#125510=DIRECTION('ref_axis',(0.,-1.,0.));
#125511=DIRECTION('center_axis',(-0.285090450253219,-0.958500602506063,
0.000173694938036217));
#125512=DIRECTION('ref_axis',(0.948384551914434,-0.282055327364791,0.144953558063258));
#125513=DIRECTION('center_axis',(-0.245755087316061,0.969331938266294,0.000174685963067071));
#125514=DIRECTION('ref_axis',(0.956680664197139,0.242518576376685,0.161080249762494));
#125515=DIRECTION('center_axis',(0.,-4.12699273797265E-32,1.));
#125516=DIRECTION('ref_axis',(0.,-1.,0.));
#125517=DIRECTION('center_axis',(-0.362268532688063,-0.932073752475686,
0.000173694938007782));
#125518=DIRECTION('ref_axis',(0.922238752915758,-0.358418956890768,0.144953557947781));
#125519=DIRECTION('center_axis',(-0.165927805729023,0.986137887301145,0.000174685963059481));
#125520=DIRECTION('ref_axis',(0.973264903614975,0.163733260298146,0.161080249762262));
#125521=DIRECTION('center_axis',(0.,-4.12699273797265E-32,1.));
#125522=DIRECTION('ref_axis',(0.,-1.,0.));
#125523=DIRECTION('center_axis',(-0.437035777807844,-0.899444105403978,
0.000173694938040317));
#125524=DIRECTION('ref_axis',(0.889955607146088,-0.432397367382357,0.144953558045479));
#125525=DIRECTION('center_axis',(-0.0849963019710254,0.996381251397308,
0.000174685963051347));
#125526=DIRECTION('ref_axis',(0.983372225679145,0.0838583263866241,0.16108024974676));
#125527=DIRECTION('center_axis',(0.,-4.12699273797265E-32,1.));
#125528=DIRECTION('ref_axis',(0.,-1.,0.));
#125529=DIRECTION('center_axis',(-0.50889462193225,-0.860828806208587,0.000173694938014614));
#125530=DIRECTION('ref_axis',(0.851749953658509,-0.503498244741079,0.144953558029389));
#125531=DIRECTION('center_axis',(-0.00349916184678272,0.999993862656759,
0.000174685963057099));
#125532=DIRECTION('ref_axis',(0.98693536782401,0.00342532914819454,0.161080249746247));
#125533=DIRECTION('center_axis',(0.,-4.12699273797265E-32,1.));
#125534=DIRECTION('ref_axis',(0.,-1.,0.));
#125535=DIRECTION('center_axis',(-0.577366856309305,-0.816484833334691,
0.000173694938048078));
#125536=DIRECTION('ref_axis',(0.807876044753958,-0.571248424349741,0.144953558047536));
#125537=DIRECTION('center_axis',(0.0780212646221935,0.996951679747603,0.00017468596304852));
#125538=DIRECTION('ref_axis',(0.9839306179374,-0.0770304630912104,0.161080249693373));
#125539=DIRECTION('center_axis',(0.,-4.12699273797265E-32,1.));
#125540=DIRECTION('ref_axis',(0.,-1.,0.));
#125541=DIRECTION('center_axis',(-0.641996809516522,-0.76670728860542,0.000173694938037895));
#125542=DIRECTION('ref_axis',(0.758625854057432,-0.635197039939658,0.14495355810579));
#125543=DIRECTION('center_axis',(0.159022472447753,0.987274947895174,0.000174685963063276));
#125544=DIRECTION('ref_axis',(0.974377972117496,-0.156973630308053,0.161080249689733));
#125545=DIRECTION('center_axis',(0.,-4.12699273797265E-32,1.));
#125546=DIRECTION('ref_axis',(0.,-1.,0.));
#125547=DIRECTION('center_axis',(-0.702354379878435,-0.711827433368262,
0.000173694938018697));
#125548=DIRECTION('ref_axis',(0.704327133475682,-0.694918524035963,0.144953558085365));
#125549=DIRECTION('center_axis',(0.238965411956016,0.971028064153403,0.000174685963061851));
#125550=DIRECTION('ref_axis',(0.958341001655361,-0.235872163914385,0.16108024967868));
#125551=DIRECTION('center_axis',(0.,-4.12699273797265E-32,1.));
#125552=DIRECTION('ref_axis',(0.,-1.,0.));
#125553=DIRECTION('center_axis',(-0.758037897722513,-0.652210484005357,
0.000173694938036324));
#125554=DIRECTION('ref_axis',(0.645341232020346,-0.750015440001797,0.144953558125948));
#125555=DIRECTION('center_axis',(0.317318076074206,0.948319148853053,0.000174685963053342));
#125556=DIRECTION('ref_axis',(0.935926429926839,-0.313201007181146,0.161080249767366));
#125557=DIRECTION('center_axis',(0.,-4.12699273797265E-32,1.));
#125558=DIRECTION('ref_axis',(0.,-1.,0.));
#125559=DIRECTION('center_axis',(-0.808676798424737,-0.588253181478508,
0.000173694938024896));
#125560=DIRECTION('ref_axis',(0.582060691151914,-0.800121126973516,0.144953558032864));
#125561=DIRECTION('center_axis',(0.393559040749975,0.919299326078712,0.000174685963059358));
#125562=DIRECTION('ref_axis',(0.90728342224558,-0.388445549426304,0.161080249718102));
#125563=DIRECTION('center_axis',(0.,-4.12699273797265E-32,1.));
#125564=DIRECTION('ref_axis',(0.,-1.,0.));
#125565=DIRECTION('center_axis',(-0.853934088455684,-0.520381151083923,
0.000173694938054823));
#125566=DIRECTION('ref_axis',(0.514906632408805,-0.844902139846358,0.144953558026248));
#125567=DIRECTION('center_axis',(0.467180934942176,0.884161717963048,0.000174685963059081));
#125568=DIRECTION('ref_axis',(0.872602593079875,-0.461105050630121,0.161080249669756));
#125569=DIRECTION('center_axis',(0.,-4.12699273797265E-32,1.));
#125570=DIRECTION('ref_axis',(0.,-1.,0.));
#125571=DIRECTION('center_axis',(-0.89350858801721,-0.449046069985654,0.000173694938035765));
#125572=DIRECTION('ref_axis',(0.44432595497643,-0.88406046836972,0.144953558080494));
#125573=DIRECTION('center_axis',(0.53769381709176,0.843140159490762,0.000174685963044948));
#125574=DIRECTION('ref_axis',(0.832114737608997,-0.530695973789334,0.161080249744345));
#125575=DIRECTION('center_axis',(0.,-4.12699273797265E-32,1.));
#125576=DIRECTION('ref_axis',(0.,-1.,0.));
#125577=DIRECTION('center_axis',(-0.927136935344019,-0.37472266137901,0.000173694938021475));
#125578=DIRECTION('ref_axis',(0.370788361633148,-0.91733552035926,0.144953557957756));
#125579=DIRECTION('center_axis',(0.604628435601924,0.796507642365335,0.000174685963076138));
#125580=DIRECTION('ref_axis',(0.786089295859101,-0.596755202807269,0.161080249745889));
#125581=DIRECTION('center_axis',(0.,-4.12699273797265E-32,1.));
#125582=DIRECTION('ref_axis',(0.,-1.,0.));
#125583=DIRECTION('center_axis',(-0.95459533933292,-0.297905535285827,0.000173694938038584));
#125584=DIRECTION('ref_axis',(0.294783232905703,-0.944505855777472,0.144953558078881));
#125585=DIRECTION('center_axis',(0.667539351629772,0.744574498294508,0.000174685963094329));
#125586=DIRECTION('ref_axis',(0.734832559538327,-0.658843124405789,0.16108024976877));
#125587=DIRECTION('center_axis',(0.,-4.12699273797265E-32,1.));
#125588=DIRECTION('ref_axis',(0.,-1.,0.));
#125589=DIRECTION('center_axis',(-0.975701068835708,-0.219105897006276,
0.000173694938047038));
#125590=DIRECTION('ref_axis',(0.216816370407067,-0.965390660580497,0.144953558036552));
#125591=DIRECTION('center_axis',(0.726007903408699,0.687686333783738,0.000174685963071939));
#125592=DIRECTION('ref_axis',(0.678685633776137,-0.716546553715493,0.161080249764932));
#125593=DIRECTION('center_axis',(0.,-4.12699273797265E-32,1.));
#125594=DIRECTION('ref_axis',(0.,-1.,0.));
#125595=DIRECTION('center_axis',(-0.990313668704752,-0.138848145132025,
0.000173694938038594));
#125596=DIRECTION('ref_axis',(0.137406630733052,-0.979850949805316,0.144953558066752));
#125597=DIRECTION('center_axis',(0.779644992373389,0.62622173018182,0.000174685963098564));
#125598=DIRECTION('ref_axis',(0.618022167103482,-0.7694814839412,0.161080249690531));
#125599=DIRECTION('center_axis',(0.,-4.12699273797265E-32,1.));
#125600=DIRECTION('ref_axis',(0.,-1.,0.));
#125601=DIRECTION('center_axis',(-0.998335894498814,-0.05766638176027,0.000173694938032902));
#125602=DIRECTION('ref_axis',(0.0570824726036373,-0.987790492638966,0.144953557988494));
#125603=DIRECTION('center_axis',(0.828093672546161,0.560589724284905,0.000174685963077943));
#125604=DIRECTION('ref_axis',(0.553245864863052,-0.817295641832221,0.161080249732829));
#125605=DIRECTION('center_axis',(0.,-4.12699273797265E-32,1.));
#125606=DIRECTION('ref_axis',(0.,-1.,0.));
#125607=DIRECTION('center_axis',(-0.999714359628814,0.0238991418678133,
0.000173694938034033));
#125608=DIRECTION('ref_axis',(0.0236215599645613,0.989156452705798,-0.144953557994702));
#125609=DIRECTION('center_axis',(0.871031525953977,0.491227086263675,0.000174685963068119));
#125610=DIRECTION('ref_axis',(0.484787802678601,-0.859670832082115,0.161080249693429));
#125611=DIRECTION('center_axis',(0.,-4.12699273797265E-32,1.));
#125612=DIRECTION('ref_axis',(0.,-1.,0.));
#125613=DIRECTION('center_axis',(-0.994439890636744,0.105305620649848,0.000173694938035152));
#125614=DIRECTION('ref_axis',(0.104168394946778,0.983939739764692,-0.144953558100528));
#125615=DIRECTION('center_axis',(0.908172808266673,0.4185954130301,0.000174685963064905));
#125616=DIRECTION('ref_axis',(0.413103557643788,-0.896325054765691,0.161080249755599));
#125617=DIRECTION('center_axis',(0.,-4.12699273797265E-32,1.));
#125618=DIRECTION('ref_axis',(0.,-1.,0.));
#125619=DIRECTION('center_axis',(-0.982547588243519,0.186011307900658,0.000173694938032103));
#125620=DIRECTION('ref_axis',(0.184022006446546,0.972175070204138,-0.144953558138347));
#125621=DIRECTION('center_axis',(0.939270350378314,0.343178056386206,0.000174685963062408));
#125622=DIRECTION('ref_axis',(0.338670176597351,-0.927014382107848,0.161080249716481));
#125623=DIRECTION('center_axis',(0.,-4.12699273797265E-32,1.));
#125624=DIRECTION('ref_axis',(0.,-1.,0.));
#125625=DIRECTION('center_axis',(-0.939269562412001,0.343180213526999,0.000173694938031579));
#125626=DIRECTION('ref_axis',(0.339532058317171,0.929358083503298,-0.144953558086661));
#125627=DIRECTION('center_axis',(0.982548015255807,0.186009051397209,0.000174685963063537));
#125628=DIRECTION('ref_axis',(0.183552372552309,-0.969722475602179,0.161080249696849));
#125629=DIRECTION('center_axis',(0.,-4.12699273797265E-32,1.));
#125630=DIRECTION('ref_axis',(0.,-1.,0.));
#125631=DIRECTION('center_axis',(-0.908171847095246,0.418597498766629,0.000173694938032065));
#125632=DIRECTION('ref_axis',(0.414153604942779,0.898590706322032,-0.144953558164584));
#125633=DIRECTION('center_axis',(0.994440132302203,0.105303336849277,0.000174685963054474));
#125634=DIRECTION('ref_axis',(0.103900232948935,-0.981457026442032,0.161080249691642));
#125635=DIRECTION('center_axis',(0.,-4.12699273797265E-32,1.));
#125636=DIRECTION('ref_axis',(0.,-1.,0.));
#125637=DIRECTION('center_axis',(-0.871030397973873,0.491229086715704,0.000173694938031785));
#125638=DIRECTION('ref_axis',(0.48601902766875,0.861843356269927,-0.144953558070544));
#125639=DIRECTION('center_axis',(0.999714414339203,0.0238968459684036,0.000174685963064245));
#125640=DIRECTION('ref_axis',(0.0235566544373952,-0.986660142698139,0.161080249697491));
#125641=DIRECTION('center_axis',(0.,-4.12699273797265E-32,1.));
#125642=DIRECTION('ref_axis',(0.,-1.,0.));
#125643=DIRECTION('center_axis',(-0.828092385263878,0.560591626139786,0.000173694938011966));
#125644=DIRECTION('ref_axis',(0.554650073944248,0.81936058085897,-0.144953558107731));
#125645=DIRECTION('center_axis',(0.998335761890044,-0.0576686744796514,
0.000174685963059713));
#125646=DIRECTION('ref_axis',(0.0569436897224966,0.985297198489207,-0.161080249720776));
#125647=DIRECTION('center_axis',(0.,-4.12699273797265E-32,1.));
#125648=DIRECTION('ref_axis',(0.,-1.,0.));
#125649=DIRECTION('center_axis',(-0.779643554355606,0.626223520782975,0.000173694938038147));
#125650=DIRECTION('ref_axis',(0.619590015495319,0.771425095977384,-0.144953558061866));
#125651=DIRECTION('center_axis',(0.990313349659314,-0.138850419413709,0.000174685963050317));
#125652=DIRECTION('ref_axis',(0.137065083024103,0.977377264004113,-0.161080249637969));
#125653=DIRECTION('center_axis',(0.,-4.12699273797265E-32,1.));
#125654=DIRECTION('ref_axis',(0.,-1.,0.));
#125655=DIRECTION('center_axis',(-0.726006324225229,0.68768800121497,0.000173694938033376));
#125656=DIRECTION('ref_axis',(0.68040668771909,0.718355904357349,-0.144953558017983));
#125657=DIRECTION('center_axis',(0.9757005654768,-0.219108137715302,0.000174685963060536));
#125658=DIRECTION('ref_axis',(0.216274330807799,0.962953045052486,-0.1610802497446));
#125659=DIRECTION('center_axis',(0.,-4.12699273797265E-32,1.));
#125660=DIRECTION('ref_axis',(0.,-1.,0.));
#125661=DIRECTION('center_axis',(-0.66753764178975,0.744576031459413,0.000173694938049494));
#125662=DIRECTION('ref_axis',(0.736695365690809,0.660506172708796,-0.144953558022086));
#125663=DIRECTION('center_axis',(0.954594655010301,-0.297907727510681,0.000174685963056511));
#125664=DIRECTION('ref_axis',(0.294044308610184,0.942120532495689,-0.161080249639732));
#125665=DIRECTION('center_axis',(0.,-4.12699273797265E-32,1.));
#125666=DIRECTION('ref_axis',(0.,-1.,0.));
#125667=DIRECTION('center_axis',(-0.604626606484044,0.796509031060953,0.000173694938017039));
#125668=DIRECTION('ref_axis',(0.788081457547906,0.598260881455095,-0.144953558044432));
#125669=DIRECTION('center_axis',(0.927136074611733,-0.374724790530812,0.000174685963067698));
#125670=DIRECTION('ref_axis',(0.369857470042992,0.915018363202569,-0.161080249737478));
#125671=DIRECTION('center_axis',(0.,-4.12699273797265E-32,1.));
#125672=DIRECTION('ref_axis',(0.,-1.,0.));
#125673=DIRECTION('center_axis',(-0.53769188086865,0.843141394475448,0.000173694938039761));
#125674=DIRECTION('ref_axis',(0.834222997314027,0.532034262732468,-0.144953558187165));
#125675=DIRECTION('center_axis',(0.893507556603344,-0.449048121895122,0.000174685963043604));
#125676=DIRECTION('ref_axis',(0.443209291040966,0.881826897687926,-0.161080249717502));
#125677=DIRECTION('center_axis',(0.,-4.12699273797265E-32,1.));
#125678=DIRECTION('ref_axis',(0.,-1.,0.));
#125679=DIRECTION('center_axis',(-0.467178904498963,0.88416279101827,0.000173694938045996));
#125680=DIRECTION('ref_axis',(0.874812920690553,0.462267043785389,-0.144953558158402));
#125681=DIRECTION('center_axis',(0.853932893224105,-0.520383112096006,0.000174685963043952));
#125682=DIRECTION('ref_axis',(0.513611627330155,0.842767019657086,-0.161080249719146));
#125683=DIRECTION('center_axis',(0.,-4.12699273797265E-32,1.));
#125684=DIRECTION('ref_axis',(0.,-1.,0.));
#125685=DIRECTION('center_axis',(-0.393556929598893,0.919300230063476,0.000173694938030032));
#125686=DIRECTION('ref_axis',(0.909581108427159,0.389423513935497,-0.144953558033427));
#125687=DIRECTION('center_axis',(0.808675447329435,-0.588255038543107,0.000174685963058817));
#125688=DIRECTION('ref_axis',(0.580595962980463,0.798098666158617,-0.161080249709967));
#125689=DIRECTION('center_axis',(0.,-4.12699273797265E-32,1.));
#125690=DIRECTION('ref_axis',(0.,-1.,0.));
#125691=DIRECTION('center_axis',(-0.317315898264684,0.948319877751461,0.000173694938030787));
#125692=DIRECTION('ref_axis',(0.938296183923317,0.313988434836218,-0.144953558162752));
#125693=DIRECTION('center_axis',(0.758036399754929,-0.652212224763841,0.000174685963032238));
#125694=DIRECTION('ref_axis',(0.643716528291106,0.748119097716493,-0.161080249679177));
#125695=DIRECTION('center_axis',(0.,-4.12699273797265E-32,1.));
#125696=DIRECTION('ref_axis',(0.,-1.,0.));
#125697=DIRECTION('center_axis',(-0.238963181980971,0.971028613114772,0.000173694938030256));
#125698=DIRECTION('ref_axis',(0.960767053149991,0.236463814517229,-0.1449535580986));
#125699=DIRECTION('center_axis',(0.702352745007179,-0.71182904623631,0.000174685963053707));
#125700=DIRECTION('ref_axis',(0.702553266302939,0.693160920100014,-0.161080249730294));
#125701=DIRECTION('center_axis',(0.,-4.12699273797265E-32,1.));
#125702=DIRECTION('ref_axis',(0.,-1.,0.));
#125703=DIRECTION('center_axis',(-0.159020205147339,0.987275313266247,0.000173694938038525));
#125704=DIRECTION('ref_axis',(0.976844176148955,0.157365566524177,-0.144953558067387));
#125705=DIRECTION('center_axis',(0.641995048621441,-0.766708762849602,0.000174685963078827));
#125706=DIRECTION('ref_axis',(0.756714628244622,0.633589870928856,-0.16108024974204));
#125707=DIRECTION('center_axis',(0.,-4.12699273797265E-32,1.));
#125708=DIRECTION('ref_axis',(0.,-1.,0.));
#125709=DIRECTION('center_axis',(-0.0780189750849014,0.996951859096902,
0.000173694938032577));
#125710=DIRECTION('ref_axis',(0.986420562298587,0.0772200766466855,-0.144953558208202));
#125711=DIRECTION('center_axis',(0.577364981108916,-0.816486159144119,0.000174685963063083));
#125712=DIRECTION('ref_axis',(0.80584017919105,0.569802385706794,-0.161080249702384));
#125713=DIRECTION('center_axis',(0.,-4.12699273797265E-32,1.));
#125714=DIRECTION('ref_axis',(0.,-1.,0.));
#125715=DIRECTION('center_axis',(0.00350145838446337,0.999993854790743,
0.000173694938039412));
#125716=DIRECTION('ref_axis',(0.989432482391681,-0.00343930009725844,-0.144953558090438));
#125717=DIRECTION('center_axis',(0.508892644905654,-0.860829974760256,0.000174685963037557));
#125718=DIRECTION('ref_axis',(0.849602996695427,0.502222959615186,-0.161080249694099));
#125719=DIRECTION('center_axis',(0.,-4.12699273797265E-32,1.));
#125720=DIRECTION('ref_axis',(0.,-1.,0.));
#125721=DIRECTION('center_axis',(0.0849985902259986,0.996381056368326,0.000173694938038034));
#125722=DIRECTION('ref_axis',(0.98585989253223,-0.0840757888669896,-0.144953558158235));
#125723=DIRECTION('center_axis',(0.437033712111826,-0.899445108921368,0.000174685963056523));
#125724=DIRECTION('ref_axis',(0.887711846418836,0.431301322581788,-0.161080249772778));
#125725=DIRECTION('center_axis',(0.,-4.12699273797265E-32,1.));
#125726=DIRECTION('ref_axis',(0.,-1.,0.));
#125727=DIRECTION('center_axis',(0.165930070473371,0.986137506407078,0.000173694938036312));
#125728=DIRECTION('ref_axis',(0.975726567763563,-0.164152767135129,-0.144953558087466));
#125729=DIRECTION('center_axis',(0.362266392069445,-0.932074584280572,0.000174685963047641));
#125730=DIRECTION('ref_axis',(0.919913120284889,0.357509446415818,-0.161080249724085));
#125731=DIRECTION('center_axis',(0.,-4.12699273797265E-32,1.));
#125732=DIRECTION('ref_axis',(0.,-1.,0.));
#125733=DIRECTION('center_axis',(0.245757313478258,0.969331374041931,0.000173694938041656));
#125734=DIRECTION('ref_axis',(0.95909994365823,-0.243137335820007,-0.144953558097514));
#125735=DIRECTION('center_axis',(0.28508824895752,-0.958501257062895,0.000174685963072556));
#125736=DIRECTION('ref_axis',(0.945992524106419,0.281338403866232,-0.161080249704198));
#125737=DIRECTION('center_axis',(0.,-4.12699273797265E-32,1.));
#125738=DIRECTION('ref_axis',(0.,-1.,0.));
#125739=DIRECTION('center_axis',(0.323949082109054,0.946074501310954,0.000173694938040627));
#125740=DIRECTION('ref_axis',(0.936090667680424,-0.320503865653793,-0.144953558019777));
#125741=DIRECTION('center_axis',(0.206012890585117,-0.978549262121013,0.000174685963054924));
#125742=DIRECTION('ref_axis',(0.965776503747655,0.203295100653895,-0.161080249748623));
#125743=DIRECTION('center_axis',(0.,-4.12699273797265E-32,1.));
#125744=DIRECTION('ref_axis',(0.,-1.,0.));
#125745=DIRECTION('center_axis',(0.399985023046293,0.91652165886504,0.000173694938024144));
#125746=DIRECTION('ref_axis',(0.906851862735966,-0.395737495135554,-0.144953558066528));
#125747=DIRECTION('center_axis',(0.125566550415584,-0.992085183288988,0.000174685963050411));
#125748=DIRECTION('ref_axis',(0.979133400098864,0.123898902089266,-0.161080249788461));
#125749=DIRECTION('center_axis',(0.,-4.12699273797265E-32,1.));
#125750=DIRECTION('ref_axis',(0.,-1.,0.));
#125751=DIRECTION('center_axis',(0.473359129647977,0.880869515994837,0.000173694938041029));
#125752=DIRECTION('ref_axis',(0.871578108263211,-0.468337556876952,-0.144953558131046));
#125753=DIRECTION('center_axis',(0.044284585570049,-0.999018941244711,0.000174685963050208));
#125754=DIRECTION('ref_axis',(0.985974325245433,0.0436781767754032,-0.161080249659572));
#125755=DIRECTION('center_axis',(0.,-4.12699273797265E-32,1.));
#125756=DIRECTION('ref_axis',(0.,-1.,0.));
#125757=DIRECTION('center_axis',(0.543583109340639,0.839355331828917,0.00017369493803777));
#125758=DIRECTION('ref_axis',(0.830504145292599,-0.537820909453829,-0.144953558100746));
#125759=DIRECTION('center_axis',(-0.0372920858860229,-0.999304392972974,
0.00017468596305223));
#125760=DIRECTION('ref_axis',(0.986253753914206,-0.0368332196013007,-0.16108024963955));
#125761=DIRECTION('center_axis',(0.,-4.12699273797265E-32,1.));
#125762=DIRECTION('ref_axis',(0.,-1.,0.));
#125763=DIRECTION('center_axis',(0.610189633125563,0.79225537641354,0.000173694938026845));
#125764=DIRECTION('ref_axis',(0.783903314256242,-0.603725152611619,-0.14495355808726));
#125765=DIRECTION('center_axis',(-0.118620584663302,-0.992939638839618,
0.000174685963056815));
#125766=DIRECTION('ref_axis',(0.979969826540933,-0.117099496975594,-0.161080249805483));
#125767=DIRECTION('center_axis',(0.,-4.12699273797265E-32,1.));
#125768=DIRECTION('ref_axis',(0.,-1.,0.));
#125769=DIRECTION('center_axis',(0.672735445576227,0.739883092181072,0.000173694938022371));
#125770=DIRECTION('ref_axis',(0.732085735994742,-0.665611704483453,-0.144953558106277));
#125771=DIRECTION('center_axis',(-0.199159683020644,-0.979967035233293,
0.000174685963060404));
#125772=DIRECTION('ref_axis',(0.967164361690274,-0.196586496520054,-0.161080249758361));
#125773=DIRECTION('center_axis',(0.,-4.12699273797265E-32,1.));
#125774=DIRECTION('ref_axis',(0.,-1.,0.));
#125775=DIRECTION('center_axis',(0.730804314630066,0.682587008042307,0.000173694938039999));
#125776=DIRECTION('ref_axis',(0.675396247952083,-0.723068720286077,-0.144953558066381));
#125777=DIRECTION('center_axis',(-0.278373406546575,-0.960472912690654,
0.000174685963093089));
#125778=DIRECTION('ref_axis',(0.947922577585518,-0.274765245366625,-0.161080249696373));
#125779=DIRECTION('center_axis',(0.,-4.12699273797265E-32,1.));
#125780=DIRECTION('ref_axis',(0.,-1.,0.));
#125781=DIRECTION('center_axis',(0.784009801544307,0.620748419983913,0.000173694938043742));
#125782=DIRECTION('ref_axis',(0.614212109297605,-0.775713833036737,-0.144953558175163));
#125783=DIRECTION('center_axis',(-0.355734600980206,-0.934587001380967,
0.000174685963059907));
#125784=DIRECTION('ref_axis',(0.922372525104978,-0.351115476833086,-0.161080249750679));
#125785=DIRECTION('center_axis',(0.,-4.12699273797265E-32,1.));
#125786=DIRECTION('ref_axis',(0.,-1.,0.));
#125787=DIRECTION('center_axis',(0.831997832581782,0.554778853606809,0.000173694938052519));
#125788=DIRECTION('ref_axis',(0.548940490414457,-0.823196698238963,-0.14495355805224));
#125789=DIRECTION('center_axis',(-0.430728440336455,-0.902481567773071,
0.000174685963073157));
#125790=DIRECTION('ref_axis',(0.890684235670549,-0.42512909273917,-0.161080249673074));
#125791=DIRECTION('center_axis',(0.,-4.12699273797265E-32,1.));
#125792=DIRECTION('ref_axis',(0.,-1.,0.));
#125793=DIRECTION('center_axis',(0.874449055313417,0.485117325491,0.000173694938044398));
#125794=DIRECTION('ref_axis',(0.480015763116306,-0.865201325202067,-0.144953558177983));
#125795=DIRECTION('center_axis',(-0.502855852987447,-0.864370268230624,
0.000174685963069477));
#125796=DIRECTION('ref_axis',(0.853068589594169,-0.496313544673254,-0.161080249632552));
#125797=DIRECTION('center_axis',(0.,-4.12699273797265E-32,1.));
#125798=DIRECTION('ref_axis',(0.,-1.,0.));
#125799=DIRECTION('center_axis',(0.911080963855876,0.412227421612775,0.000173694938031732));
#125800=DIRECTION('ref_axis',(0.407896610121612,-0.901448180108941,-0.144953558181837));
#125801=DIRECTION('center_axis',(-0.57163684290217,-0.820506727164168,0.000174685963066123));
#125802=DIRECTION('ref_axis',(0.809775912776532,-0.564195111838173,-0.161080249766526));
#125803=DIRECTION('center_axis',(0.,-4.12699273797265E-32,1.));
#125804=DIRECTION('ref_axis',(0.,-1.,0.));
#125805=DIRECTION('center_axis',(0.941649778901648,0.336594212256459,0.00017369493803296));
#125806=DIRECTION('ref_axis',(0.333062972491066,-0.931696046123075,-0.144953558059274));
#125807=DIRECTION('center_axis',(-0.63661368394079,-0.771182849202542,0.00017468596305796));
#125808=DIRECTION('ref_axis',(0.761094310895386,-0.628322053641482,-0.16108024965969));
#125809=DIRECTION('center_axis',(0.,-4.12699273797265E-32,1.));
#125810=DIRECTION('ref_axis',(0.,-1.,0.));
#125811=DIRECTION('center_axis',(0.965952070030099,0.258721023951739,0.000173694938034315));
#125812=DIRECTION('ref_axis',(0.256012855721305,-0.955743628647454,-0.144953558097827));
#125813=DIRECTION('center_axis',(-0.697353965946701,-0.716726876615648,
0.000174685963046821));
#125814=DIRECTION('ref_axis',(0.707347751921464,-0.688267615822936,-0.161080249754778));
#125815=DIRECTION('center_axis',(0.,-4.12699273797265E-32,1.));
#125816=DIRECTION('ref_axis',(0.,-1.,0.));
#125817=DIRECTION('center_axis',(0.983826109503387,0.179126089918523,0.000173694938024096));
#125818=DIRECTION('ref_axis',(0.177259015639969,-0.973430895027676,-0.144953558010722));
#125819=DIRECTION('center_axis',(-0.753453472364535,-0.657501204916493,
0.000174685963058063));
#125820=DIRECTION('ref_axis',(0.648893910389724,-0.743632870604353,-0.161080249614477));
#125821=DIRECTION('center_axis',(0.,-4.12699273797265E-32,1.));
#125822=DIRECTION('ref_axis',(0.,-1.,0.));
#125823=DIRECTION('center_axis',(0.995152948537796,0.0983391013107115,0.000173694938042572));
#125824=DIRECTION('ref_axis',(0.0973255460498904,-0.984640139371994,-0.144953558161193));
#125825=DIRECTION('center_axis',(-0.804538870234896,-0.593899971178624,
0.000174685963083651));
#125826=DIRECTION('ref_axis',(0.586121786917812,-0.794049371293258,-0.161080249717499));
#125827=DIRECTION('center_axis',(0.,-4.12699273797265E-32,1.));
#125828=DIRECTION('ref_axis',(0.,-1.,0.));
#125829=DIRECTION('center_axis',(0.999857208888375,0.0168976822084356,0.000173694938038329));
#125830=DIRECTION('ref_axis',(0.0167443910123756,-0.989296766069278,-0.144953558129814));
#125831=DIRECTION('center_axis',(-0.850270194663315,-0.526346431119299,
0.00017468596304367));
#125832=DIRECTION('ref_axis',(0.519449119674191,-0.839181604446911,-0.161080249650962));
#125833=DIRECTION('center_axis',(0.,-4.12699273797265E-32,1.));
#125834=DIRECTION('ref_axis',(0.,-1.,0.));
#125835=DIRECTION('center_axis',(0.997907584478628,-0.0646561881810041,
0.00017369493803715));
#125836=DIRECTION('ref_axis',(0.0639481951858162,0.98736978601666,0.144953558058749));
#125837=DIRECTION('center_axis',(-0.890343111231032,-0.455290142401809,
0.000174685963060243));
#125838=DIRECTION('ref_axis',(0.449319604233089,-0.878729222464582,-0.16108024968509));
#125839=DIRECTION('center_axis',(0.,-4.12699273797265E-32,1.));
#125840=DIRECTION('ref_axis',(0.,-1.,0.));
#125841=DIRECTION('center_axis',(-0.831996558357966,0.554780764235129,0.000174685963036686));
#125842=DIRECTION('ref_axis',(0.547559474507209,0.8211161763256,0.161080249732285));
#125843=DIRECTION('center_axis',(0.430726367814519,-0.902482557116413,0.00017369493803426));
#125844=DIRECTION('ref_axis',(0.892940119914814,0.426199962750572,0.144953558072679));
#125845=DIRECTION('center_axis',(0.,-4.12699273797265E-32,1.));
#125846=DIRECTION('ref_axis',(0.,-1.,0.));
#125847=DIRECTION('center_axis',(-0.874447941063388,0.485119333622992,0.00017468596306053));
#125848=DIRECTION('ref_axis',(0.47880892428474,0.863015160451995,0.161080249736917));
#125849=DIRECTION('center_axis',(0.502853868002302,-0.8643714232118,0.000173694938021085));
#125850=DIRECTION('ref_axis',(0.855229681726789,0.497564726964118,0.144953557992271));
#125851=DIRECTION('center_axis',(0.,-4.12699273797265E-32,1.));
#125852=DIRECTION('ref_axis',(0.,-1.,0.));
#125853=DIRECTION('center_axis',(-0.911080016994841,0.412229513884554,0.000174685963026989));
#125854=DIRECTION('ref_axis',(0.406871979675512,0.89917092108733,0.161080249645609));
#125855=DIRECTION('center_axis',(0.571634958663587,-0.820508040096956,0.000173694938017433));
#125856=DIRECTION('ref_axis',(0.811827831091178,0.565618280001494,0.144953558058938));
#125857=DIRECTION('center_axis',(0.,-4.12699273797265E-32,1.));
#125858=DIRECTION('ref_axis',(0.,-1.,0.));
#125859=DIRECTION('center_axis',(-0.941649005730778,0.33659637474437,0.000174685963048853));
#125860=DIRECTION('ref_axis',(0.332227369159855,0.929342847572107,0.16108024971327));
#125861=DIRECTION('center_axis',(0.636611912988104,-0.77118431134956,0.000173694938013388));
#125862=DIRECTION('ref_axis',(0.763023400189289,0.629907736710017,0.144953558067543));
#125863=DIRECTION('center_axis',(0.,-4.12699273797265E-32,1.));
#125864=DIRECTION('ref_axis',(0.,-1.,0.));
#125865=DIRECTION('center_axis',(-0.965951475694722,0.258723242264785,0.000174685963070544));
#125866=DIRECTION('ref_axis',(0.255371840321265,0.953330150749369,0.161080249699075));
#125867=DIRECTION('center_axis',(0.697352320065293,-0.716728478246555,0.00017369493803279));
#125868=DIRECTION('ref_axis',(0.70914117443807,0.690005261347236,0.144953558182362));
#125869=DIRECTION('center_axis',(0.,-4.12699273797265E-32,1.));
#125870=DIRECTION('ref_axis',(0.,-1.,0.));
#125871=DIRECTION('center_axis',(-0.983825697958711,0.179128349294213,0.000174685963070963));
#125872=DIRECTION('ref_axis',(0.176816854017924,0.970973199059766,0.161080249698242));
#125873=DIRECTION('center_axis',(0.753451962507452,-0.657502935372716,0.000173694938036256));
#125874=DIRECTION('ref_axis',(0.650539731194123,0.745510914835243,0.14495355807774));
#125875=DIRECTION('center_axis',(0.,-4.12699273797265E-32,1.));
#125876=DIRECTION('ref_axis',(0.,-1.,0.));
#125877=DIRECTION('center_axis',(-0.9951527225226,0.0983413867131789,0.000174685963064377));
#125878=DIRECTION('ref_axis',(0.0970851807228342,0.982154580919935,0.161080249757698));
#125879=DIRECTION('center_axis',(0.804537506449909,-0.59390181894437,0.000173694938015236));
#125880=DIRECTION('ref_axis',(0.58760905336439,0.796055316181374,0.144953558023174));
#125881=DIRECTION('center_axis',(0.,-4.12699273797265E-32,1.));
#125882=DIRECTION('ref_axis',(0.,-1.,0.));
#125883=DIRECTION('center_axis',(-0.999857169906744,0.0168999784287159,
0.000174685963049014));
#125884=DIRECTION('ref_axis',(0.0167074215697249,0.98679988610253,0.161080249728283));
#125885=DIRECTION('center_axis',(0.85026898602633,-0.526348383897799,0.000173694938027909));
#125886=DIRECTION('ref_axis',(0.520767934225771,0.841302100728855,0.144953558050291));
#125887=DIRECTION('center_axis',(0.,-4.12699273797265E-32,1.));
#125888=DIRECTION('ref_axis',(0.,-1.,0.));
#125889=DIRECTION('center_axis',(-0.997907732789978,-0.0646538964238091,
0.0001746859630669));
#125890=DIRECTION('ref_axis',(0.0637815227177578,-0.984878200848485,-0.161080249730545));
#125891=DIRECTION('center_axis',(0.890342065785251,-0.455292187197761,0.000173694938023638));
#125892=DIRECTION('ref_axis',(0.450461190401379,0.880950158591516,0.144953558147968));
#125893=DIRECTION('center_axis',(0.,-4.12699273797265E-32,1.));
#125894=DIRECTION('ref_axis',(0.,-1.,0.));
#125895=DIRECTION('center_axis',(-0.989317384354678,-0.145777510262838,
0.000174685963054987));
#125896=DIRECTION('ref_axis',(0.143846011496079,-0.976402313670072,-0.161080249678226));
#125897=DIRECTION('center_axis',(0.924490065992462,-0.381206096109862,0.000173694938023807));
#125898=DIRECTION('ref_axis',(0.37715670168693,0.914735638516238,0.144953558083019));
#125899=DIRECTION('center_axis',(0.,-4.12699273797265E-32,1.));
#125900=DIRECTION('ref_axis',(0.,-1.,0.));
#125901=DIRECTION('center_axis',(-0.974143291952382,-0.225930998822629,
0.00017468596306252));
#125902=DIRECTION('ref_axis',(0.222953228798234,-0.961428630172209,-0.161080249731719));
#125903=DIRECTION('center_axis',(0.952485737340632,-0.304583141346891,0.000173694938041347));
#125904=DIRECTION('ref_axis',(0.301342297345122,0.942433703679797,0.144953558076867));
#125905=DIRECTION('center_axis',(0.,-4.12699273797265E-32,1.));
#125906=DIRECTION('ref_axis',(0.,-1.,0.));
#125907=DIRECTION('center_axis',(0.989317049737339,-0.145779782305628,0.000173694938037687));
#125908=DIRECTION('ref_axis',(0.144215216694403,0.97887202292198,0.144953558129552));
#125909=DIRECTION('center_axis',(-0.92449094128977,-0.38120397290423,0.000174685963069724));
#125910=DIRECTION('ref_axis',(0.376199940957144,-0.912429042481591,-0.161080249751384));
#125911=DIRECTION('center_axis',(0.,0.,1.));
#125912=DIRECTION('ref_axis',(1.,0.,0.));
#125913=DIRECTION('',(0.,0.,1.));
#125914=DIRECTION('',(0.,0.,1.));
#125915=DIRECTION('center_axis',(0.,-0.3396732719682,-0.940543496235245));
#125916=DIRECTION('ref_axis',(0.000119202233163679,0.940543489553072,-0.339673269554962));
#125917=DIRECTION('center_axis',(0.,-0.3396732719682,-0.940543496235245));
#125918=DIRECTION('ref_axis',(0.000119202233163679,0.940543489553072,-0.339673269554962));
#125919=DIRECTION('center_axis',(-0.923076923076923,-0.384615384615384,
0.));
#125920=DIRECTION('ref_axis',(0.384615384615384,-0.923076923076923,0.));
#125921=DIRECTION('center_axis',(0.923076923076904,0.384615384615431,2.59253294309151E-14));
#125922=DIRECTION('ref_axis',(0.381730136921527,-0.916152328611528,-0.122257978658025));
#125923=DIRECTION('',(0.281464519857291,-0.675514847657501,0.68151112584885));
#125924=DIRECTION('',(1.46520452235715E-32,-3.51649085365717E-32,1.));
#125925=DIRECTION('center_axis',(0.923076923076923,-0.384615384615384,0.));
#125926=DIRECTION('ref_axis',(0.384615384615384,0.923076923076923,0.));
#125927=DIRECTION('',(0.281464519857292,0.675514847657501,-0.68151112584885));
#125928=DIRECTION('center_axis',(-0.92307507402904,0.384619822294333,2.13514021449077E-6));
#125929=DIRECTION('ref_axis',(0.381364544927114,0.915263234831132,-0.129824091905111));
#125930=DIRECTION('',(1.46520452235715E-32,3.51649085365717E-32,-1.));
#125931=DIRECTION('center_axis',(0.,-4.12699273797265E-32,1.));
#125932=DIRECTION('ref_axis',(0.,-1.,-4.12699273797265E-32));
#125933=DIRECTION('center_axis',(0.,4.12699273797265E-32,-1.));
#125934=DIRECTION('ref_axis',(0.,1.,4.12699273797265E-32));
#125935=DIRECTION('',(-0.866025403784439,0.5,0.));
#125936=DIRECTION('',(4.50694379621149E-16,1.,0.));
#125937=DIRECTION('center_axis',(0.,4.12699273797265E-32,-1.));
#125938=DIRECTION('ref_axis',(0.,1.,4.12699273797265E-32));
#125939=DIRECTION('',(4.50694379621149E-16,1.,0.));
#125940=DIRECTION('',(0.866025403784439,0.5,0.));
#125941=DIRECTION('center_axis',(0.,4.12699273797265E-32,-1.));
#125942=DIRECTION('ref_axis',(0.,1.,4.12699273797265E-32));
#125943=DIRECTION('',(0.866025403784439,0.5,0.));
#125944=DIRECTION('',(0.866025403784439,-0.5,0.));
#125945=DIRECTION('center_axis',(0.,4.12699273797265E-32,-1.));
#125946=DIRECTION('ref_axis',(0.,1.,4.12699273797265E-32));
#125947=DIRECTION('',(0.866025403784439,-0.5,0.));
#125948=DIRECTION('',(0.,-1.,0.));
#125949=DIRECTION('center_axis',(0.,4.12699273797265E-32,-1.));
#125950=DIRECTION('ref_axis',(0.,1.,4.12699273797265E-32));
#125951=DIRECTION('',(0.,-1.,0.));
#125952=DIRECTION('',(-0.866025403784439,-0.5,0.));
#125953=DIRECTION('center_axis',(0.,4.12699273797265E-32,-1.));
#125954=DIRECTION('ref_axis',(0.,1.,4.12699273797265E-32));
#125955=DIRECTION('center_axis',(0.,0.,1.));
#125956=DIRECTION('ref_axis',(1.,0.,0.));
#125957=DIRECTION('center_axis',(0.,0.,1.));
#125958=DIRECTION('ref_axis',(1.,0.,0.));
#125959=DIRECTION('center_axis',(0.,0.,1.));
#125960=DIRECTION('ref_axis',(1.,0.,0.));
#125961=DIRECTION('center_axis',(0.,0.,1.));
#125962=DIRECTION('ref_axis',(1.,0.,0.));
#125963=DIRECTION('center_axis',(0.,0.,1.));
#125964=DIRECTION('ref_axis',(1.,0.,0.));
#125965=DIRECTION('center_axis',(0.,-4.12699273797265E-32,1.));
#125966=DIRECTION('ref_axis',(0.,-1.,0.));
#125967=DIRECTION('center_axis',(0.974142773255869,-0.225933236030987,0.000173694938032367));
#125968=DIRECTION('ref_axis',(0.223522509730735,0.963860028028979,0.144953558120001));
#125969=DIRECTION('center_axis',(-0.952486436664481,-0.304580953861225,
0.000174685963071088));
#125970=DIRECTION('ref_axis',(0.300576729150183,-0.940056797778399,-0.161080249701816));
#125971=DIRECTION('center_axis',(0.5,0.866025403784439,0.));
#125972=DIRECTION('ref_axis',(-0.866025403784439,0.5,0.));
#125973=DIRECTION('',(0.,0.,1.));
#125974=DIRECTION('',(0.,0.,1.));
#125975=DIRECTION('',(-0.866025403784439,0.5,0.));
#125976=DIRECTION('center_axis',(1.,-4.50694379621149E-16,0.));
#125977=DIRECTION('ref_axis',(4.50694379621149E-16,1.,0.));
#125978=DIRECTION('',(0.,0.,1.));
#125979=DIRECTION('center_axis',(0.5,-0.866025403784439,0.));
#125980=DIRECTION('ref_axis',(0.866025403784439,0.5,0.));
#125981=DIRECTION('',(0.,0.,1.));
#125982=DIRECTION('center_axis',(-0.5,-0.866025403784439,0.));
#125983=DIRECTION('ref_axis',(0.866025403784439,-0.5,0.));
#125984=DIRECTION('',(0.,0.,1.));
#125985=DIRECTION('center_axis',(-1.,0.,0.));
#125986=DIRECTION('ref_axis',(0.,0.,1.));
#125987=DIRECTION('',(0.,0.,1.));
#125988=DIRECTION('center_axis',(-0.5,0.866025403784439,0.));
#125989=DIRECTION('ref_axis',(-0.866025403784439,-0.5,0.));
#125990=DIRECTION('',(-0.866025403784439,-0.5,0.));
#125991=DIRECTION('center_axis',(0.,4.12699273797265E-32,-1.));
#125992=DIRECTION('ref_axis',(0.,1.,4.12699273797265E-32));
#125993=DIRECTION('center_axis',(0.,0.,1.));
#125994=DIRECTION('ref_axis',(1.,0.,0.));
#125995=DIRECTION('center_axis',(0.,0.,1.));
#125996=DIRECTION('ref_axis',(1.,0.,0.));
#125997=DIRECTION('center_axis',(0.,0.,1.));
#125998=DIRECTION('ref_axis',(1.,0.,0.));
#125999=DIRECTION('center_axis',(0.,0.,1.));
#126000=DIRECTION('ref_axis',(-1.,-1.22464679914735E-16,0.));
#126001=DIRECTION('center_axis',(0.,0.,1.));
#126002=DIRECTION('ref_axis',(1.,0.,0.));
#126003=DIRECTION('center_axis',(0.,-4.12699273797265E-32,1.));
#126004=DIRECTION('ref_axis',(0.,-1.,-4.12699273797265E-32));
#126005=DIRECTION('center_axis',(0.,0.,1.));
#126006=DIRECTION('ref_axis',(0.,1.,0.));
#126007=DIRECTION('center_axis',(0.,0.,-1.));
#126008=DIRECTION('ref_axis',(1.,0.,0.));
#126009=DIRECTION('center_axis',(-0.931957757426395,0.361751902433362,-0.0242960790789018));
#126010=DIRECTION('ref_axis',(0.265681371836198,0.635785003161866,-0.724700516360863));
#126011=DIRECTION('center_axis',(-0.282388053744349,0.677731328986489,-0.678923583927297));
#126012=DIRECTION('ref_axis',(-5.21804821573824E-15,0.707727927194326,0.706485089063614));
#126013=DIRECTION('center_axis',(0.,-4.12699273797265E-32,1.));
#126014=DIRECTION('ref_axis',(0.543398865272314,0.839474641201723,3.4645057479517E-32));
#126015=DIRECTION('center_axis',(0.,0.,1.));
#126016=DIRECTION('ref_axis',(1.,0.,0.));
#126017=DIRECTION('center_axis',(0.,0.,-1.));
#126018=DIRECTION('ref_axis',(-1.,0.,0.));
#126019=DIRECTION('center_axis',(-0.28238805374435,-0.677731328986489,0.678923583927297));
#126020=DIRECTION('ref_axis',(-5.19029264012261E-15,-0.707727927194326,
-0.706485089063614));
#126021=DIRECTION('center_axis',(0.281341523064402,-0.675219655354574,0.681854357192688));
#126022=DIRECTION('ref_axis',(-4.6074255521944E-15,-0.71055531721483,-0.703641344136153));
#126023=DIRECTION('center_axis',(0.281589094373317,-0.675813826495969,0.681163162426516));
#126024=DIRECTION('ref_axis',(2.41473507855972E-15,-0.709888749373493,-0.704313824593084));
#126025=DIRECTION('center_axis',(0.,0.,1.));
#126026=DIRECTION('ref_axis',(-1.,0.,0.));
#126027=DIRECTION('center_axis',(0.281589094373317,0.675813826495969,-0.681163162426516));
#126028=DIRECTION('ref_axis',(2.52575738102223E-15,0.709888749373494,0.704313824593084));
#126029=DIRECTION('center_axis',(0.,-4.12699273797265E-32,1.));
#126030=DIRECTION('ref_axis',(-0.543398865272315,0.839474641201722,3.4645057479517E-32));
#126031=DIRECTION('center_axis',(0.,0.,1.));
#126032=DIRECTION('ref_axis',(1.,0.,0.));
#126033=DIRECTION('center_axis',(0.281341523064402,0.675219655354575,-0.681854357192686));
#126034=DIRECTION('ref_axis',(-5.19029264012261E-15,0.710555317214828,0.703641344136155));
#126035=DIRECTION('center_axis',(0.951355185205049,-0.308096269992785,3.1537277192308E-33));
#126036=DIRECTION('ref_axis',(0.308096269992785,0.951355185205049,1.16548576868668E-33));
#126037=DIRECTION('',(-3.35939703647716E-33,-1.37139182454908E-34,1.));
#126038=DIRECTION('',(0.225467238628688,0.696209099085459,-0.68151112584885));
#126039=DIRECTION('center_axis',(-0.951353704021749,0.308100843620298,2.13514021596686E-6));
#126040=DIRECTION('ref_axis',(0.305493135327841,0.943302522722636,-0.129824092111888));
#126041=DIRECTION('',(1.50964222874619E-32,3.63793170954444E-32,-1.));
#126042=DIRECTION('center_axis',(-0.888655736322693,-0.45857494731044,-3.04823604041934E-33));
#126043=DIRECTION('ref_axis',(0.45857494731044,-0.888655736322693,1.4186657978342E-33));
#126044=DIRECTION('center_axis',(0.888655736322668,0.458574947310488,2.22108072553328E-14));
#126045=DIRECTION('ref_axis',(0.45513488130679,-0.881989357347002,-0.122257978653648));
#126046=DIRECTION('',(0.335588701144621,-0.650325156370489,0.681511125848849));
#126047=DIRECTION('',(-3.35939703647716E-33,-1.37139182454908E-34,1.));
#126048=DIRECTION('',(1.41101612161355E-32,-3.39907616780994E-32,1.));
#126049=DIRECTION('center_axis',(-3.35939703647716E-33,-1.37139182454908E-34,
1.));
#126050=DIRECTION('ref_axis',(0.996672582494194,0.0815092835470589,3.35939703647716E-33));
#126051=DIRECTION('center_axis',(0.027686525038222,-0.338543037176896,-0.940543496235209));
#126052=DIRECTION('ref_axis',(-0.0765442203803849,0.937423624769578,-0.33967326955506));
#126053=DIRECTION('center_axis',(0.027686525038222,-0.338543037176896,-0.940543496235209));
#126054=DIRECTION('ref_axis',(-0.0765442203803849,0.937423624769578,-0.33967326955506));
#126055=DIRECTION('center_axis',(-0.336689825853977,0.652458985955234,-0.678923583927297));
#126056=DIRECTION('ref_axis',(-0.0576863962918622,0.705373020900031,0.706485089063614));
#126057=DIRECTION('center_axis',(-0.226207035727802,-0.698493481841137,
0.678923583927297));
#126058=DIRECTION('ref_axis',(0.0576863962918529,-0.705373020900032,-0.706485089063614));
#126059=DIRECTION('center_axis',(-0.958342883256615,0.284584993724602,-0.0242960790698013));
#126060=DIRECTION('ref_axis',(0.212974880022829,0.655324689333347,-0.724700801730903));
#126061=DIRECTION('center_axis',(3.35939703647716E-33,1.37139182454908E-34,
-1.));
#126062=DIRECTION('ref_axis',(-0.996672582494194,-0.0815092835470579,-3.35939703647716E-33));
#126063=DIRECTION('center_axis',(4.48517628368065E-36,-4.12697442833547E-32,
1.));
#126064=DIRECTION('ref_axis',(0.473165773815097,0.880973410773538,3.63554251511517E-32));
#126065=DIRECTION('center_axis',(-3.35939703647716E-33,-1.37139182454908E-34,
1.));
#126066=DIRECTION('ref_axis',(0.996672582494194,0.0815092835470579,3.35939703647716E-33));
#126067=DIRECTION('center_axis',(0.335442052700293,-0.650040971676063,0.681854357192688));
#126068=DIRECTION('ref_axis',(0.0579168548267297,-0.708191003013486,-0.703641344136153));
#126069=DIRECTION('center_axis',(0.33573723070014,-0.650612986401985,0.681163162426516));
#126070=DIRECTION('ref_axis',(0.0578625233595577,-0.707526653121652,-0.704313824593084));
#126071=DIRECTION('center_axis',(0.225567029082369,0.696517237076055,-0.681163162426516));
#126072=DIRECTION('ref_axis',(-0.0578625233595519,0.707526653121653,0.704313824593084));
#126073=DIRECTION('center_axis',(0.225368712010601,0.695904863630102,-0.681854357192686));
#126074=DIRECTION('ref_axis',(-0.0579168548267439,0.708191003013484,0.703641344136154));
#126075=DIRECTION('center_axis',(-3.35939703647716E-33,-1.37139182454908E-34,
1.));
#126076=DIRECTION('ref_axis',(0.996672582494194,0.0815092835470579,3.35939703647716E-33));
#126077=DIRECTION('center_axis',(4.48517628368065E-36,-4.12697442833547E-32,
1.));
#126078=DIRECTION('ref_axis',(-0.610015726935623,0.792389306396296,3.27044400759111E-32));
#126079=DIRECTION('center_axis',(-3.35939703647716E-33,-1.37139182454908E-34,
1.));
#126080=DIRECTION('ref_axis',(-0.996672582494194,-0.0815092835470579,-3.35939703647716E-33));
#126081=DIRECTION('center_axis',(3.35939703647716E-33,1.37139182454908E-34,
-1.));
#126082=DIRECTION('ref_axis',(0.996672582494193,0.0815092835470633,3.35939703647716E-33));
#126083=DIRECTION('center_axis',(0.888655736322699,-0.458574947310428,-3.04823604041885E-33));
#126084=DIRECTION('ref_axis',(0.458574947310428,0.888655736322699,-1.41866579783395E-33));
#126085=DIRECTION('',(3.35939703647662E-33,-1.37139182454862E-34,1.));
#126086=DIRECTION('',(0.335588701144614,0.65032515637049,-0.681511125848851));
#126087=DIRECTION('center_axis',(-0.888653531715357,0.458579219508761,2.13514018757357E-6));
#126088=DIRECTION('ref_axis',(0.454698036374906,0.881133021060312,-0.129824092193755));
#126089=DIRECTION('',(1.41101612161356E-32,3.39907616780996E-32,-1.));
#126090=DIRECTION('center_axis',(-0.951355185205045,-0.308096269992797,
3.15372771923029E-33));
#126091=DIRECTION('ref_axis',(0.308096269992797,-0.951355185205045,-1.16548576868652E-33));
#126092=DIRECTION('center_axis',(0.951355185205055,0.308096269992766,-1.17032890463339E-14));
#126093=DIRECTION('ref_axis',(0.305785041452959,-0.944218457273914,-0.122257978745287));
#126094=DIRECTION('',(0.225467238628697,-0.696209099085458,0.681511125848849));
#126095=DIRECTION('',(3.35939703647662E-33,-1.37139182454862E-34,1.));
#126096=DIRECTION('',(1.50964222874619E-32,-3.63793170954442E-32,1.));
#126097=DIRECTION('center_axis',(3.35939703647662E-33,-1.37139182454862E-34,
1.));
#126098=DIRECTION('ref_axis',(0.996672582494195,-0.0815092835470462,-3.35939703647662E-33));
#126099=DIRECTION('center_axis',(-0.0276865250382154,-0.338543037176888,
-0.940543496235212));
#126100=DIRECTION('ref_axis',(0.0767818315756177,0.937404192592328,-0.339673269555052));
#126101=DIRECTION('center_axis',(-0.0276865250382154,-0.338543037176888,
-0.940543496235212));
#126102=DIRECTION('ref_axis',(0.0767818315756177,0.937404192592328,-0.339673269555052));
#126103=DIRECTION('center_axis',(-0.226207035727811,0.698493481841134,-0.678923583927297));
#126104=DIRECTION('ref_axis',(0.0576863962918442,0.705373020900032,0.706485089063614));
#126105=DIRECTION('center_axis',(-0.336689825853969,-0.652458985955238,
0.678923583927297));
#126106=DIRECTION('ref_axis',(-0.0576863962918536,-0.705373020900031,-0.706485089063614));
#126107=DIRECTION('center_axis',(-0.899370606478019,0.436511411929941,-0.0242960790723403));
#126108=DIRECTION('ref_axis',(0.316619608623823,0.612013741106922,-0.724700768684018));
#126109=DIRECTION('center_axis',(-3.35939703647662E-33,1.37139182454862E-34,
-1.));
#126110=DIRECTION('ref_axis',(-0.996672582494194,0.0815092835470578,3.35939703647662E-33));
#126111=DIRECTION('center_axis',(-4.48517628367996E-36,-4.12697442833547E-32,
1.));
#126112=DIRECTION('ref_axis',(0.610015726935643,0.792389306396281,3.27044400759104E-32));
#126113=DIRECTION('center_axis',(3.35939703647662E-33,-1.37139182454862E-34,
1.));
#126114=DIRECTION('ref_axis',(0.996672582494194,-0.0815092835470578,-3.35939703647662E-33));
#126115=DIRECTION('center_axis',(0.22536871201061,-0.695904863630098,0.681854357192688));
#126116=DIRECTION('ref_axis',(-0.0579168548267348,-0.708191003013486,-0.703641344136153));
#126117=DIRECTION('center_axis',(0.225567029082378,-0.696517237076053,0.681163162426516));
#126118=DIRECTION('ref_axis',(-0.057862523359542,-0.707526653121654,-0.704313824593084));
#126119=DIRECTION('center_axis',(0.335737230700132,0.650612986401989,-0.681163162426516));
#126120=DIRECTION('ref_axis',(0.0578625233595482,0.707526653121653,0.704313824593084));
#126121=DIRECTION('center_axis',(0.335442052700285,0.650040971676069,-0.681854357192686));
#126122=DIRECTION('ref_axis',(0.0579168548267194,0.708191003013486,0.703641344136154));
#126123=DIRECTION('center_axis',(3.35939703647662E-33,-1.37139182454862E-34,
1.));
#126124=DIRECTION('ref_axis',(0.996672582494194,-0.0815092835470577,-3.35939703647662E-33));
#126125=DIRECTION('center_axis',(-4.48517628367996E-36,-4.12697442833547E-32,
1.));
#126126=DIRECTION('ref_axis',(-0.473165773815079,0.880973410773547,3.63554251511521E-32));
#126127=DIRECTION('center_axis',(3.35939703647662E-33,-1.37139182454862E-34,
1.));
#126128=DIRECTION('ref_axis',(-0.996672582494195,0.0815092835470381,3.35939703647662E-33));
#126129=DIRECTION('center_axis',(-3.35939703647662E-33,1.37139182454862E-34,
-1.));
#126130=DIRECTION('ref_axis',(0.996672582494194,-0.0815092835470502,-3.35939703647662E-33));
#126131=DIRECTION('center_axis',(0.848320692261118,-0.529482769390674,-5.9706948941013E-33));
#126132=DIRECTION('ref_axis',(0.529482769390674,0.848320692261118,-3.08107063799443E-33));
#126133=DIRECTION('',(6.69643783993752E-33,-5.47644091186675E-34,1.));
#126134=DIRECTION('',(0.387479594994063,0.620807658463935,-0.681511125848847));
#126135=DIRECTION('center_axis',(-0.848318146765595,0.529486847677661,2.13514020029428E-6));
#126136=DIRECTION('ref_axis',(0.525005587425765,0.841139012446968,-0.12982409218426));
#126137=DIRECTION('',(1.3474376413819E-32,3.28646902736504E-32,-1.));
#126138=DIRECTION('center_axis',(-0.973302335538189,-0.229526825525702,
6.39195957962951E-33));
#126139=DIRECTION('ref_axis',(0.229526825525702,-0.973302335538189,-2.07003539272673E-33));
#126140=DIRECTION('center_axis',(0.973302335538189,0.229526825525702,-1.99719171769005E-15));
#126141=DIRECTION('ref_axis',(0.227804996989923,-0.966000967903135,-0.122257978703341));
#126142=DIRECTION('',(0.167969510126494,-0.712270193825424,0.681511125848844));
#126143=DIRECTION('',(6.69643783993752E-33,-5.47644091186675E-34,1.));
#126144=DIRECTION('',(1.54403351517636E-32,-3.76259056661214E-32,1.));
#126145=DIRECTION('center_axis',(6.69643783993752E-33,-5.47644091186674E-34,
1.));
#126146=DIRECTION('ref_axis',(0.986712473391291,-0.162476136260194,-6.69643783993752E-33));
#126147=DIRECTION('center_axis',(-0.0551888008202638,-0.335159854328745,
-0.940543496235212));
#126148=DIRECTION('ref_axis',(0.152933490497652,0.928026625390665,-0.339673269555052));
#126149=DIRECTION('center_axis',(-0.0551888008202638,-0.335159854328745,
-0.940543496235212));
#126150=DIRECTION('ref_axis',(0.152933490497652,0.928026625390665,-0.339673269555052));
#126151=DIRECTION('center_axis',(-0.168520647210029,0.714607275817443,-0.678923583927297));
#126152=DIRECTION('ref_axis',(0.114988899133967,0.698323973530006,0.706485089063614));
#126153=DIRECTION('center_axis',(-0.388750982722451,-0.622844636020608,
0.678923583927297));
#126154=DIRECTION('ref_axis',(-0.114988899133973,-0.698323973530004,-0.706485089063614));
#126155=DIRECTION('center_axis',(-0.86079829254277,0.508366009973053,-0.0242960790978609));
#126156=DIRECTION('ref_axis',(0.365450838207706,0.584169795627829,-0.724700858788939));
#126157=DIRECTION('center_axis',(-6.69643783993752E-33,5.47644091186674E-34,
-1.));
#126158=DIRECTION('ref_axis',(-0.98671247339129,0.162476136260201,6.69643783993751E-33));
#126159=DIRECTION('center_axis',(-8.94050445919518E-36,-4.12691962127156E-32,
1.));
#126160=DIRECTION('ref_axis',(0.672573034581739,0.740030751491795,3.05464874289731E-32));
#126161=DIRECTION('center_axis',(6.69643783993752E-33,-5.47644091186674E-34,
1.));
#126162=DIRECTION('ref_axis',(0.98671247339129,-0.162476136260201,-6.69643783993751E-33));
#126163=DIRECTION('center_axis',(0.167896109361599,-0.711958939854388,0.681854357192688));
#126164=DIRECTION('ref_axis',(-0.115448282540208,-0.701113794530378,-0.703641344136153));
#126165=DIRECTION('center_axis',(0.168043852428827,-0.712585440360654,0.681163162426516));
#126166=DIRECTION('ref_axis',(-0.115339981172784,-0.70045608372697,-0.704313824593084));
#126167=DIRECTION('center_axis',(0.387651091149391,0.621082424227087,-0.681163162426516));
#126168=DIRECTION('ref_axis',(0.115339981172785,0.700456083726971,0.704313824593083));
#126169=DIRECTION('center_axis',(0.3873102708195,0.620536372580266,-0.681854357192686));
#126170=DIRECTION('ref_axis',(0.115448282540195,0.701113794530378,0.703641344136155));
#126171=DIRECTION('center_axis',(6.69643783993752E-33,-5.47644091186674E-34,
1.));
#126172=DIRECTION('ref_axis',(0.98671247339129,-0.162476136260201,-6.69643783993751E-33));
#126173=DIRECTION('center_axis',(-8.94050445919518E-36,-4.12691962127156E-32,
1.));
#126174=DIRECTION('ref_axis',(-0.399783842199965,0.916609447647052,3.78241608761511E-32));
#126175=DIRECTION('center_axis',(6.69643783993752E-33,-5.47644091186674E-34,
1.));
#126176=DIRECTION('ref_axis',(-0.986712473391296,0.162476136260162,6.69643783993754E-33));
#126177=DIRECTION('center_axis',(-6.69643783993752E-33,5.47644091186674E-34,
-1.));
#126178=DIRECTION('ref_axis',(0.986712473391291,-0.162476136260193,-6.69643783993752E-33));
#126179=DIRECTION('center_axis',(0.802340213955601,-0.596866970999133,-8.74792807954735E-33));
#126180=DIRECTION('ref_axis',(0.596866970999133,0.802340213955601,-4.97615149054745E-33));
#126181=DIRECTION('',(9.98891495440811E-33,-1.22878288375636E-33,1.));
#126182=DIRECTION('',(0.436791876068461,0.587158788016352,-0.681511125848847));
#126183=DIRECTION('center_axis',(-0.802337344511779,0.596870828234408,2.13514018553818E-6));
#126184=DIRECTION('ref_axis',(0.591819312914846,0.795547362487343,-0.129824092141757));
#126185=DIRECTION('',(1.27489218595841E-32,3.17941881426319E-32,-1.));
#126186=DIRECTION('center_axis',(-0.988772319411909,-0.149429917903995,
9.69314568243686E-33));
#126187=DIRECTION('ref_axis',(0.149429917903995,-0.988772319411909,-2.70762924361262E-33));
#126188=DIRECTION('center_axis',(0.988772319411903,0.14942991790403,1.57485563471379E-14));
#126189=DIRECTION('ref_axis',(0.148308947855242,-0.981354901463211,-0.122257978717968));
#126190=DIRECTION('',(0.109353972247421,-0.723591247941779,0.681511125848852));
#126191=DIRECTION('',(9.98891495440811E-33,-1.22878288375636E-33,1.));
#126192=DIRECTION('',(1.56814951331063E-32,-3.88963784073378E-32,1.));
#126193=DIRECTION('center_axis',(9.98891495440811E-33,-1.22878288375636E-33,
1.));
#126194=DIRECTION('ref_axis',(0.970185955574067,-0.242361737093202,-9.9889149544081E-33));
#126195=DIRECTION('center_axis',(-0.0823238042383858,-0.329546237947602,
-0.940543496235183));
#126196=DIRECTION('ref_axis',(0.228067402272856,0.912473194110511,-0.339673269555131));
#126197=DIRECTION('center_axis',(-0.0823238042383858,-0.329546237947602,
-0.940543496235183));
#126198=DIRECTION('ref_axis',(0.228067402272856,0.912473194110511,-0.339673269555131));
#126199=DIRECTION('center_axis',(-0.109712781589014,0.725965476275088,-0.678923583927297));
#126200=DIRECTION('ref_axis',(0.171526169824185,0.686627695331482,0.706485089063614));
#126201=DIRECTION('center_axis',(-0.438225065940312,-0.589085357795391,
0.678923583927297));
#126202=DIRECTION('ref_axis',(-0.171526169824195,-0.686627695331478,-0.706485089063615));
#126203=DIRECTION('center_axis',(-0.816497507979672,0.576837516120213,-0.0242960790920933));
#126204=DIRECTION('ref_axis',(0.411849783893902,0.552437924326749,-0.724701383517445));
#126205=DIRECTION('center_axis',(-9.98891495440811E-33,1.22878288375636E-33,
-1.));
#126206=DIRECTION('ref_axis',(-0.970185955574069,0.242361737093194,9.98891495440811E-33));
#126207=DIRECTION('center_axis',(-1.3336335052612E-35,-4.12682868151287E-32,
1.));
#126208=DIRECTION('ref_axis',(0.730654479649428,0.682747414032615,2.81855603575337E-32));
#126209=DIRECTION('center_axis',(9.98891495440811E-33,-1.22878288375636E-33,
1.));
#126210=DIRECTION('ref_axis',(0.970185955574069,-0.242361737093194,-9.98891495440811E-33));
#126211=DIRECTION('center_axis',(0.109306185805694,-0.723275046798904,0.681854357192688));
#126212=DIRECTION('ref_axis',(-0.172211420981001,-0.689370789420303,-0.703641344136153));
#126213=DIRECTION('center_axis',(0.109402371662647,-0.723911505107977,0.681163162426516));
#126214=DIRECTION('ref_axis',(-0.172049870441076,-0.688724094662203,-0.704313824593084));
#126215=DIRECTION('center_axis',(0.436985197544978,0.58741866099034,-0.681163162426516));
#126216=DIRECTION('ref_axis',(0.172049870441082,0.688724094662202,0.704313824593084));
#126217=DIRECTION('center_axis',(0.436601002988107,0.586902206306236,-0.681854357192686));
#126218=DIRECTION('ref_axis',(0.172211420980992,0.689370789420304,0.703641344136155));
#126219=DIRECTION('center_axis',(9.98891495440811E-33,-1.22878288375636E-33,
1.));
#126220=DIRECTION('ref_axis',(0.970185955574069,-0.242361737093194,-9.98891495440811E-33));
#126221=DIRECTION('center_axis',(-1.3336335052612E-35,-4.12682868151287E-32,
1.));
#126222=DIRECTION('ref_axis',(-0.323741415074715,0.946145599876373,3.90414904605883E-32));
#126223=DIRECTION('center_axis',(9.98891495440811E-33,-1.22878288375636E-33,
1.));
#126224=DIRECTION('ref_axis',(-0.970185955574059,0.242361737093233,9.98891495440806E-33));
#126225=DIRECTION('center_axis',(-9.98891495440811E-33,1.22878288375636E-33,
-1.));
#126226=DIRECTION('ref_axis',(0.970185955574068,-0.2423617370932,-9.98891495440811E-33));
#126227=DIRECTION('center_axis',(0.751020293903028,-0.660279121391711,-1.13614535681191E-32));
#126228=DIRECTION('ref_axis',(0.660279121391711,0.751020293903028,-7.0912969050856E-33));
#126229=DIRECTION('',(1.32149174879121E-32,-2.17602269387938E-33,1.));
#126230=DIRECTION('',(0.483197379273213,0.549602472708897,-0.681511125848848));
#126231=DIRECTION('center_axis',(-0.751017119606567,0.660282731906035,2.13514017760057E-6));
#126232=DIRECTION('ref_axis',(0.654694578522591,0.744661476088215,-0.129824092075573));
#126233=DIRECTION('',(1.19386253337977E-32,3.0786379300106E-32,-1.));
#126234=DIRECTION('center_axis',(-0.997662186635891,-0.0683385788328371,
1.30353171787955E-32));
#126235=DIRECTION('ref_axis',(0.0683385788328371,-0.997662186635891,-3.07402423946213E-33));
#126236=DIRECTION('center_axis',(0.997662186635891,0.0683385788328493,8.00466807870197E-15));
#126237=DIRECTION('ref_axis',(0.0678259271421216,-0.99017808006695,-0.122257978726304));
#126238=DIRECTION('',(0.0500107017251773,-0.73009692168724,0.681511125848853));
#126239=DIRECTION('',(1.32149174879121E-32,-2.17602269387938E-33,1.));
#126240=DIRECTION('',(1.58182973516027E-32,-4.01822805326139E-32,1.));
#126241=DIRECTION('center_axis',(1.32149174879121E-32,-2.17602269387938E-33,
1.));
#126242=DIRECTION('ref_axis',(0.947203010291915,-0.320634460552722,-1.32149174879121E-32));
#126243=DIRECTION('center_axis',(-0.108910956321728,-0.321739545724065,
-0.940543496235213));
#126244=DIRECTION('ref_axis',(0.301683563113628,0.890847404271264,-0.339673269555048));
#126245=DIRECTION('center_axis',(-0.108910956321728,-0.321739545724065,
-0.940543496235213));
#126246=DIRECTION('ref_axis',(0.301683563113628,0.890847404271264,-0.339673269555048));
#126247=DIRECTION('center_axis',(-0.0501747955078592,0.732492496263995,
-0.678923583927297));
#126248=DIRECTION('ref_axis',(0.226921962154045,0.670362023106124,0.706485089063615));
#126249=DIRECTION('center_axis',(-0.484782833646386,-0.551405813706289,
0.678923583927297));
#126250=DIRECTION('ref_axis',(-0.226921962154054,-0.670362023106121,-0.706485089063614));
#126251=DIRECTION('center_axis',(-0.766763067216207,0.641470263764373,-0.0242960790923158));
#126252=DIRECTION('ref_axis',(0.455508349976982,0.517030330878251,-0.724701166035472));
#126253=DIRECTION('center_axis',(-1.32149174879121E-32,2.17602269387938E-33,
-1.));
#126254=DIRECTION('ref_axis',(-0.947203010291914,0.320634460552723,1.32149174879121E-32));
#126255=DIRECTION('center_axis',(-1.76434145365967E-35,-4.1267022142485E-32,
1.));
#126256=DIRECTION('ref_axis',(0.783873539704558,0.620920505178438,2.56373704417269E-32));
#126257=DIRECTION('center_axis',(1.32149174879121E-32,-2.17602269387938E-33,
1.));
#126258=DIRECTION('ref_axis',(0.947203010291914,-0.320634460552723,-1.32149174879121E-32));
#126259=DIRECTION('center_axis',(0.0499888476175039,-0.729777877638957,
0.681854357192688));
#126260=DIRECTION('ref_axis',(-0.227828520828051,-0.673040135444811,-0.703641344136153));
#126261=DIRECTION('center_axis',(0.0500328361631726,-0.730420058225798,
0.681163162426516));
#126262=DIRECTION('ref_axis',(-0.227614796207816,-0.672408760378936,-0.704313824593084));
#126263=DIRECTION('center_axis',(0.483411239548387,0.549845723481961,-0.681163162426516));
#126264=DIRECTION('ref_axis',(0.227614796207819,0.672408760378935,0.704313824593084));
#126265=DIRECTION('center_axis',(0.482986227515924,0.549362302681286,-0.681854357192686));
#126266=DIRECTION('ref_axis',(0.227828520828041,0.673040135444813,0.703641344136155));
#126267=DIRECTION('center_axis',(1.32149174879121E-32,-2.17602269387938E-33,
1.));
#126268=DIRECTION('ref_axis',(0.947203010291914,-0.320634460552723,-1.32149174879121E-32));
#126269=DIRECTION('center_axis',(-1.76434145365967E-35,-4.1267022142485E-32,
1.));
#126270=DIRECTION('ref_axis',(-0.24554454224571,0.969385309241555,3.99993127769249E-32));
#126271=DIRECTION('center_axis',(1.32149174879121E-32,-2.17602269387938E-33,
1.));
#126272=DIRECTION('ref_axis',(-0.947203010291915,0.320634460552722,1.32149174879121E-32));
#126273=DIRECTION('center_axis',(-1.32149174879121E-32,2.17602269387938E-33,
-1.));
#126274=DIRECTION('ref_axis',(0.947203010291914,-0.320634460552723,-1.32149174879121E-32));
#126275=DIRECTION('center_axis',(0.694702457704156,-0.719297223169814,-1.37938787788914E-32));
#126276=DIRECTION('ref_axis',(0.719297223169814,0.694702457704156,-9.41243093784955E-33));
#126277=DIRECTION('',(1.63529769258419E-32,-3.3830597969029E-33,1.));
#126278=DIRECTION('',(0.526387283640853,0.508388643623594,-0.68151112584885));
#126279=DIRECTION('center_axis',(-0.694698999679441,0.719300562935846,2.13514020416028E-6));
#126280=DIRECTION('ref_axis',(0.713212959724422,0.688819990421442,-0.129824092051258));
#126281=DIRECTION('',(1.10488792261493E-32,2.98479705476426E-32,-1.));
#126282=DIRECTION('center_axis',(-0.999912776610487,0.0132075422053813,
1.63962324688167E-32));
#126283=DIRECTION('ref_axis',(-0.0132075422053813,-0.999912776610487,-3.16678208202881E-33));
#126284=DIRECTION('center_axis',(0.999912776610487,-0.0132075422053234,
2.36411209098337E-14));
#126285=DIRECTION('ref_axis',(0.013108463925482,0.992411786921792,0.122257978685276));
#126286=DIRECTION('',(-0.00966538176586899,-0.73174392087639,0.68151112584885));
#126287=DIRECTION('',(1.63529769258419E-32,-3.3830597969029E-33,1.));
#126288=DIRECTION('',(1.58498314110597E-32,-4.14750545754649E-32,1.));
#126289=DIRECTION('center_axis',(1.63529769258419E-32,-3.3830597969029E-33,
1.));
#126290=DIRECTION('ref_axis',(0.917916585253764,-0.396773414578232,-1.63529769258419E-32));
#126291=DIRECTION('center_axis',(-0.134773323959819,-0.311791729907105,
-0.940543496235212));
#126292=DIRECTION('ref_axis',(0.373292069616715,0.863293171935844,-0.339673269555051));
#126293=DIRECTION('center_axis',(-0.134773323959819,-0.311791729907105,
-0.940543496235212));
#126294=DIRECTION('ref_axis',(0.373292069616715,0.863293171935844,-0.339673269555051));
#126295=DIRECTION('center_axis',(0.009697095559142,0.73414489954302,-0.678923583927297));
#126296=DIRECTION('ref_axis',(0.280807626265263,0.649635202218942,0.706485089063614));
#126297=DIRECTION('center_axis',(-0.528114451578082,-0.510056754902527,
0.678923583927297));
#126298=DIRECTION('ref_axis',(-0.280807626265268,-0.64963520221894,-0.706485089063614));
#126299=DIRECTION('center_axis',(-0.711925944736631,0.701834132649891,-0.0242960790752475));
#126300=DIRECTION('ref_axis',(-0.496135854106694,-0.478182219455507,0.72470061354081));
#126301=DIRECTION('center_axis',(-1.63529769258419E-32,3.3830597969029E-33,
-1.));
#126302=DIRECTION('ref_axis',(-0.917916585253767,0.396773414578224,1.63529769258419E-32));
#126303=DIRECTION('center_axis',(-2.18330800077971E-35,-4.12654106109723E-32,
1.));
#126304=DIRECTION('ref_axis',(0.831876050682982,0.554961472806973,2.29188754650208E-32));
#126305=DIRECTION('center_axis',(1.63529769258419E-32,-3.3830597969029E-33,
1.));
#126306=DIRECTION('ref_axis',(0.917916585253767,-0.396773414578224,-1.63529769258419E-32));
#126307=DIRECTION('center_axis',(-0.00966115810400148,-0.731424157108197,
0.681854357192688));
#126308=DIRECTION('ref_axis',(-0.281929459458053,-0.65223051041174,-0.703641344136153));
#126309=DIRECTION('center_axis',(-0.00966965960613086,-0.732067786366952,
0.681163162426516));
#126310=DIRECTION('ref_axis',(-0.281664983059587,-0.651618656734984,-0.704313824593084));
#126311=DIRECTION('center_axis',(0.526620259509841,0.508613653401967,-0.681163162426516));
#126312=DIRECTION('ref_axis',(0.28166498305959,0.651618656734984,0.704313824593083));
#126313=DIRECTION('center_axis',(0.52615725838674,0.508166483570392,-0.681854357192686));
#126314=DIRECTION('ref_axis',(0.281929459458042,0.652230510411742,0.703641344136155));
#126315=DIRECTION('center_axis',(1.63529769258419E-32,-3.3830597969029E-33,
1.));
#126316=DIRECTION('ref_axis',(0.917916585253767,-0.396773414578224,-1.63529769258419E-32));
#126317=DIRECTION('center_axis',(-2.18330800077971E-35,-4.12654106109723E-32,
1.));
#126318=DIRECTION('ref_axis',(-0.165713611000076,0.986173919311049,4.06912536756749E-32));
#126319=DIRECTION('center_axis',(1.63529769258419E-32,-3.3830597969029E-33,
1.));
#126320=DIRECTION('ref_axis',(-0.917916585253776,0.396773414578204,1.6352976925842E-32));
#126321=DIRECTION('center_axis',(-1.63529769258419E-32,3.3830597969029E-33,
-1.));
#126322=DIRECTION('ref_axis',(0.917916585253764,-0.396773414578231,-1.63529769258419E-32));
#126323=DIRECTION('center_axis',(0.6337614912671,-0.773528520603411,-1.60290163234086E-32));
#126324=DIRECTION('ref_axis',(0.773528520603411,0.6337614912671,-1.19241068248114E-32));
#126325=DIRECTION('',(1.93822100003815E-32,-4.84186156005344E-33,1.));
#126326=DIRECTION('',(0.566074167483658,0.463791571993196,-0.681511125848847));
#126327=DIRECTION('center_axis',(-0.633757772526766,0.773531567395509,2.13514017139377E-6));
#126328=DIRECTION('ref_axis',(0.766985026313205,0.628394521334046,-0.129824092404638));
#126329=DIRECTION('',(1.00856046501877E-32,2.8985206840663E-32,-1.));
#126330=DIRECTION('center_axis',(-0.995509112030735,0.0946657692293139,
1.97535252157573E-32));
#126331=DIRECTION('ref_axis',(-0.0946657692293139,-0.995509112030735,-2.98528548317433E-33));
#126332=DIRECTION('center_axis',(0.995509112030737,-0.0946657692292906,
9.50256186696977E-15));
#126333=DIRECTION('ref_axis',(0.0939556203289657,0.988041157067433,0.122257978673981));
#126334=DIRECTION('',(-0.0692771437359349,-0.728521285001353,0.681511125848851));
#126335=DIRECTION('',(1.93822100003815E-32,-4.84186156005344E-33,1.));
#126336=DIRECTION('',(1.57758874575141E-32,-4.27660973379283E-32,1.));
#126337=DIRECTION('center_axis',(1.93822100003815E-32,-4.84186156005343E-33,
1.));
#126338=DIRECTION('ref_axis',(0.882521576786326,-0.470271906992728,-1.93822100003815E-32));
#126339=DIRECTION('center_axis',(-0.159738797363072,-0.299768991569782,
-0.940543496235148));
#126340=DIRECTION('ref_axis',(0.4424163789848,0.829993865974706,-0.33967326955523));
#126341=DIRECTION('center_axis',(-0.159738797363072,-0.299768991569782,
-0.940543496235148));
#126342=DIRECTION('ref_axis',(0.4424163789848,0.829993865974706,-0.33967326955523));
#126343=DIRECTION('center_axis',(0.0695044540551054,0.730911689640969,-0.678923583927297));
#126344=DIRECTION('ref_axis',(0.332824561953684,0.624585166243257,0.706485089063614));
#126345=DIRECTION('center_axis',(-0.567931554967276,-0.46531335254833,0.678923583927297));
#126346=DIRECTION('ref_axis',(-0.332824561953689,-0.624585166243253,-0.706485089063614));
#126347=DIRECTION('center_axis',(-0.652351072554589,0.757527411173429,-0.0242960790614626));
#126348=DIRECTION('ref_axis',(-0.533461682387404,-0.436151780773054,0.724700115601546));
#126349=DIRECTION('center_axis',(-1.93822100003815E-32,4.84186156005343E-33,
-1.));
#126350=DIRECTION('ref_axis',(-0.882521576786327,0.470271906992727,1.93822100003815E-32));
#126351=DIRECTION('center_axis',(-2.58774499337554E-35,-4.12634629450669E-32,
1.));
#126352=DIRECTION('ref_axis',(0.874342563793993,0.485309263396185,2.00481665629657E-32));
#126353=DIRECTION('center_axis',(1.93822100003815E-32,-4.84186156005344E-33,
1.));
#126354=DIRECTION('ref_axis',(0.882521576786327,-0.470271906992727,-1.93822100003815E-32));
#126355=DIRECTION('center_axis',(-0.0692468704123036,-0.728202929488373,
0.681854357192688));
#126356=DIRECTION('ref_axis',(-0.334154204050443,-0.627080398942338,-0.703641344136153));
#126357=DIRECTION('center_axis',(-0.0693078053861371,-0.728843724172518,
0.681163162426516));
#126358=DIRECTION('ref_axis',(-0.333840735920551,-0.626492138439971,-0.704313824593084));
#126359=DIRECTION('center_axis',(0.566324708530484,0.463996843373929,-0.681163162426516));
#126360=DIRECTION('ref_axis',(0.333840735920556,0.626492138439969,0.704313824593084));
#126361=DIRECTION('center_axis',(0.56582679951283,0.463588900352905,-0.681854357192686));
#126362=DIRECTION('ref_axis',(0.33415420405043,0.627080398942345,0.703641344136154));
#126363=DIRECTION('center_axis',(1.93822100003815E-32,-4.84186156005343E-33,
1.));
#126364=DIRECTION('ref_axis',(0.882521576786327,-0.470271906992727,-1.93822100003815E-32));
#126365=DIRECTION('center_axis',(-2.58774499337554E-35,-4.12634629450669E-32,
1.));
#126366=DIRECTION('ref_axis',(-0.0847798830140404,0.996399704654776,4.11127084043199E-32));
#126367=DIRECTION('center_axis',(1.93822100003815E-32,-4.84186156005344E-33,
1.));
#126368=DIRECTION('ref_axis',(-0.882521576786316,0.470271906992746,1.93822100003814E-32));
#126369=DIRECTION('center_axis',(-1.93822100003815E-32,4.84186156005343E-33,
-1.));
#126370=DIRECTION('ref_axis',(0.882521576786327,-0.470271906992726,-1.93822100003815E-32));
#126371=DIRECTION('center_axis',(0.568602946668948,-0.822612113355614,-1.80519917300835E-32));
#126372=DIRECTION('ref_axis',(0.822612113355614,0.568602946668948,-1.46096097773409E-32));
#126373=DIRECTION('',(2.22824576652082E-32,-6.54271989828255E-33,1.));
#126374=DIRECTION('',(0.601993921137519,0.416108043971408,-0.681511125848848));
#126375=DIRECTION('center_axis',(-0.568598991960532,0.822614846897932,2.13514021179288E-6));
#126376=DIRECTION('ref_axis',(0.815652934166245,0.563787190442918,-0.129824092057199));
#126377=DIRECTION('',(9.05521203928678E-33,2.82038297292912E-32,-1.));
#126378=DIRECTION('center_axis',(-0.984480498557861,0.175494011177778,2.30848531903008E-32));
#126379=DIRECTION('ref_axis',(-0.175494011177778,-0.984480498557861,-2.53074227281923E-33));
#126380=DIRECTION('center_axis',(0.98448049855786,-0.17549401117778,-2.26433201113865E-15));
#126381=DIRECTION('ref_axis',(0.174177517580498,0.977095276325475,0.122257978684169));
#126382=DIRECTION('',(-0.128427877744355,-0.720450460172188,0.681511125848848));
#126383=DIRECTION('',(2.22824576652082E-32,-6.54271989828255E-33,1.));
#126384=DIRECTION('',(1.5596957575777E-32,-4.4046817143427E-32,1.));
#126385=DIRECTION('center_axis',(2.22824576652082E-32,-6.54271989828255E-33,
1.));
#126386=DIRECTION('ref_axis',(0.841253532831189,-0.540640817455585,-2.22824576652082E-32));
#126387=DIRECTION('center_axis',(-0.183641235424748,-0.28575134005165,-0.940543496235213));
#126388=DIRECTION('ref_axis',(0.508596480344212,0.791171087775118,-0.339673269555049));
#126389=DIRECTION('center_axis',(-0.183641235424748,-0.28575134005165,-0.940543496235213));
#126390=DIRECTION('ref_axis',(0.508596480344212,0.791171087775118,-0.339673269555049));
#126391=DIRECTION('center_axis',(0.12884927187676,0.722814383036297,-0.678923583927297));
#126392=DIRECTION('ref_axis',(0.382626605094485,0.595378619035523,0.706485089063614));
#126393=DIRECTION('center_axis',(-0.603969167560274,-0.417473366604222,
0.678923583927297));
#126394=DIRECTION('ref_axis',(-0.382626605094491,-0.595378619035519,-0.706485089063614));
#126395=DIRECTION('center_axis',(-0.588434911639695,0.808179469737246,-0.0242960790830131));
#126396=DIRECTION('ref_axis',(-0.567236981821274,-0.39121838869147,0.724700199257556));
#126397=DIRECTION('center_axis',(-2.22824576652082E-32,6.54271989828255E-33,
-1.));
#126398=DIRECTION('ref_axis',(-0.841253532831187,0.540640817455589,2.22824576652081E-32));
#126399=DIRECTION('center_axis',(-2.97496096998732E-35,-4.1261192106164E-32,
1.));
#126400=DIRECTION('ref_axis',(0.91099047139933,0.412427400907876,1.70443478296702E-32));
#126401=DIRECTION('center_axis',(2.22824576652082E-32,-6.54271989828255E-33,
1.));
#126402=DIRECTION('ref_axis',(0.841253532831187,-0.540640817455589,-2.22824576652081E-32));
#126403=DIRECTION('center_axis',(-0.128371756222941,-0.72013563151783,0.681854357192688));
#126404=DIRECTION('ref_axis',(-0.38415520754645,-0.597757170878956,-0.703641344136152));
#126405=DIRECTION('center_axis',(-0.128484719156282,-0.720769327244466,
0.681163162426516));
#126406=DIRECTION('ref_axis',(-0.383794833763806,-0.597196418327567,-0.704313824593084));
#126407=DIRECTION('center_axis',(0.602260360052857,0.416292210907329,-0.681163162426516));
#126408=DIRECTION('ref_axis',(0.383794833763808,0.597196418327568,0.704313824593083));
#126409=DIRECTION('center_axis',(0.601730856643013,0.415926209490355,-0.681854357192686));
#126410=DIRECTION('ref_axis',(0.384155207546438,0.597757170878959,0.703641344136156));
#126411=DIRECTION('center_axis',(2.22824576652082E-32,-6.54271989828255E-33,
1.));
#126412=DIRECTION('ref_axis',(0.841253532831187,-0.540640817455589,-2.22824576652081E-32));
#126413=DIRECTION('center_axis',(-2.97496096998732E-35,-4.1261192106164E-32,
1.));
#126414=DIRECTION('ref_axis',(-0.00328195889422331,0.999994614358406,4.12608722511754E-32));
#126415=DIRECTION('center_axis',(2.22824576652082E-32,-6.54271989828255E-33,
1.));
#126416=DIRECTION('ref_axis',(-0.841253532831199,0.54064081745557,2.22824576652083E-32));
#126417=DIRECTION('center_axis',(-2.22824576652082E-32,6.54271989828255E-33,
-1.));
#126418=DIRECTION('ref_axis',(0.841253532831188,-0.540640817455587,-2.22824576652082E-32));
#126419=DIRECTION('center_axis',(0.499660443273597,-0.866221358214881,-1.98493424313522E-32));
#126420=DIRECTION('ref_axis',(0.866221358214881,0.499660443273597,-1.74510682163656E-32));
#126421=DIRECTION('',(2.50344192506196E-32,-8.47431587997121E-33,1.));
#126422=DIRECTION('',(0.633907504568215,0.365655385569985,-0.681511125848848));
#126423=DIRECTION('center_axis',(-0.499656278915068,0.866223760316114,2.13514019205242E-6));
#126424=DIRECTION('ref_axis',(0.858892806234444,0.495427948762394,-0.129824092462874));
#126425=DIRECTION('',(7.96455848626919E-33,2.7509039149285E-32,-1.));
#126426=DIRECTION('center_axis',(-0.966900329794933,0.255154369436328,2.6368046954407E-32));
#126427=DIRECTION('ref_axis',(-0.255154369436328,-0.966900329794933,-1.80617736103409E-33));
#126428=DIRECTION('center_axis',(0.966900329794936,-0.255154369436314,1.27209663547126E-17));
#126429=DIRECTION('ref_axis',(0.253240292188925,0.959646987726596,0.122257978714434));
#126430=DIRECTION('',(-0.186723945415513,-0.70758515639653,0.681511125848847));
#126431=DIRECTION('',(2.50344192506196E-32,-8.47431587997121E-33,1.));
#126432=DIRECTION('',(1.53142325146899E-32,-4.53086910129593E-32,1.));
#126433=DIRECTION('center_axis',(2.50344192506196E-32,-8.47431587997121E-33,
1.));
#126434=DIRECTION('ref_axis',(0.794387085412117,-0.607411852477742,-2.50344192506195E-32));
#126435=DIRECTION('center_axis',(-0.206321571363482,-0.269832060511356,
-0.940543496235182));
#126436=DIRECTION('ref_axis',(0.571391956039873,0.747083196520074,-0.339673269555135));
#126437=DIRECTION('center_axis',(-0.206321571363482,-0.269832060511356,
-0.940543496235182));
#126438=DIRECTION('ref_axis',(0.571391956039873,0.747083196520074,-0.339673269555135));
#126439=DIRECTION('center_axis',(0.187336619052708,0.709906865968498,-0.678923583927297));
#126440=DIRECTION('ref_axis',(0.42988233130733,0.562209925348665,0.706485089063615));
#126441=DIRECTION('center_axis',(-0.635987464991058,-0.366855164283621,
0.678923583927297));
#126442=DIRECTION('ref_axis',(-0.429882331307336,-0.562209925348662,-0.706485089063613));
#126443=DIRECTION('center_axis',(-0.520602813447602,0.853453227290336,-0.0242960790695151));
#126444=DIRECTION('ref_axis',(-0.597236896350991,-0.343681188212525,0.724700855874934));
#126445=DIRECTION('center_axis',(-2.50344192506196E-32,8.47431587997121E-33,
-1.));
#126446=DIRECTION('ref_axis',(-0.794387085412123,0.607411852477734,2.50344192506196E-32));
#126447=DIRECTION('center_axis',(-3.34237907217862E-35,-4.1258613206322E-32,
1.));
#126448=DIRECTION('ref_axis',(0.941575887720349,0.336800902112267,1.39274091832102E-32));
#126449=DIRECTION('center_axis',(2.50344192506196E-32,-8.47431587997121E-33,
1.));
#126450=DIRECTION('ref_axis',(0.794387085412123,-0.607411852477734,-2.50344192506196E-32));
#126451=DIRECTION('center_axis',(-0.186642349175764,-0.707275949733552,
0.681854357192688));
#126452=DIRECTION('ref_axis',(-0.431599721517371,-0.56445596746637,-0.703641344136153));
#126453=DIRECTION('center_axis',(-0.186806588318928,-0.70789832936217,0.681163162426516));
#126454=DIRECTION('ref_axis',(-0.43119484031005,-0.563926454581669,-0.704313824593085));
#126455=DIRECTION('center_axis',(0.634188068245042,0.36581722246052,-0.681163162426516));
#126456=DIRECTION('ref_axis',(0.431194840310054,0.563926454581671,0.704313824593082));
#126457=DIRECTION('center_axis',(0.633630494200839,0.36549559832664,-0.681854357192686));
#126458=DIRECTION('ref_axis',(0.431599721517362,0.564455967466375,0.703641344136155));
#126459=DIRECTION('center_axis',(2.50344192506196E-32,-8.47431587997121E-33,
1.));
#126460=DIRECTION('ref_axis',(0.794387085412123,-0.607411852477734,-2.50344192506196E-32));
#126461=DIRECTION('center_axis',(-3.34237907217862E-35,-4.1258613206322E-32,
1.));
#126462=DIRECTION('ref_axis',(0.0782378061205324,0.996934724890976,4.11347592102861E-32));
#126463=DIRECTION('center_axis',(2.50344192506196E-32,-8.47431587997121E-33,
1.));
#126464=DIRECTION('ref_axis',(-0.79438708541211,0.607411852477751,2.50344192506194E-32));
#126465=DIRECTION('center_axis',(-2.50344192506196E-32,8.47431587997121E-33,
-1.));
#126466=DIRECTION('ref_axis',(0.79438708541212,-0.607411852477738,-2.50344192506196E-32));
#126467=DIRECTION('center_axis',(0.42739278206643,-0.904066042851692,-2.14091073548399E-32));
#126468=DIRECTION('ref_axis',(0.904066042851692,0.427392782066429,-2.04295727047815E-32));
#126469=DIRECTION('',(2.76197809063066E-32,-1.06237950525522E-32,1.));
#126470=DIRECTION('',(0.661602538143388,0.312769350906479,-0.68151112584885));
#126471=DIRECTION('center_axis',(-0.42738843577091,0.904068097526252,2.13514020324528E-6));
#126472=DIRECTION('ref_axis',(0.896416888448679,0.423771715862612,-0.129824092289708));
#126473=DIRECTION('',(6.82090211058513E-33,2.69054588173222E-32,-1.));
#126474=DIRECTION('center_axis',(-0.942885598864545,0.333116717463787,2.95812573952646E-32));
#126475=DIRECTION('ref_axis',(-0.333116717463787,-0.942885598864545,-8.16412607762027E-34));
#126476=DIRECTION('center_axis',(0.942885598864544,-0.33311671746379,-8.77746678475083E-15));
#126477=DIRECTION('ref_axis',(0.330617794436068,0.935812406761036,0.122257978694019));
#126478=DIRECTION('',(-0.243777396037202,-0.690010990148384,0.681511125848851));
#126479=DIRECTION('',(2.76197809063066E-32,-1.06237950525522E-32,1.));
#126480=DIRECTION('',(1.49295937628881E-32,-4.65433213841181E-32,1.));
#126481=DIRECTION('center_axis',(2.76197809063066E-32,-1.06237950525522E-32,
1.));
#126482=DIRECTION('ref_axis',(0.742234123004276,-0.670140661837553,-2.76197809063066E-32));
#126483=DIRECTION('center_axis',(-0.22762887128535,-0.25211709312737,-0.940543496235215));
#126484=DIRECTION('ref_axis',(0.630384912541233,0.698023589852212,-0.339673269555043));
#126485=DIRECTION('center_axis',(-0.22762887128535,-0.25211709312737,-0.940543496235215));
#126486=DIRECTION('ref_axis',(0.630384912541233,0.698023589852212,-0.339673269555043));
#126487=DIRECTION('center_axis',(0.244577271937227,0.692275035834066,-0.678923583927297));
#126488=DIRECTION('ref_axis',(0.474277261530919,0.525299817366719,0.706485089063614));
#126489=DIRECTION('center_axis',(-0.663773370772871,-0.313795601371554,
0.678923583927297));
#126490=DIRECTION('ref_axis',(-0.474277261530926,-0.525299817366714,-0.706485089063614));
#126491=DIRECTION('center_axis',(-0.449306189438012,0.893047394416651,-0.0242960790730498));
#126492=DIRECTION('ref_axis',(-0.623262680235246,-0.29385717695526,0.724701035584925));
#126493=DIRECTION('center_axis',(-2.76197809063066E-32,1.06237950525522E-32,
-1.));
#126494=DIRECTION('ref_axis',(-0.742234123004278,0.67014066183755,2.76197809063066E-32));
#126495=DIRECTION('center_axis',(-3.68755419309748E-35,-4.12557434076937E-32,
1.));
#126496=DIRECTION('ref_axis',(0.965895271857685,0.258933048881306,1.07180933360173E-32));
#126497=DIRECTION('center_axis',(2.76197809063066E-32,-1.06237950525522E-32,
1.));
#126498=DIRECTION('ref_axis',(0.742234123004278,-0.67014066183755,-2.76197809063066E-32));
#126499=DIRECTION('center_axis',(-0.243670868088643,-0.689709463196115,
0.681854357192688));
#126500=DIRECTION('ref_axis',(-0.476172010550545,-0.52739840271897,-0.703641344136152));
#126501=DIRECTION('center_axis',(-0.243885290457229,-0.690316384892972,
0.681163162426516));
#126502=DIRECTION('ref_axis',(-0.475725316336185,-0.526903653321838,-0.704313824593083));
#126503=DIRECTION('center_axis',(0.661895359476724,0.312907780753829,-0.681163162426516));
#126504=DIRECTION('ref_axis',(0.475725316336192,0.52690365332183,0.704313824593086));
#126505=DIRECTION('center_axis',(0.661313425361432,0.31263267425859,-0.681854357192686));
#126506=DIRECTION('ref_axis',(0.476172010550534,0.527398402718976,0.703641344136155));
#126507=DIRECTION('center_axis',(2.76197809063066E-32,-1.06237950525522E-32,
1.));
#126508=DIRECTION('ref_axis',(0.742234123004278,-0.67014066183755,-2.76197809063066E-32));
#126509=DIRECTION('center_axis',(-3.68755419309748E-35,-4.12557434076937E-32,
1.));
#126510=DIRECTION('ref_axis',(0.159236911443873,0.98724039931205,4.07352085431319E-32));
#126511=DIRECTION('center_axis',(2.76197809063066E-32,-1.06237950525522E-32,
1.));
#126512=DIRECTION('ref_axis',(-0.742234123004274,0.670140661837555,2.76197809063065E-32));
#126513=DIRECTION('center_axis',(-2.76197809063066E-32,1.06237950525522E-32,
-1.));
#126514=DIRECTION('ref_axis',(0.742234123004278,-0.670140661837551,-2.76197809063066E-32));
#126515=DIRECTION('center_axis',(0.352280892409456,-0.935894317133723,-2.27209065223236E-32));
#126516=DIRECTION('ref_axis',(0.935894317133723,0.352280892409456,-2.35253017866368E-32));
#126517=DIRECTION('',(3.00213374770052E-32,-1.2976852986771E-32,1.));
#126518=DIRECTION('',(0.68489471598395,0.257801887816007,-0.68151112584885));
#126519=DIRECTION('center_axis',(-0.352276393100843,0.935896010708081,2.13514019485086E-6));
#126520=DIRECTION('ref_axis',(0.927975464140372,0.349295352096607,-0.129824092360271));
#126521=DIRECTION('',(5.63185375672478E-33,2.63971054609281E-32,-1.));
#126522=DIRECTION('center_axis',(-0.912596119838887,0.408862228696914,3.27031011275321E-32));
#126523=DIRECTION('ref_axis',(-0.408862228696914,-0.912596119838887,4.31965265863604E-34));
#126524=DIRECTION('center_axis',(0.912596119838905,-0.408862228696875,2.54164907767165E-14));
#126525=DIRECTION('ref_axis',(0.40579508981168,0.905750148631062,0.122257978633466));
#126526=DIRECTION('',(-0.299208548308696,-0.66784491460461,0.681511125848847));
#126527=DIRECTION('',(3.00213374770052E-32,-1.2976852986771E-32,1.));
#126528=DIRECTION('',(1.44456010278039E-32,-4.77424919954828E-32,1.));
#126529=DIRECTION('center_axis',(3.00213374770052E-32,-1.2976852986771E-32,
1.));
#126530=DIRECTION('ref_axis',(0.685141714967854,-0.72840979565826,-3.00213374770052E-32));
#126531=DIRECTION('center_axis',(-0.247421338625061,-0.232724328085158,
-0.94054349623518));
#126532=DIRECTION('ref_axis',(0.685182761455578,0.644318751359782,-0.339673269555142));
#126533=DIRECTION('center_axis',(-0.247421338625061,-0.232724328085158,
-0.94054349623518));
#126534=DIRECTION('ref_axis',(0.685182761455578,0.644318751359782,-0.339673269555142));
#126535=DIRECTION('center_axis',(0.300190303429413,0.670036229553501,-0.678923583927297));
#126536=DIRECTION('ref_axis',(0.51551595482926,0.484893925768568,0.706485089063615));
#126537=DIRECTION('center_axis',(-0.687141974287088,-0.258647780504989,
0.678923583927297));
#126538=DIRECTION('ref_axis',(-0.515515954829265,-0.484893925768564,-0.706485089063614));
#126539=DIRECTION('center_axis',(-0.375019506858782,0.926698478480159,-0.0242960790654331));
#126540=DIRECTION('ref_axis',(-0.645140812230435,-0.242077653382994,0.724701139868869));
#126541=DIRECTION('center_axis',(-3.00213374770052E-32,1.2976852986771E-32,
-1.));
#126542=DIRECTION('ref_axis',(-0.685141714967848,0.728409795658265,3.00213374770051E-32));
#126543=DIRECTION('center_axis',(-4.00818924926656E-35,-4.12526018083156E-32,
1.));
#126544=DIRECTION('ref_axis',(0.983786782322298,0.179342038931033,7.43775775555807E-33));
#126545=DIRECTION('center_axis',(3.00213374770052E-32,-1.2976852986771E-32,
1.));
#126546=DIRECTION('ref_axis',(0.685141714967848,-0.728409795658265,-3.00213374770051E-32));
#126547=DIRECTION('center_axis',(-0.299077797577255,-0.66755307397516,0.681854357192688));
#126548=DIRECTION('ref_axis',(-0.517575453416348,-0.486831088616092,-0.703641344136154));
#126549=DIRECTION('center_axis',(-0.299340976225778,-0.668140498776498,
0.681163162426516));
#126550=DIRECTION('ref_axis',(-0.517089918871244,-0.486374395182141,-0.704313824593084));
#126551=DIRECTION('center_axis',(0.685197846296135,0.257915989392372,-0.681163162426516));
#126552=DIRECTION('ref_axis',(0.517089918871247,0.486374395182137,0.704313824593084));
#126553=DIRECTION('center_axis',(0.68459542478528,0.25768923132411,-0.681854357192686));
#126554=DIRECTION('ref_axis',(0.517575453416338,0.486831088616102,0.703641344136154));
#126555=DIRECTION('center_axis',(3.00213374770052E-32,-1.2976852986771E-32,
1.));
#126556=DIRECTION('ref_axis',(0.685141714967854,-0.72840979565826,-3.00213374770052E-32));
#126557=DIRECTION('center_axis',(-4.00818924926656E-35,-4.12526018083156E-32,
1.));
#126558=DIRECTION('ref_axis',(0.239176321393792,0.970976151758906,4.00648791934816E-32));
#126559=DIRECTION('center_axis',(3.00213374770052E-32,-1.2976852986771E-32,
1.));
#126560=DIRECTION('ref_axis',(-0.685141714967843,0.72840979565827,3.0021337477005E-32));
#126561=DIRECTION('center_axis',(-3.00213374770052E-32,1.2976852986771E-32,
-1.));
#126562=DIRECTION('ref_axis',(0.685141714967852,-0.728409795658261,-3.00213374770052E-32));
#126563=DIRECTION('center_axis',(0.274824631535754,-0.961494369146922,-2.37760101267756E-32));
#126564=DIRECTION('ref_axis',(0.961494369146922,0.274824631535754,-2.67176538956511E-32));
#126565=DIRECTION('',(3.22231069999663E-32,-1.55178304703028E-32,1.));
#126566=DIRECTION('',(0.703629032489313,0.201118795696443,-0.681511125848849));
#126567=DIRECTION('center_axis',(-0.274820009156125,0.961495690350648,2.13514022130774E-6));
#126568=DIRECTION('ref_axis',(0.953358516276989,0.272494485408876,-0.129824092001024));
#126569=DIRECTION('',(4.40532634530388E-33,2.59873620878172E-32,-1.));
#126570=DIRECTION('center_axis',(-0.876233464203463,0.481886829255582,3.57128027962392E-32));
#126571=DIRECTION('ref_axis',(-0.481886829255582,-0.876233464203463,1.93064851106168E-33));
#126572=DIRECTION('center_axis',(0.876233464203449,-0.481886829255608,-1.7249630376986E-14));
#126573=DIRECTION('ref_axis',(0.478271885807456,0.86966027268176,0.122257978738674));
#126574=DIRECTION('',(-0.352648517057147,-0.641234441340787,0.681511125848848));
#126575=DIRECTION('',(3.22231069999663E-32,-1.55178304703028E-32,1.));
#126576=DIRECTION('',(1.3865475201236E-32,-4.88982225644841E-32,1.));
#126577=DIRECTION('center_axis',(3.22231069999663E-32,-1.55178304703028E-32,
1.));
#126578=DIRECTION('ref_axis',(0.623489801858739,-0.781831482468025,-3.22231069999663E-32));
#126579=DIRECTION('center_axis',(-0.265567257777731,-0.211782821036219,
-0.940543496235213));
#126580=DIRECTION('ref_axis',(0.735420832139579,0.586326077882361,-0.33967326955505));
#126581=DIRECTION('center_axis',(-0.265567257777731,-0.211782821036219,
-0.940543496235213));
#126582=DIRECTION('ref_axis',(0.735420832139579,0.586326077882361,-0.33967326955505));
#126583=DIRECTION('center_axis',(0.35380561798019,0.643338442713452,-0.678923583927297));
#126584=DIRECTION('ref_axis',(0.553323974502355,0.441261145096295,0.706485089063615));
#126585=DIRECTION('center_axis',(-0.70593776133287,-0.201778701333043,0.678923583927297));
#126586=DIRECTION('ref_axis',(-0.553323974502362,-0.441261145096289,-0.706485089063613));
#126587=DIRECTION('center_axis',(-0.298237131350729,0.954182537057364,-0.0242960790758392));
#126588=DIRECTION('ref_axis',(-0.662725964726312,-0.188687272070395,0.72470091005615));
#126589=DIRECTION('center_axis',(-3.22231069999663E-32,1.55178304703028E-32,
-1.));
#126590=DIRECTION('ref_axis',(-0.623489801858739,0.781831482468025,3.22231069999663E-32));
#126591=DIRECTION('center_axis',(-4.30215046728545E-35,-4.12492093150131E-32,
1.));
#126592=DIRECTION('ref_axis',(0.995131354063957,0.0985575373009913,4.10823253389977E-33));
#126593=DIRECTION('center_axis',(3.22231069999663E-32,-1.55178304703028E-32,
1.));
#126594=DIRECTION('ref_axis',(0.623489801858739,-0.781831482468025,-3.22231069999663E-32));
#126595=DIRECTION('center_axis',(-0.352494413667353,-0.640954229185404,
0.681854357192688));
#126596=DIRECTION('ref_axis',(-0.555534517033615,-0.443023993939942,-0.703641344136152));
#126597=DIRECTION('center_axis',(-0.352804597185329,-0.641518247876089,
0.681163162426516));
#126598=DIRECTION('ref_axis',(-0.55501337331005,-0.442608395688629,-0.704313824593083));
#126599=DIRECTION('center_axis',(0.703940454498133,0.201207809674652,-0.681163162426516));
#126600=DIRECTION('ref_axis',(0.555013373310052,0.442608395688626,0.704313824593084));
#126601=DIRECTION('center_axis',(0.703321554607476,0.201030909070899,-0.681854357192686));
#126602=DIRECTION('ref_axis',(0.555534517033603,0.443023993939952,0.703641344136155));
#126603=DIRECTION('center_axis',(3.22231069999663E-32,-1.55178304703028E-32,
1.));
#126604=DIRECTION('ref_axis',(0.623489801858739,-0.781831482468025,-3.22231069999663E-32));
#126605=DIRECTION('center_axis',(-4.30215046728545E-35,-4.12492093150131E-32,
1.));
#126606=DIRECTION('ref_axis',(0.317524052386177,0.948250218115588,3.91282320925602E-32));
#126607=DIRECTION('center_axis',(3.22231069999663E-32,-1.55178304703028E-32,
1.));
#126608=DIRECTION('ref_axis',(-0.623489801858734,0.781831482468029,3.22231069999662E-32));
#126609=DIRECTION('center_axis',(-3.22231069999663E-32,1.55178304703028E-32,
-1.));
#126610=DIRECTION('ref_axis',(0.623489801858742,-0.781831482468023,-3.22231069999663E-32));
#126611=DIRECTION('center_axis',(0.973302335538192,-0.229526825525689,6.39195957963004E-33));
#126612=DIRECTION('ref_axis',(0.229526825525689,0.973302335538192,2.07003539272685E-33));
#126613=DIRECTION('',(-6.69643783993806E-33,-5.47644091186761E-34,1.));
#126614=DIRECTION('',(0.167969510126485,0.712270193825419,-0.681511125848851));
#126615=DIRECTION('center_axis',(-0.973301232076518,0.229531504664986,2.13514020350011E-6));
#126616=DIRECTION('ref_axis',(0.227588719328633,0.965064287994901,-0.129824092029358));
#126617=DIRECTION('',(1.54403351517636E-32,3.76259056661216E-32,-1.));
#126618=DIRECTION('center_axis',(-0.848320692261111,-0.529482769390685,
-5.97069489410176E-33));
#126619=DIRECTION('ref_axis',(0.529482769390685,-0.848320692261111,3.08107063799472E-33));
#126620=DIRECTION('center_axis',(0.848320692261124,0.529482769390664,-1.61810692031897E-14));
#126621=DIRECTION('ref_axis',(0.525510778145861,-0.84195689242242,-0.122257978696332));
#126622=DIRECTION('',(0.387479594994073,-0.620807658463926,0.681511125848849));
#126623=DIRECTION('',(-6.69643783993806E-33,-5.47644091186761E-34,1.));
#126624=DIRECTION('',(1.34743764138189E-32,-3.28646902736502E-32,1.));
#126625=DIRECTION('center_axis',(-6.69643783993806E-33,-5.47644091186761E-34,
1.));
#126626=DIRECTION('ref_axis',(0.986712473391289,0.162476136260207,6.69643783993806E-33));
#126627=DIRECTION('center_axis',(0.0551888008202831,-0.335159854328824,
-0.940543496235182));
#126628=DIRECTION('ref_axis',(-0.152698253836419,0.928065360427289,-0.339673269555134));
#126629=DIRECTION('center_axis',(0.0551888008202831,-0.335159854328824,
-0.940543496235182));
#126630=DIRECTION('ref_axis',(-0.152698253836419,0.928065360427289,-0.339673269555134));
#126631=DIRECTION('center_axis',(-0.388750982722458,0.622844636020603,-0.678923583927297));
#126632=DIRECTION('ref_axis',(-0.11498889913398,0.698323973530004,0.706485089063614));
#126633=DIRECTION('center_axis',(-0.16852064721002,-0.714607275817445,0.678923583927297));
#126634=DIRECTION('ref_axis',(0.114988899133974,-0.698323973530004,-0.706485089063614));
#126635=DIRECTION('center_axis',(-0.978350395317852,0.205524218823469,-0.02429607907475));
#126636=DIRECTION('ref_axis',(0.15885123442695,0.670503884894633,-0.724700507563116));
#126637=DIRECTION('center_axis',(6.69643783993806E-33,5.47644091186761E-34,
-1.));
#126638=DIRECTION('ref_axis',(-0.98671247339129,-0.162476136260201,-6.69643783993806E-33));
#126639=DIRECTION('center_axis',(8.94050445919518E-36,-4.12691962127155E-32,
1.));
#126640=DIRECTION('ref_axis',(0.399783842199988,0.916609447647042,3.78241608761507E-32));
#126641=DIRECTION('center_axis',(-6.69643783993806E-33,-5.47644091186761E-34,
1.));
#126642=DIRECTION('ref_axis',(0.98671247339129,0.162476136260201,6.69643783993806E-33));
#126643=DIRECTION('center_axis',(0.387310270819507,-0.620536372580259,0.681854357192688));
#126644=DIRECTION('ref_axis',(0.115448282540205,-0.701113794530378,-0.703641344136153));
#126645=DIRECTION('center_axis',(0.387651091149399,-0.621082424227082,0.681163162426516));
#126646=DIRECTION('ref_axis',(0.115339981172796,-0.700456083726969,-0.704313824593084));
#126647=DIRECTION('center_axis',(0.168043852428818,0.712585440360656,-0.681163162426516));
#126648=DIRECTION('ref_axis',(-0.115339981172794,0.700456083726969,0.704313824593084));
#126649=DIRECTION('center_axis',(0.16789610936159,0.711958939854392,-0.681854357192686));
#126650=DIRECTION('ref_axis',(-0.115448282540218,0.701113794530375,0.703641344136154));
#126651=DIRECTION('center_axis',(-6.69643783993806E-33,-5.47644091186761E-34,
1.));
#126652=DIRECTION('ref_axis',(0.98671247339129,0.162476136260201,6.69643783993806E-33));
#126653=DIRECTION('center_axis',(8.94050445919518E-36,-4.12691962127155E-32,
1.));
#126654=DIRECTION('ref_axis',(-0.67257303458172,0.740030751491812,3.05464874289737E-32));
#126655=DIRECTION('center_axis',(-6.69643783993806E-33,-5.47644091186761E-34,
1.));
#126656=DIRECTION('ref_axis',(-0.98671247339129,-0.162476136260201,-6.69643783993806E-33));
#126657=DIRECTION('center_axis',(6.69643783993806E-33,5.47644091186761E-34,
-1.));
#126658=DIRECTION('ref_axis',(0.986712473391289,0.162476136260206,6.69643783993805E-33));
#126659=DIRECTION('center_axis',(0.988772319411911,-0.149429917903982,9.6931456824374E-33));
#126660=DIRECTION('ref_axis',(0.149429917903982,0.988772319411911,2.70762924361271E-33));
#126661=DIRECTION('',(-9.98891495440864E-33,-1.2287828837565E-33,1.));
#126662=DIRECTION('',(0.109353972247411,0.72359124794178,-0.681511125848853));
#126663=DIRECTION('center_axis',(-0.988771601015213,0.149434671416156,2.1351401804249E-6));
#126664=DIRECTION('ref_axis',(0.148169737941467,0.980403709598452,-0.129824092386398));
#126665=DIRECTION('',(1.56814951331063E-32,3.8896378407338E-32,-1.));
#126666=DIRECTION('center_axis',(-0.802340213955593,-0.596866970999144,
-8.74792807954779E-33));
#126667=DIRECTION('ref_axis',(0.596866970999144,-0.802340213955593,4.97615149054778E-33));
#126668=DIRECTION('center_axis',(0.802340213955602,0.596866970999133,-1.20340341715621E-14));
#126669=DIRECTION('ref_axis',(0.59238948746369,-0.79632134329872,-0.122257978673905));
#126670=DIRECTION('',(0.436791876068471,-0.587158788016343,0.681511125848849));
#126671=DIRECTION('',(-9.98891495440864E-33,-1.2287828837565E-33,1.));
#126672=DIRECTION('',(1.2748921859584E-32,-3.17941881426318E-32,1.));
#126673=DIRECTION('center_axis',(-9.98891495440864E-33,-1.2287828837565E-33,
1.));
#126674=DIRECTION('ref_axis',(0.970185955574064,0.242361737093215,9.98891495440864E-33));
#126675=DIRECTION('center_axis',(0.0823238042383934,-0.329546237947607,
-0.940543496235181));
#126676=DIRECTION('ref_axis',(-0.227836105607519,0.912530974231188,-0.339673269555138));
#126677=DIRECTION('center_axis',(0.0823238042383934,-0.329546237947607,
-0.940543496235181));
#126678=DIRECTION('ref_axis',(-0.227836105607519,0.912530974231188,-0.339673269555138));
#126679=DIRECTION('center_axis',(-0.438225065940319,0.589085357795385,-0.678923583927297));
#126680=DIRECTION('ref_axis',(-0.1715261698242,0.686627695331478,0.706485089063614));
#126681=DIRECTION('center_axis',(-0.109712781589005,-0.725965476275089,
0.678923583927297));
#126682=DIRECTION('ref_axis',(0.17152616982419,-0.68662769533148,-0.706485089063615));
#126683=DIRECTION('center_axis',(-0.991847146913457,0.125095714160269,-0.0242960790739686));
#126684=DIRECTION('ref_axis',(0.103670414118919,0.681221032856078,-0.724700179129901));
#126685=DIRECTION('center_axis',(9.98891495440864E-33,1.2287828837565E-33,
-1.));
#126686=DIRECTION('ref_axis',(-0.970185955574064,-0.242361737093213,-9.98891495440864E-33));
#126687=DIRECTION('center_axis',(1.3336335052612E-35,-4.12682868151287E-32,
1.));
#126688=DIRECTION('ref_axis',(0.323741415074756,0.946145599876359,3.90414904605877E-32));
#126689=DIRECTION('center_axis',(-9.98891495440864E-33,-1.2287828837565E-33,
1.));
#126690=DIRECTION('ref_axis',(0.970185955574064,0.242361737093213,9.98891495440864E-33));
#126691=DIRECTION('center_axis',(0.436601002988114,-0.586902206306229,0.681854357192688));
#126692=DIRECTION('ref_axis',(0.172211420981002,-0.689370789420303,-0.703641344136154));
#126693=DIRECTION('center_axis',(0.436985197544986,-0.587418660990335,0.681163162426516));
#126694=DIRECTION('ref_axis',(0.17204987044109,-0.6887240946622,-0.704313824593084));
#126695=DIRECTION('center_axis',(0.109402371662638,0.723911505107978,-0.681163162426516));
#126696=DIRECTION('ref_axis',(-0.172049870441086,0.688724094662201,0.704313824593084));
#126697=DIRECTION('center_axis',(0.109306185805685,0.723275046798907,-0.681854357192686));
#126698=DIRECTION('ref_axis',(-0.172211420981012,0.689370789420299,0.703641344136154));
#126699=DIRECTION('center_axis',(-9.98891495440864E-33,-1.2287828837565E-33,
1.));
#126700=DIRECTION('ref_axis',(0.970185955574064,0.242361737093213,9.98891495440864E-33));
#126701=DIRECTION('center_axis',(1.3336335052612E-35,-4.12682868151287E-32,
1.));
#126702=DIRECTION('ref_axis',(-0.730654479649412,0.682747414032633,2.81855603575344E-32));
#126703=DIRECTION('center_axis',(-9.98891495440864E-33,-1.2287828837565E-33,
1.));
#126704=DIRECTION('ref_axis',(-0.970185955574069,-0.242361737093194,-9.98891495440866E-33));
#126705=DIRECTION('center_axis',(9.98891495440864E-33,1.2287828837565E-33,
-1.));
#126706=DIRECTION('ref_axis',(0.970185955574064,0.242361737093213,9.98891495440864E-33));
#126707=DIRECTION('center_axis',(0.997662186635892,-0.0683385788328237,
1.30353171787961E-32));
#126708=DIRECTION('ref_axis',(0.0683385788328237,0.997662186635892,3.07402423946217E-33));
#126709=DIRECTION('',(-1.32149174879126E-32,-2.17602269387955E-33,1.));
#126710=DIRECTION('',(0.0500107017251656,0.730096921687246,-0.681511125848848));
#126711=DIRECTION('center_axis',(-0.99766185808497,0.0683433750840998,2.13514018679782E-6));
#126712=DIRECTION('ref_axis',(0.0677647114083837,0.989218706359218,-0.129824092050492));
#126713=DIRECTION('',(1.58182973516028E-32,4.01822805326141E-32,-1.));
#126714=DIRECTION('center_axis',(-0.751020293903019,-0.660279121391721,
-1.13614535681195E-32));
#126715=DIRECTION('ref_axis',(0.660279121391721,-0.751020293903019,7.09129690508596E-33));
#126716=DIRECTION('center_axis',(0.751020293903004,0.660279121391738,4.604989820407E-15));
#126717=DIRECTION('ref_axis',(0.655325942479862,-0.745386407018453,-0.122257978655797));
#126718=DIRECTION('',(0.483197379273218,-0.549602472708896,0.681511125848846));
#126719=DIRECTION('',(-1.32149174879126E-32,-2.17602269387955E-33,1.));
#126720=DIRECTION('',(1.19386253337975E-32,-3.07863793001058E-32,1.));
#126721=DIRECTION('center_axis',(-1.32149174879126E-32,-2.17602269387955E-33,
1.));
#126722=DIRECTION('ref_axis',(0.94720301029191,0.320634460552734,1.32149174879126E-32));
#126723=DIRECTION('center_axis',(0.108910956321738,-0.321739545724076,-0.940543496235208));
#126724=DIRECTION('ref_axis',(-0.301457745685325,0.890923844958758,-0.339673269555061));
#126725=DIRECTION('center_axis',(0.108910956321738,-0.321739545724076,-0.940543496235208));
#126726=DIRECTION('ref_axis',(-0.301457745685325,0.890923844958758,-0.339673269555061));
#126727=DIRECTION('center_axis',(-0.484782833646393,0.551405813706283,-0.678923583927297));
#126728=DIRECTION('ref_axis',(-0.226921962154062,0.670362023106118,0.706485089063614));
#126729=DIRECTION('center_axis',(-0.05017479550785,-0.732492496263996,0.678923583927297));
#126730=DIRECTION('ref_axis',(0.226921962154054,-0.670362023106121,-0.706485089063614));
#126731=DIRECTION('center_axis',(-0.998743319389926,0.0438347181477059,
-0.0242960790849923));
#126732=DIRECTION('ref_axis',(0.0477996139550044,0.687404086140894,-0.724700503147718));
#126733=DIRECTION('center_axis',(1.32149174879126E-32,2.17602269387955E-33,
-1.));
#126734=DIRECTION('ref_axis',(-0.947203010291908,-0.320634460552743,-1.32149174879126E-32));
#126735=DIRECTION('center_axis',(1.76434145365967E-35,-4.1267022142485E-32,
1.));
#126736=DIRECTION('ref_axis',(0.245544542245741,0.969385309241547,3.99993127769245E-32));
#126737=DIRECTION('center_axis',(-1.32149174879126E-32,-2.17602269387955E-33,
1.));
#126738=DIRECTION('ref_axis',(0.947203010291908,0.320634460552741,1.32149174879126E-32));
#126739=DIRECTION('center_axis',(0.48298622751593,-0.549362302681278,0.681854357192688));
#126740=DIRECTION('ref_axis',(0.227828520828051,-0.673040135444811,-0.703641344136153));
#126741=DIRECTION('center_axis',(0.483411239548394,-0.549845723481955,0.681163162426516));
#126742=DIRECTION('ref_axis',(0.227614796207828,-0.672408760378932,-0.704313824593084));
#126743=DIRECTION('center_axis',(0.0500328361631631,0.730420058225798,-0.681163162426516));
#126744=DIRECTION('ref_axis',(-0.227614796207826,0.672408760378933,0.704313824593083));
#126745=DIRECTION('center_axis',(0.0499888476174943,0.729777877638959,-0.681854357192686));
#126746=DIRECTION('ref_axis',(-0.227828520828061,0.673040135444807,0.703641344136154));
#126747=DIRECTION('center_axis',(-1.32149174879126E-32,-2.17602269387955E-33,
1.));
#126748=DIRECTION('ref_axis',(0.947203010291908,0.320634460552741,1.32149174879126E-32));
#126749=DIRECTION('center_axis',(1.76434145365967E-35,-4.1267022142485E-32,
1.));
#126750=DIRECTION('ref_axis',(-0.783873539704543,0.620920505178457,2.56373704417276E-32));
#126751=DIRECTION('center_axis',(-1.32149174879126E-32,-2.17602269387955E-33,
1.));
#126752=DIRECTION('ref_axis',(-0.947203010291908,-0.320634460552741,-1.32149174879126E-32));
#126753=DIRECTION('center_axis',(1.32149174879126E-32,2.17602269387955E-33,
-1.));
#126754=DIRECTION('ref_axis',(0.94720301029191,0.320634460552736,1.32149174879126E-32));
#126755=DIRECTION('center_axis',(0.999912776610487,0.0132075422053949,1.63962324688173E-32));
#126756=DIRECTION('ref_axis',(-0.0132075422053949,0.999912776610487,3.1667820820288E-33));
#126757=DIRECTION('',(-1.63529769258424E-32,-3.38305979690313E-33,1.));
#126758=DIRECTION('',(-0.00966538176587747,0.731743920876393,-0.681511125848848));
#126759=DIRECTION('center_axis',(-0.999912840091796,-0.013202735133283,
2.13514020082165E-6));
#126760=DIRECTION('ref_axis',(0.0130912781053972,-0.991450615801791,0.129824092000736));
#126761=DIRECTION('',(1.58498314110597E-32,4.14750545754651E-32,-1.));
#126762=DIRECTION('center_axis',(-0.694702457704146,-0.719297223169824,
-1.37938787788918E-32));
#126763=DIRECTION('ref_axis',(0.719297223169824,-0.694702457704146,9.41243093784996E-33));
#126764=DIRECTION('center_axis',(0.694702457704154,0.719297223169816,-1.24411050949079E-14));
#126765=DIRECTION('ref_axis',(0.71390131146342,-0.68949104717282,-0.122257978714422));
#126766=DIRECTION('',(0.52638728364086,-0.508388643623588,0.681511125848848));
#126767=DIRECTION('',(-1.63529769258424E-32,-3.38305979690313E-33,1.));
#126768=DIRECTION('',(1.10488792261492E-32,-2.98479705476425E-32,1.));
#126769=DIRECTION('center_axis',(-1.63529769258424E-32,-3.38305979690313E-33,
1.));
#126770=DIRECTION('ref_axis',(0.917916585253758,0.396773414578245,1.63529769258424E-32));
#126771=DIRECTION('center_axis',(0.134773323959819,-0.311791729907097,-0.940543496235215));
#126772=DIRECTION('ref_axis',(-0.373073234202291,0.863387764490341,-0.339673269555044));
#126773=DIRECTION('center_axis',(0.134773323959819,-0.311791729907097,-0.940543496235215));
#126774=DIRECTION('ref_axis',(-0.373073234202291,0.863387764490341,-0.339673269555044));
#126775=DIRECTION('center_axis',(-0.528114451578088,0.51005675490252,-0.678923583927297));
#126776=DIRECTION('ref_axis',(-0.280807626265276,0.649635202218937,0.706485089063614));
#126777=DIRECTION('center_axis',(0.00969709555915143,-0.73414489954302,
0.678923583927297));
#126778=DIRECTION('ref_axis',(0.280807626265272,-0.649635202218938,-0.706485089063614));
#126779=DIRECTION('center_axis',(-0.998993019856255,-0.0377179906659659,
-0.024296079078787));
#126780=DIRECTION('ref_axis',(-0.0083891685448101,0.689011582292177,-0.724701774054927));
#126781=DIRECTION('center_axis',(1.63529769258424E-32,3.38305979690313E-33,
-1.));
#126782=DIRECTION('ref_axis',(-0.917916585253758,-0.396773414578245,-1.63529769258424E-32));
#126783=DIRECTION('center_axis',(2.18330800078025E-35,-4.12654106109723E-32,
1.));
#126784=DIRECTION('ref_axis',(0.16571361100008,0.986173919311048,4.06912536756749E-32));
#126785=DIRECTION('center_axis',(-1.63529769258424E-32,-3.38305979690313E-33,
1.));
#126786=DIRECTION('ref_axis',(0.917916585253758,0.396773414578245,1.63529769258424E-32));
#126787=DIRECTION('center_axis',(0.526157258386746,-0.508166483570384,0.681854357192688));
#126788=DIRECTION('ref_axis',(0.281929459458051,-0.65223051041174,-0.703641344136154));
#126789=DIRECTION('center_axis',(0.526620259509848,-0.50861365340196,0.681163162426515));
#126790=DIRECTION('ref_axis',(0.281664983059597,-0.651618656734981,-0.704313824593083));
#126791=DIRECTION('center_axis',(-0.00966965960614047,0.732067786366952,
-0.681163162426516));
#126792=DIRECTION('ref_axis',(-0.281664983059596,0.65161865673498,0.704313824593084));
#126793=DIRECTION('center_axis',(-0.00966115810401136,0.731424157108198,
-0.681854357192686));
#126794=DIRECTION('ref_axis',(-0.281929459458062,0.652230510411734,0.703641344136154));
#126795=DIRECTION('center_axis',(-1.63529769258424E-32,-3.38305979690313E-33,
1.));
#126796=DIRECTION('ref_axis',(0.917916585253758,0.396773414578245,1.63529769258424E-32));
#126797=DIRECTION('center_axis',(2.18330800078025E-35,-4.12654106109723E-32,
1.));
#126798=DIRECTION('ref_axis',(-0.831876050682975,0.554961472806984,2.29188754650213E-32));
#126799=DIRECTION('center_axis',(-1.63529769258424E-32,-3.38305979690313E-33,
1.));
#126800=DIRECTION('ref_axis',(-0.917916585253758,-0.396773414578245,-1.63529769258424E-32));
#126801=DIRECTION('center_axis',(1.63529769258424E-32,3.38305979690313E-33,
-1.));
#126802=DIRECTION('ref_axis',(0.917916585253759,0.396773414578243,1.63529769258424E-32));
#126803=DIRECTION('center_axis',(0.995509112030734,0.0946657692293274,1.97535252157579E-32));
#126804=DIRECTION('ref_axis',(-0.0946657692293274,0.995509112030734,2.98528548317427E-33));
#126805=DIRECTION('',(-1.9382210000382E-32,-4.8418615600537E-33,1.));
#126806=DIRECTION('',(-0.0692771437359437,0.72852128500135,-0.681511125848853));
#126807=DIRECTION('center_axis',(-0.995509567121819,-0.0946609833266599,
2.13514020730258E-6));
#126808=DIRECTION('ref_axis',(0.0938601473240115,-0.987084584970317,0.129824091979465));
#126809=DIRECTION('',(1.57758874575141E-32,4.27660973379285E-32,-1.));
#126810=DIRECTION('center_axis',(-0.63376149126709,-0.773528520603419,-1.60290163234089E-32));
#126811=DIRECTION('ref_axis',(0.773528520603419,-0.63376149126709,1.19241068248119E-32));
#126812=DIRECTION('center_axis',(0.633761491266992,0.773528520603499,5.86436548952487E-14));
#126813=DIRECTION('ref_axis',(0.76772578501665,-0.629007238177413,-0.122257978639401));
#126814=DIRECTION('',(0.566074167483661,-0.463791571993187,0.681511125848851));
#126815=DIRECTION('',(-1.9382210000382E-32,-4.8418615600537E-33,1.));
#126816=DIRECTION('',(1.00856046501876E-32,-2.89852068406629E-32,1.));
#126817=DIRECTION('center_axis',(-1.9382210000382E-32,-4.8418615600537E-33,
1.));
#126818=DIRECTION('ref_axis',(0.882521576786319,0.47027190699274,1.9382210000382E-32));
#126819=DIRECTION('center_axis',(0.159738797363031,-0.2997689915697,-0.940543496235181));
#126820=DIRECTION('ref_axis',(-0.442205981897974,0.830105980898446,-0.339673269555138));
#126821=DIRECTION('center_axis',(0.159738797363031,-0.2997689915697,-0.940543496235181));
#126822=DIRECTION('ref_axis',(-0.442205981897974,0.830105980898446,-0.339673269555138));
#126823=DIRECTION('center_axis',(-0.567931554967282,0.465313352548322,-0.678923583927297));
#126824=DIRECTION('ref_axis',(-0.332824561953696,0.62458516624325,0.706485089063614));
#126825=DIRECTION('center_axis',(0.0695044540551147,-0.730911689640968,
0.678923583927297));
#126826=DIRECTION('ref_axis',(0.332824561953692,-0.624585166243252,-0.706485089063614));
#126827=DIRECTION('center_axis',(-0.9925945865974,-0.119019692483191,-0.0242960790816824));
#126828=DIRECTION('ref_axis',(-0.0645222095089911,0.686035958596192,-0.724701005928018));
#126829=DIRECTION('center_axis',(1.9382210000382E-32,4.8418615600537E-33,
-1.));
#126830=DIRECTION('ref_axis',(-0.882521576786316,-0.470271906992746,-1.9382210000382E-32));
#126831=DIRECTION('center_axis',(2.58774499337527E-35,-4.12634629450669E-32,
1.));
#126832=DIRECTION('ref_axis',(0.0847798830140602,0.996399704654775,4.11127084043198E-32));
#126833=DIRECTION('center_axis',(-1.9382210000382E-32,-4.8418615600537E-33,
1.));
#126834=DIRECTION('ref_axis',(0.882521576786316,0.470271906992746,1.9382210000382E-32));
#126835=DIRECTION('center_axis',(0.565826799512835,-0.463588900352897,0.681854357192688));
#126836=DIRECTION('ref_axis',(0.334154204050439,-0.627080398942342,-0.703641344136152));
#126837=DIRECTION('center_axis',(0.56632470853049,-0.463996843373922,0.681163162426516));
#126838=DIRECTION('ref_axis',(0.333840735920563,-0.626492138439965,-0.704313824593083));
#126839=DIRECTION('center_axis',(-0.0693078053861466,0.728843724172517,
-0.681163162426516));
#126840=DIRECTION('ref_axis',(-0.333840735920559,0.626492138439966,0.704313824593084));
#126841=DIRECTION('center_axis',(-0.0692468704123135,0.728202929488373,
-0.681854357192686));
#126842=DIRECTION('ref_axis',(-0.334154204050452,0.627080398942332,0.703641344136155));
#126843=DIRECTION('center_axis',(-1.9382210000382E-32,-4.8418615600537E-33,
1.));
#126844=DIRECTION('ref_axis',(0.882521576786316,0.470271906992746,1.9382210000382E-32));
#126845=DIRECTION('center_axis',(2.58774499337527E-35,-4.12634629450669E-32,
1.));
#126846=DIRECTION('ref_axis',(-0.874342563793985,0.485309263396199,2.00481665629663E-32));
#126847=DIRECTION('center_axis',(-1.9382210000382E-32,-4.8418615600537E-33,
1.));
#126848=DIRECTION('ref_axis',(-0.882521576786316,-0.470271906992746,-1.9382210000382E-32));
#126849=DIRECTION('center_axis',(1.9382210000382E-32,4.8418615600537E-33,
-1.));
#126850=DIRECTION('ref_axis',(0.882521576786321,0.470271906992738,1.9382210000382E-32));
#126851=DIRECTION('center_axis',(0.984480498557858,0.175494011177791,2.30848531903014E-32));
#126852=DIRECTION('ref_axis',(-0.175494011177791,0.984480498557858,2.53074227281913E-33));
#126853=DIRECTION('',(-2.22824576652086E-32,-6.54271989828285E-33,1.));
#126854=DIRECTION('',(-0.128427877744372,0.720450460172186,-0.681511125848846));
#126855=DIRECTION('center_axis',(-0.984481342230153,-0.175489278294025,
2.13514017808401E-6));
#126856=DIRECTION('ref_axis',(0.174004392741512,-0.976149669043933,0.129824092263641));
#126857=DIRECTION('',(1.55969575757769E-32,4.40468171434272E-32,-1.));
#126858=DIRECTION('center_axis',(-0.568602946668937,-0.822612113355622,
-1.80519917300838E-32));
#126859=DIRECTION('ref_axis',(0.822612113355622,-0.568602946668937,1.46096097773413E-32));
#126860=DIRECTION('center_axis',(0.568602946668932,0.822612113355625,-5.82620259045788E-15));
#126861=DIRECTION('ref_axis',(0.816441170119489,-0.564337489777616,-0.122257978739302));
#126862=DIRECTION('',(0.601993921137532,-0.416108043971394,0.681511125848844));
#126863=DIRECTION('',(-2.22824576652086E-32,-6.54271989828285E-33,1.));
#126864=DIRECTION('',(9.0552120392866E-33,-2.8203829729291E-32,1.));
#126865=DIRECTION('center_axis',(-2.22824576652086E-32,-6.54271989828285E-33,
1.));
#126866=DIRECTION('ref_axis',(0.841253532831182,0.540640817455597,2.22824576652086E-32));
#126867=DIRECTION('center_axis',(0.183641235424755,-0.285751340051653,-0.940543496235211));
#126868=DIRECTION('ref_axis',(-0.508395921744393,0.791299978960854,-0.339673269555054));
#126869=DIRECTION('center_axis',(0.183641235424755,-0.285751340051653,-0.940543496235211));
#126870=DIRECTION('ref_axis',(-0.508395921744393,0.791299978960854,-0.339673269555054));
#126871=DIRECTION('center_axis',(-0.60396916756028,0.417473366604215,-0.678923583927297));
#126872=DIRECTION('ref_axis',(-0.382626605094497,0.595378619035516,0.706485089063613));
#126873=DIRECTION('center_axis',(0.128849271876769,-0.722814383036296,0.678923583927297));
#126874=DIRECTION('ref_axis',(0.382626605094492,-0.595378619035518,-0.706485089063614));
#126875=DIRECTION('center_axis',(-0.979590600131391,-0.199529337881564,
-0.0242960790821469));
#126876=DIRECTION('ref_axis',(-0.120225842285555,0.678494183971453,-0.724700896345272));
#126877=DIRECTION('center_axis',(2.22824576652086E-32,6.54271989828285E-33,
-1.));
#126878=DIRECTION('ref_axis',(-0.841253532831175,-0.540640817455607,-2.22824576652086E-32));
#126879=DIRECTION('center_axis',(2.97496096998759E-35,-4.1261192106164E-32,
1.));
#126880=DIRECTION('ref_axis',(0.00328195889423764,0.999994614358406,4.12608722511754E-32));
#126881=DIRECTION('center_axis',(-2.22824576652086E-32,-6.54271989828285E-33,
1.));
#126882=DIRECTION('ref_axis',(0.841253532831175,0.540640817455607,2.22824576652086E-32));
#126883=DIRECTION('center_axis',(0.601730856643017,-0.415926209490346,0.681854357192688));
#126884=DIRECTION('ref_axis',(0.384155207546441,-0.597757170878961,-0.703641344136152));
#126885=DIRECTION('center_axis',(0.602260360052862,-0.416292210907321,0.681163162426516));
#126886=DIRECTION('ref_axis',(0.383794833763824,-0.597196418327555,-0.704313824593085));
#126887=DIRECTION('center_axis',(-0.128484719156291,0.720769327244464,-0.681163162426516));
#126888=DIRECTION('ref_axis',(-0.38379483376382,0.59719641832756,0.704313824593083));
#126889=DIRECTION('center_axis',(-0.128371756222951,0.72013563151783,-0.681854357192686));
#126890=DIRECTION('ref_axis',(-0.384155207546449,0.597757170878953,0.703641344136155));
#126891=DIRECTION('center_axis',(-2.22824576652086E-32,-6.54271989828285E-33,
1.));
#126892=DIRECTION('ref_axis',(0.841253532831175,0.540640817455607,2.22824576652086E-32));
#126893=DIRECTION('center_axis',(2.97496096998759E-35,-4.1261192106164E-32,
1.));
#126894=DIRECTION('ref_axis',(-0.91099047139932,0.412427400907898,1.70443478296712E-32));
#126895=DIRECTION('center_axis',(-2.22824576652086E-32,-6.54271989828285E-33,
1.));
#126896=DIRECTION('ref_axis',(-0.841253532831175,-0.540640817455607,-2.22824576652086E-32));
#126897=DIRECTION('center_axis',(2.22824576652086E-32,6.54271989828285E-33,
-1.));
#126898=DIRECTION('ref_axis',(0.841253532831181,0.540640817455599,2.22824576652086E-32));
#126899=DIRECTION('center_axis',(0.966900329794929,0.255154369436341,2.63680469544076E-32));
#126900=DIRECTION('ref_axis',(-0.255154369436341,0.966900329794929,1.80617736103395E-33));
#126901=DIRECTION('',(-2.503441925062E-32,-8.47431587997155E-33,1.));
#126902=DIRECTION('',(-0.186723945415519,0.707585156396526,-0.681511125848849));
#126903=DIRECTION('center_axis',(-0.966901556433968,-0.255149721067868,
2.13514022410592E-6));
#126904=DIRECTION('ref_axis',(0.252990667638338,-0.958718638164101,0.129824092235145));
#126905=DIRECTION('',(1.53142325146899E-32,4.53086910129595E-32,-1.));
#126906=DIRECTION('center_axis',(-0.499660443273585,-0.866221358214888,
-1.98493424313525E-32));
#126907=DIRECTION('ref_axis',(0.866221358214888,-0.499660443273585,1.7451068216366E-32));
#126908=DIRECTION('center_axis',(0.499660443273578,0.866221358214892,8.62481518849798E-15));
#126909=DIRECTION('ref_axis',(0.859723273961663,-0.495912168508003,-0.122257978612151));
#126910=DIRECTION('',(0.633907504568221,-0.365655385569965,0.681511125848853));
#126911=DIRECTION('',(-2.503441925062E-32,-8.47431587997155E-33,1.));
#126912=DIRECTION('',(7.964558486269E-33,-2.75090391492849E-32,1.));
#126913=DIRECTION('center_axis',(-2.503441925062E-32,-8.47431587997155E-33,
1.));
#126914=DIRECTION('ref_axis',(0.794387085412114,0.607411852477745,2.50344192506201E-32));
#126915=DIRECTION('center_axis',(0.206321571363439,-0.269832060511291,-0.94054349623521));
#126916=DIRECTION('ref_axis',(-0.571202570610379,0.7472280062189,-0.339673269555058));
#126917=DIRECTION('center_axis',(0.206321571363439,-0.269832060511291,-0.94054349623521));
#126918=DIRECTION('ref_axis',(-0.571202570610379,0.7472280062189,-0.339673269555058));
#126919=DIRECTION('center_axis',(-0.635987464991062,0.366855164283613,-0.678923583927297));
#126920=DIRECTION('ref_axis',(-0.429882331307342,0.562209925348658,0.706485089063613));
#126921=DIRECTION('center_axis',(0.187336619052717,-0.709906865968496,0.678923583927297));
#126922=DIRECTION('ref_axis',(0.429882331307337,-0.56220992534866,-0.706485089063615));
#126923=DIRECTION('center_axis',(-0.960067599843407,-0.278711148453534,
-0.0242960790793859));
#126924=DIRECTION('ref_axis',(-0.175129429493246,0.666437199283665,-0.724700726049254));
#126925=DIRECTION('center_axis',(2.503441925062E-32,8.47431587997155E-33,
-1.));
#126926=DIRECTION('ref_axis',(-0.79438708541211,-0.607411852477751,-2.503441925062E-32));
#126927=DIRECTION('center_axis',(3.34237907217807E-35,-4.1258613206322E-32,
1.));
#126928=DIRECTION('ref_axis',(-0.0782378061205037,0.996934724890978,4.11347592102862E-32));
#126929=DIRECTION('center_axis',(-2.503441925062E-32,-8.47431587997155E-33,
1.));
#126930=DIRECTION('ref_axis',(0.79438708541211,0.607411852477751,2.503441925062E-32));
#126931=DIRECTION('center_axis',(0.633630494200843,-0.365495598326631,0.681854357192688));
#126932=DIRECTION('ref_axis',(0.431599721517369,-0.564455967466372,-0.703641344136153));
#126933=DIRECTION('center_axis',(0.634188068245048,-0.365817222460512,0.681163162426516));
#126934=DIRECTION('ref_axis',(0.431194840310069,-0.563926454581656,-0.704313824593084));
#126935=DIRECTION('center_axis',(-0.186806588318937,0.707898329362167,-0.681163162426516));
#126936=DIRECTION('ref_axis',(-0.431194840310065,0.56392645458166,0.704313824593084));
#126937=DIRECTION('center_axis',(-0.186642349175774,0.707275949733551,-0.681854357192686));
#126938=DIRECTION('ref_axis',(-0.431599721517378,0.564455967466363,0.703641344136155));
#126939=DIRECTION('center_axis',(-2.503441925062E-32,-8.47431587997155E-33,
1.));
#126940=DIRECTION('ref_axis',(0.79438708541211,0.607411852477751,2.503441925062E-32));
#126941=DIRECTION('center_axis',(3.34237907217807E-35,-4.1258613206322E-32,
1.));
#126942=DIRECTION('ref_axis',(-0.941575887720347,0.336800902112274,1.39274091832105E-32));
#126943=DIRECTION('center_axis',(-2.503441925062E-32,-8.47431587997155E-33,
1.));
#126944=DIRECTION('ref_axis',(-0.794387085412093,-0.607411852477773,-2.50344192506198E-32));
#126945=DIRECTION('center_axis',(2.503441925062E-32,8.47431587997155E-33,
-1.));
#126946=DIRECTION('ref_axis',(0.794387085412112,0.607411852477749,2.503441925062E-32));
#126947=DIRECTION('center_axis',(0.942885598864541,0.333116717463799,2.95812573952651E-32));
#126948=DIRECTION('ref_axis',(-0.333116717463799,0.942885598864541,8.16412607761849E-34));
#126949=DIRECTION('',(-2.7619780906307E-32,-1.06237950525526E-32,1.));
#126950=DIRECTION('',(-0.243777396037203,0.690010990148381,-0.681511125848853));
#126951=DIRECTION('center_axis',(-0.942887200307189,-0.333112184544956,
2.13514018502994E-6));
#126952=DIRECTION('ref_axis',(0.330293331385506,-0.934907492930652,0.12982409215699));
#126953=DIRECTION('',(1.4929593762888E-32,4.65433213841183E-32,-1.));
#126954=DIRECTION('center_axis',(-0.427392782066418,-0.904066042851698,
-2.14091073548401E-32));
#126955=DIRECTION('ref_axis',(0.904066042851698,-0.427392782066418,2.0429572704782E-32));
#126956=DIRECTION('center_axis',(0.427392782066393,0.904066042851709,6.1569477156822E-15));
#126957=DIRECTION('ref_axis',(0.897284061240695,-0.424186633564772,-0.122257978669661));
#126958=DIRECTION('',(0.661602538143392,-0.312769350906473,0.681511125848849));
#126959=DIRECTION('',(-2.7619780906307E-32,-1.06237950525526E-32,1.));
#126960=DIRECTION('',(6.82090211058494E-33,-2.69054588173221E-32,1.));
#126961=DIRECTION('center_axis',(-2.7619780906307E-32,-1.06237950525526E-32,
1.));
#126962=DIRECTION('ref_axis',(0.742234123004267,0.670140661837563,2.7619780906307E-32));
#126963=DIRECTION('center_axis',(0.227628871285482,-0.252117093127508,-0.940543496235147));
#126964=DIRECTION('ref_axis',(-0.630207960610639,0.698183354379519,-0.339673269555233));
#126965=DIRECTION('center_axis',(0.227628871285482,-0.252117093127508,-0.940543496235147));
#126966=DIRECTION('ref_axis',(-0.630207960610639,0.698183354379519,-0.339673269555233));
#126967=DIRECTION('center_axis',(-0.663773370772875,0.313795601371545,-0.678923583927297));
#126968=DIRECTION('ref_axis',(-0.474277261530931,0.525299817366711,0.706485089063613));
#126969=DIRECTION('center_axis',(0.244577271937235,-0.692275035834063,0.678923583927297));
#126970=DIRECTION('ref_axis',(0.474277261530926,-0.525299817366713,-0.706485089063615));
#126971=DIRECTION('center_axis',(-0.934155508074011,-0.356038182328548,
-0.0242960790904556));
#126972=DIRECTION('ref_axis',(-0.228867508979934,0.649944984589603,-0.724700752269611));
#126973=DIRECTION('center_axis',(2.7619780906307E-32,1.06237950525526E-32,
-1.));
#126974=DIRECTION('ref_axis',(-0.742234123004264,-0.670140661837566,-2.76197809063069E-32));
#126975=DIRECTION('center_axis',(3.68755419309802E-35,-4.12557434076937E-32,
1.));
#126976=DIRECTION('ref_axis',(-0.159236911443844,0.987240399312055,4.07352085431321E-32));
#126977=DIRECTION('center_axis',(-2.7619780906307E-32,-1.06237950525526E-32,
1.));
#126978=DIRECTION('ref_axis',(0.742234123004264,0.670140661837566,2.76197809063069E-32));
#126979=DIRECTION('center_axis',(0.661313425361435,-0.312632674258581,0.681854357192688));
#126980=DIRECTION('ref_axis',(0.476172010550541,-0.527398402718972,-0.703641344136153));
#126981=DIRECTION('center_axis',(0.661895359476728,-0.312907780753821,0.681163162426516));
#126982=DIRECTION('ref_axis',(0.475725316336193,-0.52690365332183,-0.704313824593084));
#126983=DIRECTION('center_axis',(-0.243885290457238,0.690316384892969,-0.681163162426516));
#126984=DIRECTION('ref_axis',(-0.475725316336185,0.526903653321837,0.704313824593085));
#126985=DIRECTION('center_axis',(-0.243670868088652,0.689709463196114,-0.681854357192686));
#126986=DIRECTION('ref_axis',(-0.476172010550551,0.527398402718963,0.703641344136154));
#126987=DIRECTION('center_axis',(-2.7619780906307E-32,-1.06237950525526E-32,
1.));
#126988=DIRECTION('ref_axis',(0.742234123004264,0.670140661837566,2.76197809063069E-32));
#126989=DIRECTION('center_axis',(3.68755419309802E-35,-4.12557434076937E-32,
1.));
#126990=DIRECTION('ref_axis',(-0.965895271857674,0.258933048881347,1.0718093336019E-32));
#126991=DIRECTION('center_axis',(-2.7619780906307E-32,-1.06237950525526E-32,
1.));
#126992=DIRECTION('ref_axis',(-0.74223412300426,-0.670140661837571,-2.76197809063068E-32));
#126993=DIRECTION('center_axis',(2.7619780906307E-32,1.06237950525526E-32,
-1.));
#126994=DIRECTION('ref_axis',(0.742234123004269,0.670140661837561,2.7619780906307E-32));
#126995=DIRECTION('center_axis',(0.912596119838882,0.408862228696926,3.27031011275326E-32));
#126996=DIRECTION('ref_axis',(-0.408862228696926,0.912596119838882,-4.31965265863823E-34));
#126997=DIRECTION('',(-3.00213374770056E-32,-1.29768529867714E-32,1.));
#126998=DIRECTION('',(-0.299208548308713,0.667844914604604,-0.681511125848846));
#126999=DIRECTION('center_axis',(-0.91259808542786,-0.40885784139337,2.13514020802859E-6));
#127000=DIRECTION('ref_axis',(0.405397947498362,-0.904874692557993,0.129824092264084));
#127001=DIRECTION('',(1.44456010278038E-32,4.7742491995483E-32,-1.));
#127002=DIRECTION('center_axis',(-0.352280892409444,-0.935894317133727,
-2.27209065223238E-32));
#127003=DIRECTION('ref_axis',(0.935894317133727,-0.352280892409444,2.35253017866373E-32));
#127004=DIRECTION('center_axis',(0.352280892409472,0.935894317133717,-2.12694557450725E-14));
#127005=DIRECTION('ref_axis',(0.928873571132182,-0.349638206561809,-0.122257978735087));
#127006=DIRECTION('',(0.684894715983951,-0.257801887816002,0.681511125848851));
#127007=DIRECTION('',(-3.00213374770056E-32,-1.29768529867714E-32,1.));
#127008=DIRECTION('',(5.63185375672457E-33,-2.6397105460928E-32,1.));
#127009=DIRECTION('center_axis',(-3.00213374770056E-32,-1.29768529867714E-32,
1.));
#127010=DIRECTION('ref_axis',(0.685141714967841,0.728409795658272,3.00213374770055E-32));
#127011=DIRECTION('center_axis',(0.247421338625064,-0.232724328085156,-0.940543496235179));
#127012=DIRECTION('ref_axis',(-0.685019420610463,0.644492407508595,-0.339673269555143));
#127013=DIRECTION('center_axis',(0.247421338625064,-0.232724328085156,-0.940543496235179));
#127014=DIRECTION('ref_axis',(-0.685019420610463,0.644492407508595,-0.339673269555143));
#127015=DIRECTION('center_axis',(-0.687141974287091,0.25864778050498,-0.678923583927297));
#127016=DIRECTION('ref_axis',(-0.515515954829271,0.484893925768558,0.706485089063613));
#127017=DIRECTION('center_axis',(0.300190303429421,-0.670036229553497,0.678923583927297));
#127018=DIRECTION('ref_axis',(0.51551595482927,-0.484893925768558,-0.706485089063614));
#127019=DIRECTION('center_axis',(-0.90202676553384,-0.430995840817816,-0.0242960790726165));
#127020=DIRECTION('ref_axis',(-0.281082723153935,0.629127918196647,-0.72470032792177));
#127021=DIRECTION('center_axis',(3.00213374770056E-32,1.29768529867714E-32,
-1.));
#127022=DIRECTION('ref_axis',(-0.685141714967838,-0.728409795658274,-3.00213374770055E-32));
#127023=DIRECTION('center_axis',(4.00818924926601E-35,-4.12526018083156E-32,
1.));
#127024=DIRECTION('ref_axis',(-0.239176321393795,0.970976151758905,4.00648791934816E-32));
#127025=DIRECTION('center_axis',(-3.00213374770056E-32,-1.29768529867714E-32,
1.));
#127026=DIRECTION('ref_axis',(0.685141714967838,0.728409795658274,3.00213374770055E-32));
#127027=DIRECTION('center_axis',(0.684595424785282,-0.257689231324101,0.681854357192688));
#127028=DIRECTION('ref_axis',(0.517575453416346,-0.486831088616096,-0.703641344136152));
#127029=DIRECTION('center_axis',(0.685197846296139,-0.257915989392363,0.681163162426516));
#127030=DIRECTION('ref_axis',(0.517089918871253,-0.486374395182131,-0.704313824593084));
#127031=DIRECTION('center_axis',(-0.299340976225786,0.668140498776494,-0.681163162426516));
#127032=DIRECTION('ref_axis',(-0.517089918871254,0.486374395182132,0.704313824593083));
#127033=DIRECTION('center_axis',(-0.299077797577264,0.667553073975157,-0.681854357192686));
#127034=DIRECTION('ref_axis',(-0.517575453416357,0.486831088616081,0.703641344136154));
#127035=DIRECTION('center_axis',(-3.00213374770056E-32,-1.29768529867714E-32,
1.));
#127036=DIRECTION('ref_axis',(0.685141714967838,0.728409795658274,3.00213374770055E-32));
#127037=DIRECTION('center_axis',(4.00818924926601E-35,-4.12526018083156E-32,
1.));
#127038=DIRECTION('ref_axis',(-0.983786782322297,0.179342038931035,7.43775775555815E-33));
#127039=DIRECTION('center_axis',(-3.00213374770056E-32,-1.29768529867714E-32,
1.));
#127040=DIRECTION('ref_axis',(-0.685141714967838,-0.728409795658274,-3.00213374770055E-32));
#127041=DIRECTION('center_axis',(3.00213374770056E-32,1.29768529867714E-32,
-1.));
#127042=DIRECTION('ref_axis',(0.685141714967843,0.72840979565827,3.00213374770056E-32));
#127043=DIRECTION('center_axis',(0.876233464203457,0.481886829255594,3.57128027962397E-32));
#127044=DIRECTION('ref_axis',(-0.481886829255594,0.876233464203457,-1.93064851106194E-33));
#127045=DIRECTION('',(-3.22231069999667E-32,-1.55178304703032E-32,1.));
#127046=DIRECTION('',(-0.352648517057139,0.641234441340786,-0.681511125848853));
#127047=DIRECTION('center_axis',(-0.876235780858048,-0.481882616764217,
2.13514019795421E-6));
#127048=DIRECTION('ref_axis',(0.477804707150802,-0.868820100394176,0.12982409243122));
#127049=DIRECTION('',(1.38654752012359E-32,4.88982225644843E-32,-1.));
#127050=DIRECTION('center_axis',(-0.274824631535741,-0.961494369146925,
-2.37760101267757E-32));
#127051=DIRECTION('ref_axis',(0.961494369146926,-0.274824631535741,2.67176538956517E-32));
#127052=DIRECTION('center_axis',(0.274824631535787,0.961494369146912,-2.06334074273449E-14));
#127053=DIRECTION('ref_axis',(0.954281580675183,-0.272762994985753,-0.122257978678188));
#127054=DIRECTION('',(0.703629032489319,-0.201118795696426,0.681511125848848));
#127055=DIRECTION('',(-3.22231069999667E-32,-1.55178304703032E-32,1.));
#127056=DIRECTION('',(4.40532634530366E-33,-2.59873620878172E-32,1.));
#127057=DIRECTION('center_axis',(-3.22231069999667E-32,-1.55178304703032E-32,
1.));
#127058=DIRECTION('ref_axis',(0.623489801858728,0.781831482468034,3.22231069999666E-32));
#127059=DIRECTION('center_axis',(0.2655672577778,-0.211782821036267,-0.940543496235182));
#127060=DIRECTION('ref_axis',(0.735272189385988,-0.586512469999794,0.339673269555135));
#127061=DIRECTION('center_axis',(0.2655672577778,-0.211782821036267,-0.940543496235182));
#127062=DIRECTION('ref_axis',(0.735272189385988,-0.586512469999794,0.339673269555135));
#127063=DIRECTION('center_axis',(-0.705937761332873,0.201778701333035,-0.678923583927297));
#127064=DIRECTION('ref_axis',(-0.553323974502371,0.441261145096274,0.706485089063615));
#127065=DIRECTION('center_axis',(0.353805617980198,-0.643338442713448,0.678923583927297));
#127066=DIRECTION('ref_axis',(0.553323974502369,-0.44126114509628,-0.706485089063613));
#127067=DIRECTION('center_axis',(-0.863895183680872,-0.503085293120479,
-0.0242960790843667));
#127068=DIRECTION('ref_axis',(-0.331427070555256,0.604123469235223,-0.724700580117306));
#127069=DIRECTION('center_axis',(3.22231069999667E-32,1.55178304703032E-32,
-1.));
#127070=DIRECTION('ref_axis',(-0.623489801858734,-0.781831482468029,-3.22231069999667E-32));
#127071=DIRECTION('center_axis',(4.30215046728491E-35,-4.12492093150131E-32,
1.));
#127072=DIRECTION('ref_axis',(-0.317524052386152,0.948250218115597,3.91282320925606E-32));
#127073=DIRECTION('center_axis',(-3.22231069999667E-32,-1.55178304703032E-32,
1.));
#127074=DIRECTION('ref_axis',(0.623489801858734,0.781831482468029,3.22231069999667E-32));
#127075=DIRECTION('center_axis',(0.703321554607477,-0.201030909070889,0.681854357192688));
#127076=DIRECTION('ref_axis',(0.55553451703361,-0.443023993939946,-0.703641344136153));
#127077=DIRECTION('center_axis',(0.703940454498135,-0.201207809674643,0.681163162426516));
#127078=DIRECTION('ref_axis',(0.555013373310054,-0.442608395688626,-0.704313824593083));
#127079=DIRECTION('center_axis',(-0.352804597185337,0.641518247876084,-0.681163162426516));
#127080=DIRECTION('ref_axis',(-0.555013373310049,0.442608395688628,0.704313824593085));
#127081=DIRECTION('center_axis',(-0.352494413667362,0.640954229185401,-0.681854357192686));
#127082=DIRECTION('ref_axis',(-0.555534517033618,0.443023993939935,0.703641344136154));
#127083=DIRECTION('center_axis',(-3.22231069999667E-32,-1.55178304703032E-32,
1.));
#127084=DIRECTION('ref_axis',(0.623489801858734,0.781831482468029,3.22231069999667E-32));
#127085=DIRECTION('center_axis',(4.30215046728491E-35,-4.12492093150131E-32,
1.));
#127086=DIRECTION('ref_axis',(-0.995131354063954,0.0985575373010178,4.10823253390086E-33));
#127087=DIRECTION('center_axis',(-3.22231069999667E-32,-1.55178304703032E-32,
1.));
#127088=DIRECTION('ref_axis',(-0.623489801858718,-0.781831482468042,-3.22231069999664E-32));
#127089=DIRECTION('center_axis',(3.22231069999667E-32,1.55178304703032E-32,
-1.));
#127090=DIRECTION('ref_axis',(0.623489801858732,0.781831482468031,3.22231069999667E-32));
#127091=DIRECTION('center_axis',(0.834039619432103,0.551704552471296,3.8590333333347E-32));
#127092=DIRECTION('ref_axis',(-0.551704552471296,0.834039619432103,-3.66966363810105E-33));
#127093=DIRECTION('',(-3.42104370622815E-32,-1.82298177172267E-32,1.));
#127094=DIRECTION('',(-0.403741668107477,0.610356658666085,-0.681511125848848));
#127095=DIRECTION('center_axis',(-0.834042271735419,-0.55170054282542,2.13514023031498E-6));
#127096=DIRECTION('ref_axis',(0.547031755324907,-0.826983653837606,0.129824092338646));
#127097=DIRECTION('',(1.31930769248462E-32,5.00028218948676E-32,-1.));
#127098=DIRECTION('center_axis',(-0.195539458082041,-0.980695834768855,
-2.4567396627788E-32));
#127099=DIRECTION('ref_axis',(0.980695834768855,-0.195539458082041,2.99853844552406E-32));
#127100=DIRECTION('center_axis',(0.195539458081979,0.980695834768868,2.63196793879087E-14));
#127101=DIRECTION('ref_axis',(0.973339003741128,-0.194072590678889,-0.122257978649298));
#127102=DIRECTION('',(0.71768081387408,-0.143097291173766,0.681511125848851));
#127103=DIRECTION('',(-3.42104370622815E-32,-1.82298177172267E-32,1.));
#127104=DIRECTION('',(3.14948221388244E-33,-2.56789554725346E-32,1.));
#127105=DIRECTION('center_axis',(-3.42104370622815E-32,-1.82298177172267E-32,
1.));
#127106=DIRECTION('ref_axis',(0.557688666986824,0.830050209755084,3.42104370622814E-32));
#127107=DIRECTION('center_axis',(0.281945870645546,-0.189431934255097,-0.940543496235181));
#127108=DIRECTION('ref_axis',(0.780631843052823,-0.524629388770469,0.339673269555138));
#127109=DIRECTION('center_axis',(0.281945870645546,-0.189431934255097,-0.940543496235181));
#127110=DIRECTION('ref_axis',(0.780631843052823,-0.524629388770469,0.339673269555138));
#127111=DIRECTION('center_axis',(-0.720035649048516,0.14356681819486,-0.678923583927297));
#127112=DIRECTION('ref_axis',(-0.587449714417181,0.394691844306352,0.706485089063614));
#127113=DIRECTION('center_axis',(0.405066414517134,-0.612359344680513,0.678923583927297));
#127114=DIRECTION('ref_axis',(0.58744971441718,-0.394691844306355,-0.706485089063614));
#127115=DIRECTION('center_axis',(-0.820014521923814,-0.571826795783192,
-0.0242960790743142));
#127116=DIRECTION('ref_axis',(-0.379566263881805,0.575099350020013,-0.72470006825539));
#127117=DIRECTION('center_axis',(3.42104370622815E-32,1.82298177172267E-32,
-1.));
#127118=DIRECTION('ref_axis',(-0.557688666986826,-0.830050209755083,-3.42104370622814E-32));
#127119=DIRECTION('center_axis',(4.56748158374851E-35,-4.12455885042696E-32,
1.));
#127120=DIRECTION('ref_axis',(-0.393758713197673,0.919213835721,3.79315004722893E-32));
#127121=DIRECTION('center_axis',(-3.42104370622815E-32,-1.82298177172267E-32,
1.));
#127122=DIRECTION('ref_axis',(0.557688666986826,0.830050209755083,3.42104370622814E-32));
#127123=DIRECTION('center_axis',(0.717367195523648,-0.143034759285577,0.681854357192688));
#127124=DIRECTION('ref_axis',(0.589796590096754,-0.396268647677949,-0.703641344136152));
#127125=DIRECTION('center_axis',(0.717998455117447,-0.143160625180489,0.681163162426516));
#127126=DIRECTION('ref_axis',(0.589243305320241,-0.39589691034705,-0.704313824593083));
#127127=DIRECTION('center_axis',(-0.40392036175928,0.610626798879119,-0.681163162426516));
#127128=DIRECTION('ref_axis',(-0.589243305320237,0.395896910347054,0.704313824593084));
#127129=DIRECTION('center_axis',(-0.403565237591988,0.61008993975042,-0.681854357192686));
#127130=DIRECTION('ref_axis',(-0.58979659009676,0.396268647677936,0.703641344136155));
#127131=DIRECTION('center_axis',(-3.42104370622815E-32,-1.82298177172267E-32,
1.));
#127132=DIRECTION('ref_axis',(0.557688666986826,0.830050209755083,3.42104370622814E-32));
#127133=DIRECTION('center_axis',(4.56748158374851E-35,-4.12455885042696E-32,
1.));
#127134=DIRECTION('ref_axis',(-0.999853490829433,0.0171171515211064,7.5167511206289E-34));
#127135=DIRECTION('center_axis',(-3.42104370622815E-32,-1.82298177172267E-32,
1.));
#127136=DIRECTION('ref_axis',(-0.557688666986844,-0.830050209755071,-3.42104370622818E-32));
#127137=DIRECTION('center_axis',(3.42104370622815E-32,1.82298177172267E-32,
-1.));
#127138=DIRECTION('ref_axis',(0.557688666986828,0.830050209755082,3.42104370622815E-32));
#127139=DIRECTION('center_axis',(0.786295378600279,0.617850772915146,4.13165432478892E-32));
#127140=DIRECTION('ref_axis',(-0.617850772915146,0.78629537860028,-5.63743778822801E-33));
#127141=DIRECTION('',(-3.59701023102716E-32,-2.10947668998601E-32,1.));
#127142=DIRECTION('',(-0.452147984969248,0.575417053129711,-0.68151112584885));
#127143=DIRECTION('center_axis',(-0.786298348901551,-0.617846992798489,
2.13514017688966E-6));
#127144=DIRECTION('ref_axis',(0.612618397399368,-0.779643767476114,0.129824092538636));
#127145=DIRECTION('',(1.24328808982261E-32,5.10489390603353E-32,-1.));
#127146=DIRECTION('center_axis',(-0.114953001796544,-0.993370931413822,
-2.5089799478766E-32));
#127147=DIRECTION('ref_axis',(0.993370931413822,-0.114953001796544,3.33067472576676E-32));
#127148=DIRECTION('center_axis',(0.114953001796478,0.993370931413829,1.98701494460553E-14));
#127149=DIRECTION('ref_axis',(0.985919016308877,-0.114090665298237,-0.122257978767613));
#127150=DIRECTION('',(0.726956547851517,-0.0841234977877295,0.681511125848846));
#127151=DIRECTION('',(-3.59701023102716E-32,-2.10947668998601E-32,1.));
#127152=DIRECTION('',(1.87267879795583E-33,-2.54739380102216E-32,1.));
#127153=DIRECTION('center_axis',(-3.59701023102716E-32,-2.10947668998601E-32,
1.));
#127154=DIRECTION('ref_axis',(0.488176206048277,0.872745089844858,3.59701023102715E-32));
#127155=DIRECTION('center_axis',(0.296448180261865,-0.165820409205486,-0.940543496235211));
#127156=DIRECTION('ref_axis',(0.820796520599088,-0.459254985516989,0.339673269555055));
#127157=DIRECTION('center_axis',(0.296448180261865,-0.165820409205486,-0.940543496235211));
#127158=DIRECTION('ref_axis',(0.820796520599088,-0.459254985516989,0.339673269555055));
#127159=DIRECTION('center_axis',(-0.729341818317262,0.084399521568456,-0.678923583927297));
#127160=DIRECTION('ref_axis',(-0.617666073404929,0.345495934412133,0.706485089063615));
#127161=DIRECTION('center_axis',(0.453631560896713,-0.577305096240909,0.678923583927297));
#127162=DIRECTION('ref_axis',(0.617666073404927,-0.34549593441214,-0.706485089063614));
#127163=DIRECTION('center_axis',(-0.770676798808639,-0.636762885475809,
-0.0242960790785247));
#127164=DIRECTION('ref_axis',(-0.425178902774582,0.542247208642873,-0.724700534948344));
#127165=DIRECTION('center_axis',(3.59701023102716E-32,2.10947668998601E-32,
-1.));
#127166=DIRECTION('ref_axis',(-0.488176206048286,-0.872745089844853,-3.59701023102717E-32));
#127167=DIRECTION('center_axis',(4.80241686385389E-35,-4.1241763471983E-32,
1.));
#127168=DIRECTION('ref_axis',(-0.467372974738498,0.884060236909277,3.64826483841536E-32));
#127169=DIRECTION('center_axis',(-3.59701023102716E-32,-2.10947668998601E-32,
1.));
#127170=DIRECTION('ref_axis',(0.488176206048286,0.872745089844853,3.59701023102717E-32));
#127171=DIRECTION('center_axis',(0.726638876110865,-0.0840867367762921,
0.681854357192688));
#127172=DIRECTION('ref_axis',(0.620133664162395,-0.346876198945372,-0.703641344136153));
#127173=DIRECTION('center_axis',(0.727278294479358,-0.0841607303456,0.681163162426516));
#127174=DIRECTION('ref_axis',(0.619551920351823,-0.346550796385511,-0.704313824593083));
#127175=DIRECTION('center_axis',(-0.452348102967884,0.575671729281945,-0.681163162426516));
#127176=DIRECTION('ref_axis',(-0.619551920351822,0.346550796385512,0.704313824593084));
#127177=DIRECTION('center_axis',(-0.451950401444018,0.575165602424154,-0.681854357192686));
#127178=DIRECTION('ref_axis',(-0.620133664162403,0.346876198945357,0.703641344136154));
#127179=DIRECTION('center_axis',(-3.59701023102716E-32,-2.10947668998601E-32,
1.));
#127180=DIRECTION('ref_axis',(0.488176206048286,0.872745089844853,3.59701023102717E-32));
#127181=DIRECTION('center_axis',(4.80241686385389E-35,-4.1241763471983E-32,
1.));
#127182=DIRECTION('ref_axis',(-0.997921767577657,-0.06443714607805,-2.60957717410633E-33));
#127183=DIRECTION('center_axis',(-3.59701023102716E-32,-2.10947668998601E-32,
1.));
#127184=DIRECTION('ref_axis',(-0.488176206048267,-0.872745089844864,-3.59701023102713E-32));
#127185=DIRECTION('center_axis',(3.59701023102716E-32,2.10947668998601E-32,
-1.));
#127186=DIRECTION('ref_axis',(0.488176206048279,0.872745089844857,3.59701023102716E-32));
#127187=DIRECTION('center_axis',(0.733318471753477,0.679885298403447,4.38732900626779E-32));
#127188=DIRECTION('ref_axis',(-0.679885298403447,0.733318471753477,-7.82087574913358E-33));
#127189=DIRECTION('',(-3.7490392462036E-32,-2.40936122540763E-32,1.));
#127190=DIRECTION('',(-0.497545331590198,0.536648142041903,-0.681511125848855));
#127191=DIRECTION('center_axis',(-0.733321740285969,-0.67988177297189,2.13514019561374E-6));
#127192=DIRECTION('ref_axis',(0.674128165144339,-0.727115480513455,0.129824092358906));
#127193=DIRECTION('',(1.15899461005092E-32,5.20296123237483E-32,-1.));
#127194=DIRECTION('center_axis',(-0.0336015522500017,-0.999435308404896,
-2.53397421749269E-32));
#127195=DIRECTION('ref_axis',(0.999435308404897,-0.0336015522500017,3.66596391814689E-32));
#127196=DIRECTION('center_axis',(0.0336015522499427,0.999435308404898,2.27466779630292E-14));
#127197=DIRECTION('ref_axis',(0.991937900519573,-0.0333494853670919,-0.122257978629503));
#127198=DIRECTION('',(0.731394505942389,-0.0245898764033206,0.681511125848843));
#127199=DIRECTION('',(-3.7490392462036E-32,-2.40936122540763E-32,1.));
#127200=DIRECTION('',(5.83413013599077E-34,-2.53736740582643E-32,1.));
#127201=DIRECTION('center_axis',(-3.7490392462036E-32,-2.40936122540763E-32,
1.));
#127202=DIRECTION('ref_axis',(0.415415013001888,0.909631995354517,3.74903924620361E-32));
#127203=DIRECTION('center_axis',(0.308977676149196,-0.141105376691133,-0.94054349623518));
#127204=DIRECTION('ref_axis',(0.855498932722574,-0.390824316106684,0.339673269555141));
#127205=DIRECTION('center_axis',(0.308977676149196,-0.141105376691133,-0.94054349623518));
#127206=DIRECTION('ref_axis',(0.855498932722574,-0.390824316106684,0.339673269555141));
#127207=DIRECTION('center_axis',(-0.733794338118036,0.024670560050955,-0.678923583927297));
#127208=DIRECTION('ref_axis',(-0.643771966581894,0.294000806077225,0.706485089063614));
#127209=DIRECTION('center_axis',(0.499177864082464,-0.538408977634459,0.678923583927297));
#127210=DIRECTION('ref_axis',(0.643771966581889,-0.294000806077234,-0.706485089063615));
#127211=DIRECTION('center_axis',(-0.716210348753134,-0.697461423220216,
-0.0242960790775933));
#127212=DIRECTION('ref_axis',(-0.46796256549965,0.505787122557392,-0.724700230402957));
#127213=DIRECTION('center_axis',(3.7490392462036E-32,2.40936122540763E-32,
-1.));
#127214=DIRECTION('ref_axis',(-0.415415013001888,-0.909631995354518,-3.74903924620361E-32));
#127215=DIRECTION('center_axis',(5.00539285207499E-35,-4.12377596731122E-32,
1.));
#127216=DIRECTION('ref_axis',(-0.537876946243531,0.843023363080605,3.47913176997571E-32));
#127217=DIRECTION('center_axis',(-3.7490392462036E-32,-2.40936122540763E-32,
1.));
#127218=DIRECTION('ref_axis',(0.415415013001888,0.909631995354518,3.74903924620361E-32));
#127219=DIRECTION('center_axis',(0.73107489486454,-0.0245791309070966,0.681854357192688));
#127220=DIRECTION('ref_axis',(0.646343851007887,-0.295175346339363,-0.703641344136153));
#127221=DIRECTION('center_axis',(0.731718216783982,-0.0246007597358041,
0.681163162426516));
#127222=DIRECTION('ref_axis',(0.645737519572335,-0.294898444050882,-0.704313824593083));
#127223=DIRECTION('center_axis',(-0.497765542183421,0.536885659305548,-0.681163162426516));
#127224=DIRECTION('ref_axis',(-0.645737519572333,0.294898444050884,0.704313824593084));
#127225=DIRECTION('center_axis',(-0.497327909941004,0.5364136329094,-0.681854357192686));
#127226=DIRECTION('ref_axis',(-0.646343851007887,0.295175346339356,0.703641344136156));
#127227=DIRECTION('center_axis',(-3.7490392462036E-32,-2.40936122540763E-32,
1.));
#127228=DIRECTION('ref_axis',(0.415415013001888,0.909631995354518,3.74903924620361E-32));
#127229=DIRECTION('center_axis',(5.00539285207499E-35,-4.12377596731122E-32,
1.));
#127230=DIRECTION('ref_axis',(-0.989349039608151,-0.145562625101462,-5.95315574521082E-33));
#127231=DIRECTION('center_axis',(-3.7490392462036E-32,-2.40936122540763E-32,
1.));
#127232=DIRECTION('ref_axis',(-0.415415013001908,-0.909631995354509,-3.74903924620366E-32));
#127233=DIRECTION('center_axis',(3.7490392462036E-32,2.40936122540763E-32,
-1.));
#127234=DIRECTION('ref_axis',(0.415415013001884,0.909631995354519,3.7490392462036E-32));
#127235=DIRECTION('center_axis',(0.675461451466187,0.737395299404053,4.62435590494944E-32));
#127236=DIRECTION('ref_axis',(-0.737395299404053,0.675461451466187,-1.02054471014299E-32));
#127237=DIRECTION('',(-3.87611902374449E-32,-2.72063969588177E-32,1.));
#127238=DIRECTION('',(-0.539631596118643,0.494307926109506,-0.681511125848849));
#127239=DIRECTION('center_axis',(-0.675464996478299,-0.737392052118826,
2.13514020039549E-6));
#127240=DIRECTION('ref_axis',(0.731151721197705,-0.669748360010381,0.12982409195923));
#127241=DIRECTION('',(1.06698821237E-32,5.29383154663385E-32,-1.));
#127242=DIRECTION('center_axis',(0.0479735100828988,-0.998848608313755,
-2.53155613888654E-32));
#127243=DIRECTION('ref_axis',(0.998848608313755,0.0479735100828988,4.00217472840797E-32));
#127244=DIRECTION('center_axis',(-0.0479735100828819,0.998848608313756,
-9.89055134078661E-15));
#127245=DIRECTION('ref_axis',(0.991355601632822,0.0476136298882577,-0.122257978717502));
#127246=DIRECTION('',(0.730965154267811,0.0351073865515132,0.681511125848843));
#127247=DIRECTION('',(-3.87611902374449E-32,-2.72063969588177E-32,1.));
#127248=DIRECTION('',(-7.09735288106811E-34,-2.53788308567206E-32,1.));
#127249=DIRECTION('center_axis',(-3.87611902374449E-32,-2.72063969588177E-32,
1.));
#127250=DIRECTION('ref_axis',(0.339889301582619,0.940465450013811,3.8761190237445E-32));
#127251=DIRECTION('center_axis',(0.319450976579402,-0.115451311175611,-0.940543496235182));
#127252=DIRECTION('ref_axis',(0.884508140596374,-0.319792775353774,0.339673269555136));
#127253=DIRECTION('center_axis',(0.319450976579402,-0.115451311175611,-0.940543496235182));
#127254=DIRECTION('ref_axis',(0.884508140596374,-0.319792775353774,0.339673269555136));
#127255=DIRECTION('center_axis',(-0.733363577666178,-0.0352225799733294,
-0.678923583927297));
#127256=DIRECTION('ref_axis',(-0.665593663536156,0.240549150884587,0.706485089063614));
#127257=DIRECTION('center_axis',(0.541402220941297,-0.495929836113079,0.678923583927297));
#127258=DIRECTION('ref_axis',(0.665593663536153,-0.240549150884594,-0.706485089063614));
#127259=DIRECTION('center_axis',(-0.656977636984026,-0.753518470273803,
-0.0242960790892854));
#127260=DIRECTION('ref_axis',(-0.50763101857097,0.465960210135762,-0.724701201568506));
#127261=DIRECTION('center_axis',(3.87611902374449E-32,2.72063969588177E-32,
-1.));
#127262=DIRECTION('ref_axis',(-0.339889301582622,-0.94046545001381,-3.87611902374451E-32));
#127263=DIRECTION('center_axis',(5.17505877669541E-35,-4.12336037522781E-32,
1.));
#127264=DIRECTION('ref_axis',(-0.604801435414764,0.796376307859696,3.2868763945754E-32));
#127265=DIRECTION('center_axis',(-3.87611902374449E-32,-2.72063969588177E-32,
1.));
#127266=DIRECTION('ref_axis',(0.339889301582622,0.94046545001381,3.87611902374451E-32));
#127267=DIRECTION('center_axis',(0.730645730811759,0.0350920450230146,0.681854357192688));
#127268=DIRECTION('ref_axis',(0.66825272616415,-0.241510150503968,-0.703641344136153));
#127269=DIRECTION('center_axis',(0.731288675080916,0.0351229248711943,0.681163162426515));
#127270=DIRECTION('ref_axis',(0.667625842139285,-0.241283591225913,-0.704313824593084));
#127271=DIRECTION('center_axis',(-0.53987043384126,0.494526703846372,-0.681163162426516));
#127272=DIRECTION('ref_axis',(-0.667625842139283,0.241283591225916,0.704313824593084));
#127273=DIRECTION('center_axis',(-0.539395783250663,0.494091919169655,-0.681854357192686));
#127274=DIRECTION('ref_axis',(-0.668252726164153,0.241510150503956,0.703641344136155));
#127275=DIRECTION('center_axis',(-3.87611902374449E-32,-2.72063969588177E-32,
1.));
#127276=DIRECTION('ref_axis',(0.339889301582622,0.94046545001381,3.87611902374451E-32));
#127277=DIRECTION('center_axis',(5.17505877669541E-35,-4.12336037522781E-32,
1.));
#127278=DIRECTION('ref_axis',(-0.97419235701116,-0.225719408870926,-9.25680963750882E-33));
#127279=DIRECTION('center_axis',(-3.87611902374449E-32,-2.72063969588177E-32,
1.));
#127280=DIRECTION('ref_axis',(-0.339889301582586,-0.940465450013823,-3.87611902374441E-32));
#127281=DIRECTION('center_axis',(3.87611902374449E-32,2.72063969588177E-32,
-1.));
#127282=DIRECTION('ref_axis',(0.339889301582614,0.940465450013812,3.87611902374449E-32));
#127283=DIRECTION('center_axis',(0.613109346662684,0.789998056348784,4.84115764592981E-32));
#127284=DIRECTION('ref_axis',(-0.789998056348784,0.613109346662684,-1.27752829161939E-32));
#127285=DIRECTION('',(-3.97740386869698E-32,-3.04124059454475E-32,1.));
#127286=DIRECTION('',(-0.578126701407848,0.44867817248392,-0.681511125848853));
#127287=DIRECTION('center_axis',(-0.613113144562907,-0.789995108820064,
2.13514017973777E-6));
#127288=DIRECTION('ref_axis',(0.783309583130661,-0.607924174624544,0.129824092073606));
#127289=DIRECTION('',(9.67881184176422E-33,5.37690012186172E-32,-1.));
#127290=DIRECTION('center_axis',(0.129229316621269,-0.991614735532707,-2.50174180397231E-32));
#127291=DIRECTION('ref_axis',(0.991614735532707,0.129229316621269,4.3370697290786E-32));
#127292=DIRECTION('center_axis',(-0.129229316621292,0.991614735532704,1.20022317556764E-14));
#127293=DIRECTION('ref_axis',(0.984175994800074,0.12825988429344,-0.122257978636643));
#127294=DIRECTION('',(0.725671350092337,0.0945710156411612,0.681511125848848));
#127295=DIRECTION('',(-3.97740386869698E-32,-3.04124059454475E-32,1.));
#127296=DIRECTION('',(-1.99816041856844E-33,-2.54893740879476E-32,1.));
#127297=DIRECTION('center_axis',(-3.97740386869698E-32,-3.04124059454475E-32,
1.));
#127298=DIRECTION('ref_axis',(0.262101682939102,0.96504026226914,3.97740386869699E-32));
#127299=DIRECTION('center_axis',(0.327798383466009,-0.0890289362322958,
-0.940543496235244));
#127300=DIRECTION('ref_axis',(0.907631092727719,-0.24663306644432,0.339673269554962));
#127301=DIRECTION('center_axis',(0.327798383466009,-0.0890289362322958,
-0.940543496235244));
#127302=DIRECTION('ref_axis',(0.907631092727719,-0.24663306644432,0.339673269554962));
#127303=DIRECTION('center_axis',(-0.728052403601425,-0.0948813195392077,
-0.678923583927297));
#127304=DIRECTION('ref_axis',(-0.682985944474809,0.185496680780628,0.706485089063615));
#127305=DIRECTION('center_axis',(0.580023635344843,-0.450150363355031,0.678923583927297));
#127306=DIRECTION('ref_axis',(0.682985944474808,-0.185496680780635,-0.706485089063613));
#127307=DIRECTION('center_axis',(-0.593372847443218,-0.804560976221234,
-0.0242960790882418));
#127308=DIRECTION('ref_axis',(-0.54392253522018,0.423033500529492,-0.724700581695238));
#127309=DIRECTION('center_axis',(3.97740386869698E-32,3.04124059454475E-32,
-1.));
#127310=DIRECTION('ref_axis',(-0.262101682939102,-0.96504026226914,-3.97740386869699E-32));
#127311=DIRECTION('center_axis',(5.3102855389809E-35,-4.12293233664482E-32,
1.));
#127312=DIRECTION('ref_axis',(-0.667701070818532,0.744429499702817,3.0727781400178E-32));
#127313=DIRECTION('center_axis',(-3.97740386869698E-32,-3.04124059454475E-32,
1.));
#127314=DIRECTION('ref_axis',(0.262101682939102,0.96504026226914,3.97740386869699E-32));
#127315=DIRECTION('center_axis',(0.725354239968486,0.0945296891832773,0.681854357192688));
#127316=DIRECTION('ref_axis',(0.685714489681731,-0.186237744463339,-0.703641344136153));
#127317=DIRECTION('center_axis',(0.725992527899325,0.0946128722080492,0.681163162426516));
#127318=DIRECTION('ref_axis',(0.685071224877309,-0.186063035910322,-0.704313824593084));
#127319=DIRECTION('center_axis',(-0.578382576834238,0.448876754764262,-0.681163162426516));
#127320=DIRECTION('ref_axis',(-0.68507122487731,0.186063035910324,0.704313824593083));
#127321=DIRECTION('center_axis',(-0.577874066616828,0.448482105227263,-0.681854357192686));
#127322=DIRECTION('ref_axis',(-0.685714489681731,0.186237744463328,0.703641344136155));
#127323=DIRECTION('center_axis',(-3.97740386869698E-32,-3.04124059454475E-32,
1.));
#127324=DIRECTION('ref_axis',(0.262101682939102,0.96504026226914,3.97740386869699E-32));
#127325=DIRECTION('center_axis',(5.3102855389809E-35,-4.12293233664482E-32,
1.));
#127326=DIRECTION('ref_axis',(-0.952552585008684,-0.304374067215448,-1.24985535794138E-32));
#127327=DIRECTION('center_axis',(-3.97740386869698E-32,-3.04124059454475E-32,
1.));
#127328=DIRECTION('ref_axis',(-0.262101682939063,-0.965040262269151,-3.97740386869687E-32));
#127329=DIRECTION('center_axis',(3.97740386869698E-32,3.04124059454475E-32,
-1.));
#127330=DIRECTION('ref_axis',(0.262101682939099,0.965040262269141,3.97740386869698E-32));
#127331=DIRECTION('center_axis',(0.546677100313063,0.837343506569019,5.03629144939245E-32));
#127332=DIRECTION('ref_axis',(-0.837343506569019,0.546677100313063,-1.55132813600715E-32));
#127333=DIRECTION('',(-4.05221974712874E-32,-3.36903037531139E-32,1.));
#127334=DIRECTION('',(-0.612774468883391,0.400062539647137,-0.681511125848845));
#127335=DIRECTION('center_axis',(-0.546681125827074,-0.837340878412062,
2.13514019490064E-6));
#127336=DIRECTION('ref_axis',(0.830254649042338,-0.542054354171433,0.129824092014448));
#127337=DIRECTION('',(8.62333066391302E-33,5.45161415039565E-32,-1.));
#127338=DIRECTION('center_axis',(0.209625123378862,-0.977781830291603,-2.44472962222985E-32));
#127339=DIRECTION('ref_axis',(0.977781830291603,0.209625123378862,4.6684202491831E-32));
#127340=DIRECTION('center_axis',(-0.209625123378866,0.977781830291602,-1.86998205414277E-15));
#127341=DIRECTION('ref_axis',(0.970446859081431,0.208052590327751,-0.122257978704452));
#127342=DIRECTION('',(0.715548322809351,0.153405290224829,0.681511125848846));
#127343=DIRECTION('',(-4.05221974712874E-32,-3.36903037531139E-32,1.));
#127344=DIRECTION('',(-3.27328812111774E-33,-2.57045681049799E-32,1.));
#127345=DIRECTION('center_axis',(-4.05221974712874E-32,-3.36903037531139E-32,
1.));
#127346=DIRECTION('ref_axis',(0.182569820839361,0.983192890799503,4.05221974712875E-32));
#127347=DIRECTION('center_axis',(0.333964346193912,-0.0620140884071856,
-0.940543496235182));
#127348=DIRECTION('ref_axis',(0.924713909685948,-0.171832055167397,0.339673269555136));
#127349=DIRECTION('center_axis',(0.333964346193912,-0.0620140884071856,
-0.940543496235182));
#127350=DIRECTION('ref_axis',(0.924713909685948,-0.171832055167397,0.339673269555136));
#127351=DIRECTION('center_axis',(-0.717896160910897,-0.153908639577868,
-0.678923583927297));
#127352=DIRECTION('ref_axis',(-0.695833066637731,0.129209760870875,0.706485089063614));
#127353=DIRECTION('center_axis',(0.614785088152334,-0.401375214198437,0.678923583927297));
#127354=DIRECTION('ref_axis',(0.695833066637729,-0.129209760870883,-0.706485089063614));
#127355=DIRECTION('center_axis',(-0.525819259512051,-0.850249261609663,
-0.0242960790750349));
#127356=DIRECTION('ref_axis',(-0.576593278623329,0.377290828495695,-0.724701194824069));
#127357=DIRECTION('center_axis',(4.05221974712874E-32,3.36903037531139E-32,
-1.));
#127358=DIRECTION('ref_axis',(-0.182569820839353,-0.983192890799505,-4.05221974712873E-32));
#127359=DIRECTION('center_axis',(5.41017322714156E-35,-4.12249470008839E-32,
1.));
#127360=DIRECTION('ref_axis',(-0.726157265758901,0.687528636047661,2.83826179486338E-32));
#127361=DIRECTION('center_axis',(-4.05221974712875E-32,-3.36903037531139E-32,
1.));
#127362=DIRECTION('ref_axis',(0.182569820839353,0.983192890799505,4.05221974712873E-32));
#127363=DIRECTION('center_axis',(0.715235636333248,0.153338253858326,0.681854357192688));
#127364=DIRECTION('ref_axis',(0.698612936405406,-0.129725956960371,-0.703641344136153));
#127365=DIRECTION('center_axis',(0.7158650202249,0.153473186490385,0.681163162426516));
#127366=DIRECTION('ref_axis',(0.69795757164257,-0.129604261788992,-0.704313824593084));
#127367=DIRECTION('center_axis',(-0.613045679204792,0.400239604938646,-0.681163162426516));
#127368=DIRECTION('ref_axis',(-0.697957571642569,0.129604261788998,0.704313824593084));
#127369=DIRECTION('center_axis',(-0.612506693412169,0.399887716868923,-0.681854357192686));
#127370=DIRECTION('ref_axis',(-0.698612936405406,0.129725956960361,0.703641344136155));
#127371=DIRECTION('center_axis',(-4.05221974712874E-32,-3.36903037531139E-32,
1.));
#127372=DIRECTION('ref_axis',(0.182569820839353,0.983192890799505,4.05221974712873E-32));
#127373=DIRECTION('center_axis',(5.41017322714156E-35,-4.12249470008839E-32,
1.));
#127374=DIRECTION('ref_axis',(-0.924573732713088,-0.381003166360843,-1.56568142998423E-32));
#127375=DIRECTION('center_axis',(-4.05221974712875E-32,-3.36903037531139E-32,
1.));
#127376=DIRECTION('ref_axis',(-0.182569820839333,-0.983192890799508,-4.05221974712866E-32));
#127377=DIRECTION('center_axis',(4.05221974712874E-32,3.36903037531139E-32,
-1.));
#127378=DIRECTION('ref_axis',(0.182569820839359,0.983192890799503,4.05221974712874E-32));
#127379=DIRECTION('center_axis',(0.476606808056231,0.879116573904992,5.20845873207013E-32));
#127380=DIRECTION('ref_axis',(-0.879116573904992,0.476606808056231,-1.84012215051566E-32));
#127381=DIRECTION('',(-4.10006877171256E-32,-3.7018276512722E-32,1.));
#127382=DIRECTION('',(-0.643344323369166,0.348784556614685,-0.68151112584885));
#127383=DIRECTION('center_axis',(-0.476611034394921,-0.879114282609744,
2.13514022319101E-6));
#127384=DIRECTION('ref_axis',(0.871674507249432,-0.472577251423886,0.129824091940232));
#127385=DIRECTION('',(7.51046264324289E-33,5.51747642270271E-32,-1.));
#127386=DIRECTION('center_axis',(0.288625909526079,-0.957441948292555,-2.36089900032229E-32));
#127387=DIRECTION('ref_axis',(0.957441948292555,0.288625909526079,4.99402120567917E-32));
#127388=DIRECTION('center_axis',(-0.288625909526091,0.957441948292551,1.95902881862569E-15));
#127389=DIRECTION('ref_axis',(0.950259559641614,0.28646074070239,-0.12225797865973));
#127390=DIRECTION('',(0.700663439495228,0.211218677912143,0.681511125848847));
#127391=DIRECTION('',(-4.10006877171256E-32,-3.7018276512722E-32,1.));
#127392=DIRECTION('',(-4.52663263127555E-33,-2.60229808271385E-32,1.));
#127393=DIRECTION('center_axis',(-4.10006877171256E-32,-3.7018276512722E-32,
1.));
#127394=DIRECTION('ref_axis',(0.101822986703838,0.994802532857004,4.10006877171259E-32));
#127395=DIRECTION('center_axis',(0.337907831297878,-0.0345865470552739,
-0.940543496235213));
#127396=DIRECTION('ref_axis',(0.935642908142144,-0.0958875299144513,0.339673269555049));
#127397=DIRECTION('center_axis',(0.337907831297878,-0.0345865470552739,
-0.940543496235213));
#127398=DIRECTION('ref_axis',(0.935642908142144,-0.0958875299144513,0.339673269555049));
#127399=DIRECTION('center_axis',(-0.702962437714035,-0.211911723013277,
-0.678923583927297));
#127400=DIRECTION('ref_axis',(-0.704049534546554,0.0720629713206354,0.706485089063614));
#127401=DIRECTION('center_axis',(0.645455247630571,-0.349928979213601,0.678923583927297));
#127402=DIRECTION('ref_axis',(0.704049534546552,-0.072062971320644,-0.706485089063614));
#127403=DIRECTION('center_axis',(-0.454766431155998,-0.890279278448852,
-0.0242960790710806));
#127404=DIRECTION('ref_axis',(-0.60542764494557,0.329037829144449,-0.724700954689291));
#127405=DIRECTION('center_axis',(4.10006877171256E-32,3.7018276512722E-32,
-1.));
#127406=DIRECTION('ref_axis',(-0.101822986703825,-0.994802532857005,-4.10006877171253E-32));
#127407=DIRECTION('center_axis',(5.47405710508952E-35,-4.1220503779576E-32,
1.));
#127408=DIRECTION('ref_axis',(-0.779781003903195,0.626052382753812,2.58488802669644E-32));
#127409=DIRECTION('center_axis',(-4.10006877171256E-32,-3.7018276512722E-32,
1.));
#127410=DIRECTION('ref_axis',(0.101822986703825,0.994802532857005,4.10006877171253E-32));
#127411=DIRECTION('center_axis',(0.700357257543786,0.211126377752979,0.681854357192688));
#127412=DIRECTION('ref_axis',(0.706862229300325,-0.0723508646171092,-0.703641344136153));
#127413=DIRECTION('center_axis',(0.700973548950293,0.21131216203792,0.681163162426516));
#127414=DIRECTION('ref_axis',(0.706199125923443,-0.0722829926886559,-0.704313824593084));
#127415=DIRECTION('center_axis',(-0.643629063725655,0.348938926577051,-0.681163162426516));
#127416=DIRECTION('ref_axis',(-0.706199125923443,0.0722829926886583,0.704313824593083));
#127417=DIRECTION('center_axis',(-0.643063189219342,0.34863214173165,-0.681854357192686));
#127418=DIRECTION('ref_axis',(-0.706862229300325,0.0723508646170959,0.703641344136154));
#127419=DIRECTION('center_axis',(-4.10006877171256E-32,-3.7018276512722E-32,
1.));
#127420=DIRECTION('ref_axis',(0.101822986703825,0.994802532857005,4.10006877171253E-32));
#127421=DIRECTION('center_axis',(5.47405710508952E-35,-4.1220503779576E-32,
1.));
#127422=DIRECTION('ref_axis',(-0.89044199477021,-0.455096752295211,-1.87105740947761E-32));
#127423=DIRECTION('center_axis',(-4.10006877171256E-32,-3.7018276512722E-32,
1.));
#127424=DIRECTION('ref_axis',(-0.101822986703824,-0.994802532857005,-4.10006877171254E-32));
#127425=DIRECTION('center_axis',(4.10006877171256E-32,3.7018276512722E-32,
-1.));
#127426=DIRECTION('ref_axis',(0.101822986703832,0.994802532857004,4.10006877171256E-32));
#127427=DIRECTION('center_axis',(0.403364776126373,0.915039265485652,5.35651374910224E-32));
#127428=DIRECTION('ref_axis',(-0.915039265485652,0.403364776126373,-2.14198845862603E-32));
#127429=DIRECTION('',(-4.12063251508437E-32,-4.03741771146334E-32,1.));
#127430=DIRECTION('',(-0.669632827527267,0.295185469903361,-0.681511125848852));
#127431=DIRECTION('center_axis',(-0.403369175164062,-0.915037326300357,
2.13514020751955E-6));
#127432=DIRECTION('ref_axis',(0.907293515386185,-0.399955225018066,0.129824092212985));
#127433=DIRECTION('',(6.34761373282109E-33,5.5740486362272E-32,-1.));
#127434=DIRECTION('center_axis',(0.365705937865323,-0.930730448094423,-2.25080781720736E-32));
#127435=DIRECTION('ref_axis',(0.930730448094423,0.365705937865323,5.31170577792169E-32));
#127436=DIRECTION('center_axis',(-0.365705937865339,0.930730448094416,6.81843796612823E-15));
#127437=DIRECTION('ref_axis',(0.923748439609161,0.362962542109338,-0.122257978656478));
#127438=DIRECTION('',(0.681115756592596,0.267626440146581,0.681511125848847));
#127439=DIRECTION('',(-4.12063251508437E-32,-4.03741771146334E-32,1.));
#127440=DIRECTION('',(-5.74985314811402E-33,-2.64424932702919E-32,1.));
#127441=DIRECTION('center_axis',(-4.12063251508437E-32,-4.03741771146334E-32,
1.));
#127442=DIRECTION('ref_axis',(0.0203985373914037,0.999791928189207,4.12063251508437E-32));
#127443=DIRECTION('center_axis',(0.339602595535507,-0.0069288379391035,
-0.940543496235214));
#127444=DIRECTION('ref_axis',(0.940345357414828,-0.0193048889705321,0.339673269555046));
#127445=DIRECTION('center_axis',(0.339602595535507,-0.0069288379391035,
-0.940543496235214));
#127446=DIRECTION('ref_axis',(0.940345357414828,-0.0193048889705321,0.339673269555046));
#127447=DIRECTION('center_axis',(-0.683350615474825,-0.268504568895005,
-0.678923583927297));
#127448=DIRECTION('ref_axis',(-0.707580668962966,0.0144366145858088,0.706485089063614));
#127449=DIRECTION('center_axis',(0.671830008928446,-0.296154024606316,0.678923583927297));
#127450=DIRECTION('ref_axis',(0.707580668962966,-0.014436614585817,-0.706485089063614));
#127451=DIRECTION('center_axis',(-0.380687207232623,-0.924384633575987,
-0.0242960790666857));
#127452=DIRECTION('ref_axis',(-0.630232780927451,0.278595012725823,-0.724700945720889));
#127453=DIRECTION('center_axis',(4.12063251508437E-32,4.03741771146334E-32,
-1.));
#127454=DIRECTION('ref_axis',(-0.0203985373913968,-0.999791928189207,-4.12063251508434E-32));
#127455=DIRECTION('center_axis',(5.50151203616034E-35,-4.12160232714292E-32,
1.));
#127456=DIRECTION('ref_axis',(-0.828215428121308,0.560409854144125,2.31434299614059E-32));
#127457=DIRECTION('center_axis',(-4.12063251508437E-32,-4.03741771146334E-32,
1.));
#127458=DIRECTION('ref_axis',(0.0203985373913968,0.999791928189207,4.12063251508434E-32));
#127459=DIRECTION('center_axis',(0.680818116756184,0.267509490437086,0.681854357192688));
#127460=DIRECTION('ref_axis',(0.710407470683308,-0.0144942892068718,-0.703641344136153));
#127461=DIRECTION('center_axis',(0.681417214359916,0.267744890011146,0.681163162426516));
#127462=DIRECTION('ref_axis',(0.70974104153595,-0.0144806921978297,-0.704313824593084));
#127463=DIRECTION('center_axis',(-0.669929203018745,0.295316117229956,-0.681163162426516));
#127464=DIRECTION('ref_axis',(-0.70974104153595,0.0144806921978318,0.704313824593083));
#127465=DIRECTION('center_axis',(-0.669340205600219,0.295056477211407,-0.681854357192686));
#127466=DIRECTION('ref_axis',(-0.710407470683307,0.0144942892068606,0.703641344136155));
#127467=DIRECTION('center_axis',(-4.12063251508437E-32,-4.03741771146334E-32,
1.));
#127468=DIRECTION('ref_axis',(0.0203985373913968,0.999791928189207,4.12063251508434E-32));
#127469=DIRECTION('center_axis',(5.50151203616034E-35,-4.12160232714292E-32,
1.));
#127470=DIRECTION('ref_axis',(-0.850384512264726,-0.52616174442873,-2.16395106966144E-32));
#127471=DIRECTION('center_axis',(-4.12063251508437E-32,-4.03741771146334E-32,
1.));
#127472=DIRECTION('ref_axis',(-0.0203985373913968,-0.999791928189207,-4.12063251508434E-32));
#127473=DIRECTION('center_axis',(4.12063251508437E-32,4.03741771146334E-32,
-1.));
#127474=DIRECTION('ref_axis',(0.0203985373914021,0.999791928189207,4.12063251508437E-32));
#127475=DIRECTION('center_axis',(0.327438418161898,0.944872521725357,5.47947121877778E-32));
#127476=DIRECTION('ref_axis',(-0.944872521725356,0.327438418161898,-2.45491818986221E-32));
#127477=DIRECTION('',(-4.11377412892479E-32,-4.37356725940272E-32,1.));
#127478=DIRECTION('',(-0.691465035699823,0.239621972591999,-0.681511125848846));
#127479=DIRECTION('center_axis',(-0.327442960623831,-0.944870947554925,
2.13514022945096E-6));
#127480=DIRECTION('ref_axis',(0.936874634876281,-0.324671562585836,0.129824092423197));
#127481=DIRECTION('',(5.14252250028993E-33,5.62095431222186E-32,-1.));
#127482=DIRECTION('center_axis',(0.440352253525306,-0.897825090323936,-2.11518871154492E-32));
#127483=DIRECTION('ref_axis',(0.897825090323936,0.440352253525306,5.61935982749666E-32));
#127484=DIRECTION('center_axis',(-0.440352253525287,0.897825090323946,-7.17462502405725E-15));
#127485=DIRECTION('ref_axis',(0.891089926119414,0.43704888768344,-0.12225797864829));
#127486=DIRECTION('',(0.657035360706024,0.322253192577101,0.681511125848853));
#127487=DIRECTION('',(-4.11377412892479E-32,-4.37356725940272E-32,1.));
#127488=DIRECTION('',(-6.9348093409108E-33,-2.69603136483457E-32,1.));
#127489=DIRECTION('center_axis',(-4.11377412892479E-32,-4.37356725940272E-32,
1.));
#127490=DIRECTION('ref_axis',(-0.0611616608218504,0.998127873193366,4.11377412892477E-32));
#127491=DIRECTION('center_axis',(0.339037360530247,0.0207749814503661,-0.940543496235246));
#127492=DIRECTION('ref_axis',(0.938789963480034,0.0574062228247189,0.339673269554958));
#127493=DIRECTION('center_axis',(0.339037360530247,0.0207749814503661,-0.940543496235246));
#127494=DIRECTION('ref_axis',(0.938789963480034,0.0574062228247189,0.339673269554958));
#127495=DIRECTION('center_axis',(-0.659191207634545,-0.323310561170872,
-0.678923583927297));
#127496=DIRECTION('ref_axis',(-0.706402970770023,-0.0432858154372093,0.706485089063614));
#127497=DIRECTION('center_axis',(0.693733852361051,-0.240408213827251,0.678923583927297));
#127498=DIRECTION('ref_axis',(0.706402970770023,0.0432858154372054,-0.706485089063614));
#127499=DIRECTION('center_axis',(-0.304074572747413,-0.952338361482043,
-0.0242960790700016));
#127500=DIRECTION('ref_axis',(-0.650843724041517,0.226298162138698,-0.724701034005345));
#127501=DIRECTION('center_axis',(4.11377412892479E-32,4.37356725940272E-32,
-1.));
#127502=DIRECTION('ref_axis',(0.0611616608218468,-0.998127873193367,-4.11377412892479E-32));
#127503=DIRECTION('center_axis',(5.49235531231428E-35,-4.12115352934861E-32,
1.));
#127504=DIRECTION('ref_axis',(-0.871138215311196,0.491037890416234,2.02842713573738E-32));
#127505=DIRECTION('center_axis',(-4.11377412892479E-32,-4.37356725940272E-32,
1.));
#127506=DIRECTION('ref_axis',(-0.0611616608218468,0.998127873193367,4.11377412892479E-32));
#127507=DIRECTION('center_axis',(0.656748243728652,0.322112371598294,0.681854357192688));
#127508=DIRECTION('ref_axis',(0.709225067557877,0.0434587433066445,-0.703641344136153));
#127509=DIRECTION('center_axis',(0.657326160633901,0.322395819916145,0.681163162426516));
#127510=DIRECTION('ref_axis',(0.708559747616064,0.0434179749104281,-0.704313824593084));
#127511=DIRECTION('center_axis',(-0.691771073996284,0.239728027846425,-0.681163162426516));
#127512=DIRECTION('ref_axis',(-0.708559747616064,-0.0434179749104245,0.704313824593084));
#127513=DIRECTION('center_axis',(-0.691162873346186,0.239517260516214,-0.681854357192686));
#127514=DIRECTION('ref_axis',(-0.709225067557875,-0.043458743306661,0.703641344136154));
#127515=DIRECTION('center_axis',(-4.11377412892479E-32,-4.37356725940272E-32,
1.));
#127516=DIRECTION('ref_axis',(-0.0611616608218468,0.998127873193367,4.11377412892479E-32));
#127517=DIRECTION('center_axis',(5.49235531231428E-35,-4.12115352934861E-32,
1.));
#127518=DIRECTION('ref_axis',(-0.804667861133695,-0.593725216963643,-2.44241325155124E-32));
#127519=DIRECTION('center_axis',(-4.11377412892479E-32,-4.37356725940272E-32,
1.));
#127520=DIRECTION('ref_axis',(0.0611616608218468,-0.998127873193367,-4.11377412892479E-32));
#127521=DIRECTION('center_axis',(4.11377412892479E-32,4.37356725940272E-32,
-1.));
#127522=DIRECTION('ref_axis',(-0.0611616608218463,0.998127873193367,4.11377412892479E-32));
#127523=DIRECTION('center_axis',(0.249333011548091,0.968417807225972,5.57651287942261E-32));
#127524=DIRECTION('ref_axis',(-0.968417807225972,0.249333011548091,-2.7768288484926E-32));
#127525=DIRECTION('',(-4.07953925466218E-32,-4.70803927530955E-32,1.));
#127526=DIRECTION('',(-0.708695658143486,0.182463830587886,-0.681511125848849));
#127527=DIRECTION('center_axis',(-0.249337667204796,-0.968416608546297,
2.13514020965652E-6));
#127528=DIRECTION('ref_axis',(0.960221008293694,-0.247227264488722,0.129824092235863));
#127529=DIRECTION('',(3.90320862897581E-33,5.65788130115185E-32,-1.));
#127530=DIRECTION('center_axis',(0.512068097591086,-0.858944854708058,-1.95494420610757E-32));
#127531=DIRECTION('ref_axis',(0.858944854708058,0.512068097591086,5.9149359674635E-32));
#127532=DIRECTION('center_axis',(-0.512068097591103,0.858944854708047,4.5541059549879E-15));
#127533=DIRECTION('ref_axis',(0.852501356187244,0.508226745016147,-0.122257978672975));
#127534=DIRECTION('',(0.628582502897165,0.374735403179052,0.681511125848852));
#127535=DIRECTION('',(-4.07953925466218E-32,-4.70803927530955E-32,1.));
#127536=DIRECTION('',(-8.0736155217068E-33,-2.75729959521182E-32,1.));
#127537=DIRECTION('center_axis',(-4.07953925466218E-32,-4.70803927530955E-32,
1.));
#127538=DIRECTION('ref_axis',(-0.142314838273288,0.989821441880932,4.07953925466219E-32));
#127539=DIRECTION('center_axis',(0.336215887827956,0.048340546765909,-0.940543496235252));
#127540=DIRECTION('ref_axis',(0.930987077227732,0.133735305678126,0.33967326955494));
#127541=DIRECTION('center_axis',(0.336215887827956,0.048340546765909,-0.940543496235252));
#127542=DIRECTION('ref_axis',(0.930987077227732,0.133735305678126,0.33967326955494));
#127543=DIRECTION('center_axis',(-0.630644991066351,-0.375964975004635,
-0.678923583927297));
#127544=DIRECTION('ref_axis',(-0.700524277354892,-0.100720185500151,0.706485089063614));
#127545=DIRECTION('center_axis',(0.711021011464223,-0.183062526049729,0.678923583927297));
#127546=DIRECTION('ref_axis',(0.700524277354892,0.100720185500147,-0.706485089063614));
#127547=DIRECTION('center_axis',(-0.225438372144987,-0.97395443471759,-0.0242960790778839));
#127548=DIRECTION('ref_axis',(-0.66712375661312,0.172495421980205,-0.724700781535572));
#127549=DIRECTION('center_axis',(4.07953925466218E-32,4.70803927530955E-32,
-1.));
#127550=DIRECTION('ref_axis',(0.142314838273279,-0.989821441880933,-4.07953925466223E-32));
#127551=DIRECTION('center_axis',(5.44664787004251E-35,-4.12070697124994E-32,
1.));
#127552=DIRECTION('ref_axis',(-0.908263721405877,0.418398150543173,1.72904316836497E-32));
#127553=DIRECTION('center_axis',(-4.07953925466218E-32,-4.70803927530955E-32,
1.));
#127554=DIRECTION('ref_axis',(-0.142314838273279,0.989821441880933,4.07953925466223E-32));
#127555=DIRECTION('center_axis',(0.628307819494939,0.374571648071316,0.681854357192688));
#127556=DIRECTION('ref_axis',(0.703322888621748,0.101122565053646,-0.703641344136153));
#127557=DIRECTION('center_axis',(0.62886070976005,0.374901258831168,0.681163162426516));
#127558=DIRECTION('ref_axis',(0.702663105479923,0.101027702559117,-0.704313824593084));
#127559=DIRECTION('center_axis',(-0.70900932261057,0.182544587989916,-0.681163162426516));
#127560=DIRECTION('ref_axis',(-0.702663105479923,-0.101027702559114,0.704313824593084));
#127561=DIRECTION('center_axis',(-0.708385966203883,0.182384095969852,-0.681854357192686));
#127562=DIRECTION('ref_axis',(-0.703322888621744,-0.101122565053659,0.703641344136155));
#127563=DIRECTION('center_axis',(-4.07953925466218E-32,-4.70803927530955E-32,
1.));
#127564=DIRECTION('ref_axis',(-0.142314838273279,0.989821441880933,4.07953925466223E-32));
#127565=DIRECTION('center_axis',(5.44664787004251E-35,-4.12070697124994E-32,
1.));
#127566=DIRECTION('ref_axis',(-0.753596278147675,-0.657337546137426,-2.70459083526957E-32));
#127567=DIRECTION('center_axis',(-4.07953925466218E-32,-4.70803927530955E-32,
1.));
#127568=DIRECTION('ref_axis',(0.142314838273299,-0.989821441880931,-4.07953925466213E-32));
#127569=DIRECTION('center_axis',(4.07953925466218E-32,4.70803927530955E-32,
-1.));
#127570=DIRECTION('ref_axis',(-0.142314838273289,0.989821441880932,4.07953925466218E-32));
#127571=DIRECTION('center_axis',(0.169568334879484,0.98551843199719,5.64699293479589E-32));
#127572=DIRECTION('ref_axis',(-0.98551843199719,0.169568334879484,-3.10557817219554E-32));
#127573=DIRECTION('',(-4.01815571973639E-32,-5.03860790310199E-32,1.));
#127574=DIRECTION('',(-0.721210027908761,0.124091421895619,-0.68151112584885));
#127575=DIRECTION('center_axis',(-0.169573072748393,-0.985517616785266,
2.13514019657982E-6));
#127576=DIRECTION('ref_axis',(0.977177269309663,-0.168137709729232,0.129824092184458));
#127577=DIRECTION('',(2.63791954821996E-33,5.68458385999837E-32,-1.));
#127578=DIRECTION('center_axis',(0.580376212952687,-0.814348482800022,-1.77114070164052E-32));
#127579=DIRECTION('ref_axis',(0.814348482800022,0.580376212952687,6.19646718737737E-32));
#127580=DIRECTION('center_axis',(-0.580376212952658,0.814348482800042,-1.36623178649604E-14));
#127581=DIRECTION('ref_axis',(0.808239530379992,0.576022437209787,-0.12225797872543));
#127582=DIRECTION('',(0.595946532240335,0.424723811499838,0.681511125848852));
#127583=DIRECTION('',(-4.01815571973639E-32,-5.03860790310199E-32,1.));
#127584=DIRECTION('',(-9.15869312325864E-33,-2.82764628819632E-32,1.));
#127585=DIRECTION('center_axis',(-4.01815571973639E-32,-5.03860790310199E-32,
1.));
#127586=DIRECTION('ref_axis',(-0.222520933956323,0.974927912181822,4.01815571973636E-32));
#127587=DIRECTION('center_axis',(0.331156953864098,0.0755844137184014,-0.940543496235181));
#127588=DIRECTION('ref_axis',(0.916988625578409,0.209174402137411,0.339673269555138));
#127589=DIRECTION('center_axis',(0.331156953864098,0.0755844137184014,-0.940543496235181));
#127590=DIRECTION('ref_axis',(0.916988625578409,0.209174402137411,0.339673269555138));
#127591=DIRECTION('center_axis',(-0.59790193613171,-0.426117403959597,-0.678923583927297));
#127592=DIRECTION('ref_axis',(-0.68998371045233,-0.157484279346259,0.706485089063615));
#127593=DIRECTION('center_axis',(0.723576443046309,-0.124498587364537,0.678923583927297));
#127594=DIRECTION('ref_axis',(0.689983710452334,0.157484279346249,-0.706485089063614));
#127595=DIRECTION('center_axis',(-0.145301916380709,-0.989089001878846,
-0.0242960790746493));
#127596=DIRECTION('ref_axis',(-0.678963644165877,0.117544642290695,-0.724701060417153));
#127597=DIRECTION('center_axis',(4.01815571973639E-32,5.03860790310199E-32,
-1.));
#127598=DIRECTION('ref_axis',(0.222520933956312,-0.974927912181824,-4.01815571973642E-32));
#127599=DIRECTION('center_axis',(5.36469388482745E-35,-4.12026562461737E-32,
1.));
#127600=DIRECTION('ref_axis',(-0.939344882287572,0.342974040009076,1.41818344493129E-32));
#127601=DIRECTION('center_axis',(-4.01815571973639E-32,-5.03860790310199E-32,
1.));
#127602=DIRECTION('ref_axis',(-0.222520933956312,0.974927912181824,4.01815571973642E-32));
#127603=DIRECTION('center_axis',(0.595686110385981,0.424538212026394,0.681854357192688));
#127604=DIRECTION('ref_axis',(0.692740211901949,0.158113432814265,-0.703641344136153));
#127605=DIRECTION('center_axis',(0.596210294617459,0.424911791723024,0.681163162426516));
#127606=DIRECTION('ref_axis',(0.692090356308065,0.157965107515673,-0.704313824593084));
#127607=DIRECTION('center_axis',(-0.721529231161188,0.124146344018072,-0.681163162426516));
#127608=DIRECTION('ref_axis',(-0.692090356308066,-0.157965107515671,0.704313824593084));
#127609=DIRECTION('center_axis',(-0.720894867331949,0.124037195356069,-0.681854357192686));
#127610=DIRECTION('ref_axis',(-0.692740211901944,-0.158113432814279,0.703641344136154));
#127611=DIRECTION('center_axis',(-4.01815571973639E-32,-5.03860790310199E-32,
1.));
#127612=DIRECTION('ref_axis',(-0.222520933956312,0.974927912181824,4.01815571973642E-32));
#127613=DIRECTION('center_axis',(5.36469388482745E-35,-4.12026562461737E-32,
1.));
#127614=DIRECTION('ref_axis',(-0.697509636265204,-0.71657540239474,-2.94873907225313E-32));
#127615=DIRECTION('center_axis',(-4.01815571973639E-32,-5.03860790310199E-32,
1.));
#127616=DIRECTION('ref_axis',(0.222520933956312,-0.974927912181824,-4.01815571973642E-32));
#127617=DIRECTION('center_axis',(4.01815571973639E-32,5.03860790310199E-32,
-1.));
#127618=DIRECTION('ref_axis',(-0.222520933956318,0.974927912181823,4.01815571973639E-32));
#127619=DIRECTION('center_axis',(0.088675208919059,0.996060594202562,5.69044235175751E-32));
#127620=DIRECTION('ref_axis',(-0.996060594202562,0.088675208919059,-3.4389783884616E-32));
#127621=DIRECTION('',(-3.93003202144478E-32,-5.36307326310205E-32,1.));
#127622=DIRECTION('',(-0.728924863929587,0.0648932052642835,-0.681511125848845));
#127623=DIRECTION('center_axis',(-0.0886799974704105,-0.996060167883491,
2.13514018734458E-6));
#127624=DIRECTION('ref_axis',(0.987630576850999,-0.0879292262537851,0.129824091906604));
#127625=DIRECTION('',(1.35507554809678E-33,5.70088428763789E-32,-1.));
#127626=DIRECTION('center_axis',(0.644822020372422,-0.764332756096995,-1.56500138014056E-32));
#127627=DIRECTION('ref_axis',(0.764332756096995,0.644822020372422,6.46207994341911E-32));
#127628=DIRECTION('center_axis',(-0.644822020372427,0.76433275609699,-1.04311924108636E-15));
#127629=DIRECTION('ref_axis',(0.758599003860373,0.639984795129837,-0.122257978654446));
#127630=DIRECTION('',(0.559344635735712,0.471885752929584,0.681511125848847));
#127631=DIRECTION('',(-3.93003202144478E-32,-5.36307326310205E-32,1.));
#127632=DIRECTION('',(-1.01828211331532E-32,-2.90660329815266E-32,1.));
#127633=DIRECTION('center_axis',(-3.93003202144478E-32,-5.36307326310205E-32,
1.));
#127634=DIRECTION('ref_axis',(-0.301246189537239,0.953546398078926,3.93003202144478E-32));
#127635=DIRECTION('center_axis',(0.323894225008962,0.102325278868066,-0.940543496235244));
#127636=DIRECTION('ref_axis',(0.896887765918468,0.283221477461758,0.339673269554964));
#127637=DIRECTION('center_axis',(0.323894225008962,0.102325278868066,-0.940543496235244));
#127638=DIRECTION('ref_axis',(0.896887765918468,0.283221477461758,0.339673269554964));
#127639=DIRECTION('center_axis',(-0.561179942458989,-0.473434091895631,
-0.678923583927297));
#127640=DIRECTION('ref_axis',(-0.674851415796016,-0.213200341296378,0.706485089063613));
#127641=DIRECTION('center_axis',(0.731316592781633,-0.0651061311212549,
0.678923583927297));
#127642=DIRECTION('ref_axis',(0.674851415796015,0.213200341296374,-0.706485089063615));
#127643=DIRECTION('center_axis',(-0.0641985003308254,-0.997641344921486,
-0.0242960790771001));
#127644=DIRECTION('ref_axis',(-0.686286248571427,0.0618117157998334,-0.724700280675838));
#127645=DIRECTION('center_axis',(3.93003202144478E-32,5.36307326310205E-32,
-1.));
#127646=DIRECTION('ref_axis',(0.301246189537229,-0.953546398078929,-3.93003202144483E-32));
#127647=DIRECTION('center_axis',(5.24703874692283E-35,-4.11983242653993E-32,
1.));
#127648=DIRECTION('ref_axis',(-0.964174857958642,0.265267493825445,1.09791668560757E-32));
#127649=DIRECTION('center_axis',(-3.93003202144478E-32,-5.36307326310205E-32,
1.));
#127650=DIRECTION('ref_axis',(-0.301246189537229,0.953546398078929,3.93003202144483E-32));
#127651=DIRECTION('center_axis',(0.559100208493694,0.471679544224312,0.681854357192688));
#127652=DIRECTION('ref_axis',(0.677547463366034,0.214052081766382,-0.703641344136152));
#127653=DIRECTION('center_axis',(0.559592198331965,0.472094606746474,0.681163162426516));
#127654=DIRECTION('ref_axis',(0.676911860001846,0.213851280744125,-0.704313824593085));
#127655=DIRECTION('center_axis',(-0.729247481722371,0.0649219266094926,
-0.681163162426516));
#127656=DIRECTION('ref_axis',(-0.676911860001849,-0.21385128074412,0.704313824593084));
#127657=DIRECTION('center_axis',(-0.728606332057203,0.0648648476718873,
-0.681854357192686));
#127658=DIRECTION('ref_axis',(-0.677547463366027,-0.214052081766397,0.703641344136154));
#127659=DIRECTION('center_axis',(-3.93003202144478E-32,-5.36307326310205E-32,
1.));
#127660=DIRECTION('ref_axis',(-0.301246189537229,0.953546398078929,3.93003202144483E-32));
#127661=DIRECTION('center_axis',(5.24703874692283E-35,-4.11983242653993E-32,
1.));
#127662=DIRECTION('ref_axis',(-0.63678118283439,-0.771044567575724,-3.17323319626628E-32));
#127663=DIRECTION('center_axis',(-3.93003202144478E-32,-5.36307326310205E-32,
1.));
#127664=DIRECTION('ref_axis',(0.301246189537247,-0.953546398078924,-3.93003202144473E-32));
#127665=DIRECTION('center_axis',(3.93003202144478E-32,5.36307326310205E-32,
-1.));
#127666=DIRECTION('ref_axis',(-0.301246189537238,0.953546398078926,3.93003202144478E-32));
#127667=DIRECTION('center_axis',(0.00719196407365769,0.999974137491947,
5.70657198160623E-32));
#127668=DIRECTION('ref_axis',(-0.999974137491947,0.00719196407365769,-3.77481077385869E-32));
#127669=DIRECTION('',(-3.8157546084601E-32,-5.67927609187195E-32,1.));
#127670=DIRECTION('',(-0.731788825245097,0.00526313505853439,-0.681511125848842));
#127671=DIRECTION('center_axis',(-0.00719677144045609,-0.999974102902808,
2.13514018812815E-6));
#127672=DIRECTION('ref_axis',(0.991511365803085,-0.00713558827868622,0.129824091998437));
#127673=DIRECTION('',(6.32137437727758E-35,5.70667410741387E-32,-1.));
#127674=DIRECTION('center_axis',(0.704976643634723,-0.70923052100817,-1.33789806478166E-32));
#127675=DIRECTION('ref_axis',(0.70923052100817,0.704976643634723,6.7100066265203E-32));
#127676=DIRECTION('center_axis',(-0.704976643634742,0.709230521008152,5.59722519607366E-15));
#127677=DIRECTION('ref_axis',(0.703910126118507,0.699688159818815,-0.122257978705639));
#127678=DIRECTION('',(0.519020392965623,0.515907372529259,0.68151112584885));
#127679=DIRECTION('',(-3.8157546084601E-32,-5.67927609187195E-32,1.));
#127680=DIRECTION('',(-1.11391841484539E-32,-2.99364517920656E-32,1.));
#127681=DIRECTION('center_axis',(-3.8157546084601E-32,-5.67927609187195E-32,
1.));
#127682=DIRECTION('ref_axis',(-0.377966701428907,0.925819190020898,3.81575460846012E-32));
#127683=DIRECTION('center_axis',(0.314476033525515,0.12838518616945,-0.940543496235179));
#127684=DIRECTION('ref_axis',(0.870818266152426,0.355383760581436,0.339673269555142));
#127685=DIRECTION('center_axis',(0.314476033525515,0.12838518616945,-0.940543496235179));
#127686=DIRECTION('ref_axis',(0.870818266152426,0.355383760581436,0.339673269555142));
#127687=DIRECTION('center_axis',(-0.520723388857375,-0.517600154061226,
-0.678923583927297));
#127688=DIRECTION('ref_axis',(-0.655228096310218,-0.267497590150762,0.706485089063614));
#127689=DIRECTION('center_axis',(0.734189951250739,-0.00528040431711646,
0.678923583927297));
#127690=DIRECTION('ref_axis',(0.655228096310221,0.267497590150755,-0.706485089063614));
#127691=DIRECTION('center_axis',(0.0173321461446417,-0.999554549412633,
-0.0242960790772608));
#127692=DIRECTION('ref_axis',(-0.689040598198203,0.00566735485295386,-0.724700583084927));
#127693=DIRECTION('center_axis',(3.8157546084601E-32,5.67927609187195E-32,
-1.));
#127694=DIRECTION('ref_axis',(0.377966701428909,-0.925819190020897,-3.81575460846011E-32));
#127695=DIRECTION('center_axis',(5.09446543185543E-35,-4.11941025987936E-32,
1.));
#127696=DIRECTION('ref_axis',(-0.982588409027649,0.185795636236468,7.70374212836853E-33));
#127697=DIRECTION('center_axis',(-3.8157546084601E-32,-5.67927609187195E-32,
1.));
#127698=DIRECTION('ref_axis',(-0.377966701428909,0.925819190020897,3.81575460846011E-32));
#127699=DIRECTION('center_axis',(0.518793586958923,0.515681926877064,0.681854357192688));
#127700=DIRECTION('ref_axis',(0.657845748248879,0.268566249430454,-0.703641344136152));
#127701=DIRECTION('center_axis',(0.519250108292784,0.516135710052153,0.681163162426516));
#127702=DIRECTION('ref_axis',(0.657228626949917,0.268314308982192,-0.704313824593083));
#127703=DIRECTION('center_axis',(-0.732112710610057,0.00526546449069082,
-0.681163162426516));
#127704=DIRECTION('ref_axis',(-0.657228626949916,-0.268314308982189,0.704313824593084));
#127705=DIRECTION('center_axis',(-0.731469041854199,0.00526083512839615,
-0.681854357192686));
#127706=DIRECTION('ref_axis',(-0.657845748248872,-0.268566249430465,0.703641344136155));
#127707=DIRECTION('center_axis',(-3.8157546084601E-32,-5.67927609187195E-32,
1.));
#127708=DIRECTION('ref_axis',(-0.377966701428909,0.925819190020897,3.81575460846011E-32));
#127709=DIRECTION('center_axis',(5.09446543185543E-35,-4.11941025987936E-32,
1.));
#127710=DIRECTION('ref_axis',(-0.571815055693287,-0.820382558372911,-3.37657923595281E-32));
#127711=DIRECTION('center_axis',(-3.8157546084601E-32,-5.67927609187195E-32,
1.));
#127712=DIRECTION('ref_axis',(0.377966701428889,-0.925819190020905,-3.81575460846024E-32));
#127713=DIRECTION('center_axis',(3.8157546084601E-32,5.67927609187195E-32,
-1.));
#127714=DIRECTION('ref_axis',(-0.37796670142891,0.925819190020897,3.8157546084601E-32));
#127715=DIRECTION('center_axis',(-0.0743391421060632,0.997233017880442,
5.69527448431661E-32));
#127716=DIRECTION('ref_axis',(-0.997233017880442,-0.0743391421060632,-4.11084041927044E-32));
#127717=DIRECTION('',(-3.67608397811132E-32,-5.98511211175602E-32,1.));
#127718=DIRECTION('',(-0.729782852665248,-0.0544019604426628,-0.68151112584885));
#127719=DIRECTION('center_axis',(0.0743343479160154,-0.997233375251421,
2.13514020042163E-6));
#127720=DIRECTION('ref_axis',(0.988793810213182,0.0737055358578386,0.129824092016876));
#127721=DIRECTION('',(-1.22906873758652E-33,5.70191478903094E-32,-1.));
#127722=DIRECTION('center_axis',(0.760439763646594,-0.649408473816836,-1.09134209065814E-32));
#127723=DIRECTION('ref_axis',(0.649408473816836,0.760439763646594,6.93859732550991E-32));
#127724=DIRECTION('center_axis',(-0.760439763646603,0.649408473816825,4.04526730079985E-15));
#127725=DIRECTION('ref_axis',(0.644536842633876,0.754735215254185,-0.122257978646687));
#127726=DIRECTION('',(0.475242155112692,0.556495713683474,0.681511125848848));
#127727=DIRECTION('',(-3.67608397811132E-32,-5.98511211175602E-32,1.));
#127728=DIRECTION('',(-1.20214177310826E-32,-3.08819268200052E-32,1.));
#127729=DIRECTION('center_axis',(-3.67608397811132E-32,-5.98511211175602E-32,
1.));
#127730=DIRECTION('ref_axis',(-0.452171907282689,0.891930808002692,3.67608397811132E-32));
#127731=DIRECTION('center_axis',(0.302965055923512,0.153590711238812,-0.940543496235245));
#127732=DIRECTION('ref_axis',(0.838953614500091,0.425181023408944,0.339673269554959));
#127733=DIRECTION('center_axis',(0.302965055923512,0.153590711238812,-0.940543496235245));
#127734=DIRECTION('ref_axis',(0.838953614500091,0.425181023408944,0.339673269554959));
#127735=DIRECTION('center_axis',(-0.476801507016228,-0.558321672599558,
-0.678923583927297));
#127736=DIRECTION('ref_axis',(-0.631244341948508,-0.320014686676681,0.706485089063613));
#127737=DIRECTION('center_axis',(0.732177396727087,0.054580462706547,0.678923583927297));
#127738=DIRECTION('ref_axis',(0.631244341948508,0.320014686676676,-0.706485089063615));
#127739=DIRECTION('center_axis',(0.0987474500471282,-0.994815883292307,
-0.0242960790774368));
#127740=DIRECTION('ref_axis',(-0.687209671238742,-0.0505146907306731,-0.724700720143374));
#127741=DIRECTION('center_axis',(3.67608397811132E-32,5.98511211175602E-32,
-1.));
#127742=DIRECTION('ref_axis',(0.452171907282684,-0.891930808002695,-3.67608397811135E-32));
#127743=DIRECTION('center_axis',(4.90798928986703E-35,-4.11900193408512E-32,
1.));
#127744=DIRECTION('ref_axis',(-0.994462996350253,0.105087339342457,4.37735767734696E-33));
#127745=DIRECTION('center_axis',(-3.67608397811132E-32,-5.98511211175602E-32,
1.));
#127746=DIRECTION('ref_axis',(-0.452171907282684,0.891930808002695,3.67608397811135E-32));
#127747=DIRECTION('center_axis',(0.475034479697857,0.556252531387978,0.681854357192688));
#127748=DIRECTION('ref_axis',(0.633766178214038,0.321293153014877,-0.703641344136152));
#127749=DIRECTION('center_axis',(0.475452494453153,0.556742015363834,0.681163162426516));
#127750=DIRECTION('ref_axis',(0.633171645820719,0.320991749762738,-0.704313824593084));
#127751=DIRECTION('center_axis',(-0.730105850198729,-0.0544260384255558,
-0.681163162426516));
#127752=DIRECTION('ref_axis',(-0.633171645820721,-0.320991749762735,0.704313824593083));
#127753=DIRECTION('center_axis',(-0.729463945861553,-0.0543781874048979,
-0.681854357192686));
#127754=DIRECTION('ref_axis',(-0.633766178214029,-0.321293153014888,0.703641344136155));
#127755=DIRECTION('center_axis',(-3.67608397811132E-32,-5.98511211175602E-32,
1.));
#127756=DIRECTION('ref_axis',(-0.452171907282684,0.891930808002695,3.67608397811135E-32));
#127757=DIRECTION('center_axis',(4.90798928986703E-35,-4.11900193408512E-32,
1.));
#127758=DIRECTION('ref_axis',(-0.503043593699408,-0.864261038597706,-3.55742395696816E-32));
#127759=DIRECTION('center_axis',(-3.67608397811132E-32,-5.98511211175602E-32,
1.));
#127760=DIRECTION('ref_axis',(0.4521719072827,-0.891930808002687,-3.67608397811125E-32));
#127761=DIRECTION('center_axis',(3.67608397811132E-32,5.98511211175602E-32,
-1.));
#127762=DIRECTION('ref_axis',(-0.452171907282689,0.891930808002692,3.67608397811132E-32));
#127763=DIRECTION('center_axis',(-0.155375533560164,0.98785547706681,5.65662504286916E-32));
#127764=DIRECTION('ref_axis',(-0.98785547706681,-0.155375533560164,-4.44483110284763E-32));
#127765=DIRECTION('',(-3.51194961539937E-32,-6.27854603450134E-32,1.));
#127766=DIRECTION('',(-0.722920295606614,-0.113705019872821,-0.68151112584885));
#127767=DIRECTION('center_axis',(0.15537078445142,-0.987856224019666,2.13514022059604E-6));
#127768=DIRECTION('ref_axis',(0.979495994957281,0.154056161813633,0.129824092024161));
#127769=DIRECTION('',(-2.51317196927925E-33,5.68663800496771E-32,-1.));
#127770=DIRECTION('center_axis',(0.810842282495128,-0.585264720377106,-8.26974247098904E-33));
#127771=DIRECTION('ref_axis',(0.585264720377106,0.810842282495128,7.14633080700099E-32));
#127772=DIRECTION('center_axis',(-0.810842282495157,0.585264720377065,3.42448414268799E-14));
#127773=DIRECTION('ref_axis',(0.580874272795154,0.804759632346359,-0.122257978678096));
#127774=DIRECTION('',(0.428301259126908,0.593380667678461,0.681511125848852));
#127775=DIRECTION('',(-3.51194961539937E-32,-6.27854603450134E-32,1.));
#127776=DIRECTION('',(-1.28236507621053E-32,-3.18961660850267E-32,1.));
#127777=DIRECTION('center_axis',(-3.51194961539936E-32,-6.27854603450134E-32,
1.));
#127778=DIRECTION('ref_axis',(-0.523367983696617,0.852106773615454,3.51194961539936E-32));
#127779=DIRECTION('center_axis',(0.289437895860302,0.177774115465673,-0.940543496235213));
#127780=DIRECTION('ref_axis',(0.801505864960677,0.492148776675732,0.339673269555049));
#127781=DIRECTION('center_axis',(0.289437895860302,0.177774115465673,-0.940543496235213));
#127782=DIRECTION('ref_axis',(0.801505864960677,0.492148776675732,0.339673269555049));
#127783=DIRECTION('center_axis',(-0.429706589812599,-0.595327652523332,
-0.678923583927297));
#127784=DIRECTION('ref_axis',(-0.603059760639106,-0.370402138261486,0.706485089063615));
#127785=DIRECTION('center_axis',(0.725292322428983,0.114078105756041,0.678923583927297));
#127786=DIRECTION('ref_axis',(0.603059760639111,0.37040213826148,-0.706485089063613));
#127787=DIRECTION('center_axis',(0.179505605959122,-0.983456881602261,-0.0242960790746993));
#127788=DIRECTION('ref_axis',(-0.680805576941664,-0.106360566013795,-0.724700763351573));
#127789=DIRECTION('center_axis',(3.51194961539936E-32,6.27854603450134E-32,
-1.));
#127790=DIRECTION('ref_axis',(0.523367983696608,-0.852106773615459,-3.51194961539942E-32));
#127791=DIRECTION('center_axis',(4.6888512889172E-35,-4.11861016649801E-32,
1.));
#127792=DIRECTION('ref_axis',(-0.999719596506991,0.023679703543321,1.02215004271818E-33));
#127793=DIRECTION('center_axis',(-3.51194961539936E-32,-6.27854603450134E-32,
1.));
#127794=DIRECTION('ref_axis',(-0.523367983696608,0.852106773615459,3.51194961539942E-32));
#127795=DIRECTION('center_axis',(0.428114096349574,0.593121367077712,0.681854357192688));
#127796=DIRECTION('ref_axis',(0.605468998827241,0.371881903675627,-0.703641344136152));
#127797=DIRECTION('center_axis',(0.428490822707076,0.593643294419234,0.681163162426516));
#127798=DIRECTION('ref_axis',(0.604901011854561,0.371533043408514,-0.704313824593082));
#127799=DIRECTION('center_axis',(-0.723240255813313,-0.113755345035745,
-0.681163162426516));
#127800=DIRECTION('ref_axis',(-0.60490101185456,-0.37153304340851,0.704313824593085));
#127801=DIRECTION('center_axis',(-0.722604387662277,-0.113655332072782,
-0.681854357192686));
#127802=DIRECTION('ref_axis',(-0.60546899882723,-0.371881903675639,0.703641344136154));
#127803=DIRECTION('center_axis',(-3.51194961539936E-32,-6.27854603450134E-32,
1.));
#127804=DIRECTION('ref_axis',(-0.523367983696608,0.852106773615459,3.51194961539942E-32));
#127805=DIRECTION('center_axis',(4.6888512889172E-35,-4.11861016649801E-32,
1.));
#127806=DIRECTION('ref_axis',(-0.430924459585822,-0.902388004203661,-3.7145638675313E-32));
#127807=DIRECTION('center_axis',(-3.51194961539936E-32,-6.27854603450134E-32,
1.));
#127808=DIRECTION('ref_axis',(0.52336798369665,-0.852106773615433,-3.51194961539911E-32));
#127809=DIRECTION('center_axis',(3.51194961539936E-32,6.27854603450134E-32,
-1.));
#127810=DIRECTION('ref_axis',(-0.523367983696616,0.852106773615454,3.51194961539936E-32));
#127811=DIRECTION('center_axis',(-0.23537792647358,0.971903921037979,5.59088086291999E-32));
#127812=DIRECTION('ref_axis',(-0.971903921037979,-0.23537792647358,-4.77456017169564E-32));
#127813=DIRECTION('',(-3.32444380742783E-32,-6.5576251057652E-32,1.));
#127814=DIRECTION('',(-0.711246823254172,-0.172251391155723,-0.68151112584885));
#127815=DIRECTION('center_axis',(0.235373254050727,-0.971905052601854,2.13514020080356E-6));
#127816=DIRECTION('ref_axis',(0.963679795426648,0.233381569421748,0.129824092296828));
#127817=DIRECTION('',(-3.78055045616061E-33,5.66094541970164E-32,-1.));
#127818=DIRECTION('center_axis',(0.855848779733215,-0.517226126785149,-5.46553858485233E-33));
#127819=DIRECTION('ref_axis',(0.517226126785149,0.855848779733215,7.33182463894781E-32));
#127820=DIRECTION('center_axis',(-0.855848779733223,0.517226126785135,3.05303192513103E-16));
#127821=DIRECTION('ref_axis',(0.513346080509126,0.849428506860947,-0.122257978708549));
#127822=DIRECTION('',(0.378510088926399,0.626316771230954,0.681511125848847));
#127823=DIRECTION('',(-3.32444380742783E-32,-6.5576251057652E-32,1.));
#127824=DIRECTION('',(-1.35405445130596E-32,-3.29724199921591E-32,1.));
#127825=DIRECTION('center_axis',(-3.32444380742783E-32,-6.5576251057652E-32,
1.));
#127826=DIRECTION('ref_axis',(-0.591081132528682,0.806612109237526,3.32444380742781E-32));
#127827=DIRECTION('center_axis',(0.273984574353956,0.200774462284739,-0.940543496235212));
#127828=DIRECTION('ref_axis',(0.75872422612919,0.555841361032482,0.339673269555053));
#127829=DIRECTION('center_axis',(0.273984574353956,0.200774462284739,-0.940543496235212));
#127830=DIRECTION('ref_axis',(0.75872422612919,0.555841361032482,0.339673269555053));
#127831=DIRECTION('center_axis',(-0.379752046150365,-0.628371825141711,
-0.678923583927297));
#127832=DIRECTION('ref_axis',(-0.570861916120514,-0.418324624728203,0.706485089063615));
#127833=DIRECTION('center_axis',(0.713580547389924,0.172816577833291,0.678923583927297));
#127834=DIRECTION('ref_axis',(0.57086191612052,0.418324624728196,-0.706485089063614));
#127835=DIRECTION('center_axis',(0.2590691816723,-0.965553136626766,-0.0242960790634893));
#127836=DIRECTION('ref_axis',(-0.669870625097031,-0.161498560364775,-0.72470101464826));
#127837=DIRECTION('center_axis',(3.32444380742783E-32,6.5576251057652E-32,
-1.));
#127838=DIRECTION('ref_axis',(0.59108113252868,-0.806612109237527,-3.32444380742783E-32));
#127839=DIRECTION('center_axis',(4.43850975624469E-35,-4.11823756426669E-32,
1.));
#127840=DIRECTION('ref_axis',(-0.998323227691098,-0.0578855167760327,-2.33955242228056E-33));
#127841=DIRECTION('center_axis',(-3.32444380742783E-32,-6.5576251057652E-32,
1.));
#127842=DIRECTION('ref_axis',(-0.59108113252868,0.806612109237527,3.32444380742783E-32));
#127843=DIRECTION('center_axis',(0.378344684323938,0.626043077927682,0.681854357192688));
#127844=DIRECTION('ref_axis',(0.573142523148597,0.419995841623614,-0.703641344136153));
#127845=DIRECTION('center_axis',(0.378677615231892,0.626593975294525,0.681163162426516));
#127846=DIRECTION('ref_axis',(0.572604861456137,0.41960184594906,-0.704313824593086));
#127847=DIRECTION('center_axis',(-0.711561616851703,-0.172327628593032,
-0.681163162426516));
#127848=DIRECTION('ref_axis',(-0.572604861456143,-0.419601845949057,0.704313824593082));
#127849=DIRECTION('center_axis',(-0.710936016484441,-0.172176119257531,
-0.681854357192686));
#127850=DIRECTION('ref_axis',(-0.573142523148589,-0.419995841623623,0.703641344136154));
#127851=DIRECTION('center_axis',(-3.32444380742783E-32,-6.5576251057652E-32,
1.));
#127852=DIRECTION('ref_axis',(-0.59108113252868,0.806612109237527,3.32444380742783E-32));
#127853=DIRECTION('center_axis',(4.43850975624469E-35,-4.11823756426669E-32,
1.));
#127854=DIRECTION('ref_axis',(-0.355937594291196,-0.934509726525196,-3.84695322746377E-32));
#127855=DIRECTION('center_axis',(-3.32444380742783E-32,-6.5576251057652E-32,
1.));
#127856=DIRECTION('ref_axis',(0.591081132528663,-0.80661210923754,-3.32444380742797E-32));
#127857=DIRECTION('center_axis',(3.32444380742783E-32,6.5576251057652E-32,
-1.));
#127858=DIRECTION('ref_axis',(-0.59108113252868,0.806612109237527,3.32444380742783E-32));
#127859=DIRECTION('center_axis',(-0.313813918120938,0.9494845047675,5.49847946113966E-32));
#127860=DIRECTION('ref_axis',(-0.9494845047675,-0.313813918120938,-5.09783333326273E-32));
#127861=DIRECTION('',(-3.11481437441248E-32,-6.82049210037316E-32,1.));
#127862=DIRECTION('',(-0.694840120640444,-0.229651457849954,-0.681511125848848));
#127863=DIRECTION('center_axis',(0.31380935347816,-0.949486013412025,2.13514018838833E-6));
#127864=DIRECTION('ref_axis',(0.941450465909118,0.311153861202889,0.129824092132539));
#127865=DIRECTION('',(-5.02277000350315E-33,5.62500801314868E-32,-1.));
#127866=DIRECTION('center_axis',(0.895159744547287,-0.44574547865574,-2.51947076237234E-33));
#127867=DIRECTION('ref_axis',(0.44574547865574,0.895159744547288,7.4938443905031E-32));
#127868=DIRECTION('center_axis',(-0.895159744547308,0.445745478655699,2.32539264964185E-14));
#127869=DIRECTION('ref_axis',(0.442401654758204,0.888444574816553,-0.122257978660848));
#127870=DIRECTION('',(0.326199996533836,0.655084840005904,0.681511125848848));
#127871=DIRECTION('',(-3.11481437441248E-32,-6.82049210037316E-32,1.));
#127872=DIRECTION('',(-1.41673281743121E-32,-3.41035262492199E-32,1.));
#127873=DIRECTION('center_axis',(-3.11481437441248E-32,-6.82049210037316E-32,
1.));
#127874=DIRECTION('ref_axis',(-0.654860733945287,0.755749574354256,3.1148143744125E-32));
#127875=DIRECTION('center_axis',(0.256707930709546,0.222438688182747,-0.940543496235215));
#127876=DIRECTION('ref_axis',(0.710893402753043,0.615834912839461,0.339673269555044));
#127877=DIRECTION('center_axis',(0.256707930709546,0.222438688182747,-0.940543496235215));
#127878=DIRECTION('ref_axis',(0.710893402753043,0.615834912839461,0.339673269555044));
#127879=DIRECTION('center_axis',(-0.327270315275677,-0.657234286937827,
-0.678923583927297));
#127880=DIRECTION('ref_axis',(-0.534865079735733,-0.463463229836053,0.706485089063613));
#127881=DIRECTION('center_axis',(0.697120011540489,0.230404984097789,0.678923583927297));
#127882=DIRECTION('ref_axis',(0.534865079735735,0.463463229836049,-0.706485089063615));
#127883=DIRECTION('center_axis',(0.336908694744834,-0.941223794826141,-0.0242960790748523));
#127884=DIRECTION('ref_axis',(-0.654478525247296,-0.215562043042521,-0.724700535110509));
#127885=DIRECTION('center_axis',(3.11481437441248E-32,6.82049210037316E-32,
-1.));
#127886=DIRECTION('ref_axis',(0.654860733945285,-0.755749574354258,-3.11481437441251E-32));
#127887=DIRECTION('center_axis',(4.1586306734472E-35,-4.11788660699752E-32,
1.));
#127888=DIRECTION('ref_axis',(-0.990283182506659,-0.139065518531672,-5.68537814238565E-33));
#127889=DIRECTION('center_axis',(-3.11481437441248E-32,-6.82049210037316E-32,
1.));
#127890=DIRECTION('ref_axis',(-0.654860733945285,0.755749574354258,3.11481437441251E-32));
#127891=DIRECTION('center_axis',(0.326057450846606,0.65479857538388,0.681854357192688));
#127892=DIRECTION('ref_axis',(0.537001878540266,0.465314776540025,-0.703641344136153));
#127893=DIRECTION('center_axis',(0.32634437070475,0.655374776644959,0.681163162426516));
#127894=DIRECTION('ref_axis',(0.536498120177896,0.464878267434227,-0.704313824593083));
#127895=DIRECTION('center_axis',(-0.695147652729348,-0.22975310021409,-0.681163162426516));
#127896=DIRECTION('ref_axis',(-0.536498120177896,-0.464878267434224,0.704313824593084));
#127897=DIRECTION('center_axis',(-0.694536483413087,-0.229551102775682,
-0.681854357192686));
#127898=DIRECTION('ref_axis',(-0.537001878540256,-0.465314776540035,0.703641344136155));
#127899=DIRECTION('center_axis',(-3.11481437441248E-32,-6.82049210037316E-32,
1.));
#127900=DIRECTION('ref_axis',(-0.654860733945285,0.755749574354258,3.11481437441251E-32));
#127901=DIRECTION('center_axis',(4.1586306734472E-35,-4.11788660699752E-32,
1.));
#127902=DIRECTION('ref_axis',(-0.278582023032155,-0.960412440799947,-3.95371100741784E-32));
#127903=DIRECTION('center_axis',(-3.11481437441248E-32,-6.82049210037316E-32,
1.));
#127904=DIRECTION('ref_axis',(0.654860733945243,-0.755749574354294,-3.11481437441289E-32));
#127905=DIRECTION('center_axis',(3.11481437441248E-32,6.82049210037316E-32,
-1.));
#127906=DIRECTION('ref_axis',(-0.654860733945289,0.755749574354255,3.11481437441248E-32));
#127907=DIRECTION('center_axis',(-0.390161529918854,0.92074642577171,5.38003575361184E-32));
#127908=DIRECTION('ref_axis',(-0.92074642577171,-0.390161529918854,-5.41249925799502E-32));
#127909=DIRECTION('',(-2.88445636564362E-32,-7.06539768184611E-32,1.));
#127910=DIRECTION('',(-0.673809371664394,-0.285523231982033,-0.681511125848851));
#127911=DIRECTION('center_axis',(0.390157103433078,-0.920748301457109,2.13514019164445E-6));
#127912=DIRECTION('ref_axis',(0.912955938858505,0.386855475373679,0.129824092049167));
#127913=DIRECTION('',(-6.23156384517107E-33,5.57906494282019E-32,-1.));
#127914=DIRECTION('center_axis',(0.928513568952359,-0.371298467908706,5.48855401159282E-34));
#127915=DIRECTION('ref_axis',(0.371298467908706,0.928513568952359,7.63131184695165E-32));
#127916=DIRECTION('center_axis',(-0.928513568952349,0.371298467908731,-1.56722305490052E-14));
#127917=DIRECTION('ref_axis',(0.368513118979584,0.921548190696015,-0.122257978736933));
#127918=DIRECTION('',(0.271719096983559,0.679493427252001,0.681511125848851));
#127919=DIRECTION('',(-2.88445636564362E-32,-7.06539768184611E-32,1.));
#127920=DIRECTION('',(-1.46998306040091E-32,-3.52819575306877E-32,1.));
#127921=DIRECTION('center_axis',(-2.88445636564362E-32,-7.06539768184611E-32,
1.));
#127922=DIRECTION('ref_axis',(-0.714282345221906,0.69985765074356,2.88445636564363E-32));
#127923=DIRECTION('center_axis',(0.237722938140168,0.242622621310774,-0.94054349623518));
#127924=DIRECTION('ref_axis',(0.658331701071381,0.671730184906247,0.339673269555142));
#127925=DIRECTION('center_axis',(0.237722938140168,0.242622621310774,-0.94054349623518));
#127926=DIRECTION('ref_axis',(0.658331701071381,0.671730184906247,0.339673269555142));
#127927=DIRECTION('center_axis',(-0.27261065444863,-0.681722962990395,-0.678923583927297));
#127928=DIRECTION('ref_axis',(-0.495308804491826,-0.505517563615405,0.706485089063614));
#127929=DIRECTION('center_axis',(0.676020257030958,0.286460083207263,0.678923583927297));
#127930=DIRECTION('ref_axis',(0.495308804491831,0.505517563615401,-0.706485089063614));
#127931=DIRECTION('center_axis',(0.412506136031845,-0.910630763963938,-0.0242960790773052));
#127932=DIRECTION('ref_axis',(-0.63473071784112,-0.268190961384672,-0.724700299475902));
#127933=DIRECTION('center_axis',(2.88445636564362E-32,7.06539768184611E-32,
-1.));
#127934=DIRECTION('ref_axis',(0.714282345221904,-0.699857650743561,-2.88445636564365E-32));
#127935=DIRECTION('center_axis',(3.85107658964331E-35,-4.11755963025323E-32,
1.));
#127936=DIRECTION('ref_axis',(-0.975652966127864,-0.219320062205675,-8.99306119945245E-33));
#127937=DIRECTION('center_axis',(-2.88445636564362E-32,-7.06539768184611E-32,
1.));
#127938=DIRECTION('ref_axis',(-0.714282345221904,0.699857650743561,2.88445636564365E-32));
#127939=DIRECTION('center_axis',(0.271600358829583,0.679196496355059,0.681854357192688));
#127940=DIRECTION('ref_axis',(0.497287575029324,0.507537118390098,-0.703641344136152));
#127941=DIRECTION('center_axis',(0.271839358233598,0.679794166986047,0.681163162426516));
#127942=DIRECTION('ref_axis',(0.496821072425813,0.507061000749148,-0.704313824593084));
#127943=DIRECTION('center_axis',(-0.674107595669369,-0.285649602859816,
-0.681163162426516));
#127944=DIRECTION('ref_axis',(-0.496821072425817,-0.507061000749145,0.704313824593083));
#127945=DIRECTION('center_axis',(-0.673514924635072,-0.285398461578126,
-0.681854357192686));
#127946=DIRECTION('ref_axis',(-0.497287575029312,-0.507537118390104,0.703641344136156));
#127947=DIRECTION('center_axis',(-2.88445636564362E-32,-7.06539768184611E-32,
1.));
#127948=DIRECTION('ref_axis',(-0.714282345221904,0.699857650743561,2.88445636564365E-32));
#127949=DIRECTION('center_axis',(3.85107658964331E-35,-4.11755963025323E-32,
1.));
#127950=DIRECTION('ref_axis',(-0.199372534372617,-0.979923768738079,-4.03412675198177E-32));
#127951=DIRECTION('center_axis',(-2.88445636564362E-32,-7.06539768184611E-32,
1.));
#127952=DIRECTION('ref_axis',(0.714282345221909,-0.699857650743556,-2.8844563656436E-32));
#127953=DIRECTION('center_axis',(2.88445636564362E-32,7.06539768184611E-32,
-1.));
#127954=DIRECTION('ref_axis',(-0.714282345221907,0.699857650743558,2.88445636564362E-32));
#127955=DIRECTION('center_axis',(-0.463912681107281,0.885880931224876,5.2363379636683E-32));
#127956=DIRECTION('ref_axis',(-0.885880931224876,-0.463912681107281,-5.71646389607962E-32));
#127957=DIRECTION('',(-2.6349027756632E-32,-7.29071204394592E-32,1.));
#127958=DIRECTION('',(-0.648294532490652,-0.339494896113273,-0.681511125848848));
#127959=DIRECTION('center_axis',(0.463908422236103,-0.885883161468741,2.13514017017263E-6));
#127960=DIRECTION('ref_axis',(0.878385840636379,0.459982630171223,0.129824092179707));
#127961=DIRECTION('',(-7.39888765758507E-33,5.52342195226914E-32,-1.));
#127962=DIRECTION('center_axis',(0.955688288750009,-0.294380527117673,3.71902070136243E-33));
#127963=DIRECTION('ref_axis',(0.294380527117673,0.955688288750009,7.74331218505131E-32));
#127964=DIRECTION('center_axis',(-0.955688288750012,0.294380527117663,1.47563209714676E-15));
#127965=DIRECTION('ref_axis',(0.292172189203034,0.948519055433948,-0.122257978614886));
#127966=DIRECTION('',(0.215429951673331,0.699380097848275,0.681511125848847));
#127967=DIRECTION('',(-2.6349027756632E-32,-7.29071204394592E-32,1.));
#127968=DIRECTION('',(-1.51345080863378E-32,-3.64998715708118E-32,1.));
#127969=DIRECTION('center_axis',(-2.6349027756632E-32,-7.29071204394592E-32,
1.));
#127970=DIRECTION('ref_axis',(-0.768950525339364,0.639308289935549,2.63490277566321E-32));
#127971=DIRECTION('center_axis',(0.217155938638854,0.26119194092375,-0.940543496235215));
#127972=DIRECTION('ref_axis',(0.601388910536204,0.723155203420306,0.339673269555043));
#127973=DIRECTION('center_axis',(0.217155938638854,0.26119194092375,-0.940543496235215));
#127974=DIRECTION('ref_axis',(0.601388910536204,0.723155203420306,0.339673269555043));
#127975=DIRECTION('center_axis',(-0.21613681469382,-0.701674885200634,-0.678923583927297));
#127976=DIRECTION('ref_axis',(-0.452456330874236,-0.544207761413417,0.706485089063613));
#127977=DIRECTION('center_axis',(0.650421699246377,0.340608837725579,0.678923583927297));
#127978=DIRECTION('ref_axis',(0.45245633087424,0.544207761413411,-0.706485089063615));
#127979=DIRECTION('center_axis',(0.485358417045744,-0.87397763560859,-0.0242960790842656));
#127980=DIRECTION('ref_axis',(-0.610758275705588,-0.319034804460315,-0.724700712156478));
#127981=DIRECTION('center_axis',(2.6349027756632E-32,7.29071204394592E-32,
-1.));
#127982=DIRECTION('ref_axis',(0.768950525339369,-0.639308289935542,-2.63490277566315E-32));
#127983=DIRECTION('center_axis',(3.51789422651897E-35,-4.1172588100101E-32,
1.));
#127984=DIRECTION('ref_axis',(-0.954529940230895,-0.298115067050969,-1.22405895084658E-32));
#127985=DIRECTION('center_axis',(-2.6349027756632E-32,-7.29071204394592E-32,
1.));
#127986=DIRECTION('ref_axis',(-0.768950525339369,0.639308289935542,2.63490277566315E-32));
#127987=DIRECTION('center_axis',(0.215335811235453,0.69907447670253,0.681854357192688));
#127988=DIRECTION('ref_axis',(0.454263904753227,0.54638188445502,-0.703641344136153));
#127989=DIRECTION('center_axis',(0.215525299683739,0.699689639303987,0.681163162426516));
#127990=DIRECTION('ref_axis',(0.453837762406455,0.545869326763252,-0.704313824593083));
#127991=DIRECTION('center_axis',(-0.648581463780135,-0.339645154527377,
-0.681163162426516));
#127992=DIRECTION('ref_axis',(-0.453837762406457,-0.545869326763248,0.704313824593085));
#127993=DIRECTION('center_axis',(-0.648011235155752,-0.3393465407062,-0.681854357192686));
#127994=DIRECTION('ref_axis',(-0.454263904753214,-0.54638188445503,0.703641344136153));
#127995=DIRECTION('center_axis',(-2.6349027756632E-32,-7.29071204394592E-32,
1.));
#127996=DIRECTION('ref_axis',(-0.768950525339369,0.639308289935542,2.63490277566315E-32));
#127997=DIRECTION('center_axis',(3.51789422651897E-35,-4.1172588100101E-32,
1.));
#127998=DIRECTION('ref_axis',(-0.118836254390997,-0.992913865671297,-4.08766530764311E-32));
#127999=DIRECTION('center_axis',(-2.6349027756632E-32,-7.29071204394592E-32,
1.));
#128000=DIRECTION('ref_axis',(0.768950525339356,-0.639308289935559,-2.63490277566331E-32));
#128001=DIRECTION('center_axis',(2.6349027756632E-32,7.29071204394592E-32,
-1.));
#128002=DIRECTION('ref_axis',(-0.768950525339365,0.639308289935547,2.6349027756632E-32));
#128003=DIRECTION('center_axis',(-0.534576569943144,0.845120045240807,5.06834237639265E-32));
#128004=DIRECTION('ref_axis',(-0.845120045240807,-0.534576569943144,-6.00770441300072E-32));
#128005=DIRECTION('',(-2.3678143424391E-32,-7.49493575676706E-32,1.));
#128006=DIRECTION('',(-0.618465400164238,-0.391207277723611,-0.681511125848852));
#128007=DIRECTION('center_axis',(0.534572507028513,-0.845122615201304,2.13514020294021E-6));
#128008=DIRECTION('ref_axis',(0.837970229577547,0.530048676459173,0.129824092238814));
#128009=DIRECTION('',(-8.51697309336836E-33,5.4584493364172E-32,-1.));
#128010=DIRECTION('center_axis',(0.976503060663496,-0.215503532488041,6.96992821120469E-33));
#128011=DIRECTION('ref_axis',(0.215503532488041,0.976503060663496,7.82910006103078E-32));
#128012=DIRECTION('center_axis',(-0.97650306066349,0.215503532488069,-1.70588158816704E-14));
#128013=DIRECTION('ref_axis',(0.213886901704482,0.969177682327868,-0.122257978704212));
#128014=DIRECTION('',(0.157707155578177,0.714612509282951,0.681511125848848));
#128015=DIRECTION('',(-2.3678143424391E-32,-7.49493575676706E-32,1.));
#128016=DIRECTION('',(-1.54684679143701E-32,-3.7749163352597E-32,1.));
#128017=DIRECTION('center_axis',(-2.36781434243909E-32,-7.49493575676706E-32,
1.));
#128018=DIRECTION('ref_axis',(-0.818501466578596,0.574504437936459,2.3678143424391E-32));
#128019=DIRECTION('center_axis',(0.195143802194235,0.278023071263677,-0.940543496235177));
#128020=DIRECTION('ref_axis',(0.540443976022996,0.769767743368199,0.33967326955515));
#128021=DIRECTION('center_axis',(0.195143802194235,0.278023071263677,-0.940543496235177));
#128022=DIRECTION('ref_axis',(0.540443976022996,0.769767743368199,0.33967326955515));
#128023=DIRECTION('center_axis',(-0.158224620097287,-0.716957276818071,
-0.678923583927297));
#128024=DIRECTION('ref_axis',(-0.406592835024712,-0.579276346347187,0.706485089063613));
#128025=DIRECTION('center_axis',(0.620494692365338,0.392490896625334,0.678923583927297));
#128026=DIRECTION('ref_axis',(0.406592835024718,0.57927634634718,-0.706485089063615));
#128027=DIRECTION('center_axis',(0.5549807178787,-0.83150833027891,-0.0242960790997562));
#128028=DIRECTION('ref_axis',(-0.582721524349687,-0.367755567997614,-0.724700950231424));
#128029=DIRECTION('center_axis',(2.36781434243909E-32,7.49493575676706E-32,
-1.));
#128030=DIRECTION('ref_axis',(0.818501466578592,-0.574504437936465,-2.36781434243915E-32));
#128031=DIRECTION('center_axis',(3.1613008577281E-35,-4.11698614817723E-32,
1.));
#128032=DIRECTION('ref_axis',(-0.927054675068042,-0.374926165310569,-1.54063513043337E-32));
#128033=DIRECTION('center_axis',(-2.3678143424391E-32,-7.49493575676706E-32,
1.));
#128034=DIRECTION('ref_axis',(-0.818501466578592,0.574504437936465,2.36781434243915E-32));
#128035=DIRECTION('center_axis',(0.15763823934546,0.714300231746714,0.681854357192688));
#128036=DIRECTION('ref_axis',(0.408217183139275,0.581590569225554,-0.703641344136152));
#128037=DIRECTION('center_axis',(0.157776955823656,0.714928792513023,0.681163162426516));
#128038=DIRECTION('ref_axis',(0.407834236956233,0.581044982469851,-0.704313824593084));
#128039=DIRECTION('center_axis',(-0.618739129257853,-0.391380423729065,
-0.681163162426516));
#128040=DIRECTION('ref_axis',(-0.407834236956234,-0.581044982469851,0.704313824593083));
#128041=DIRECTION('center_axis',(-0.618195137820799,-0.391036324594112,
-0.681854357192686));
#128042=DIRECTION('ref_axis',(-0.408217183139263,-0.58159056922556,0.703641344136155));
#128043=DIRECTION('center_axis',(-2.36781434243909E-32,-7.49493575676706E-32,
1.));
#128044=DIRECTION('ref_axis',(-0.818501466578592,0.574504437936465,2.36781434243915E-32));
#128045=DIRECTION('center_axis',(3.1613008577281E-35,-4.11698614817723E-32,
1.));
#128046=DIRECTION('ref_axis',(-0.0375091387429898,-0.999296284647731,-4.1139703841472E-32));
#128047=DIRECTION('center_axis',(-2.3678143424391E-32,-7.49493575676706E-32,
1.));
#128048=DIRECTION('ref_axis',(0.818501466578589,-0.57450443793647,-2.3678143424392E-32));
#128049=DIRECTION('center_axis',(2.36781434243909E-32,7.49493575676706E-32,
-1.));
#128050=DIRECTION('ref_axis',(-0.818501466578597,0.574504437936459,2.36781434243909E-32));
#128051=DIRECTION('center_axis',(-0.601682939904961,0.798735024790652,4.87716697470088E-32));
#128052=DIRECTION('ref_axis',(-0.798735024790652,-0.601682939904961,-6.2842826511695E-32));
#128053=DIRECTION('',(-2.08496849542793E-32,-7.67670974519526E-32,1.));
#128054=DIRECTION('',(-0.584520482639347,-0.440316239445355,-0.681511125848849));
#128055=DIRECTION('center_axis',(0.601679099984979,-0.798737917365081,2.13514018879469E-6));
#128056=DIRECTION('ref_axis',(0.791978064924971,0.596587336277332,0.129824092029237));
#128057=DIRECTION('',(-9.57837947841694E-33,5.38457947730313E-32,-1.));
#128058=DIRECTION('center_axis',(0.990819365819932,-0.135192397405281,1.02799436775701E-32));
#128059=DIRECTION('ref_axis',(0.135192397405281,0.990819365819932,7.88810457072945E-32));
#128060=DIRECTION('center_axis',(-0.990819365819942,0.135192397405208,3.91233320239215E-14));
#128061=DIRECTION('ref_axis',(0.134178232167426,0.983386591662394,-0.12225797868051));
#128062=DIRECTION('',(0.0989348443824835,0.725089292371126,0.681511125848841));
#128063=DIRECTION('',(-2.08496849542793E-32,-7.67670974519526E-32,1.));
#128064=DIRECTION('',(-1.56994876405497E-32,-3.90215190453539E-32,1.));
#128065=DIRECTION('center_axis',(-2.08496849542793E-32,-7.67670974519526E-32,
1.));
#128066=DIRECTION('ref_axis',(-0.862605415600981,0.505877353689468,2.08496849542797E-32));
#128067=DIRECTION('center_axis',(0.171833015942407,0.293004003934834,-0.940543496235178));
#128068=DIRECTION('ref_axis',(0.475902476016994,0.811257605986293,0.339673269555146));
#128069=DIRECTION('center_axis',(0.171833015942407,0.293004003934834,-0.940543496235178));
#128070=DIRECTION('ref_axis',(0.475902476016994,0.811257605986293,0.339673269555146));
#128071=DIRECTION('center_axis',(-0.099259466759231,-0.727468436047907,
-0.678923583927297));
#128072=DIRECTION('ref_axis',(-0.358023530941186,-0.610489942769888,0.706485089063615));
#128073=DIRECTION('center_axis',(0.586438395681026,0.441760993364488,0.678923583927297));
#128074=DIRECTION('ref_axis',(0.358023530941192,0.610489942769888,-0.706485089063612));
#128075=DIRECTION('center_axis',(0.620909713570593,-0.783505474221586,-0.0242960790765126));
#128076=DIRECTION('ref_axis',(-0.550807437478925,-0.414029407872834,-0.724700501058451));
#128077=DIRECTION('center_axis',(2.08496849542793E-32,7.67670974519526E-32,
-1.));
#128078=DIRECTION('ref_axis',(0.862605415600986,-0.505877353689459,-2.08496849542789E-32));
#128079=DIRECTION('center_axis',(2.78366955330785E-35,-4.11674345927412E-32,
1.));
#128080=DIRECTION('ref_axis',(-0.89341001399587,-0.449242191798477,-1.84692789646177E-32));
#128081=DIRECTION('center_axis',(-2.08496849542793E-32,-7.67670974519526E-32,
1.));
#128082=DIRECTION('ref_axis',(-0.862605415600986,0.505877353689459,2.08496849542789E-32));
#128083=DIRECTION('center_axis',(0.0988916109811012,0.724772436599867,0.681854357192688));
#128084=DIRECTION('ref_axis',(0.359453843522623,0.612928864713583,-0.703641344136152));
#128085=DIRECTION('center_axis',(0.0989786323539316,0.725410212562833,0.681163162426516));
#128086=DIRECTION('ref_axis',(0.359116641946984,0.612353879683786,-0.704313824593084));
#128087=DIRECTION('center_axis',(-0.584779187915131,-0.44051112078406,-0.681163162426516));
#128088=DIRECTION('ref_axis',(-0.359116641946989,-0.612353879683783,0.704313824593084));
#128089=DIRECTION('center_axis',(-0.584265053838666,-0.440123826258303,
-0.681854357192686));
#128090=DIRECTION('ref_axis',(-0.359453843522612,-0.612928864713587,0.703641344136155));
#128091=DIRECTION('center_axis',(-2.08496849542793E-32,-7.67670974519526E-32,
1.));
#128092=DIRECTION('ref_axis',(-0.862605415600986,0.505877353689459,2.08496849542789E-32));
#128093=DIRECTION('center_axis',(2.78366955330785E-35,-4.11674345927412E-32,
1.));
#128094=DIRECTION('ref_axis',(0.0440675940347559,-0.999028551722116,-4.11286692554992E-32));
#128095=DIRECTION('center_axis',(-2.08496849542793E-32,-7.67670974519526E-32,
1.));
#128096=DIRECTION('ref_axis',(0.862605415600975,-0.505877353689478,-2.08496849542806E-32));
#128097=DIRECTION('center_axis',(2.08496849542793E-32,7.67670974519526E-32,
-1.));
#128098=DIRECTION('ref_axis',(-0.862605415600984,0.505877353689463,2.08496849542793E-32));
#128099=DIRECTION('center_axis',(-0.664785209172408,0.747034554532518,4.66408399934953E-32));
#128100=DIRECTION('ref_axis',(-0.747034554532518,-0.664785209172408,-6.54435802804316E-32));
#128101=DIRECTION('',(-1.78824752707528E-32,-7.83482433332812E-32,1.));
#128102=DIRECTION('',(-0.546685677741588,-0.486494969240645,-0.681511125848848));
#128103=DIRECTION('center_axis',(0.664781617801125,-0.747037750471259,2.1351401964272E-6));
#128104=DIRECTION('ref_axis',(0.740715416865343,0.659155805762135,0.129824092325236));
#128105=DIRECTION('',(-1.0576043328358E-32,5.30230396665167E-32,-1.));
#128106=DIRECTION('center_axis',(0.998541931570525,-0.0539815792229644,
1.3627039493644E-32));
#128107=DIRECTION('ref_axis',(0.0539815792229644,0.998541931570525,7.9199330488703E-32));
#128108=DIRECTION('center_axis',(-0.998541931570525,0.0539815792229708,
-4.59862933722826E-15));
#128109=DIRECTION('ref_axis',(0.0535766286324845,0.991051225469743,-0.122257978714264));
#128110=DIRECTION('',(0.0395041381205371,0.730740725849866,0.681511125848848));
#128111=DIRECTION('',(-1.78824752707528E-32,-7.83482433332812E-32,1.));
#128112=DIRECTION('',(-1.58260298667146E-32,-4.03084713318713E-32,1.));
#128113=DIRECTION('center_axis',(-1.78824752707528E-32,-7.83482433332812E-32,
1.));
#128114=DIRECTION('ref_axis',(-0.900968867902422,0.433883739117552,1.78824752707527E-32));
#128115=DIRECTION('center_axis',(0.147378709319891,0.306035043301973,-0.940543496235215));
#128116=DIRECTION('ref_axis',(0.408193923551509,0.847348683084722,0.339673269555042));
#128117=DIRECTION('center_axis',(0.147378709319891,0.306035043301973,-0.940543496235215));
#128118=DIRECTION('ref_axis',(0.408193923551509,0.847348683084722,0.339673269555042));
#128119=DIRECTION('center_axis',(-0.0396337580465518,-0.733138412859687,
-0.678923583927297));
#128120=DIRECTION('ref_axis',(-0.307071639328989,-0.6376408293472,0.706485089063613));
#128121=DIRECTION('center_axis',(0.548479448228981,0.488091243578234,0.678923583927297));
#128122=DIRECTION('ref_axis',(0.307071639328996,0.637640829347195,-0.706485089063615));
#128123=DIRECTION('center_axis',(0.682706657579583,-0.73028851848977,-0.024296079077326));
#128124=DIRECTION('ref_axis',(-0.515227392569887,-0.457547641377844,-0.724700551824826));
#128125=DIRECTION('center_axis',(1.78824752707528E-32,7.83482433332812E-32,
-1.));
#128126=DIRECTION('ref_axis',(0.900968867902418,-0.433883739117559,-1.78824752707533E-32));
#128127=DIRECTION('center_axis',(2.3875133872833E-35,-4.11653235835539E-32,
1.));
#128128=DIRECTION('ref_axis',(-0.853819856682831,-0.520568585619714,-2.14089892110869E-32));
#128129=DIRECTION('center_axis',(-1.78824752707528E-32,-7.83482433332812E-32,
1.));
#128130=DIRECTION('ref_axis',(-0.900968867902418,0.433883739117559,1.78824752707533E-32));
#128131=DIRECTION('center_axis',(0.0394868752616308,0.730421400466483,0.681854357192688));
#128132=DIRECTION('ref_axis',(0.308298397883036,0.640188219733089,-0.703641344136153));
#128133=DIRECTION('center_axis',(0.039521622416217,0.731064147332297,0.681163162426516));
#128134=DIRECTION('ref_axis',(0.30800918493565,0.639587662859704,-0.704313824593085));
#128135=DIRECTION('center_axis',(-0.546927637558608,-0.486710289009456,
-0.681163162426516));
#128136=DIRECTION('ref_axis',(-0.308009184935655,-0.639587662859703,0.704313824593083));
#128137=DIRECTION('center_axis',(-0.546446782320186,-0.486282376474064,
-0.681854357192686));
#128138=DIRECTION('ref_axis',(-0.308298397883024,-0.640188219733093,0.703641344136155));
#128139=DIRECTION('center_axis',(-1.78824752707528E-32,-7.83482433332812E-32,
1.));
#128140=DIRECTION('ref_axis',(-0.900968867902418,0.433883739117559,1.78824752707533E-32));
#128141=DIRECTION('center_axis',(2.3875133872833E-35,-4.11653235835539E-32,
1.));
#128142=DIRECTION('ref_axis',(0.125351064244853,-0.992112448612899,-4.08436227518619E-32));
#128143=DIRECTION('center_axis',(-1.78824752707528E-32,-7.83482433332812E-32,
1.));
#128144=DIRECTION('ref_axis',(0.900968867902418,-0.433883739117559,-1.78824752707533E-32));
#128145=DIRECTION('center_axis',(1.78824752707528E-32,7.83482433332812E-32,
-1.));
#128146=DIRECTION('ref_axis',(-0.900968867902422,0.433883739117553,1.78824752707528E-32));
#128147=DIRECTION('center_axis',(-0.723463442554651,0.690362692565997,4.43051148238335E-32));
#128148=DIRECTION('ref_axis',(-0.690362692565997,-0.723463442554651,-6.78619978489802E-32));
#128149=DIRECTION('',(-1.47962606647001E-32,-7.96822729466869E-32,1.));
#128150=DIRECTION('',(-0.505212769855237,-0.529436155281667,-0.68151112584885));
#128151=DIRECTION('center_axis',(0.723460123632049,-0.690366170600603,2.13514018696377E-6));
#128152=DIRECTION('ref_axis',(0.68452342996416,0.717337702154071,0.129824092134003));
#128153=DIRECTION('',(-1.15033253548732E-32,5.2121703344117E-32,-1.));
#128154=DIRECTION('center_axis',(0.999619365514338,0.0275884774627474,1.69889412890025E-32));
#128155=DIRECTION('ref_axis',(-0.0275884774627475,0.999619365514338,7.92437368218264E-32));
#128156=DIRECTION('center_axis',(-0.999619365514337,-0.0275884774627805,
1.09002780451937E-14));
#128157=DIRECTION('ref_axis',(0.0273815185261964,-0.992120576893031,0.122257978670674));
#128158=DIRECTION('',(-0.0201894616628749,0.731529200361817,0.681511125848847));
#128159=DIRECTION('',(-1.47962606647001E-32,-7.96822729466869E-32,1.));
#128160=DIRECTION('',(-1.58472524752277E-32,-4.16014557570146E-32,1.));
#128161=DIRECTION('center_axis',(-1.47962606647001E-32,-7.96822729466869E-32,
1.));
#128162=DIRECTION('ref_axis',(-0.933336521037368,0.359002699847595,1.47962606647003E-32));
#128163=DIRECTION('center_axis',(0.121943621702684,0.317029469948265,-0.940543496235211));
#128164=DIRECTION('ref_axis',(0.337768907871411,0.877800794500173,0.339673269555054));
#128165=DIRECTION('center_axis',(0.121943621702684,0.317029469948265,-0.940543496235211));
#128166=DIRECTION('ref_axis',(0.337768907871411,0.877800794500173,0.339673269555054));
#128167=DIRECTION('center_axis',(0.0202557067868174,-0.733929474493211,
-0.678923583927297));
#128168=DIRECTION('ref_axis',(-0.254076236620299,-0.660548321408542,0.706485089063614));
#128169=DIRECTION('center_axis',(0.506870460541712,0.531173327095353,0.678923583927297));
#128170=DIRECTION('ref_axis',(0.254076236620306,0.66054832140854,-0.706485089063614));
#128171=DIRECTION('center_axis',(0.739960301410276,-0.672211613168882,-0.0242960790602786));
#128172=DIRECTION('ref_axis',(0.476218817981084,0.498021215428875,0.724700287279815));
#128173=DIRECTION('center_axis',(1.47962606647001E-32,7.96822729466869E-32,
-1.));
#128174=DIRECTION('ref_axis',(0.93333652103737,-0.35900269984759,-1.47962606646999E-32));
#128175=DIRECTION('center_axis',(1.97546871357812E-35,-4.11635425026281E-32,
1.));
#128176=DIRECTION('ref_axis',(-0.808547669093927,-0.588430681391426,-2.42059187570691E-32));
#128177=DIRECTION('center_axis',(-1.47962606647001E-32,-7.96822729466869E-32,
1.));
#128178=DIRECTION('ref_axis',(-0.933336521037369,0.359002699847592,1.47962606647E-32));
#128179=DIRECTION('center_axis',(-0.02018063909783,0.731209530424043,0.681854357192688));
#128180=DIRECTION('ref_axis',(0.255091277271195,0.663187227773891,-0.703641344136153));
#128181=DIRECTION('center_axis',(-0.0201983973980688,0.731852970818359,
0.681163162426516));
#128182=DIRECTION('ref_axis',(0.254851977616513,0.662565095663826,-0.704313824593084));
#128183=DIRECTION('center_axis',(-0.505436374010841,-0.52967048056304,-0.681163162426516));
#128184=DIRECTION('ref_axis',(-0.254851977616511,-0.662565095663829,0.704313824593082));
#128185=DIRECTION('center_axis',(-0.504991997622738,-0.529204797705336,
-0.681854357192686));
#128186=DIRECTION('ref_axis',(-0.255091277271183,-0.663187227773893,0.703641344136155));
#128187=DIRECTION('center_axis',(-1.47962606647001E-32,-7.96822729466869E-32,
1.));
#128188=DIRECTION('ref_axis',(-0.933336521037369,0.359002699847592,1.47962606647E-32));
#128189=DIRECTION('center_axis',(1.97546871357812E-35,-4.11635425026281E-32,
1.));
#128190=DIRECTION('ref_axis',(0.205800343803877,-0.978594000845195,-4.02864612680124E-32));
#128191=DIRECTION('center_axis',(-1.47962606647001E-32,-7.96822729466869E-32,
1.));
#128192=DIRECTION('ref_axis',(0.933336521037371,-0.359002699847589,-1.47962606646997E-32));
#128193=DIRECTION('center_axis',(1.47962606647001E-32,7.96822729466869E-32,
-1.));
#128194=DIRECTION('ref_axis',(-0.933336521037369,0.359002699847593,1.47962606647001E-32));
#128195=DIRECTION('center_axis',(-0.77732714608976,0.629096580782275,4.178003810366E-32));
#128196=DIRECTION('ref_axis',(-0.629096580782275,-0.77732714608976,-7.00819850474328E-32));
#128197=DIRECTION('',(-1.16115793851351E-32,-8.07603085451918E-32,1.));
#128198=DIRECTION('',(-0.460377754339743,-0.568854031060101,-0.681511125848851));
#128199=DIRECTION('center_axis',(0.777324121702722,-0.629100317766994,2.13514018757423E-6));
#128200=DIRECTION('ref_axis',(0.623776052559492,0.7707458344779,0.129824092094895));
#128201=DIRECTION('',(-1.23540546490668E-32,5.11477840503477E-32,-1.));
#128202=DIRECTION('center_axis',(0.994044497506239,0.108974937382723,2.03432761618721E-32));
#128203=DIRECTION('ref_axis',(-0.108974937382723,0.994044497506239,7.90139691898444E-32));
#128204=DIRECTION('center_axis',(-0.99404449750624,-0.108974937382713,-6.7166702352874E-15));
#128205=DIRECTION('ref_axis',(0.108157446196492,-0.986587529556189,0.122257978702698));
#128206=DIRECTION('',(-0.0797487039099568,0.727449468739176,0.681511125848855));
#128207=DIRECTION('',(-1.16115793851351E-32,-8.07603085451918E-32,1.));
#128208=DIRECTION('',(-1.57630142331307E-32,-4.28918677227618E-32,1.));
#128209=DIRECTION('center_axis',(-1.16115793851351E-32,-8.07603085451918E-32,
1.));
#128210=DIRECTION('ref_axis',(-0.959492973614498,0.281732556841428,1.16115793851355E-32));
#128211=DIRECTION('center_axis',(0.0956970194023197,0.325914117778219,-0.940543496235212));
#128212=DIRECTION('ref_axis',(0.265096095837727,0.902411286455005,0.33967326955505));
#128213=DIRECTION('center_axis',(0.0956970194023197,0.325914117778219,-0.940543496235212));
#128214=DIRECTION('ref_axis',(0.265096095837727,0.902411286455005,0.33967326955505));
#128215=DIRECTION('center_axis',(0.080010373233477,-0.729836356563822,-0.678923583927297));
#128216=DIRECTION('ref_axis',(-0.199389998476538,-0.67905997337371,0.706485089063613));
#128217=DIRECTION('center_axis',(0.461888333567277,0.570720539758084,0.678923583927297));
#128218=DIRECTION('ref_axis',(0.199389998476547,0.679059973373706,-0.706485089063615));
#128219=DIRECTION('center_axis',(0.792289631536735,-0.609661250450763,-0.0242960790704409));
#128220=DIRECTION('ref_axis',(0.434040406814599,0.535179691247669,0.724701057904752));
#128221=DIRECTION('center_axis',(1.16115793851351E-32,8.07603085451918E-32,
-1.));
#128222=DIRECTION('ref_axis',(0.959492973614501,-0.281732556841418,-1.16115793851346E-32));
#128223=DIRECTION('center_axis',(1.5502776215132E-35,-4.11621032027636E-32,
1.));
#128224=DIRECTION('ref_axis',(-0.757894730168191,-0.65237686806269,-2.68414544978957E-32));
#128225=DIRECTION('center_axis',(-1.16115793851351E-32,-8.07603085451918E-32,
1.));
#128226=DIRECTION('ref_axis',(-0.959492973614501,0.281732556841418,1.16115793851346E-32));
#128227=DIRECTION('center_axis',(-0.0797138546336661,0.727131581597711,
0.681854357192688));
#128228=DIRECTION('ref_axis',(0.200186566296209,0.681772834232049,-0.703641344136153));
#128229=DIRECTION('center_axis',(-0.0797840002101718,0.727771433530866,
0.681163162426516));
#128230=DIRECTION('ref_axis',(0.199998772433955,0.681133267071852,-0.704313824593083));
#128231=DIRECTION('center_axis',(-0.460581514785163,-0.569105802457955,
-0.681163162426516));
#128232=DIRECTION('ref_axis',(-0.19999877243396,-0.681133267071849,0.704313824593084));
#128233=DIRECTION('center_axis',(-0.460176574498925,-0.568605448320524,
-0.681854357192686));
#128234=DIRECTION('ref_axis',(-0.200186566296196,-0.681772834232052,0.703641344136154));
#128235=DIRECTION('center_axis',(-1.16115793851351E-32,-8.07603085451918E-32,
1.));
#128236=DIRECTION('ref_axis',(-0.959492973614501,0.281732556841418,1.16115793851346E-32));
#128237=DIRECTION('center_axis',(1.5502776215132E-35,-4.11621032027636E-32,
1.));
#128238=DIRECTION('ref_axis',(0.284880056029549,-0.958563171458512,-3.94608926217004E-32));
#128239=DIRECTION('center_axis',(-1.16115793851351E-32,-8.07603085451918E-32,
1.));
#128240=DIRECTION('ref_axis',(0.959492973614495,-0.281732556841437,-1.16115793851362E-32));
#128241=DIRECTION('center_axis',(1.16115793851351E-32,8.07603085451918E-32,
-1.));
#128242=DIRECTION('ref_axis',(-0.959492973614499,0.281732556841424,1.16115793851351E-32));
#128243=DIRECTION('center_axis',(-0.826017865717592,0.563643935047077,3.90824138019391E-32));
#128244=DIRECTION('ref_axis',(-0.563643935047077,-0.826017865717592,-7.2088768227256E-32));
#128245=DIRECTION('',(-8.34962496053772E-33,-8.15751759797513E-32,1.));
#128246=DIRECTION('',(-0.412479000826099,-0.60448627711615,-0.681511125848844));
#128247=DIRECTION('center_axis',(0.826015155992845,-0.563647906112989,2.13514022960205E-6));
#128248=DIRECTION('ref_axis',(0.558877548446757,0.819024780447331,0.129824091968115));
#128249=DIRECTION('',(-1.31225697478464E-32,5.01077630574236E-32,-1.));
#128250=DIRECTION('center_axis',(0.981854427373034,0.189636187074016,2.36677215671002E-32));
#128251=DIRECTION('ref_axis',(-0.189636187074016,0.981854427373034,7.85115566584388E-32));
#128252=DIRECTION('center_axis',(-0.981854427373031,-0.189636187074032,
7.88699913992152E-15));
#128253=DIRECTION('ref_axis',(0.188213603907529,-0.974488904990992,0.122257978690955));
#128254=DIRECTION('',(-0.138777231690123,0.718528680922799,0.681511125848851));
#128255=DIRECTION('',(-8.34962496053772E-33,-8.15751759797513E-32,1.));
#128256=DIRECTION('',(-1.55738757320265E-32,-4.41711197503839E-32,1.));
#128257=DIRECTION('center_axis',(-8.34962496053772E-33,-8.15751759797513E-32,
1.));
#128258=DIRECTION('ref_axis',(-0.979264158757423,0.202587530152072,8.34962496053749E-33));
#128259=DIRECTION('center_axis',(0.0688135692266905,0.332629860926233,-0.940543496235277));
#128260=DIRECTION('ref_axis',(0.190659113023962,0.921016380185944,0.339673269554872));
#128261=DIRECTION('center_axis',(0.0688135692266905,0.332629860926233,-0.940543496235277));
#128262=DIRECTION('ref_axis',(0.190659113023962,0.921016380185944,0.339673269554872));
#128263=DIRECTION('center_axis',(0.13923258384705,-0.720886298096023,-0.678923583927297));
#128264=DIRECTION('ref_axis',(-0.143376852789944,-0.693052593253087,0.706485089063614));
#128265=DIRECTION('center_axis',(0.413832415939163,0.606469701390985,0.678923583927297));
#128266=DIRECTION('ref_axis',(0.143376852789952,0.693052593253084,-0.706485089063615));
#128267=DIRECTION('center_axis',(0.839346404882638,-0.543053692697053,-0.0242960790804773));
#128268=DIRECTION('ref_axis',(0.388973769514727,0.568776775077145,0.724701584628009));
#128269=DIRECTION('center_axis',(8.34962496053772E-33,8.15751759797513E-32,
-1.));
#128270=DIRECTION('ref_axis',(0.979264158757421,-0.202587530152081,-8.34962496053827E-33));
#128271=DIRECTION('center_axis',(1.11476968765511E-35,-4.11610152622635E-32,
1.));
#128272=DIRECTION('ref_axis',(-0.702198126856995,-0.711981594311628,-2.92980573780462E-32));
#128273=DIRECTION('center_axis',(-8.34962496053772E-33,-8.15751759797513E-32,
1.));
#128274=DIRECTION('ref_axis',(-0.979264158757421,0.202587530152081,8.34962496053823E-33));
#128275=DIRECTION('center_axis',(-0.138716587618775,0.718214692064113,0.681854357192688));
#128276=DIRECTION('ref_axis',(0.143949646750982,0.695821354962993,-0.703641344136153));
#128277=DIRECTION('center_axis',(-0.138838653664309,0.71884669742706,0.681163162426516));
#128278=DIRECTION('ref_axis',(0.14381460841832,0.695168608966593,-0.704313824593084));
#128279=DIRECTION('center_axis',(-0.412661561569192,-0.60475381913336,-0.681163162426516));
#128280=DIRECTION('ref_axis',(-0.143814608418327,-0.695168608966591,0.704313824593084));
#128281=DIRECTION('center_axis',(-0.412298752195612,-0.604222123490434,
-0.681854357192686));
#128282=DIRECTION('ref_axis',(-0.143949646750973,-0.695821354962993,0.703641344136155));
#128283=DIRECTION('center_axis',(-8.34962496053772E-33,-8.15751759797513E-32,
1.));
#128284=DIRECTION('ref_axis',(-0.979264158757421,0.202587530152081,8.34962496053827E-33));
#128285=DIRECTION('center_axis',(1.11476968765511E-35,-4.11610152622635E-32,
1.));
#128286=DIRECTION('ref_axis',(0.362063938484242,-0.932153262317565,-3.83724108360582E-32));
#128287=DIRECTION('center_axis',(-8.34962496053772E-33,-8.15751759797513E-32,
1.));
#128288=DIRECTION('ref_axis',(0.979264158757421,-0.202587530152081,-8.34962496053827E-33));
#128289=DIRECTION('center_axis',(8.34962496053772E-33,8.15751759797513E-32,
-1.));
#128290=DIRECTION('ref_axis',(-0.979264158757422,0.202587530152075,8.34962496053772E-33));
#128291=DIRECTION('center_axis',(-0.869211572732429,0.494440331918844,3.62301941633223E-32));
#128292=DIRECTION('ref_axis',(-0.494440331918845,-0.869211572732429,-7.38689925774838E-32));
#128293=DIRECTION('',(-5.03210515941913E-33,-8.2121452442032E-32,1.));
#128294=DIRECTION('',(-0.361835267616208,-0.636095766731185,-0.681511125848854));
#128295=DIRECTION('center_axis',(0.869209195702802,-0.494444510639091,2.13514022868713E-6));
#128296=DIRECTION('ref_axis',(0.490259806413637,0.861853251561129,0.129824092481988));
#128297=DIRECTION('',(-1.38037563100257E-32,4.90085615334611E-32,-1.));
#128298=DIRECTION('center_axis',(0.963130278020239,0.269035439228099,2.694015386901E-32));
#128299=DIRECTION('ref_axis',(-0.269035439228099,0.963130278020239,7.77398427001138E-32));
#128300=DIRECTION('center_axis',(-0.963130278020243,-0.269035439228087,
-8.44672165952822E-15));
#128301=DIRECTION('ref_axis',(0.267017231139236,-0.955905217547563,0.122257978635677));
#128302=DIRECTION('',(-0.196882219890024,0.704826203283764,0.681511125848853));
#128303=DIRECTION('',(-5.03210515941913E-33,-8.2121452442032E-32,1.));
#128304=DIRECTION('',(-1.52810956574343E-32,-4.54306986286987E-32,1.));
#128305=DIRECTION('center_axis',(-5.03210515941913E-33,-8.2121452442032E-32,
1.));
#128306=DIRECTION('ref_axis',(-0.992518502491028,0.122094316874159,5.03210515941961E-33));
#128307=DIRECTION('center_axis',(0.0414721761013757,0.337132007230186,-0.940543496235215));
#128308=DIRECTION('ref_axis',(0.114953325269262,0.933492261863657,0.339673269555043));
#128309=DIRECTION('center_axis',(0.0414721761013757,0.337132007230186,-0.940543496235215));
#128310=DIRECTION('ref_axis',(0.114953325269262,0.933492261863657,0.339673269555043));
#128311=DIRECTION('center_axis',(0.19752822458688,-0.707138860252263,-0.678923583927297));
#128312=DIRECTION('ref_axis',(-0.0864095578035487,-0.702433062469993,0.706485089063614));
#128313=DIRECTION('center_axis',(0.363022511860516,0.638182907221586,0.678923583927297));
#128314=DIRECTION('ref_axis',(0.0864095578035559,0.702433062469992,-0.706485089063614));
#128315=DIRECTION('center_axis',(0.880817466376868,-0.472832202231631,-0.0242960790709246));
#128316=DIRECTION('ref_axis',(0.341319657785829,0.598590676133594,0.724700002521658));
#128317=DIRECTION('center_axis',(5.03210515941913E-33,8.2121452442032E-32,
-1.));
#128318=DIRECTION('ref_axis',(0.992518502491028,-0.122094316874158,-5.03210515941954E-33));
#128319=DIRECTION('center_axis',(6.71843145449713E-36,-4.11602859211924E-32,
1.));
#128320=DIRECTION('ref_axis',(-0.641828510866114,-0.766848200519103,-3.15593791106624E-32));
#128321=DIRECTION('center_axis',(-5.03210515941913E-33,-8.2121452442032E-32,
1.));
#128322=DIRECTION('ref_axis',(-0.992518502491028,0.122094316874158,5.03210515941954E-33));
#128323=DIRECTION('center_axis',(-0.196796184599907,0.704518202251912,0.681854357192688));
#128324=DIRECTION('ref_axis',(0.0867547660566476,0.7052392993791,-0.703641344136153));
#128325=DIRECTION('center_axis',(-0.196969358785076,0.705138155153233,0.681163162426516));
#128326=DIRECTION('ref_axis',(0.0866733819114015,0.704577718463409,-0.704313824593084));
#128327=DIRECTION('center_axis',(-0.361995413745342,-0.636377298919789,
-0.681163162426516));
#128328=DIRECTION('ref_axis',(-0.086673381911405,-0.704577718463409,0.704313824593084));
#128329=DIRECTION('center_axis',(-0.361677149720944,-0.635817800118149,
-0.681854357192686));
#128330=DIRECTION('ref_axis',(-0.0867547660566364,-0.7052392993791,0.703641344136155));
#128331=DIRECTION('center_axis',(-5.03210515941913E-33,-8.2121452442032E-32,
1.));
#128332=DIRECTION('ref_axis',(-0.992518502491028,0.122094316874158,5.03210515941954E-33));
#128333=DIRECTION('center_axis',(6.71843145449713E-36,-4.11602859211924E-32,
1.));
#128334=DIRECTION('ref_axis',(0.436838345164685,-0.899540027010349,-3.70282595777818E-32));
#128335=DIRECTION('center_axis',(-5.03210515941913E-33,-8.2121452442032E-32,
1.));
#128336=DIRECTION('ref_axis',(0.992518502491028,-0.122094316874158,-5.03210515941954E-33));
#128337=DIRECTION('center_axis',(5.03210515941913E-33,8.2121452442032E-32,
-1.));
#128338=DIRECTION('ref_axis',(-0.992518502491028,0.122094316874153,5.03210515941913E-33));
#128339=DIRECTION('center_axis',(-0.906620820140547,0.421946309958604,3.32423602389212E-32));
#128340=DIRECTION('ref_axis',(-0.421946309958604,-0.906620820140547,-7.54108109987818E-32));
#128341=DIRECTION('',(-1.68109752870352E-33,-8.23955025523068E-32,1.));
#128342=DIRECTION('',(-0.308783580398942,-0.663472143967058,-0.681511125848849));
#128343=DIRECTION('center_axis',(0.906618791624814,-0.421950668524419,2.13514018813373E-6));
#128344=DIRECTION('ref_axis',(0.418379466321284,0.898946231596081,0.12982409198574));
#128345=DIRECTION('',(-1.43930811514213E-32,4.78574944832467E-32,-1.));
#128346=DIRECTION('center_axis',(0.937996655572531,0.346644304921843,3.01387955705455E-32));
#128347=DIRECTION('ref_axis',(-0.346644304921843,0.937996655572531,7.67039629439384E-32));
#128348=DIRECTION('center_axis',(-0.937996655572521,-0.346644304921869,
1.02276569491927E-14));
#128349=DIRECTION('ref_axis',(0.3440439027509,-0.930960138587007,0.122257978643482));
#128350=DIRECTION('',(-0.253676989399839,0.686433223550012,0.681511125848854));
#128351=DIRECTION('',(-1.68109752870352E-33,-8.23955025523068E-32,1.));
#128352=DIRECTION('',(-1.48866224124453E-32,-4.66622220680871E-32,1.));
#128353=DIRECTION('center_axis',(-1.68109752870351E-33,-8.23955025523068E-32,
1.));
#128354=DIRECTION('ref_axis',(-0.999167799344583,0.040788586061579,1.68109752870351E-33));
#128355=DIRECTION('center_axis',(0.0138547924865009,0.339390595648716,-0.940543496235217));
#128356=DIRECTION('ref_axis',(0.038482542101349,0.939755906554042,0.339673269555038));
#128357=DIRECTION('center_axis',(0.0138547924865009,0.339390595648716,-0.940543496235217));
#128358=DIRECTION('ref_axis',(0.038482542101349,0.939755906554042,0.339673269555038));
#128359=DIRECTION('center_axis',(0.254509347581947,-0.688685529963223,-0.678923583927297));
#128360=DIRECTION('ref_axis',(-0.0288672214665463,-0.707138955549458,0.706485089063614));
#128361=DIRECTION('center_axis',(0.309796752859936,0.665649111097397,0.678923583927297));
#128362=DIRECTION('ref_axis',(0.028867221466551,0.707138955549458,-0.706485089063614));
#128363=DIRECTION('center_axis',(0.916426832965552,-0.399464091455001,-0.0242960790819855));
#128364=DIRECTION('ref_axis',(0.291392765240331,0.624418455476463,0.724701213484552));
#128365=DIRECTION('center_axis',(1.68109752870351E-33,8.23955025523068E-32,
-1.));
#128366=DIRECTION('ref_axis',(0.999167799344583,-0.0407885860615856,-1.68109752870405E-33));
#128367=DIRECTION('center_axis',(2.24445597957705E-36,-4.11599200331947E-32,
1.));
#128368=DIRECTION('ref_axis',(-0.577187632029668,-0.816611558473173,-3.36103709727063E-32));
#128369=DIRECTION('center_axis',(-1.68109752870351E-33,-8.23955025523068E-32,
1.));
#128370=DIRECTION('ref_axis',(-0.999167799344583,0.0407885860615856,1.68109752870405E-33));
#128371=DIRECTION('center_axis',(-0.253566135441612,0.686133260041045,0.681854357192688));
#128372=DIRECTION('ref_axis',(0.0289825467077354,0.709963992614134,-0.703641344136153));
#128373=DIRECTION('center_axis',(-0.253789265320785,0.686737034796468,0.681163162426516));
#128374=DIRECTION('ref_axis',(0.0289553583479641,0.709297979490992,-0.704313824593084));
#128375=DIRECTION('center_axis',(-0.308920246168057,-0.663765792776771,
-0.681163162426516));
#128376=DIRECTION('ref_axis',(-0.0289553583479713,-0.709297979490991,0.704313824593084));
#128377=DIRECTION('center_axis',(-0.308648645487412,-0.66318221418863,-0.681854357192686));
#128378=DIRECTION('ref_axis',(-0.0289825467077237,-0.709963992614133,0.703641344136154));
#128379=DIRECTION('center_axis',(-1.68109752870351E-33,-8.23955025523068E-32,
1.));
#128380=DIRECTION('ref_axis',(-0.999167799344583,0.0407885860615856,1.68109752870405E-33));
#128381=DIRECTION('center_axis',(2.24445597957705E-36,-4.11599200331947E-32,
1.));
#128382=DIRECTION('ref_axis',(0.508705664731289,-0.860940501237047,-3.54373839517265E-32));
#128383=DIRECTION('center_axis',(-1.68109752870351E-33,-8.23955025523068E-32,
1.));
#128384=DIRECTION('ref_axis',(0.999167799344584,-0.0407885860615658,-1.68109752870242E-33));
#128385=DIRECTION('center_axis',(1.68109752870351E-33,8.23955025523068E-32,
-1.));
#128386=DIRECTION('ref_axis',(-0.999167799344583,0.0407885860615791,1.68109752870351E-33));
#128387=DIRECTION('center_axis',(-0.937996655572535,0.34664430492183,3.01387955705449E-32));
#128388=DIRECTION('ref_axis',(-0.34664430492183,-0.937996655572535,-7.67039629439386E-32));
#128389=DIRECTION('',(1.68109752870407E-33,-8.23955025523068E-32,1.));
#128390=DIRECTION('',(-0.25367698939983,-0.686433223550014,-0.681511125848856));
#128391=DIRECTION('center_axis',(0.937994989070099,-0.346648814327739,2.13514018660772E-6));
#128392=DIRECTION('ref_axis',(0.343714879873078,0.930056872710369,0.129824092055537));
#128393=DIRECTION('',(-1.48866224124453E-32,4.66622220680869E-32,-1.));
#128394=DIRECTION('center_axis',(0.906620820140541,0.421946309958617,3.32423602389217E-32));
#128395=DIRECTION('ref_axis',(-0.421946309958617,0.906620820140541,7.54108109987816E-32));
#128396=DIRECTION('center_axis',(-0.906620820140535,-0.42194630995863,4.98661881104643E-15));
#128397=DIRECTION('ref_axis',(0.418781018951358,-0.89981967349873,0.12225797867911));
#128398=DIRECTION('',(-0.30878358039895,0.663472143967056,0.681511125848847));
#128399=DIRECTION('',(1.68109752870407E-33,-8.23955025523068E-32,1.));
#128400=DIRECTION('',(-1.43930811514212E-32,-4.78574944832469E-32,1.));
#128401=DIRECTION('center_axis',(1.68109752870407E-33,-8.23955025523068E-32,
1.));
#128402=DIRECTION('ref_axis',(-0.999167799344583,-0.0407885860615916,-1.68109752870399E-33));
#128403=DIRECTION('center_axis',(-0.0138547924865081,0.33939059564882,-0.940543496235179));
#128404=DIRECTION('ref_axis',(-0.0382443360354119,0.939765630735095,0.339673269555142));
#128405=DIRECTION('center_axis',(-0.0138547924865081,0.33939059564882,-0.940543496235179));
#128406=DIRECTION('ref_axis',(-0.0382443360354119,0.939765630735095,0.339673269555142));
#128407=DIRECTION('center_axis',(0.309796752859944,-0.665649111097393,-0.678923583927297));
#128408=DIRECTION('ref_axis',(0.0288672214665601,-0.707138955549458,0.706485089063614));
#128409=DIRECTION('center_axis',(0.254509347581939,0.688685529963227,0.678923583927297));
#128410=DIRECTION('ref_axis',(-0.0288672214665556,0.707138955549458,-0.706485089063614));
#128411=DIRECTION('center_axis',(0.945937530174914,-0.323437613069393,-0.0242960790778483));
#128412=DIRECTION('ref_axis',(0.23952750141689,0.646092673476846,0.724700512863433));
#128413=DIRECTION('center_axis',(-1.68109752870407E-33,8.23955025523068E-32,
-1.));
#128414=DIRECTION('ref_axis',(0.999167799344583,0.0407885860615856,1.68109752870349E-33));
#128415=DIRECTION('center_axis',(-2.24445597957774E-36,-4.11599200331947E-32,
1.));
#128416=DIRECTION('ref_axis',(-0.508705664731306,-0.860940501237037,-3.5437383951726E-32));
#128417=DIRECTION('center_axis',(1.68109752870407E-33,-8.23955025523068E-32,
1.));
#128418=DIRECTION('ref_axis',(-0.999167799344583,-0.0407885860615856,-1.68109752870349E-33));
#128419=DIRECTION('center_axis',(-0.30864864548742,0.663182214188625,0.681854357192688));
#128420=DIRECTION('ref_axis',(-0.028982546707734,0.709963992614134,-0.703641344136153));
#128421=DIRECTION('center_axis',(-0.308920246168066,0.663765792776767,0.681163162426516));
#128422=DIRECTION('ref_axis',(-0.028955358347981,0.709297979490991,-0.704313824593084));
#128423=DIRECTION('center_axis',(-0.253789265320776,-0.686737034796471,
-0.681163162426516));
#128424=DIRECTION('ref_axis',(0.0289553583479736,-0.709297979490991,0.704313824593084));
#128425=DIRECTION('center_axis',(-0.253566135441603,-0.68613326004105,-0.681854357192686));
#128426=DIRECTION('ref_axis',(0.0289825467077455,-0.709963992614132,0.703641344136154));
#128427=DIRECTION('center_axis',(1.68109752870407E-33,-8.23955025523068E-32,
1.));
#128428=DIRECTION('ref_axis',(-0.999167799344583,-0.0407885860615856,-1.68109752870349E-33));
#128429=DIRECTION('center_axis',(-2.24445597957774E-36,-4.11599200331947E-32,
1.));
#128430=DIRECTION('ref_axis',(0.577187632029642,-0.816611558473192,-3.3610370972707E-32));
#128431=DIRECTION('center_axis',(1.68109752870407E-33,-8.23955025523068E-32,
1.));
#128432=DIRECTION('ref_axis',(0.999167799344582,0.0407885860616053,1.68109752870512E-33));
#128433=DIRECTION('center_axis',(-1.68109752870407E-33,8.23955025523068E-32,
-1.));
#128434=DIRECTION('ref_axis',(-0.999167799344583,-0.0407885860615926,-1.68109752870407E-33));
#128435=DIRECTION('center_axis',(-0.963130278020243,0.269035439228086,2.69401538690095E-32));
#128436=DIRECTION('ref_axis',(-0.269035439228086,-0.963130278020243,-7.7739842700114E-32));
#128437=DIRECTION('',(5.03210515941968E-33,-8.2121452442032E-32,1.));
#128438=DIRECTION('',(-0.196882219890014,-0.704826203283771,-0.681511125848848));
#128439=DIRECTION('center_axis',(0.963128984621398,-0.269040069464747,2.13514019551156E-6));
#128440=DIRECTION('ref_axis',(0.266762927617273,0.95497813881199,0.129824091909976));
#128441=DIRECTION('',(-1.52810956574344E-32,4.54306986286985E-32,-1.));
#128442=DIRECTION('center_axis',(0.869211572732422,0.494440331918856,3.62301941633227E-32));
#128443=DIRECTION('ref_axis',(-0.494440331918856,0.869211572732422,7.38689925774835E-32));
#128444=DIRECTION('center_axis',(-0.869211572732398,-0.4944403319189,1.68425594536402E-14));
#128445=DIRECTION('ref_axis',(0.490731216567359,-0.86269105694913,0.122257978661159));
#128446=DIRECTION('',(-0.361835267616211,0.636095766731196,0.681511125848842));
#128447=DIRECTION('',(5.03210515941968E-33,-8.2121452442032E-32,1.));
#128448=DIRECTION('',(-1.38037563100256E-32,-4.90085615334613E-32,1.));
#128449=DIRECTION('center_axis',(5.03210515941968E-33,-8.2121452442032E-32,
1.));
#128450=DIRECTION('ref_axis',(-0.992518502491026,-0.122094316874172,-5.0321051594201E-33));
#128451=DIRECTION('center_axis',(-0.0414721761013823,0.337132007230191,
-0.940543496235213));
#128452=DIRECTION('ref_axis',(-0.114716704425453,0.933521369694099,0.339673269555049));
#128453=DIRECTION('center_axis',(-0.0414721761013823,0.337132007230191,
-0.940543496235213));
#128454=DIRECTION('ref_axis',(-0.114716704425453,0.933521369694099,0.339673269555049));
#128455=DIRECTION('center_axis',(0.363022511860524,-0.638182907221582,-0.678923583927297));
#128456=DIRECTION('ref_axis',(0.0864095578035654,-0.70243306246999,0.706485089063614));
#128457=DIRECTION('center_axis',(0.197528224586871,0.707138860252265,0.678923583927297));
#128458=DIRECTION('ref_axis',(-0.0864095578035587,0.702433062469992,-0.706485089063614));
#128459=DIRECTION('center_axis',(0.969153169190729,-0.245258710730287,-0.0242960790763212));
#128460=DIRECTION('ref_axis',(0.186067957636303,0.663466634656043,0.724700448350379));
#128461=DIRECTION('center_axis',(-5.03210515941968E-33,8.2121452442032E-32,
-1.));
#128462=DIRECTION('ref_axis',(0.992518502491028,0.122094316874159,5.03210515941902E-33));
#128463=DIRECTION('center_axis',(-6.7184314544985E-36,-4.11602859211924E-32,
1.));
#128464=DIRECTION('ref_axis',(-0.436838345164698,-0.899540027010343,-3.70282595777815E-32));
#128465=DIRECTION('center_axis',(5.03210515941968E-33,-8.2121452442032E-32,
1.));
#128466=DIRECTION('ref_axis',(-0.992518502491028,-0.122094316874159,-5.03210515941902E-33));
#128467=DIRECTION('center_axis',(-0.361677149720952,0.635817800118143,0.681854357192688));
#128468=DIRECTION('ref_axis',(-0.0867547660566466,0.7052392993791,-0.703641344136153));
#128469=DIRECTION('center_axis',(-0.361995413745351,0.636377298919785,0.681163162426516));
#128470=DIRECTION('ref_axis',(-0.0866733819114143,0.704577718463408,-0.704313824593084));
#128471=DIRECTION('center_axis',(-0.196969358785067,-0.705138155153235,
-0.681163162426516));
#128472=DIRECTION('ref_axis',(0.0866733819114115,-0.704577718463408,0.704313824593084));
#128473=DIRECTION('center_axis',(-0.196796184599898,-0.704518202251916,
-0.681854357192686));
#128474=DIRECTION('ref_axis',(0.0867547660566579,-0.705239299379098,0.703641344136154));
#128475=DIRECTION('center_axis',(5.03210515941968E-33,-8.2121452442032E-32,
1.));
#128476=DIRECTION('ref_axis',(-0.992518502491028,-0.122094316874159,-5.032105159419E-33));
#128477=DIRECTION('center_axis',(-6.7184314544985E-36,-4.11602859211924E-32,
1.));
#128478=DIRECTION('ref_axis',(0.641828510866092,-0.766848200519122,-3.15593791106632E-32));
#128479=DIRECTION('center_axis',(5.03210515941968E-33,-8.2121452442032E-32,
1.));
#128480=DIRECTION('ref_axis',(0.992518502491028,0.122094316874158,5.03210515941899E-33));
#128481=DIRECTION('center_axis',(-5.03210515941968E-33,8.2121452442032E-32,
-1.));
#128482=DIRECTION('ref_axis',(-0.992518502491027,-0.122094316874167,-5.03210515941968E-33));
#128483=DIRECTION('center_axis',(-0.981854427373037,0.189636187074003,2.36677215670997E-32));
#128484=DIRECTION('ref_axis',(-0.189636187074003,-0.981854427373037,-7.85115566584389E-32));
#128485=DIRECTION('',(8.34962496053827E-33,-8.15751759797512E-32,1.));
#128486=DIRECTION('',(-0.13877723169011,-0.718528680922806,-0.681511125848846));
#128487=DIRECTION('center_axis',(0.981853515685139,-0.189640907327967,2.13514020548389E-6));
#128488=DIRECTION('ref_axis',(0.18803571207698,0.973544182904009,0.129824092207375));
#128489=DIRECTION('',(-1.55738757320266E-32,4.41711197503837E-32,-1.));
#128490=DIRECTION('center_axis',(0.826017865717585,0.563643935047088,3.90824138019396E-32));
#128491=DIRECTION('ref_axis',(-0.563643935047088,0.826017865717585,7.20887682272556E-32));
#128492=DIRECTION('center_axis',(-0.82601786571759,-0.56364393504708,2.03535461675383E-16));
#128493=DIRECTION('ref_axis',(0.559415678899174,-0.819821373744855,0.122257978687999));
#128494=DIRECTION('',(-0.412479000826111,0.604486277116134,0.681511125848852));
#128495=DIRECTION('',(8.34962496053827E-33,-8.15751759797512E-32,1.));
#128496=DIRECTION('',(-1.31225697478463E-32,-5.01077630574238E-32,1.));
#128497=DIRECTION('center_axis',(8.34962496053827E-33,-8.15751759797512E-32,
1.));
#128498=DIRECTION('ref_axis',(-0.97926415875742,-0.202587530152084,-8.34962496053794E-33));
#128499=DIRECTION('center_axis',(-0.0688135692267322,0.332629860926406,
-0.940543496235213));
#128500=DIRECTION('ref_axis',(-0.190425652074282,0.921064677957996,0.339673269555049));
#128501=DIRECTION('center_axis',(-0.0688135692267322,0.332629860926406,
-0.940543496235213));
#128502=DIRECTION('ref_axis',(-0.190425652074282,0.921064677957996,0.339673269555049));
#128503=DIRECTION('center_axis',(0.41383241593917,-0.606469701390979,-0.678923583927297));
#128504=DIRECTION('ref_axis',(0.143376852789961,-0.693052593253083,0.706485089063614));
#128505=DIRECTION('center_axis',(0.139232583847041,0.720886298096025,0.678923583927297));
#128506=DIRECTION('ref_axis',(-0.143376852789953,0.693052593253085,-0.706485089063614));
#128507=DIRECTION('center_axis',(0.985919253765162,-0.165447652133925,-0.024296079077036));
#128508=DIRECTION('ref_axis',(0.131370100254809,0.676424981841651,0.724700724919993));
#128509=DIRECTION('center_axis',(-8.34962496053827E-33,8.15751759797512E-32,
-1.));
#128510=DIRECTION('ref_axis',(0.979264158757421,0.202587530152081,8.34962496053771E-33));
#128511=DIRECTION('center_axis',(-1.11476968765511E-35,-4.11610152622635E-32,
1.));
#128512=DIRECTION('ref_axis',(-0.362063938484265,-0.932153262317556,-3.83724108360578E-32));
#128513=DIRECTION('center_axis',(8.34962496053827E-33,-8.15751759797512E-32,
1.));
#128514=DIRECTION('ref_axis',(-0.979264158757421,-0.202587530152081,-8.34962496053772E-33));
#128515=DIRECTION('center_axis',(-0.41229875219562,0.604222123490427,0.681854357192688));
#128516=DIRECTION('ref_axis',(-0.143949646750983,0.695821354962992,-0.703641344136154));
#128517=DIRECTION('center_axis',(-0.4126615615692,0.604753819133354,0.681163162426516));
#128518=DIRECTION('ref_axis',(-0.143814608418336,0.695168608966589,-0.704313824593084));
#128519=DIRECTION('center_axis',(-0.1388386536643,-0.718846697427061,-0.681163162426516));
#128520=DIRECTION('ref_axis',(0.14381460841833,-0.695168608966591,0.704313824593083));
#128521=DIRECTION('center_axis',(-0.138716587618766,-0.718214692064117,
-0.681854357192686));
#128522=DIRECTION('ref_axis',(0.143949646750992,-0.695821354962989,0.703641344136154));
#128523=DIRECTION('center_axis',(8.34962496053827E-33,-8.15751759797512E-32,
1.));
#128524=DIRECTION('ref_axis',(-0.979264158757421,-0.202587530152082,-8.34962496053776E-33));
#128525=DIRECTION('center_axis',(-1.11476968765511E-35,-4.11610152622635E-32,
1.));
#128526=DIRECTION('ref_axis',(0.702198126856968,-0.711981594311654,-2.92980573780472E-32));
#128527=DIRECTION('center_axis',(8.34962496053827E-33,-8.15751759797512E-32,
1.));
#128528=DIRECTION('ref_axis',(0.979264158757421,0.202587530152081,8.34962496053772E-33));
#128529=DIRECTION('center_axis',(-8.34962496053827E-33,8.15751759797512E-32,
-1.));
#128530=DIRECTION('ref_axis',(-0.97926415875742,-0.202587530152088,-8.34962496053827E-33));
#128531=DIRECTION('center_axis',(-0.994044497506241,0.10897493738271,2.03432761618715E-32));
#128532=DIRECTION('ref_axis',(-0.10897493738271,-0.994044497506241,-7.90139691898445E-32));
#128533=DIRECTION('',(1.16115793851356E-32,-8.07603085451917E-32,1.));
#128534=DIRECTION('',(-0.0797487039099476,-0.727449468739181,-0.681511125848849));
#128535=DIRECTION('center_axis',(0.994043973596433,-0.108979716241397,2.13514018988893E-6));
#128536=DIRECTION('ref_axis',(0.108057149906186,0.985631451112966,0.129824092259876));
#128537=DIRECTION('',(-1.57630142331307E-32,4.28918677227616E-32,-1.));
#128538=DIRECTION('center_axis',(0.777327146089751,0.629096580782285,4.17800381036604E-32));
#128539=DIRECTION('ref_axis',(-0.629096580782285,0.777327146089751,7.00819850474325E-32));
#128540=DIRECTION('center_axis',(-0.777327146089761,-0.629096580782273,
-4.29968662789252E-15));
#128541=DIRECTION('ref_axis',(0.624377322184423,-0.771495914559359,0.122257978717246));
#128542=DIRECTION('',(-0.46037775433975,0.568854031060099,0.681511125848848));
#128543=DIRECTION('',(1.16115793851356E-32,-8.07603085451917E-32,1.));
#128544=DIRECTION('',(-1.23540546490667E-32,-5.11477840503479E-32,1.));
#128545=DIRECTION('center_axis',(1.16115793851356E-32,-8.07603085451917E-32,
1.));
#128546=DIRECTION('ref_axis',(-0.959492973614494,-0.281732556841442,-1.1611579385136E-32));
#128547=DIRECTION('center_axis',(-0.0956970194023252,0.325914117778227,
-0.940543496235209));
#128548=DIRECTION('ref_axis',(-0.264867348426973,0.90247845275499,0.339673269555059));
#128549=DIRECTION('center_axis',(-0.0956970194023252,0.325914117778227,
-0.940543496235209));
#128550=DIRECTION('ref_axis',(-0.264867348426973,0.90247845275499,0.339673269555059));
#128551=DIRECTION('center_axis',(0.461888333567284,-0.570720539758078,-0.678923583927297));
#128552=DIRECTION('ref_axis',(0.199389998476552,-0.679059973373706,0.706485089063614));
#128553=DIRECTION('center_axis',(0.0800103732334678,0.729836356563823,0.678923583927297));
#128554=DIRECTION('ref_axis',(-0.199389998476543,0.679059973373708,-0.706485089063614));
#128555=DIRECTION('center_axis',(0.996124208370885,-0.0845355667096835,
-0.0242960790776955));
#128556=DIRECTION('ref_axis',(0.0757980692347224,0.684882242683267,0.724700604634374));
#128557=DIRECTION('center_axis',(-1.16115793851356E-32,8.07603085451917E-32,
-1.));
#128558=DIRECTION('ref_axis',(0.959492973614495,0.281732556841437,1.16115793851356E-32));
#128559=DIRECTION('center_axis',(-1.55027762151293E-35,-4.11621032027636E-32,
1.));
#128560=DIRECTION('ref_axis',(-0.284880056029572,-0.958563171458506,-3.94608926217002E-32));
#128561=DIRECTION('center_axis',(1.16115793851356E-32,-8.07603085451917E-32,
1.));
#128562=DIRECTION('ref_axis',(-0.959492973614495,-0.281732556841437,-1.16115793851356E-32));
#128563=DIRECTION('center_axis',(-0.460176574498932,0.568605448320517,0.681854357192688));
#128564=DIRECTION('ref_axis',(-0.200186566296206,0.68177283423205,-0.703641344136153));
#128565=DIRECTION('center_axis',(-0.460581514785171,0.569105802457949,0.681163162426516));
#128566=DIRECTION('ref_axis',(-0.199998772433969,0.681133267071847,-0.704313824593085));
#128567=DIRECTION('center_axis',(-0.0797840002101624,-0.727771433530867,
-0.681163162426516));
#128568=DIRECTION('ref_axis',(0.199998772433964,-0.681133267071849,0.704313824593083));
#128569=DIRECTION('center_axis',(-0.0797138546336566,-0.727131581597714,
-0.681854357192686));
#128570=DIRECTION('ref_axis',(0.200186566296219,-0.681772834232045,0.703641344136154));
#128571=DIRECTION('center_axis',(1.16115793851356E-32,-8.07603085451917E-32,
1.));
#128572=DIRECTION('ref_axis',(-0.959492973614495,-0.281732556841437,-1.16115793851356E-32));
#128573=DIRECTION('center_axis',(-1.55027762151293E-35,-4.11621032027636E-32,
1.));
#128574=DIRECTION('ref_axis',(0.757894730168159,-0.652376868062727,-2.68414544978973E-32));
#128575=DIRECTION('center_axis',(1.16115793851356E-32,-8.07603085451917E-32,
1.));
#128576=DIRECTION('ref_axis',(0.959492973614495,0.281732556841437,1.16115793851356E-32));
#128577=DIRECTION('center_axis',(-1.16115793851356E-32,8.07603085451917E-32,
-1.));
#128578=DIRECTION('ref_axis',(-0.959492973614495,-0.281732556841437,-1.16115793851356E-32));
#128579=DIRECTION('center_axis',(-0.999619365514338,0.0275884774627343,
1.69889412890019E-32));
#128580=DIRECTION('ref_axis',(-0.0275884774627343,-0.999619365514338,-7.92437368218264E-32));
#128581=DIRECTION('',(1.47962606647006E-32,-7.96822729466867E-32,1.));
#128582=DIRECTION('',(-0.020189461662872,-0.731529200361817,-0.681511125848847));
#128583=DIRECTION('center_axis',(0.999619232869144,-0.027593283123731,2.13514020813021E-6));
#128584=DIRECTION('ref_axis',(0.0273594852325617,0.9911595046472,0.129824092199122));
#128585=DIRECTION('',(-1.58472524752277E-32,4.16014557570144E-32,-1.));
#128586=DIRECTION('center_axis',(0.723463442554642,0.690362692566006,4.43051148238339E-32));
#128587=DIRECTION('ref_axis',(-0.690362692566006,0.723463442554642,6.78619978489798E-32));
#128588=DIRECTION('center_axis',(-0.723463442554664,-0.690362692565983,
-7.07285729322285E-15));
#128589=DIRECTION('ref_axis',(0.685183837413238,-0.718036277359265,0.122257978650548));
#128590=DIRECTION('',(-0.505212769855248,0.529436155281655,0.68151112584885));
#128591=DIRECTION('',(1.47962606647006E-32,-7.96822729466867E-32,1.));
#128592=DIRECTION('',(-1.15033253548731E-32,-5.21217033441171E-32,1.));
#128593=DIRECTION('center_axis',(1.47962606647006E-32,-7.96822729466867E-32,
1.));
#128594=DIRECTION('ref_axis',(-0.933336521037364,-0.359002699847607,-1.47962606647007E-32));
#128595=DIRECTION('center_axis',(-0.121943621702652,0.317029469948172,-0.940543496235247));
#128596=DIRECTION('ref_axis',(-0.337546396275881,0.877886382347404,0.339673269554955));
#128597=DIRECTION('center_axis',(-0.121943621702652,0.317029469948172,-0.940543496235247));
#128598=DIRECTION('ref_axis',(-0.337546396275881,0.877886382347404,0.339673269554955));
#128599=DIRECTION('center_axis',(0.506870460541718,-0.531173327095347,-0.678923583927297));
#128600=DIRECTION('ref_axis',(0.254076236620314,-0.660548321408537,0.706485089063614));
#128601=DIRECTION('center_axis',(0.0202557067868084,0.733929474493211,0.678923583927297));
#128602=DIRECTION('ref_axis',(-0.254076236620308,0.660548321408539,-0.706485089063614));
#128603=DIRECTION('center_axis',(0.999700120718703,-0.00306091103506829,
-0.0242960790796926));
#128604=DIRECTION('ref_axis',(0.0197215887137683,0.688781988546106,0.72470023540294));
#128605=DIRECTION('center_axis',(-1.47962606647006E-32,7.96822729466867E-32,
-1.));
#128606=DIRECTION('ref_axis',(0.933336521037363,0.359002699847609,1.4796260664701E-32));
#128607=DIRECTION('center_axis',(-1.9754687135784E-35,-4.11635425026281E-32,
1.));
#128608=DIRECTION('ref_axis',(-0.205800343803899,-0.978594000845191,-4.02864612680122E-32));
#128609=DIRECTION('center_axis',(1.47962606647006E-32,-7.96822729466867E-32,
1.));
#128610=DIRECTION('ref_axis',(-0.933336521037363,-0.359002699847609,-1.4796260664701E-32));
#128611=DIRECTION('center_axis',(-0.504991997622744,0.529204797705328,0.681854357192688));
#128612=DIRECTION('ref_axis',(-0.255091277271192,0.663187227773891,-0.703641344136153));
#128613=DIRECTION('center_axis',(-0.505436374010848,0.529670480563034,0.681163162426516));
#128614=DIRECTION('ref_axis',(-0.254851977616527,0.66256509566382,-0.704313824593084));
#128615=DIRECTION('center_axis',(-0.0201983973980596,-0.731852970818359,
-0.681163162426516));
#128616=DIRECTION('ref_axis',(0.254851977616525,-0.662565095663822,0.704313824593083));
#128617=DIRECTION('center_axis',(-0.0201806390978207,-0.731209530424045,
-0.681854357192686));
#128618=DIRECTION('ref_axis',(0.255091277271204,-0.663187227773886,0.703641344136154));
#128619=DIRECTION('center_axis',(1.47962606647006E-32,-7.96822729466867E-32,
1.));
#128620=DIRECTION('ref_axis',(-0.933336521037363,-0.359002699847609,-1.4796260664701E-32));
#128621=DIRECTION('center_axis',(-1.9754687135784E-35,-4.11635425026281E-32,
1.));
#128622=DIRECTION('ref_axis',(0.808547669093915,-0.588430681391443,-2.42059187570697E-32));
#128623=DIRECTION('center_axis',(1.47962606647006E-32,-7.96822729466867E-32,
1.));
#128624=DIRECTION('ref_axis',(0.933336521037362,0.359002699847611,1.47962606647011E-32));
#128625=DIRECTION('center_axis',(-1.47962606647006E-32,7.96822729466867E-32,
-1.));
#128626=DIRECTION('ref_axis',(-0.933336521037364,-0.359002699847605,-1.47962606647006E-32));
#128627=DIRECTION('center_axis',(-0.998541931570524,-0.0539815792229779,
1.36270394936435E-32));
#128628=DIRECTION('ref_axis',(0.0539815792229779,-0.998541931570524,-7.91993304887029E-32));
#128629=DIRECTION('',(1.78824752707533E-32,-7.8348243333281E-32,1.));
#128630=DIRECTION('',(0.0395041381205485,-0.730740725849866,-0.681511125848848));
#128631=DIRECTION('center_axis',(0.998542191072677,0.0539767787406583,2.13514018280428E-6));
#128632=DIRECTION('ref_axis',(0.053520252301274,-0.990091555181766,-0.1298240923379));
#128633=DIRECTION('',(-1.58260298667146E-32,4.03084713318711E-32,-1.));
#128634=DIRECTION('center_axis',(0.664785209172398,0.747034554532527,4.66408399934957E-32));
#128635=DIRECTION('ref_axis',(-0.747034554532527,0.664785209172398,6.54435802804312E-32));
#128636=DIRECTION('center_axis',(-0.664785209172376,-0.747034554532547,
9.84602795854721E-15));
#128637=DIRECTION('ref_axis',(0.74143056723946,-0.659798227188434,0.122257978725204));
#128638=DIRECTION('',(-0.546685677741585,0.486494969240643,0.681511125848852));
#128639=DIRECTION('',(1.78824752707533E-32,-7.8348243333281E-32,1.));
#128640=DIRECTION('',(-1.05760433283579E-32,-5.30230396665168E-32,1.));
#128641=DIRECTION('center_axis',(1.78824752707533E-32,-7.8348243333281E-32,
1.));
#128642=DIRECTION('ref_axis',(-0.900968867902416,-0.433883739117564,-1.78824752707532E-32));
#128643=DIRECTION('center_axis',(-0.147378709319897,0.306035043301976,-0.940543496235213));
#128644=DIRECTION('ref_axis',(-0.407979128548356,0.847452122906485,0.339673269555048));
#128645=DIRECTION('center_axis',(-0.147378709319897,0.306035043301976,-0.940543496235213));
#128646=DIRECTION('ref_axis',(-0.407979128548356,0.847452122906485,0.339673269555048));
#128647=DIRECTION('center_axis',(0.548479448228987,-0.488091243578226,-0.678923583927297));
#128648=DIRECTION('ref_axis',(0.307071639329003,-0.637640829347192,0.706485089063615));
#128649=DIRECTION('center_axis',(-0.0396337580465611,0.733138412859687,
0.678923583927297));
#128650=DIRECTION('ref_axis',(-0.307071639328998,0.637640829347196,-0.706485089063613));
#128651=DIRECTION('center_axis',(0.996623193701797,0.0784341144969083,-0.0242960790811355));
#128652=DIRECTION('ref_axis',(-0.0364860723690897,0.688096759915976,0.724701052514906));
#128653=DIRECTION('center_axis',(-1.78824752707533E-32,7.8348243333281E-32,
-1.));
#128654=DIRECTION('ref_axis',(0.900968867902417,0.433883739117563,1.78824752707531E-32));
#128655=DIRECTION('center_axis',(-2.38751338728303E-35,-4.11653235835539E-32,
1.));
#128656=DIRECTION('ref_axis',(-0.125351064244871,-0.992112448612897,-4.08436227518618E-32));
#128657=DIRECTION('center_axis',(1.78824752707533E-32,-7.8348243333281E-32,
1.));
#128658=DIRECTION('ref_axis',(-0.900968867902417,-0.433883739117563,-1.78824752707531E-32));
#128659=DIRECTION('center_axis',(-0.546446782320192,0.486282376474056,0.681854357192688));
#128660=DIRECTION('ref_axis',(-0.308298397883032,0.64018821973309,-0.703641344136153));
#128661=DIRECTION('center_axis',(-0.546927637558614,0.486710289009449,0.681163162426516));
#128662=DIRECTION('ref_axis',(-0.308009184935663,0.639587662859699,-0.704313824593083));
#128663=DIRECTION('center_axis',(0.0395216224162265,-0.731064147332296,
-0.681163162426516));
#128664=DIRECTION('ref_axis',(0.308009184935658,-0.6395876628597,0.704313824593084));
#128665=DIRECTION('center_axis',(0.0394868752616406,-0.730421400466484,
-0.681854357192686));
#128666=DIRECTION('ref_axis',(0.308298397883045,-0.640188219733083,0.703641344136154));
#128667=DIRECTION('center_axis',(1.78824752707533E-32,-7.8348243333281E-32,
1.));
#128668=DIRECTION('ref_axis',(-0.900968867902417,-0.433883739117563,-1.78824752707531E-32));
#128669=DIRECTION('center_axis',(-2.38751338728303E-35,-4.11653235835539E-32,
1.));
#128670=DIRECTION('ref_axis',(0.85381985668282,-0.520568585619733,-2.14089892110877E-32));
#128671=DIRECTION('center_axis',(1.78824752707533E-32,-7.8348243333281E-32,
1.));
#128672=DIRECTION('ref_axis',(0.900968867902428,0.43388373911754,1.7882475270751E-32));
#128673=DIRECTION('center_axis',(-1.78824752707533E-32,7.8348243333281E-32,
-1.));
#128674=DIRECTION('ref_axis',(-0.900968867902416,-0.433883739117565,-1.78824752707533E-32));
#128675=DIRECTION('center_axis',(-0.99081936581993,-0.135192397405294,1.02799436775695E-32));
#128676=DIRECTION('ref_axis',(0.135192397405294,-0.99081936581993,-7.88810457072944E-32));
#128677=DIRECTION('',(2.08496849542798E-32,-7.67670974519523E-32,1.));
#128678=DIRECTION('',(0.0989348443825012,-0.725089292371119,-0.681511125848845));
#128679=DIRECTION('center_axis',(0.990820015742491,0.135187634047982,2.13514019614746E-6));
#128680=DIRECTION('ref_axis',(0.134043821391896,-0.98243470983393,-0.129824091986731));
#128681=DIRECTION('',(-1.56994876405497E-32,3.90215190453537E-32,-1.));
#128682=DIRECTION('center_axis',(0.60168293990495,0.79873502479066,4.87716697470091E-32));
#128683=DIRECTION('ref_axis',(-0.79873502479066,0.60168293990495,6.28428265116946E-32));
#128684=DIRECTION('center_axis',(-0.601682939904999,-0.798735024790623,
-3.64582895726031E-14));
#128685=DIRECTION('ref_axis',(0.792743198971836,-0.597169328679565,0.122257978751077));
#128686=DIRECTION('',(-0.584520482639353,0.440316239445344,0.68151112584885));
#128687=DIRECTION('',(2.08496849542798E-32,-7.67670974519523E-32,1.));
#128688=DIRECTION('',(-9.57837947841676E-33,-5.38457947730315E-32,1.));
#128689=DIRECTION('center_axis',(2.08496849542798E-32,-7.67670974519523E-32,
1.));
#128690=DIRECTION('ref_axis',(-0.862605415600979,-0.505877353689471,-2.08496849542794E-32));
#128691=DIRECTION('center_axis',(-0.171833015942314,0.293004003934667,-0.940543496235247));
#128692=DIRECTION('ref_axis',(-0.475696827032618,0.81137820940727,0.339673269554954));
#128693=DIRECTION('center_axis',(-0.171833015942314,0.293004003934667,-0.940543496235247));
#128694=DIRECTION('ref_axis',(-0.475696827032618,0.81137820940727,0.339673269554954));
#128695=DIRECTION('center_axis',(0.586438395681031,-0.44176099336448,-0.678923583927297));
#128696=DIRECTION('ref_axis',(0.358023530941208,-0.610489942769876,0.706485089063615));
#128697=DIRECTION('center_axis',(-0.0992594667592402,0.727468436047905,
0.678923583927297));
#128698=DIRECTION('ref_axis',(-0.3580235309412,0.610489942769881,-0.706485089063614));
#128699=DIRECTION('center_axis',(0.986913903762582,0.159407173933681,-0.0242960790782657));
#128700=DIRECTION('ref_axis',(-0.0924509953873511,0.682833509827438,0.724700773636009));
#128701=DIRECTION('center_axis',(-2.08496849542798E-32,7.67670974519523E-32,
-1.));
#128702=DIRECTION('ref_axis',(0.862605415600975,0.505877353689478,2.084968495428E-32));
#128703=DIRECTION('center_axis',(-2.7836695533073E-35,-4.11674345927413E-32,
1.));
#128704=DIRECTION('ref_axis',(-0.0440675940347879,-0.999028551722114,-4.11286692554992E-32));
#128705=DIRECTION('center_axis',(2.08496849542798E-32,-7.67670974519523E-32,
1.));
#128706=DIRECTION('ref_axis',(-0.862605415600975,-0.505877353689478,-2.084968495428E-32));
#128707=DIRECTION('center_axis',(-0.584265053838671,0.440123826258294,0.681854357192688));
#128708=DIRECTION('ref_axis',(-0.35945384352262,0.612928864713584,-0.703641344136153));
#128709=DIRECTION('center_axis',(-0.584779187915136,0.440511120784053,0.681163162426516));
#128710=DIRECTION('ref_axis',(-0.359116641946996,0.612353879683779,-0.704313824593084));
#128711=DIRECTION('center_axis',(0.0989786323539411,-0.725410212562831,
-0.681163162426516));
#128712=DIRECTION('ref_axis',(0.359116641946992,-0.612353879683781,0.704313824593084));
#128713=DIRECTION('center_axis',(0.098891610981111,-0.724772436599868,-0.681854357192686));
#128714=DIRECTION('ref_axis',(0.359453843522631,-0.612928864713577,0.703641344136154));
#128715=DIRECTION('center_axis',(2.08496849542798E-32,-7.67670974519523E-32,
1.));
#128716=DIRECTION('ref_axis',(-0.862605415600975,-0.505877353689478,-2.084968495428E-32));
#128717=DIRECTION('center_axis',(-2.7836695533073E-35,-4.11674345927413E-32,
1.));
#128718=DIRECTION('ref_axis',(0.893410013995863,-0.44924219179849,-1.84692789646182E-32));
#128719=DIRECTION('center_axis',(2.08496849542798E-32,-7.67670974519523E-32,
1.));
#128720=DIRECTION('ref_axis',(0.862605415600984,0.505877353689463,2.08496849542787E-32));
#128721=DIRECTION('center_axis',(-2.08496849542798E-32,7.67670974519523E-32,
-1.));
#128722=DIRECTION('ref_axis',(-0.862605415600977,-0.505877353689475,-2.08496849542798E-32));
#128723=DIRECTION('center_axis',(-0.976503060663493,-0.215503532488054,
6.96992821120416E-33));
#128724=DIRECTION('ref_axis',(0.215503532488054,-0.976503060663493,-7.82910006103078E-32));
#128725=DIRECTION('',(2.36781434243914E-32,-7.49493575676703E-32,1.));
#128726=DIRECTION('',(0.157707155578178,-0.714612509282946,-0.681511125848854));
#128727=DIRECTION('center_axis',(0.976504096681335,0.215498837955129,2.1351402057377E-6));
#128728=DIRECTION('ref_axis',(0.213675350959354,-0.968239923513829,-0.129824092164478));
#128729=DIRECTION('',(-1.546846791437E-32,3.77491633525967E-32,-1.));
#128730=DIRECTION('center_axis',(0.534576569943133,0.845120045240814,5.06834237639268E-32));
#128731=DIRECTION('ref_axis',(-0.845120045240814,0.534576569943133,6.00770441300067E-32));
#128732=DIRECTION('center_axis',(-0.53457656994313,-0.845120045240815,-5.3936897343997E-15));
#128733=DIRECTION('ref_axis',(0.838780255517472,-0.530566366820449,0.122257978688485));
#128734=DIRECTION('',(-0.618465400164244,0.3912072777236,0.681511125848853));
#128735=DIRECTION('',(2.36781434243914E-32,-7.49493575676703E-32,1.));
#128736=DIRECTION('',(-8.51697309336819E-33,-5.45844933641721E-32,1.));
#128737=DIRECTION('center_axis',(2.36781434243914E-32,-7.49493575676703E-32,
1.));
#128738=DIRECTION('ref_axis',(-0.818501466578588,-0.574504437936471,-2.36781434243915E-32));
#128739=DIRECTION('center_axis',(-0.195143802194123,0.278023071263506,-0.94054349623525));
#128740=DIRECTION('ref_axis',(-0.540248841617448,0.769904707792372,0.339673269554946));
#128741=DIRECTION('center_axis',(-0.195143802194123,0.278023071263506,-0.94054349623525));
#128742=DIRECTION('ref_axis',(-0.540248841617448,0.769904707792372,0.339673269554946));
#128743=DIRECTION('center_axis',(0.620494692365343,-0.392490896625326,-0.678923583927297));
#128744=DIRECTION('ref_axis',(0.406592835024724,-0.579276346347177,0.706485089063615));
#128745=DIRECTION('center_axis',(-0.158224620097296,0.716957276818069,0.678923583927297));
#128746=DIRECTION('ref_axis',(-0.406592835024719,0.579276346347181,-0.706485089063613));
#128747=DIRECTION('center_axis',(0.970636864621209,0.239319404937,-0.0242960790850888));
#128748=DIRECTION('ref_axis',(-0.147800561463386,0.673025524458571,0.724701067653673));
#128749=DIRECTION('center_axis',(-2.36781434243914E-32,7.49493575676703E-32,
-1.));
#128750=DIRECTION('ref_axis',(0.818501466578589,0.57450443793647,2.36781434243914E-32));
#128751=DIRECTION('center_axis',(-3.16130085772864E-35,-4.11698614817723E-32,
1.));
#128752=DIRECTION('ref_axis',(0.0375091387429715,-0.999296284647732,-4.11397038414721E-32));
#128753=DIRECTION('center_axis',(2.36781434243914E-32,-7.49493575676703E-32,
1.));
#128754=DIRECTION('ref_axis',(-0.818501466578589,-0.57450443793647,-2.36781434243914E-32));
#128755=DIRECTION('center_axis',(-0.618195137820803,0.391036324594103,0.681854357192688));
#128756=DIRECTION('ref_axis',(-0.40821718313927,0.581590569225557,-0.703641344136153));
#128757=DIRECTION('center_axis',(-0.618739129257858,0.391380423729057,0.681163162426516));
#128758=DIRECTION('ref_axis',(-0.407834236956245,0.581044982469842,-0.704313824593084));
#128759=DIRECTION('center_axis',(0.157776955823665,-0.714928792513021,-0.681163162426516));
#128760=DIRECTION('ref_axis',(0.40783423695624,-0.581044982469846,0.704313824593084));
#128761=DIRECTION('center_axis',(0.15763823934547,-0.714300231746714,-0.681854357192686));
#128762=DIRECTION('ref_axis',(0.408217183139275,-0.581590569225551,0.703641344136156));
#128763=DIRECTION('center_axis',(2.36781434243914E-32,-7.49493575676703E-32,
1.));
#128764=DIRECTION('ref_axis',(-0.818501466578589,-0.57450443793647,-2.36781434243914E-32));
#128765=DIRECTION('center_axis',(-3.16130085772864E-35,-4.11698614817723E-32,
1.));
#128766=DIRECTION('ref_axis',(0.927054675068037,-0.374926165310579,-1.54063513043341E-32));
#128767=DIRECTION('center_axis',(2.36781434243914E-32,-7.49493575676703E-32,
1.));
#128768=DIRECTION('ref_axis',(0.818501466578589,0.57450443793647,2.36781434243914E-32));
#128769=DIRECTION('center_axis',(-2.36781434243914E-32,7.49493575676703E-32,
-1.));
#128770=DIRECTION('ref_axis',(-0.818501466578589,-0.57450443793647,-2.36781434243914E-32));
#128771=DIRECTION('center_axis',(-0.955688288750005,-0.294380527117686,
3.7190207013619E-33));
#128772=DIRECTION('ref_axis',(0.294380527117686,-0.955688288750005,-7.74331218505129E-32));
#128773=DIRECTION('',(2.63490277566324E-32,-7.29071204394588E-32,1.));
#128774=DIRECTION('',(0.215429951673336,-0.699380097848277,-0.681511125848844));
#128775=DIRECTION('center_axis',(0.955689703968581,0.29437593265056,2.13514017770259E-6));
#128776=DIRECTION('ref_axis',(0.291884906313846,-0.947601660243299,-0.129824092410852));
#128777=DIRECTION('',(-1.51345080863378E-32,3.64998715708116E-32,-1.));
#128778=DIRECTION('center_axis',(0.463912681107269,0.885880931224883,5.23633796366833E-32));
#128779=DIRECTION('ref_axis',(-0.885880931224883,0.463912681107269,5.71646389607957E-32));
#128780=DIRECTION('center_axis',(-0.463912681107264,-0.885880931224885,
5.80076065774857E-15));
#128781=DIRECTION('ref_axis',(0.879235367844626,-0.460432573322416,0.122257978695964));
#128782=DIRECTION('',(-0.648294532490651,0.339494896113278,0.681511125848847));
#128783=DIRECTION('',(2.63490277566324E-32,-7.29071204394588E-32,1.));
#128784=DIRECTION('',(-7.39888765758488E-33,-5.52342195226915E-32,1.));
#128785=DIRECTION('center_axis',(2.63490277566324E-32,-7.29071204394588E-32,
1.));
#128786=DIRECTION('ref_axis',(-0.768950525339359,-0.639308289935555,-2.63490277566321E-32));
#128787=DIRECTION('center_axis',(-0.217155938638808,0.261191940923687,-0.940543496235244));
#128788=DIRECTION('ref_axis',(-0.601205589296476,0.723307617372109,0.339673269554964));
#128789=DIRECTION('center_axis',(-0.217155938638808,0.261191940923687,-0.940543496235244));
#128790=DIRECTION('ref_axis',(-0.601205589296476,0.723307617372109,0.339673269554964));
#128791=DIRECTION('center_axis',(0.650421699246381,-0.340608837725571,-0.678923583927297));
#128792=DIRECTION('ref_axis',(0.452456330874242,-0.544207761413412,0.706485089063613));
#128793=DIRECTION('center_axis',(-0.216136814693829,0.701674885200632,0.678923583927297));
#128794=DIRECTION('ref_axis',(-0.452456330874235,0.544207761413415,-0.706485089063615));
#128795=DIRECTION('center_axis',(0.947900397295688,0.317639004765663,-0.0242960790695897));
#128796=DIRECTION('ref_axis',(-0.202166797592671,0.658739529255004,0.724700502654731));
#128797=DIRECTION('center_axis',(-2.63490277566324E-32,7.29071204394588E-32,
-1.));
#128798=DIRECTION('ref_axis',(0.768950525339356,0.639308289935559,2.63490277566325E-32));
#128799=DIRECTION('center_axis',(-3.51789422651897E-35,-4.1172588100101E-32,
1.));
#128800=DIRECTION('ref_axis',(0.118836254390979,-0.992913865671299,-4.08766530764312E-32));
#128801=DIRECTION('center_axis',(2.63490277566324E-32,-7.29071204394588E-32,
1.));
#128802=DIRECTION('ref_axis',(-0.768950525339356,-0.639308289935559,-2.63490277566325E-32));
#128803=DIRECTION('center_axis',(-0.648011235155756,0.339346540706191,0.681854357192688));
#128804=DIRECTION('ref_axis',(-0.454263904753227,0.54638188445502,-0.703641344136153));
#128805=DIRECTION('center_axis',(-0.648581463780139,0.339645154527369,0.681163162426516));
#128806=DIRECTION('ref_axis',(-0.453837762406458,0.545869326763249,-0.704313824593083));
#128807=DIRECTION('center_axis',(0.215525299683748,-0.699689639303984,-0.681163162426516));
#128808=DIRECTION('ref_axis',(0.453837762406454,-0.54586932676325,0.704313824593085));
#128809=DIRECTION('center_axis',(0.215335811235463,-0.699074476702528,-0.681854357192686));
#128810=DIRECTION('ref_axis',(0.454263904753234,-0.546381884455012,0.703641344136155));
#128811=DIRECTION('center_axis',(2.63490277566324E-32,-7.29071204394588E-32,
1.));
#128812=DIRECTION('ref_axis',(-0.768950525339356,-0.639308289935559,-2.63490277566325E-32));
#128813=DIRECTION('center_axis',(-3.51789422651897E-35,-4.1172588100101E-32,
1.));
#128814=DIRECTION('ref_axis',(0.954529940230887,-0.298115067050994,-1.22405895084668E-32));
#128815=DIRECTION('center_axis',(2.63490277566324E-32,-7.29071204394588E-32,
1.));
#128816=DIRECTION('ref_axis',(0.768950525339356,0.639308289935559,2.63490277566325E-32));
#128817=DIRECTION('center_axis',(-2.63490277566324E-32,7.29071204394588E-32,
-1.));
#128818=DIRECTION('ref_axis',(-0.768950525339357,-0.639308289935558,-2.63490277566324E-32));
#128819=DIRECTION('center_axis',(-0.928513568952355,-0.371298467908718,
5.48855401158773E-34));
#128820=DIRECTION('ref_axis',(0.371298467908718,-0.928513568952355,-7.63131184695163E-32));
#128821=DIRECTION('',(2.88445636564366E-32,-7.06539768184607E-32,1.));
#128822=DIRECTION('',(0.271719096983558,-0.679493427252004,-0.681511125848849));
#128823=DIRECTION('center_axis',(0.928515353953652,0.371294004082703,2.13514021011526E-6));
#128824=DIRECTION('ref_axis',(0.368152015798042,-0.92065726434055,-0.129824092066201));
#128825=DIRECTION('',(-1.4699830604009E-32,3.52819575306875E-32,-1.));
#128826=DIRECTION('center_axis',(0.390161529918842,0.920746425771715,5.38003575361186E-32));
#128827=DIRECTION('ref_axis',(-0.920746425771715,0.390161529918842,5.41249925799497E-32));
#128828=DIRECTION('center_axis',(-0.39016152991884,-0.920746425771716,-4.1979188970568E-15));
#128829=DIRECTION('ref_axis',(0.913839313871822,-0.387234677019114,0.122257978619719));
#128830=DIRECTION('',(-0.673809371664399,0.285523231982022,0.68151112584885));
#128831=DIRECTION('',(2.88445636564366E-32,-7.06539768184607E-32,1.));
#128832=DIRECTION('',(-6.23156384517089E-33,-5.5790649428202E-32,1.));
#128833=DIRECTION('center_axis',(2.88445636564366E-32,-7.06539768184607E-32,
1.));
#128834=DIRECTION('ref_axis',(-0.7142823452219,-0.699857650743566,-2.88445636564364E-32));
#128835=DIRECTION('center_axis',(-0.237722938140167,0.242622621310766,-0.940543496235182));
#128836=DIRECTION('ref_axis',(-0.658161412970005,0.671897034096037,0.339673269555136));
#128837=DIRECTION('center_axis',(-0.237722938140167,0.242622621310766,-0.940543496235182));
#128838=DIRECTION('ref_axis',(-0.658161412970005,0.671897034096037,0.339673269555136));
#128839=DIRECTION('center_axis',(0.676020257030961,-0.286460083207254,-0.678923583927297));
#128840=DIRECTION('ref_axis',(0.49530880449184,-0.50551756361539,0.706485089063615));
#128841=DIRECTION('center_axis',(-0.272610654448639,0.681722962990392,0.678923583927297));
#128842=DIRECTION('ref_axis',(-0.495308804491836,0.505517563615396,-0.706485089063613));
#128843=DIRECTION('center_axis',(0.918855809212912,0.393844769442579,-0.0242960790747627));
#128844=DIRECTION('ref_axis',(-0.255187276864415,0.640068686911497,0.724700993349614));
#128845=DIRECTION('center_axis',(-2.88445636564366E-32,7.06539768184607E-32,
-1.));
#128846=DIRECTION('ref_axis',(0.714282345221899,0.699857650743566,2.88445636564364E-32));
#128847=DIRECTION('center_axis',(-3.85107658964385E-35,-4.11755963025323E-32,
1.));
#128848=DIRECTION('ref_axis',(0.199372534372595,-0.979923768738083,-4.03412675198179E-32));
#128849=DIRECTION('center_axis',(2.88445636564366E-32,-7.06539768184607E-32,
1.));
#128850=DIRECTION('ref_axis',(-0.714282345221899,-0.699857650743566,-2.88445636564364E-32));
#128851=DIRECTION('center_axis',(-0.673514924635075,0.285398461578117,0.681854357192688));
#128852=DIRECTION('ref_axis',(-0.497287575029315,0.507537118390106,-0.703641344136152));
#128853=DIRECTION('center_axis',(-0.674107595669373,0.285649602859807,0.681163162426516));
#128854=DIRECTION('ref_axis',(-0.496821072425826,0.507061000749135,-0.704313824593084));
#128855=DIRECTION('center_axis',(0.271839358233607,-0.679794166986044,-0.681163162426516));
#128856=DIRECTION('ref_axis',(0.496821072425819,-0.507061000749142,0.704313824593084));
#128857=DIRECTION('center_axis',(0.271600358829592,-0.679196496355057,-0.681854357192686));
#128858=DIRECTION('ref_axis',(0.497287575029323,-0.507537118390095,0.703641344136155));
#128859=DIRECTION('center_axis',(2.88445636564366E-32,-7.06539768184607E-32,
1.));
#128860=DIRECTION('ref_axis',(-0.714282345221899,-0.699857650743566,-2.88445636564364E-32));
#128861=DIRECTION('center_axis',(-3.85107658964385E-35,-4.11755963025323E-32,
1.));
#128862=DIRECTION('ref_axis',(0.975652966127861,-0.219320062205688,-8.99306119945298E-33));
#128863=DIRECTION('center_axis',(2.88445636564366E-32,-7.06539768184607E-32,
1.));
#128864=DIRECTION('ref_axis',(0.714282345221914,0.699857650743551,2.88445636564349E-32));
#128865=DIRECTION('center_axis',(-2.88445636564366E-32,7.06539768184607E-32,
-1.));
#128866=DIRECTION('ref_axis',(-0.714282345221898,-0.699857650743568,-2.88445636564366E-32));
#128867=DIRECTION('center_axis',(-0.895159744547281,-0.445745478655752,
-2.51947076237285E-33));
#128868=DIRECTION('ref_axis',(0.445745478655752,-0.895159744547281,-7.49384439050308E-32));
#128869=DIRECTION('',(3.11481437441252E-32,-6.82049210037312E-32,1.));
#128870=DIRECTION('',(0.326199996533838,-0.655084840005901,-0.68151112584885));
#128871=DIRECTION('center_axis',(0.895161887452382,0.445741175176952,2.13514017251284E-6));
#128872=DIRECTION('ref_axis',(0.441969134348745,-0.887586046206353,-0.129824091996805));
#128873=DIRECTION('',(-1.4167328174312E-32,3.41035262492197E-32,-1.));
#128874=DIRECTION('center_axis',(0.313813918120925,0.949484504767504,5.49847946113968E-32));
#128875=DIRECTION('ref_axis',(-0.949484504767504,0.313813918120925,5.09783333326269E-32));
#128876=DIRECTION('center_axis',(-0.313813918120886,-0.949484504767517,
1.07873794688004E-14));
#128877=DIRECTION('ref_axis',(0.942361810024425,-0.311459797823307,0.122257978665416));
#128878=DIRECTION('',(-0.694840120640441,0.229651457849955,0.68151112584885));
#128879=DIRECTION('',(3.11481437441252E-32,-6.82049210037312E-32,1.));
#128880=DIRECTION('',(-5.02277000350294E-33,-5.62500801314869E-32,1.));
#128881=DIRECTION('center_axis',(3.11481437441252E-32,-6.82049210037312E-32,
1.));
#128882=DIRECTION('ref_axis',(-0.654860733945281,-0.755749574354262,-3.1148143744125E-32));
#128883=DIRECTION('center_axis',(-0.256707930709543,0.222438688182738,-0.940543496235218));
#128884=DIRECTION('ref_axis',(0.710737281029233,-0.616015086913434,-0.339673269555036));
#128885=DIRECTION('center_axis',(-0.256707930709543,0.222438688182738,-0.940543496235218));
#128886=DIRECTION('ref_axis',(0.710737281029233,-0.616015086913434,-0.339673269555036));
#128887=DIRECTION('center_axis',(0.697120011540492,-0.23040498409778,-0.678923583927297));
#128888=DIRECTION('ref_axis',(0.534865079735741,-0.463463229836042,0.706485089063615));
#128889=DIRECTION('center_axis',(-0.327270315275685,0.657234286937823,0.678923583927297));
#128890=DIRECTION('ref_axis',(-0.534865079735737,0.463463229836048,-0.706485089063613));
#128891=DIRECTION('center_axis',(0.883696387322955,0.467429562152471,-0.0242960790726872));
#128892=DIRECTION('ref_axis',(-0.306509859595482,0.617139060430464,0.724700687223189));
#128893=DIRECTION('center_axis',(-3.11481437441252E-32,6.82049210037312E-32,
-1.));
#128894=DIRECTION('ref_axis',(0.65486073394528,0.755749574354262,3.1148143744125E-32));
#128895=DIRECTION('center_axis',(-4.15863067344775E-35,-4.11788660699752E-32,
1.));
#128896=DIRECTION('ref_axis',(0.278582023032134,-0.960412440799953,-3.95371100741787E-32));
#128897=DIRECTION('center_axis',(3.11481437441252E-32,-6.82049210037312E-32,
1.));
#128898=DIRECTION('ref_axis',(-0.65486073394528,-0.755749574354262,-3.1148143744125E-32));
#128899=DIRECTION('center_axis',(-0.694536483413088,0.229551102775672,0.681854357192688));
#128900=DIRECTION('ref_axis',(-0.537001878540263,0.465314776540028,-0.703641344136153));
#128901=DIRECTION('center_axis',(-0.695147652729352,0.229753100214081,0.681163162426516));
#128902=DIRECTION('ref_axis',(-0.536498120177901,0.464878267434217,-0.704313824593085));
#128903=DIRECTION('center_axis',(0.326344370704758,-0.655374776644954,-0.681163162426516));
#128904=DIRECTION('ref_axis',(0.5364981201779,-0.464878267434222,0.704313824593083));
#128905=DIRECTION('center_axis',(0.326057450846616,-0.654798575383877,-0.681854357192686));
#128906=DIRECTION('ref_axis',(0.537001878540269,-0.465314776540019,0.703641344136155));
#128907=DIRECTION('center_axis',(3.11481437441252E-32,-6.82049210037312E-32,
1.));
#128908=DIRECTION('ref_axis',(-0.65486073394528,-0.755749574354262,-3.1148143744125E-32));
#128909=DIRECTION('center_axis',(-4.15863067344775E-35,-4.11788660699752E-32,
1.));
#128910=DIRECTION('ref_axis',(0.990283182506655,-0.139065518531698,-5.68537814238674E-33));
#128911=DIRECTION('center_axis',(3.11481437441252E-32,-6.82049210037312E-32,
1.));
#128912=DIRECTION('ref_axis',(0.65486073394528,0.755749574354262,3.1148143744125E-32));
#128913=DIRECTION('center_axis',(-3.11481437441252E-32,6.82049210037312E-32,
-1.));
#128914=DIRECTION('ref_axis',(-0.654860733945278,-0.755749574354264,-3.11481437441252E-32));
#128915=DIRECTION('center_axis',(-0.855848779733208,-0.51722612678516,-5.46553858485279E-33));
#128916=DIRECTION('ref_axis',(0.51722612678516,-0.855848779733208,-7.33182463894778E-32));
#128917=DIRECTION('',(3.32444380742786E-32,-6.55762510576516E-32,1.));
#128918=DIRECTION('',(0.378510088926395,-0.626316771230952,-0.681511125848851));
#128919=DIRECTION('center_axis',(0.855851266281428,0.517222012292514,2.13514017393721E-6));
#128920=DIRECTION('ref_axis',(0.512845021223353,-0.848608089361961,-0.129824092047128));
#128921=DIRECTION('',(-1.35405445130595E-32,3.29724199921589E-32,-1.));
#128922=DIRECTION('center_axis',(0.235377926473567,0.971903921037982,5.59088086292001E-32));
#128923=DIRECTION('ref_axis',(-0.971903921037982,0.235377926473567,4.77456017169558E-32));
#128924=DIRECTION('center_axis',(-0.235377926473611,-0.971903921037972,
-2.4983977920653E-14));
#128925=DIRECTION('ref_axis',(0.964613043805694,-0.233612205060252,0.122257978744951));
#128926=DIRECTION('',(-0.711246823254173,0.172251391155712,0.681511125848851));
#128927=DIRECTION('',(3.32444380742786E-32,-6.55762510576516E-32,1.));
#128928=DIRECTION('',(-3.78055045616041E-33,-5.66094541970164E-32,1.));
#128929=DIRECTION('center_axis',(3.32444380742786E-32,-6.55762510576516E-32,
1.));
#128930=DIRECTION('ref_axis',(-0.591081132528671,-0.806612109237534,-3.32444380742785E-32));
#128931=DIRECTION('center_axis',(-0.273984574353886,0.200774462284682,-0.940543496235244));
#128932=DIRECTION('ref_axis',(0.758583309747373,-0.556033660961783,-0.339673269554962));
#128933=DIRECTION('center_axis',(-0.273984574353886,0.200774462284682,-0.940543496235244));
#128934=DIRECTION('ref_axis',(0.758583309747373,-0.556033660961783,-0.339673269554962));
#128935=DIRECTION('center_axis',(0.713580547389926,-0.172816577833282,-0.678923583927297));
#128936=DIRECTION('ref_axis',(0.570861916120529,-0.418324624728181,0.706485089063615));
#128937=DIRECTION('center_axis',(-0.379752046150372,0.628371825141707,0.678923583927297));
#128938=DIRECTION('ref_axis',(-0.570861916120528,0.418324624728188,-0.706485089063612));
#128939=DIRECTION('center_axis',(0.842656111769909,0.537903688254794,-0.0242960790809713));
#128940=DIRECTION('ref_axis',(-0.355792274931549,0.590101793195228,0.724701132030859));
#128941=DIRECTION('center_axis',(-3.32444380742786E-32,6.55762510576516E-32,
-1.));
#128942=DIRECTION('ref_axis',(0.591081132528676,0.806612109237531,3.32444380742781E-32));
#128943=DIRECTION('center_axis',(-4.43850975624469E-35,-4.11823756426669E-32,
1.));
#128944=DIRECTION('ref_axis',(0.355937594291176,-0.934509726525203,-3.8469532274638E-32));
#128945=DIRECTION('center_axis',(3.32444380742786E-32,-6.55762510576516E-32,
1.));
#128946=DIRECTION('ref_axis',(-0.591081132528676,-0.806612109237531,-3.32444380742781E-32));
#128947=DIRECTION('center_axis',(-0.710936016484441,0.172176119257522,0.681854357192688));
#128948=DIRECTION('ref_axis',(-0.573142523148596,0.419995841623616,-0.703641344136153));
#128949=DIRECTION('center_axis',(-0.711561616851706,0.172327628593023,0.681163162426516));
#128950=DIRECTION('ref_axis',(-0.572604861456151,0.419601845949043,-0.704313824593084));
#128951=DIRECTION('center_axis',(0.3786776152319,-0.62659397529452,-0.681163162426516));
#128952=DIRECTION('ref_axis',(0.572604861456151,-0.419601845949045,0.704313824593083));
#128953=DIRECTION('center_axis',(0.378344684323947,-0.626043077927678,-0.681854357192686));
#128954=DIRECTION('ref_axis',(0.5731425231486,-0.419995841623607,0.703641344136155));
#128955=DIRECTION('center_axis',(3.32444380742786E-32,-6.55762510576516E-32,
1.));
#128956=DIRECTION('ref_axis',(-0.591081132528676,-0.806612109237531,-3.32444380742781E-32));
#128957=DIRECTION('center_axis',(-4.43850975624469E-35,-4.11823756426669E-32,
1.));
#128958=DIRECTION('ref_axis',(0.998323227691097,-0.0578855167760517,-2.33955242228133E-33));
#128959=DIRECTION('center_axis',(3.32444380742786E-32,-6.55762510576516E-32,
1.));
#128960=DIRECTION('ref_axis',(0.59108113252868,0.806612109237527,3.32444380742778E-32));
#128961=DIRECTION('center_axis',(-3.32444380742786E-32,6.55762510576516E-32,
-1.));
#128962=DIRECTION('ref_axis',(-0.59108113252867,-0.806612109237535,-3.32444380742786E-32));
#128963=DIRECTION('center_axis',(-0.810842282495119,-0.585264720377117,
-8.26974247098951E-33));
#128964=DIRECTION('ref_axis',(0.585264720377117,-0.810842282495119,-7.14633080700095E-32));
#128965=DIRECTION('',(3.51194961539939E-32,-6.27854603450129E-32,1.));
#128966=DIRECTION('',(0.428301259126928,-0.593380667678451,-0.681511125848847));
#128967=DIRECTION('center_axis',(0.810845096138937,0.585260822251823,2.13514021087779E-6));
#128968=DIRECTION('ref_axis',(0.580308009067981,-0.803982785657608,-0.129824092439688));
#128969=DIRECTION('',(-1.28236507621051E-32,3.18961660850265E-32,-1.));
#128970=DIRECTION('center_axis',(0.15537553356015,0.987855477066812,5.65662504286917E-32));
#128971=DIRECTION('ref_axis',(-0.987855477066812,0.15537553356015,4.44483110284758E-32));
#128972=DIRECTION('center_axis',(-0.155375533560178,-0.987855477066808,
-1.41457145864412E-14));
#128973=DIRECTION('ref_axis',(0.980444936943974,-0.154209961619461,0.122257978709985));
#128974=DIRECTION('',(-0.722920295606621,0.113705019872803,0.681511125848845));
#128975=DIRECTION('',(3.51194961539939E-32,-6.27854603450129E-32,1.));
#128976=DIRECTION('',(-2.51317196927904E-33,-5.68663800496772E-32,1.));
#128977=DIRECTION('center_axis',(3.51194961539939E-32,-6.27854603450129E-32,
1.));
#128978=DIRECTION('ref_axis',(-0.523367983696605,-0.852106773615461,-3.51194961539939E-32));
#128979=DIRECTION('center_axis',(-0.289437895860387,0.177774115465721,-0.940543496235178));
#128980=DIRECTION('ref_axis',(0.801381091695437,-0.492351922736925,-0.339673269555146));
#128981=DIRECTION('center_axis',(-0.289437895860387,0.177774115465721,-0.940543496235178));
#128982=DIRECTION('ref_axis',(0.801381091695437,-0.492351922736925,-0.339673269555146));
#128983=DIRECTION('center_axis',(0.725292322428984,-0.114078105756032,-0.678923583927297));
#128984=DIRECTION('ref_axis',(0.603059760639116,-0.370402138261472,0.706485089063613));
#128985=DIRECTION('center_axis',(-0.429706589812607,0.595327652523326,0.678923583927297));
#128986=DIRECTION('ref_axis',(-0.603059760639109,0.370402138261479,-0.706485089063615));
#128987=DIRECTION('center_axis',(0.796008098829182,0.604798154048084,-0.0242960790742329));
#128988=DIRECTION('ref_axis',(-0.402707478164874,0.559138279076155,0.724700677453694));
#128989=DIRECTION('center_axis',(-3.51194961539939E-32,6.27854603450129E-32,
-1.));
#128990=DIRECTION('ref_axis',(0.523367983696608,0.852106773615459,3.51194961539936E-32));
#128991=DIRECTION('center_axis',(-4.6888512889172E-35,-4.11861016649801E-32,
1.));
#128992=DIRECTION('ref_axis',(0.4309244595858,-0.902388004203672,-3.71456386753134E-32));
#128993=DIRECTION('center_axis',(3.51194961539939E-32,-6.27854603450129E-32,
1.));
#128994=DIRECTION('ref_axis',(-0.523367983696608,-0.852106773615459,-3.51194961539936E-32));
#128995=DIRECTION('center_axis',(-0.722604387662277,0.113655332072772,0.681854357192688));
#128996=DIRECTION('ref_axis',(-0.605468998827237,0.371881903675631,-0.703641344136153));
#128997=DIRECTION('center_axis',(-0.723240255813315,0.113755345035735,0.681163162426516));
#128998=DIRECTION('ref_axis',(-0.604901011854562,0.371533043408511,-0.704313824593083));
#128999=DIRECTION('center_axis',(0.428490822707084,-0.593643294419229,-0.681163162426516));
#129000=DIRECTION('ref_axis',(0.60490101185456,-0.371533043408513,0.704313824593084));
#129001=DIRECTION('center_axis',(0.428114096349583,-0.593121367077708,-0.681854357192686));
#129002=DIRECTION('ref_axis',(0.605468998827243,-0.371881903675619,0.703641344136154));
#129003=DIRECTION('center_axis',(3.51194961539939E-32,-6.27854603450129E-32,
1.));
#129004=DIRECTION('ref_axis',(-0.523367983696608,-0.852106773615459,-3.51194961539936E-32));
#129005=DIRECTION('center_axis',(-4.6888512889172E-35,-4.11861016649801E-32,
1.));
#129006=DIRECTION('ref_axis',(0.999719596506991,0.023679703543303,1.02215004271744E-33));
#129007=DIRECTION('center_axis',(3.51194961539939E-32,-6.27854603450129E-32,
1.));
#129008=DIRECTION('ref_axis',(0.52336798369659,0.85210677361547,3.5119496153995E-32));
#129009=DIRECTION('center_axis',(-3.51194961539939E-32,6.27854603450129E-32,
-1.));
#129010=DIRECTION('ref_axis',(-0.523367983696604,-0.852106773615461,-3.51194961539939E-32));
#129011=DIRECTION('center_axis',(-0.760439763646586,-0.649408473816846,
-1.09134209065818E-32));
#129012=DIRECTION('ref_axis',(0.649408473816846,-0.760439763646586,-6.93859732550988E-32));
#129013=DIRECTION('',(3.67608397811134E-32,-5.98511211175597E-32,1.));
#129014=DIRECTION('',(0.475242155112699,-0.556495713683465,-0.681511125848851));
#129015=DIRECTION('center_axis',(0.760442885661614,0.649404818000358,2.13514019846297E-6));
#129016=DIRECTION('ref_axis',(0.643909142906818,-0.754007109234366,-0.129824092159517));
#129017=DIRECTION('',(-1.20214177310824E-32,3.0881926820005E-32,-1.));
#129018=DIRECTION('center_axis',(0.0743391421060497,0.997233017880443,5.69527448431661E-32));
#129019=DIRECTION('ref_axis',(-0.997233017880443,0.0743391421060497,4.11084041927039E-32));
#129020=DIRECTION('center_axis',(-0.0743391421060833,-0.997233017880441,
-1.97365792993271E-14));
#129021=DIRECTION('ref_axis',(0.989752130775784,-0.0737814763252889,0.122257978782798));
#129022=DIRECTION('',(-0.729782852665251,0.054401960442657,0.681511125848848));
#129023=DIRECTION('',(3.67608397811134E-32,-5.98511211175597E-32,1.));
#129024=DIRECTION('',(-1.22906873758631E-33,-5.70191478903094E-32,1.));
#129025=DIRECTION('center_axis',(3.67608397811134E-32,-5.98511211175597E-32,
1.));
#129026=DIRECTION('ref_axis',(-0.452171907282676,-0.891930808002699,-3.67608397811135E-32));
#129027=DIRECTION('center_axis',(-0.302965055923595,0.153590711238846,-0.940543496235213));
#129028=DIRECTION('ref_axis',(0.838845814697296,-0.425393663698242,-0.339673269555049));
#129029=DIRECTION('center_axis',(-0.302965055923595,0.153590711238846,-0.940543496235213));
#129030=DIRECTION('ref_axis',(0.838845814697296,-0.425393663698242,-0.339673269555049));
#129031=DIRECTION('center_axis',(0.732177396727087,-0.0545804627065377,
-0.678923583927297));
#129032=DIRECTION('ref_axis',(0.631244341948513,-0.320014686676667,0.706485089063615));
#129033=DIRECTION('center_axis',(-0.476801507016236,0.558321672599552,0.678923583927297));
#129034=DIRECTION('ref_axis',(-0.631244341948511,0.320014686676674,-0.706485089063613));
#129035=DIRECTION('center_axis',(0.744062783317934,0.667667787917529,-0.0242960790763298));
#129036=DIRECTION('ref_axis',(-0.446942527076936,0.52445346295967,0.724700588298155));
#129037=DIRECTION('center_axis',(-3.67608397811134E-32,5.98511211175597E-32,
-1.));
#129038=DIRECTION('ref_axis',(0.45217190728268,0.891930808002697,3.67608397811132E-32));
#129039=DIRECTION('center_axis',(-4.90798928986758E-35,-4.11900193408512E-32,
1.));
#129040=DIRECTION('ref_axis',(0.503043593699387,-0.864261038597718,-3.55742395696821E-32));
#129041=DIRECTION('center_axis',(3.67608397811134E-32,-5.98511211175597E-32,
1.));
#129042=DIRECTION('ref_axis',(-0.45217190728268,-0.891930808002697,-3.67608397811132E-32));
#129043=DIRECTION('center_axis',(-0.729463945861552,0.054378187404888,0.681854357192688));
#129044=DIRECTION('ref_axis',(-0.633766178214033,0.321293153014888,-0.703641344136152));
#129045=DIRECTION('center_axis',(-0.730105850198729,0.0544260384255464,
0.681163162426516));
#129046=DIRECTION('ref_axis',(-0.633171645820725,0.320991749762727,-0.704313824593084));
#129047=DIRECTION('center_axis',(0.47545249445316,-0.556742015363827,-0.681163162426516));
#129048=DIRECTION('ref_axis',(0.633171645820723,-0.32099174976273,0.704313824593084));
#129049=DIRECTION('center_axis',(0.475034479697865,-0.556252531387972,-0.681854357192686));
#129050=DIRECTION('ref_axis',(0.633766178214041,-0.321293153014869,0.703641344136154));
#129051=DIRECTION('center_axis',(3.67608397811134E-32,-5.98511211175597E-32,
1.));
#129052=DIRECTION('ref_axis',(-0.45217190728268,-0.891930808002697,-3.67608397811132E-32));
#129053=DIRECTION('center_axis',(-4.90798928986758E-35,-4.11900193408512E-32,
1.));
#129054=DIRECTION('ref_axis',(0.994462996350255,0.105087339342442,4.37735767734634E-33));
#129055=DIRECTION('center_axis',(3.67608397811134E-32,-5.98511211175597E-32,
1.));
#129056=DIRECTION('ref_axis',(0.45217190728268,0.891930808002697,3.67608397811132E-32));
#129057=DIRECTION('center_axis',(-3.67608397811134E-32,5.98511211175597E-32,
-1.));
#129058=DIRECTION('ref_axis',(-0.452171907282677,-0.891930808002698,-3.67608397811134E-32));
#129059=DIRECTION('center_axis',(-0.704976643634714,-0.70923052100818,-1.3378980647817E-32));
#129060=DIRECTION('ref_axis',(0.70923052100818,-0.704976643634714,-6.71000662652026E-32));
#129061=DIRECTION('',(3.81575460846013E-32,-5.6792760918719E-32,1.));
#129062=DIRECTION('',(0.519020392965634,-0.515907372529247,-0.68151112584885));
#129063=DIRECTION('center_axis',(0.704980053244474,0.709227131829331,2.13514018106101E-6));
#129064=DIRECTION('ref_axis',(0.703225167629535,-0.699013639885662,-0.129824092009961));
#129065=DIRECTION('',(-1.11391841484537E-32,2.99364517920655E-32,-1.));
#129066=DIRECTION('center_axis',(-0.00719196407367123,0.999974137491947,
5.70657198160623E-32));
#129067=DIRECTION('ref_axis',(-0.999974137491947,-0.00719196407367123,3.77481077385863E-32));
#129068=DIRECTION('center_axis',(0.00719196407364449,-0.999974137491947,
-1.32083383781831E-14));
#129069=DIRECTION('ref_axis',(0.992472687497606,0.00713801251946082,0.122257978670317));
#129070=DIRECTION('',(-0.731788825245092,-0.00526313505855431,0.681511125848847));
#129071=DIRECTION('',(3.81575460846013E-32,-5.6792760918719E-32,1.));
#129072=DIRECTION('',(6.32137437729893E-35,-5.70667410741387E-32,1.));
#129073=DIRECTION('center_axis',(3.81575460846012E-32,-5.6792760918719E-32,
1.));
#129074=DIRECTION('ref_axis',(-0.377966701428894,-0.925819190020903,-3.81575460846015E-32));
#129075=DIRECTION('center_axis',(-0.314476033525425,0.128385186169416,-0.940543496235214));
#129076=DIRECTION('ref_axis',(0.870728157202492,-0.355604480011906,-0.339673269555046));
#129077=DIRECTION('center_axis',(-0.314476033525425,0.128385186169416,-0.940543496235214));
#129078=DIRECTION('ref_axis',(0.870728157202492,-0.355604480011906,-0.339673269555046));
#129079=DIRECTION('center_axis',(0.734189951250738,0.00528040431712579,
-0.678923583927297));
#129080=DIRECTION('ref_axis',(0.655228096310224,-0.267497590150746,0.706485089063614));
#129081=DIRECTION('center_axis',(-0.520723388857382,0.517600154061219,0.678923583927297));
#129082=DIRECTION('ref_axis',(-0.655228096310221,0.267497590150754,-0.706485089063614));
#129083=DIRECTION('center_axis',(0.687165852736339,0.726094202823528,-0.0242960790911833));
#129084=DIRECTION('ref_axis',(-0.488202805279804,0.486278075709505,0.724701079067218));
#129085=DIRECTION('center_axis',(-3.81575460846012E-32,5.6792760918719E-32,
-1.));
#129086=DIRECTION('ref_axis',(0.377966701428891,0.925819190020905,3.81575460846017E-32));
#129087=DIRECTION('center_axis',(-5.09446543185489E-35,-4.11941025987936E-32,
1.));
#129088=DIRECTION('ref_axis',(0.57181505569327,-0.820382558372923,-3.37657923595285E-32));
#129089=DIRECTION('center_axis',(3.81575460846013E-32,-5.6792760918719E-32,
1.));
#129090=DIRECTION('ref_axis',(-0.377966701428889,-0.925819190020905,-3.81575460846018E-32));
#129091=DIRECTION('center_axis',(-0.731469041854198,-0.00526083512840586,
0.681854357192688));
#129092=DIRECTION('ref_axis',(-0.657845748248876,0.26856624943046,-0.703641344136153));
#129093=DIRECTION('center_axis',(-0.732112710610057,-0.00526546449070042,
0.681163162426516));
#129094=DIRECTION('ref_axis',(-0.657228626949919,0.268314308982185,-0.704313824593084));
#129095=DIRECTION('center_axis',(0.519250108292791,-0.516135710052146,-0.681163162426516));
#129096=DIRECTION('ref_axis',(0.65722862694992,-0.268314308982184,0.704313824593083));
#129097=DIRECTION('center_axis',(0.518793586958931,-0.515681926877058,-0.681854357192686));
#129098=DIRECTION('ref_axis',(0.657845748248881,-0.268566249430445,0.703641344136154));
#129099=DIRECTION('center_axis',(3.81575460846012E-32,-5.6792760918719E-32,
1.));
#129100=DIRECTION('ref_axis',(-0.377966701428889,-0.925819190020905,-3.81575460846018E-32));
#129101=DIRECTION('center_axis',(-5.09446543185489E-35,-4.11941025987936E-32,
1.));
#129102=DIRECTION('ref_axis',(0.982588409027654,0.18579563623644,7.70374212836736E-33));
#129103=DIRECTION('center_axis',(3.81575460846013E-32,-5.6792760918719E-32,
1.));
#129104=DIRECTION('ref_axis',(0.377966701428909,0.925819190020897,3.81575460846005E-32));
#129105=DIRECTION('center_axis',(-3.81575460846012E-32,5.6792760918719E-32,
-1.));
#129106=DIRECTION('ref_axis',(-0.377966701428898,-0.925819190020902,-3.81575460846012E-32));
#129107=DIRECTION('center_axis',(-0.644822020372411,-0.764332756097003,
-1.56500138014059E-32));
#129108=DIRECTION('ref_axis',(0.764332756097004,-0.644822020372411,-6.46207994341907E-32));
#129109=DIRECTION('',(3.9300320214448E-32,-5.363073263102E-32,1.));
#129110=DIRECTION('',(0.559344635735722,-0.471885752929575,-0.681511125848846));
#129111=DIRECTION('center_axis',(0.644825694886489,0.76432965611024,2.13514017444585E-6));
#129112=DIRECTION('ref_axis',(0.757861344882821,-0.639368350086046,-0.129824091911515));
#129113=DIRECTION('',(-1.0182821133153E-32,2.90660329815265E-32,-1.));
#129114=DIRECTION('center_axis',(-0.0886752089190725,0.996060594202561,
5.6904423517575E-32));
#129115=DIRECTION('ref_axis',(-0.996060594202561,-0.0886752089190725,3.43897838846154E-32));
#129116=DIRECTION('center_axis',(0.0886752089190568,-0.996060594202562,
-1.22948139818278E-14));
#129117=DIRECTION('ref_axis',(0.988588502211445,0.0880099990691413,0.122257978713791));
#129118=DIRECTION('',(-0.728924863929587,-0.0648932052642919,0.681511125848845));
#129119=DIRECTION('',(3.9300320214448E-32,-5.363073263102E-32,1.));
#129120=DIRECTION('',(1.355075548097E-33,-5.70088428763789E-32,1.));
#129121=DIRECTION('center_axis',(3.9300320214448E-32,-5.363073263102E-32,
1.));
#129122=DIRECTION('ref_axis',(-0.301246189537227,-0.95354639807893,-3.93003202144479E-32));
#129123=DIRECTION('center_axis',(-0.323894225009133,0.102325278868117,-0.94054349623518));
#129124=DIRECTION('ref_axis',(0.896815947481311,-0.283448807182034,-0.339673269555142));
#129125=DIRECTION('center_axis',(-0.323894225009133,0.102325278868117,-0.94054349623518));
#129126=DIRECTION('ref_axis',(0.896815947481311,-0.283448807182034,-0.339673269555142));
#129127=DIRECTION('center_axis',(0.731316592781632,0.0651061311212643,-0.678923583927297));
#129128=DIRECTION('ref_axis',(0.674851415796019,-0.213200341296364,0.706485089063614));
#129129=DIRECTION('center_axis',(-0.561179942458995,0.473434091895624,0.678923583927297));
#129130=DIRECTION('ref_axis',(-0.674851415796018,0.213200341296369,-0.706485089063613));
#129131=DIRECTION('center_axis',(0.625695946790193,0.779688580595619,-0.0242960790892782));
#129132=DIRECTION('ref_axis',(-0.526214352956803,0.444866830484855,0.724701288722887));
#129133=DIRECTION('center_axis',(-3.9300320214448E-32,5.363073263102E-32,
-1.));
#129134=DIRECTION('ref_axis',(0.301246189537228,0.95354639807893,3.93003202144479E-32));
#129135=DIRECTION('center_axis',(-5.24703874692173E-35,-4.11983242653994E-32,
1.));
#129136=DIRECTION('ref_axis',(0.636781182834359,-0.771044567575749,-3.17323319626639E-32));
#129137=DIRECTION('center_axis',(3.9300320214448E-32,-5.363073263102E-32,
1.));
#129138=DIRECTION('ref_axis',(-0.301246189537228,-0.95354639807893,-3.93003202144479E-32));
#129139=DIRECTION('center_axis',(-0.728606332057201,-0.064864847671897,
0.681854357192688));
#129140=DIRECTION('ref_axis',(-0.677547463366032,0.214052081766387,-0.703641344136153));
#129141=DIRECTION('center_axis',(-0.72924748172237,-0.0649219266095021,
0.681163162426516));
#129142=DIRECTION('ref_axis',(-0.676911860001852,0.21385128074411,-0.704313824593084));
#129143=DIRECTION('center_axis',(0.559592198331971,-0.472094606746467,-0.681163162426516));
#129144=DIRECTION('ref_axis',(0.676911860001849,-0.213851280744116,0.704313824593085));
#129145=DIRECTION('center_axis',(0.559100208493701,-0.471679544224305,-0.681854357192686));
#129146=DIRECTION('ref_axis',(0.677547463366035,-0.214052081766373,0.703641344136154));
#129147=DIRECTION('center_axis',(3.9300320214448E-32,-5.363073263102E-32,
1.));
#129148=DIRECTION('ref_axis',(-0.301246189537228,-0.95354639807893,-3.93003202144479E-32));
#129149=DIRECTION('center_axis',(-5.24703874692173E-35,-4.11983242653994E-32,
1.));
#129150=DIRECTION('ref_axis',(0.96417485795865,0.265267493825414,1.09791668560744E-32));
#129151=DIRECTION('center_axis',(3.9300320214448E-32,-5.363073263102E-32,
1.));
#129152=DIRECTION('ref_axis',(0.301246189537229,0.953546398078929,3.93003202144478E-32));
#129153=DIRECTION('center_axis',(-3.9300320214448E-32,5.363073263102E-32,
-1.));
#129154=DIRECTION('ref_axis',(-0.301246189537225,-0.95354639807893,-3.9300320214448E-32));
#129155=DIRECTION('center_axis',(-0.580376212952675,-0.81434848280003,-1.77114070164055E-32));
#129156=DIRECTION('ref_axis',(0.81434848280003,-0.580376212952675,-6.19646718737732E-32));
#129157=DIRECTION('',(4.0181557197364E-32,-5.03860790310193E-32,1.));
#129158=DIRECTION('',(0.595946532240344,-0.42472381149983,-0.681511125848849));
#129159=DIRECTION('center_axis',(0.580380127917873,0.814345692635182,2.13514021281083E-6));
#129160=DIRECTION('ref_axis',(0.807454079866993,-0.575468169361725,-0.129824092361983));
#129161=DIRECTION('',(-9.15869312325847E-33,2.82764628819631E-32,-1.));
#129162=DIRECTION('center_axis',(-0.169568334879497,0.985518431997187,5.64699293479588E-32));
#129163=DIRECTION('ref_axis',(-0.985518431997187,-0.169568334879497,3.10557817219548E-32));
#129164=DIRECTION('center_axis',(0.169568334879536,-0.985518431997181,1.77457480648256E-14));
#129165=DIRECTION('ref_axis',(0.978125423555369,0.168296293595959,0.122257978702795));
#129166=DIRECTION('',(-0.72121002790876,-0.124091421895629,0.68151112584885));
#129167=DIRECTION('',(4.0181557197364E-32,-5.03860790310193E-32,1.));
#129168=DIRECTION('',(2.63791954822017E-33,-5.68458385999836E-32,1.));
#129169=DIRECTION('center_axis',(4.0181557197364E-32,-5.03860790310193E-32,
1.));
#129170=DIRECTION('ref_axis',(-0.222520933956311,-0.974927912181825,-4.01815571973637E-32));
#129171=DIRECTION('center_axis',(-0.331156953863924,0.0755844137183558,
-0.940543496235245));
#129172=DIRECTION('ref_axis',(0.916935575593894,-0.209406829306347,-0.339673269554959));
#129173=DIRECTION('center_axis',(-0.331156953863924,0.0755844137183558,
-0.940543496235245));
#129174=DIRECTION('ref_axis',(0.916935575593894,-0.209406829306347,-0.339673269554959));
#129175=DIRECTION('center_axis',(0.723576443046308,0.124498587364546,-0.678923583927297));
#129176=DIRECTION('ref_axis',(0.689983710452336,-0.157484279346239,0.706485089063614));
#129177=DIRECTION('center_axis',(-0.597901936131716,0.42611740395959,0.678923583927297));
#129178=DIRECTION('ref_axis',(-0.689983710452336,0.157484279346243,-0.706485089063614));
#129179=DIRECTION('center_axis',(0.560062137560471,0.828094259497534,-0.0242960790751506));
#129180=DIRECTION('ref_axis',(-0.560724628992771,0.40049549721625,0.724700798364696));
#129181=DIRECTION('center_axis',(-4.0181557197364E-32,5.03860790310193E-32,
-1.));
#129182=DIRECTION('ref_axis',(0.222520933956312,0.974927912181824,4.01815571973637E-32));
#129183=DIRECTION('center_axis',(-5.36469388482745E-35,-4.12026562461737E-32,
1.));
#129184=DIRECTION('ref_axis',(0.697509636265186,-0.716575402394757,-2.9487390722532E-32));
#129185=DIRECTION('center_axis',(4.0181557197364E-32,-5.03860790310193E-32,
1.));
#129186=DIRECTION('ref_axis',(-0.222520933956312,-0.974927912181824,-4.01815571973637E-32));
#129187=DIRECTION('center_axis',(-0.720894867331946,-0.124037195356078,
0.681854357192688));
#129188=DIRECTION('ref_axis',(-0.692740211901948,0.158113432814269,-0.703641344136153));
#129189=DIRECTION('center_axis',(-0.721529231161186,-0.124146344018081,
0.681163162426516));
#129190=DIRECTION('ref_axis',(-0.692090356308068,0.157965107515661,-0.704313824593084));
#129191=DIRECTION('center_axis',(0.596210294617465,-0.424911791723016,-0.681163162426516));
#129192=DIRECTION('ref_axis',(0.692090356308068,-0.157965107515664,0.704313824593083));
#129193=DIRECTION('center_axis',(0.595686110385987,-0.424538212026387,-0.681854357192686));
#129194=DIRECTION('ref_axis',(0.692740211901949,-0.158113432814256,0.703641344136154));
#129195=DIRECTION('center_axis',(4.0181557197364E-32,-5.03860790310193E-32,
1.));
#129196=DIRECTION('ref_axis',(-0.222520933956312,-0.974927912181824,-4.01815571973637E-32));
#129197=DIRECTION('center_axis',(-5.36469388482745E-35,-4.12026562461737E-32,
1.));
#129198=DIRECTION('ref_axis',(0.939344882287581,0.342974040009052,1.41818344493119E-32));
#129199=DIRECTION('center_axis',(4.0181557197364E-32,-5.03860790310193E-32,
1.));
#129200=DIRECTION('ref_axis',(0.222520933956292,0.974927912181829,4.01815571973647E-32));
#129201=DIRECTION('center_axis',(-4.0181557197364E-32,5.03860790310193E-32,
-1.));
#129202=DIRECTION('ref_axis',(-0.222520933956305,-0.974927912181826,-4.0181557197364E-32));
#129203=DIRECTION('center_axis',(-0.512068097591075,-0.858944854708064,
-1.9549442061076E-32));
#129204=DIRECTION('ref_axis',(0.858944854708064,-0.512068097591075,-5.91493596746345E-32));
#129205=DIRECTION('',(4.07953925466219E-32,-4.7080392753095E-32,1.));
#129206=DIRECTION('',(0.628582502897166,-0.374735403179047,-0.681511125848853));
#129207=DIRECTION('center_axis',(0.512072226953903,0.858942392933258,2.13514021047182E-6));
#129208=DIRECTION('ref_axis',(0.851673341205892,-0.507738342948244,-0.12982409244575));
#129209=DIRECTION('',(-8.07361552170662E-33,2.75729959521181E-32,-1.));
#129210=DIRECTION('center_axis',(-0.249333011548104,0.968417807225968,5.57651287942259E-32));
#129211=DIRECTION('ref_axis',(-0.968417807225968,-0.249333011548104,2.77682884849255E-32));
#129212=DIRECTION('center_axis',(0.24933301154813,-0.968417807225962,1.37386436630902E-14));
#129213=DIRECTION('ref_axis',(0.961153081584414,0.247462604055867,0.122257978695353));
#129214=DIRECTION('',(-0.708695658143485,-0.182463830587896,0.681511125848848));
#129215=DIRECTION('',(4.07953925466219E-32,-4.7080392753095E-32,1.));
#129216=DIRECTION('',(3.90320862897602E-33,-5.65788130115185E-32,1.));
#129217=DIRECTION('center_axis',(4.07953925466219E-32,-4.7080392753095E-32,
1.));
#129218=DIRECTION('ref_axis',(-0.142314838273275,-0.989821441880934,-4.07953925466219E-32));
#129219=DIRECTION('center_axis',(-0.336215887828166,0.0483405467659331,
-0.940543496235176));
#129220=DIRECTION('ref_axis',(0.930953148734462,-0.133971283531599,-0.339673269555151));
#129221=DIRECTION('center_axis',(-0.336215887828166,0.0483405467659331,
-0.940543496235176));
#129222=DIRECTION('ref_axis',(0.930953148734462,-0.133971283531599,-0.339673269555151));
#129223=DIRECTION('center_axis',(0.71102101146422,0.183062526049738,-0.678923583927297));
#129224=DIRECTION('ref_axis',(0.700524277354893,-0.100720185500137,0.706485089063614));
#129225=DIRECTION('center_axis',(-0.630644991066356,0.375964975004627,0.678923583927297));
#129226=DIRECTION('ref_axis',(-0.700524277354893,0.100720185500142,-0.706485089063613));
#129227=DIRECTION('center_axis',(0.490701207201861,0.870989107734654,-0.0242960790710487));
#129228=DIRECTION('ref_axis',(-0.591503219222111,0.353458754255722,0.724700524830686));
#129229=DIRECTION('center_axis',(-4.07953925466219E-32,4.7080392753095E-32,
-1.));
#129230=DIRECTION('ref_axis',(0.142314838273279,0.989821441880934,4.07953925466217E-32));
#129231=DIRECTION('center_axis',(-5.44664787004196E-35,-4.12070697124994E-32,
1.));
#129232=DIRECTION('ref_axis',(0.753596278147652,-0.657337546137452,-2.70459083526968E-32));
#129233=DIRECTION('center_axis',(4.07953925466219E-32,-4.7080392753095E-32,
1.));
#129234=DIRECTION('ref_axis',(-0.142314838273279,-0.989821441880934,-4.07953925466217E-32));
#129235=DIRECTION('center_axis',(-0.708385966203879,-0.182384095969861,
0.681854357192688));
#129236=DIRECTION('ref_axis',(-0.703322888621747,0.101122565053652,-0.703641344136153));
#129237=DIRECTION('center_axis',(-0.709009322610568,-0.182544587989925,
0.681163162426516));
#129238=DIRECTION('ref_axis',(-0.702663105479925,0.101027702559104,-0.704313824593084));
#129239=DIRECTION('center_axis',(0.628860709760055,-0.37490125883116,-0.681163162426516));
#129240=DIRECTION('ref_axis',(0.702663105479925,-0.101027702559108,0.704313824593083));
#129241=DIRECTION('center_axis',(0.628307819494945,-0.374571648071308,-0.681854357192686));
#129242=DIRECTION('ref_axis',(0.703322888621748,-0.101122565053635,0.703641344136154));
#129243=DIRECTION('center_axis',(4.07953925466219E-32,-4.7080392753095E-32,
1.));
#129244=DIRECTION('ref_axis',(-0.142314838273279,-0.989821441880934,-4.07953925466217E-32));
#129245=DIRECTION('center_axis',(-5.44664787004196E-35,-4.12070697124994E-32,
1.));
#129246=DIRECTION('ref_axis',(0.908263721405892,0.41839815054314,1.72904316836483E-32));
#129247=DIRECTION('center_axis',(4.07953925466219E-32,-4.7080392753095E-32,
1.));
#129248=DIRECTION('ref_axis',(0.142314838273279,0.989821441880934,4.07953925466217E-32));
#129249=DIRECTION('center_axis',(-4.07953925466219E-32,4.7080392753095E-32,
-1.));
#129250=DIRECTION('ref_axis',(-0.142314838273276,-0.989821441880934,-4.07953925466219E-32));
#129251=DIRECTION('center_axis',(-0.440352253525294,-0.897825090323942,
-2.11518871154494E-32));
#129252=DIRECTION('ref_axis',(0.897825090323942,-0.440352253525294,-5.61935982749661E-32));
#129253=DIRECTION('',(4.1137741289248E-32,-4.37356725940266E-32,1.));
#129254=DIRECTION('',(0.657035360706032,-0.322253192577091,-0.68151112584885));
#129255=DIRECTION('center_axis',(0.440356569805478,0.89782297332191,2.13514019612196E-6));
#129256=DIRECTION('ref_axis',(0.890224857059004,-0.436629601676368,-0.129824091809693));
#129257=DIRECTION('',(-6.93480934091059E-33,2.69603136483456E-32,-1.));
#129258=DIRECTION('center_axis',(-0.32743841816191,0.944872521725352,5.47947121877776E-32));
#129259=DIRECTION('ref_axis',(-0.944872521725352,-0.32743841816191,2.45491818986216E-32));
#129260=DIRECTION('center_axis',(0.327438418161922,-0.944872521725348,7.70890561095581E-15));
#129261=DIRECTION('ref_axis',(0.937784424431734,0.324982091713398,0.122257978712338));
#129262=DIRECTION('',(-0.691465035699815,-0.239621972592011,0.68151112584885));
#129263=DIRECTION('',(4.1137741289248E-32,-4.37356725940266E-32,1.));
#129264=DIRECTION('',(5.14252250029012E-33,-5.62095431222185E-32,1.));
#129265=DIRECTION('center_axis',(4.1137741289248E-32,-4.37356725940266E-32,
1.));
#129266=DIRECTION('ref_axis',(-0.0611616608218378,-0.998127873193367,-4.11377412892478E-32));
#129267=DIRECTION('center_axis',(-0.339037360530528,0.0207749814503773,
-0.940543496235145));
#129268=DIRECTION('ref_axis',(0.938775382266798,-0.0576441809680795,-0.339673269555239));
#129269=DIRECTION('center_axis',(-0.339037360530528,0.0207749814503773,
-0.940543496235145));
#129270=DIRECTION('ref_axis',(0.938775382266798,-0.0576441809680795,-0.339673269555239));
#129271=DIRECTION('center_axis',(0.693733852361048,0.24040821382726,-0.678923583927297));
#129272=DIRECTION('ref_axis',(0.706402970770023,-0.0432858154371954,0.706485089063614));
#129273=DIRECTION('center_axis',(-0.659191207634549,0.323310561170864,0.678923583927297));
#129274=DIRECTION('ref_axis',(-0.706402970770023,0.0432858154371997,-0.706485089063614));
#129275=DIRECTION('center_axis',(0.418074741256616,0.908087667169007,-0.0242960790821249));
#129276=DIRECTION('ref_axis',(-0.618344947077174,0.304069531647683,0.724700797810852));
#129277=DIRECTION('center_axis',(-4.1137741289248E-32,4.37356725940266E-32,
-1.));
#129278=DIRECTION('ref_axis',(0.0611616608218271,0.998127873193368,4.11377412892482E-32));
#129279=DIRECTION('center_axis',(-5.49235531231592E-35,-4.12115352934861E-32,
1.));
#129280=DIRECTION('ref_axis',(0.804667861133691,-0.593725216963649,-2.44241325155126E-32));
#129281=DIRECTION('center_axis',(4.1137741289248E-32,-4.37356725940266E-32,
1.));
#129282=DIRECTION('ref_axis',(-0.0611616608218271,-0.998127873193368,-4.11377412892482E-32));
#129283=DIRECTION('center_axis',(-0.691162873346182,-0.239517260516223,
0.681854357192688));
#129284=DIRECTION('ref_axis',(-0.709225067557877,0.0434587433066506,-0.703641344136153));
#129285=DIRECTION('center_axis',(-0.691771073996281,-0.239728027846433,
0.681163162426516));
#129286=DIRECTION('ref_axis',(-0.708559747616065,0.0434179749104152,-0.704313824593084));
#129287=DIRECTION('center_axis',(0.657326160633905,-0.322395819916137,-0.681163162426516));
#129288=DIRECTION('ref_axis',(0.708559747616065,-0.0434179749104186,0.704313824593084));
#129289=DIRECTION('center_axis',(0.656748243728657,-0.322112371598286,-0.681854357192686));
#129290=DIRECTION('ref_axis',(0.709225067557877,-0.0434587433066342,0.703641344136154));
#129291=DIRECTION('center_axis',(4.1137741289248E-32,-4.37356725940266E-32,
1.));
#129292=DIRECTION('ref_axis',(-0.0611616608218271,-0.998127873193368,-4.11377412892482E-32));
#129293=DIRECTION('center_axis',(-5.49235531231592E-35,-4.12115352934861E-32,
1.));
#129294=DIRECTION('ref_axis',(0.87113821531121,0.491037890416208,2.02842713573728E-32));
#129295=DIRECTION('center_axis',(4.1137741289248E-32,-4.37356725940266E-32,
1.));
#129296=DIRECTION('ref_axis',(0.0611616608218468,0.998127873193367,4.11377412892474E-32));
#129297=DIRECTION('center_axis',(-4.1137741289248E-32,4.37356725940266E-32,
-1.));
#129298=DIRECTION('ref_axis',(-0.061161660821833,-0.998127873193367,-4.1137741289248E-32));
#129299=DIRECTION('center_axis',(-0.365705937865311,-0.930730448094427,
-2.25080781720738E-32));
#129300=DIRECTION('ref_axis',(0.930730448094427,-0.365705937865311,-5.31170577792164E-32));
#129301=DIRECTION('',(4.12063251508437E-32,-4.03741771146329E-32,1.));
#129302=DIRECTION('',(0.681115756592598,-0.267626440146573,-0.681511125848849));
#129303=DIRECTION('center_axis',(0.365710412338692,0.930728689953471,2.13514017632895E-6));
#129304=DIRECTION('ref_axis',(0.922852073287589,-0.362615162399107,-0.129824091859205));
#129305=DIRECTION('',(-5.74985314811383E-33,2.64424932702918E-32,-1.));
#129306=DIRECTION('center_axis',(-0.403364776126385,0.915039265485646,5.35651374910222E-32));
#129307=DIRECTION('ref_axis',(-0.915039265485647,-0.403364776126385,2.14198845862598E-32));
#129308=DIRECTION('center_axis',(0.403364776126428,-0.915039265485627,1.55704628181689E-14));
#129309=DIRECTION('ref_axis',(0.908174966659921,0.400338877169377,0.122257978713101));
#129310=DIRECTION('',(-0.669632827527271,-0.295185469903366,0.681511125848845));
#129311=DIRECTION('',(4.12063251508437E-32,-4.03741771146329E-32,1.));
#129312=DIRECTION('',(6.34761373282129E-33,-5.57404863622719E-32,1.));
#129313=DIRECTION('center_axis',(4.12063251508437E-32,-4.03741771146329E-32,
1.));
#129314=DIRECTION('ref_axis',(0.0203985373914164,-0.999791928189206,-4.12063251508437E-32));
#129315=DIRECTION('center_axis',(-0.339602595535508,-0.00692883793910648,
-0.940543496235214));
#129316=DIRECTION('ref_axis',(0.940350220517251,0.0190665341093361,-0.339673269555047));
#129317=DIRECTION('center_axis',(-0.339602595535508,-0.00692883793910648,
-0.940543496235214));
#129318=DIRECTION('ref_axis',(0.940350220517251,0.0190665341093361,-0.339673269555047));
#129319=DIRECTION('center_axis',(0.671830008928442,0.296154024606325,-0.678923583927297));
#129320=DIRECTION('ref_axis',(0.707580668962965,0.0144366145858262,0.706485089063614));
#129321=DIRECTION('center_axis',(-0.683350615474828,0.268504568894996,0.678923583927297));
#129322=DIRECTION('ref_axis',(-0.707580668962965,-0.0144366145858181,-0.706485089063614));
#129323=DIRECTION('center_axis',(0.342666056897038,0.939143052996711,-0.0242960790798164));
#129324=DIRECTION('ref_axis',(-0.641072217977139,0.252657004280955,0.72470052402744));
#129325=DIRECTION('center_axis',(-4.12063251508437E-32,4.03741771146329E-32,
-1.));
#129326=DIRECTION('ref_axis',(-0.0203985373914165,0.999791928189206,4.12063251508437E-32));
#129327=DIRECTION('center_axis',(-5.50151203615979E-35,-4.12160232714292E-32,
1.));
#129328=DIRECTION('ref_axis',(0.850384512264717,-0.526161744428744,-2.16395106966151E-32));
#129329=DIRECTION('center_axis',(4.12063251508437E-32,-4.03741771146329E-32,
1.));
#129330=DIRECTION('ref_axis',(0.0203985373914165,-0.999791928189206,-4.12063251508437E-32));
#129331=DIRECTION('center_axis',(-0.669340205600213,-0.295056477211415,
0.681854357192688));
#129332=DIRECTION('ref_axis',(-0.710407470683308,-0.0144942892068705,-0.703641344136153));
#129333=DIRECTION('center_axis',(-0.669929203018742,-0.295316117229964,
0.681163162426516));
#129334=DIRECTION('ref_axis',(-0.70974104153595,-0.0144806921978409,-0.704313824593084));
#129335=DIRECTION('center_axis',(0.681417214359919,-0.267744890011138,-0.681163162426516));
#129336=DIRECTION('ref_axis',(0.70974104153595,0.014480692197839,0.704313824593084));
#129337=DIRECTION('center_axis',(0.680818116756189,-0.267509490437078,-0.681854357192686));
#129338=DIRECTION('ref_axis',(0.710407470683307,0.0144942892068817,0.703641344136154));
#129339=DIRECTION('center_axis',(4.12063251508437E-32,-4.03741771146329E-32,
1.));
#129340=DIRECTION('ref_axis',(0.0203985373914165,-0.999791928189206,-4.12063251508437E-32));
#129341=DIRECTION('center_axis',(-5.50151203615979E-35,-4.12160232714292E-32,
1.));
#129342=DIRECTION('ref_axis',(0.828215428121325,0.560409854144099,2.31434299614049E-32));
#129343=DIRECTION('center_axis',(4.12063251508437E-32,-4.03741771146329E-32,
1.));
#129344=DIRECTION('ref_axis',(-0.0203985373914165,0.999791928189206,4.12063251508437E-32));
#129345=DIRECTION('center_axis',(-4.12063251508437E-32,4.03741771146329E-32,
-1.));
#129346=DIRECTION('ref_axis',(0.0203985373914152,-0.999791928189206,-4.12063251508436E-32));
#129347=DIRECTION('center_axis',(-0.288625909526066,-0.957441948292559,
-2.36089900032231E-32));
#129348=DIRECTION('ref_axis',(0.957441948292559,-0.288625909526066,-4.99402120567912E-32));
#129349=DIRECTION('',(4.10006877171256E-32,-3.70182765127214E-32,1.));
#129350=DIRECTION('',(0.700663439495224,-0.211218677912134,-0.681511125848854));
#129351=DIRECTION('center_axis',(0.288630512415857,0.957440560712779,2.13514019988738E-6));
#129352=DIRECTION('ref_axis',(0.949337861193843,-0.286187579034176,-0.129824092180372));
#129353=DIRECTION('',(-4.52663263127535E-33,2.60229808271384E-32,-1.));
#129354=DIRECTION('center_axis',(-0.476606808056242,0.879116573904986,5.20845873207011E-32));
#129355=DIRECTION('ref_axis',(-0.879116573904986,-0.476606808056242,1.84012215051561E-32));
#129356=DIRECTION('center_axis',(0.476606808056274,-0.879116573904968,1.26700824892938E-14));
#129357=DIRECTION('ref_axis',(0.872521754329768,0.473031473452491,0.122257978654438));
#129358=DIRECTION('',(-0.643344323369171,-0.348784556614691,0.681511125848843));
#129359=DIRECTION('',(4.10006877171256E-32,-3.70182765127214E-32,1.));
#129360=DIRECTION('',(7.51046264324308E-33,-5.5174764227027E-32,1.));
#129361=DIRECTION('center_axis',(4.10006877171256E-32,-3.70182765127214E-32,
1.));
#129362=DIRECTION('ref_axis',(0.101822986703851,-0.994802532857002,-4.10006877171258E-32));
#129363=DIRECTION('center_axis',(-0.337907831297874,-0.0345865470552825,
-0.940543496235214));
#129364=DIRECTION('ref_axis',(0.935667183196969,0.0956503645473177,-0.339673269555046));
#129365=DIRECTION('center_axis',(-0.337907831297874,-0.0345865470552825,
-0.940543496235214));
#129366=DIRECTION('ref_axis',(0.935667183196969,0.0956503645473177,-0.339673269555046));
#129367=DIRECTION('center_axis',(0.645455247630566,0.349928979213609,-0.678923583927297));
#129368=DIRECTION('ref_axis',(0.704049534546552,0.0720629713206514,0.706485089063614));
#129369=DIRECTION('center_axis',(-0.702962437714038,0.211911723013268,0.678923583927297));
#129370=DIRECTION('ref_axis',(-0.704049534546553,-0.072062971320643,-0.706485089063614));
#129371=DIRECTION('center_axis',(0.264976986461482,0.96394859675559,-0.0242960790812061));
#129372=DIRECTION('ref_axis',(-0.65953300266963,0.199562973807333,0.724700515989023));
#129373=DIRECTION('center_axis',(-4.10006877171256E-32,3.70182765127214E-32,
-1.));
#129374=DIRECTION('ref_axis',(-0.101822986703844,0.994802532857003,4.10006877171255E-32));
#129375=DIRECTION('center_axis',(-5.47405710508952E-35,-4.1220503779576E-32,
1.));
#129376=DIRECTION('ref_axis',(0.890441994770205,-0.455096752295222,-1.87105740947765E-32));
#129377=DIRECTION('center_axis',(4.10006877171256E-32,-3.70182765127214E-32,
1.));
#129378=DIRECTION('ref_axis',(0.101822986703844,-0.994802532857003,-4.10006877171255E-32));
#129379=DIRECTION('center_axis',(-0.643063189219336,-0.348632141731658,
0.681854357192688));
#129380=DIRECTION('ref_axis',(-0.706862229300326,-0.072350864617104,-0.703641344136153));
#129381=DIRECTION('center_axis',(-0.643629063725651,-0.348938926577059,
0.681163162426516));
#129382=DIRECTION('ref_axis',(-0.706199125923442,-0.0722829926886655,-0.704313824593083));
#129383=DIRECTION('center_axis',(0.700973548950295,-0.211312162037912,-0.681163162426516));
#129384=DIRECTION('ref_axis',(0.706199125923442,0.0722829926886657,0.704313824593083));
#129385=DIRECTION('center_axis',(0.70035725754379,-0.211126377752971,-0.681854357192686));
#129386=DIRECTION('ref_axis',(0.706862229300322,0.0723508646171196,0.703641344136154));
#129387=DIRECTION('center_axis',(4.10006877171256E-32,-3.70182765127214E-32,
1.));
#129388=DIRECTION('ref_axis',(0.101822986703844,-0.994802532857003,-4.10006877171255E-32));
#129389=DIRECTION('center_axis',(-5.47405710508952E-35,-4.1220503779576E-32,
1.));
#129390=DIRECTION('ref_axis',(0.779781003903207,0.626052382753797,2.58488802669637E-32));
#129391=DIRECTION('center_axis',(4.10006877171256E-32,-3.70182765127214E-32,
1.));
#129392=DIRECTION('ref_axis',(-0.101822986703844,0.994802532857003,4.10006877171255E-32));
#129393=DIRECTION('center_axis',(-4.10006877171256E-32,3.70182765127214E-32,
-1.));
#129394=DIRECTION('ref_axis',(0.101822986703845,-0.994802532857003,-4.10006877171256E-32));
#129395=DIRECTION('center_axis',(-0.209625123378848,-0.977781830291606,
-2.44472962222986E-32));
#129396=DIRECTION('ref_axis',(0.977781830291606,-0.209625123378848,-4.66842024918305E-32));
#129397=DIRECTION('',(4.05221974712874E-32,-3.36903037531133E-32,1.));
#129398=DIRECTION('',(0.715548322809352,-0.153405290224818,-0.681511125848847));
#129399=DIRECTION('center_axis',(0.209629824053555,0.977780822507128,2.13514020421289E-6));
#129400=DIRECTION('ref_axis',(0.969505962273401,-0.207855464557473,-0.129824092409397));
#129401=DIRECTION('',(-3.27328812111754E-33,2.57045681049798E-32,-1.));
#129402=DIRECTION('center_axis',(-0.546677100313074,0.837343506569012,5.03629144939242E-32));
#129403=DIRECTION('ref_axis',(-0.837343506569012,-0.546677100313074,1.5513281360071E-32));
#129404=DIRECTION('center_axis',(0.54667710031302,-0.837343506569048,-3.81120151987269E-14));
#129405=DIRECTION('ref_axis',(0.831062053671047,0.542576123319591,0.122257978682561));
#129406=DIRECTION('',(-0.612774468883382,-0.400062539647147,0.681511125848848));
#129407=DIRECTION('',(4.05221974712874E-32,-3.36903037531133E-32,1.));
#129408=DIRECTION('',(8.62333066391321E-33,-5.45161415039564E-32,1.));
#129409=DIRECTION('center_axis',(4.05221974712873E-32,-3.36903037531133E-32,
1.));
#129410=DIRECTION('ref_axis',(0.182569820839374,-0.983192890799501,-4.05221974712874E-32));
#129411=DIRECTION('center_axis',(-0.333964346193833,-0.0620140884071742,
-0.94054349623521));
#129412=DIRECTION('ref_axis',(0.924757435146628,0.171597657591262,-0.339673269555057));
#129413=DIRECTION('center_axis',(-0.333964346193833,-0.0620140884071742,
-0.94054349623521));
#129414=DIRECTION('ref_axis',(0.924757435146628,0.171597657591262,-0.339673269555057));
#129415=DIRECTION('center_axis',(0.614785088152329,0.401375214198445,-0.678923583927297));
#129416=DIRECTION('ref_axis',(0.695833066637727,0.129209760870893,0.706485089063614));
#129417=DIRECTION('center_axis',(-0.717896160910899,0.153908639577859,0.678923583927297));
#129418=DIRECTION('ref_axis',(-0.695833066637729,-0.129209760870885,-0.706485089063614));
#129419=DIRECTION('center_axis',(0.185524537903959,0.982339221642399,-0.0242960790772642));
#129420=DIRECTION('ref_axis',(-0.673604703596412,0.145140883200304,0.724700508704544));
#129421=DIRECTION('center_axis',(-4.05221974712873E-32,3.36903037531133E-32,
-1.));
#129422=DIRECTION('ref_axis',(-0.182569820839372,0.983192890799501,4.05221974712873E-32));
#129423=DIRECTION('center_axis',(-5.41017322714046E-35,-4.12249470008839E-32,
1.));
#129424=DIRECTION('ref_axis',(0.924573732713069,-0.381003166360887,-1.56568142998441E-32));
#129425=DIRECTION('center_axis',(4.05221974712874E-32,-3.36903037531133E-32,
1.));
#129426=DIRECTION('ref_axis',(0.182569820839372,-0.983192890799501,-4.05221974712873E-32));
#129427=DIRECTION('center_axis',(-0.612506693412162,-0.399887716868931,
0.681854357192688));
#129428=DIRECTION('ref_axis',(-0.698612936405406,-0.129725956960371,-0.703641344136153));
#129429=DIRECTION('center_axis',(-0.613045679204787,-0.400239604938655,
0.681163162426516));
#129430=DIRECTION('ref_axis',(-0.697957571642567,-0.129604261789008,-0.704313824593084));
#129431=DIRECTION('center_axis',(0.715865020224902,-0.153473186490375,-0.681163162426516));
#129432=DIRECTION('ref_axis',(0.697957571642568,0.129604261789002,0.704313824593084));
#129433=DIRECTION('center_axis',(0.715235636333251,-0.153338253858317,-0.681854357192686));
#129434=DIRECTION('ref_axis',(0.698612936405403,0.129725956960381,0.703641344136154));
#129435=DIRECTION('center_axis',(4.05221974712873E-32,-3.36903037531133E-32,
1.));
#129436=DIRECTION('ref_axis',(0.182569820839373,-0.983192890799501,-4.05221974712874E-32));
#129437=DIRECTION('center_axis',(-5.41017322714046E-35,-4.12249470008839E-32,
1.));
#129438=DIRECTION('ref_axis',(0.726157265758936,0.687528636047624,2.83826179486323E-32));
#129439=DIRECTION('center_axis',(4.05221974712874E-32,-3.36903037531133E-32,
1.));
#129440=DIRECTION('ref_axis',(-0.182569820839373,0.983192890799501,4.05221974712874E-32));
#129441=DIRECTION('center_axis',(-4.05221974712873E-32,3.36903037531133E-32,
-1.));
#129442=DIRECTION('ref_axis',(0.182569820839372,-0.983192890799501,-4.05221974712874E-32));
#129443=DIRECTION('center_axis',(-0.129229316621256,-0.991614735532708,
-2.50174180397232E-32));
#129444=DIRECTION('ref_axis',(0.991614735532709,-0.129229316621256,-4.33706972907855E-32));
#129445=DIRECTION('',(3.97740386869697E-32,-3.04124059454469E-32,1.));
#129446=DIRECTION('',(0.725671350092338,-0.0945710156411471,-0.681511125848849));
#129447=DIRECTION('center_axis',(0.129234083798628,0.991614114250181,2.1351401914929E-6));
#129448=DIRECTION('ref_axis',(0.983222161215371,-0.12814010627372,-0.129824091982705));
#129449=DIRECTION('',(-1.99816041856823E-33,2.54893740879476E-32,-1.));
#129450=DIRECTION('center_axis',(-0.613109346662695,0.789998056348776,4.84115764592977E-32));
#129451=DIRECTION('ref_axis',(-0.789998056348776,-0.613109346662695,1.27752829161934E-32));
#129452=DIRECTION('center_axis',(0.613109346662686,-0.789998056348782,-1.11181245940181E-14));
#129453=DIRECTION('ref_axis',(0.784071772166395,0.608510018608646,0.122257978654787));
#129454=DIRECTION('',(-0.578126701407853,-0.448678172483924,0.681511125848846));
#129455=DIRECTION('',(3.97740386869697E-32,-3.04124059454469E-32,1.));
#129456=DIRECTION('',(9.67881184176439E-33,-5.3769001218617E-32,1.));
#129457=DIRECTION('center_axis',(3.97740386869697E-32,-3.04124059454469E-32,
1.));
#129458=DIRECTION('ref_axis',(0.262101682939114,-0.965040262269137,-3.97740386869697E-32));
#129459=DIRECTION('center_axis',(-0.327798383466007,-0.0890289362323012,
-0.940543496235245));
#129460=DIRECTION('ref_axis',(0.907693578939827,0.246402996534641,-0.339673269554961));
#129461=DIRECTION('center_axis',(-0.327798383466007,-0.0890289362323012,
-0.940543496235245));
#129462=DIRECTION('ref_axis',(0.907693578939827,0.246402996534641,-0.339673269554961));
#129463=DIRECTION('center_axis',(0.580023635344838,0.450150363355038,-0.678923583927297));
#129464=DIRECTION('ref_axis',(0.682985944474806,0.185496680780643,0.706485089063614));
#129465=DIRECTION('center_axis',(-0.728052403601427,0.0948813195391983,
0.678923583927297));
#129466=DIRECTION('ref_axis',(-0.682985944474806,-0.185496680780638,-0.706485089063615));
#129467=DIRECTION('center_axis',(0.104837454158456,0.994192541084149,-0.0242960790708589));
#129468=DIRECTION('ref_axis',(-0.683193733447373,0.0897529074021294,0.724700447213264));
#129469=DIRECTION('center_axis',(-3.97740386869697E-32,3.04124059454469E-32,
-1.));
#129470=DIRECTION('ref_axis',(-0.262101682939122,0.965040262269135,3.977403868697E-32));
#129471=DIRECTION('center_axis',(-5.31028553898035E-35,-4.12293233664482E-32,
1.));
#129472=DIRECTION('ref_axis',(0.952552585008677,-0.304374067215469,-1.24985535794147E-32));
#129473=DIRECTION('center_axis',(3.97740386869697E-32,-3.04124059454469E-32,
1.));
#129474=DIRECTION('ref_axis',(0.262101682939122,-0.965040262269135,-3.977403868697E-32));
#129475=DIRECTION('center_axis',(-0.577874066616821,-0.44848210522727,0.681854357192688));
#129476=DIRECTION('ref_axis',(-0.68571448968173,-0.186237744463338,-0.703641344136153));
#129477=DIRECTION('center_axis',(-0.578382576834232,-0.448876754764269,
0.681163162426516));
#129478=DIRECTION('ref_axis',(-0.685071224877307,-0.186063035910333,-0.704313824593083));
#129479=DIRECTION('center_axis',(0.725992527899326,-0.0946128722080396,
-0.681163162426516));
#129480=DIRECTION('ref_axis',(0.685071224877307,0.186063035910332,0.704313824593084));
#129481=DIRECTION('center_axis',(0.725354239968488,-0.0945296891832677,
-0.681854357192686));
#129482=DIRECTION('ref_axis',(0.685714489681727,0.186237744463349,0.703641344136154));
#129483=DIRECTION('center_axis',(3.97740386869697E-32,-3.04124059454469E-32,
1.));
#129484=DIRECTION('ref_axis',(0.262101682939122,-0.965040262269135,-3.977403868697E-32));
#129485=DIRECTION('center_axis',(-5.31028553898035E-35,-4.12293233664482E-32,
1.));
#129486=DIRECTION('ref_axis',(0.667701070818543,0.744429499702807,3.07277814001776E-32));
#129487=DIRECTION('center_axis',(3.97740386869697E-32,-3.04124059454469E-32,
1.));
#129488=DIRECTION('ref_axis',(-0.262101682939102,0.96504026226914,3.97740386869693E-32));
#129489=DIRECTION('center_axis',(-3.97740386869697E-32,3.04124059454469E-32,
-1.));
#129490=DIRECTION('ref_axis',(0.262101682939113,-0.965040262269137,-3.97740386869697E-32));
#129491=DIRECTION('center_axis',(-0.0479735100828851,-0.998848608313756,
-2.53155613888654E-32));
#129492=DIRECTION('ref_axis',(0.998848608313756,-0.0479735100828851,-4.00217472840792E-32));
#129493=DIRECTION('',(3.87611902374447E-32,-2.72063969588172E-32,1.));
#129494=DIRECTION('',(0.730965154267801,-0.0351073865515025,-0.681511125848855));
#129495=DIRECTION('center_axis',(0.0479783120381316,0.998848377667708,2.13514018274057E-6));
#129496=DIRECTION('ref_axis',(0.990395178825938,-0.0475719967119414,-0.12982409209071));
#129497=DIRECTION('',(-7.09735288106608E-34,2.53788308567206E-32,-1.));
#129498=DIRECTION('center_axis',(-0.675461451466197,0.737395299404043,4.6243559049494E-32));
#129499=DIRECTION('ref_axis',(-0.737395299404043,-0.675461451466197,1.02054471014294E-32));
#129500=DIRECTION('center_axis',(0.675461451466204,-0.737395299404037,2.77317066532683E-15));
#129501=DIRECTION('ref_axis',(0.731863622371199,0.670394380112939,0.122257978728159));
#129502=DIRECTION('',(-0.539631596118641,-0.494307926109512,0.681511125848846));
#129503=DIRECTION('',(3.87611902374447E-32,-2.72063969588172E-32,1.));
#129504=DIRECTION('',(1.06698821237002E-32,-5.29383154663383E-32,1.));
#129505=DIRECTION('center_axis',(3.87611902374447E-32,-2.72063969588172E-32,
1.));
#129506=DIRECTION('ref_axis',(0.339889301582633,-0.940465450013806,-3.87611902374448E-32));
#129507=DIRECTION('center_axis',(-0.319450976579395,-0.115451311175618,
-0.940543496235183));
#129508=DIRECTION('ref_axis',(0.88458917172373,0.319568564190617,-0.339673269555132));
#129509=DIRECTION('center_axis',(-0.319450976579395,-0.115451311175618,
-0.940543496235183));
#129510=DIRECTION('ref_axis',(0.88458917172373,0.319568564190617,-0.339673269555132));
#129511=DIRECTION('center_axis',(0.54140222094129,0.495929836113086,-0.678923583927297));
#129512=DIRECTION('ref_axis',(0.66559366353615,0.240549150884602,0.706485089063614));
#129513=DIRECTION('center_axis',(-0.733363577666179,0.0352225799733199,
0.678923583927297));
#129514=DIRECTION('ref_axis',(-0.665593663536153,-0.240549150884596,-0.706485089063614));
#129515=DIRECTION('center_axis',(0.0234526944418836,0.999429673196143,-0.0242960790759765));
#129516=DIRECTION('ref_axis',(-0.68823614950775,0.0337676302669961,0.724700455123975));
#129517=DIRECTION('center_axis',(-3.87611902374447E-32,2.72063969588172E-32,
-1.));
#129518=DIRECTION('ref_axis',(-0.339889301582625,0.940465450013808,3.87611902374446E-32));
#129519=DIRECTION('center_axis',(-5.17505877669431E-35,-4.12336037522781E-32,
1.));
#129520=DIRECTION('ref_axis',(0.974192357011155,-0.225719408870948,-9.25680963750974E-33));
#129521=DIRECTION('center_axis',(3.87611902374447E-32,-2.72063969588172E-32,
1.));
#129522=DIRECTION('ref_axis',(0.339889301582624,-0.940465450013809,-3.87611902374446E-32));
#129523=DIRECTION('center_axis',(-0.539395783250655,-0.494091919169661,
0.681854357192688));
#129524=DIRECTION('ref_axis',(-0.668252726164151,-0.241510150503965,-0.703641344136153));
#129525=DIRECTION('center_axis',(-0.539870433841254,-0.49452670384638,0.681163162426516));
#129526=DIRECTION('ref_axis',(-0.667625842139282,-0.241283591225921,-0.704313824593083));
#129527=DIRECTION('center_axis',(0.731288675080916,-0.0351229248711846,
-0.681163162426516));
#129528=DIRECTION('ref_axis',(0.667625842139283,0.241283591225917,0.704313824593084));
#129529=DIRECTION('center_axis',(0.730645730811761,-0.0350920450230047,
-0.681854357192686));
#129530=DIRECTION('ref_axis',(0.668252726164146,0.241510150503977,0.703641344136154));
#129531=DIRECTION('center_axis',(3.87611902374447E-32,-2.72063969588172E-32,
1.));
#129532=DIRECTION('ref_axis',(0.339889301582624,-0.940465450013809,-3.87611902374446E-32));
#129533=DIRECTION('center_axis',(-5.17505877669431E-35,-4.12336037522781E-32,
1.));
#129534=DIRECTION('ref_axis',(0.604801435414776,0.796376307859687,3.28687639457536E-32));
#129535=DIRECTION('center_axis',(3.87611902374447E-32,-2.72063969588172E-32,
1.));
#129536=DIRECTION('ref_axis',(-0.339889301582644,0.940465450013802,3.87611902374452E-32));
#129537=DIRECTION('center_axis',(-3.87611902374447E-32,2.72063969588172E-32,
-1.));
#129538=DIRECTION('ref_axis',(0.339889301582627,-0.940465450013808,-3.87611902374447E-32));
#129539=DIRECTION('center_axis',(0.0336015522500152,-0.999435308404896,
-2.53397421749269E-32));
#129540=DIRECTION('ref_axis',(0.999435308404896,0.0336015522500152,-3.66596391814683E-32));
#129541=DIRECTION('',(3.74903924620357E-32,-2.40936122540758E-32,1.));
#129542=DIRECTION('',(0.731394505942384,0.0245898764033321,-0.681511125848849));
#129543=DIRECTION('center_axis',(-0.0335967474730231,0.999435469930238,
2.13514021539847E-6));
#129544=DIRECTION('ref_axis',(0.990977279923771,0.0333126966366988,-0.129824092208173));
#129545=DIRECTION('',(5.8341301359928E-34,2.53736740582643E-32,-1.));
#129546=DIRECTION('center_axis',(-0.733318471753486,0.679885298403438,4.38732900626775E-32));
#129547=DIRECTION('ref_axis',(-0.679885298403438,-0.733318471753486,7.82087574913321E-33));
#129548=DIRECTION('center_axis',(0.73331847175353,-0.67988529840339,3.17515320213748E-14));
#129549=DIRECTION('ref_axis',(0.674785040937491,0.727817377643653,0.122257978581793));
#129550=DIRECTION('',(-0.497545331590206,-0.536648142041902,0.68151112584885));
#129551=DIRECTION('',(3.74903924620357E-32,-2.40936122540758E-32,1.));
#129552=DIRECTION('',(1.15899461005094E-32,-5.20296123237482E-32,1.));
#129553=DIRECTION('center_axis',(3.74903924620357E-32,-2.40936122540758E-32,
1.));
#129554=DIRECTION('ref_axis',(0.415415013001901,-0.909631995354512,-3.74903924620359E-32));
#129555=DIRECTION('center_axis',(-0.308977676149106,-0.141105376691099,
-0.940543496235214));
#129556=DIRECTION('ref_axis',(0.855597969517219,0.390607455775997,-0.339673269555045));
#129557=DIRECTION('center_axis',(-0.308977676149106,-0.141105376691099,
-0.940543496235214));
#129558=DIRECTION('ref_axis',(0.855597969517219,0.390607455775997,-0.339673269555045));
#129559=DIRECTION('center_axis',(0.499177864082457,0.538408977634465,-0.678923583927297));
#129560=DIRECTION('ref_axis',(0.643771966581886,0.294000806077242,0.706485089063615));
#129561=DIRECTION('center_axis',(-0.733794338118036,-0.0246705600509643,
0.678923583927297));
#129562=DIRECTION('ref_axis',(-0.64377196658189,-0.294000806077234,-0.706485089063614));
#129563=DIRECTION('center_axis',(-0.0580881390785779,0.998015765727227,
-0.0242960790722294));
#129564=DIRECTION('ref_axis',(-0.688697894046278,-0.0224423168364948,0.724701009486831));
#129565=DIRECTION('center_axis',(-3.74903924620357E-32,2.40936122540758E-32,
-1.));
#129566=DIRECTION('ref_axis',(-0.415415013001888,0.909631995354518,3.74903924620355E-32));
#129567=DIRECTION('center_axis',(-5.00539285207335E-35,-4.12377596731122E-32,
1.));
#129568=DIRECTION('ref_axis',(0.989349039608153,-0.145562625101453,-5.95315574521045E-33));
#129569=DIRECTION('center_axis',(3.74903924620357E-32,-2.40936122540758E-32,
1.));
#129570=DIRECTION('ref_axis',(0.415415013001888,-0.909631995354518,-3.74903924620355E-32));
#129571=DIRECTION('center_axis',(-0.497327909940996,-0.536413632909406,
0.681854357192688));
#129572=DIRECTION('ref_axis',(-0.646343851007884,-0.295175346339365,-0.703641344136154));
#129573=DIRECTION('center_axis',(-0.497765542183414,-0.536885659305555,
0.681163162426516));
#129574=DIRECTION('ref_axis',(-0.64573751957233,-0.294898444050892,-0.704313824593084));
#129575=DIRECTION('center_axis',(0.731718216783981,0.0246007597358135,-0.681163162426516));
#129576=DIRECTION('ref_axis',(0.645737519572332,0.294898444050891,0.704313824593083));
#129577=DIRECTION('center_axis',(0.731074894864541,0.0245791309071065,-0.681854357192686));
#129578=DIRECTION('ref_axis',(0.64634385100788,0.295175346339376,0.703641344136153));
#129579=DIRECTION('center_axis',(3.74903924620357E-32,-2.40936122540758E-32,
1.));
#129580=DIRECTION('ref_axis',(0.415415013001888,-0.909631995354518,-3.74903924620355E-32));
#129581=DIRECTION('center_axis',(-5.00539285207335E-35,-4.12377596731122E-32,
1.));
#129582=DIRECTION('ref_axis',(0.537876946243533,0.843023363080604,3.4791317699757E-32));
#129583=DIRECTION('center_axis',(3.74903924620357E-32,-2.40936122540758E-32,
1.));
#129584=DIRECTION('ref_axis',(-0.415415013001928,0.9096319953545,3.74903924620366E-32));
#129585=DIRECTION('center_axis',(-3.74903924620357E-32,2.40936122540758E-32,
-1.));
#129586=DIRECTION('ref_axis',(0.415415013001897,-0.909631995354514,-3.74903924620357E-32));
#129587=DIRECTION('center_axis',(0.114953001796558,-0.99337093141382,-2.5089799478766E-32));
#129588=DIRECTION('ref_axis',(0.99337093141382,0.114953001796558,-3.33067472576671E-32));
#129589=DIRECTION('',(3.59701023102713E-32,-2.10947668998596E-32,1.));
#129590=DIRECTION('',(0.726956547851512,0.0841234977877359,-0.681511125848852));
#129591=DIRECTION('center_axis',(-0.114948226172968,0.99337148403562,2.13514017304701E-6));
#129592=DIRECTION('ref_axis',(0.984964590732422,0.113975699484092,-0.129824092257272));
#129593=DIRECTION('',(1.87267879795604E-33,2.54739380102217E-32,-1.));
#129594=DIRECTION('center_axis',(-0.786295378600288,0.617850772915135,4.13165432478888E-32));
#129595=DIRECTION('ref_axis',(-0.617850772915135,-0.786295378600288,5.63743778822766E-33));
#129596=DIRECTION('center_axis',(0.786295378600298,-0.617850772915122,1.21103599696864E-14));
#129597=DIRECTION('ref_axis',(0.613215876366603,0.780396870584852,0.122257978689773));
#129598=DIRECTION('',(-0.452147984969242,-0.575417053129717,0.68151112584885));
#129599=DIRECTION('',(3.59701023102713E-32,-2.10947668998596E-32,1.));
#129600=DIRECTION('',(1.24328808982262E-32,-5.10489390603351E-32,1.));
#129601=DIRECTION('center_axis',(3.59701023102713E-32,-2.10947668998596E-32,
1.));
#129602=DIRECTION('ref_axis',(0.48817620604829,-0.872745089844851,-3.59701023102713E-32));
#129603=DIRECTION('center_axis',(-0.29644818026194,-0.165820409205535,-0.940543496235179));
#129604=DIRECTION('ref_axis',(0.820912903986917,0.459046919189624,-0.339673269555144));
#129605=DIRECTION('center_axis',(-0.29644818026194,-0.165820409205535,-0.940543496235179));
#129606=DIRECTION('ref_axis',(0.820912903986917,0.459046919189624,-0.339673269555144));
#129607=DIRECTION('center_axis',(0.453631560896706,0.577305096240915,-0.678923583927297));
#129608=DIRECTION('ref_axis',(0.617666073404923,0.345495934412147,0.706485089063613));
#129609=DIRECTION('center_axis',(-0.729341818317261,-0.0843995215684652,
0.678923583927297));
#129610=DIRECTION('ref_axis',(-0.617666073404925,-0.345495934412141,-0.706485089063615));
#129611=DIRECTION('center_axis',(-0.139242405632141,0.989960227996504,-0.024296079084576));
#129612=DIRECTION('ref_axis',(-0.684577178647174,-0.0785029346967517,0.724700887069605));
#129613=DIRECTION('center_axis',(-3.59701023102713E-32,2.10947668998596E-32,
-1.));
#129614=DIRECTION('ref_axis',(-0.48817620604829,0.872745089844851,3.59701023102713E-32));
#129615=DIRECTION('center_axis',(-4.80241686385389E-35,-4.1241763471983E-32,
1.));
#129616=DIRECTION('ref_axis',(0.997921767577655,-0.0644371460780812,-2.60957717410763E-33));
#129617=DIRECTION('center_axis',(3.59701023102713E-32,-2.10947668998597E-32,
1.));
#129618=DIRECTION('ref_axis',(0.48817620604829,-0.872745089844851,-3.59701023102713E-32));
#129619=DIRECTION('center_axis',(-0.451950401444009,-0.575165602424159,
0.681854357192688));
#129620=DIRECTION('ref_axis',(-0.620133664162392,-0.346876198945375,-0.703641344136154));
#129621=DIRECTION('center_axis',(-0.452348102967877,-0.575671729281951,
0.681163162426516));
#129622=DIRECTION('ref_axis',(-0.619551920351823,-0.346550796385513,-0.704313824593082));
#129623=DIRECTION('center_axis',(0.727278294479357,0.0841607303456094,-0.681163162426516));
#129624=DIRECTION('ref_axis',(0.619551920351821,0.346550796385511,0.704313824593085));
#129625=DIRECTION('center_axis',(0.726638876110865,0.0840867367763019,-0.681854357192686));
#129626=DIRECTION('ref_axis',(0.620133664162387,0.346876198945386,0.703641344136153));
#129627=DIRECTION('center_axis',(3.59701023102713E-32,-2.10947668998596E-32,
1.));
#129628=DIRECTION('ref_axis',(0.48817620604829,-0.872745089844851,-3.59701023102713E-32));
#129629=DIRECTION('center_axis',(-4.80241686385389E-35,-4.1241763471983E-32,
1.));
#129630=DIRECTION('ref_axis',(0.467372974738516,0.884060236909268,3.64826483841532E-32));
#129631=DIRECTION('center_axis',(3.59701023102713E-32,-2.10947668998597E-32,
1.));
#129632=DIRECTION('ref_axis',(-0.488176206048286,0.872745089844853,3.59701023102712E-32));
#129633=DIRECTION('center_axis',(-3.59701023102713E-32,2.10947668998596E-32,
-1.));
#129634=DIRECTION('ref_axis',(0.488176206048291,-0.872745089844851,-3.59701023102713E-32));
#129635=DIRECTION('center_axis',(0.195539458082054,-0.980695834768853,-2.45673966277879E-32));
#129636=DIRECTION('ref_axis',(0.980695834768853,0.195539458082054,-2.99853844552401E-32));
#129637=DIRECTION('',(3.42104370622812E-32,-1.82298177172263E-32,1.));
#129638=DIRECTION('',(0.717680813874082,0.143097291173771,-0.681511125848848));
#129639=DIRECTION('center_axis',(-0.195534743392682,0.980696774809523,2.13514020054857E-6));
#129640=DIRECTION('ref_axis',(0.97239712468431,0.193880212852231,-0.129824092409923));
#129641=DIRECTION('',(3.14948221388265E-33,2.56789554725347E-32,-1.));
#129642=DIRECTION('center_axis',(-0.83403961943211,0.551704552471285,3.85903333333466E-32));
#129643=DIRECTION('ref_axis',(-0.551704552471285,-0.83403961943211,3.66966363810075E-33));
#129644=DIRECTION('center_axis',(0.834039619432123,-0.551704552471265,-1.65372562611265E-15));
#129645=DIRECTION('ref_axis',(0.54756586131972,0.827782951116591,0.122257978708552));
#129646=DIRECTION('',(-0.403741668107477,-0.610356658666085,0.681511125848848));
#129647=DIRECTION('',(3.42104370622812E-32,-1.82298177172263E-32,1.));
#129648=DIRECTION('',(1.31930769248463E-32,-5.00028218948674E-32,1.));
#129649=DIRECTION('center_axis',(3.42104370622812E-32,-1.82298177172263E-32,
1.));
#129650=DIRECTION('ref_axis',(0.557688666986836,-0.830050209755076,-3.42104370622811E-32));
#129651=DIRECTION('center_axis',(-0.281945870645394,-0.189431934254999,
-0.940543496235246));
#129652=DIRECTION('ref_axis',(0.780764798521982,0.524431501093111,-0.339673269554957));
#129653=DIRECTION('center_axis',(-0.281945870645394,-0.189431934254999,
-0.940543496235246));
#129654=DIRECTION('ref_axis',(0.780764798521982,0.524431501093111,-0.339673269554957));
#129655=DIRECTION('center_axis',(0.405066414517127,0.612359344680518,-0.678923583927297));
#129656=DIRECTION('ref_axis',(0.587449714417171,0.394691844306367,0.706485089063614));
#129657=DIRECTION('center_axis',(-0.720035649048515,-0.143566818194869,
0.678923583927297));
#129658=DIRECTION('ref_axis',(-0.587449714417177,-0.394691844306358,-0.706485089063614));
#129659=DIRECTION('center_axis',(-0.219470036920007,0.97531666828596,-0.0242960790644273));
#129660=DIRECTION('ref_axis',(-0.675901111825593,-0.134041249019664,0.724700372977809));
#129661=DIRECTION('center_axis',(-3.42104370622812E-32,1.82298177172263E-32,
-1.));
#129662=DIRECTION('ref_axis',(-0.557688666986844,0.830050209755071,3.42104370622813E-32));
#129663=DIRECTION('center_axis',(-4.56748158374851E-35,-4.12455885042696E-32,
1.));
#129664=DIRECTION('ref_axis',(0.999853490829434,0.0171171515210855,7.51675112062014E-34));
#129665=DIRECTION('center_axis',(3.42104370622812E-32,-1.82298177172263E-32,
1.));
#129666=DIRECTION('ref_axis',(0.557688666986844,-0.830050209755071,-3.42104370622813E-32));
#129667=DIRECTION('center_axis',(-0.40356523759198,-0.610089939750423,0.681854357192688));
#129668=DIRECTION('ref_axis',(-0.589796590096757,-0.396268647677944,-0.703641344136153));
#129669=DIRECTION('center_axis',(-0.403920361759272,-0.610626798879125,
0.681163162426516));
#129670=DIRECTION('ref_axis',(-0.589243305320234,-0.39589691034706,-0.704313824593084));
#129671=DIRECTION('center_axis',(0.717998455117445,0.143160625180498,-0.681163162426516));
#129672=DIRECTION('ref_axis',(0.589243305320236,0.395896910347057,0.704313824593083));
#129673=DIRECTION('center_axis',(0.717367195523647,0.143034759285586,-0.681854357192686));
#129674=DIRECTION('ref_axis',(0.589796590096751,0.396268647677949,0.703641344136156));
#129675=DIRECTION('center_axis',(3.42104370622812E-32,-1.82298177172263E-32,
1.));
#129676=DIRECTION('ref_axis',(0.557688666986844,-0.830050209755071,-3.42104370622813E-32));
#129677=DIRECTION('center_axis',(-4.56748158374851E-35,-4.12455885042696E-32,
1.));
#129678=DIRECTION('ref_axis',(0.393758713197697,0.919213835720989,3.79315004722889E-32));
#129679=DIRECTION('center_axis',(3.42104370622812E-32,-1.82298177172263E-32,
1.));
#129680=DIRECTION('ref_axis',(-0.557688666986862,0.830050209755059,3.42104370622817E-32));
#129681=DIRECTION('center_axis',(-3.42104370622812E-32,1.82298177172263E-32,
-1.));
#129682=DIRECTION('ref_axis',(0.557688666986839,-0.830050209755074,-3.42104370622812E-32));
#129683=DIRECTION('axis',(0.,0.,1.));
#129684=DIRECTION('refdir',(1.,0.,0.));
#129685=DIRECTION('axis',(0.,0.,1.));
#129686=DIRECTION('refdir',(1.,0.,0.));
#129687=DIRECTION('center_axis',(0.,-1.,0.));
#129688=DIRECTION('ref_axis',(0.707106781186548,0.,0.707106781186547));
#129689=DIRECTION('',(0.,-1.,0.));
#129690=DIRECTION('center_axis',(0.,1.,0.));
#129691=DIRECTION('ref_axis',(0.707106781186548,0.,0.707106781186547));
#129692=DIRECTION('center_axis',(0.,-1.,0.));
#129693=DIRECTION('ref_axis',(0.707106781186548,0.,0.707106781186547));
#129694=DIRECTION('',(0.,-1.,0.));
#129695=DIRECTION('center_axis',(0.,1.,0.));
#129696=DIRECTION('ref_axis',(0.707106781186548,0.,0.707106781186547));
#129697=DIRECTION('center_axis',(0.,-1.,0.));
#129698=DIRECTION('ref_axis',(0.707106781186548,0.,0.707106781186547));
#129699=DIRECTION('',(0.,-1.,0.));
#129700=DIRECTION('center_axis',(0.,-1.,0.));
#129701=DIRECTION('ref_axis',(0.707106781186548,0.,0.707106781186547));
#129702=DIRECTION('',(0.,-1.,0.));
#129703=DIRECTION('center_axis',(0.,-1.,0.));
#129704=DIRECTION('ref_axis',(0.707106781186548,0.,0.707106781186547));
#129705=DIRECTION('',(0.,-1.,0.));
#129706=DIRECTION('center_axis',(0.,-1.,0.));
#129707=DIRECTION('ref_axis',(0.707106781186548,0.,0.707106781186547));
#129708=DIRECTION('',(0.,-1.,0.));
#129709=DIRECTION('center_axis',(0.,-1.,0.));
#129710=DIRECTION('ref_axis',(0.707106781186548,0.,0.707106781186547));
#129711=DIRECTION('',(0.,-1.,0.));
#129712=DIRECTION('center_axis',(0.,-1.,0.));
#129713=DIRECTION('ref_axis',(0.409955339817897,0.,0.912105596603152));
#129714=DIRECTION('',(0.,-1.,0.));
#129715=DIRECTION('center_axis',(0.,-1.,0.));
#129716=DIRECTION('ref_axis',(0.707106781186548,0.,0.707106781186547));
#129717=DIRECTION('center_axis',(0.,-1.,0.));
#129718=DIRECTION('ref_axis',(0.843556936084309,0.,-0.53703975233129));
#129719=DIRECTION('',(8.6595605623547E-17,-1.,8.65956056235516E-17));
#129720=DIRECTION('center_axis',(0.,1.,0.));
#129721=DIRECTION('ref_axis',(0.707106781186529,0.,0.707106781186566));
#129722=DIRECTION('center_axis',(0.,-1.,0.));
#129723=DIRECTION('ref_axis',(0.707106781186529,0.,0.707106781186566));
#129724=DIRECTION('',(8.6595605623547E-17,-1.,8.65956056235516E-17));
#129725=DIRECTION('center_axis',(0.,-1.,0.));
#129726=DIRECTION('ref_axis',(0.707106781186529,0.,0.707106781186566));
#129727=DIRECTION('',(8.6595605623547E-17,-1.,8.65956056235516E-17));
#129728=DIRECTION('center_axis',(0.,-1.,0.));
#129729=DIRECTION('ref_axis',(0.707106781186529,0.,0.707106781186566));
#129730=DIRECTION('',(8.6595605623547E-17,-1.,8.65956056235516E-17));
#129731=DIRECTION('center_axis',(0.,-1.,0.));
#129732=DIRECTION('ref_axis',(0.707106781186529,0.,0.707106781186566));
#129733=DIRECTION('',(8.6595605623547E-17,-1.,8.65956056235516E-17));
#129734=DIRECTION('center_axis',(0.,-1.,0.));
#129735=DIRECTION('ref_axis',(0.707106781186529,0.,0.707106781186566));
#129736=DIRECTION('',(8.6595605623547E-17,-1.,8.65956056235516E-17));
#129737=DIRECTION('center_axis',(0.,-1.,0.));
#129738=DIRECTION('ref_axis',(0.707106781186529,0.,0.707106781186566));
#129739=DIRECTION('',(8.6595605623547E-17,-1.,8.65956056235516E-17));
#129740=DIRECTION('center_axis',(0.,-1.,0.));
#129741=DIRECTION('ref_axis',(-0.991406989026756,0.,0.130813539470888));
#129742=DIRECTION('',(8.6595605623547E-17,-1.,8.65956056235516E-17));
#129743=DIRECTION('center_axis',(0.,-1.,0.));
#129744=DIRECTION('ref_axis',(0.707106781186529,0.,0.707106781186566));
#129745=DIRECTION('center_axis',(0.,-1.,0.));
#129746=DIRECTION('ref_axis',(0.707106781186547,0.,-0.707106781186548));
#129747=DIRECTION('',(0.,-1.,0.));
#129748=DIRECTION('center_axis',(0.,1.,0.));
#129749=DIRECTION('ref_axis',(0.707106781186547,0.,-0.707106781186548));
#129750=DIRECTION('center_axis',(0.,-1.,0.));
#129751=DIRECTION('ref_axis',(0.707106781186547,0.,-0.707106781186548));
#129752=DIRECTION('',(0.,-1.,0.));
#129753=DIRECTION('center_axis',(0.,1.,0.));
#129754=DIRECTION('ref_axis',(0.707106781186547,0.,-0.707106781186548));
#129755=DIRECTION('center_axis',(0.,-1.,0.));
#129756=DIRECTION('ref_axis',(0.707106781186547,0.,-0.707106781186548));
#129757=DIRECTION('',(0.,-1.,0.));
#129758=DIRECTION('center_axis',(0.,-1.,0.));
#129759=DIRECTION('ref_axis',(0.707106781186547,0.,-0.707106781186548));
#129760=DIRECTION('',(0.,-1.,0.));
#129761=DIRECTION('center_axis',(0.,-1.,0.));
#129762=DIRECTION('ref_axis',(0.707106781186547,0.,-0.707106781186548));
#129763=DIRECTION('',(0.,-1.,0.));
#129764=DIRECTION('center_axis',(0.,-1.,0.));
#129765=DIRECTION('ref_axis',(0.707106781186547,0.,-0.707106781186548));
#129766=DIRECTION('',(0.,-1.,0.));
#129767=DIRECTION('center_axis',(0.,-1.,0.));
#129768=DIRECTION('ref_axis',(0.707106781186547,0.,-0.707106781186548));
#129769=DIRECTION('',(0.,-1.,0.));
#129770=DIRECTION('center_axis',(0.,-1.,0.));
#129771=DIRECTION('ref_axis',(0.912105596603152,0.,-0.409955339817897));
#129772=DIRECTION('',(0.,-1.,0.));
#129773=DIRECTION('center_axis',(0.,-1.,0.));
#129774=DIRECTION('ref_axis',(0.707106781186547,0.,-0.707106781186548));
#129775=DIRECTION('center_axis',(0.,-1.,0.));
#129776=DIRECTION('ref_axis',(-0.53703975233129,0.,-0.843556936084309));
#129777=DIRECTION('',(8.65956056235516E-17,-1.,-8.6595605623547E-17));
#129778=DIRECTION('center_axis',(0.,1.,0.));
#129779=DIRECTION('ref_axis',(0.707106781186566,0.,-0.707106781186529));
#129780=DIRECTION('center_axis',(0.,-1.,0.));
#129781=DIRECTION('ref_axis',(0.707106781186566,0.,-0.707106781186529));
#129782=DIRECTION('',(8.65956056235516E-17,-1.,-8.6595605623547E-17));
#129783=DIRECTION('center_axis',(0.,-1.,0.));
#129784=DIRECTION('ref_axis',(0.707106781186566,0.,-0.707106781186529));
#129785=DIRECTION('',(8.65956056235516E-17,-1.,-8.6595605623547E-17));
#129786=DIRECTION('center_axis',(0.,-1.,0.));
#129787=DIRECTION('ref_axis',(0.707106781186566,0.,-0.707106781186529));
#129788=DIRECTION('',(8.65956056235516E-17,-1.,-8.6595605623547E-17));
#129789=DIRECTION('center_axis',(0.,-1.,0.));
#129790=DIRECTION('ref_axis',(0.707106781186566,0.,-0.707106781186529));
#129791=DIRECTION('',(8.65956056235516E-17,-1.,-8.6595605623547E-17));
#129792=DIRECTION('center_axis',(0.,-1.,0.));
#129793=DIRECTION('ref_axis',(0.707106781186566,0.,-0.707106781186529));
#129794=DIRECTION('',(8.65956056235516E-17,-1.,-8.6595605623547E-17));
#129795=DIRECTION('center_axis',(0.,-1.,0.));
#129796=DIRECTION('ref_axis',(0.707106781186566,0.,-0.707106781186529));
#129797=DIRECTION('',(8.65956056235516E-17,-1.,-8.6595605623547E-17));
#129798=DIRECTION('center_axis',(0.,-1.,0.));
#129799=DIRECTION('ref_axis',(0.130813539470888,0.,0.991406989026756));
#129800=DIRECTION('',(8.65956056235516E-17,-1.,-8.6595605623547E-17));
#129801=DIRECTION('center_axis',(0.,-1.,0.));
#129802=DIRECTION('ref_axis',(0.707106781186566,0.,-0.707106781186529));
#129803=DIRECTION('center_axis',(0.,-1.,0.));
#129804=DIRECTION('ref_axis',(-0.707106781186548,0.,-0.707106781186547));
#129805=DIRECTION('',(0.,-1.,0.));
#129806=DIRECTION('center_axis',(0.,1.,0.));
#129807=DIRECTION('ref_axis',(-0.707106781186548,0.,-0.707106781186547));
#129808=DIRECTION('center_axis',(0.,-1.,0.));
#129809=DIRECTION('ref_axis',(-0.707106781186548,0.,-0.707106781186547));
#129810=DIRECTION('',(0.,-1.,0.));
#129811=DIRECTION('center_axis',(0.,1.,0.));
#129812=DIRECTION('ref_axis',(-0.707106781186548,0.,-0.707106781186547));
#129813=DIRECTION('center_axis',(0.,-1.,0.));
#129814=DIRECTION('ref_axis',(-0.707106781186548,0.,-0.707106781186547));
#129815=DIRECTION('',(0.,-1.,0.));
#129816=DIRECTION('center_axis',(0.,-1.,0.));
#129817=DIRECTION('ref_axis',(-0.707106781186548,0.,-0.707106781186547));
#129818=DIRECTION('',(0.,-1.,0.));
#129819=DIRECTION('center_axis',(0.,-1.,0.));
#129820=DIRECTION('ref_axis',(-0.707106781186548,0.,-0.707106781186547));
#129821=DIRECTION('',(0.,-1.,0.));
#129822=DIRECTION('center_axis',(0.,-1.,0.));
#129823=DIRECTION('ref_axis',(-0.707106781186548,0.,-0.707106781186547));
#129824=DIRECTION('',(0.,-1.,0.));
#129825=DIRECTION('center_axis',(0.,-1.,0.));
#129826=DIRECTION('ref_axis',(-0.707106781186548,0.,-0.707106781186547));
#129827=DIRECTION('',(0.,-1.,0.));
#129828=DIRECTION('center_axis',(0.,-1.,0.));
#129829=DIRECTION('ref_axis',(-0.409955339817898,0.,-0.912105596603152));
#129830=DIRECTION('',(0.,-1.,0.));
#129831=DIRECTION('center_axis',(0.,-1.,0.));
#129832=DIRECTION('ref_axis',(-0.707106781186548,0.,-0.707106781186547));
#129833=DIRECTION('center_axis',(0.,-1.,0.));
#129834=DIRECTION('ref_axis',(-0.843556936084309,0.,0.53703975233129));
#129835=DIRECTION('',(-8.6595605623547E-17,-1.,-8.65956056235516E-17));
#129836=DIRECTION('center_axis',(0.,1.,0.));
#129837=DIRECTION('ref_axis',(-0.707106781186529,0.,-0.707106781186566));
#129838=DIRECTION('center_axis',(0.,-1.,0.));
#129839=DIRECTION('ref_axis',(-0.707106781186529,0.,-0.707106781186566));
#129840=DIRECTION('',(-8.6595605623547E-17,-1.,-8.65956056235516E-17));
#129841=DIRECTION('center_axis',(0.,-1.,0.));
#129842=DIRECTION('ref_axis',(-0.707106781186529,0.,-0.707106781186566));
#129843=DIRECTION('',(-8.6595605623547E-17,-1.,-8.65956056235516E-17));
#129844=DIRECTION('center_axis',(0.,-1.,0.));
#129845=DIRECTION('ref_axis',(-0.707106781186529,0.,-0.707106781186566));
#129846=DIRECTION('',(-8.6595605623547E-17,-1.,-8.65956056235516E-17));
#129847=DIRECTION('center_axis',(0.,-1.,0.));
#129848=DIRECTION('ref_axis',(-0.707106781186529,0.,-0.707106781186566));
#129849=DIRECTION('',(-8.6595605623547E-17,-1.,-8.65956056235516E-17));
#129850=DIRECTION('center_axis',(0.,-1.,0.));
#129851=DIRECTION('ref_axis',(-0.707106781186529,0.,-0.707106781186566));
#129852=DIRECTION('',(-8.6595605623547E-17,-1.,-8.65956056235516E-17));
#129853=DIRECTION('center_axis',(0.,-1.,0.));
#129854=DIRECTION('ref_axis',(-0.707106781186529,0.,-0.707106781186566));
#129855=DIRECTION('',(-8.6595605623547E-17,-1.,-8.65956056235516E-17));
#129856=DIRECTION('center_axis',(0.,-1.,0.));
#129857=DIRECTION('ref_axis',(0.991406989026756,0.,-0.130813539470888));
#129858=DIRECTION('',(-8.6595605623547E-17,-1.,-8.65956056235516E-17));
#129859=DIRECTION('center_axis',(0.,-1.,0.));
#129860=DIRECTION('ref_axis',(-0.707106781186529,0.,-0.707106781186566));
#129861=DIRECTION('center_axis',(0.,-1.,0.));
#129862=DIRECTION('ref_axis',(-0.707106781186547,0.,0.707106781186548));
#129863=DIRECTION('',(0.,-1.,0.));
#129864=DIRECTION('center_axis',(0.,1.,0.));
#129865=DIRECTION('ref_axis',(-0.707106781186547,0.,0.707106781186548));
#129866=DIRECTION('center_axis',(0.,-1.,0.));
#129867=DIRECTION('ref_axis',(-0.707106781186547,0.,0.707106781186548));
#129868=DIRECTION('',(0.,-1.,0.));
#129869=DIRECTION('center_axis',(0.,1.,0.));
#129870=DIRECTION('ref_axis',(-0.707106781186547,0.,0.707106781186548));
#129871=DIRECTION('center_axis',(0.,-1.,0.));
#129872=DIRECTION('ref_axis',(-0.707106781186547,0.,0.707106781186548));
#129873=DIRECTION('',(0.,-1.,0.));
#129874=DIRECTION('center_axis',(0.,-1.,0.));
#129875=DIRECTION('ref_axis',(-0.707106781186547,0.,0.707106781186548));
#129876=DIRECTION('',(0.,-1.,0.));
#129877=DIRECTION('center_axis',(0.,-1.,0.));
#129878=DIRECTION('ref_axis',(-0.707106781186547,0.,0.707106781186548));
#129879=DIRECTION('',(0.,-1.,0.));
#129880=DIRECTION('center_axis',(0.,-1.,0.));
#129881=DIRECTION('ref_axis',(-0.707106781186547,0.,0.707106781186548));
#129882=DIRECTION('',(0.,-1.,0.));
#129883=DIRECTION('center_axis',(0.,-1.,0.));
#129884=DIRECTION('ref_axis',(-0.707106781186547,0.,0.707106781186548));
#129885=DIRECTION('',(0.,-1.,0.));
#129886=DIRECTION('center_axis',(0.,-1.,0.));
#129887=DIRECTION('ref_axis',(-0.912105596603152,0.,0.409955339817897));
#129888=DIRECTION('',(0.,-1.,0.));
#129889=DIRECTION('center_axis',(0.,-1.,0.));
#129890=DIRECTION('ref_axis',(-0.707106781186547,0.,0.707106781186548));
#129891=DIRECTION('center_axis',(0.,-1.,0.));
#129892=DIRECTION('ref_axis',(0.537039752331291,0.,0.843556936084308));
#129893=DIRECTION('',(-8.65956056235516E-17,-1.,8.6595605623547E-17));
#129894=DIRECTION('center_axis',(0.,1.,0.));
#129895=DIRECTION('ref_axis',(-0.707106781186566,0.,0.707106781186529));
#129896=DIRECTION('center_axis',(0.,-1.,0.));
#129897=DIRECTION('ref_axis',(-0.707106781186566,0.,0.707106781186529));
#129898=DIRECTION('',(-8.65956056235516E-17,-1.,8.6595605623547E-17));
#129899=DIRECTION('center_axis',(0.,-1.,0.));
#129900=DIRECTION('ref_axis',(-0.707106781186566,0.,0.707106781186529));
#129901=DIRECTION('',(-8.65956056235516E-17,-1.,8.6595605623547E-17));
#129902=DIRECTION('center_axis',(0.,-1.,0.));
#129903=DIRECTION('ref_axis',(-0.707106781186566,0.,0.707106781186529));
#129904=DIRECTION('',(-8.65956056235516E-17,-1.,8.6595605623547E-17));
#129905=DIRECTION('center_axis',(0.,-1.,0.));
#129906=DIRECTION('ref_axis',(-0.707106781186566,0.,0.707106781186529));
#129907=DIRECTION('',(-8.65956056235516E-17,-1.,8.6595605623547E-17));
#129908=DIRECTION('center_axis',(0.,-1.,0.));
#129909=DIRECTION('ref_axis',(-0.707106781186566,0.,0.707106781186529));
#129910=DIRECTION('',(-8.65956056235516E-17,-1.,8.6595605623547E-17));
#129911=DIRECTION('center_axis',(0.,-1.,0.));
#129912=DIRECTION('ref_axis',(-0.707106781186566,0.,0.707106781186529));
#129913=DIRECTION('',(-8.65956056235516E-17,-1.,8.6595605623547E-17));
#129914=DIRECTION('center_axis',(0.,-1.,0.));
#129915=DIRECTION('ref_axis',(-0.130813539470888,0.,-0.991406989026756));
#129916=DIRECTION('',(-8.65956056235516E-17,-1.,8.6595605623547E-17));
#129917=DIRECTION('center_axis',(0.,-1.,0.));
#129918=DIRECTION('ref_axis',(-0.707106781186566,0.,0.707106781186529));
#129919=DIRECTION('center_axis',(0.,1.,0.));
#129920=DIRECTION('ref_axis',(0.707106781186548,0.,0.707106781186547));
#129921=DIRECTION('center_axis',(0.,1.,0.));
#129922=DIRECTION('ref_axis',(0.707106781186548,0.,0.707106781186547));
#129923=DIRECTION('',(0.500000000000002,-0.707106781186545,0.500000000000001));
#129924=DIRECTION('center_axis',(0.,-1.,0.));
#129925=DIRECTION('ref_axis',(0.707106781186548,0.,0.707106781186547));
#129926=DIRECTION('center_axis',(0.,1.,0.));
#129927=DIRECTION('ref_axis',(0.707106781186548,0.,0.707106781186547));
#129928=DIRECTION('center_axis',(0.,-1.,0.));
#129929=DIRECTION('ref_axis',(-0.707106781186548,0.,-0.707106781186547));
#129930=DIRECTION('center_axis',(0.,-1.,0.));
#129931=DIRECTION('ref_axis',(-0.707106781186548,0.,-0.707106781186547));
#129932=DIRECTION('',(0.,1.,0.));
#129933=DIRECTION('center_axis',(0.,1.,0.));
#129934=DIRECTION('ref_axis',(0.707106781186548,0.,0.707106781186547));
#129935=DIRECTION('center_axis',(0.,-1.,0.));
#129936=DIRECTION('ref_axis',(-0.707106781186548,0.,-0.707106781186547));
#129937=DIRECTION('center_axis',(0.,-1.,0.));
#129938=DIRECTION('ref_axis',(-0.707106781186566,0.,0.707106781186529));
#129939=DIRECTION('center_axis',(0.,-1.,0.));
#129940=DIRECTION('ref_axis',(-0.707106781186548,0.,-0.707106781186547));
#129941=DIRECTION('center_axis',(0.,1.,0.));
#129942=DIRECTION('ref_axis',(-0.707106781186548,0.,-0.707106781186547));
#129943=DIRECTION('center_axis',(0.,-1.,0.));
#129944=DIRECTION('ref_axis',(-0.707106781186548,0.,-0.707106781186547));
#129945=DIRECTION('center_axis',(0.,-1.,0.));
#129946=DIRECTION('ref_axis',(-0.707106781186547,0.,0.707106781186548));
#129947=DIRECTION('center_axis',(0.,-1.,0.));
#129948=DIRECTION('ref_axis',(-0.707106781186548,0.,-0.707106781186547));
#129949=DIRECTION('center_axis',(0.,-1.,0.));
#129950=DIRECTION('ref_axis',(-0.707106781186548,0.,-0.707106781186547));
#129951=DIRECTION('',(0.,1.,0.));
#129952=DIRECTION('center_axis',(0.,1.,0.));
#129953=DIRECTION('ref_axis',(-0.707106781186548,0.,-0.707106781186547));
#129954=DIRECTION('center_axis',(0.,-1.,0.));
#129955=DIRECTION('ref_axis',(-0.707106781186548,0.,-0.707106781186548));
#129956=DIRECTION('',(0.500000000000003,-0.707106781186543,0.500000000000003));
#129957=DIRECTION('center_axis',(0.,1.,0.));
#129958=DIRECTION('ref_axis',(-0.707106781186548,0.,-0.707106781186547));
#129959=DIRECTION('center_axis',(0.,-1.,0.));
#129960=DIRECTION('ref_axis',(-0.707106781186548,0.,-0.707106781186547));
#129961=DIRECTION('',(0.,-1.,0.));
#129962=DIRECTION('center_axis',(0.,-1.,0.));
#129963=DIRECTION('ref_axis',(-0.707106781186548,0.,-0.707106781186547));
#129964=DIRECTION('center_axis',(0.,-1.,0.));
#129965=DIRECTION('ref_axis',(-0.707106781186548,0.,-0.707106781186547));
#129966=DIRECTION('center_axis',(0.,1.,0.));
#129967=DIRECTION('ref_axis',(-0.707106781186548,0.,-0.707106781186547));
#129968=DIRECTION('',(0.,1.,0.));
#129969=DIRECTION('center_axis',(0.,-1.,0.));
#129970=DIRECTION('ref_axis',(-0.707106781186548,0.,-0.707106781186547));
#129971=DIRECTION('',(0.,1.,0.));
#129972=DIRECTION('center_axis',(0.,-1.,0.));
#129973=DIRECTION('ref_axis',(-0.707106781186548,0.,-0.707106781186547));
#129974=DIRECTION('center_axis',(0.,-1.,0.));
#129975=DIRECTION('ref_axis',(-0.707106781186548,0.,-0.707106781186547));
#129976=DIRECTION('center_axis',(0.,-1.,0.));
#129977=DIRECTION('ref_axis',(-0.707106781186548,0.,-0.707106781186547));
#129978=DIRECTION('',(0.,1.,0.));
#129979=DIRECTION('center_axis',(0.,-1.,0.));
#129980=DIRECTION('ref_axis',(-0.707106781186548,0.,-0.707106781186547));
#129981=DIRECTION('center_axis',(0.,1.,0.));
#129982=DIRECTION('ref_axis',(-0.707106781186548,0.,-0.707106781186547));
#129983=DIRECTION('',(0.,1.,0.));
#129984=DIRECTION('center_axis',(0.,-1.,0.));
#129985=DIRECTION('ref_axis',(-0.707106781186548,0.,-0.707106781186547));
#129986=DIRECTION('center_axis',(0.,-1.,0.));
#129987=DIRECTION('ref_axis',(-0.707106781186548,0.,-0.707106781186547));
#129988=DIRECTION('center_axis',(0.,-1.,0.));
#129989=DIRECTION('ref_axis',(-0.707106781186548,0.,-0.707106781186547));
#129990=DIRECTION('',(0.,1.,0.));
#129991=DIRECTION('center_axis',(0.,-1.,0.));
#129992=DIRECTION('ref_axis',(-0.707106781186548,0.,-0.707106781186547));
#129993=DIRECTION('center_axis',(0.,-1.,0.));
#129994=DIRECTION('ref_axis',(-0.707106781186548,0.,-0.707106781186547));
#129995=DIRECTION('center_axis',(0.,1.,0.));
#129996=DIRECTION('ref_axis',(-0.707106781186548,0.,-0.707106781186547));
#129997=DIRECTION('',(0.,1.,0.));
#129998=DIRECTION('center_axis',(0.,-1.,0.));
#129999=DIRECTION('ref_axis',(-0.707106781186548,0.,-0.707106781186547));
#130000=DIRECTION('center_axis',(0.,-1.,0.));
#130001=DIRECTION('ref_axis',(-0.707106781186548,0.,-0.707106781186547));
#130002=DIRECTION('center_axis',(0.,-1.,0.));
#130003=DIRECTION('ref_axis',(-0.707106781186548,0.,-0.707106781186547));
#130004=DIRECTION('',(0.,1.,0.));
#130005=DIRECTION('center_axis',(0.,-1.,0.));
#130006=DIRECTION('ref_axis',(-0.707106781186548,0.,-0.707106781186547));
#130007=DIRECTION('center_axis',(0.,-1.,0.));
#130008=DIRECTION('ref_axis',(-0.707106781186548,0.,-0.707106781186547));
#130009=DIRECTION('center_axis',(0.,1.,0.));
#130010=DIRECTION('ref_axis',(-0.707106781186548,0.,-0.707106781186547));
#130011=DIRECTION('',(0.,1.,0.));
#130012=DIRECTION('center_axis',(0.,-1.,0.));
#130013=DIRECTION('ref_axis',(-0.707106781186548,0.,-0.707106781186547));
#130014=DIRECTION('center_axis',(0.,-1.,0.));
#130015=DIRECTION('ref_axis',(-0.707106781186548,0.,-0.707106781186547));
#130016=DIRECTION('center_axis',(0.,-1.,0.));
#130017=DIRECTION('ref_axis',(-0.707106781186548,0.,-0.707106781186547));
#130018=DIRECTION('',(0.,1.,0.));
#130019=DIRECTION('center_axis',(0.,-1.,0.));
#130020=DIRECTION('ref_axis',(-0.707106781186548,0.,-0.707106781186547));
#130021=DIRECTION('center_axis',(0.,-1.,0.));
#130022=DIRECTION('ref_axis',(-0.707106781186548,0.,-0.707106781186547));
#130023=DIRECTION('center_axis',(0.,1.,0.));
#130024=DIRECTION('ref_axis',(-0.707106781186548,0.,-0.707106781186547));
#130025=DIRECTION('',(0.,1.,0.));
#130026=DIRECTION('center_axis',(0.,-1.,0.));
#130027=DIRECTION('ref_axis',(-0.707106781186548,0.,-0.707106781186547));
#130028=DIRECTION('center_axis',(0.,-1.,0.));
#130029=DIRECTION('ref_axis',(-0.707106781186548,0.,-0.707106781186547));
#130030=DIRECTION('center_axis',(0.,-1.,0.));
#130031=DIRECTION('ref_axis',(-0.707106781186548,0.,-0.707106781186547));
#130032=DIRECTION('',(0.,1.,0.));
#130033=DIRECTION('center_axis',(0.,-1.,0.));
#130034=DIRECTION('ref_axis',(-0.707106781186548,0.,-0.707106781186547));
#130035=DIRECTION('center_axis',(0.,-1.,0.));
#130036=DIRECTION('ref_axis',(-0.707106781186548,0.,-0.707106781186547));
#130037=DIRECTION('center_axis',(0.,1.,0.));
#130038=DIRECTION('ref_axis',(-0.707106781186548,0.,-0.707106781186547));
#130039=DIRECTION('',(0.,1.,0.));
#130040=DIRECTION('center_axis',(0.,-1.,0.));
#130041=DIRECTION('ref_axis',(-0.707106781186548,0.,-0.707106781186547));
#130042=DIRECTION('center_axis',(0.,-1.,0.));
#130043=DIRECTION('ref_axis',(-0.707106781186548,0.,-0.707106781186547));
#130044=DIRECTION('center_axis',(0.,-1.,0.));
#130045=DIRECTION('ref_axis',(-0.707106781186548,0.,-0.707106781186547));
#130046=DIRECTION('',(0.,1.,0.));
#130047=DIRECTION('center_axis',(0.,-1.,0.));
#130048=DIRECTION('ref_axis',(-0.707106781186548,0.,-0.707106781186547));
#130049=DIRECTION('center_axis',(0.,-1.,0.));
#130050=DIRECTION('ref_axis',(-0.707106781186548,0.,-0.707106781186547));
#130051=DIRECTION('center_axis',(0.,1.,0.));
#130052=DIRECTION('ref_axis',(-0.707106781186548,0.,-0.707106781186547));
#130053=DIRECTION('',(0.,1.,0.));
#130054=DIRECTION('center_axis',(0.,-1.,0.));
#130055=DIRECTION('ref_axis',(-0.707106781186548,0.,-0.707106781186547));
#130056=DIRECTION('center_axis',(0.,-1.,0.));
#130057=DIRECTION('ref_axis',(-0.707106781186548,0.,-0.707106781186547));
#130058=DIRECTION('center_axis',(0.,-1.,0.));
#130059=DIRECTION('ref_axis',(-0.707106781186548,0.,-0.707106781186547));
#130060=DIRECTION('',(0.,1.,0.));
#130061=DIRECTION('center_axis',(0.,-1.,0.));
#130062=DIRECTION('ref_axis',(-0.707106781186548,0.,-0.707106781186547));
#130063=DIRECTION('center_axis',(0.,-1.,0.));
#130064=DIRECTION('ref_axis',(-0.707106781186548,0.,-0.707106781186547));
#130065=DIRECTION('center_axis',(0.,1.,0.));
#130066=DIRECTION('ref_axis',(-0.707106781186548,0.,-0.707106781186547));
#130067=DIRECTION('',(0.,1.,0.));
#130068=DIRECTION('center_axis',(0.,-1.,0.));
#130069=DIRECTION('ref_axis',(-0.707106781186548,0.,-0.707106781186547));
#130070=DIRECTION('center_axis',(0.,-1.,0.));
#130071=DIRECTION('ref_axis',(-0.707106781186548,0.,-0.707106781186547));
#130072=DIRECTION('center_axis',(0.,-1.,0.));
#130073=DIRECTION('ref_axis',(-0.707106781186548,0.,-0.707106781186547));
#130074=DIRECTION('',(0.,1.,0.));
#130075=DIRECTION('center_axis',(0.,-1.,0.));
#130076=DIRECTION('ref_axis',(-0.707106781186548,0.,-0.707106781186547));
#130077=DIRECTION('center_axis',(0.,-1.,0.));
#130078=DIRECTION('ref_axis',(-0.707106781186548,0.,-0.707106781186547));
#130079=DIRECTION('center_axis',(0.,1.,0.));
#130080=DIRECTION('ref_axis',(-0.707106781186548,0.,-0.707106781186547));
#130081=DIRECTION('',(0.,1.,0.));
#130082=DIRECTION('center_axis',(0.,-1.,0.));
#130083=DIRECTION('ref_axis',(-0.707106781186548,0.,-0.707106781186547));
#130084=DIRECTION('center_axis',(0.,-1.,0.));
#130085=DIRECTION('ref_axis',(-0.707106781186548,0.,-0.707106781186547));
#130086=DIRECTION('center_axis',(0.,-1.,0.));
#130087=DIRECTION('ref_axis',(-0.707106781186548,0.,-0.707106781186547));
#130088=DIRECTION('',(0.,1.,0.));
#130089=DIRECTION('center_axis',(0.,-1.,0.));
#130090=DIRECTION('ref_axis',(-0.707106781186548,0.,-0.707106781186547));
#130091=DIRECTION('center_axis',(0.,-1.,0.));
#130092=DIRECTION('ref_axis',(-0.707106781186548,0.,-0.707106781186547));
#130093=DIRECTION('center_axis',(0.,1.,0.));
#130094=DIRECTION('ref_axis',(-0.707106781186548,0.,-0.707106781186547));
#130095=DIRECTION('',(0.,1.,0.));
#130096=DIRECTION('center_axis',(0.,-1.,0.));
#130097=DIRECTION('ref_axis',(-0.707106781186548,0.,-0.707106781186547));
#130098=DIRECTION('center_axis',(0.,-1.,0.));
#130099=DIRECTION('ref_axis',(-0.707106781186548,0.,-0.707106781186547));
#130100=DIRECTION('center_axis',(0.,1.,0.));
#130101=DIRECTION('ref_axis',(0.707106781186548,0.,0.707106781186547));
#130102=DIRECTION('center_axis',(0.,-1.,0.));
#130103=DIRECTION('ref_axis',(-0.707106781186548,0.,-0.707106781186547));
#130104=DIRECTION('center_axis',(0.,1.,0.));
#130105=DIRECTION('ref_axis',(0.707106781186548,0.,0.707106781186547));
#130106=DIRECTION('center_axis',(0.,-1.,0.));
#130107=DIRECTION('ref_axis',(-0.707106781186548,0.,-0.707106781186547));
#130108=DIRECTION('center_axis',(0.,1.,0.));
#130109=DIRECTION('ref_axis',(0.707106781186548,0.,0.707106781186547));
#130110=DIRECTION('center_axis',(0.,-1.,0.));
#130111=DIRECTION('ref_axis',(-0.707106781186548,0.,-0.707106781186547));
#130112=DIRECTION('center_axis',(0.,1.,0.));
#130113=DIRECTION('ref_axis',(0.707106781186548,0.,0.707106781186547));
#130114=DIRECTION('center_axis',(0.,-1.,0.));
#130115=DIRECTION('ref_axis',(-0.707106781186548,0.,-0.707106781186547));
#130116=DIRECTION('center_axis',(0.,1.,0.));
#130117=DIRECTION('ref_axis',(0.707106781186548,0.,0.707106781186547));
#130118=DIRECTION('center_axis',(0.,-1.,0.));
#130119=DIRECTION('ref_axis',(-0.707106781186548,0.,-0.707106781186547));
#130120=DIRECTION('center_axis',(0.,1.,0.));
#130121=DIRECTION('ref_axis',(0.707106781186548,0.,0.707106781186547));
#130122=DIRECTION('center_axis',(0.,-1.,0.));
#130123=DIRECTION('ref_axis',(-0.707106781186548,0.,-0.707106781186547));
#130124=DIRECTION('center_axis',(0.,1.,0.));
#130125=DIRECTION('ref_axis',(0.707106781186548,0.,0.707106781186547));
#130126=DIRECTION('center_axis',(0.,-1.,0.));
#130127=DIRECTION('ref_axis',(-0.707106781186548,0.,-0.707106781186547));
#130128=DIRECTION('center_axis',(0.,1.,0.));
#130129=DIRECTION('ref_axis',(0.707106781186548,0.,0.707106781186547));
#130130=DIRECTION('center_axis',(0.,-1.,0.));
#130131=DIRECTION('ref_axis',(-0.707106781186548,0.,-0.707106781186547));
#130132=DIRECTION('center_axis',(0.,1.,0.));
#130133=DIRECTION('ref_axis',(0.707106781186548,0.,0.707106781186547));
#130134=DIRECTION('center_axis',(0.,1.,0.));
#130135=DIRECTION('ref_axis',(0.707106781186548,0.,0.707106781186547));
#130136=DIRECTION('center_axis',(0.,-1.,0.));
#130137=DIRECTION('ref_axis',(-0.707106781186548,0.,-0.707106781186547));
#130138=DIRECTION('center_axis',(0.,-1.,0.));
#130139=DIRECTION('ref_axis',(-0.707106781186529,0.,-0.707106781186566));
#130140=DIRECTION('center_axis',(0.,-1.,0.));
#130141=DIRECTION('ref_axis',(-0.707106781186548,0.,-0.707106781186547));
#130142=DIRECTION('center_axis',(0.,-1.,0.));
#130143=DIRECTION('ref_axis',(0.707106781186566,0.,-0.707106781186529));
#130144=DIRECTION('center_axis',(0.,-1.,0.));
#130145=DIRECTION('ref_axis',(0.707106781186547,0.,-0.707106781186548));
#130146=DIRECTION('center_axis',(0.,-1.,0.));
#130147=DIRECTION('ref_axis',(0.707106781186529,0.,0.707106781186566));
#130148=DIRECTION('center_axis',(0.,-1.,0.));
#130149=DIRECTION('ref_axis',(0.707106781186548,0.,0.707106781186547));
#130150=DIRECTION('axis',(0.,0.,1.));
#130151=DIRECTION('refdir',(1.,0.,0.));
#130152=DIRECTION('center_axis',(0.,1.,0.));
#130153=DIRECTION('ref_axis',(0.,0.,1.));
#130154=DIRECTION('',(0.,-1.,0.));
#130155=DIRECTION('center_axis',(0.,-1.,0.));
#130156=DIRECTION('ref_axis',(0.,0.,1.));
#130157=DIRECTION('center_axis',(0.,1.,0.));
#130158=DIRECTION('ref_axis',(0.,0.,1.));
#130159=DIRECTION('',(0.,-1.,0.));
#130160=DIRECTION('center_axis',(0.,1.,0.));
#130161=DIRECTION('ref_axis',(0.,0.,1.));
#130162=DIRECTION('',(0.,-1.,0.));
#130163=DIRECTION('center_axis',(0.,1.,0.));
#130164=DIRECTION('ref_axis',(0.,0.,1.));
#130165=DIRECTION('',(0.,-1.,0.));
#130166=DIRECTION('center_axis',(0.,1.,0.));
#130167=DIRECTION('ref_axis',(0.,0.,1.));
#130168=DIRECTION('',(0.,-1.,0.));
#130169=DIRECTION('center_axis',(0.,1.,0.));
#130170=DIRECTION('ref_axis',(0.,0.,1.));
#130171=DIRECTION('',(0.,-1.,0.));
#130172=DIRECTION('center_axis',(0.,1.,0.));
#130173=DIRECTION('ref_axis',(0.,0.,1.));
#130174=DIRECTION('',(0.,-1.,0.));
#130175=DIRECTION('center_axis',(0.,1.,0.));
#130176=DIRECTION('ref_axis',(0.,0.,1.));
#130177=DIRECTION('',(0.,-1.,0.));
#130178=DIRECTION('center_axis',(0.,1.,0.));
#130179=DIRECTION('ref_axis',(0.,0.,1.));
#130180=DIRECTION('',(0.,-1.,0.));
#130181=DIRECTION('center_axis',(0.,1.,0.));
#130182=DIRECTION('ref_axis',(0.,0.,1.));
#130183=DIRECTION('',(0.,-1.,0.));
#130184=DIRECTION('center_axis',(0.,1.,0.));
#130185=DIRECTION('ref_axis',(5.13873024532413E-14,0.,1.));
#130186=DIRECTION('',(0.,1.,0.));
#130187=DIRECTION('center_axis',(0.,1.,0.));
#130188=DIRECTION('ref_axis',(5.13873024532413E-14,0.,1.));
#130189=DIRECTION('center_axis',(0.,1.,0.));
#130190=DIRECTION('ref_axis',(5.13873024532413E-14,0.,1.));
#130191=DIRECTION('',(0.,1.,0.));
#130192=DIRECTION('center_axis',(0.,1.,0.));
#130193=DIRECTION('ref_axis',(5.13873024532413E-14,0.,1.));
#130194=DIRECTION('center_axis',(0.,1.,0.));
#130195=DIRECTION('ref_axis',(5.13873024532413E-14,0.,1.));
#130196=DIRECTION('',(0.,1.,0.));
#130197=DIRECTION('center_axis',(0.,1.,0.));
#130198=DIRECTION('ref_axis',(5.13873024532413E-14,0.,1.));
#130199=DIRECTION('',(0.,1.,0.));
#130200=DIRECTION('center_axis',(0.,1.,0.));
#130201=DIRECTION('ref_axis',(5.13873024532413E-14,0.,1.));
#130202=DIRECTION('',(0.,1.,0.));
#130203=DIRECTION('center_axis',(0.,1.,0.));
#130204=DIRECTION('ref_axis',(5.13873024532413E-14,0.,1.));
#130205=DIRECTION('',(0.,1.,0.));
#130206=DIRECTION('center_axis',(0.,1.,0.));
#130207=DIRECTION('ref_axis',(5.13873024532413E-14,0.,1.));
#130208=DIRECTION('',(0.,1.,0.));
#130209=DIRECTION('center_axis',(0.,1.,0.));
#130210=DIRECTION('ref_axis',(5.13873024532413E-14,0.,1.));
#130211=DIRECTION('',(0.,1.,0.));
#130212=DIRECTION('center_axis',(0.,1.,0.));
#130213=DIRECTION('ref_axis',(5.13873024532413E-14,0.,1.));
#130214=DIRECTION('',(0.,1.,0.));
#130215=DIRECTION('center_axis',(0.,1.,0.));
#130216=DIRECTION('ref_axis',(5.13873024532413E-14,0.,1.));
#130217=DIRECTION('',(0.,1.,0.));
#130218=DIRECTION('center_axis',(0.,1.,0.));
#130219=DIRECTION('ref_axis',(0.,0.,1.));
#130220=DIRECTION('',(0.,-1.,0.));
#130221=DIRECTION('center_axis',(0.,-1.,0.));
#130222=DIRECTION('ref_axis',(0.,0.,1.));
#130223=DIRECTION('center_axis',(0.,1.,0.));
#130224=DIRECTION('ref_axis',(0.,0.,1.));
#130225=DIRECTION('',(0.,-1.,0.));
#130226=DIRECTION('center_axis',(0.,1.,0.));
#130227=DIRECTION('ref_axis',(0.,0.,1.));
#130228=DIRECTION('',(0.,-1.,0.));
#130229=DIRECTION('center_axis',(0.,1.,0.));
#130230=DIRECTION('ref_axis',(0.,0.,1.));
#130231=DIRECTION('',(0.,-1.,0.));
#130232=DIRECTION('center_axis',(0.,1.,0.));
#130233=DIRECTION('ref_axis',(0.,0.,1.));
#130234=DIRECTION('',(0.,-1.,0.));
#130235=DIRECTION('center_axis',(0.,1.,0.));
#130236=DIRECTION('ref_axis',(4.71072660257168E-15,0.,1.));
#130237=DIRECTION('',(0.,1.,0.));
#130238=DIRECTION('center_axis',(0.,1.,0.));
#130239=DIRECTION('ref_axis',(4.71072660257168E-15,0.,1.));
#130240=DIRECTION('center_axis',(0.,1.,0.));
#130241=DIRECTION('ref_axis',(4.71072660257168E-15,0.,1.));
#130242=DIRECTION('',(0.,1.,0.));
#130243=DIRECTION('center_axis',(0.,1.,0.));
#130244=DIRECTION('ref_axis',(4.71072660257168E-15,0.,1.));
#130245=DIRECTION('',(0.,1.,0.));
#130246=DIRECTION('center_axis',(0.,1.,0.));
#130247=DIRECTION('ref_axis',(4.71072660257168E-15,0.,1.));
#130248=DIRECTION('',(0.,1.,0.));
#130249=DIRECTION('center_axis',(0.,1.,0.));
#130250=DIRECTION('ref_axis',(4.71072660257168E-15,0.,1.));
#130251=DIRECTION('',(0.,1.,0.));
#130252=DIRECTION('center_axis',(0.,1.,0.));
#130253=DIRECTION('ref_axis',(0.457752838279926,0.,0.889079489723316));
#130254=DIRECTION('center_axis',(0.,-1.,0.));
#130255=DIRECTION('ref_axis',(4.71072660257168E-15,0.,1.));
#130256=DIRECTION('center_axis',(0.,-1.,0.));
#130257=DIRECTION('ref_axis',(0.,0.,-1.));
#130258=DIRECTION('center_axis',(0.,1.,0.));
#130259=DIRECTION('ref_axis',(0.,0.,1.));
#130260=DIRECTION('center_axis',(0.,1.,0.));
#130261=DIRECTION('ref_axis',(0.,0.,1.));
#130262=DIRECTION('center_axis',(0.,1.,0.));
#130263=DIRECTION('ref_axis',(0.,0.,1.));
#130264=DIRECTION('center_axis',(0.,1.,0.));
#130265=DIRECTION('ref_axis',(0.,0.,1.));
#130266=DIRECTION('center_axis',(0.,1.,0.));
#130267=DIRECTION('ref_axis',(0.,0.,1.));
#130268=DIRECTION('center_axis',(0.,1.,0.));
#130269=DIRECTION('ref_axis',(0.,0.,1.));
#130270=DIRECTION('center_axis',(0.,1.,0.));
#130271=DIRECTION('ref_axis',(5.13873024532413E-14,0.,1.));
#130272=DIRECTION('center_axis',(0.,-1.,0.));
#130273=DIRECTION('ref_axis',(5.13873024532413E-14,0.,1.));
#130274=DIRECTION('center_axis',(0.,-1.,0.));
#130275=DIRECTION('ref_axis',(0.,0.,-1.));
#130276=DIRECTION('center_axis',(0.,-1.,0.));
#130277=DIRECTION('ref_axis',(0.,0.,-1.));
#130278=DIRECTION('center_axis',(0.,-1.,0.));
#130279=DIRECTION('ref_axis',(0.,0.,-1.));
#130280=DIRECTION('',(8.65956056235495E-17,0.707106781186546,-0.707106781186549));
#130281=DIRECTION('center_axis',(0.,1.,0.));
#130282=DIRECTION('ref_axis',(0.,0.,-1.));
#130283=DIRECTION('center_axis',(0.,1.,0.));
#130284=DIRECTION('ref_axis',(0.,0.,1.));
#130285=DIRECTION('center_axis',(0.,1.,0.));
#130286=DIRECTION('ref_axis',(0.,0.,1.));
#130287=DIRECTION('',(0.,-1.,0.));
#130288=DIRECTION('center_axis',(0.,1.,0.));
#130289=DIRECTION('ref_axis',(0.,0.,1.));
#130290=DIRECTION('center_axis',(0.,1.,0.));
#130291=DIRECTION('ref_axis',(0.,0.,1.));
#130292=DIRECTION('center_axis',(0.,1.,0.));
#130293=DIRECTION('ref_axis',(0.,0.,1.));
#130294=DIRECTION('',(0.,-1.,0.));
#130295=DIRECTION('center_axis',(0.,1.,0.));
#130296=DIRECTION('ref_axis',(0.,0.,1.));
#130297=DIRECTION('center_axis',(0.,1.,0.));
#130298=DIRECTION('ref_axis',(0.,0.,1.));
#130299=DIRECTION('center_axis',(0.,1.,0.));
#130300=DIRECTION('ref_axis',(0.,0.,1.));
#130301=DIRECTION('',(0.,1.,0.));
#130302=DIRECTION('center_axis',(0.,1.,0.));
#130303=DIRECTION('ref_axis',(0.,0.,1.));
#130304=DIRECTION('center_axis',(0.,1.,0.));
#130305=DIRECTION('ref_axis',(0.,0.,1.));
#130306=DIRECTION('center_axis',(0.,1.,0.));
#130307=DIRECTION('ref_axis',(0.,0.,1.));
#130308=DIRECTION('',(-8.65956056235495E-17,0.707106781186546,-0.707106781186549));
#130309=DIRECTION('center_axis',(0.,1.,0.));
#130310=DIRECTION('ref_axis',(0.,0.,1.));
#130311=DIRECTION('center_axis',(0.,1.,0.));
#130312=DIRECTION('ref_axis',(0.,0.,1.));
#130313=DIRECTION('',(0.,1.,0.));
#130314=DIRECTION('center_axis',(0.,-1.,0.));
#130315=DIRECTION('ref_axis',(0.,0.,-1.));
#130316=DIRECTION('center_axis',(0.,-1.,0.));
#130317=DIRECTION('ref_axis',(0.,0.,-1.));
#130318=DIRECTION('center_axis',(0.,1.,0.));
#130319=DIRECTION('ref_axis',(0.,0.,1.));
#130320=DIRECTION('center_axis',(0.,1.,0.));
#130321=DIRECTION('ref_axis',(0.,0.,1.));
#130322=DIRECTION('axis',(0.,0.,1.));
#130323=DIRECTION('refdir',(1.,0.,0.));
#130324=DIRECTION('center_axis',(-1.07601673699754E-16,-5.16454430761843E-15,
-1.));
#130325=DIRECTION('ref_axis',(1.,1.29806344583732E-24,-1.07601673699754E-16));
#130326=DIRECTION('center_axis',(1.07601673699754E-16,5.16454430761843E-15,
1.));
#130327=DIRECTION('ref_axis',(1.,1.29806344583732E-24,-1.07601673699754E-16));
#130328=DIRECTION('center_axis',(-1.07601673699754E-16,-5.16454430761843E-15,
-1.));
#130329=DIRECTION('ref_axis',(1.,1.29806344583732E-24,-1.07601673699754E-16));
#130330=DIRECTION('center_axis',(-9.91270557701033E-17,-5.16454430759884E-15,
-1.));
#130331=DIRECTION('ref_axis',(1.,1.29806348960486E-24,-9.91270557701033E-17));
#130332=DIRECTION('center_axis',(1.07601673699754E-16,5.16454430761843E-15,
1.));
#130333=DIRECTION('ref_axis',(1.,1.29806344583732E-24,-1.07601673699754E-16));
#130334=DIRECTION('',(9.91270557701033E-17,5.16454430759884E-15,1.));
#130335=DIRECTION('center_axis',(-9.91270557701033E-17,-5.16454430759884E-15,
-1.));
#130336=DIRECTION('ref_axis',(1.,1.29806348960486E-24,-9.91270557701033E-17));
#130337=DIRECTION('center_axis',(-1.07601673699754E-16,-5.16454430761843E-15,
-1.));
#130338=DIRECTION('ref_axis',(1.,1.29806344583732E-24,-1.07601673699754E-16));
#130339=DIRECTION('',(9.91270557701033E-17,5.16454430759884E-15,1.));
#130340=DIRECTION('center_axis',(-1.07601673699754E-16,-5.16454430761843E-15,
-1.));
#130341=DIRECTION('ref_axis',(1.,1.29806344583732E-24,-1.07601673699754E-16));
#130342=DIRECTION('axis',(0.,0.,1.));
#130343=DIRECTION('refdir',(1.,0.,0.));
#130344=DIRECTION('center_axis',(0.,1.,0.));
#130345=DIRECTION('ref_axis',(0.,0.,1.));
#130346=DIRECTION('',(0.,-1.,0.));
#130347=DIRECTION('center_axis',(0.,-1.,0.));
#130348=DIRECTION('ref_axis',(0.,0.,1.));
#130349=DIRECTION('center_axis',(0.,1.,0.));
#130350=DIRECTION('ref_axis',(0.,0.,1.));
#130351=DIRECTION('',(0.,-1.,0.));
#130352=DIRECTION('center_axis',(0.,1.,0.));
#130353=DIRECTION('ref_axis',(0.,0.,1.));
#130354=DIRECTION('',(0.,-1.,0.));
#130355=DIRECTION('center_axis',(0.,1.,0.));
#130356=DIRECTION('ref_axis',(0.,0.,1.));
#130357=DIRECTION('',(0.,-1.,0.));
#130358=DIRECTION('center_axis',(0.,1.,0.));
#130359=DIRECTION('ref_axis',(0.,0.,1.));
#130360=DIRECTION('',(0.,-1.,0.));
#130361=DIRECTION('center_axis',(0.,1.,0.));
#130362=DIRECTION('ref_axis',(0.,0.,1.));
#130363=DIRECTION('',(0.,-1.,0.));
#130364=DIRECTION('center_axis',(0.,1.,0.));
#130365=DIRECTION('ref_axis',(-0.889062766616259,0.,-0.457785317607111));
#130366=DIRECTION('',(0.,1.,0.));
#130367=DIRECTION('center_axis',(0.,1.,0.));
#130368=DIRECTION('ref_axis',(2.23383579178976E-14,0.,1.));
#130369=DIRECTION('center_axis',(0.,1.,0.));
#130370=DIRECTION('ref_axis',(2.23383579178976E-14,0.,1.));
#130371=DIRECTION('',(0.,1.,0.));
#130372=DIRECTION('center_axis',(0.,1.,0.));
#130373=DIRECTION('ref_axis',(2.23383579178976E-14,0.,1.));
#130374=DIRECTION('',(0.,1.,0.));
#130375=DIRECTION('center_axis',(0.,1.,0.));
#130376=DIRECTION('ref_axis',(2.23383579178976E-14,0.,1.));
#130377=DIRECTION('',(0.,1.,0.));
#130378=DIRECTION('center_axis',(0.,1.,0.));
#130379=DIRECTION('ref_axis',(2.23383579178976E-14,0.,1.));
#130380=DIRECTION('',(0.,1.,0.));
#130381=DIRECTION('center_axis',(0.,1.,0.));
#130382=DIRECTION('ref_axis',(2.23383579178976E-14,0.,1.));
#130383=DIRECTION('',(0.,1.,0.));
#130384=DIRECTION('center_axis',(0.,1.,0.));
#130385=DIRECTION('ref_axis',(0.,0.,1.));
#130386=DIRECTION('center_axis',(0.,1.,0.));
#130387=DIRECTION('ref_axis',(0.,0.,1.));
#130388=DIRECTION('center_axis',(0.,-1.,0.));
#130389=DIRECTION('ref_axis',(2.23383579178976E-14,0.,1.));
#130390=DIRECTION('center_axis',(0.,1.,0.));
#130391=DIRECTION('ref_axis',(2.23383579178976E-14,0.,1.));
#130392=DIRECTION('center_axis',(0.,1.,0.));
#130393=DIRECTION('ref_axis',(0.,0.,1.));
#130394=DIRECTION('center_axis',(0.,1.,0.));
#130395=DIRECTION('ref_axis',(0.,0.,1.));
#130396=DIRECTION('center_axis',(0.,1.,0.));
#130397=DIRECTION('ref_axis',(0.,0.,1.));
#130398=DIRECTION('center_axis',(0.,-1.,0.));
#130399=DIRECTION('ref_axis',(0.,0.,-1.));
#130400=DIRECTION('center_axis',(0.,1.,0.));
#130401=DIRECTION('ref_axis',(0.,0.,1.));
#130402=DIRECTION('center_axis',(0.,1.,0.));
#130403=DIRECTION('ref_axis',(0.,0.,1.));
#130404=DIRECTION('center_axis',(0.,1.,0.));
#130405=DIRECTION('ref_axis',(0.,0.,1.));
#130406=DIRECTION('center_axis',(0.,1.,0.));
#130407=DIRECTION('ref_axis',(0.,0.,1.));
#130408=DIRECTION('center_axis',(0.,1.,0.));
#130409=DIRECTION('ref_axis',(0.,0.,1.));
#130410=DIRECTION('',(-9.061652424452E-17,0.672672793996312,-0.739940073395944));
#130411=DIRECTION('center_axis',(0.,1.,0.));
#130412=DIRECTION('ref_axis',(0.,0.,1.));
#130413=DIRECTION('center_axis',(0.,1.,0.));
#130414=DIRECTION('ref_axis',(0.,0.,1.));
#130415=DIRECTION('center_axis',(0.,1.,0.));
#130416=DIRECTION('ref_axis',(0.,0.,1.));
#130417=DIRECTION('center_axis',(0.,1.,0.));
#130418=DIRECTION('ref_axis',(0.,0.,1.));
#130419=DIRECTION('',(0.,1.,0.));
#130420=DIRECTION('center_axis',(0.,1.,0.));
#130421=DIRECTION('ref_axis',(0.,0.,1.));
#130422=DIRECTION('center_axis',(0.,1.,0.));
#130423=DIRECTION('ref_axis',(0.,0.,1.));
#130424=DIRECTION('',(-9.061652424452E-17,0.672672793996312,-0.739940073395944));
#130425=DIRECTION('center_axis',(0.,1.,0.));
#130426=DIRECTION('ref_axis',(0.,0.,1.));
#130427=DIRECTION('center_axis',(0.,-1.,0.));
#130428=DIRECTION('ref_axis',(0.,0.,1.));
#130429=DIRECTION('',(8.65956056235491E-17,-0.707106781186549,0.707106781186546));
#130430=DIRECTION('center_axis',(0.,1.,0.));
#130431=DIRECTION('ref_axis',(0.,0.,1.));
#130432=DIRECTION('center_axis',(0.,1.,0.));
#130433=DIRECTION('ref_axis',(0.,0.,1.));
#130434=DIRECTION('',(0.,-1.,0.));
#130435=DIRECTION('center_axis',(0.,1.,0.));
#130436=DIRECTION('ref_axis',(0.,0.,1.));
#130437=DIRECTION('center_axis',(0.,1.,0.));
#130438=DIRECTION('ref_axis',(0.,0.,1.));
#130439=DIRECTION('center_axis',(0.,1.,0.));
#130440=DIRECTION('ref_axis',(0.,0.,1.));
#130441=DIRECTION('center_axis',(0.,1.,0.));
#130442=DIRECTION('ref_axis',(0.,0.,1.));
#130443=DIRECTION('',(-8.65956056235491E-17,0.707106781186549,-0.707106781186546));
#130444=DIRECTION('center_axis',(0.,-1.,0.));
#130445=DIRECTION('ref_axis',(0.,0.,-1.));
#130446=DIRECTION('',(0.,-1.,0.));
#130447=DIRECTION('center_axis',(0.,1.,0.));
#130448=DIRECTION('ref_axis',(0.,0.,1.));
#130449=DIRECTION('center_axis',(0.,1.,0.));
#130450=DIRECTION('ref_axis',(0.,0.,1.));
#130451=DIRECTION('',(0.,1.,0.));
#130452=DIRECTION('center_axis',(0.,1.,0.));
#130453=DIRECTION('ref_axis',(0.,0.,1.));
#130454=DIRECTION('',(1.,0.,0.));
#130455=DIRECTION('',(0.5,0.,0.866025403784438));
#130456=DIRECTION('',(-0.5,0.,0.866025403784439));
#130457=DIRECTION('',(-1.,0.,0.));
#130458=DIRECTION('',(-0.5,0.,-0.866025403784438));
#130459=DIRECTION('',(0.5,0.,-0.866025403784439));
#130460=DIRECTION('center_axis',(0.,1.,0.));
#130461=DIRECTION('ref_axis',(0.,0.,1.));
#130462=DIRECTION('',(1.,0.,0.));
#130463=DIRECTION('',(0.5,0.,-0.866025403784439));
#130464=DIRECTION('',(-0.5,0.,-0.866025403784438));
#130465=DIRECTION('',(-1.,0.,0.));
#130466=DIRECTION('',(-0.5,0.,0.866025403784439));
#130467=DIRECTION('',(0.5,0.,0.866025403784438));
#130468=DIRECTION('center_axis',(0.,0.,-1.));
#130469=DIRECTION('ref_axis',(-1.,0.,0.));
#130470=DIRECTION('',(0.,-1.,0.));
#130471=DIRECTION('',(0.,-1.,0.));
#130472=DIRECTION('center_axis',(-0.866025403784439,0.,-0.5));
#130473=DIRECTION('ref_axis',(-0.5,0.,0.866025403784439));
#130474=DIRECTION('',(0.,-1.,0.));
#130475=DIRECTION('center_axis',(-0.866025403784438,0.,0.500000000000001));
#130476=DIRECTION('ref_axis',(0.500000000000001,0.,0.866025403784438));
#130477=DIRECTION('',(0.,-1.,0.));
#130478=DIRECTION('center_axis',(0.,0.,1.));
#130479=DIRECTION('ref_axis',(1.,0.,0.));
#130480=DIRECTION('',(0.,-1.,0.));
#130481=DIRECTION('center_axis',(0.866025403784439,0.,0.5));
#130482=DIRECTION('ref_axis',(0.5,0.,-0.866025403784439));
#130483=DIRECTION('',(0.,-1.,0.));
#130484=DIRECTION('center_axis',(0.866025403784439,0.,-0.5));
#130485=DIRECTION('ref_axis',(-0.5,0.,-0.866025403784439));
#130486=DIRECTION('center_axis',(0.,1.,0.));
#130487=DIRECTION('ref_axis',(0.,0.,1.));
#130488=DIRECTION('axis',(0.,0.,1.));
#130489=DIRECTION('refdir',(1.,0.,0.));
#130490=DIRECTION('center_axis',(0.,1.,0.));
#130491=DIRECTION('ref_axis',(0.,0.,1.));
#130492=DIRECTION('center_axis',(0.,1.,0.));
#130493=DIRECTION('ref_axis',(0.,0.,1.));
#130494=DIRECTION('',(0.,1.,0.));
#130495=DIRECTION('center_axis',(0.,1.,0.));
#130496=DIRECTION('ref_axis',(0.,0.,1.));
#130497=DIRECTION('center_axis',(0.,1.,0.));
#130498=DIRECTION('ref_axis',(0.,0.,1.));
#130499=DIRECTION('center_axis',(0.,1.,0.));
#130500=DIRECTION('ref_axis',(0.,0.,1.));
#130501=DIRECTION('',(0.,1.,0.));
#130502=DIRECTION('center_axis',(1.56508116445277E-16,-1.,0.));
#130503=DIRECTION('ref_axis',(1.,1.56508116445277E-16,0.));
#130504=DIRECTION('center_axis',(0.,1.,0.));
#130505=DIRECTION('ref_axis',(0.,0.,1.));
#130506=DIRECTION('center_axis',(-1.56508116445277E-16,1.,0.));
#130507=DIRECTION('ref_axis',(-1.,-1.56508116445277E-16,0.));
#130508=DIRECTION('',(0.,1.,0.));
#130509=DIRECTION('center_axis',(0.,1.,0.));
#130510=DIRECTION('ref_axis',(0.,0.,1.));
#130511=DIRECTION('center_axis',(0.,0.,1.));
#130512=DIRECTION('ref_axis',(1.,0.,0.));
#130513=DIRECTION('center_axis',(0.,0.,1.));
#130514=DIRECTION('ref_axis',(1.,0.,0.));
#130515=DIRECTION('',(0.,0.,1.));
#130516=DIRECTION('center_axis',(0.,0.,1.));
#130517=DIRECTION('ref_axis',(1.,0.,0.));
#130518=DIRECTION('center_axis',(0.,0.,1.));
#130519=DIRECTION('ref_axis',(1.,0.,0.));
#130520=DIRECTION('center_axis',(0.,0.,1.));
#130521=DIRECTION('ref_axis',(1.,0.,0.));
#130522=DIRECTION('',(0.,0.,1.));
#130523=DIRECTION('center_axis',(0.,0.,1.));
#130524=DIRECTION('ref_axis',(1.,0.,0.));
#130525=DIRECTION('center_axis',(0.,0.,1.));
#130526=DIRECTION('ref_axis',(1.,0.,0.));
#130527=DIRECTION('center_axis',(0.,0.,1.));
#130528=DIRECTION('ref_axis',(1.,0.,0.));
#130529=DIRECTION('',(0.,0.,1.));
#130530=DIRECTION('center_axis',(0.,0.,1.));
#130531=DIRECTION('ref_axis',(1.,0.,0.));
#130532=DIRECTION('',(0.,0.,1.));
#130533=DIRECTION('center_axis',(1.,0.,-1.0842021724855E-16));
#130534=DIRECTION('ref_axis',(-1.0842021724855E-16,0.,-1.));
#130535=DIRECTION('',(1.0842021724855E-16,0.,1.));
#130536=DIRECTION('',(0.,1.,0.));
#130537=DIRECTION('',(0.,0.,1.));
#130538=DIRECTION('',(0.,-1.,0.));
#130539=DIRECTION('center_axis',(1.,0.,-1.0842021724855E-16));
#130540=DIRECTION('ref_axis',(-1.0842021724855E-16,0.,-1.));
#130541=DIRECTION('',(0.,0.,1.));
#130542=DIRECTION('',(0.,1.,0.));
#130543=DIRECTION('',(-1.0842021724855E-16,0.,-1.));
#130544=DIRECTION('',(0.,-1.,0.));
#130545=DIRECTION('center_axis',(0.,0.,-1.));
#130546=DIRECTION('ref_axis',(-1.,0.,0.));
#130547=DIRECTION('',(1.,1.56508116445277E-16,0.));
#130548=DIRECTION('',(0.,-1.,0.));
#130549=DIRECTION('',(1.,0.,0.));
#130550=DIRECTION('',(0.,1.,0.));
#130551=DIRECTION('',(-1.,0.,0.));
#130552=DIRECTION('',(0.,-1.,0.));
#130553=DIRECTION('',(-1.,-1.56508116445277E-16,0.));
#130554=DIRECTION('center_axis',(-1.,0.,2.16840434497101E-16));
#130555=DIRECTION('ref_axis',(2.16840434497101E-16,0.,1.));
#130556=DIRECTION('',(2.16840434497101E-16,0.,1.));
#130557=DIRECTION('',(0.,-1.,0.));
#130558=DIRECTION('',(-2.16840434497101E-16,0.,-1.));
#130559=DIRECTION('',(0.,1.,0.));
#130560=DIRECTION('center_axis',(0.,0.,1.));
#130561=DIRECTION('ref_axis',(1.,0.,0.));
#130562=DIRECTION('',(-1.,0.,0.));
#130563=DIRECTION('',(0.,1.,0.));
#130564=DIRECTION('',(1.,1.56508116445277E-16,0.));
#130565=DIRECTION('',(-1.,-1.56508116445277E-16,0.));
#130566=DIRECTION('',(0.,1.,0.));
#130567=DIRECTION('',(1.,0.,0.));
#130568=DIRECTION('',(0.,-1.,0.));
#130569=DIRECTION('center_axis',(0.,1.,0.));
#130570=DIRECTION('ref_axis',(0.,0.,1.));
#130571=DIRECTION('',(1.,0.,0.));
#130572=DIRECTION('',(-2.16840434497101E-16,0.,-1.));
#130573=DIRECTION('',(-1.,0.,0.));
#130574=DIRECTION('',(1.0842021724855E-16,0.,1.));
#130575=DIRECTION('center_axis',(0.,1.,0.));
#130576=DIRECTION('ref_axis',(0.,0.,1.));
#130577=DIRECTION('',(1.,0.,0.));
#130578=DIRECTION('',(2.16840434497101E-16,0.,1.));
#130579=DIRECTION('',(-1.,0.,0.));
#130580=DIRECTION('',(-1.0842021724855E-16,0.,-1.));
#130581=DIRECTION('center_axis',(1.56508116445277E-16,-1.,0.));
#130582=DIRECTION('ref_axis',(1.,1.56508116445277E-16,0.));
#130583=DIRECTION('',(0.707106781186543,1.10667950449189E-16,0.707106781186552));
#130584=DIRECTION('',(-0.707106781186552,-1.1066795044919E-16,0.707106781186543));
#130585=DIRECTION('center_axis',(-1.56508116445277E-16,1.,0.));
#130586=DIRECTION('ref_axis',(-1.,-1.56508116445277E-16,0.));
#130587=DIRECTION('',(-0.707106781186543,-1.10667950449189E-16,-0.707106781186552));
#130588=DIRECTION('',(0.707106781186543,1.10667950449189E-16,-0.707106781186552));
#130589=DIRECTION('center_axis',(0.,0.,1.));
#130590=DIRECTION('ref_axis',(1.,0.,0.));
#130591=DIRECTION('center_axis',(0.,0.,1.));
#130592=DIRECTION('ref_axis',(1.,0.,0.));
#130593=DIRECTION('center_axis',(0.707106781186552,0.,0.707106781186543));
#130594=DIRECTION('ref_axis',(0.,-1.,0.));
#130595=DIRECTION('',(-0.707106781186543,-1.64540693022729E-16,0.707106781186552));
#130596=DIRECTION('center_axis',(0.707106781186543,0.,0.707106781186552));
#130597=DIRECTION('ref_axis',(0.,-1.,0.));
#130598=DIRECTION('',(0.707106781186553,0.,-0.707106781186542));
#130599=DIRECTION('center_axis',(-0.577350269189633,0.57735026918962,-0.577350269189624));
#130600=DIRECTION('ref_axis',(-0.707106781186542,-2.77555756156289E-17,
0.707106781186553));
#130601=DIRECTION('',(5.02745856021284E-15,0.707106781186552,0.707106781186543));
#130602=DIRECTION('',(-0.707106781186546,-0.707106781186549,1.21565128983085E-14));
#130603=DIRECTION('center_axis',(-0.577350269189615,-0.577350269189639,
-0.577350269189623));
#130604=DIRECTION('ref_axis',(-6.38378239159465E-16,0.707106781186538,-0.707106781186557));
#130605=DIRECTION('',(0.707106781186556,-0.707106781186539,1.22847104107341E-14));
#130606=DIRECTION('',(-9.90325783487554E-15,0.707106781186543,-0.707106781186552));
#130607=DIRECTION('center_axis',(0.707106781186552,0.,-0.707106781186543));
#130608=DIRECTION('ref_axis',(0.,-1.,0.));
#130609=DIRECTION('',(0.707106781186543,1.23903709934808E-16,0.707106781186552));
#130610=DIRECTION('center_axis',(-0.707106781186549,0.707106781186546,7.66646708341689E-17));
#130611=DIRECTION('ref_axis',(-1.0842021724855E-16,4.68386162474976E-31,
-1.));
#130612=DIRECTION('',(-0.707106781186546,-0.707106781186549,-1.22206116545212E-14));
#130613=DIRECTION('center_axis',(0.,0.707106781186543,-0.707106781186552));
#130614=DIRECTION('ref_axis',(1.,0.,0.));
#130615=DIRECTION('',(0.,0.707106781186552,0.707106781186543));
#130616=DIRECTION('center_axis',(-0.707106781186552,0.,0.707106781186543));
#130617=DIRECTION('ref_axis',(0.,-1.,0.));
#130618=DIRECTION('',(0.707106781186543,0.,0.707106781186552));
#130619=DIRECTION('',(-0.707106781186543,9.61481343191795E-17,-0.707106781186552));
#130620=DIRECTION('center_axis',(0.,0.707106781186552,0.707106781186543));
#130621=DIRECTION('ref_axis',(-1.,0.,0.));
#130622=DIRECTION('',(9.90325783487536E-15,0.707106781186543,-0.707106781186552));
#130623=DIRECTION('center_axis',(0.707106781186539,0.707106781186556,-7.66646708341678E-17));
#130624=DIRECTION('ref_axis',(1.0842021724855E-16,4.31408307542741E-31,
1.));
#130625=DIRECTION('',(0.707106781186556,-0.707106781186539,-2.3796250225573E-15));
#130626=DIRECTION('center_axis',(0.707106781186552,0.,-0.707106781186543));
#130627=DIRECTION('ref_axis',(0.,-1.,0.));
#130628=DIRECTION('',(-0.707106781186542,4.06369830879181E-17,-0.707106781186553));
#130629=DIRECTION('center_axis',(-0.577350269189633,0.57735026918962,0.577350269189625));
#130630=DIRECTION('ref_axis',(0.707106781186543,-1.38777878078144E-16,0.707106781186553));
#130631=DIRECTION('',(-4.90355485027803E-15,-0.707106781186552,0.707106781186543));
#130632=DIRECTION('center_axis',(0.577350269189634,0.577350269189618,-0.577350269189626));
#130633=DIRECTION('ref_axis',(-0.707106781186543,-1.38777878078144E-16,
-0.707106781186553));
#130634=DIRECTION('',(-0.707106781186543,0.707106781186552,-9.90508538817675E-15));
#130635=DIRECTION('center_axis',(0.577350269189626,-0.577350269189634,-0.577350269189618));
#130636=DIRECTION('ref_axis',(0.707106781186553,0.707106781186543,1.38777878078144E-16));
#130637=DIRECTION('',(0.707106781186552,0.707106781186543,-1.19609907444045E-16));
#130638=DIRECTION('center_axis',(-0.577350269189623,-0.577350269189639,
0.577350269189615));
#130639=DIRECTION('ref_axis',(0.707106781186557,-0.707106781186538,-6.38378239159465E-16));
#130640=DIRECTION('',(1.96142194011124E-14,-0.707106781186543,-0.707106781186552));
#130641=DIRECTION('center_axis',(0.,0.707106781186543,0.707106781186552));
#130642=DIRECTION('ref_axis',(-1.,0.,0.));
#130643=DIRECTION('',(-1.46829089752187E-14,-0.707106781186552,0.707106781186543));
#130644=DIRECTION('center_axis',(0.707106781186552,0.707106781186543,-1.53329341668338E-16));
#130645=DIRECTION('ref_axis',(2.16840434497101E-16,-6.28623533847994E-31,
1.));
#130646=DIRECTION('',(-0.707106781186542,0.707106781186553,2.77555756156289E-17));
#130647=DIRECTION('center_axis',(-0.707106781186543,0.707106781186552,1.53329341668336E-16));
#130648=DIRECTION('ref_axis',(-2.16840434497101E-16,-6.77927340424307E-31,
-1.));
#130649=DIRECTION('',(0.707106781186552,0.707106781186543,9.90508538817668E-15));
#130650=DIRECTION('center_axis',(0.,0.707106781186552,-0.707106781186543));
#130651=DIRECTION('ref_axis',(1.,0.,0.));
#130652=DIRECTION('',(4.77965114034336E-15,-0.707106781186543,-0.707106781186552));
#130653=DIRECTION('center_axis',(0.577350269189624,0.577350269189617,0.577350269189636));
#130654=DIRECTION('ref_axis',(0.707106781186555,-2.22044604925031E-16,-0.70710678118654));
#130655=DIRECTION('',(-0.707106781186555,6.83925587035508E-17,0.70710678118654));
#130656=DIRECTION('center_axis',(0.577350269189617,-0.577350269189632,0.577350269189628));
#130657=DIRECTION('ref_axis',(1.11022302462516E-16,-0.707106781186545,-0.70710678118655));
#130658=DIRECTION('',(0.707106781186555,5.55111512312578E-17,-0.70710678118654));
#130659=DIRECTION('center_axis',(-0.70710678118654,0.,-0.707106781186555));
#130660=DIRECTION('ref_axis',(0.,-1.,0.));
#130661=DIRECTION('',(-7.98460980840786E-17,1.,-5.26168882227312E-15));
#130662=DIRECTION('',(1.,7.9846098084027E-17,-7.23198349299978E-31));
#130663=DIRECTION('',(-3.2543412409325E-15,1.,-4.12170297892093E-15));
#130664=DIRECTION('',(1.,1.97758476261357E-15,-7.74081827338172E-30));
#130665=DIRECTION('',(0.,0.,1.));
#130666=DIRECTION('',(1.,0.,0.));
#130667=DIRECTION('',(2.07971999539315E-17,1.,-4.12170297892093E-15));
#130668=DIRECTION('',(1.,-2.08166817117129E-17,1.15262392111919E-31));
#130669=DIRECTION('',(1.,6.1131655293423E-15,1.22464679914696E-16));
#130670=DIRECTION('',(-6.14092110495792E-15,1.,-4.01367313797697E-15));
#130671=DIRECTION('',(-3.12070361428227E-17,-1.,9.71464625616431E-17));
#130672=DIRECTION('',(0.707106781186549,7.78339902308997E-17,0.707106781186549));
#130673=DIRECTION('',(1.59594559789645E-16,2.19609194571417E-16,0.999999999999999));
#130674=DIRECTION('',(1.,6.9388939039072E-18,6.93889390390724E-18));
#130675=DIRECTION('',(0.,0.,1.));
#130676=DIRECTION('',(1.,0.,0.));
#130677=DIRECTION('',(-6.75514372791703E-18,3.60822483003176E-16,1.));
#130678=DIRECTION('',(0.999999999999998,-5.93500594022055E-32,6.9388939039072E-18));
#130679=DIRECTION('',(6.93889390390717E-18,-1.,-2.53201652600347E-17));
#130680=DIRECTION('',(1.,6.93889390390719E-18,6.93889390390722E-18));
#130681=DIRECTION('',(3.33066907387539E-16,-5.02035771436917E-16,1.));
#130682=DIRECTION('',(0.999999999999998,6.93889390390744E-18,-3.33066907387551E-16));
#130683=DIRECTION('',(-1.08415542651314E-29,-4.18769044590029E-16,1.));
#130684=DIRECTION('',(0.999999999999998,6.93889390390731E-18,3.01106021115399E-31));
#130685=DIRECTION('',(3.33066907387539E-16,-5.02035771436917E-16,1.));
#130686=DIRECTION('',(0.999999999999998,6.93889390390744E-18,-3.33066907387551E-16));
#130687=DIRECTION('',(6.93889390390714E-18,-1.,2.28847549044396E-17));
#130688=DIRECTION('',(1.,6.93889390390731E-18,2.46519032881566E-31));
#130689=DIRECTION('',(-1.08414448429446E-29,-4.18769044590029E-16,1.));
#130690=DIRECTION('',(0.999999999999998,6.93889390390731E-18,3.01215443302163E-31));
#130691=DIRECTION('',(-6.93889390391932E-18,2.19609189225654E-16,1.));
#130692=DIRECTION('',(0.999999999999999,6.93889390390716E-18,6.93889390390724E-18));
#130693=DIRECTION('',(6.93889390390717E-18,-1.,2.19609194569436E-16));
#130694=DIRECTION('',(1.,6.93889390390723E-18,6.93889390390723E-18));
#130695=DIRECTION('',(6.93889390390703E-18,-1.,2.28847549044396E-17));
#130696=DIRECTION('',(1.,6.93889390390731E-18,2.46519032881566E-31));
#130697=DIRECTION('',(1.3877786463362E-17,1.,-4.99600361081319E-16));
#130698=DIRECTION('',(-6.75514372791544E-18,3.19189119579732E-16,1.));
#130699=DIRECTION('',(6.93889390390717E-18,-1.,2.19609194569436E-16));
#130700=DIRECTION('',(1.,6.93889390390723E-18,6.93889390390723E-18));
#130701=DIRECTION('',(-1.68707298753438E-12,-1.09186707627277E-16,1.));
#130702=DIRECTION('',(-1.,1.91513471747517E-15,-1.68718058920808E-12));
#130703=DIRECTION('',(-9.57368529015522E-17,-1.,2.0580904343381E-16));
#130704=DIRECTION('',(0.999999999999999,-9.57368529015413E-17,5.15004705547994E-14));
#130705=DIRECTION('',(-1.68707298753438E-12,-1.09186707627277E-16,1.));
#130706=DIRECTION('',(-1.,1.91513471747517E-15,-1.68718058920808E-12));
#130707=DIRECTION('',(-1.68707298753438E-12,-1.09186707627277E-16,1.));
#130708=DIRECTION('',(-1.,1.91513471747517E-15,-1.68718058920808E-12));
#130709=DIRECTION('',(-1.68707298753438E-12,-1.09186707627277E-16,1.));
#130710=DIRECTION('',(-1.,1.91513471747517E-15,-1.68718058920808E-12));
#130711=DIRECTION('',(6.93889390390718E-18,-1.,9.71445146547006E-17));
#130712=DIRECTION('',(1.,6.93889390390723E-18,6.93889390390723E-18));
#130713=DIRECTION('',(6.93889390390718E-18,-1.,9.71445146547006E-17));
#130714=DIRECTION('',(1.,6.93889390390723E-18,6.93889390390723E-18));
#130715=DIRECTION('',(1.07601673699705E-16,9.95799250102958E-17,-0.999999999999999));
#130716=DIRECTION('',(1.,6.93889390390694E-18,-3.45776087865591E-33));
#130717=DIRECTION('',(0.,0.,1.));
#130718=DIRECTION('',(1.,0.,0.));
#130719=CARTESIAN_POINT('',(0.,0.,0.));
#130720=CARTESIAN_POINT('',(0.,0.,0.));
#130721=CARTESIAN_POINT('',(0.,0.,0.));
#130722=CARTESIAN_POINT('Origin',(-21.9500000210213,0.999999999999992,-6.00000000000001));
#130723=CARTESIAN_POINT('',(-21.5093868137065,-0.185251134376082,-7.65234634179685));
#130724=CARTESIAN_POINT('',(-21.5094163772775,-0.185130046756847,-7.7903497740652));
#130725=CARTESIAN_POINT('',(-21.5093868137063,-0.185251134376008,-6.00000000000001));
#130726=CARTESIAN_POINT('',(-23.2143447276962,0.9984309442522,-7.94368623524854));
#130727=CARTESIAN_POINT('Ctrl Pts',(-21.5094163780221,-0.185130047031939,
-7.79034977411791));
#130728=CARTESIAN_POINT('Ctrl Pts',(-21.5560227037756,-0.202348715799771,
-7.79364848584603));
#130729=CARTESIAN_POINT('Ctrl Pts',(-21.6036752898958,-0.21684557206526,
-7.79691771167341));
#130730=CARTESIAN_POINT('Ctrl Pts',(-21.6520290024672,-0.228522300280214,
-7.80012768793153));
#130731=CARTESIAN_POINT('Ctrl Pts',(-21.7003642493108,-0.240194569286675,
-7.80333643833655));
#130732=CARTESIAN_POINT('Ctrl Pts',(-21.7494000855687,-0.24904888749276,
-7.80648593753533));
#130733=CARTESIAN_POINT('Ctrl Pts',(-21.7987843632908,-0.255021079848016,
-7.80957109983421));
#130734=CARTESIAN_POINT('Ctrl Pts',(-21.8482059171473,-0.260997780120666,
-7.81265859086867));
#130735=CARTESIAN_POINT('Ctrl Pts',(-21.8979764202531,-0.264087851279457,
-7.81568173932712));
#130736=CARTESIAN_POINT('Ctrl Pts',(-21.9477356337069,-0.264262041475781,
-7.8186598005637));
#130737=CARTESIAN_POINT('Ctrl Pts',(-21.9975111599162,-0.264436288777552,
-7.82163883810962));
#130738=CARTESIAN_POINT('Ctrl Pts',(-22.0472753250638,-0.261692426856607,
-7.82457301529161));
#130739=CARTESIAN_POINT('Ctrl Pts',(-22.0966608194572,-0.256039733590408,
-7.82750339621611));
#130740=CARTESIAN_POINT('Ctrl Pts',(-22.1461396084972,-0.250376361763082,
-7.83043931295342));
#130741=CARTESIAN_POINT('Ctrl Pts',(-22.1952381051126,-0.241792640298569,
-7.83337189951185));
#130742=CARTESIAN_POINT('Ctrl Pts',(-22.2435819516393,-0.230342864021984,
-7.83635887232752));
#130743=CARTESIAN_POINT('Ctrl Pts',(-22.2879715574474,-0.219829611725669,
-7.83910152843317));
#130744=CARTESIAN_POINT('Ctrl Pts',(-22.3317245576032,-0.206900089373834,
-7.84189069189933));
#130745=CARTESIAN_POINT('Ctrl Pts',(-22.3745509540369,-0.191636072322134,
-7.84477645837742));
#130746=CARTESIAN_POINT('Ctrl Pts',(-22.3745684736764,-0.191629828040586,
-7.84477763890141));
#130747=CARTESIAN_POINT('Ctrl Pts',(-22.3745859931617,-0.191623583368604,
-7.84477881944157));
#130748=CARTESIAN_POINT('Ctrl Pts',(-22.3746035124926,-0.191617338306218,
-7.8447799999979));
#130749=CARTESIAN_POINT('Ctrl Pts',(-22.4174213951043,-0.176354178445099,
-7.84766532265466));
#130750=CARTESIAN_POINT('Ctrl Pts',(-22.4594737121133,-0.158695428803833,
-7.85065492207322));
#130751=CARTESIAN_POINT('Ctrl Pts',(-22.5004931234151,-0.1387643463029,
-7.85368972442065));
#130752=CARTESIAN_POINT('Ctrl Pts',(-22.5053443484456,-0.136407165562289,
-7.85404864008139));
#130753=CARTESIAN_POINT('Ctrl Pts',(-22.5101810940409,-0.134018252268478,
-7.85440818799464));
#130754=CARTESIAN_POINT('Ctrl Pts',(-22.5150028933519,-0.131597851584441,
-7.85476827044094));
#130755=CARTESIAN_POINT('Ctrl Pts',(-22.5589591683231,-0.109533101240051,
-7.85805083821301));
#130756=CARTESIAN_POINT('Ctrl Pts',(-22.6016771164603,-0.0848470764096622,
-7.86137728959589));
#130757=CARTESIAN_POINT('Ctrl Pts',(-22.6428506708358,-0.0577313326929714,
-7.86468832169072));
#130758=CARTESIAN_POINT('Ctrl Pts',(-22.6839864864387,-0.0306404426694719,
-7.86799631896649));
#130759=CARTESIAN_POINT('Ctrl Pts',(-22.7235809510388,-0.00112451343309885,
-7.8712886285325));
#130760=CARTESIAN_POINT('Ctrl Pts',(-22.7613552207452,0.0305978737586179,
-7.8745272073172));
#130761=CARTESIAN_POINT('Ctrl Pts',(-22.7991113553565,0.0623050313107944,
-7.87776423128866));
#130762=CARTESIAN_POINT('Ctrl Pts',(-22.8350490983818,0.0962164620954286,
-7.88094747473338));
#130763=CARTESIAN_POINT('Ctrl Pts',(-22.868914357826,0.1320884559541,-7.88406294348325));
#130764=CARTESIAN_POINT('Ctrl Pts',(-22.9027781399198,0.167958884919679,
-7.88717827632276));
#130765=CARTESIAN_POINT('Ctrl Pts',(-22.9345695304503,0.205789724678508,
-7.89022588030349));
#130766=CARTESIAN_POINT('Ctrl Pts',(-22.9640590917588,0.245312165147836,
-7.8932161980417));
#130767=CARTESIAN_POINT('Ctrl Pts',(-22.9935811343522,0.284878137619522,
-7.89620980946617));
#130768=CARTESIAN_POINT('Ctrl Pts',(-23.0207960397528,0.326139522802212,
-7.89914618738315));
#130769=CARTESIAN_POINT('Ctrl Pts',(-23.0455007030266,0.368800646431264,
-7.90205868834638));
#130770=CARTESIAN_POINT('Ctrl Pts',(-23.0702217701547,0.411490096973965,
-7.9049731232053));
#130771=CARTESIAN_POINT('Ctrl Pts',(-23.0924288439946,0.455581259255592,
-7.90786402195172));
#130772=CARTESIAN_POINT('Ctrl Pts',(-23.1119503464419,0.500750344982422,
-7.91078362691741));
#130773=CARTESIAN_POINT('Ctrl Pts',(-23.1302244959823,0.543033290642225,
-7.91351667975933));
#130774=CARTESIAN_POINT('Ctrl Pts',(-23.1461451885907,0.586261260105575,
-7.9162754435804));
#130775=CARTESIAN_POINT('Ctrl Pts',(-23.1596031204119,0.630143818282359,
-7.91911205284188));
#130776=CARTESIAN_POINT('Ctrl Pts',(-23.1605484930719,0.633226414575799,
-7.91931131472539));
#130777=CARTESIAN_POINT('Ctrl Pts',(-23.1614817293283,0.636312254833964,
-7.91951096074278));
#130778=CARTESIAN_POINT('Ctrl Pts',(-23.1624027985064,0.639401244864388,
-7.91971100896574));
#130779=CARTESIAN_POINT('Ctrl Pts',(-23.1660690594275,0.651696785420236,
-7.92050728898423));
#130780=CARTESIAN_POINT('Ctrl Pts',(-23.1695424991904,0.664041822917359,
-7.92130997070593));
#130781=CARTESIAN_POINT('Ctrl Pts',(-23.172821312714,0.676429714133373,
-7.92212022415011));
#130782=CARTESIAN_POINT('Ctrl Pts',(-23.1728251181124,0.676444091548047,
-7.9221211645321));
#130783=CARTESIAN_POINT('Ctrl Pts',(-23.1728289232487,0.676458469020474,
-7.92212210492429));
#130784=CARTESIAN_POINT('Ctrl Pts',(-23.1728327281229,0.676472846550637,
-7.92212304532667));
#130785=CARTESIAN_POINT('Ctrl Pts',(-23.185485780736,0.724285109732905,
-7.92525033950908));
#130786=CARTESIAN_POINT('Ctrl Pts',(-23.1952650209804,0.772848506784041,
-7.92849472874584));
#130787=CARTESIAN_POINT('Ctrl Pts',(-23.2021445513064,0.821870800689957,
-7.93179069122616));
#130788=CARTESIAN_POINT('Ctrl Pts',(-23.2043730055447,0.837750364185012,
-7.93285833701164));
#130789=CARTESIAN_POINT('Ctrl Pts',(-23.2062971123773,0.853677678218472,
-7.93393139425532));
#130790=CARTESIAN_POINT('Ctrl Pts',(-23.207915830539,0.869641649335481,
-7.9350076359548));
#130791=CARTESIAN_POINT('Ctrl Pts',(-23.2122479261328,0.912365238020205,
-7.93788792854347));
#130792=CARTESIAN_POINT('Ctrl Pts',(-23.2143946495102,0.955357932434763,
-7.94079152872966));
#130793=CARTESIAN_POINT('Ctrl Pts',(-23.2143447276962,0.998430944252203,
-7.94368623524854));
#130794=CARTESIAN_POINT('',(-22.9081161737437,1.82521129893649,-8.00000000000001));
#130795=CARTESIAN_POINT('Ctrl Pts',(-23.214499040964,0.998425654430992,
-7.94377502574648));
#130796=CARTESIAN_POINT('Ctrl Pts',(-23.2145652572834,1.05160995694309,
-7.94742259194512));
#130797=CARTESIAN_POINT('Ctrl Pts',(-23.2112760714399,1.10474931579339,
-7.95103824992359));
#130798=CARTESIAN_POINT('Ctrl Pts',(-23.2046495127751,1.15752746694461,
-7.95457642429432));
#130799=CARTESIAN_POINT('Ctrl Pts',(-23.200690529771,1.18905933951439,-7.95669027748839));
#130800=CARTESIAN_POINT('Ctrl Pts',(-23.1955440476404,1.22043256383109,
-7.95877520624573));
#130801=CARTESIAN_POINT('Ctrl Pts',(-23.1892205216726,1.25158060490748,
-7.96082825372533));
#130802=CARTESIAN_POINT('Ctrl Pts',(-23.1830565039967,1.28194294970399,
-7.96282951394283));
#130803=CARTESIAN_POINT('Ctrl Pts',(-23.1757783610785,1.3120702156534,-7.96479911529432));
#130804=CARTESIAN_POINT('Ctrl Pts',(-23.167400318562,1.34190168988727,-7.96673896897314));
#130805=CARTESIAN_POINT('Ctrl Pts',(-23.1581792637964,1.37473485552339,
-7.96887401388065));
#130806=CARTESIAN_POINT('Ctrl Pts',(-23.1476332527721,1.40718326839631,
-7.97097123410555));
#130807=CARTESIAN_POINT('Ctrl Pts',(-23.1357875330326,1.43916765176641,
-7.97303937742848));
#130808=CARTESIAN_POINT('Ctrl Pts',(-23.1223190451642,1.47553363786722,
-7.97539083971763));
#130809=CARTESIAN_POINT('Ctrl Pts',(-23.1071842951135,1.5112621136308,-7.97770216398833));
#130810=CARTESIAN_POINT('Ctrl Pts',(-23.0904306503722,1.54624008424715,
-7.97999558215418));
#130811=CARTESIAN_POINT('Ctrl Pts',(-23.0519689624722,1.62653973306939,
-7.98526062955616));
#130812=CARTESIAN_POINT('Ctrl Pts',(-23.0051370109133,1.70254619131719,
-7.99039898368457));
#130813=CARTESIAN_POINT('Ctrl Pts',(-22.9507170505117,1.77299785050667,
-7.99582789768067));
#130814=CARTESIAN_POINT('Ctrl Pts',(-22.9369822977737,1.79077875500949,
-7.99719807124974));
#130815=CARTESIAN_POINT('Ctrl Pts',(-22.9227769036649,1.80818937719799,
-7.99858622413477));
#130816=CARTESIAN_POINT('Ctrl Pts',(-22.9081161737437,1.82521129893648,
-8.));
#130817=CARTESIAN_POINT('',(-21.0014870926804,1.83623171117239,-8.00000000000001));
#130818=CARTESIAN_POINT('Origin',(-21.9500000210213,0.999999999999992,-8.00000000000001));
#130819=CARTESIAN_POINT('Ctrl Pts',(-21.0014870926799,1.83623171117168,
-8.00000000000009));
#130820=CARTESIAN_POINT('Ctrl Pts',(-21.0556763883481,1.89769702853811,
-7.99452566673546));
#130821=CARTESIAN_POINT('Ctrl Pts',(-21.115703404117,1.95374207720739,-7.98885938194356));
#130822=CARTESIAN_POINT('Ctrl Pts',(-21.213056154207,2.02836378585187,-7.98055621038558));
#130823=CARTESIAN_POINT('Ctrl Pts',(-21.2465536944085,2.05156172433473,
-7.97783121513637));
#130824=CARTESIAN_POINT('Ctrl Pts',(-21.3106622633174,2.09152175596766,
-7.97286867380942));
#130825=CARTESIAN_POINT('Ctrl Pts',(-21.340959808357,2.10871226662972,-7.97061964930845));
#130826=CARTESIAN_POINT('Ctrl Pts',(-21.3973158518954,2.13767970829369,
-7.96660205612705));
#130827=CARTESIAN_POINT('Ctrl Pts',(-21.4231368507775,2.14986534191615,
-7.96482102287359));
#130828=CARTESIAN_POINT('Ctrl Pts',(-21.4861731928968,2.17704416147748,
-7.96060134739312));
#130829=CARTESIAN_POINT('Ctrl Pts',(-21.5237330243955,2.19116126746671,
-7.95819131267466));
#130830=CARTESIAN_POINT('Ctrl Pts',(-21.6583691063655,2.23457891380381,
-7.94982112103086));
#130831=CARTESIAN_POINT('Ctrl Pts',(-21.7582174921326,2.2539741076228,-7.94411972376694));
#130832=CARTESIAN_POINT('Ctrl Pts',(-21.8895157725744,2.26341575427773,
-7.93630584710667));
#130833=CARTESIAN_POINT('Ctrl Pts',(-21.9197934212877,2.264501873635,-7.93447981764929));
#130834=CARTESIAN_POINT('Ctrl Pts',(-21.9669493180662,2.26449895246781,
-7.93155976036272));
#130835=CARTESIAN_POINT('Ctrl Pts',(-21.9838161661189,2.26416032272429,
-7.93049969359661));
#130836=CARTESIAN_POINT('Ctrl Pts',(-22.0226124674591,2.26260437420453,
-7.92801863944682));
#130837=CARTESIAN_POINT('Ctrl Pts',(-22.0445240111228,2.26115322396874,
-7.92658780616593));
#130838=CARTESIAN_POINT('Ctrl Pts',(-22.1632250073712,2.25018136775124,
-7.91871275381176));
#130839=CARTESIAN_POINT('Ctrl Pts',(-22.2587071691502,2.23008884080025,
-7.91195899415794));
#130840=CARTESIAN_POINT('Ctrl Pts',(-22.4009517577418,2.18253252411451,
-7.90184864474664));
#130841=CARTESIAN_POINT('Ctrl Pts',(-22.4498700097206,2.16270019663609,
-7.89835563899462));
#130842=CARTESIAN_POINT('Ctrl Pts',(-22.5239328467189,2.12713217698962,
-7.89305789733272));
#130843=CARTESIAN_POINT('Ctrl Pts',(-22.5500028089861,2.11347326322552,
-7.89119048019733));
#130844=CARTESIAN_POINT('Ctrl Pts',(-22.6022588512574,2.08372574464128,
-7.8874344850262));
#130845=CARTESIAN_POINT('Ctrl Pts',(-22.6283827348897,2.06756742002737,
-7.88554983023936));
#130846=CARTESIAN_POINT('Ctrl Pts',(-22.7335197672645,1.99711787732585,
-7.87790034022239));
#130847=CARTESIAN_POINT('Ctrl Pts',(-22.8068207268085,1.93488341748448,
-7.87243807537444));
#130848=CARTESIAN_POINT('Ctrl Pts',(-22.8989371498963,1.83665093413516,
-7.86464977578417));
#130849=CARTESIAN_POINT('Ctrl Pts',(-22.9241656815761,1.8071353071863,-7.8623919306256));
#130850=CARTESIAN_POINT('Ctrl Pts',(-22.9646626696585,1.75508715350208,
-7.85846180110323));
#130851=CARTESIAN_POINT('Ctrl Pts',(-22.9806344570043,1.73313664296803,
-7.85681841327607));
#130852=CARTESIAN_POINT('Ctrl Pts',(-23.0050187130218,1.69725162314212,
-7.85412509710346));
#130853=CARTESIAN_POINT('Ctrl Pts',(-23.0138897256297,1.68363947155786,
-7.85310140435618));
#130854=CARTESIAN_POINT('Ctrl Pts',(-23.0341402611235,1.6512167808574,-7.85065386673856));
#130855=CARTESIAN_POINT('Ctrl Pts',(-23.0452949934441,1.6322753712771,-7.84921881753903));
#130856=CARTESIAN_POINT('Ctrl Pts',(-23.1028803348784,1.52839144417269,
-7.84135796533044));
#130857=CARTESIAN_POINT('Ctrl Pts',(-23.139933742053,1.43862136049432,-7.83462861707198));
#130858=CARTESIAN_POINT('Ctrl Pts',(-23.1807277311189,1.2950011794314,-7.8245579547231));
#130859=CARTESIAN_POINT('Ctrl Pts',(-23.1919145282173,1.24365110826614,
-7.82107875406906));
#130860=CARTESIAN_POINT('Ctrl Pts',(-23.2043044865844,1.16288957147469,
-7.81580897792239));
#130861=CARTESIAN_POINT('Ctrl Pts',(-23.2077313062482,1.13388404288782,
-7.8139553759453));
#130862=CARTESIAN_POINT('Ctrl Pts',(-23.2126607866774,1.07460118431117,
-7.81023886929075));
#130863=CARTESIAN_POINT('Ctrl Pts',(-23.2140854828188,1.04433639642869,
-7.80837943730091));
#130864=CARTESIAN_POINT('Ctrl Pts',(-23.2150862913203,0.954254188213088,
-7.80293295978635));
#130865=CARTESIAN_POINT('Ctrl Pts',(-23.2115085428974,0.894486043265319,
-7.79943821327412));
#130866=CARTESIAN_POINT('Ctrl Pts',(-23.1955279036933,0.772920406599362,
-7.79234913308464));
#130867=CARTESIAN_POINT('Ctrl Pts',(-23.1827144823299,0.711349155456169,
-7.78876811501925));
#130868=CARTESIAN_POINT('Ctrl Pts',(-23.1556706852961,0.617173452003201,
-7.78301166934413));
#130869=CARTESIAN_POINT('Ctrl Pts',(-23.1445544577311,0.583782274133964,
-7.78091228675576));
#130870=CARTESIAN_POINT('Ctrl Pts',(-23.1259795189943,0.53489166656199,
-7.77769300599477));
#130871=CARTESIAN_POINT('Ctrl Pts',(-23.1195727673118,0.519008204948834,
-7.77662339963613));
#130872=CARTESIAN_POINT('Ctrl Pts',(-23.1051572771907,0.485262213960005,
-7.77429082755341));
#130873=CARTESIAN_POINT('Ctrl Pts',(-23.0970527916685,0.467446608869917,
-7.77302360369203));
#130874=CARTESIAN_POINT('Ctrl Pts',(-23.0561066392935,0.382711771129634,
-7.76684632678012));
#130875=CARTESIAN_POINT('Ctrl Pts',(-23.017805651613,0.318599687827898,
-7.76172380252077));
#130876=CARTESIAN_POINT('Ctrl Pts',(-22.929838491173,0.197151195717176,
-7.75149424034105));
#130877=CARTESIAN_POINT('Ctrl Pts',(-22.880209696823,0.140138106763055,
-7.74641058976998));
#130878=CARTESIAN_POINT('Ctrl Pts',(-22.8037491759279,0.0667229190159224,
-7.7395349037698));
#130879=CARTESIAN_POINT('Ctrl Pts',(-22.7809495947314,0.0463665362775556,
-7.73758457285688));
#130880=CARTESIAN_POINT('Ctrl Pts',(-22.734813362694,0.00808661056340476,
-7.73382093612577));
#130881=CARTESIAN_POINT('Ctrl Pts',(-22.7115447180439,-0.0098881306651899,
-7.73200638408686));
#130882=CARTESIAN_POINT('Ctrl Pts',(-22.6445653140699,-0.0579960945008118,
-7.72699187665342));
#130883=CARTESIAN_POINT('Ctrl Pts',(-22.5995528326252,-0.0862129826772939,
-7.72386041324328));
#130884=CARTESIAN_POINT('Ctrl Pts',(-22.4904547549625,-0.145388578462997,
-7.71663893156329));
#130885=CARTESIAN_POINT('Ctrl Pts',(-22.4252726569225,-0.1739342571129,
-7.71259883893754));
#130886=CARTESIAN_POINT('Ctrl Pts',(-22.3327810959289,-0.205467181841179,
-7.70686664940803));
#130887=CARTESIAN_POINT('Ctrl Pts',(-22.3072562013548,-0.213276696797498,
-7.70528386166558));
#130888=CARTESIAN_POINT('Ctrl Pts',(-22.2608925002553,-0.225872074130784,
-7.70237736538823));
#130889=CARTESIAN_POINT('Ctrl Pts',(-22.2401429436037,-0.230948185930413,
-7.70106544925019));
#130890=CARTESIAN_POINT('Ctrl Pts',(-22.2030075761668,-0.239041835201648,
-7.69868207233511));
#130891=CARTESIAN_POINT('Ctrl Pts',(-22.1866727945651,-0.242265421525683,
-7.69762058317892));
#130892=CARTESIAN_POINT('Ctrl Pts',(-22.1408160050136,-0.250377868835656,
-7.69460880869523));
#130893=CARTESIAN_POINT('Ctrl Pts',(-22.111178368738,-0.254542471526902,
-7.69262714430821));
#130894=CARTESIAN_POINT('Ctrl Pts',(-22.0027027415514,-0.265878073123162,
-7.68530725561696));
#130895=CARTESIAN_POINT('Ctrl Pts',(-21.9233840061674,-0.266695228159861,
-7.6798396469926));
#130896=CARTESIAN_POINT('Ctrl Pts',(-21.789564541093,-0.255492211394217,
-7.67076523367455));
#130897=CARTESIAN_POINT('Ctrl Pts',(-21.734975291159,-0.247303436806563,
-7.6671033899489));
#130898=CARTESIAN_POINT('Ctrl Pts',(-21.6522347269965,-0.229295773689886,
-7.66163623693413));
#130899=CARTESIAN_POINT('Ctrl Pts',(-21.6236073933802,-0.222006688364611,
-7.65975956079658));
#130900=CARTESIAN_POINT('Ctrl Pts',(-21.5663065847785,-0.205259094257848,
-7.65602639139567));
#130901=CARTESIAN_POINT('Ctrl Pts',(-21.5376640869836,-0.195763117627018,
-7.65417242371063));
#130902=CARTESIAN_POINT('Ctrl Pts',(-21.5093868137067,-0.185251134376157,
-7.65234634179685));
#130903=CARTESIAN_POINT('Origin',(-21.9500000210213,0.999999999999992,-6.00000000000001));
#130904=CARTESIAN_POINT('',(-21.5093868140292,-0.185251134496023,-7.15421782883515));
#130905=CARTESIAN_POINT('',(-21.5093591526456,-0.185356720995697,-7.28986799996607));
#130906=CARTESIAN_POINT('',(-21.5093868137063,-0.185251134376008,-6.00000000000001));
#130907=CARTESIAN_POINT('',(-23.2145649522473,1.00099359444644,-7.44330650983136));
#130908=CARTESIAN_POINT('Ctrl Pts',(-21.5093591533682,-0.185356721266173,
-7.28986800001162));
#130909=CARTESIAN_POINT('Ctrl Pts',(-21.5559477712327,-0.202794731700962,
-7.29280447580565));
#130910=CARTESIAN_POINT('Ctrl Pts',(-21.6035192041601,-0.217456141425245,
-7.29574978827595));
#130911=CARTESIAN_POINT('Ctrl Pts',(-21.6517131024261,-0.22921970626668,
-7.2987642189804));
#130912=CARTESIAN_POINT('Ctrl Pts',(-21.682553520669,-0.236747490338739,
-7.3006932246644));
#130913=CARTESIAN_POINT('Ctrl Pts',(-21.7136482905638,-0.24308939355335,
-7.30265082761511));
#130914=CARTESIAN_POINT('Ctrl Pts',(-21.744897502386,-0.248224113096361,
-7.30465399011448));
#130915=CARTESIAN_POINT('Ctrl Pts',(-21.7449142057305,-0.248226857709235,
-7.3046550608459));
#130916=CARTESIAN_POINT('Ctrl Pts',(-21.7449309091192,-0.248229601977445,
-7.30465613159035));
#130917=CARTESIAN_POINT('Ctrl Pts',(-21.7449476125523,-0.248232345901003,
-7.30465720234781));
#130918=CARTESIAN_POINT('Ctrl Pts',(-21.7902341497497,-0.255671702564202,
-7.30756025212355));
#130919=CARTESIAN_POINT('Ctrl Pts',(-21.8360112373321,-0.260597049194722,
-7.31056635456357));
#130920=CARTESIAN_POINT('Ctrl Pts',(-21.8819794934509,-0.262988071267566,
-7.31361640347263));
#130921=CARTESIAN_POINT('Ctrl Pts',(-21.8869280447319,-0.263245468357217,
-7.31394474578339));
#130922=CARTESIAN_POINT('Ctrl Pts',(-21.891878767541,-0.26347351898473,
-7.3142735973829));
#130923=CARTESIAN_POINT('Ctrl Pts',(-21.8968312572195,-0.263672215633016,
-7.31460288453286));
#130924=CARTESIAN_POINT('Ctrl Pts',(-21.9463665079808,-0.265659597523184,
-7.31789644446016));
#130925=CARTESIAN_POINT('Ctrl Pts',(-21.9960839415655,-0.264708253779789,
-7.32123302732497));
#130926=CARTESIAN_POINT('Ctrl Pts',(-22.0456178331554,-0.260838765858485,
-7.32455387831832));
#130927=CARTESIAN_POINT('Ctrl Pts',(-22.095105553473,-0.256972884744047,
-7.32787163389738));
#130928=CARTESIAN_POINT('Ctrl Pts',(-22.1444101675817,-0.250194598032994,
-7.33117339343978));
#130929=CARTESIAN_POINT('Ctrl Pts',(-22.1931768119306,-0.240561133120324,
-7.33442197708555));
#130930=CARTESIAN_POINT('Ctrl Pts',(-22.2419183466623,-0.230932628413967,
-7.33766888805745));
#130931=CARTESIAN_POINT('Ctrl Pts',(-22.2901224986033,-0.2184519603325,
-7.34086258283539));
#130932=CARTESIAN_POINT('Ctrl Pts',(-22.3374437766807,-0.203210226153336,
-7.34399017411066));
#130933=CARTESIAN_POINT('Ctrl Pts',(-22.3872426403831,-0.187170485178113,
-7.34728151572192));
#130934=CARTESIAN_POINT('Ctrl Pts',(-22.4360636024974,-0.168072553915644,
-7.3504994700433));
#130935=CARTESIAN_POINT('Ctrl Pts',(-22.4835147951651,-0.14606334295329,
-7.3536583656872));
#130936=CARTESIAN_POINT('Ctrl Pts',(-22.5286447817275,-0.125130773314123,
-7.35666273522874));
#130937=CARTESIAN_POINT('Ctrl Pts',(-22.5725356502153,-0.101564875153868,
-7.35961410525478));
#130938=CARTESIAN_POINT('Ctrl Pts',(-22.6148612676838,-0.0755294153820678,
-7.36254805775375));
#130939=CARTESIAN_POINT('Ctrl Pts',(-22.6572125276212,-0.0494781823385375,
-7.36548378775273));
#130940=CARTESIAN_POINT('Ctrl Pts',(-22.6979963045529,-0.0209540568645315,
-7.36840249209481));
#130941=CARTESIAN_POINT('Ctrl Pts',(-22.736900303818,0.0098381933498575,
-7.3713578778588));
#130942=CARTESIAN_POINT('Ctrl Pts',(-22.7728194553863,0.0382679569595985,
-7.37408651633313));
#130943=CARTESIAN_POINT('Ctrl Pts',(-22.8071364286681,0.0686316194067912,
-7.37684701091451));
#130944=CARTESIAN_POINT('Ctrl Pts',(-22.8396201836745,0.100731293851856,
-7.3796893756947));
#130945=CARTESIAN_POINT('Ctrl Pts',(-22.8423776955289,0.103456201510709,
-7.37993066105639));
#130946=CARTESIAN_POINT('Ctrl Pts',(-22.8451220276651,0.106193624252658,
-7.3801725363857));
#130947=CARTESIAN_POINT('Ctrl Pts',(-22.8478530557851,0.108943444354392,
-7.38041503227729));
#130948=CARTESIAN_POINT('Ctrl Pts',(-22.8531147285129,0.114241322222942,
-7.38088223142842));
#130949=CARTESIAN_POINT('Ctrl Pts',(-22.8583269358697,0.119585102091055,
-7.38135173993085));
#130950=CARTESIAN_POINT('Ctrl Pts',(-22.863488735766,0.124973820686968,
-7.38182377860623));
#130951=CARTESIAN_POINT('Ctrl Pts',(-22.8635004657162,0.124986066299377,
-7.38182485129217));
#130952=CARTESIAN_POINT('Ctrl Pts',(-22.8635121954061,0.124998312143855,
-7.38182592399117));
#130953=CARTESIAN_POINT('Ctrl Pts',(-22.8635239248358,0.125010558220377,
-7.38182699670324));
#130954=CARTESIAN_POINT('Ctrl Pts',(-22.8949165401771,0.157785925944268,
-7.38469800053578));
#130955=CARTESIAN_POINT('Ctrl Pts',(-22.9245616292306,0.192357156123483,
-7.38767052255618));
#130956=CARTESIAN_POINT('Ctrl Pts',(-22.9522727798873,0.228494562091567,
-7.39068702879009));
#130957=CARTESIAN_POINT('Ctrl Pts',(-22.954373707634,0.231234328470557,
-7.39091572595693));
#130958=CARTESIAN_POINT('Ctrl Pts',(-22.956463517418,0.233983072408943,
-7.3911446759429));
#130959=CARTESIAN_POINT('Ctrl Pts',(-22.9585421274439,0.23674068165377,
-7.39137385367572));
#130960=CARTESIAN_POINT('Ctrl Pts',(-22.9879960567569,0.275816038146746,
-7.39462130493333));
#130961=CARTESIAN_POINT('Ctrl Pts',(-23.0152020207889,0.316676836926239,
-7.39791390493542));
#130962=CARTESIAN_POINT('Ctrl Pts',(-23.0399707714754,0.359018681242872,
-7.40119395866403));
#130963=CARTESIAN_POINT('Ctrl Pts',(-23.0647157848571,0.401319946957919,
-7.40447086893029));
#130964=CARTESIAN_POINT('Ctrl Pts',(-23.0870285259997,0.445099283089772,
-7.40773496054836));
#130965=CARTESIAN_POINT('Ctrl Pts',(-23.1067566936188,0.49003959928208,
-7.4109488033226));
#130966=CARTESIAN_POINT('Ctrl Pts',(-23.1264821046171,0.534973635955073,
-7.41416219702595));
#130967=CARTESIAN_POINT('Ctrl Pts',(-23.1436237351315,0.581068267085949,
-7.4173252525692));
#130968=CARTESIAN_POINT('Ctrl Pts',(-23.1580632312311,0.627994354630757,
-7.42042358804598));
#130969=CARTESIAN_POINT('Ctrl Pts',(-23.1725011666005,0.674915370048347,
-7.42352158863119));
#130970=CARTESIAN_POINT('Ctrl Pts',(-23.1842374649771,0.722667611815115,
-7.42655492468563));
#130971=CARTESIAN_POINT('Ctrl Pts',(-23.1931878410699,0.770910674421012,
-7.42953268626117));
#130972=CARTESIAN_POINT('Ctrl Pts',(-23.2021471186336,0.81920171648744,
-7.43251340932768));
#130973=CARTESIAN_POINT('Ctrl Pts',(-23.208314693299,0.86798449478743,-7.43543862806872));
#130974=CARTESIAN_POINT('Ctrl Pts',(-23.2116425566531,0.916907003400649,
-7.43833933475804));
#130975=CARTESIAN_POINT('Ctrl Pts',(-23.2135475958525,0.944912749646556,
-7.43999984763397));
#130976=CARTESIAN_POINT('Ctrl Pts',(-23.2145227439249,0.972964093664828,
-7.44165272227882));
#130977=CARTESIAN_POINT('Ctrl Pts',(-23.2145649522472,1.00099359438948,
-7.44330650982799));
#130978=CARTESIAN_POINT('Ctrl Pts',(-23.214564952248,1.00099359495523,-7.44330650986139));
#130979=CARTESIAN_POINT('Ctrl Pts',(-23.2146393694028,1.05041219770429,
-7.44622229030034));
#130980=CARTESIAN_POINT('Ctrl Pts',(-23.2118128350904,1.09973542603955,
-7.44913831688056));
#130981=CARTESIAN_POINT('Ctrl Pts',(-23.2061009251658,1.14865878337265,
-7.45211749203754));
#130982=CARTESIAN_POINT('Ctrl Pts',(-23.2040398687697,1.16631203769178,
-7.4531924823811));
#130983=CARTESIAN_POINT('Ctrl Pts',(-23.2016030199901,1.18391370803345,
-7.4542756947842));
#130984=CARTESIAN_POINT('Ctrl Pts',(-23.1987905854071,1.20145107483144,
-7.45537008448875));
#130985=CARTESIAN_POINT('Ctrl Pts',(-23.19572307147,1.22057902802819,-7.45656373204649));
#130986=CARTESIAN_POINT('Ctrl Pts',(-23.1922094223436,1.23962911438569,
-7.45777087145966));
#130987=CARTESIAN_POINT('Ctrl Pts',(-23.1882513857817,1.25858259771115,
-7.45899564334432));
#130988=CARTESIAN_POINT('Ctrl Pts',(-23.1882479227424,1.25859918084688,
-7.45899671494462));
#130989=CARTESIAN_POINT('Ctrl Pts',(-23.1882444593629,1.25861576390876,
-7.45899778655841));
#130990=CARTESIAN_POINT('Ctrl Pts',(-23.1882409956433,1.25863234689677,
-7.45899885818571));
#130991=CARTESIAN_POINT('Ctrl Pts',(-23.178858317585,1.30355308333993,-7.46190172993643));
#130992=CARTESIAN_POINT('Ctrl Pts',(-23.1669541409773,1.34802527177939,
-7.46490770785243));
#130993=CARTESIAN_POINT('Ctrl Pts',(-23.1526174063115,1.3917624131088,-7.46795770494442));
#130994=CARTESIAN_POINT('Ctrl Pts',(-23.1510731139209,1.39647359289396,
-7.46828623772474));
#130995=CARTESIAN_POINT('Ctrl Pts',(-23.1495006350576,1.40117621164047,
-7.46861528124578));
#130996=CARTESIAN_POINT('Ctrl Pts',(-23.1479001088029,1.4058698886138,-7.46894476166106));
#130997=CARTESIAN_POINT('Ctrl Pts',(-23.1318984622988,1.45279605399784,
-7.47223882142405));
#130998=CARTESIAN_POINT('Ctrl Pts',(-23.1130894263544,1.49883274547285,
-7.4755759996429));
#130999=CARTESIAN_POINT('Ctrl Pts',(-23.0916240611239,1.54364618065664,
-7.47889751215052));
#131000=CARTESIAN_POINT('Ctrl Pts',(-23.0701787308529,1.58841778867625,
-7.48221592448409));
#131001=CARTESIAN_POINT('Ctrl Pts',(-23.0460822749542,1.63196861918501,
-7.48551840643433));
#131002=CARTESIAN_POINT('Ctrl Pts',(-23.0195160219019,1.67398824230252,
-7.48876774034043));
#131003=CARTESIAN_POINT('Ctrl Pts',(-22.9929634873123,1.7159861670407,-7.49201539633335));
#131004=CARTESIAN_POINT('Ctrl Pts',(-22.9639437641233,1.75645452377927,
-7.49520986386834));
#131005=CARTESIAN_POINT('Ctrl Pts',(-22.9326663926893,1.79510384012078,
-7.49833821419827));
#131006=CARTESIAN_POINT('Ctrl Pts',(-22.8997571778103,1.83576961854437,
-7.50162978086466));
#131007=CARTESIAN_POINT('Ctrl Pts',(-22.8643482441511,1.8744212906144,-7.5048479713041));
#131008=CARTESIAN_POINT('Ctrl Pts',(-22.8267177637578,1.91074639753886,
-7.50800705489195));
#131009=CARTESIAN_POINT('Ctrl Pts',(-22.7909220328329,1.94530040109382,
-7.51101211102989));
#131010=CARTESIAN_POINT('Ctrl Pts',(-22.7531162199469,1.97774913637893,
-7.51396410504403));
#131011=CARTESIAN_POINT('Ctrl Pts',(-22.7135706565953,2.0078473789134,-7.51689857384268));
#131012=CARTESIAN_POINT('Ctrl Pts',(-22.6740012133173,2.03796379652875,
-7.51983481464538));
#131013=CARTESIAN_POINT('Ctrl Pts',(-22.632689723638,2.06572644802876,-7.52275392175664));
#131014=CARTESIAN_POINT('Ctrl Pts',(-22.589939769477,2.09091779020453,-7.52570956219129));
#131015=CARTESIAN_POINT('Ctrl Pts',(-22.5504634189498,2.11418009009463,
-7.52843887266941));
#131016=CARTESIAN_POINT('Ctrl Pts',(-22.509759964922,2.13524983913903,-7.53119992281915));
#131017=CARTESIAN_POINT('Ctrl Pts',(-22.4680974026757,2.15398274420328,
-7.53404272752769));
#131018=CARTESIAN_POINT('Ctrl Pts',(-22.4645681084673,2.15556963492209,
-7.53428354551037));
#131019=CARTESIAN_POINT('Ctrl Pts',(-22.4610319158699,2.15713978306097,
-7.53452495016558));
#131020=CARTESIAN_POINT('Ctrl Pts',(-22.4574889786075,2.15869311549852,
-7.53476697189692));
#131021=CARTESIAN_POINT('Ctrl Pts',(-22.4506735258064,2.16168121918994,
-7.53523254257023));
#131022=CARTESIAN_POINT('Ctrl Pts',(-22.4438332508344,2.16460706131475,
-7.53570040262063));
#131023=CARTESIAN_POINT('Ctrl Pts',(-22.4369693789612,2.16747011554173,
-7.5361707705175));
#131024=CARTESIAN_POINT('Ctrl Pts',(-22.4369538236924,2.16747660394636,
-7.53617183649006));
#131025=CARTESIAN_POINT('Ctrl Pts',(-22.4369382683024,2.16748309202853,
-7.5361729024755));
#131026=CARTESIAN_POINT('Ctrl Pts',(-22.4369227127913,2.16748957978826,
-7.53617396847382));
#131027=CARTESIAN_POINT('Ctrl Pts',(-22.39454825699,2.18516275586588,-7.53907783310896));
#131028=CARTESIAN_POINT('Ctrl Pts',(-22.3511170053128,2.20050050116548,
-7.54208464648229));
#131029=CARTESIAN_POINT('Ctrl Pts',(-22.3069159212396,2.21341408117809,
-7.5451352773389));
#131030=CARTESIAN_POINT('Ctrl Pts',(-22.3021767343903,2.21479865963033,
-7.54546236229486));
#131031=CARTESIAN_POINT('Ctrl Pts',(-22.2974287453871,2.21615538274289,
-7.5457899509709));
#131032=CARTESIAN_POINT('Ctrl Pts',(-22.2926723419464,2.21748415115904,
-7.54611797048339));
#131033=CARTESIAN_POINT('Ctrl Pts',(-22.2449183024701,2.23082491591788,
-7.54941126907427));
#131034=CARTESIAN_POINT('Ctrl Pts',(-22.1963103279221,2.24134704271031,
-7.55274744660515));
#131035=CARTESIAN_POINT('Ctrl Pts',(-22.1472091448079,2.24898636163867,
-7.55606780468917));
#131036=CARTESIAN_POINT('Ctrl Pts',(-22.0981536426899,2.2566185733717,-7.55938507369762));
#131037=CARTESIAN_POINT('Ctrl Pts',(-22.0486058268957,2.26137365277867,
-7.56268625982269));
#131038=CARTESIAN_POINT('Ctrl Pts',(-21.9989242977315,2.26322557817672,
-7.56593426134831));
#131039=CARTESIAN_POINT('Ctrl Pts',(-21.9492682801424,2.26507655260697,
-7.56918059501796));
#131040=CARTESIAN_POINT('Ctrl Pts',(-21.8994786712579,2.26402743422841,
-7.57237370416246));
#131041=CARTESIAN_POINT('Ctrl Pts',(-21.8499127601215,2.26008731348708,
-7.57550079317662));
#131042=CARTESIAN_POINT('Ctrl Pts',(-21.7977645584286,2.25594191988083,
-7.57879079763499));
#131043=CARTESIAN_POINT('Ctrl Pts',(-21.7458640239365,2.24859598694143,
-7.58200754494334));
#131044=CARTESIAN_POINT('Ctrl Pts',(-21.6946261564365,2.2381021989578,-7.58516546343385));
#131045=CARTESIAN_POINT('Ctrl Pts',(-21.6458826984808,2.22811927932562,
-7.58816964519785));
#131046=CARTESIAN_POINT('Ctrl Pts',(-21.5977390586478,2.2152876048066,-7.5911210087776));
#131047=CARTESIAN_POINT('Ctrl Pts',(-21.550550456418,2.19969145104377,-7.59405522457834));
#131048=CARTESIAN_POINT('Ctrl Pts',(-21.5033332598102,2.18408584664461,
-7.5969912183948));
#131049=CARTESIAN_POINT('Ctrl Pts',(-21.4570725070522,2.16571200475415,
-7.59991045784023));
#131050=CARTESIAN_POINT('Ctrl Pts',(-21.4121194101045,2.1446973198645,-7.60286672036657));
#131051=CARTESIAN_POINT('Ctrl Pts',(-21.3706341752131,2.12530379198745,
-7.60559492495387));
#131052=CARTESIAN_POINT('Ctrl Pts',(-21.3302623001994,2.10366075919581,
-7.60835524906842));
#131053=CARTESIAN_POINT('Ctrl Pts',(-21.2912739573576,2.07990746880294,
-7.61119766217468));
#131054=CARTESIAN_POINT('Ctrl Pts',(-21.2879450475958,2.07787936105329,
-7.61144035360619));
#131055=CARTESIAN_POINT('Ctrl Pts',(-21.2846261925295,2.0758358713926,-7.61168364347605));
#131056=CARTESIAN_POINT('Ctrl Pts',(-21.2813175426721,2.07377708720797,
-7.61192756288755));
#131057=CARTESIAN_POINT('Ctrl Pts',(-21.2750097212594,2.06985208954314,
-7.61239258643285));
#131058=CARTESIAN_POINT('Ctrl Pts',(-21.2687390975643,2.06587159496297,
-7.61285990383907));
#131059=CARTESIAN_POINT('Ctrl Pts',(-21.2625067931607,2.06183631316588,
-7.61332973251004));
#131060=CARTESIAN_POINT('Ctrl Pts',(-21.2624924207027,2.06182700731134,
-7.61333081599256));
#131061=CARTESIAN_POINT('Ctrl Pts',(-21.2624780484484,2.06181770116543,
-7.61333189948843));
#131062=CARTESIAN_POINT('Ctrl Pts',(-21.262463676398,2.06180839472818,-7.61333298299766));
#131063=CARTESIAN_POINT('Ctrl Pts',(-21.2239835549963,2.03689108484768,
-7.61623400026946));
#131064=CARTESIAN_POINT('Ctrl Pts',(-21.1868270745706,2.00978717511707,
-7.6192381826602));
#131065=CARTESIAN_POINT('Ctrl Pts',(-21.1512291127379,1.98068235067877,
-7.62228642094879));
#131066=CARTESIAN_POINT('Ctrl Pts',(-21.1473532623951,1.9775134629681,-7.62261830836052));
#131067=CARTESIAN_POINT('Ctrl Pts',(-21.1434959046142,1.97432090331687,
-7.62295071803349));
#131068=CARTESIAN_POINT('Ctrl Pts',(-21.139657354002,1.97110494676656,-7.62328357367537));
#131069=CARTESIAN_POINT('Ctrl Pts',(-21.1016922462611,1.93929759309203,
-7.62657567571661));
#131070=CARTESIAN_POINT('Ctrl Pts',(-21.0655642803586,1.90519630825761,
-7.62991085463807));
#131071=CARTESIAN_POINT('Ctrl Pts',(-21.0315299705495,1.86906168717004,
-7.63323029595846));
#131072=CARTESIAN_POINT('Ctrl Pts',(-20.9975273948489,1.83296075855307,
-7.63654664218125));
#131073=CARTESIAN_POINT('Ctrl Pts',(-20.9656143026336,1.79483044489107,
-7.63984698647441));
#131074=CARTESIAN_POINT('Ctrl Pts',(-20.9360145328724,1.75495119320424,
-7.6430940527343));
#131075=CARTESIAN_POINT('Ctrl Pts',(-20.9064299391394,1.71509238791451,
-7.64633945419851));
#131076=CARTESIAN_POINT('Ctrl Pts',(-20.8791562220223,1.67348647321077,
-7.64953153657534));
#131077=CARTESIAN_POINT('Ctrl Pts',(-20.8543874954893,1.63043266892735,
-7.65265728570438));
#131078=CARTESIAN_POINT('Ctrl Pts',(-20.8296210733621,1.58738287023691,
-7.65578274402337));
#131079=CARTESIAN_POINT('Ctrl Pts',(-20.807359269724,1.54288543394258,-7.65884193058603));
#131080=CARTESIAN_POINT('Ctrl Pts',(-20.7877665861249,1.49725860380221,
-7.661846368462));
#131081=CARTESIAN_POINT('Ctrl Pts',(-20.7681549102342,1.4515875450057,-7.6648537187088));
#131082=CARTESIAN_POINT('Ctrl Pts',(-20.7512177926814,1.40478485484132,
-7.66780640875322));
#131083=CARTESIAN_POINT('Ctrl Pts',(-20.7370879415237,1.35718935752958,
-7.6707387833695));
#131084=CARTESIAN_POINT('Ctrl Pts',(-20.7229496925521,1.30956557272042,
-7.67367290078801));
#131085=CARTESIAN_POINT('Ctrl Pts',(-20.7116225068754,1.26114801133181,
-7.67658707574696));
#131086=CARTESIAN_POINT('Ctrl Pts',(-20.703201683773,1.21229639639102,-7.67953414160623));
#131087=CARTESIAN_POINT('Ctrl Pts',(-20.6953790276158,1.16691491981061,
-7.6822718648204));
#131088=CARTESIAN_POINT('Ctrl Pts',(-20.6900646801056,1.1211584099592,-7.68503854900198));
#131089=CARTESIAN_POINT('Ctrl Pts',(-20.687299148992,1.0753326793911,-7.68788495294579));
#131090=CARTESIAN_POINT('Ctrl Pts',(-20.6870826550185,1.07174530535956,
-7.68810777788419));
#131091=CARTESIAN_POINT('Ctrl Pts',(-20.6868817645872,1.06815748613482,
-7.68833109136304));
#131092=CARTESIAN_POINT('Ctrl Pts',(-20.6866964891666,1.06456935749218,
-7.68855491773312));
#131093=CARTESIAN_POINT('Ctrl Pts',(-20.6861601106909,1.05418160629602,
-7.6892029024837));
#131094=CARTESIAN_POINT('Ctrl Pts',(-20.6857545740246,1.043791532,-7.68985520057486));
#131095=CARTESIAN_POINT('Ctrl Pts',(-20.6854800248292,1.03340277176877,
-7.69051241219103));
#131096=CARTESIAN_POINT('Ctrl Pts',(-20.6854795792906,1.03338591287967,
-7.69051347871461));
#131097=CARTESIAN_POINT('Ctrl Pts',(-20.6854791340968,1.03336905399399,
-7.69051454525113));
#131098=CARTESIAN_POINT('Ctrl Pts',(-20.685478689248,1.03335219511177,-7.69051561180059));
#131099=CARTESIAN_POINT('Ctrl Pts',(-20.68426768411,0.987457518912684,-7.6934190630238));
#131100=CARTESIAN_POINT('Ctrl Pts',(-20.6856160866493,0.941419909381913,
-7.69642583461519));
#131101=CARTESIAN_POINT('Ctrl Pts',(-20.6895030751693,0.895538674509048,
-7.69947695126876));
#131102=CARTESIAN_POINT('Ctrl Pts',(-20.6899194512904,0.890623854074188,
-7.69980378838462));
#131103=CARTESIAN_POINT('Ctrl Pts',(-20.6903649281569,0.885710867824233,
-7.70013113435119));
#131104=CARTESIAN_POINT('Ctrl Pts',(-20.6908394585241,0.880800111615071,
-7.70045891667684));
#131105=CARTESIAN_POINT('Ctrl Pts',(-20.6956140374226,0.831389589990802,
-7.70375696182499));
#131106=CARTESIAN_POINT('Ctrl Pts',(-20.7033327684018,0.782199754485548,
-7.70709862514005));
#131107=CARTESIAN_POINT('Ctrl Pts',(-20.7139251171565,0.733591049100032,
-7.71042500202741));
#131108=CARTESIAN_POINT('Ctrl Pts',(-20.7245075061223,0.685028049577832,
-7.71374825118433));
#131109=CARTESIAN_POINT('Ctrl Pts',(-20.7379578231943,0.63704495025831,
-7.71705594647716));
#131110=CARTESIAN_POINT('Ctrl Pts',(-20.7541707021653,0.589986349436577,
-7.72031073035324));
#131111=CARTESIAN_POINT('Ctrl Pts',(-20.7703750410767,0.542952536516657,
-7.72356379978687));
#131112=CARTESIAN_POINT('Ctrl Pts',(-20.789338961905,0.496842201669888,
-7.7267639173308));
#131113=CARTESIAN_POINT('Ctrl Pts',(-20.8109248380533,0.451986005087727,
-7.72989801760503));
#131114=CARTESIAN_POINT('Ctrl Pts',(-20.8335840862821,0.404899304229897,
-7.73318796310456));
#131115=CARTESIAN_POINT('Ctrl Pts',(-20.8591329218472,0.359194773336397,
-7.73640499458669));
#131116=CARTESIAN_POINT('Ctrl Pts',(-20.8873736002875,0.315238832915532,
-7.73956310094918));
#131117=CARTESIAN_POINT('Ctrl Pts',(-20.9142987152029,0.273330535650482,
-7.74257409011167));
#131118=CARTESIAN_POINT('Ctrl Pts',(-20.9436706362759,0.233011785794678,
-7.7455319278408));
#131119=CARTESIAN_POINT('Ctrl Pts',(-20.9752824841326,0.194584241866766,
-7.7484719707215));
#131120=CARTESIAN_POINT('Ctrl Pts',(-21.006912832425,0.156134208702855,
-7.75141373422526));
#131121=CARTESIAN_POINT('Ctrl Pts',(-21.0407860208494,0.119577973306089,
-7.75433809542381));
#131122=CARTESIAN_POINT('Ctrl Pts',(-21.0766564070754,0.0851979572082941,
-7.75729853809533));
#131123=CARTESIAN_POINT('Ctrl Pts',(-21.1097881797831,0.0534427686284415,
-7.76003295843553));
#131124=CARTESIAN_POINT('Ctrl Pts',(-21.1446243140553,0.0235440379982971,
-7.76279874938703));
#131125=CARTESIAN_POINT('Ctrl Pts',(-21.1809367785472,-0.00429528527658141,
-7.76564580898741));
#131126=CARTESIAN_POINT('Ctrl Pts',(-21.1840016610854,-0.0066450089038303,
-7.76588610948412));
#131127=CARTESIAN_POINT('Ctrl Pts',(-21.1870770699707,-0.0089800909533138,
-7.76612698892844));
#131128=CARTESIAN_POINT('Ctrl Pts',(-21.1901628736014,-0.0113004255346918,
-7.76636847732289));
#131129=CARTESIAN_POINT('Ctrl Pts',(-21.195838300467,-0.0155679975503176,
-7.76681262409486));
#131130=CARTESIAN_POINT('Ctrl Pts',(-21.201548775814,-0.0197856245643231,
-7.76725883603628));
#131131=CARTESIAN_POINT('Ctrl Pts',(-21.2072933722109,-0.0239526163666588,
-7.76770730157324));
#131132=CARTESIAN_POINT('Ctrl Pts',(-21.2073066081804,-0.0239622174199971,
-7.76770833487058));
#131133=CARTESIAN_POINT('Ctrl Pts',(-21.2073198443311,-0.0239718182045455,
-7.76770936817989));
#131134=CARTESIAN_POINT('Ctrl Pts',(-21.2073330806628,-0.0239814187202979,
-7.76771040150115));
#131135=CARTESIAN_POINT('Ctrl Pts',(-21.2445607881007,-0.0509832495781172,
-7.77061665850255));
#131136=CARTESIAN_POINT('Ctrl Pts',(-21.2833587804813,-0.0759491526982826,
-7.77362476915587));
#131137=CARTESIAN_POINT('Ctrl Pts',(-21.3234665167027,-0.098725861531078,
-7.77667545105122));
#131138=CARTESIAN_POINT('Ctrl Pts',(-21.3265580603532,-0.100481512590064,
-7.77691060060419));
#131139=CARTESIAN_POINT('Ctrl Pts',(-21.3296573601806,-0.102224157158229,
-7.77714600309324));
#131140=CARTESIAN_POINT('Ctrl Pts',(-21.3327642840652,-0.103953725668209,
-7.77738163136852));
#131141=CARTESIAN_POINT('Ctrl Pts',(-21.376109675984,-0.128083323849993,
-7.78066893428247));
#131142=CARTESIAN_POINT('Ctrl Pts',(-21.4209445151194,-0.149668228400233,
-7.7839995919757));
#131143=CARTESIAN_POINT('Ctrl Pts',(-21.4669324790524,-0.168561791557893,
-7.78731487504472));
#131144=CARTESIAN_POINT('Ctrl Pts',(-21.4809893493312,-0.17433687581252,
-7.78832823810872));
#131145=CARTESIAN_POINT('Ctrl Pts',(-21.4951538992482,-0.179860785953845,
-7.78934030157835));
#131146=CARTESIAN_POINT('Ctrl Pts',(-21.5094163772775,-0.18513004675685,
-7.79034977406521));
#131147=CARTESIAN_POINT('Ctrl Pts',(-21.5093868137067,-0.185251134376157,
-7.65234634179685));
#131148=CARTESIAN_POINT('Ctrl Pts',(-21.5093128480698,-0.185223637894142,
-7.65234156526446));
#131149=CARTESIAN_POINT('Ctrl Pts',(-21.509238884932,-0.185196134460566,
-7.65233678892048));
#131150=CARTESIAN_POINT('Ctrl Pts',(-21.4510434928494,-0.163549787454182,
-7.64857870542183));
#131151=CARTESIAN_POINT('Ctrl Pts',(-21.3945883018176,-0.137683887915379,
-7.64495533318918));
#131152=CARTESIAN_POINT('Ctrl Pts',(-21.2863501577122,-0.0781071893864338,
-7.63781023021484));
#131153=CARTESIAN_POINT('Ctrl Pts',(-21.2346855626873,-0.0445433913468252,
-7.63429654681614));
#131154=CARTESIAN_POINT('Ctrl Pts',(-21.1579041077945,0.0137144298681591,
-7.62862794366726));
#131155=CARTESIAN_POINT('Ctrl Pts',(-21.1310219340692,0.0359203108878381,
-7.62654580317381));
#131156=CARTESIAN_POINT('Ctrl Pts',(-21.0923432432901,0.0706567948773928,
-7.62334378722566));
#131157=CARTESIAN_POINT('Ctrl Pts',(-21.0798274758663,0.0823651831614658,
-7.62227282675557));
#131158=CARTESIAN_POINT('Ctrl Pts',(-21.053424423381,0.108091031660806,
-7.61992833542388));
#131159=CARTESIAN_POINT('Ctrl Pts',(-21.0396202195877,0.12218571245985,
-7.61865021649861));
#131160=CARTESIAN_POINT('Ctrl Pts',(-20.9935903068346,0.171438038912264,
-7.61422250868857));
#131161=CARTESIAN_POINT('Ctrl Pts',(-20.9630278008428,0.20809116472436,
-7.61099322679332));
#131162=CARTESIAN_POINT('Ctrl Pts',(-20.8949084606398,0.29987162568279,
-7.60320127747352));
#131163=CARTESIAN_POINT('Ctrl Pts',(-20.8594929686099,0.356421459397041,
-7.59863436844913));
#131164=CARTESIAN_POINT('Ctrl Pts',(-20.8132087185071,0.445213092888341,
-7.59193440148952));
#131165=CARTESIAN_POINT('Ctrl Pts',(-20.7989066664431,0.475531357136871,
-7.58972102651659));
#131166=CARTESIAN_POINT('Ctrl Pts',(-20.7737610005966,0.53483648235841,
-7.58553587033554));
#131167=CARTESIAN_POINT('Ctrl Pts',(-20.7627434091212,0.563723338294082,
-7.5835600388979));
#131168=CARTESIAN_POINT('Ctrl Pts',(-20.7434424683484,0.620495943478359,
-7.57979047079808));
#131169=CARTESIAN_POINT('Ctrl Pts',(-20.7350406710656,0.648320546348082,
-7.57799402259526));
#131170=CARTESIAN_POINT('Ctrl Pts',(-20.71487682135,0.724492028471393,-7.57319542971564));
#131171=CARTESIAN_POINT('Ctrl Pts',(-20.704996179733,0.773284073757678,
-7.57025088306412));
#131172=CARTESIAN_POINT('Ctrl Pts',(-20.6874731010391,0.896906627558796,
-7.56296848958778));
#131173=CARTESIAN_POINT('Ctrl Pts',(-20.683579241259,0.972066347095177,
-7.55870572283618));
#131174=CARTESIAN_POINT('Ctrl Pts',(-20.687799559305,1.08523111887321,-7.55207258970493));
#131175=CARTESIAN_POINT('Ctrl Pts',(-20.6909435456879,1.12325029369719,
-7.54980526507213));
#131176=CARTESIAN_POINT('Ctrl Pts',(-20.6980259515646,1.17840015803419,
-7.54638822984118));
#131177=CARTESIAN_POINT('Ctrl Pts',(-20.7006111008889,1.19568590989837,
-7.54529854448084));
#131178=CARTESIAN_POINT('Ctrl Pts',(-20.70677304212,1.2317596251916,-7.54297547560186));
#131179=CARTESIAN_POINT('Ctrl Pts',(-20.7104193626123,1.25053051708427,
-7.5417393621425));
#131180=CARTESIAN_POINT('Ctrl Pts',(-20.7246473159491,1.31582812592224,
-7.53735964333183));
#131181=CARTESIAN_POINT('Ctrl Pts',(-20.7374346160178,1.36183015848023,
-7.5341327517182));
#131182=CARTESIAN_POINT('Ctrl Pts',(-20.7745565649186,1.47102742105603,
-7.52627390124519));
#131183=CARTESIAN_POINT('Ctrl Pts',(-20.8014278417162,1.53321397034375,
-7.52163491577533));
#131184=CARTESIAN_POINT('Ctrl Pts',(-20.8489477410753,1.62271968376971,
-7.51485171981006));
#131185=CARTESIAN_POINT('Ctrl Pts',(-20.8659348897925,1.65184278272168,
-7.51262475197985));
#131186=CARTESIAN_POINT('Ctrl Pts',(-20.9007519695144,1.70639986519932,
-7.50841839191507));
#131187=CARTESIAN_POINT('Ctrl Pts',(-20.9183947454039,1.73192421582375,
-7.50643478318591));
#131188=CARTESIAN_POINT('Ctrl Pts',(-20.9543374638286,1.78003810793221,
-7.50265830531034));
#131189=CARTESIAN_POINT('Ctrl Pts',(-20.9725123016609,1.80269629318323,
-7.50086245105653));
#131190=CARTESIAN_POINT('Ctrl Pts',(-21.0236277815069,1.86210702135917,
-7.49608800789188));
#131191=CARTESIAN_POINT('Ctrl Pts',(-21.0579659069959,1.89759115647615,
-7.49316564719757));
#131192=CARTESIAN_POINT('Ctrl Pts',(-21.1499307329358,1.9821202753915,-7.48587650808767));
#131193=CARTESIAN_POINT('Ctrl Pts',(-21.2100388991139,2.02816732924938,
-7.48158794822996));
#131194=CARTESIAN_POINT('Ctrl Pts',(-21.296982874725,2.08317828786665,-7.47556149025012));
#131195=CARTESIAN_POINT('Ctrl Pts',(-21.3205352869499,2.09703262517965,
-7.4739438021616));
#131196=CARTESIAN_POINT('Ctrl Pts',(-21.3635559169022,2.12049716782942,
-7.47098307056637));
#131197=CARTESIAN_POINT('Ctrl Pts',(-21.3828580838653,2.13038952792014,
-7.46965260643455));
#131198=CARTESIAN_POINT('Ctrl Pts',(-21.4173154645289,2.14694424479858,
-7.46725760019654));
#131199=CARTESIAN_POINT('Ctrl Pts',(-21.4323641988047,2.15381410324062,
-7.46620405613973));
#131200=CARTESIAN_POINT('Ctrl Pts',(-21.4741114699702,2.1718910349841,-7.46326462807476));
#131201=CARTESIAN_POINT('Ctrl Pts',(-21.5010656623271,2.18247883336374,
-7.46134987780624));
#131202=CARTESIAN_POINT('Ctrl Pts',(-21.6033286098363,2.21864803269781,
-7.45407955987269));
#131203=CARTESIAN_POINT('Ctrl Pts',(-21.6806335164803,2.23803312710359,
-7.44858492562844));
#131204=CARTESIAN_POINT('Ctrl Pts',(-21.798601560024,2.25603485389948,-7.440515329707));
#131205=CARTESIAN_POINT('Ctrl Pts',(-21.8382195982436,2.26017880398547,
-7.43785432010282));
#131206=CARTESIAN_POINT('Ctrl Pts',(-21.9121184193655,2.26439517210371,
-7.43299655949922));
#131207=CARTESIAN_POINT('Ctrl Pts',(-21.946334149411,2.2649573398176,-7.43078902702736));
#131208=CARTESIAN_POINT('Ctrl Pts',(-22.0087315120385,2.2634502239286,-7.42683450174997));
#131209=CARTESIAN_POINT('Ctrl Pts',(-22.0369006154249,2.26182579380693,
-7.42507566455904));
#131210=CARTESIAN_POINT('Ctrl Pts',(-22.1043473439633,2.25566666981565,
-7.42091574432761));
#131211=CARTESIAN_POINT('Ctrl Pts',(-22.1435132377278,2.25022995576206,
-7.41854266342653));
#131212=CARTESIAN_POINT('Ctrl Pts',(-22.2704368832692,2.22650256725899,
-7.41091220876748));
#131213=CARTESIAN_POINT('Ctrl Pts',(-22.3565077899392,2.20072452498635,
-7.40584924890605));
#131214=CARTESIAN_POINT('Ctrl Pts',(-22.465886440877,2.15484340357353,-7.3989214784988));
#131215=CARTESIAN_POINT('Ctrl Pts',(-22.4922466068292,2.14270317193148,
-7.39720917694569));
#131216=CARTESIAN_POINT('Ctrl Pts',(-22.5383232603339,2.11952900541771,
-7.39410139725384));
#131217=CARTESIAN_POINT('Ctrl Pts',(-22.558205766686,2.10885303674972,-7.39272060157604));
#131218=CARTESIAN_POINT('Ctrl Pts',(-22.5920355531881,2.08950443854627,
-7.39028359658388));
#131219=CARTESIAN_POINT('Ctrl Pts',(-22.6061183725347,2.08108193923269,
-7.38924083654891));
#131220=CARTESIAN_POINT('Ctrl Pts',(-22.6431720870343,2.05793060827983,
-7.38642314567974));
#131221=CARTESIAN_POINT('Ctrl Pts',(-22.6658355054383,2.04272911982829,
-7.3846237033285));
#131222=CARTESIAN_POINT('Ctrl Pts',(-22.7572247189644,1.97704583085346,
-7.37709999255782));
#131223=CARTESIAN_POINT('Ctrl Pts',(-22.8212506335037,1.92040917538642,
-7.37119834080684));
#131224=CARTESIAN_POINT('Ctrl Pts',(-22.9052763692649,1.82939589070396,
-7.36283540900043));
#131225=CARTESIAN_POINT('Ctrl Pts',(-22.9301513626988,1.79984635806805,
-7.36026001192446));
#131226=CARTESIAN_POINT('Ctrl Pts',(-22.9740680342113,1.74254496491024,
-7.35552955680058));
#131227=CARTESIAN_POINT('Ctrl Pts',(-22.9934301718599,1.71508193014595,
-7.35336510357126));
#131228=CARTESIAN_POINT('Ctrl Pts',(-23.0270378623879,1.66313602362411,
-7.34944986184622));
#131229=CARTESIAN_POINT('Ctrl Pts',(-23.0415986212628,1.63888385892045,
-7.34768880532691));
#131230=CARTESIAN_POINT('Ctrl Pts',(-23.0750806023269,1.57862486948262,
-7.34345998022255));
#131231=CARTESIAN_POINT('Ctrl Pts',(-23.0931022476479,1.54215386032964,
-7.34102321569987));
#131232=CARTESIAN_POINT('Ctrl Pts',(-23.1443560744998,1.42446052567096,
-7.33345141585946));
#131233=CARTESIAN_POINT('Ctrl Pts',(-23.1709128055311,1.34062394588982,
-7.328492951158));
#131234=CARTESIAN_POINT('Ctrl Pts',(-23.1943824618809,1.22650020510776,
-7.32168560447237));
#131235=CARTESIAN_POINT('Ctrl Pts',(-23.1992187795557,1.19809672397422,
-7.31998496927588));
#131236=CARTESIAN_POINT('Ctrl Pts',(-23.2060921657341,1.14729946626292,
-7.31689526533917));
#131237=CARTESIAN_POINT('Ctrl Pts',(-23.2085098817673,1.12496959265478,
-7.31552061435563));
#131238=CARTESIAN_POINT('Ctrl Pts',(-23.2116640666705,1.08621956374519,
-7.31308895189193));
#131239=CARTESIAN_POINT('Ctrl Pts',(-23.2126772837488,1.06982843393177,
-7.31204509285436));
#131240=CARTESIAN_POINT('Ctrl Pts',(-23.2145314387803,1.02598028471857,
-7.30921417255426));
#131241=CARTESIAN_POINT('Ctrl Pts',(-23.2147973285713,0.998509380542609,
-7.3074021279492));
#131242=CARTESIAN_POINT('Ctrl Pts',(-23.2123334479862,0.890904014894769,
-7.30020459773971));
#131243=CARTESIAN_POINT('Ctrl Pts',(-23.2028802398318,0.811111535271158,
-7.29466403780639));
#131244=CARTESIAN_POINT('Ctrl Pts',(-23.1738147555945,0.676693413761247,
-7.28535531233618));
#131245=CARTESIAN_POINT('Ctrl Pts',(-23.1578923622944,0.621519951837084,
-7.28153872289362));
#131246=CARTESIAN_POINT('Ctrl Pts',(-23.1281229394914,0.539708387752511,
-7.27591270783948));
#131247=CARTESIAN_POINT('Ctrl Pts',(-23.1169889697294,0.512169085648075,
-7.27402397704424));
#131248=CARTESIAN_POINT('Ctrl Pts',(-23.0926636182677,0.457614320444355,
-7.27028577726325));
#131249=CARTESIAN_POINT('Ctrl Pts',(-23.0794582857638,0.430626159808112,
-7.26843821782838));
#131250=CARTESIAN_POINT('Ctrl Pts',(-23.0153806046644,0.310690073313094,
-7.26020026219811));
#131251=CARTESIAN_POINT('Ctrl Pts',(-22.9539151000919,0.223894592919347,
-7.25420360320425));
#131252=CARTESIAN_POINT('Ctrl Pts',(-22.8491318254017,0.10952865726046,
-7.24520234435516));
#131253=CARTESIAN_POINT('Ctrl Pts',(-22.813837741004,0.0752510174626142,
-7.24231659755144));
#131254=CARTESIAN_POINT('Ctrl Pts',(-22.7627146329513,0.0310862001168211,
-7.2381843280834));
#131255=CARTESIAN_POINT('Ctrl Pts',(-22.7485269620261,0.0193606015539327,
-7.23704203663595));
#131256=CARTESIAN_POINT('Ctrl Pts',(-22.7199392281353,-0.00323435670909866,
-7.23473782211452));
#131257=CARTESIAN_POINT('Ctrl Pts',(-22.7055524116394,-0.0141134290087086,
-7.23357685387326));
#131258=CARTESIAN_POINT('Ctrl Pts',(-22.6612846585523,-0.0461231219848734,
-7.23001230202803));
#131259=CARTESIAN_POINT('Ctrl Pts',(-22.630715726351,-0.0662669117592296,
-7.22756153146986));
#131260=CARTESIAN_POINT('Ctrl Pts',(-22.5330388149527,-0.124718759276647,
-7.21985299147399));
#131261=CARTESIAN_POINT('Ctrl Pts',(-22.4632587741855,-0.158228408759995,
-7.21452800356339));
#131262=CARTESIAN_POINT('Ctrl Pts',(-22.3456686073162,-0.201969702661744,
-7.20610337869806));
#131263=CARTESIAN_POINT('Ctrl Pts',(-22.2995520214518,-0.216182172964166,
-7.20292312325515));
#131264=CARTESIAN_POINT('Ctrl Pts',(-22.2246434384929,-0.234653053251299,
-7.19795982609677));
#131265=CARTESIAN_POINT('Ctrl Pts',(-22.1963241977393,-0.240613468952686,
-7.19612777170259));
#131266=CARTESIAN_POINT('Ctrl Pts',(-22.1370813601368,-0.250973542719044,
-7.19237882547494));
#131267=CARTESIAN_POINT('Ctrl Pts',(-22.10614903939,-0.255209925563125,
-7.19046796589624));
#131268=CARTESIAN_POINT('Ctrl Pts',(-21.9765490294657,-0.268093689543489,
-7.18261589499013));
#131269=CARTESIAN_POINT('Ctrl Pts',(-21.8772009745272,-0.266281092757907,
-7.17699752398702));
#131270=CARTESIAN_POINT('Ctrl Pts',(-21.7439922827288,-0.248108567641219,
-7.1692039962486));
#131271=CARTESIAN_POINT('Ctrl Pts',(-21.7091247077903,-0.24185063319301,
-7.16713536098795));
#131272=CARTESIAN_POINT('Ctrl Pts',(-21.6495482977929,-0.228554502269538,
-7.16348626729058));
#131273=CARTESIAN_POINT('Ctrl Pts',(-21.6247062113893,-0.222211580319089,
-7.16192942345191));
#131274=CARTESIAN_POINT('Ctrl Pts',(-21.5843858365215,-0.210600311004532,
-7.15931959009562));
#131275=CARTESIAN_POINT('Ctrl Pts',(-21.5687871891666,-0.205779236362664,
-7.15828840693354));
#131276=CARTESIAN_POINT('Ctrl Pts',(-21.5385579660834,-0.195791061480555,
-7.15624577799516));
#131277=CARTESIAN_POINT('Ctrl Pts',(-21.5239226312969,-0.190654776703856,
-7.15523709376975));
#131278=CARTESIAN_POINT('Ctrl Pts',(-21.509386814352,-0.185251134616039,
-7.15421782883515));
#131279=CARTESIAN_POINT('Origin',(-21.9500000210213,0.999999999999992,-6.00000000000001));
#131280=CARTESIAN_POINT('',(-21.5093868153863,-0.18525113500052,-6.6522544014516));
#131281=CARTESIAN_POINT('',(-21.5094433440835,-0.185020348671028,-6.79053824099259));
#131282=CARTESIAN_POINT('',(-21.5093868137063,-0.185251134376008,-6.00000000000001));
#131283=CARTESIAN_POINT('',(-23.2143063419907,0.999065236394241,-6.94375433137471));
#131284=CARTESIAN_POINT('Ctrl Pts',(-21.5094433447348,-0.185020348911781,
-6.79053824103847));
#131285=CARTESIAN_POINT('Ctrl Pts',(-21.5560295243835,-0.202240840674773,
-6.79382015535907));
#131286=CARTESIAN_POINT('Ctrl Pts',(-21.603654065421,-0.216746349867037,
-6.79706007406326));
#131287=CARTESIAN_POINT('Ctrl Pts',(-21.6519736785055,-0.228436706932433,
-6.80023581525148));
#131288=CARTESIAN_POINT('Ctrl Pts',(-21.7002809854702,-0.240124086678163,
-6.80341074763663));
#131289=CARTESIAN_POINT('Ctrl Pts',(-21.7492830036594,-0.248997715194778,
-6.80652153338587));
#131290=CARTESIAN_POINT('Ctrl Pts',(-21.7986280584045,-0.254991264796082,
-6.80957069021685));
#131291=CARTESIAN_POINT('Ctrl Pts',(-21.8480147108248,-0.260989866934682,
-6.81262241747432));
#131292=CARTESIAN_POINT('Ctrl Pts',(-21.8977449542218,-0.264103330875337,
-6.81561254855112));
#131293=CARTESIAN_POINT('Ctrl Pts',(-21.9474577719668,-0.264300760927358,
-6.81856734041095));
#131294=CARTESIAN_POINT('Ctrl Pts',(-21.9971927366036,-0.264498278933798,
-6.82152344862055));
#131295=CARTESIAN_POINT('Ctrl Pts',(-22.0469101804872,-0.261776790501234,
-6.82444450254065));
#131296=CARTESIAN_POINT('Ctrl Pts',(-22.0962408692552,-0.256145263090496,
-6.82737719120075));
#131297=CARTESIAN_POINT('Ctrl Pts',(-22.1456589885209,-0.250503754727602,
-6.8303150775671));
#131298=CARTESIAN_POINT('Ctrl Pts',(-22.1946887394418,-0.241941306091203,
-6.83326520328801));
#131299=CARTESIAN_POINT('Ctrl Pts',(-22.2429534108828,-0.230514129940558,
-6.83628844575657));
#131300=CARTESIAN_POINT('Ctrl Pts',(-22.2708986835911,-0.223897788333286,
-6.83803890489625));
#131301=CARTESIAN_POINT('Ctrl Pts',(-22.29858737022,-0.216321987947828,
-6.83981410345112));
#131302=CARTESIAN_POINT('Ctrl Pts',(-22.3259462504358,-0.207806132960166,
-6.84162661025685));
#131303=CARTESIAN_POINT('Ctrl Pts',(-22.3259624236005,-0.207801098824114,
-6.84162768171777));
#131304=CARTESIAN_POINT('Ctrl Pts',(-22.3259785966501,-0.207796064359656,
-6.84162875319173));
#131305=CARTESIAN_POINT('Ctrl Pts',(-22.3259947695848,-0.207791029566808,
-6.84162982467873));
#131306=CARTESIAN_POINT('Ctrl Pts',(-22.3698112732581,-0.194150523147158,
-6.84453274953983));
#131307=CARTESIAN_POINT('Ctrl Pts',(-22.4129399665384,-0.178042987725401,
-6.8475387403743));
#131308=CARTESIAN_POINT('Ctrl Pts',(-22.4551041379781,-0.159584384076933,
-6.85058869343851));
#131309=CARTESIAN_POINT('Ctrl Pts',(-22.4596460256163,-0.157596039450061,
-6.85091723171274));
#131310=CARTESIAN_POINT('Ctrl Pts',(-22.4641766927377,-0.155580455081427,
-6.85124628009874));
#131311=CARTESIAN_POINT('Ctrl Pts',(-22.4686957735709,-0.153537805872149,
-6.8515757647222));
#131312=CARTESIAN_POINT('Ctrl Pts',(-22.5138689232656,-0.13311929557977,
-6.85486932347165));
#131313=CARTESIAN_POINT('Ctrl Pts',(-22.5578882557163,-0.10999210798179,
-6.85820592152001));
#131314=CARTESIAN_POINT('Ctrl Pts',(-22.6004360534522,-0.0843385029327583,
-6.86152679697928));
#131315=CARTESIAN_POINT('Ctrl Pts',(-22.6429441827154,-0.0587088154396544,
-6.86484457629575));
#131316=CARTESIAN_POINT('Ctrl Pts',(-22.6839837385748,-0.0305576463727556,
-6.86814636878));
#131317=CARTESIAN_POINT('Ctrl Pts',(-22.7232631349714,-9.51512544804245E-5,
-6.87139498460364));
#131318=CARTESIAN_POINT('Ctrl Pts',(-22.7625223016828,0.0303516550615235,
-6.87464192732429));
#131319=CARTESIAN_POINT('Ctrl Pts',(-22.8000231848581,0.0631073546523845,
-6.87783565303744));
#131320=CARTESIAN_POINT('Ctrl Pts',(-22.835497755303,0.0979357123471776,
-6.88096326252241));
#131321=CARTESIAN_POINT('Ctrl Pts',(-22.8728317763673,0.134589648490881,
-6.88425481015578));
#131322=CARTESIAN_POINT('Ctrl Pts',(-22.9079211560354,0.173539537848562,
-6.88747294771169));
#131323=CARTESIAN_POINT('Ctrl Pts',(-22.9404813706637,0.214478419093898,
-6.89063199209422));
#131324=CARTESIAN_POINT('Ctrl Pts',(-22.9714470610841,0.253412459832623,
-6.89363633317399));
#131325=CARTESIAN_POINT('Ctrl Pts',(-23.0001252022708,0.294145335391891,
-6.89658764971792));
#131326=CARTESIAN_POINT('Ctrl Pts',(-23.0262976368862,0.336384522477805,
-6.89952151269442));
#131327=CARTESIAN_POINT('Ctrl Pts',(-23.0524859312349,0.378649305281093,
-6.90245715350645));
#131328=CARTESIAN_POINT('Ctrl Pts',(-23.0761650308708,0.422422377383413,
-6.90537573239366));
#131329=CARTESIAN_POINT('Ctrl Pts',(-23.0971475208172,0.467380767602949,
-6.90833094800898));
#131330=CARTESIAN_POINT('Ctrl Pts',(-23.1165213823974,0.508892410463372,
-6.91105960120586));
#131331=CARTESIAN_POINT('Ctrl Pts',(-23.1335962467152,0.551415101151114,
-6.91382007620338));
#131332=CARTESIAN_POINT('Ctrl Pts',(-23.1482542287364,0.594668377259283,
-6.91666239450767));
#131333=CARTESIAN_POINT('Ctrl Pts',(-23.1494975356539,0.598337169956046,
-6.9169034832199));
#131334=CARTESIAN_POINT('Ctrl Pts',(-23.1507234790972,0.60201123727547,
-6.91714516076426));
#131335=CARTESIAN_POINT('Ctrl Pts',(-23.1519320008278,0.605690418647588,
-6.9173874576667));
#131336=CARTESIAN_POINT('Ctrl Pts',(-23.1542648310407,0.612792405518175,
-6.9178551675309));
#131337=CARTESIAN_POINT('Ctrl Pts',(-23.1565327240052,0.619913307396138,
-6.9183251911209));
#131338=CARTESIAN_POINT('Ctrl Pts',(-23.1587352677353,0.627051836558025,
-6.91879775004721));
#131339=CARTESIAN_POINT('Ctrl Pts',(-23.1587402617275,0.627068022279061,
-6.91879882151541));
#131340=CARTESIAN_POINT('Ctrl Pts',(-23.1587452553836,0.627084208090731,
-6.91879989299664));
#131341=CARTESIAN_POINT('Ctrl Pts',(-23.1587502487039,0.627100393993012,
-6.9188009644909));
#131342=CARTESIAN_POINT('Ctrl Pts',(-23.1730618829199,0.673491713118847,
-6.92187203408926));
#131343=CARTESIAN_POINT('Ctrl Pts',(-23.1846450412562,0.720746808245064,
-6.92505497657824));
#131344=CARTESIAN_POINT('Ctrl Pts',(-23.1934542128594,0.768570359867943,
-6.92828320901063));
#131345=CARTESIAN_POINT('Ctrl Pts',(-23.1953339441314,0.778775113455718,
-6.92897206032716));
#131346=CARTESIAN_POINT('Ctrl Pts',(-23.1970873498032,0.789005562115176,
-6.92966297380755));
#131347=CARTESIAN_POINT('Ctrl Pts',(-23.198713972783,0.799258529773055,
-6.93035530253995));
#131348=CARTESIAN_POINT('Ctrl Pts',(-23.2067014127284,0.849605146319679,
-6.93375494353926));
#131349=CARTESIAN_POINT('Ctrl Pts',(-23.2116327500809,0.900501157908817,
-6.93718796717115));
#131350=CARTESIAN_POINT('Ctrl Pts',(-23.2134794075178,0.951614527615504,
-6.94059891598172));
#131351=CARTESIAN_POINT('Ctrl Pts',(-23.2137476794667,0.95903998890203,
-6.94109443933478));
#131352=CARTESIAN_POINT('Ctrl Pts',(-23.2139508123716,0.966469956080461,
-6.94158949680679));
#131353=CARTESIAN_POINT('Ctrl Pts',(-23.2140886840524,0.973903326322752,
-6.94208391836729));
#131354=CARTESIAN_POINT('Ctrl Pts',(-23.2142441750389,0.982286643806755,
-6.94264152451061));
#131355=CARTESIAN_POINT('Ctrl Pts',(-23.2143167590587,0.990674437415963,
-6.94319838748987));
#131356=CARTESIAN_POINT('Ctrl Pts',(-23.2143063419907,0.999065236394238,
-6.94375433137472));
#131357=CARTESIAN_POINT('Ctrl Pts',(-23.2143063419899,0.999065237017194,
-6.94375433141597));
#131358=CARTESIAN_POINT('Ctrl Pts',(-23.2142449304963,1.04853129529665,
-6.94703177289403));
#131359=CARTESIAN_POINT('Ctrl Pts',(-23.2112979786896,1.09803111854625,
-6.95027178254654));
#131360=CARTESIAN_POINT('Ctrl Pts',(-23.2054908873639,1.1472102603586,-6.95344951713272));
#131361=CARTESIAN_POINT('Ctrl Pts',(-23.1996856242933,1.19637391902914,
-6.95662625126802));
#131362=CARTESIAN_POINT('Ctrl Pts',(-23.1910220147896,1.24521707334982,
-6.95974073011287));
#131363=CARTESIAN_POINT('Ctrl Pts',(-23.1795602753263,1.29338964514839,
-6.9627924293001));
#131364=CARTESIAN_POINT('Ctrl Pts',(-23.1680890707961,1.34160199769903,
-6.96584664857053));
#131365=CARTESIAN_POINT('Ctrl Pts',(-23.1538149580717,1.38914256170667,
-6.96883810142336));
#131366=CARTESIAN_POINT('Ctrl Pts',(-23.1368344520235,1.4356653418018,-6.97178988093841));
#131367=CARTESIAN_POINT('Ctrl Pts',(-23.119847002301,1.48220714600778,-6.97474286749614));
#131368=CARTESIAN_POINT('Ctrl Pts',(-23.1001506564016,1.52773013236868,
-6.97765643608188));
#131369=CARTESIAN_POINT('Ctrl Pts',(-23.0778815359588,1.57189502631101,
-6.98057434528757));
#131370=CARTESIAN_POINT('Ctrl Pts',(-23.0555709030587,1.61614224920202,
-6.98349769384511));
#131371=CARTESIAN_POINT('Ctrl Pts',(-23.0306774731456,1.65902590948432,
-6.98642591920524));
#131372=CARTESIAN_POINT('Ctrl Pts',(-23.0033831563308,1.70021640929234,
-6.98941774821354));
#131373=CARTESIAN_POINT('Ctrl Pts',(-22.9838335136706,1.72971923794742,
-6.99156065541322));
#131374=CARTESIAN_POINT('Ctrl Pts',(-22.9630530934144,1.75835361120176,
-6.99373656868135));
#131375=CARTESIAN_POINT('Ctrl Pts',(-22.941124785344,1.78600440442,-6.99596889953907));
#131376=CARTESIAN_POINT('Ctrl Pts',(-22.9411142602947,1.7860176761217,-6.99596997100306));
#131377=CARTESIAN_POINT('Ctrl Pts',(-22.9411037349809,1.78603094759722,
-6.99597104248005));
#131378=CARTESIAN_POINT('Ctrl Pts',(-22.9410932094026,1.78604421884654,
-6.99597211397003));
#131379=CARTESIAN_POINT('Ctrl Pts',(-22.912576857981,1.82199926106907,-6.99887504095237));
#131380=CARTESIAN_POINT('Ctrl Pts',(-22.8820072023488,1.85642353740065,
-7.0018810339252));
#131381=CARTESIAN_POINT('Ctrl Pts',(-22.8495921433793,1.88910073118473,
-7.00493098947793));
#131382=CARTESIAN_POINT('Ctrl Pts',(-22.8461004042992,1.89262070733762,
-7.00525952964829));
#131383=CARTESIAN_POINT('Ctrl Pts',(-22.8425873003403,1.89612039899188,
-7.00558857993955));
#131384=CARTESIAN_POINT('Ctrl Pts',(-22.8390531264866,1.89959952799682,
-7.0059180664767));
#131385=CARTESIAN_POINT('Ctrl Pts',(-22.803725316634,1.9343771063016,-7.00921163329467));
#131386=CARTESIAN_POINT('Ctrl Pts',(-22.766286751363,1.9671021311174,-7.01254823995152));
#131387=CARTESIAN_POINT('Ctrl Pts',(-22.7270219553802,1.99754393105081,
-7.01586912436756));
#131388=CARTESIAN_POINT('Ctrl Pts',(-22.6877937667188,2.02795734951106,
-7.01918691265946));
#131389=CARTESIAN_POINT('Ctrl Pts',(-22.646742884109,2.05609208436683,-7.02248871446112));
#131390=CARTESIAN_POINT('Ctrl Pts',(-22.6041704344222,2.08175189380834,
-7.02573733960189));
#131391=CARTESIAN_POINT('Ctrl Pts',(-22.5616199101788,2.10739848806722,
-7.02898429165251));
#131392=CARTESIAN_POINT('Ctrl Pts',(-22.5175494119718,2.1305727835755,-7.03217802669126));
#131393=CARTESIAN_POINT('Ctrl Pts',(-22.4722759027838,2.15110991198693,
-7.03530564507152));
#131394=CARTESIAN_POINT('Ctrl Pts',(-22.4246294094362,2.17272348181581,
-7.03859719571607));
#131395=CARTESIAN_POINT('Ctrl Pts',(-22.3756503149998,2.19141575935739,
-7.04181533609651));
#131396=CARTESIAN_POINT('Ctrl Pts',(-22.3257274976715,2.20703198304337,
-7.04497438246277));
#131397=CARTESIAN_POINT('Ctrl Pts',(-22.2782493866987,2.22188348463761,
-7.04797873121496));
#131398=CARTESIAN_POINT('Ctrl Pts',(-22.229917840384,2.23395283501891,-7.05093005445304));
#131399=CARTESIAN_POINT('Ctrl Pts',(-22.1810843510732,2.24314197341103,
-7.0538639226357));
#131400=CARTESIAN_POINT('Ctrl Pts',(-22.1322212702386,2.25233668012545,
-7.05679956864811));
#131401=CARTESIAN_POINT('Ctrl Pts',(-22.0828556587913,2.25864720832972,
-7.05971815124153));
#131402=CARTESIAN_POINT('Ctrl Pts',(-22.0333563299529,2.26201514749797,
-7.06267336862066));
#131403=CARTESIAN_POINT('Ctrl Pts',(-21.987651789829,2.26512488887148,-7.06540202887625));
#131404=CARTESIAN_POINT('Ctrl Pts',(-21.9418327785334,2.26572573150678,
-7.06816250939777));
#131405=CARTESIAN_POINT('Ctrl Pts',(-21.89620339875,2.26380880003273,-7.07100483175053));
#131406=CARTESIAN_POINT('Ctrl Pts',(-21.8923331613894,2.26364620786417,
-7.07124591462768));
#131407=CARTESIAN_POINT('Ctrl Pts',(-21.8884642621432,2.26346551897568,
-7.07148758629616));
#131408=CARTESIAN_POINT('Ctrl Pts',(-21.8845968717678,2.26326673691656,
-7.07172987727963));
#131409=CARTESIAN_POINT('Ctrl Pts',(-21.8771317025742,2.26288303070643,
-7.07219756815386));
#131410=CARTESIAN_POINT('Ctrl Pts',(-21.8696722944172,2.26243193962731,
-7.07266757251858));
#131411=CARTESIAN_POINT('Ctrl Pts',(-21.8622199967995,2.26191354350392,
-7.07314011195715));
#131412=CARTESIAN_POINT('Ctrl Pts',(-21.8622031005723,2.26191236816994,
-7.07314118332253));
#131413=CARTESIAN_POINT('Ctrl Pts',(-21.8621862043817,2.26191119248999,
-7.07314225470095));
#131414=CARTESIAN_POINT('Ctrl Pts',(-21.8621693082276,2.26191001646409,
-7.07314332609239));
#131415=CARTESIAN_POINT('Ctrl Pts',(-21.8163890542696,2.25872356562301,
-7.07604626911741));
#131416=CARTESIAN_POINT('Ctrl Pts',(-21.7707101713037,2.25297796441622,
-7.07905227638415));
#131417=CARTESIAN_POINT('Ctrl Pts',(-21.7254286398517,2.24472235522329,
-7.08210224404713));
#131418=CARTESIAN_POINT('Ctrl Pts',(-21.7205513644241,2.24383314325175,
-7.08243075617693));
#131419=CARTESIAN_POINT('Ctrl Pts',(-21.7156787362091,2.24291484448638,
-7.08275977831116));
#131420=CARTESIAN_POINT('Ctrl Pts',(-21.7108111513254,2.24196754490119,
-7.08308923659407));
#131421=CARTESIAN_POINT('Ctrl Pts',(-21.6621503478251,2.23249747708056,
-7.08638280109261));
#131422=CARTESIAN_POINT('Ctrl Pts',(-21.6139887726528,2.22012582692901,
-7.08971940313857));
#131423=CARTESIAN_POINT('Ctrl Pts',(-21.5666775724656,2.20495681385013,
-7.0930402816706));
#131424=CARTESIAN_POINT('Ctrl Pts',(-21.5194104800731,2.18980194270201,
-7.09635806417826));
#131425=CARTESIAN_POINT('Ctrl Pts',(-21.4729920172914,2.17185519352251,
-7.09965985893461));
#131426=CARTESIAN_POINT('Ctrl Pts',(-21.4277543235725,2.15125394795828,
-7.1029084772408));
#131427=CARTESIAN_POINT('Ctrl Pts',(-21.3825399271753,2.13066331199429,
-7.10615542251506));
#131428=CARTESIAN_POINT('Ctrl Pts',(-21.338505034419,2.1074209788545,-7.10934915099599));
#131429=CARTESIAN_POINT('Ctrl Pts',(-21.2959648649725,2.08169513258941,
-7.11247676481419));
#131430=CARTESIAN_POINT('Ctrl Pts',(-21.2511953191224,2.05462108777754,
-7.11576828555935));
#131431=CARTESIAN_POINT('Ctrl Pts',(-21.2080815227602,2.02479601831224,
-7.11898639941982));
#131432=CARTESIAN_POINT('Ctrl Pts',(-21.166971020738,1.99245313066713,-7.12214542445695));
#131433=CARTESIAN_POINT('Ctrl Pts',(-21.1278733914934,1.96169383151852,
-7.12514977574436));
#131434=CARTESIAN_POINT('Ctrl Pts',(-21.0905877461024,1.9286573436738,-7.12810110538412));
#131435=CARTESIAN_POINT('Ctrl Pts',(-21.055393731583,1.89357810922764,-7.1310349855263));
#131436=CARTESIAN_POINT('Ctrl Pts',(-21.0201783912629,1.85847761853181,
-7.13397064345211));
#131437=CARTESIAN_POINT('Ctrl Pts',(-20.987057620879,1.82133165357159,-7.13688924355075));
#131438=CARTESIAN_POINT('Ctrl Pts',(-20.9562881608786,1.78241136479329,
-7.13984448534541));
#131439=CARTESIAN_POINT('Ctrl Pts',(-20.9278778618936,1.74647517869324,
-7.14257314236305));
#131440=CARTESIAN_POINT('Ctrl Pts',(-20.9014720289848,1.70902582344569,
-7.14533362496862));
#131441=CARTESIAN_POINT('Ctrl Pts',(-20.8772499490538,1.67030908489392,
-7.14817595367336));
#131442=CARTESIAN_POINT('Ctrl Pts',(-20.8751952104047,1.66702477655643,
-7.14841706602456));
#131443=CARTESIAN_POINT('Ctrl Pts',(-20.8731561573652,1.66373133608191,
-7.14865876733914));
#131444=CARTESIAN_POINT('Ctrl Pts',(-20.8711328836023,1.66042890635819,
-7.14890108815111));
#131445=CARTESIAN_POINT('Ctrl Pts',(-20.8672284359895,1.65405598535886,
-7.14936871093808));
#131446=CARTESIAN_POINT('Ctrl Pts',(-20.863382803979,1.64764972012479,-7.14983864665092));
#131447=CARTESIAN_POINT('Ctrl Pts',(-20.8595966845555,1.64121126826339,
-7.15031111676707));
#131448=CARTESIAN_POINT('Ctrl Pts',(-20.859588097591,1.64119666577696,-7.15031218833499));
#131449=CARTESIAN_POINT('Ctrl Pts',(-20.8595795109326,1.64118206312495,
-7.15031325991594));
#131450=CARTESIAN_POINT('Ctrl Pts',(-20.8595709245804,1.6411674603074,-7.15031433150994));
#131451=CARTESIAN_POINT('Ctrl Pts',(-20.8363107889786,1.60160892540201,
-7.15321724310814));
#131452=CARTESIAN_POINT('Ctrl Pts',(-20.8152185566105,1.5606868361378,-7.15622322004602));
#131453=CARTESIAN_POINT('Ctrl Pts',(-20.7964210724615,1.5186730818474,-7.15927315818181));
#131454=CARTESIAN_POINT('Ctrl Pts',(-20.7943960233729,1.51414694876722,
-7.15960172738783));
#131455=CARTESIAN_POINT('Ctrl Pts',(-20.7923976004164,1.50960819559947,
-7.15993080679469));
#131456=CARTESIAN_POINT('Ctrl Pts',(-20.7904259567716,1.50505719785523,
-7.16026032250563));
#131457=CARTESIAN_POINT('Ctrl Pts',(-20.7707192361575,1.45956964674653,
-7.16355385583285));
#131458=CARTESIAN_POINT('Ctrl Pts',(-20.7536878133768,1.41285302912484,
-7.16689042625828));
#131459=CARTESIAN_POINT('Ctrl Pts',(-20.7394443043776,1.36525587718589,
-7.17021127213291));
#131460=CARTESIAN_POINT('Ctrl Pts',(-20.725214074249,1.31770309889276,-7.17352902206518));
#131461=CARTESIAN_POINT('Ctrl Pts',(-20.713766247517,1.26927144844836,-7.17683078321331));
#131462=CARTESIAN_POINT('Ctrl Pts',(-20.7051753409973,1.22031253559512,
-7.18007936578263));
#131463=CARTESIAN_POINT('Ctrl Pts',(-20.6965888582513,1.1713788334866,-7.18332627553731));
#131464=CARTESIAN_POINT('Ctrl Pts',(-20.690856271928,1.12191840822583,-7.18651996635826));
#131465=CARTESIAN_POINT('Ctrl Pts',(-20.6880171262504,1.07228633367087,
-7.18964753880948));
#131466=CARTESIAN_POINT('Ctrl Pts',(-20.6850290984163,1.02005159932611,
-7.19293911824876));
#131467=CARTESIAN_POINT('Ctrl Pts',(-20.6852463899028,0.967626732948496,
-7.19615728196852));
#131468=CARTESIAN_POINT('Ctrl Pts',(-20.6886731968112,0.915430274980151,
-7.19931634765498));
#131469=CARTESIAN_POINT('Ctrl Pts',(-20.6919321189101,0.865791005856937,
-7.20232064560722));
#131470=CARTESIAN_POINT('Ctrl Pts',(-20.6980937253409,0.816358423504461,
-7.20527191696333));
#131471=CARTESIAN_POINT('Ctrl Pts',(-20.7071227968265,0.767495730525501,
-7.20820573284366));
#131472=CARTESIAN_POINT('Ctrl Pts',(-20.7161573411168,0.718603420329508,
-7.21114132700219));
#131473=CARTESIAN_POINT('Ctrl Pts',(-20.7280632629945,0.670281881205839,
-7.21405985729603));
#131474=CARTESIAN_POINT('Ctrl Pts',(-20.7427621154086,0.622896180656631,
-7.21701502282478));
#131475=CARTESIAN_POINT('Ctrl Pts',(-20.7563341399243,0.579143112632761,
-7.2197436425751));
#131476=CARTESIAN_POINT('Ctrl Pts',(-20.7722876411628,0.536187529397152,
-7.22250408312399));
#131477=CARTESIAN_POINT('Ctrl Pts',(-20.7905212898478,0.494316287094292,
-7.22534636758163));
#131478=CARTESIAN_POINT('Ctrl Pts',(-20.7920678026586,0.490764918208087,
-7.22558743997484));
#131479=CARTESIAN_POINT('Ctrl Pts',(-20.7936307122051,0.487221319441231,
-7.22582910113882));
#131480=CARTESIAN_POINT('Ctrl Pts',(-20.7952099536369,0.483685648775972,
-7.22607138159539));
#131481=CARTESIAN_POINT('Ctrl Pts',(-20.7982598732763,0.476857363256427,
-7.22653928720367));
#131482=CARTESIAN_POINT('Ctrl Pts',(-20.80137062829,0.470058766383288,-7.22700950854635));
#131483=CARTESIAN_POINT('Ctrl Pts',(-20.8045416570145,0.463291089899534,
-7.22748226752908));
#131484=CARTESIAN_POINT('Ctrl Pts',(-20.8045488444521,0.463275750318491,
-7.22748333908219));
#131485=CARTESIAN_POINT('Ctrl Pts',(-20.8045560321993,0.463260410896288,
-7.22748441064832));
#131486=CARTESIAN_POINT('Ctrl Pts',(-20.8045632202561,0.463245071632921,
-7.2274854822275));
#131487=CARTESIAN_POINT('Ctrl Pts',(-20.8240114079387,0.421742774148196,
-7.23038477385445));
#131488=CARTESIAN_POINT('Ctrl Pts',(-20.8458043791237,0.381254595946671,
-7.2333869234291));
#131489=CARTESIAN_POINT('Ctrl Pts',(-20.8697899143661,0.342038658312353,
-7.23643293100584));
#131490=CARTESIAN_POINT('Ctrl Pts',(-20.8717022609837,0.338912004479815,
-7.23667578663644));
#131491=CARTESIAN_POINT('Ctrl Pts',(-20.8736285207544,0.33579345045752,
-7.23691892106093));
#131492=CARTESIAN_POINT('Ctrl Pts',(-20.8755686037111,0.33268313320659,
-7.23716230437709));
#131493=CARTESIAN_POINT('Ctrl Pts',(-20.9018047885627,0.290621602765477,
-7.24045363253935));
#131494=CARTESIAN_POINT('Ctrl Pts',(-20.9305736436336,0.250063409448494,
-7.24378987693124));
#131495=CARTESIAN_POINT('Ctrl Pts',(-20.9616520724195,0.211299434332199,
-7.24711174941872));
#131496=CARTESIAN_POINT('Ctrl Pts',(-20.992699333437,0.172574334623922,
-7.2504302904845));
#131497=CARTESIAN_POINT('Ctrl Pts',(-21.0260513365441,0.13563960361652,
-7.25373418844991));
#131498=CARTESIAN_POINT('Ctrl Pts',(-21.0614608676151,0.100756275337532,
-7.2569856166907));
#131499=CARTESIAN_POINT('Ctrl Pts',(-21.096860231571,0.0658829630853506,
-7.26023611135107));
#131500=CARTESIAN_POINT('Ctrl Pts',(-21.1343158966728,0.0330598020658376,
-7.26343406581022));
#131501=CARTESIAN_POINT('Ctrl Pts',(-21.1735578102251,0.00252106949673933,
-7.26656589599353));
#131502=CARTESIAN_POINT('Ctrl Pts',(-21.2127920393362,-0.0280116829080256,
-7.2696971128947));
#131503=CARTESIAN_POINT('Ctrl Pts',(-21.2538118480952,-0.0562608153356255,
-7.27276227829597));
#131504=CARTESIAN_POINT('Ctrl Pts',(-21.2963243649257,-0.0820188275929159,
-7.27577239800271));
#131505=CARTESIAN_POINT('Ctrl Pts',(-21.3388708395068,-0.107797414594285,
-7.27878492210472));
#131506=CARTESIAN_POINT('Ctrl Pts',(-21.3829124909228,-0.131080651973798,
-7.28174250519655));
#131507=CARTESIAN_POINT('Ctrl Pts',(-21.4281318499633,-0.151689722525295,
-7.28467903974164));
#131508=CARTESIAN_POINT('Ctrl Pts',(-21.4548209426474,-0.163853481715013,
-7.28641222314599));
#131509=CARTESIAN_POINT('Ctrl Pts',(-21.4819198346416,-0.175086248582036,
-7.28813850257311));
#131510=CARTESIAN_POINT('Ctrl Pts',(-21.5093591526456,-0.185356720995693,
-7.28986799996607));
#131511=CARTESIAN_POINT('Ctrl Pts',(-21.509386814352,-0.185251134616039,
-7.15421782883515));
#131512=CARTESIAN_POINT('Ctrl Pts',(-21.5016774549677,-0.182385205649202,
-7.15367724142142));
#131513=CARTESIAN_POINT('Ctrl Pts',(-21.4939960892933,-0.179444071264868,
-7.15313367548889));
#131514=CARTESIAN_POINT('Ctrl Pts',(-21.3984015600881,-0.141768165447487,
-7.14631135305286));
#131515=CARTESIAN_POINT('Ctrl Pts',(-21.3146239355693,-0.0973573701928965,
-7.13974825563708));
#131516=CARTESIAN_POINT('Ctrl Pts',(-21.1935796470064,-0.0146430459551139,
-7.12986617254163));
#131517=CARTESIAN_POINT('Ctrl Pts',(-21.1524347699526,0.0173693226557914,
-7.12641723933394));
#131518=CARTESIAN_POINT('Ctrl Pts',(-21.0914272581765,0.0711997026116773,
-7.12117157061882));
#131519=CARTESIAN_POINT('Ctrl Pts',(-21.0701549147649,0.0913251467019993,
-7.11931373171925));
#131520=CARTESIAN_POINT('Ctrl Pts',(-21.028125205139,0.133950077260687,
-7.11557493377509));
#131521=CARTESIAN_POINT('Ctrl Pts',(-21.0074474826271,0.156500985871011,
-7.11369793648784));
#131522=CARTESIAN_POINT('Ctrl Pts',(-20.9399338930674,0.235717198332699,
-7.10740756164589));
#131523=CARTESIAN_POINT('Ctrl Pts',(-20.8972267836028,0.295704817465734,
-7.10315118273114));
#131524=CARTESIAN_POINT('Ctrl Pts',(-20.8333695615624,0.404306469890634,
-7.09588505622193));
#131525=CARTESIAN_POINT('Ctrl Pts',(-20.8096126817668,0.451155232483091,
-7.09287091813559));
#131526=CARTESIAN_POINT('Ctrl Pts',(-20.7761000912601,0.528880138576766,
-7.08787325911741));
#131527=CARTESIAN_POINT('Ctrl Pts',(-20.7644968367809,0.558891358881146,
-7.08594367180285));
#131528=CARTESIAN_POINT('Ctrl Pts',(-20.7485773888549,0.605249507993371,
-7.0829179856093));
#131529=CARTESIAN_POINT('Ctrl Pts',(-20.7434230764883,0.621296491904699,
-7.08186232598506));
#131530=CARTESIAN_POINT('Ctrl Pts',(-20.732727322013,0.657034019461213,
-7.07948530689958));
#131531=CARTESIAN_POINT('Ctrl Pts',(-20.7273401899309,0.676764309323121,
-7.07815729456183));
#131532=CARTESIAN_POINT('Ctrl Pts',(-20.6985124526237,0.793408050978592,
-7.07024756323032));
#131533=CARTESIAN_POINT('Ctrl Pts',(-20.6861227969027,0.892688016810053,
-7.06331200549673));
#131534=CARTESIAN_POINT('Ctrl Pts',(-20.6852927256059,1.03064934568806,
-7.0540021627203));
#131535=CARTESIAN_POINT('Ctrl Pts',(-20.6867988707224,1.06889974822124,
-7.05145126892799));
#131536=CARTESIAN_POINT('Ctrl Pts',(-20.6928651361649,1.14031504612222,
-7.04675734061466));
#131537=CARTESIAN_POINT('Ctrl Pts',(-20.6970112183015,1.17348144629345,
-7.04460530062357));
#131538=CARTESIAN_POINT('Ctrl Pts',(-20.7070879228682,1.23437365440404,
-7.04070093915766));
#131539=CARTESIAN_POINT('Ctrl Pts',(-20.7126459622716,1.26213854913644,
-7.03893881521513));
#131540=CARTESIAN_POINT('Ctrl Pts',(-20.7285317639935,1.32963475836402,
-7.03468684187248));
#131541=CARTESIAN_POINT('Ctrl Pts',(-20.7398707521148,1.36909537250101,
-7.0322289968299));
#131542=CARTESIAN_POINT('Ctrl Pts',(-20.7812107170666,1.49038695999193,
-7.02467493624276));
#131543=CARTESIAN_POINT('Ctrl Pts',(-20.8177547302236,1.56970867679766,
-7.01974972480851));
#131544=CARTESIAN_POINT('Ctrl Pts',(-20.8827946522328,1.67946388168013,
-7.01229494176093));
#131545=CARTESIAN_POINT('Ctrl Pts',(-20.905086953342,1.71327032962481,-7.00989549970564));
#131546=CARTESIAN_POINT('Ctrl Pts',(-20.9394080518768,1.76024853949107,
-7.00632464563028));
#131547=CARTESIAN_POINT('Ctrl Pts',(-20.9501555968803,1.77432877205982,
-7.00522169222732));
#131548=CARTESIAN_POINT('Ctrl Pts',(-20.9729101552694,1.8028753965415,-7.00290680536955));
#131549=CARTESIAN_POINT('Ctrl Pts',(-20.9849508885042,1.81730874680709,
-7.00169319230561));
#131550=CARTESIAN_POINT('Ctrl Pts',(-21.0350672371991,1.87473185839483,
-6.99670432905464));
#131551=CARTESIAN_POINT('Ctrl Pts',(-21.0757267801254,1.9153704359689,-6.99279993910671));
#131552=CARTESIAN_POINT('Ctrl Pts',(-21.1894280937915,2.01450513059718,
-6.98250186255384));
#131553=CARTESIAN_POINT('Ctrl Pts',(-21.2664535980987,2.06792306168562,
-6.97613524836282));
#131554=CARTESIAN_POINT('Ctrl Pts',(-21.3757443544581,2.12700391817905,
-6.96806792084893));
#131555=CARTESIAN_POINT('Ctrl Pts',(-21.4033444568525,2.14064689971433,
-6.96610134778188));
#131556=CARTESIAN_POINT('Ctrl Pts',(-21.4580076576159,2.16522693070633,
-6.96233527624186));
#131557=CARTESIAN_POINT('Ctrl Pts',(-21.4850054194939,2.1762612427356,-6.9605335530104));
#131558=CARTESIAN_POINT('Ctrl Pts',(-21.5599512854856,2.20390827574016,
-6.95567124426099));
#131559=CARTESIAN_POINT('Ctrl Pts',(-21.6085561264379,2.21858523083194,
-6.952671421686));
#131560=CARTESIAN_POINT('Ctrl Pts',(-21.7434312675698,2.25060575674037,
-6.94459283559037));
#131561=CARTESIAN_POINT('Ctrl Pts',(-21.8308242804758,2.26193527433161,
-6.93963404642151));
#131562=CARTESIAN_POINT('Ctrl Pts',(-21.9472291852791,2.26481942129707,
-6.93271586244532));
#131563=CARTESIAN_POINT('Ctrl Pts',(-21.9757926830589,2.2645593434174,-6.93099183634112));
#131564=CARTESIAN_POINT('Ctrl Pts',(-22.0208120821806,2.26262360784871,
-6.92819989584836));
#131565=CARTESIAN_POINT('Ctrl Pts',(-22.0372856779751,2.26159181437303,
-6.92716190461531));
#131566=CARTESIAN_POINT('Ctrl Pts',(-22.0755281745437,2.2584439024064,-6.92470874863353));
#131567=CARTESIAN_POINT('Ctrl Pts',(-22.0972688222191,2.25608524384247,
-6.92328314082742));
#131568=CARTESIAN_POINT('Ctrl Pts',(-22.1463492637306,2.24946883899091,
-6.92000974581403));
#131569=CARTESIAN_POINT('Ctrl Pts',(-22.173632670081,2.24487496516116,-6.91815116196387));
#131570=CARTESIAN_POINT('Ctrl Pts',(-22.2773521442516,2.2238914110896,-6.91098259487542));
#131571=CARTESIAN_POINT('Ctrl Pts',(-22.3523660892459,2.20132108028442,
-6.90559432166925));
#131572=CARTESIAN_POINT('Ctrl Pts',(-22.4686372203978,2.15421454737421,
-6.89717917424165));
#131573=CARTESIAN_POINT('Ctrl Pts',(-22.5114319616763,2.13401533467892,
-6.8940636963432));
#131574=CARTESIAN_POINT('Ctrl Pts',(-22.5781027331393,2.09784467635113,
-6.88918715892521));
#131575=CARTESIAN_POINT('Ctrl Pts',(-22.6027394544039,2.0833777666151,-6.88737928185582));
#131576=CARTESIAN_POINT('Ctrl Pts',(-22.653299041708,2.05133723980745,-6.88364899261077));
#131577=CARTESIAN_POINT('Ctrl Pts',(-22.6791019356882,2.03361024813863,
-6.88173352477339));
#131578=CARTESIAN_POINT('Ctrl Pts',(-22.731695534707,1.99452700681577,-6.87778420312835));
#131579=CARTESIAN_POINT('Ctrl Pts',(-22.7583297642959,1.97300313689141,
-6.8757578284127));
#131580=CARTESIAN_POINT('Ctrl Pts',(-22.8371991367377,1.90379009647875,
-6.86961604351262));
#131581=CARTESIAN_POINT('Ctrl Pts',(-22.8863334023872,1.8527827984822,-6.86559220198115));
#131582=CARTESIAN_POINT('Ctrl Pts',(-22.958761203722,1.76374337893306,-6.85891593393953));
#131583=CARTESIAN_POINT('Ctrl Pts',(-22.9847661437143,1.7281218705474,-6.85632013207033));
#131584=CARTESIAN_POINT('Ctrl Pts',(-23.0191027862774,1.67552268706351,
-6.85248385660168));
#131585=CARTESIAN_POINT('Ctrl Pts',(-23.0289984739246,1.6596012973375,-6.85132214409339));
#131586=CARTESIAN_POINT('Ctrl Pts',(-23.047568715109,1.62818651079117,-6.84901729150804));
#131587=CARTESIAN_POINT('Ctrl Pts',(-23.0562778972977,1.61271892664599,
-6.84787628508707));
#131588=CARTESIAN_POINT('Ctrl Pts',(-23.0839597678304,1.561040592998,-6.84405602115891));
#131589=CARTESIAN_POINT('Ctrl Pts',(-23.1015013533035,1.52409480796297,
-6.84131278764619));
#131590=CARTESIAN_POINT('Ctrl Pts',(-23.1516090040283,1.40384280193087,
-6.83247424524913));
#131591=CARTESIAN_POINT('Ctrl Pts',(-23.1771511290149,1.31789320089251,
-6.82631061008411));
#131592=CARTESIAN_POINT('Ctrl Pts',(-23.2006185206185,1.19100624080797,
-6.81774663659851));
#131593=CARTESIAN_POINT('Ctrl Pts',(-23.205989483707,1.15172673628016,-6.815162729159));
#131594=CARTESIAN_POINT('Ctrl Pts',(-23.2120118205817,1.08415662469309,
-6.81083069183341));
#131595=CARTESIAN_POINT('Ctrl Pts',(-23.213575354763,1.05597936850348,-6.80905719159886));
#131596=CARTESIAN_POINT('Ctrl Pts',(-23.2149448324097,0.993639117870933,
-6.80519683104589));
#131597=CARTESIAN_POINT('Ctrl Pts',(-23.2143120658532,0.959488398291515,
-6.80312419793399));
#131598=CARTESIAN_POINT('Ctrl Pts',(-23.2099565405224,0.885786321757234,
-6.79871234301716));
#131599=CARTESIAN_POINT('Ctrl Pts',(-23.2057515482306,0.846300300933489,
-6.79638717457841));
#131600=CARTESIAN_POINT('Ctrl Pts',(-23.1875791932575,0.728586207702584,
-6.78947305718707));
#131601=CARTESIAN_POINT('Ctrl Pts',(-23.1680956432057,0.651418263043526,
-6.78497187775141));
#131602=CARTESIAN_POINT('Ctrl Pts',(-23.1317280843806,0.549076780320772,
-6.77852669285569));
#131603=CARTESIAN_POINT('Ctrl Pts',(-23.1210008074229,0.521910198356554,
-6.77676599840483));
#131604=CARTESIAN_POINT('Ctrl Pts',(-23.1027317456309,0.479957607221917,
-6.77393297667239));
#131605=CARTESIAN_POINT('Ctrl Pts',(-23.095823007777,0.46490732177892,-6.77289241106506));
#131606=CARTESIAN_POINT('Ctrl Pts',(-23.0792448076277,0.430587102456728,
-6.77045732701787));
#131607=CARTESIAN_POINT('Ctrl Pts',(-23.0693755259031,0.411422743933523,
-6.76905319870975));
#131608=CARTESIAN_POINT('Ctrl Pts',(-23.0460177062739,0.368780362396985,
-6.76584219280443));
#131609=CARTESIAN_POINT('Ctrl Pts',(-23.0322550202698,0.345464320222795,
-6.76402508239477));
#131610=CARTESIAN_POINT('Ctrl Pts',(-22.9782548353948,0.260345066971941,
-6.75720138707321));
#131611=CARTESIAN_POINT('Ctrl Pts',(-22.933381040543,0.201651760054102,
-6.75211978654992));
#131612=CARTESIAN_POINT('Ctrl Pts',(-22.8493305018051,0.109632506664279,
-6.74372836557732));
#131613=CARTESIAN_POINT('Ctrl Pts',(-22.8127730552537,0.0741634603516683,
-6.74036233026094));
#131614=CARTESIAN_POINT('Ctrl Pts',(-22.752050691716,0.0219786042143744,
-6.73520341851663));
#131615=CARTESIAN_POINT('Ctrl Pts',(-22.7292755071091,0.00373644957244235,
-6.73335327419755));
#131616=CARTESIAN_POINT('Ctrl Pts',(-22.6812361681583,-0.0320850622434765,
-6.72961257636881));
#131617=CARTESIAN_POINT('Ctrl Pts',(-22.6559204924024,-0.0495629563493249,
-6.72772656001868));
#131618=CARTESIAN_POINT('Ctrl Pts',(-22.563394516946,-0.108578753591728,
-6.72109846518524));
#131619=CARTESIAN_POINT('Ctrl Pts',(-22.4929628250474,-0.144723789772137,
-6.71654371157681));
#131620=CARTESIAN_POINT('Ctrl Pts',(-22.3556704954303,-0.199639352037324,
-6.70801727982755));
#131621=CARTESIAN_POINT('Ctrl Pts',(-22.2897513395334,-0.219946807210785,
-6.70405517398232));
#131622=CARTESIAN_POINT('Ctrl Pts',(-22.2029902270708,-0.239094826950152,
-6.69865610670695));
#131623=CARTESIAN_POINT('Ctrl Pts',(-22.1833672854766,-0.242939921594036,
-6.69742282018039));
#131624=CARTESIAN_POINT('Ctrl Pts',(-22.1468711343587,-0.249196646176375,
-6.69509316990416));
#131625=CARTESIAN_POINT('Ctrl Pts',(-22.1300250867619,-0.251735335066461,
-6.69400290215746));
#131626=CARTESIAN_POINT('Ctrl Pts',(-22.0795657633504,-0.258300002317591,
-6.6907008151968));
#131627=CARTESIAN_POINT('Ctrl Pts',(-22.0458378928057,-0.261317130978158,
-6.68844668766188));
#131628=CARTESIAN_POINT('Ctrl Pts',(-21.9541252805914,-0.265821702660416,
-6.68225436445445));
#131629=CARTESIAN_POINT('Ctrl Pts',(-21.8960917603556,-0.264679954291367,
-6.67827112571661));
#131630=CARTESIAN_POINT('Ctrl Pts',(-21.7724231956618,-0.253716939435655,
-6.66982434090838));
#131631=CARTESIAN_POINT('Ctrl Pts',(-21.7070577889929,-0.242707042140617,
-6.66538777908186));
#131632=CARTESIAN_POINT('Ctrl Pts',(-21.6133489506423,-0.219241992523442,
-6.65912460472257));
#131633=CARTESIAN_POINT('Ctrl Pts',(-21.584124641201,-0.210793306324488,
-6.65718428603359));
#131634=CARTESIAN_POINT('Ctrl Pts',(-21.5398478262548,-0.196243134294687,
-6.65425946735996));
#131635=CARTESIAN_POINT('Ctrl Pts',(-21.5245635260665,-0.190893027184671,
-6.65325253478706));
#131636=CARTESIAN_POINT('Ctrl Pts',(-21.5093868170662,-0.185251135625031,
-6.6522544014516));
#131637=CARTESIAN_POINT('Origin',(-21.9500000210213,0.999999999999992,-6.00000000000001));
#131638=CARTESIAN_POINT('',(-21.50938681096,-0.185251133355075,-6.15441066307283));
#131639=CARTESIAN_POINT('',(-21.5093309141335,-0.185465194475762,-6.28967656064001));
#131640=CARTESIAN_POINT('',(-21.5093868137063,-0.185251134376008,-6.00000000000001));
#131641=CARTESIAN_POINT('',(-20.9918838682989,1.82521129893649,-6.00000000000001));
#131642=CARTESIAN_POINT('Ctrl Pts',(-21.5093868082137,-0.185251132334142,
-6.15441066307283));
#131643=CARTESIAN_POINT('Ctrl Pts',(-21.5035873446221,-0.183095200805407,
-6.15401289301834));
#131644=CARTESIAN_POINT('Ctrl Pts',(-21.4978038646796,-0.180896763802468,
-6.15361283867239));
#131645=CARTESIAN_POINT('Ctrl Pts',(-21.4625878473075,-0.167213685525018,
-6.1511571735926));
#131646=CARTESIAN_POINT('Ctrl Pts',(-21.4335804894447,-0.154672656841437,
-6.14905029026393));
#131647=CARTESIAN_POINT('Ctrl Pts',(-21.3135856849169,-0.0973679694903984,
-6.14005981956633));
#131648=CARTESIAN_POINT('Ctrl Pts',(-21.2276787361607,-0.0428303393803642,
-6.13297641724258));
#131649=CARTESIAN_POINT('Ctrl Pts',(-21.1170948879019,0.0476606281421388,
-6.12342269196022));
#131650=CARTESIAN_POINT('Ctrl Pts',(-21.0862990852199,0.0754987566832099,
-6.12069966452596));
#131651=CARTESIAN_POINT('Ctrl Pts',(-21.0375321827043,0.124150089584365,
-6.11627985310815));
#131652=CARTESIAN_POINT('Ctrl Pts',(-21.0187722033716,0.144122929985144,
-6.11454962951449));
#131653=CARTESIAN_POINT('Ctrl Pts',(-20.9803961525467,0.187737147608704,
-6.11093663654197));
#131654=CARTESIAN_POINT('Ctrl Pts',(-20.9609625200354,0.211515593731937,
-6.10906192121341));
#131655=CARTESIAN_POINT('Ctrl Pts',(-20.9218656015674,0.263076472741846,
-6.10517087687439));
#131656=CARTESIAN_POINT('Ctrl Pts',(-20.9024193756609,0.290992460109405,
-6.10316275680569));
#131657=CARTESIAN_POINT('Ctrl Pts',(-20.8449421166225,0.381041246971425,
-6.096924715088));
#131658=CARTESIAN_POINT('Ctrl Pts',(-20.8111395642315,0.445690125375156,
-6.09279366128499));
#131659=CARTESIAN_POINT('Ctrl Pts',(-20.7677397050999,0.54965743979662,
-6.08622680730066));
#131660=CARTESIAN_POINT('Ctrl Pts',(-20.7541383691964,0.587129276127882,
-6.08387207511793));
#131661=CARTESIAN_POINT('Ctrl Pts',(-20.7369502708294,0.642508900598489,
-6.0803260379934));
#131662=CARTESIAN_POINT('Ctrl Pts',(-20.7319450187071,0.659953651000476,
-6.07919968154447));
#131663=CARTESIAN_POINT('Ctrl Pts',(-20.7228072521544,0.694597240670247,
-6.07693335908763));
#131664=CARTESIAN_POINT('Ctrl Pts',(-20.7186567867926,0.711787064855045,
-6.07579489678123));
#131665=CARTESIAN_POINT('Ctrl Pts',(-20.7066535968606,0.766505310633434,
-6.07213793571435));
#131666=CARTESIAN_POINT('Ctrl Pts',(-20.7001468746471,0.804304586881464,
-6.06956333806152));
#131667=CARTESIAN_POINT('Ctrl Pts',(-20.6863695904695,0.913940108943603,
-6.06204794116306));
#131668=CARTESIAN_POINT('Ctrl Pts',(-20.6835176458326,0.986181954357668,
-6.05704484144758));
#131669=CARTESIAN_POINT('Ctrl Pts',(-20.689564655222,1.11725835173862,-6.04811588698487));
#131670=CARTESIAN_POINT('Ctrl Pts',(-20.6964141887923,1.17598545012247,
-6.04416858128833));
#131671=CARTESIAN_POINT('Ctrl Pts',(-20.7133990662909,1.26617387807076,
-6.03820556845549));
#131672=CARTESIAN_POINT('Ctrl Pts',(-20.7206992041205,1.29807757740358,
-6.03611489726459));
#131673=CARTESIAN_POINT('Ctrl Pts',(-20.7379454617443,1.36194169394248,
-6.03195570550728));
#131674=CARTESIAN_POINT('Ctrl Pts',(-20.7479389441103,1.39386226237218,
-6.02989035189926));
#131675=CARTESIAN_POINT('Ctrl Pts',(-20.7827238309017,1.49124604286103,
-6.02359352174865));
#131676=CARTESIAN_POINT('Ctrl Pts',(-20.8116905231942,1.55507554217424,
-6.01947811639436));
#131677=CARTESIAN_POINT('Ctrl Pts',(-20.875497414123,1.66941819395525,-6.01177893977397));
#131678=CARTESIAN_POINT('Ctrl Pts',(-20.9090124892552,1.72043080180369,
-6.00820246191594));
#131679=CARTESIAN_POINT('Ctrl Pts',(-20.9541735789873,1.77940199641434,
-6.00368204388054));
#131680=CARTESIAN_POINT('Ctrl Pts',(-20.9624409819876,1.78985118619023,
-6.00286500844259));
#131681=CARTESIAN_POINT('Ctrl Pts',(-20.977769861111,1.80860843511925,-6.00136535341716));
#131682=CARTESIAN_POINT('Ctrl Pts',(-20.9847702393647,1.81695198063206,
-6.00068598746145));
#131683=CARTESIAN_POINT('Ctrl Pts',(-20.991883868299,1.82521129893659,-6.00000000000002));
#131684=CARTESIAN_POINT('',(-22.9011121207488,1.83390790479519,-6.00000965906464));
#131685=CARTESIAN_POINT('Origin',(-21.9500000210213,0.999999999999992,-6.00000000000001));
#131686=CARTESIAN_POINT('Ctrl Pts',(-22.9011121207488,1.83390790479519,
-6.00000965906464));
#131687=CARTESIAN_POINT('Ctrl Pts',(-22.8713097432318,1.86779472815481,
-6.00298048945063));
#131688=CARTESIAN_POINT('Ctrl Pts',(-22.8396158236806,1.90012348438907,
-6.0060066212151));
#131689=CARTESIAN_POINT('Ctrl Pts',(-22.8062336014144,1.9306940554392,-6.00903832068673));
#131690=CARTESIAN_POINT('Ctrl Pts',(-22.7700412498819,1.96383806979444,
-6.01232522987281));
#131691=CARTESIAN_POINT('Ctrl Pts',(-22.7318639832695,1.99491599973358,
-6.01561829348637));
#131692=CARTESIAN_POINT('Ctrl Pts',(-22.6919801403607,2.02370789545272,
-6.01887250050576));
#131693=CARTESIAN_POINT('Ctrl Pts',(-22.652129889946,2.0524755409614,-6.02212396664258));
#131694=CARTESIAN_POINT('Ctrl Pts',(-22.6105760239588,2.07896112137499,
-6.02533647420468));
#131695=CARTESIAN_POINT('Ctrl Pts',(-22.5676151790485,2.1029762674912,-6.02848756994525));
#131696=CARTESIAN_POINT('Ctrl Pts',(-22.5246715436695,2.12698179346589,
-6.03163740339963));
#131697=CARTESIAN_POINT('Ctrl Pts',(-22.4803220859832,2.14851881515413,
-6.03472586264234));
#131698=CARTESIAN_POINT('Ctrl Pts',(-22.4348812613488,2.1674297043965,-6.03775425916792));
#131699=CARTESIAN_POINT('Ctrl Pts',(-22.3894084180212,2.18635391870427,
-6.04078478957421));
#131700=CARTESIAN_POINT('Ctrl Pts',(-22.3428426744419,2.20264809614928,
-6.04375529690198));
#131701=CARTESIAN_POINT('Ctrl Pts',(-22.295517118546,2.2161867333396,-6.04669004057557));
#131702=CARTESIAN_POINT('Ctrl Pts',(-22.2481745126847,2.2297302480911,-6.04962584154846));
#131703=CARTESIAN_POINT('Ctrl Pts',(-22.2000715613054,2.24051587094073,
-6.05252614961448));
#131704=CARTESIAN_POINT('Ctrl Pts',(-22.1515595825469,2.2484546579708,-6.05543509360173));
#131705=CARTESIAN_POINT('Ctrl Pts',(-22.1029631731448,2.25640726173059,
-6.05834910033883));
#131706=CARTESIAN_POINT('Ctrl Pts',(-22.0539564189202,2.26150252955795,
-6.06127230168759));
#131707=CARTESIAN_POINT('Ctrl Pts',(-22.0049096303005,2.26369496890294,
-6.06426284414001));
#131708=CARTESIAN_POINT('Ctrl Pts',(-21.9743762858115,2.2650598392171,-6.06612456160365));
#131709=CARTESIAN_POINT('Ctrl Pts',(-21.943827780378,2.26530060705494,-6.06801264038704));
#131710=CARTESIAN_POINT('Ctrl Pts',(-21.9133562609771,2.2644166063358,-6.06994211780836));
#131711=CARTESIAN_POINT('Ctrl Pts',(-21.9133398817407,2.26441613116235,
-6.0699431549528));
#131712=CARTESIAN_POINT('Ctrl Pts',(-21.9133235025263,2.26441565566411,
-6.0699441921092));
#131713=CARTESIAN_POINT('Ctrl Pts',(-21.9133071233339,2.26441517984107,
-6.06994522927756));
#131714=CARTESIAN_POINT('Ctrl Pts',(-21.8673192256092,2.26307921034984,
-6.07285728937845));
#131715=CARTESIAN_POINT('Ctrl Pts',(-21.821332023664,2.25917004659305,-6.07587137180823));
#131716=CARTESIAN_POINT('Ctrl Pts',(-21.775644760231,2.25272564667812,-6.07892845683477));
#131717=CARTESIAN_POINT('Ctrl Pts',(-21.7708420212566,2.25204819812217,
-6.07924982389206));
#131718=CARTESIAN_POINT('Ctrl Pts',(-21.7660426336406,2.25134276349747,
-6.07957166615584));
#131719=CARTESIAN_POINT('Ctrl Pts',(-21.7612469702657,2.25060940867523,
-6.07989391506484));
#131720=CARTESIAN_POINT('Ctrl Pts',(-21.7121703029202,2.24310458445299,
-6.08319166581872));
#131721=CARTESIAN_POINT('Ctrl Pts',(-21.6634787674,2.23267271882655,-6.08653145174611));
#131722=CARTESIAN_POINT('Ctrl Pts',(-21.6155281574828,2.21940450502726,
-6.08985485980112));
#131723=CARTESIAN_POINT('Ctrl Pts',(-21.5676209205818,2.20614829279485,
-6.09317526171645));
#131724=CARTESIAN_POINT('Ctrl Pts',(-21.5204531188573,2.19006113845352,
-6.09647902274909));
#131725=CARTESIAN_POINT('Ctrl Pts',(-21.474362858205,2.17126760454069,-6.09972932563849));
#131726=CARTESIAN_POINT('Ctrl Pts',(-21.4282952280532,2.15248329832741,
-6.10297803261629));
#131727=CARTESIAN_POINT('Ctrl Pts',(-21.3833040326441,2.13099533602493,
-6.10617323986711));
#131728=CARTESIAN_POINT('Ctrl Pts',(-21.3397116969543,2.10695972318957,
-6.10930243364974));
#131729=CARTESIAN_POINT('Ctrl Pts',(-21.2939491415504,2.08172751099815,
-6.1125874125705));
#131730=CARTESIAN_POINT('Ctrl Pts',(-21.2497284240167,2.05368728589693,
-6.11579947564642));
#131731=CARTESIAN_POINT('Ctrl Pts',(-21.2074043428962,2.02305714661068,
-6.1189532360732));
#131732=CARTESIAN_POINT('Ctrl Pts',(-21.1670505414467,1.99385290811563,
-6.12196018197049));
#131733=CARTESIAN_POINT('Ctrl Pts',(-21.1284209722979,1.96229436247761,
-6.12491454104969));
#131734=CARTESIAN_POINT('Ctrl Pts',(-21.0918052506033,1.92860514658044,
-6.12785217121838));
#131735=CARTESIAN_POINT('Ctrl Pts',(-21.0551669780058,1.89489518215779,
-6.1307916106157));
#131736=CARTESIAN_POINT('Ctrl Pts',(-21.0205454296841,1.85905165078437,
-6.13371471784211));
#131737=CARTESIAN_POINT('Ctrl Pts',(-20.9882088085043,1.82133591135897,
-6.13667539457963));
#131738=CARTESIAN_POINT('Ctrl Pts',(-20.9584022011698,1.78657104742548,
-6.13940442828013));
#131739=CARTESIAN_POINT('Ctrl Pts',(-20.9305368223933,1.75021498090851,
-6.14216597327682));
#131740=CARTESIAN_POINT('Ctrl Pts',(-20.9048013374323,1.71250560459693,
-6.14500982309761));
#131741=CARTESIAN_POINT('Ctrl Pts',(-20.9025707094642,1.70923713735855,
-6.14525631431225));
#131742=CARTESIAN_POINT('Ctrl Pts',(-20.9003560520861,1.70595849200513,
-6.14550342384911));
#131743=CARTESIAN_POINT('Ctrl Pts',(-20.898157470971,1.70266981655717,-6.14575118413152));
#131744=CARTESIAN_POINT('Ctrl Pts',(-20.8942178967889,1.69677693373415,
-6.1461951386462));
#131745=CARTESIAN_POINT('Ctrl Pts',(-20.8903299935753,1.6908519627177,-6.14664118749188));
#131746=CARTESIAN_POINT('Ctrl Pts',(-20.8864943949038,1.68489586492067,
-6.14708951858961));
#131747=CARTESIAN_POINT('Ctrl Pts',(-20.8864852551754,1.68488167232105,
-6.14709058690379));
#131748=CARTESIAN_POINT('Ctrl Pts',(-20.8864761157439,1.68486747954469,
-6.14709165523094));
#131749=CARTESIAN_POINT('Ctrl Pts',(-20.8864669766095,1.6848532865916,-6.14709272357104));
#131750=CARTESIAN_POINT('Ctrl Pts',(-20.8616393916057,1.64629638052638,
-6.14999500111978));
#131751=CARTESIAN_POINT('Ctrl Pts',(-20.8389189581031,1.60628971347035,
-6.15300031840583));
#131752=CARTESIAN_POINT('Ctrl Pts',(-20.8184436372102,1.56509934702104,
-6.15604948295174));
#131753=CARTESIAN_POINT('Ctrl Pts',(-20.8162248249759,1.5606357447414,-6.1563799062762));
#131754=CARTESIAN_POINT('Ctrl Pts',(-20.8140323731525,1.5561582925127,-6.15671084449976));
#131755=CARTESIAN_POINT('Ctrl Pts',(-20.8118664533325,1.55166736533703,
-6.15704222229796));
#131756=CARTESIAN_POINT('Ctrl Pts',(-20.790352298961,1.50705883475574,-6.16033380910543));
#131757=CARTESIAN_POINT('Ctrl Pts',(-20.7714556833859,1.46111498316825,
-6.16366822070424));
#131758=CARTESIAN_POINT('Ctrl Pts',(-20.7553034137482,1.41417869184914,
-6.16698669931937));
#131759=CARTESIAN_POINT('Ctrl Pts',(-20.7391664062568,1.36728675024439,
-6.17030204233144));
#131760=CARTESIAN_POINT('Ctrl Pts',(-20.7257682505138,1.31940427839298,
-6.17360119049667));
#131761=CARTESIAN_POINT('Ctrl Pts',(-20.715197855059,1.27087886425945,-6.17684696009321));
#131762=CARTESIAN_POINT('Ctrl Pts',(-20.7046330109948,1.2223789348416,-6.18009102506719));
#131763=CARTESIAN_POINT('Ctrl Pts',(-20.6968928772115,1.17323674002102,
-6.1832816730545));
#131764=CARTESIAN_POINT('Ctrl Pts',(-20.6920315695949,1.12380481144512,
-6.18640599515564));
#131765=CARTESIAN_POINT('Ctrl Pts',(-20.6871707749018,1.074378098503,-6.18952998760507));
#131766=CARTESIAN_POINT('Ctrl Pts',(-20.6851882933946,1.02466173578174,
-6.19258771833382));
#131767=CARTESIAN_POINT('Ctrl Pts',(-20.6861034240943,0.975013474372067,
-6.19559081097353));
#131768=CARTESIAN_POINT('Ctrl Pts',(-20.6870194252162,0.925317990247499,
-6.19859675999096));
#131769=CARTESIAN_POINT('Ctrl Pts',(-20.6908388122172,0.875690802066594,
-6.20154816281778));
#131770=CARTESIAN_POINT('Ctrl Pts',(-20.6975434174409,0.826495392766933,
-6.20447944209982));
#131771=CARTESIAN_POINT('Ctrl Pts',(-20.7042519357294,0.77727127114003,
-6.20741243218885));
#131772=CARTESIAN_POINT('Ctrl Pts',(-20.7138494721898,0.728479597982973,
-6.2103256739219));
#131773=CARTESIAN_POINT('Ctrl Pts',(-20.7262751195905,0.680487566651962,
-6.21327203433781));
#131774=CARTESIAN_POINT('Ctrl Pts',(-20.7378129540606,0.63592456759643,
-6.21600787720151));
#131775=CARTESIAN_POINT('Ctrl Pts',(-20.7517895524973,0.592050682334131,
-6.21877285310299));
#131776=CARTESIAN_POINT('Ctrl Pts',(-20.768116273302,0.549161052075565,
-6.22161762458379));
#131777=CARTESIAN_POINT('Ctrl Pts',(-20.7694019968649,0.545783508667803,
-6.22184164934464));
#131778=CARTESIAN_POINT('Ctrl Pts',(-20.7707022884922,0.542412043045365,
-6.22206616895837));
#131779=CARTESIAN_POINT('Ctrl Pts',(-20.7720171020505,0.539046785865255,
-6.22229120816688));
#131780=CARTESIAN_POINT('Ctrl Pts',(-20.7758037854877,0.529354792999785,
-6.22293932457718));
#131781=CARTESIAN_POINT('Ctrl Pts',(-20.7797107818593,0.519714530025211,
-6.22359176515896));
#131782=CARTESIAN_POINT('Ctrl Pts',(-20.7837367273305,0.510129376493374,
-6.22424912979539));
#131783=CARTESIAN_POINT('Ctrl Pts',(-20.7837433509997,0.510113606561484,
-6.22425021132168));
#131784=CARTESIAN_POINT('Ctrl Pts',(-20.7837499749908,0.510097836778732,
-6.2242512928613));
#131785=CARTESIAN_POINT('Ctrl Pts',(-20.7837565993039,0.510082067145121,
-6.22425237441425));
#131786=CARTESIAN_POINT('Ctrl Pts',(-20.801503389991,0.46783460934574,-6.22714989656084));
#131787=CARTESIAN_POINT('Ctrl Pts',(-20.8216332018884,0.426505299554568,
-6.23015053397542));
#131788=CARTESIAN_POINT('Ctrl Pts',(-20.8440044314121,0.38635801429458,
-6.23319531389269));
#131789=CARTESIAN_POINT('Ctrl Pts',(-20.8457968689767,0.383141315715649,
-6.23343926909836));
#131790=CARTESIAN_POINT('Ctrl Pts',(-20.8476036714323,0.379932218863172,
-6.23368350768151));
#131791=CARTESIAN_POINT('Ctrl Pts',(-20.849424753186,0.37673086620638,-6.23392799930922));
#131792=CARTESIAN_POINT('Ctrl Pts',(-20.8739400352976,0.333634468494913,
-6.2372193294295));
#131793=CARTESIAN_POINT('Ctrl Pts',(-20.9010476656863,0.291938329336222,
-6.24055591498521));
#131794=CARTESIAN_POINT('Ctrl Pts',(-20.930536340152,0.251942199479993,
-6.24387839074676));
#131795=CARTESIAN_POINT('Ctrl Pts',(-20.9599958277432,0.211985656415745,
-6.24719757803622));
#131796=CARTESIAN_POINT('Ctrl Pts',(-20.9918314361918,0.173725513541029,
-6.2505023823593));
#131797=CARTESIAN_POINT('Ctrl Pts',(-21.0258065615214,0.137432646464108,
-6.25375489189921));
#131798=CARTESIAN_POINT('Ctrl Pts',(-21.0597753040982,0.101146597563584,
-6.2570067904049));
#131799=CARTESIAN_POINT('Ctrl Pts',(-21.095882711719,0.0668270128838862,
-6.26020631217642));
#131800=CARTESIAN_POINT('Ctrl Pts',(-21.133868217647,0.0347190084594118,
-6.26333979107174));
#131801=CARTESIAN_POINT('Ctrl Pts',(-21.1718464646505,0.00261713978520092,
-6.26647267116797));
#131802=CARTESIAN_POINT('Ctrl Pts',(-21.2117021266801,-0.0272739097097115,
-6.26953958018813));
#131803=CARTESIAN_POINT('Ctrl Pts',(-21.2531507563779,-0.0547348690975048,
-6.2725514642462));
#131804=CARTESIAN_POINT('Ctrl Pts',(-21.2946429409792,-0.0822246849142601,
-6.27556651324171));
#131805=CARTESIAN_POINT('Ctrl Pts',(-21.3377315375078,-0.107279055106542,
-6.27852661330183));
#131806=CARTESIAN_POINT('Ctrl Pts',(-21.3821061237463,-0.129706240497145,
-6.28146565119256));
#131807=CARTESIAN_POINT('Ctrl Pts',(-21.4234870870306,-0.150620430665151,
-6.28420641407863));
#131808=CARTESIAN_POINT('Ctrl Pts',(-21.4659862143645,-0.169249924388195,
-6.2869293430793));
#131809=CARTESIAN_POINT('Ctrl Pts',(-21.5093309141335,-0.185465194475759,
-6.28967656064001));
#131810=CARTESIAN_POINT('Origin',(21.9499999789786,0.999999999999992,-6.00000000000001));
#131811=CARTESIAN_POINT('',(22.3906127228612,-0.185251306655355,-7.65234642888876));
#131812=CARTESIAN_POINT('',(22.3905831448079,-0.185130158742934,-7.79034991681388));
#131813=CARTESIAN_POINT('',(22.3906127231008,-0.185251306566283,-6.00000000000001));
#131814=CARTESIAN_POINT('',(20.6856550625054,0.998431907182509,-7.94368587507956));
#131815=CARTESIAN_POINT('Ctrl Pts',(22.390583144063,-0.185130159018148,
-7.79034991686661));
#131816=CARTESIAN_POINT('Ctrl Pts',(22.3439765723818,-0.202348905991787,
-7.79364863419787));
#131817=CARTESIAN_POINT('Ctrl Pts',(22.2963237313581,-0.216845811350756,
-7.79691786542976));
#131818=CARTESIAN_POINT('Ctrl Pts',(22.2479697582444,-0.228522558252233,
-7.80012784772216));
#131819=CARTESIAN_POINT('Ctrl Pts',(22.1996342522863,-0.240194845617333,
-7.80333660407099));
#131820=CARTESIAN_POINT('Ctrl Pts',(22.1505981513039,-0.249049151948672,
-7.80648610985219));
#131821=CARTESIAN_POINT('Ctrl Pts',(22.1012136067467,-0.255021300792385,
-7.80957128037498));
#131822=CARTESIAN_POINT('Ctrl Pts',(22.0517917907318,-0.260997956930732,
-7.81265877933481));
#131823=CARTESIAN_POINT('Ctrl Pts',(22.0020210234089,-0.264087952829062,
-7.81568193738516));
#131824=CARTESIAN_POINT('Ctrl Pts',(21.9522615474857,-0.264262035242583,
-7.81866001093743));
#131825=CARTESIAN_POINT('Ctrl Pts',(21.9024857611145,-0.264436174717843,
-7.82163906065983));
#131826=CARTESIAN_POINT('Ctrl Pts',(21.852721337544,-0.261692172686859,
-7.82457325276417));
#131827=CARTESIAN_POINT('Ctrl Pts',(21.8033355908035,-0.256039305863788,
-7.82750365227269));
#131828=CARTESIAN_POINT('Ctrl Pts',(21.7538565565994,-0.250375761028484,
-7.83043958717462));
#131829=CARTESIAN_POINT('Ctrl Pts',(21.7047578208058,-0.241791833859899,
-7.83337219559926));
#131830=CARTESIAN_POINT('Ctrl Pts',(21.6564137458961,-0.230341818590182,
-7.83635919443393));
#131831=CARTESIAN_POINT('Ctrl Pts',(21.6120256549547,-0.219828755303278,
-7.83910176787573));
#131832=CARTESIAN_POINT('Ctrl Pts',(21.5682741293063,-0.206899581905377,
-7.84189084857918));
#131833=CARTESIAN_POINT('Ctrl Pts',(21.5254491372987,-0.191636063670674,
-7.84477652606721));
#131834=CARTESIAN_POINT('Ctrl Pts',(21.5254316189557,-0.191629819850547,
-7.84477770650615));
#131835=CARTESIAN_POINT('Ctrl Pts',(21.5254141007671,-0.191623575640044,
-7.84477888696124));
#131836=CARTESIAN_POINT('Ctrl Pts',(21.5253965827328,-0.191617331039193,
-7.84478006743251));
#131837=CARTESIAN_POINT('Ctrl Pts',(21.4825790275111,-0.176354286300112,
-7.84766537366112));
#131838=CARTESIAN_POINT('Ctrl Pts',(21.4405270143201,-0.158695683813985,
-7.85065495522489));
#131839=CARTESIAN_POINT('Ctrl Pts',(21.3995078813328,-0.138764776674,-7.85368973772408));
#131840=CARTESIAN_POINT('Ctrl Pts',(21.3946563001692,-0.136407427636807,
-7.85404867982101));
#131841=CARTESIAN_POINT('Ctrl Pts',(21.3898192004068,-0.134018341350694,
-7.85440825424399));
#131842=CARTESIAN_POINT('Ctrl Pts',(21.3849970490046,-0.131597763031438,
-7.85476836324909));
#131843=CARTESIAN_POINT('Ctrl Pts',(21.3410412664877,-0.109533251718649,
-7.85805089666417));
#131844=CARTESIAN_POINT('Ctrl Pts',(21.298323773979,-0.0848475209218615,
-7.86137731033211));
#131845=CARTESIAN_POINT('Ctrl Pts',(21.2571506329473,-0.0577321201817723,
-7.86468830172209));
#131846=CARTESIAN_POINT('Ctrl Pts',(21.2160152298865,-0.0306415725419846,
-7.86799625836432));
#131847=CARTESIAN_POINT('Ctrl Pts',(21.1764211356863,-0.00112603449223744,
-7.87128852432434));
#131848=CARTESIAN_POINT('Ctrl Pts',(21.1386471893365,0.0305959184157649,
-7.87452705674012));
#131849=CARTESIAN_POINT('Ctrl Pts',(21.1008913766293,0.0623026429823067,
-7.87776403447615));
#131850=CARTESIAN_POINT('Ctrl Pts',(21.0649539086597,0.0962135978617711,
-7.88094722892417));
#131851=CARTESIAN_POINT('Ctrl Pts',(21.0310888726463,0.132085078356058,
-7.88406264585824));
#131852=CARTESIAN_POINT('Ctrl Pts',(20.9972253119952,0.167954996075296,
-7.88717792706622));
#131853=CARTESIAN_POINT('Ctrl Pts',(20.9654340915415,0.205785287335624,
-7.89022547658388));
#131854=CARTESIAN_POINT('Ctrl Pts',(20.9359446440149,0.245307147566483,
-7.89321573672232));
#131855=CARTESIAN_POINT('Ctrl Pts',(20.9064227100348,0.284872546255351,
-7.89620929102037));
#131856=CARTESIAN_POINT('Ctrl Pts',(20.879207857653,0.326133326423576,-7.8991456086336));
#131857=CARTESIAN_POINT('Ctrl Pts',(20.8545031866989,0.36879381969754,-7.9020580457105));
#131858=CARTESIAN_POINT('Ctrl Pts',(20.8297821097013,0.411482643237868,
-7.90497241689815));
#131859=CARTESIAN_POINT('Ctrl Pts',(20.8075749656334,0.455573153364719,
-7.90786324835844));
#131860=CARTESIAN_POINT('Ctrl Pts',(20.7880533274443,0.500741568539848,
-7.91078278219348));
#131861=CARTESIAN_POINT('Ctrl Pts',(20.7697789351712,0.543024154113446,
-7.91351578574777));
#131862=CARTESIAN_POINT('Ctrl Pts',(20.7538579722341,0.586251759290134,
-7.91627449720688));
#131863=CARTESIAN_POINT('Ctrl Pts',(20.740399740493,0.630133950092345,-7.91911105232861));
#131864=CARTESIAN_POINT('Ctrl Pts',(20.739454434309,0.633216235130161,-7.9193102919575));
#131865=CARTESIAN_POINT('Ctrl Pts',(20.7385212621352,0.636301763516945,
-7.91950991564037));
#131866=CARTESIAN_POINT('Ctrl Pts',(20.7376002546373,0.639390441086892,
-7.91970994144433));
#131867=CARTESIAN_POINT('Ctrl Pts',(20.7339326743821,0.651689985765733,
-7.92050647208148));
#131868=CARTESIAN_POINT('Ctrl Pts',(20.7304580418358,0.664039060394589,
-7.92130940854894));
#131869=CARTESIAN_POINT('Ctrl Pts',(20.7271781638064,0.676431015095323,
-7.92211992207834));
#131870=CARTESIAN_POINT('Ctrl Pts',(20.7271743568322,0.676445398511668,
-7.92212086284627));
#131871=CARTESIAN_POINT('Ctrl Pts',(20.7271705501204,0.676459781985813,
-7.92212180362441));
#131872=CARTESIAN_POINT('Ctrl Pts',(20.7271667436709,0.676474165517736,
-7.92212274441275));
#131873=CARTESIAN_POINT('Ctrl Pts',(20.7145136658905,0.724286687274377,
-7.92525003355821));
#131874=CARTESIAN_POINT('Ctrl Pts',(20.7047344388994,0.772850328217294,
-7.92849442468279));
#131875=CARTESIAN_POINT('Ctrl Pts',(20.6978549531996,0.821872855167937,
-7.93179039624007));
#131876=CARTESIAN_POINT('Ctrl Pts',(20.6956260182459,0.837756022690157,
-7.9328582822029));
#131877=CARTESIAN_POINT('Ctrl Pts',(20.6937015692772,0.853686960859425,
-7.93393158278377));
#131878=CARTESIAN_POINT('Ctrl Pts',(20.6920826480587,0.869654568896896,
-7.9350080695044));
#131879=CARTESIAN_POINT('Ctrl Pts',(20.6877513941166,0.912374229662736,
-7.93788809683325));
#131880=CARTESIAN_POINT('Ctrl Pts',(20.6856051097385,0.955362919347453,
-7.94079142940216));
#131881=CARTESIAN_POINT('Ctrl Pts',(20.6856550625054,0.998431907182509,
-7.94368587507956));
#131882=CARTESIAN_POINT('',(20.9918838262563,1.82521129893649,-8.00000000000001));
#131883=CARTESIAN_POINT('Ctrl Pts',(20.6855009578283,0.998426624634692,
-7.943774545494));
#131884=CARTESIAN_POINT('Ctrl Pts',(20.6854347818123,1.05161133140669,-7.94742215375545));
#131885=CARTESIAN_POINT('Ctrl Pts',(20.6887240589389,1.1047510902817,-7.95103786349476));
#131886=CARTESIAN_POINT('Ctrl Pts',(20.6953507587871,1.15752962982536,-7.95457609541917));
#131887=CARTESIAN_POINT('Ctrl Pts',(20.6993094976487,1.18905911815829,-7.95668980760494));
#131888=CARTESIAN_POINT('Ctrl Pts',(20.7044555563998,1.2204299808716,-7.95877460230176));
#131889=CARTESIAN_POINT('Ctrl Pts',(20.7107784821558,1.25157569797626,-7.96082752239111));
#131890=CARTESIAN_POINT('Ctrl Pts',(20.7169430191148,1.28194121729719,-7.96282901699239));
#131891=CARTESIAN_POINT('Ctrl Pts',(20.7242219132126,1.31207161227981,-7.96479884775945));
#131892=CARTESIAN_POINT('Ctrl Pts',(20.7326009343683,1.34190615113201,-7.96673892557842));
#131893=CARTESIAN_POINT('Ctrl Pts',(20.7418217164266,1.3747378835567,-7.9688739046425));
#131894=CARTESIAN_POINT('Ctrl Pts',(20.7523673405614,1.4071848917607,-7.970971063412));
#131895=CARTESIAN_POINT('Ctrl Pts',(20.7642125622979,1.43916790916664,-7.97303914742824));
#131896=CARTESIAN_POINT('Ctrl Pts',(20.777679644269,1.47553007499761,-7.97539039568592));
#131897=CARTESIAN_POINT('Ctrl Pts',(20.7928126393162,1.51125486619278,-7.97770151418053));
#131898=CARTESIAN_POINT('Ctrl Pts',(20.8095641954328,1.54622932327752,-7.97999472541712));
#131899=CARTESIAN_POINT('Ctrl Pts',(20.8480280883029,1.6265355205727,-7.98526025601735));
#131900=CARTESIAN_POINT('Ctrl Pts',(20.8948635669814,1.70254792840251,-7.99039904379838));
#131901=CARTESIAN_POINT('Ctrl Pts',(20.9492881987892,1.77300464616334,-7.99582841388747));
#131902=CARTESIAN_POINT('Ctrl Pts',(20.9630213219082,1.79078319141818,-7.99719842238208));
#131903=CARTESIAN_POINT('Ctrl Pts',(20.977224964316,1.80819154602769,-7.99858640426953));
#131904=CARTESIAN_POINT('Ctrl Pts',(20.9918838262562,1.82521129893648,-8.00000000000004));
#131905=CARTESIAN_POINT('',(22.898512696641,1.83623195013869,-8.00000000000001));
#131906=CARTESIAN_POINT('Origin',(21.9499999789786,0.999999999999992,-8.00000000000001));
#131907=CARTESIAN_POINT('Ctrl Pts',(22.8985126966416,1.83623195013798,-8.00000000000009));
#131908=CARTESIAN_POINT('Ctrl Pts',(22.8436297891941,1.89848397924026,-7.99445558980496));
#131909=CARTESIAN_POINT('Ctrl Pts',(22.7827601951912,1.95517447097983,-7.98871488534317));
#131910=CARTESIAN_POINT('Ctrl Pts',(22.671656060386,2.03989960638361,-7.97926197537341));
#131911=CARTESIAN_POINT('Ctrl Pts',(22.624276631408,2.07122875529249,-7.97548954756314));
#131912=CARTESIAN_POINT('Ctrl Pts',(22.5489424976922,2.11405698150326,-7.96989091770804));
#131913=CARTESIAN_POINT('Ctrl Pts',(22.5224192930673,2.1279146503469,-7.9679887303622));
#131914=CARTESIAN_POINT('Ctrl Pts',(22.4678037755625,2.15402642253875,-7.96420091867253));
#131915=CARTESIAN_POINT('Ctrl Pts',(22.4397078143008,2.16622648734987,-7.96231802136835));
#131916=CARTESIAN_POINT('Ctrl Pts',(22.3483030827951,2.20203042654509,-7.95637196138385));
#131917=CARTESIAN_POINT('Ctrl Pts',(22.2835361641471,2.22158803589501,-7.95243349309627));
#131918=CARTESIAN_POINT('Ctrl Pts',(22.1634086356694,2.24759019110203,-7.94531500915695));
#131919=CARTESIAN_POINT('Ctrl Pts',(22.1085972633573,2.25573521532646,-7.94213191053803));
#131920=CARTESIAN_POINT('Ctrl Pts',(22.0204967723728,2.2629657330336,-7.93690735040823));
#131921=CARTESIAN_POINT('Ctrl Pts',(21.9874714986606,2.26437643676886,-7.93492418251912));
#131922=CARTESIAN_POINT('Ctrl Pts',(21.9372952307496,2.26455229355907,-7.9318250472819));
#131923=CARTESIAN_POINT('Ctrl Pts',(21.9201600093796,2.26426400218925,-7.93075116236837));
#131924=CARTESIAN_POINT('Ctrl Pts',(21.8821002210124,2.26284946843498,-7.92832303891685));
#131925=CARTESIAN_POINT('Ctrl Pts',(21.8611885250819,2.26155125263614,-7.92696163658804));
#131926=CARTESIAN_POINT('Ctrl Pts',(21.7418236175042,2.25115865318114,-7.9190684694165));
#131927=CARTESIAN_POINT('Ctrl Pts',(21.6446749578416,2.23106139711964,-7.9121985977141));
#131928=CARTESIAN_POINT('Ctrl Pts',(21.5004156162989,2.18307241377343,-7.9019463906592));
#131929=CARTESIAN_POINT('Ctrl Pts',(21.451075543509,2.16312595231789,-7.89842329015815));
#131930=CARTESIAN_POINT('Ctrl Pts',(21.3765731557395,2.12739063021314,-7.89309421447382));
#131931=CARTESIAN_POINT('Ctrl Pts',(21.3504652919219,2.11372632868274,-7.89122413009542));
#131932=CARTESIAN_POINT('Ctrl Pts',(21.2982131874887,2.08400818107004,-7.88746856761019));
#131933=CARTESIAN_POINT('Ctrl Pts',(21.2721279179092,2.06789018985442,-7.88558682154398));
#131934=CARTESIAN_POINT('Ctrl Pts',(21.1887889082,2.01210973217063,-7.87952405427109));
#131935=CARTESIAN_POINT('Ctrl Pts',(21.1342206196968,1.9686659641545,-7.87547928913312));
#131936=CARTESIAN_POINT('Ctrl Pts',(21.029555947919,1.87018938372836,-7.86718547274263));
#131937=CARTESIAN_POINT('Ctrl Pts',(20.9801783651624,1.81479496458115,-7.86295438941036));
#131938=CARTESIAN_POINT('Ctrl Pts',(20.9225130888004,1.73738447022363,-7.85713500106844));
#131939=CARTESIAN_POINT('Ctrl Pts',(20.9095730760053,1.71901104711099,-7.85575932754119));
#131940=CARTESIAN_POINT('Ctrl Pts',(20.888053032726,1.68665681085156,-7.85332857558938));
#131941=CARTESIAN_POINT('Ctrl Pts',(20.8792433408731,1.67283654808712,-7.85228673397135));
#131942=CARTESIAN_POINT('Ctrl Pts',(20.8564682921383,1.63552756321596,-7.84946679521615));
#131943=CARTESIAN_POINT('Ctrl Pts',(20.8429923877664,1.61175223623375,-7.84766400755591));
#131944=CARTESIAN_POINT('Ctrl Pts',(20.7887603372009,1.50840344764925,-7.83985828040673));
#131945=CARTESIAN_POINT('Ctrl Pts',(20.7557334390164,1.4250644966225,-7.83366120327489));
#131946=CARTESIAN_POINT('Ctrl Pts',(20.718106760785,1.28982428891886,-7.82420566388658));
#131947=CARTESIAN_POINT('Ctrl Pts',(20.7074237869657,1.23992593849276,-7.82083232495627));
#131948=CARTESIAN_POINT('Ctrl Pts',(20.6954260977827,1.16077739579424,-7.815673277277));
#131949=CARTESIAN_POINT('Ctrl Pts',(20.6920619229972,1.13189790239961,-7.81382948887018));
#131950=CARTESIAN_POINT('Ctrl Pts',(20.6872141936175,1.07253872181825,-7.81011122168199));
#131951=CARTESIAN_POINT('Ctrl Pts',(20.6858322030414,1.04206980797261,-7.80824092476375));
#131952=CARTESIAN_POINT('Ctrl Pts',(20.6848879644734,0.938954808434391,
-7.80201185032114));
#131953=CARTESIAN_POINT('Ctrl Pts',(20.69048063927,0.866406014374577,-7.79780630718665));
#131954=CARTESIAN_POINT('Ctrl Pts',(20.7137856495591,0.724745150124373,
-7.78953253434507));
#131955=CARTESIAN_POINT('Ctrl Pts',(20.7311666888633,0.655856579929814,
-7.785475299777));
#131956=CARTESIAN_POINT('Ctrl Pts',(20.7614715598617,0.567730836360711,
-7.77985854089706));
#131957=CARTESIAN_POINT('Ctrl Pts',(20.7692700943263,0.546862896536249,
-7.77849508982802));
#131958=CARTESIAN_POINT('Ctrl Pts',(20.7837550108444,0.511019980259353,
-7.77607723801927));
#131959=CARTESIAN_POINT('Ctrl Pts',(20.7901887667071,0.495949766780783,
-7.7750356607319));
#131960=CARTESIAN_POINT('Ctrl Pts',(20.8081789253604,0.455979466985741,
-7.77220841384106));
#131961=CARTESIAN_POINT('Ctrl Pts',(20.8202557382879,0.431324891264073,
-7.77039770220559));
#131962=CARTESIAN_POINT('Ctrl Pts',(20.8707345097507,0.336237906654735,
-7.76319912609828));
#131963=CARTESIAN_POINT('Ctrl Pts',(20.9149998996471,0.269131350926939,
-7.75765584879279));
#131964=CARTESIAN_POINT('Ctrl Pts',(20.9908243496453,0.175018505162643,
-7.7494751762915));
#131965=CARTESIAN_POINT('Ctrl Pts',(21.017838006586,0.144613032116268,-7.74675494863844));
#131966=CARTESIAN_POINT('Ctrl Pts',(21.0705061472736,0.0907962843073573,
-7.74180810659167));
#131967=CARTESIAN_POINT('Ctrl Pts',(21.0957500988475,0.067037892260422,
-7.73956977879915));
#131968=CARTESIAN_POINT('Ctrl Pts',(21.1432732656925,0.0258598407101029,
-7.73558275663927));
#131969=CARTESIAN_POINT('Ctrl Pts',(21.1652205008591,0.00809355188603256,
-7.73382123769572));
#131970=CARTESIAN_POINT('Ctrl Pts',(21.2188884667804,-0.0324532458505455,
-7.7296866137588));
#131971=CARTESIAN_POINT('Ctrl Pts',(21.2511059609009,-0.0545289526710269,
-7.72734010877895));
#131972=CARTESIAN_POINT('Ctrl Pts',(21.3609982179887,-0.122575735708734,
-7.71969304827861));
#131973=CARTESIAN_POINT('Ctrl Pts',(21.44256021831,-0.161724533487817,-7.7145931898283));
#131974=CARTESIAN_POINT('Ctrl Pts',(21.5550025599966,-0.201575194328529,
-7.70762359246858));
#131975=CARTESIAN_POINT('Ctrl Pts',(21.5827377485318,-0.2103405208425,-7.70590705870495));
#131976=CARTESIAN_POINT('Ctrl Pts',(21.6325257859147,-0.224206440471404,
-7.70279233426908));
#131977=CARTESIAN_POINT('Ctrl Pts',(21.6544600491531,-0.229685846040324,
-7.70140885883999));
#131978=CARTESIAN_POINT('Ctrl Pts',(21.6925861538772,-0.238131211479962,
-7.69896668246375));
#131979=CARTESIAN_POINT('Ctrl Pts',(21.7087099162753,-0.2413741514721,-7.69792142887289));
#131980=CARTESIAN_POINT('Ctrl Pts',(21.7518898290421,-0.249185878852511,
-7.69509120283369));
#131981=CARTESIAN_POINT('Ctrl Pts',(21.7790375430942,-0.253189772976175,
-7.69328140865882));
#131982=CARTESIAN_POINT('Ctrl Pts',(21.8859837724665,-0.265423285936066,
-7.68608407919356));
#131983=CARTESIAN_POINT('Ctrl Pts',(21.9663611635882,-0.266935892379982,
-7.68054105196579));
#131984=CARTESIAN_POINT('Ctrl Pts',(22.1035214894421,-0.256455405429357,
-7.67123043782603));
#131985=CARTESIAN_POINT('Ctrl Pts',(22.1603447271469,-0.24820091625219,
-7.6674143525328));
#131986=CARTESIAN_POINT('Ctrl Pts',(22.2454479735416,-0.229858796370244,
-7.66178860471871));
#131987=CARTESIAN_POINT('Ctrl Pts',(22.2742508618983,-0.222580782403874,
-7.65989970020417));
#131988=CARTESIAN_POINT('Ctrl Pts',(22.3316239329181,-0.205912954943925,
-7.65616076192792));
#131989=CARTESIAN_POINT('Ctrl Pts',(22.3601688331301,-0.196505172665629,
-7.65431265162712));
#131990=CARTESIAN_POINT('Ctrl Pts',(22.3891067506122,-0.185810329809031,
-7.6524436839551));
#131991=CARTESIAN_POINT('Ctrl Pts',(22.3898598818392,-0.185531172491713,
-7.65239504564353));
#131992=CARTESIAN_POINT('Ctrl Pts',(22.3906127226216,-0.185251306744424,
-7.65234642888876));
#131993=CARTESIAN_POINT('Origin',(21.9499999789786,0.999999999999992,-6.00000000000001));
#131994=CARTESIAN_POINT('',(22.3906127229457,-0.185251306623939,-7.15421791561113));
#131995=CARTESIAN_POINT('',(22.3906403691454,-0.185356836028299,-7.28986813301021));
#131996=CARTESIAN_POINT('',(22.3906127231008,-0.185251306566283,-6.00000000000001));
#131997=CARTESIAN_POINT('',(20.6854351050354,1.00099360643116,-7.4433066090729));
#131998=CARTESIAN_POINT('Ctrl Pts',(22.3906403684231,-0.185356836298634,
-7.28986813305573));
#131999=CARTESIAN_POINT('Ctrl Pts',(22.3440517461525,-0.202794827868046,
-7.29280460895284));
#132000=CARTESIAN_POINT('Ctrl Pts',(22.2964803100234,-0.217456218389545,
-7.2957499216459));
#132001=CARTESIAN_POINT('Ctrl Pts',(22.2482864098299,-0.229219763841232,
-7.29876435271249));
#132002=CARTESIAN_POINT('Ctrl Pts',(22.217446148307,-0.236747496950825,
-7.30069334874856));
#132003=CARTESIAN_POINT('Ctrl Pts',(22.1863515382631,-0.243089361282193,
-7.30265094181487));
#132004=CARTESIAN_POINT('Ctrl Pts',(22.15510248789,-0.248224054371781,-7.30465409393146));
#132005=CARTESIAN_POINT('Ctrl Pts',(22.1550857866994,-0.248226798630788,
-7.30465516452481));
#132006=CARTESIAN_POINT('Ctrl Pts',(22.1550690854644,-0.248229542545221,
-7.30465623513116));
#132007=CARTESIAN_POINT('Ctrl Pts',(22.1550523841852,-0.248232286115091,
-7.30465730575054));
#132008=CARTESIAN_POINT('Ctrl Pts',(22.109765840256,-0.255671644239026,
-7.30756035590221));
#132009=CARTESIAN_POINT('Ctrl Pts',(22.0639887458557,-0.260596991460554,
-7.31056645868888));
#132010=CARTESIAN_POINT('Ctrl Pts',(22.0180204829633,-0.262988013273262,
-7.31361650791182));
#132011=CARTESIAN_POINT('Ctrl Pts',(22.0130719410616,-0.263245409809123,
-7.31394484958566));
#132012=CARTESIAN_POINT('Ctrl Pts',(22.0081212276411,-0.263473459992872,
-7.3142737005458));
#132013=CARTESIAN_POINT('Ctrl Pts',(22.0031687473583,-0.263672156307481,
-7.31460298705436));
#132014=CARTESIAN_POINT('Ctrl Pts',(21.9536334923752,-0.265659538799975,
-7.31789654709556));
#132015=CARTESIAN_POINT('Ctrl Pts',(21.9039160545772,-0.264708195030253,
-7.32123313004558));
#132016=CARTESIAN_POINT('Ctrl Pts',(21.854382158871,-0.260838706472937,
-7.32455398111115));
#132017=CARTESIAN_POINT('Ctrl Pts',(21.8048944344205,-0.256972824721493,
-7.32787173676373));
#132018=CARTESIAN_POINT('Ctrl Pts',(21.7555898162755,-0.250194536762391,
-7.33117349636671));
#132019=CARTESIAN_POINT('Ctrl Pts',(21.7068231680761,-0.240561070008607,
-7.3344220800825));
#132020=CARTESIAN_POINT('Ctrl Pts',(21.6580816294929,-0.230932563461495,
-7.33766899112458));
#132021=CARTESIAN_POINT('Ctrl Pts',(21.6098774738854,-0.218451892946313,
-7.34086268598225));
#132022=CARTESIAN_POINT('Ctrl Pts',(21.5625561924181,-0.203210155758827,
-7.34399027737459));
#132023=CARTESIAN_POINT('Ctrl Pts',(21.512757336974,-0.187170415426774,
-7.34728161832744));
#132024=CARTESIAN_POINT('Ctrl Pts',(21.463936382959,-0.168072485624941,
-7.35049957206803));
#132025=CARTESIAN_POINT('Ctrl Pts',(21.4164851980655,-0.146063276856775,
-7.35365846723112));
#132026=CARTESIAN_POINT('Ctrl Pts',(21.3713552082722,-0.125130704376378,
-7.35666283702268));
#132027=CARTESIAN_POINT('Ctrl Pts',(21.3274643368433,-0.101564802796739,
-7.35961420736341));
#132028=CARTESIAN_POINT('Ctrl Pts',(21.2851387168268,-0.0755293390491522,
-7.36254816026591));
#132029=CARTESIAN_POINT('Ctrl Pts',(21.2427874543799,-0.0494781020520178,
-7.36548389066589));
#132030=CARTESIAN_POINT('Ctrl Pts',(21.2020036753296,-0.0209539720715463,
-7.3684025954985));
#132031=CARTESIAN_POINT('Ctrl Pts',(21.1630996744432,0.00983828316542695,
-7.37135798185939));
#132032=CARTESIAN_POINT('Ctrl Pts',(21.1271805269864,0.0382680469734418,
-7.37408662045877));
#132033=CARTESIAN_POINT('Ctrl Pts',(21.0928635577385,0.0686317094549675,
-7.37684711524653));
#132034=CARTESIAN_POINT('Ctrl Pts',(21.0603798066664,0.100731383818771,
-7.37968948029064));
#132035=CARTESIAN_POINT('Ctrl Pts',(21.057622289732,0.103456296820673,-7.37993076614847));
#132036=CARTESIAN_POINT('Ctrl Pts',(21.0548779525668,0.106193724953976,
-7.38017264197664));
#132037=CARTESIAN_POINT('Ctrl Pts',(21.0521469194695,0.108943550494673,
-7.38041513836999));
#132038=CARTESIAN_POINT('Ctrl Pts',(21.046885270883,0.114241404879535,-7.38088233549279));
#132039=CARTESIAN_POINT('Ctrl Pts',(21.0416730872256,0.119585160851676,
-7.38135184194807));
#132040=CARTESIAN_POINT('Ctrl Pts',(21.0365113105743,0.124973855152702,
-7.38182387855428));
#132041=CARTESIAN_POINT('Ctrl Pts',(21.0364995820756,0.124986099249765,
-7.38182495110761));
#132042=CARTESIAN_POINT('Ctrl Pts',(21.036487853837,0.124998343578842,-7.381826023674));
#132043=CARTESIAN_POINT('Ctrl Pts',(21.0364761258587,0.125010588139904,
-7.38182709625346));
#132044=CARTESIAN_POINT('Ctrl Pts',(21.0050835186137,0.157785946906783,
-7.38469809966508));
#132045=CARTESIAN_POINT('Ctrl Pts',(20.9754384365615,0.192357167576284,
-7.38767062125446));
#132046=CARTESIAN_POINT('Ctrl Pts',(20.9477272918121,0.228494563598768,
-7.39068712703531));
#132047=CARTESIAN_POINT('Ctrl Pts',(20.9456263670576,0.231234325905718,
-7.39091582389083));
#132048=CARTESIAN_POINT('Ctrl Pts',(20.9435365602325,0.233983065747832,
-7.39114477356475));
#132049=CARTESIAN_POINT('Ctrl Pts',(20.9414579531322,0.236740670872581,
-7.39137395098486));
#132050=CARTESIAN_POINT('Ctrl Pts',(20.9120040321276,0.275816012956855,
-7.39462140146588));
#132051=CARTESIAN_POINT('Ctrl Pts',(20.8847980747372,0.316676796555248,
-7.3979140006635));
#132052=CARTESIAN_POINT('Ctrl Pts',(20.8600293289857,0.359018625118562,
-7.40119405356233));
#132053=CARTESIAN_POINT('Ctrl Pts',(20.8352843205297,0.40131987510317,-7.4044709630002));
#132054=CARTESIAN_POINT('Ctrl Pts',(20.812971582611,0.445099194933415,-7.40773505376474));
#132055=CARTESIAN_POINT('Ctrl Pts',(20.7932434164791,0.490039494436445,
-7.41094889565801));
#132056=CARTESIAN_POINT('Ctrl Pts',(20.7735180069206,0.534973514530128,
-7.41416228848821));
#132057=CARTESIAN_POINT('Ctrl Pts',(20.7563763761227,0.581068128698808,
-7.41732534313056));
#132058=CARTESIAN_POINT('Ctrl Pts',(20.7419368779796,0.627994199072142,
-7.42042367767064));
#132059=CARTESIAN_POINT('Ctrl Pts',(20.7274989405527,0.674915197366821,
-7.42352167732232));
#132060=CARTESIAN_POINT('Ctrl Pts',(20.7157626383642,0.72266742180228,-7.42655501240717));
#132061=CARTESIAN_POINT('Ctrl Pts',(20.7068122566636,0.770910467044918,
-7.42953277296501));
#132062=CARTESIAN_POINT('Ctrl Pts',(20.697852973447,0.819201491944744,-7.43251349502601));
#132063=CARTESIAN_POINT('Ctrl Pts',(20.6916853913536,0.867984253049784,
-7.4354387127125));
#132064=CARTESIAN_POINT('Ctrl Pts',(20.6883575187536,0.916906744626067,
-7.43833941828639));
#132065=CARTESIAN_POINT('Ctrl Pts',(20.686452467469,0.944912580975547,-7.43999993644446));
#132066=CARTESIAN_POINT('Ctrl Pts',(20.6854773133495,0.972964015475198,
-7.44165281629599));
#132067=CARTESIAN_POINT('Ctrl Pts',(20.6854351050355,1.00099360637425,-7.44330660906956));
#132068=CARTESIAN_POINT('Ctrl Pts',(20.6854351050347,1.00099360693951,-7.44330660910288));
#132069=CARTESIAN_POINT('Ctrl Pts',(20.6853606881594,1.05041219279047,-7.44622238837541));
#132070=CARTESIAN_POINT('Ctrl Pts',(20.6881872209223,1.09973540379018,-7.44913841382896));
#132071=CARTESIAN_POINT('Ctrl Pts',(20.6938991273629,1.14865874359727,-7.4521175879256));
#132072=CARTESIAN_POINT('Ctrl Pts',(20.6959601823621,1.16631199039665,-7.45319257781373));
#132073=CARTESIAN_POINT('Ctrl Pts',(20.6983970294421,1.18391365320077,-7.45427578976892));
#132074=CARTESIAN_POINT('Ctrl Pts',(20.7012094620179,1.20145101245753,-7.45537017903375));
#132075=CARTESIAN_POINT('Ctrl Pts',(20.7042769785817,1.22057898745944,-7.45656382798587));
#132076=CARTESIAN_POINT('Ctrl Pts',(20.70779063137,1.23962909537417,-7.45777096884554));
#132077=CARTESIAN_POINT('Ctrl Pts',(20.7117486726152,1.25858259994124,-7.45899574224935));
#132078=CARTESIAN_POINT('Ctrl Pts',(20.7117521352302,1.25859918104416,-7.45899681371842));
#132079=CARTESIAN_POINT('Ctrl Pts',(20.7117555981854,1.25861576207324,-7.45899788520098));
#132080=CARTESIAN_POINT('Ctrl Pts',(20.7117590614805,1.25863234302847,-7.45899895669704));
#132081=CARTESIAN_POINT('Ctrl Pts',(20.7211417365784,1.30355306361916,-7.46190182775864));
#132082=CARTESIAN_POINT('Ctrl Pts',(20.7330459087108,1.34802523649897,-7.46490780513171));
#132083=CARTESIAN_POINT('Ctrl Pts',(20.7473826374716,1.3917623628161,-7.4679578018695));
#132084=CARTESIAN_POINT('Ctrl Pts',(20.7489269335377,1.39647355413732,-7.46828633552891));
#132085=CARTESIAN_POINT('Ctrl Pts',(20.7504994162171,1.4011761843785,-7.46861537993406));
#132086=CARTESIAN_POINT('Ctrl Pts',(20.7520999464277,1.40586987280228,-7.46894486123794));
#132087=CARTESIAN_POINT('Ctrl Pts',(20.768101593778,1.45279603916396,-7.47223892191749));
#132088=CARTESIAN_POINT('Ctrl Pts',(20.7869106309768,1.49883273151624,-7.47557610128714));
#132089=CARTESIAN_POINT('Ctrl Pts',(20.8083759978131,1.54364616741722,-7.47889761510544));
#132090=CARTESIAN_POINT('Ctrl Pts',(20.8298213296407,1.58841777605368,-7.48221602874108));
#132091=CARTESIAN_POINT('Ctrl Pts',(20.8539177874338,1.63196860702536,-7.48551851215197));
#132092=CARTESIAN_POINT('Ctrl Pts',(20.8804840426551,1.67398823042049,-7.48876784757917));
#132093=CARTESIAN_POINT('Ctrl Pts',(20.9070365793477,1.71598615533367,-7.49201550508447));
#132094=CARTESIAN_POINT('Ctrl Pts',(20.9360563049012,1.75645451207017,-7.49520997419177));
#132095=CARTESIAN_POINT('Ctrl Pts',(20.9673336789034,1.79510382822157,-7.49833832604472));
#132096=CARTESIAN_POINT('Ctrl Pts',(21.0002428909582,1.83576959961621,-7.50162989376083));
#132097=CARTESIAN_POINT('Ctrl Pts',(21.0356518211773,1.87442126512674,-7.50484808522027));
#132098=CARTESIAN_POINT('Ctrl Pts',(21.0732822976041,1.91074636611629,-7.50800716965886));
#132099=CARTESIAN_POINT('Ctrl Pts',(21.109078030499,1.94530036956959,-7.5110122270882));
#132100=CARTESIAN_POINT('Ctrl Pts',(21.1468838455241,1.97774910464242,-7.51396422222195));
#132101=CARTESIAN_POINT('Ctrl Pts',(21.1864294111691,2.00784734685896,-7.51689869185879));
#132102=CARTESIAN_POINT('Ctrl Pts',(21.2259988566345,2.03796376407449,-7.51983493349222));
#132103=CARTESIAN_POINT('Ctrl Pts',(21.2673103486457,2.0657264150824,-7.52275404115145));
#132104=CARTESIAN_POINT('Ctrl Pts',(21.3100603053001,2.09091775667308,-7.52570968175975));
#132105=CARTESIAN_POINT('Ctrl Pts',(21.3495366765676,2.11418006688782,-7.52843899367297));
#132106=CARTESIAN_POINT('Ctrl Pts',(21.3902401526173,2.13524982412564,-7.53120004496706));
#132107=CARTESIAN_POINT('Ctrl Pts',(21.4319027378402,2.15398273504556,-7.53404285055596));
#132108=CARTESIAN_POINT('Ctrl Pts',(21.4354320126832,2.15556961667789,-7.53428366715902));
#132109=CARTESIAN_POINT('Ctrl Pts',(21.4389681858387,2.15713975591571,-7.53452507042564));
#132110=CARTESIAN_POINT('Ctrl Pts',(21.4425111035855,2.1586930796388,-7.53476709075887));
#132111=CARTESIAN_POINT('Ctrl Pts',(21.4493265365929,2.16168117434781,-7.53523265995508));
#132112=CARTESIAN_POINT('Ctrl Pts',(21.4561667916288,2.1646070078569,-7.53570051850504));
#132113=CARTESIAN_POINT('Ctrl Pts',(21.4630306434348,2.16747005383963,-7.53617088487625));
#132114=CARTESIAN_POINT('Ctrl Pts',(21.4630461964787,2.1674765413165,-7.536171950696));
#132115=CARTESIAN_POINT('Ctrl Pts',(21.4630617496438,2.16748302847101,-7.53617301652863));
#132116=CARTESIAN_POINT('Ctrl Pts',(21.46307730293,2.16748951530316,-7.53617408237413));
#132117=CARTESIAN_POINT('Ctrl Pts',(21.5054518069055,2.18516271254244,-7.53907794937767));
#132118=CARTESIAN_POINT('Ctrl Pts',(21.5488831083792,2.20050047344378,-7.54208476489056));
#132119=CARTESIAN_POINT('Ctrl Pts',(21.5930842430634,2.21341406344646,-7.54513539763158));
#132120=CARTESIAN_POINT('Ctrl Pts',(21.5978233774849,2.2147986260674,-7.54546247879666));
#132121=CARTESIAN_POINT('Ctrl Pts',(21.6025713138547,2.21615533396418,-7.54579006366657));
#132122=CARTESIAN_POINT('Ctrl Pts',(21.6073276644696,2.21748408778358,-7.54611807936035));
#132123=CARTESIAN_POINT('Ctrl Pts',(21.6550817372542,2.23082486346267,-7.54941137848474));
#132124=CARTESIAN_POINT('Ctrl Pts',(21.7036897457322,2.24134699705942,-7.55274755630456));
#132125=CARTESIAN_POINT('Ctrl Pts',(21.7527909628984,2.24898631868653,-7.55606791454492));
#132126=CARTESIAN_POINT('Ctrl Pts',(21.8018464991694,2.25661853313646,-7.55938518371853));
#132127=CARTESIAN_POINT('Ctrl Pts',(21.8513943492424,2.2613736111464,-7.56268636987707));
#132128=CARTESIAN_POINT('Ctrl Pts',(21.9010759123168,2.26322553102128,-7.56593437146185));
#132129=CARTESIAN_POINT('Ctrl Pts',(21.9507319638335,2.2650764999325,-7.56918070519291));
#132130=CARTESIAN_POINT('Ctrl Pts',(22.000521606279,2.26402737190795,-7.57237381442538));
#132131=CARTESIAN_POINT('Ctrl Pts',(22.050087550098,2.26008723736913,-7.57550090374385));
#132132=CARTESIAN_POINT('Ctrl Pts',(22.1022357163895,2.25594183479411,-7.57879090411957));
#132133=CARTESIAN_POINT('Ctrl Pts',(22.1541362151734,2.24859589686446,-7.58200764778882));
#132134=CARTESIAN_POINT('Ctrl Pts',(22.2053740476789,2.23810210760964,-7.58516556324541));
#132135=CARTESIAN_POINT('Ctrl Pts',(22.2541175370563,2.2281191735147,-7.58816974611158));
#132136=CARTESIAN_POINT('Ctrl Pts',(22.3022612073645,2.21528748032301,-7.59112111119599));
#132137=CARTESIAN_POINT('Ctrl Pts',(22.3494498385149,2.19969130365015,-7.59405532906684));
#132138=CARTESIAN_POINT('Ctrl Pts',(22.3966670638231,2.18408567640569,-7.59699132493987));
#132139=CARTESIAN_POINT('Ctrl Pts',(22.4429278437337,2.1657118074518,-7.59991056701147));
#132140=CARTESIAN_POINT('Ctrl Pts',(22.4878809656186,2.14469709134001,-7.6028668328478));
#132141=CARTESIAN_POINT('Ctrl Pts',(22.529366180175,2.12530355491394,-7.60559503763901));
#132142=CARTESIAN_POINT('Ctrl Pts',(22.5697380353023,2.10366051473313,-7.60835536247661));
#132143=CARTESIAN_POINT('Ctrl Pts',(22.6087263589705,2.07990721782239,-7.61119777667448));
#132144=CARTESIAN_POINT('Ctrl Pts',(22.6120553107308,2.07787908293164,-7.61144047138041));
#132145=CARTESIAN_POINT('Ctrl Pts',(22.6153742075372,2.07583556573303,-7.61168376454307));
#132146=CARTESIAN_POINT('Ctrl Pts',(22.6186828988705,2.07377675361698,-7.61192768726687));
#132147=CARTESIAN_POINT('Ctrl Pts',(22.624990550176,2.06985185775231,-7.61239269875699));
#132148=CARTESIAN_POINT('Ctrl Pts',(22.6312610057396,2.06587146792896,-7.61286000399756));
#132149=CARTESIAN_POINT('Ctrl Pts',(22.6374931440773,2.0618362937874,-7.61332982037423));
#132150=CARTESIAN_POINT('Ctrl Pts',(22.6375075149939,2.06182698893121,-7.61333090374106));
#132151=CARTESIAN_POINT('Ctrl Pts',(22.6375218857067,2.06181768378373,-7.61333198712124));
#132152=CARTESIAN_POINT('Ctrl Pts',(22.6375362562159,2.06180837834495,-7.61333307051478));
#132153=CARTESIAN_POINT('Ctrl Pts',(22.6760163315447,2.03689109935326,-7.61623408568443));
#132154=CARTESIAN_POINT('Ctrl Pts',(22.7131727705318,2.00978722455919,-7.61923826595538));
#132155=CARTESIAN_POINT('Ctrl Pts',(22.7487706957536,1.9806824384814,-7.62228650201306));
#132156=CARTESIAN_POINT('Ctrl Pts',(22.7526465906051,1.97751351529805,-7.62261839333449));
#132157=CARTESIAN_POINT('Ctrl Pts',(22.7565039924891,1.97432091962232,-7.62295080692892));
#132158=CARTESIAN_POINT('Ctrl Pts',(22.7603425867873,1.97110492650524,-7.62328366650101));
#132159=CARTESIAN_POINT('Ctrl Pts',(22.7983076326772,1.93929762498099,-7.62657576458379));
#132160=CARTESIAN_POINT('Ctrl Pts',(22.8344355438025,1.90519639880607,-7.62991093927537));
#132161=CARTESIAN_POINT('Ctrl Pts',(22.8684698064752,1.86906184187726,-7.63323037612235));
#132162=CARTESIAN_POINT('Ctrl Pts',(22.9024723351439,1.83296097729504,-7.63654671788179));
#132163=CARTESIAN_POINT('Ctrl Pts',(22.934385387942,1.79483073315077,-7.63984705746996));
#132164=CARTESIAN_POINT('Ctrl Pts',(22.9639851264058,1.75495155551915,-7.64309411880228));
#132165=CARTESIAN_POINT('Ctrl Pts',(22.9935696890332,1.71509282400997,-7.6463395153607));
#132166=CARTESIAN_POINT('Ctrl Pts',(23.0208433831259,1.67348698760192,-7.64953159260903));
#132167=CARTESIAN_POINT('Ctrl Pts',(23.0456120952103,1.63043326522119,-7.65265733638432));
#132168=CARTESIAN_POINT('Ctrl Pts',(23.0703785031404,1.58738354799096,-7.65578278938164));
#132169=CARTESIAN_POINT('Ctrl Pts',(23.0926403011044,1.5428861967377,-7.65884197039542));
#132170=CARTESIAN_POINT('Ctrl Pts',(23.1122329880627,1.49725945430186,-7.66184640247652));
#132171=CARTESIAN_POINT('Ctrl Pts',(23.1318446678839,1.45158848197234,-7.66485374700992));
#132172=CARTESIAN_POINT('Ctrl Pts',(23.1487817982646,1.40478588088184,-7.66780643108939));
#132173=CARTESIAN_POINT('Ctrl Pts',(23.1629116716654,1.35719047428455,-7.6707387994773));
#132174=CARTESIAN_POINT('Ctrl Pts',(23.1770499431126,1.3095667795047,-7.67367291070928));
#132175=CARTESIAN_POINT('Ctrl Pts',(23.1883771606077,1.26114930976549,-7.67658707921416));
#132176=CARTESIAN_POINT('Ctrl Pts',(23.1967980253659,1.21229778702165,-7.67953413838556));
#132177=CARTESIAN_POINT('Ctrl Pts',(23.2046207261191,1.16691636186671,-7.68227185745146));
#132178=CARTESIAN_POINT('Ctrl Pts',(23.2099351229296,1.1211599033523,-7.68503853732298));
#132179=CARTESIAN_POINT('Ctrl Pts',(23.2127007083018,1.07533422374036,-7.68788493701758));
#132180=CARTESIAN_POINT('Ctrl Pts',(23.2129172043911,1.07174688902004,-7.68810775942936));
#132181=CARTESIAN_POINT('Ctrl Pts',(23.2131180972758,1.06815910911293,-7.68833107037233));
#132182=CARTESIAN_POINT('Ctrl Pts',(23.2133033754879,1.06457101979013,-7.68855489419667));
#132183=CARTESIAN_POINT('Ctrl Pts',(23.2138397980788,1.05418268459507,-7.68920291510772));
#132184=CARTESIAN_POINT('Ctrl Pts',(23.2142453641124,1.04379202600083,-7.68985524985652));
#132185=CARTESIAN_POINT('Ctrl Pts',(23.2145199279081,1.03340268179491,-7.69051249873406));
#132186=CARTESIAN_POINT('Ctrl Pts',(23.2145203733976,1.03338582471378,-7.69051356514378));
#132187=CARTESIAN_POINT('Ctrl Pts',(23.2145208185423,1.03336896763607,-7.69051463156644));
#132188=CARTESIAN_POINT('Ctrl Pts',(23.2145212633422,1.03335211056181,-7.69051569800203));
#132189=CARTESIAN_POINT('Ctrl Pts',(23.2157322627867,0.987457518342025,
-7.69341914531073));
#132190=CARTESIAN_POINT('Ctrl Pts',(23.2143838631422,0.941419993553586,
-7.696425913793));
#132191=CARTESIAN_POINT('Ctrl Pts',(23.2104968860145,0.89553884262516,-7.69947702839088));
#132192=CARTESIAN_POINT('Ctrl Pts',(23.2100805041421,0.890623948891015,
-7.69980387075895));
#132193=CARTESIAN_POINT('Ctrl Pts',(23.2096350206477,0.885710889393794,
-7.70013122200685));
#132194=CARTESIAN_POINT('Ctrl Pts',(23.2091604827784,0.880800060007226,
-7.70045900963963));
#132195=CARTESIAN_POINT('Ctrl Pts',(23.2043858980581,0.831389523005676,
-7.70375706006715));
#132196=CARTESIAN_POINT('Ctrl Pts',(23.1966671585257,0.78219967260526,-7.70709872997302));
#132197=CARTESIAN_POINT('Ctrl Pts',(23.1860747987745,0.733590953170563,
-7.7104251143462));
#132198=CARTESIAN_POINT('Ctrl Pts',(23.1754923989363,0.685027940134408,
-7.71374837094617));
#132199=CARTESIAN_POINT('Ctrl Pts',(23.1620420686208,0.637044828130932,
-7.71705607456978));
#132200=CARTESIAN_POINT('Ctrl Pts',(23.1458291743831,0.58998621565744,-7.72031086711321));
#132201=CARTESIAN_POINT('Ctrl Pts',(23.1296248204055,0.542952391650794,
-7.72356394517098));
#132202=CARTESIAN_POINT('Ctrl Pts',(23.1106608825592,0.496842046723612,
-7.72676407167276));
#132203=CARTESIAN_POINT('Ctrl Pts',(23.0890749877739,0.451985841145882,
-7.7298981806231));
#132204=CARTESIAN_POINT('Ctrl Pts',(23.0664157400106,0.4048991724663,-7.73318813232209));
#132205=CARTESIAN_POINT('Ctrl Pts',(23.0408669082453,0.359194672498317,
-7.73640516982291));
#132206=CARTESIAN_POINT('Ctrl Pts',(23.0126262367103,0.315238760789114,
-7.73956328124471));
#132207=CARTESIAN_POINT('Ctrl Pts',(22.9857011055717,0.273330455399889,
-7.74257427778128));
#132208=CARTESIAN_POINT('Ctrl Pts',(22.9563291669508,0.23301169809954,-7.74553212191393));
#132209=CARTESIAN_POINT('Ctrl Pts',(22.9247173003245,0.194584147349198,
-7.74847216961083));
#132210=CARTESIAN_POINT('Ctrl Pts',(22.8930869336765,0.156134107875608,
-7.75141393789406));
#132211=CARTESIAN_POINT('Ctrl Pts',(22.8592137257373,0.119577866736777,
-7.75433830227743));
#132212=CARTESIAN_POINT('Ctrl Pts',(22.823343318757,0.0851978454080979,
-7.75729874603043));
#132213=CARTESIAN_POINT('Ctrl Pts',(22.7902114398814,0.053442568613225,
-7.76003317454963));
#132214=CARTESIAN_POINT('Ctrl Pts',(22.7553751894399,0.0235437599775924,
-7.76279897204339));
#132215=CARTESIAN_POINT('Ctrl Pts',(22.7190626003208,-0.00429562954898666,
-7.76564603671213));
#132216=CARTESIAN_POINT('Ctrl Pts',(22.7159978115506,-0.0066452788154652,
-7.76588632946007));
#132217=CARTESIAN_POINT('Ctrl Pts',(22.7129224970894,-0.00898028741680565,
-7.76612720110572));
#132218=CARTESIAN_POINT('Ctrl Pts',(22.709836788526,-0.0113005494724608,
-7.76636868164864));
#132219=CARTESIAN_POINT('Ctrl Pts',(22.7041614586551,-0.015568046639597,
-7.7668128200727));
#132220=CARTESIAN_POINT('Ctrl Pts',(22.6984510815102,-0.0197856005600674,
-7.76725902354423));
#132221=CARTESIAN_POINT('Ctrl Pts',(22.6927065844721,-0.0239525210596693,
-7.76770748047895));
#132222=CARTESIAN_POINT('Ctrl Pts',(22.6926933515776,-0.0239621198842663,
-7.76770851353428));
#132223=CARTESIAN_POINT('Ctrl Pts',(22.692680118502,-0.0239717184401977,
-7.76770954660158));
#132224=CARTESIAN_POINT('Ctrl Pts',(22.6926668852454,-0.023981316727459,
-7.76771057968083));
#132225=CARTESIAN_POINT('Ctrl Pts',(22.6554388968025,-0.0509833569147772,
-7.77061685314098));
#132226=CARTESIAN_POINT('Ctrl Pts',(22.6166406046479,-0.0759494362312827,
-7.77362497912796));
#132227=CARTESIAN_POINT('Ctrl Pts',(22.5765325545742,-0.0987262866689894,
-7.77667567508239));
#132228=CARTESIAN_POINT('Ctrl Pts',(22.573441076479,-0.100481897676706,
-7.7769108188927));
#132229=CARTESIAN_POINT('Ctrl Pts',(22.5703418425734,-0.102224502742977,
-7.77714621561684));
#132230=CARTESIAN_POINT('Ctrl Pts',(22.567234984968,-0.103954032305686,
-7.77738183810724));
#132231=CARTESIAN_POINT('Ctrl Pts',(22.5238893488562,-0.128083737812819,
-7.78066914896143));
#132232=CARTESIAN_POINT('Ctrl Pts',(22.4790542550743,-0.149668720445147,
-7.7839998130839));
#132233=CARTESIAN_POINT('Ctrl Pts',(22.4330660295219,-0.168562331668783,
-7.78731510173064));
#132234=CARTESIAN_POINT('Ctrl Pts',(22.4190094916684,-0.174337261189623,
-7.78832843677017));
#132235=CARTESIAN_POINT('Ctrl Pts',(22.4048452798424,-0.179861028530698,
-7.78934047221547));
#132236=CARTESIAN_POINT('Ctrl Pts',(22.3905831448079,-0.185130158742937,
-7.79034991681389));
#132237=CARTESIAN_POINT('Ctrl Pts',(22.3906127226216,-0.185251306744425,
-7.65234642888876));
#132238=CARTESIAN_POINT('Ctrl Pts',(22.4940424169462,-0.146801704427007,
-7.64566717319121));
#132239=CARTESIAN_POINT('Ctrl Pts',(22.5919934936769,-0.0949807286400788,
-7.63944789248604));
#132240=CARTESIAN_POINT('Ctrl Pts',(22.7077125771348,-0.0128315743679774,
-7.63118841723727));
#132241=CARTESIAN_POINT('Ctrl Pts',(22.7327516429826,0.0063925361648165,
-7.62933424545274));
#132242=CARTESIAN_POINT('Ctrl Pts',(22.7753917363593,0.0417428777677298,
-7.6260084691289));
#132243=CARTESIAN_POINT('Ctrl Pts',(22.7933044962324,0.0574685179146428,
-7.62455491237901));
#132244=CARTESIAN_POINT('Ctrl Pts',(22.8227144533301,0.0847973108693356,
-7.62205043756754));
#132245=CARTESIAN_POINT('Ctrl Pts',(22.8344499695325,0.0961334981816853,
-7.62101644374416));
#132246=CARTESIAN_POINT('Ctrl Pts',(22.8639477218394,0.12575213502005,-7.6183269698318));
#132247=CARTESIAN_POINT('Ctrl Pts',(22.8813810725006,0.144348860910135,
-7.61665160440707));
#132248=CARTESIAN_POINT('Ctrl Pts',(22.9513597169633,0.223671251125492,
-7.60960261042078));
#132249=CARTESIAN_POINT('Ctrl Pts',(22.9986229118508,0.288805660495983,
-7.60405383489559));
#132250=CARTESIAN_POINT('Ctrl Pts',(23.060750159107,0.394224365295095,-7.59575737106788));
#132251=CARTESIAN_POINT('Ctrl Pts',(23.0802892046431,0.431513556256866,
-7.59293585966622));
#132252=CARTESIAN_POINT('Ctrl Pts',(23.1127497622266,0.501781882236911,
-7.58784193887245));
#132253=CARTESIAN_POINT('Ctrl Pts',(23.1262158014048,0.534462604559476,
-7.58555598900005));
#132254=CARTESIAN_POINT('Ctrl Pts',(23.1479082255124,0.594085705701977,
-7.58152803989586));
#132255=CARTESIAN_POINT('Ctrl Pts',(23.1566368407822,0.620818967804944,
-7.57977133114387));
#132256=CARTESIAN_POINT('Ctrl Pts',(23.1749937836985,0.684122058989001,
-7.57571453740653));
#132257=CARTESIAN_POINT('Ctrl Pts',(23.1838879440589,0.720877145462882,
-7.57343804270218));
#132258=CARTESIAN_POINT('Ctrl Pts',(23.207917352637,0.844103409480788,-7.56599633376565));
#132259=CARTESIAN_POINT('Ctrl Pts',(23.2157015819628,0.931740373279695,
-7.56102594549));
#132260=CARTESIAN_POINT('Ctrl Pts',(23.2138604855805,1.05125058285275,-7.5540717139137));
#132261=CARTESIAN_POINT('Ctrl Pts',(23.212173544829,1.08299198344224,-7.55220547357544));
#132262=CARTESIAN_POINT('Ctrl Pts',(23.2071232470018,1.13847108866683,-7.54886151670606));
#132263=CARTESIAN_POINT('Ctrl Pts',(23.2042771510702,1.1622398388433,-7.54740216036922));
#132264=CARTESIAN_POINT('Ctrl Pts',(23.1983596272575,1.20205116755439,-7.54489190879501));
#132265=CARTESIAN_POINT('Ctrl Pts',(23.1956489309375,1.21814008823688,-7.54385821474024));
#132266=CARTESIAN_POINT('Ctrl Pts',(23.187928302395,1.25910935359935,-7.54117645965506));
#132267=CARTESIAN_POINT('Ctrl Pts',(23.182479673952,1.28389751965807,-7.53950880388485));
#132268=CARTESIAN_POINT('Ctrl Pts',(23.1567165702479,1.38630501446538,-7.53247368416446));
#132269=CARTESIAN_POINT('Ctrl Pts',(23.1297844725607,1.46206581161866,-7.52693026664844));
#132270=CARTESIAN_POINT('Ctrl Pts',(23.0780072942364,1.57301065407658,-7.51862840776639));
#132271=CARTESIAN_POINT('Ctrl Pts',(23.0582527008603,1.61034261579051,-7.51579724109893));
#132272=CARTESIAN_POINT('Ctrl Pts',(23.0185615338199,1.67704503166432,-7.51068859432403));
#132273=CARTESIAN_POINT('Ctrl Pts',(22.999185591811,1.70669915764103,-7.50839743056693));
#132274=CARTESIAN_POINT('Ctrl Pts',(22.9622239499138,1.75838939182723,-7.50436283716511));
#132275=CARTESIAN_POINT('Ctrl Pts',(22.945098841732,1.78072420267642,-7.50260457167021));
#132276=CARTESIAN_POINT('Ctrl Pts',(22.9032619088592,1.83167286462451,-7.49854654235209));
#132277=CARTESIAN_POINT('Ctrl Pts',(22.8779838591178,1.8597873932142,-7.49627028810481));
#132278=CARTESIAN_POINT('Ctrl Pts',(22.7865360348136,1.9527566981103,-7.48853950837726));
#132279=CARTESIAN_POINT('Ctrl Pts',(22.71453501403,2.01144637887395,-7.48330926971999));
#132280=CARTESIAN_POINT('Ctrl Pts',(22.6019953159732,2.08424059208809,-7.47548431391633));
#132281=CARTESIAN_POINT('Ctrl Pts',(22.5661384742771,2.10501055167859,-7.47303182357788));
#132282=CARTESIAN_POINT('Ctrl Pts',(22.5135061497038,2.13213868372751,-7.46939923328097));
#132283=CARTESIAN_POINT('Ctrl Pts',(22.4975115635861,2.13995974178171,-7.46829110514068));
#132284=CARTESIAN_POINT('Ctrl Pts',(22.4643986880383,2.15529369003329,-7.46597801943084));
#132285=CARTESIAN_POINT('Ctrl Pts',(22.4472685292147,2.16276972783158,-7.46477174353053));
#132286=CARTESIAN_POINT('Ctrl Pts',(22.3907808842619,2.18594590488653,-7.46077687256424));
#132287=CARTESIAN_POINT('Ctrl Pts',(22.350801022297,2.20004726641911,-7.45792353638843));
#132288=CARTESIAN_POINT('Ctrl Pts',(22.2412256319327,2.23260874400658,-7.45015260210442));
#132289=CARTESIAN_POINT('Ctrl Pts',(22.1706305908785,2.24718078234766,-7.44520570761822));
#132290=CARTESIAN_POINT('Ctrl Pts',(22.064982496159,2.25973215937322,-7.4380732599374));
#132291=CARTESIAN_POINT('Ctrl Pts',(22.0306332055258,2.26239640582401,-7.43579387888845));
#132292=CARTESIAN_POINT('Ctrl Pts',(21.964834184023,2.26480287394941,-7.43150841673015));
#132293=CARTESIAN_POINT('Ctrl Pts',(21.9334189453514,2.26478128611373,-7.4294973769525));
#132294=CARTESIAN_POINT('Ctrl Pts',(21.8735417530957,2.26250838197262,-7.42572513855168));
#132295=CARTESIAN_POINT('Ctrl Pts',(21.8450919047288,2.26046331327807,-7.42395903110725));
#132296=CARTESIAN_POINT('Ctrl Pts',(21.7702245754135,2.25252882291126,-7.41936508256022));
#132297=CARTESIAN_POINT('Ctrl Pts',(21.7240220470378,2.24502299084699,-7.41658606110863));
#132298=CARTESIAN_POINT('Ctrl Pts',(21.6013294761016,2.21803382440755,-7.40923607717549));
#132299=CARTESIAN_POINT('Ctrl Pts',(21.5260772287764,2.19392900240862,-7.40476688660263));
#132300=CARTESIAN_POINT('Ctrl Pts',(21.4280404131668,2.15208006521468,-7.39852815817694));
#132301=CARTESIAN_POINT('Ctrl Pts',(21.4028861130073,2.14034929418271,-7.39688652492375));
#132302=CARTESIAN_POINT('Ctrl Pts',(21.3585966046755,2.1178919537636,-7.39388849054287));
#132303=CARTESIAN_POINT('Ctrl Pts',(21.3393158888165,2.10747694400457,-7.39254519573733));
#132304=CARTESIAN_POINT('Ctrl Pts',(21.3060099155187,2.08835161129564,-7.39014025546559));
#132305=CARTESIAN_POINT('Ctrl Pts',(21.2918672857805,2.07985817811305,-7.38909025232836));
#132306=CARTESIAN_POINT('Ctrl Pts',(21.2537909873064,2.05596547979712,-7.38618732685736));
#132307=CARTESIAN_POINT('Ctrl Pts',(21.2302057659276,2.04003177582916,-7.38430683217135));
#132308=CARTESIAN_POINT('Ctrl Pts',(21.1426578145012,1.97648124603869,-7.37706120409505));
#132309=CARTESIAN_POINT('Ctrl Pts',(21.082710517875,1.92364829631565,-7.37155182614802));
#132310=CARTESIAN_POINT('Ctrl Pts',(20.9894976562408,1.82436776290702,-7.36233988963408));
#132311=CARTESIAN_POINT('Ctrl Pts',(20.9536540357179,1.78066832010741,-7.35858625454727));
#132312=CARTESIAN_POINT('Ctrl Pts',(20.9036342900622,1.71060309154341,-7.35302492959291));
#132313=CARTESIAN_POINT('Ctrl Pts',(20.8872727047603,1.68589275824092,-7.35114118363483));
#132314=CARTESIAN_POINT('Ctrl Pts',(20.856064081108,1.63495741887035,-7.34740385023755));
#132315=CARTESIAN_POINT('Ctrl Pts',(20.8412559616005,1.60873113725932,-7.34555246927876));
#132316=CARTESIAN_POINT('Ctrl Pts',(20.8016048229586,1.53224915517022,-7.34033520065384));
#132317=CARTESIAN_POINT('Ctrl Pts',(20.779146682433,1.48083680418887,-7.33704665955409));
#132318=CARTESIAN_POINT('Ctrl Pts',(20.7377482843471,1.36577726456233,-7.32995734862329));
#132319=CARTESIAN_POINT('Ctrl Pts',(20.7202567895926,1.30179175836331,-7.32618408331455));
#132320=CARTESIAN_POINT('Ctrl Pts',(20.7011034060175,1.20129378299635,-7.32017645307106));
#132321=CARTESIAN_POINT('Ctrl Pts',(20.6958695030891,1.165584249061,-7.31802512267355));
#132322=CARTESIAN_POINT('Ctrl Pts',(20.6903982972497,1.11252578400097,-7.31474267246062));
#132323=CARTESIAN_POINT('Ctrl Pts',(20.6889791408844,1.09531455843413,-7.31366449049371));
#132324=CARTESIAN_POINT('Ctrl Pts',(20.6867094072561,1.05862649599552,-7.31132845500143));
#132325=CARTESIAN_POINT('Ctrl Pts',(20.6859559202214,1.03914909123811,-7.31006674594604));
#132326=CARTESIAN_POINT('Ctrl Pts',(20.6841833830569,0.925175835434842,
-7.30258656709236));
#132327=CARTESIAN_POINT('Ctrl Pts',(20.6933100903781,0.830825266112662,
-7.29602917988473));
#132328=CARTESIAN_POINT('Ctrl Pts',(20.7214330497066,0.697841071848591,
-7.28681993620161));
#132329=CARTESIAN_POINT('Ctrl Pts',(20.7319924008396,0.657750486805098,
-7.28404389664926));
#132330=CARTESIAN_POINT('Ctrl Pts',(20.7550740262191,0.584863246294596,
-7.2790162876575));
#132331=CARTESIAN_POINT('Ctrl Pts',(20.767029088062,0.55192992193275,-7.27675199282445));
#132332=CARTESIAN_POINT('Ctrl Pts',(20.7910315881237,0.493497554231235,
-7.27274381050841));
#132333=CARTESIAN_POINT('Ctrl Pts',(20.8025930471859,0.467825233822383,
-7.2709860327521));
#132334=CARTESIAN_POINT('Ctrl Pts',(20.831874929885,0.408204866226418,-7.26690003541734));
#132335=CARTESIAN_POINT('Ctrl Pts',(20.8502993136262,0.374632950242004,
-7.26459659104704));
#132336=CARTESIAN_POINT('Ctrl Pts',(20.9158058648428,0.267145273476332,
-7.25714151648513));
#132337=CARTESIAN_POINT('Ctrl Pts',(20.9690395420465,0.197285777983223,
-7.25218070410798));
#132338=CARTESIAN_POINT('Ctrl Pts',(21.0505237594515,0.110683815647943,
-7.24525768449972));
#132339=CARTESIAN_POINT('Ctrl Pts',(21.072819747555,0.0886848127540274,
-7.24341714949713));
#132340=CARTESIAN_POINT('Ctrl Pts',(21.1133937292975,0.0515209482369094,
-7.24011225500614));
#132341=CARTESIAN_POINT('Ctrl Pts',(21.1313254804036,0.0360008121798749,
-7.23866560485725));
#132342=CARTESIAN_POINT('Ctrl Pts',(21.1623242857697,0.0106598629329513,
-7.23616735567625));
#132343=CARTESIAN_POINT('Ctrl Pts',(21.1751639987662,0.000572149131192745,
-7.23513233418825));
#132344=CARTESIAN_POINT('Ctrl Pts',(21.2086825114943,-0.0247280162274421,
-7.23242982649631));
#132345=CARTESIAN_POINT('Ctrl Pts',(21.2296341052558,-0.0395633249824545,
-7.23074200674234));
#132346=CARTESIAN_POINT('Ctrl Pts',(21.3180287714083,-0.0981977629417452,
-7.22367123082529));
#132347=CARTESIAN_POINT('Ctrl Pts',(21.3891218927,-0.136152072304188,-7.21811451497419));
#132348=CARTESIAN_POINT('Ctrl Pts',(21.5183012720179,-0.190018021893765,
-7.20862726820053));
#132349=CARTESIAN_POINT('Ctrl Pts',(21.5748216979094,-0.2090283171575,-7.2046571878587));
#132350=CARTESIAN_POINT('Ctrl Pts',(21.6613674114336,-0.23147970068488,
-7.19887484487606));
#132351=CARTESIAN_POINT('Ctrl Pts',(21.6905147517321,-0.237949377262141,
-7.19697507338289));
#132352=CARTESIAN_POINT('Ctrl Pts',(21.7492376808955,-0.248818246759099,
-7.19323519072459));
#132353=CARTESIAN_POINT('Ctrl Pts',(21.7787945913569,-0.253212450465656,
-7.19139632435182));
#132354=CARTESIAN_POINT('Ctrl Pts',(21.9175884525327,-0.268844003782043,
-7.18292820284992));
#132355=CARTESIAN_POINT('Ctrl Pts',(22.0278267950562,-0.266869947744044,
-7.17673034198916));
#132356=CARTESIAN_POINT('Ctrl Pts',(22.1686816030147,-0.245873999258075,
-7.16845195434581));
#132357=CARTESIAN_POINT('Ctrl Pts',(22.2007356751181,-0.239820572247473,
-7.16653915378911));
#132358=CARTESIAN_POINT('Ctrl Pts',(22.2562405272078,-0.227097918076251,
-7.16312433805001));
#132359=CARTESIAN_POINT('Ctrl Pts',(22.2797994072487,-0.220976961557628,
-7.16164183438522));
#132360=CARTESIAN_POINT('Ctrl Pts',(22.3188292636876,-0.209624457519522,
-7.15910836628414));
#132361=CARTESIAN_POINT('Ctrl Pts',(22.3344011562343,-0.204766381414831,
-7.15807567944551));
#132362=CARTESIAN_POINT('Ctrl Pts',(22.363536087041,-0.195054599578651,
-7.15610141683161));
#132363=CARTESIAN_POINT('Ctrl Pts',(22.3771172669733,-0.190268191947343,
-7.15516422911284));
#132364=CARTESIAN_POINT('Ctrl Pts',(22.3906127227906,-0.185251306681596,
-7.15421791561113));
#132365=CARTESIAN_POINT('Origin',(21.9499999789786,0.999999999999992,-6.00000000000001));
#132366=CARTESIAN_POINT('',(22.3906127230289,-0.185251306593042,-6.65225448505536));
#132367=CARTESIAN_POINT('',(22.3905561784951,-0.18502046241637,-6.79053837538029));
#132368=CARTESIAN_POINT('',(22.3906127231008,-0.185251306566283,-6.00000000000001));
#132369=CARTESIAN_POINT('',(20.6856937166152,0.999065229854255,-6.94375443275021));
#132370=CARTESIAN_POINT('Ctrl Pts',(22.3905561778436,-0.185020462657188,
-6.79053837542619));
#132371=CARTESIAN_POINT('Ctrl Pts',(22.3439699936583,-0.20224093581996,
-6.79382028946338));
#132372=CARTESIAN_POINT('Ctrl Pts',(22.2963454492253,-0.216746426185838,
-6.79706020776744));
#132373=CARTESIAN_POINT('Ctrl Pts',(22.2480258339149,-0.228436764308156,
-6.80023594852031));
#132374=CARTESIAN_POINT('Ctrl Pts',(22.199718524656,-0.240124125132281,
-6.80341088047474));
#132375=CARTESIAN_POINT('Ctrl Pts',(22.1507165053392,-0.248997734601995,
-6.80652166575826));
#132376=CARTESIAN_POINT('Ctrl Pts',(22.1013714506626,-0.254991265143792,
-6.80957082217001));
#132377=CARTESIAN_POINT('Ctrl Pts',(22.051984798257,-0.26098984821335,-6.81262254901122));
#132378=CARTESIAN_POINT('Ctrl Pts',(22.002254556072,-0.264103293065579,
-6.81561267971874));
#132379=CARTESIAN_POINT('Ctrl Pts',(21.952541740764,-0.264300704134091,
-6.81856747133101));
#132380=CARTESIAN_POINT('Ctrl Pts',(21.9028067785013,-0.26449820314882,
-6.82152357929674));
#132381=CARTESIAN_POINT('Ctrl Pts',(21.8530893382183,-0.261776695821649,
-6.82444463309553));
#132382=CARTESIAN_POINT('Ctrl Pts',(21.8037586542992,-0.256145149757803,
-6.8273773218159));
#132383=CARTESIAN_POINT('Ctrl Pts',(21.7543405399351,-0.250503622713768,
-6.83031520824001));
#132384=CARTESIAN_POINT('Ctrl Pts',(21.7053107951687,-0.241941155643439,
-6.83326533420195));
#132385=CARTESIAN_POINT('Ctrl Pts',(21.6570461311386,-0.230513961479585,
-6.83628857712534));
#132386=CARTESIAN_POINT('Ctrl Pts',(21.6291010198181,-0.223897646637129,
-6.83803902668799));
#132387=CARTESIAN_POINT('Ctrl Pts',(21.6014124921128,-0.216321883951753,
-6.83981421545855));
#132388=CARTESIAN_POINT('Ctrl Pts',(21.5740537671172,-0.207806077291614,
-6.84162671206072));
#132389=CARTESIAN_POINT('Ctrl Pts',(21.5740375959949,-0.207801043791291,
-6.84162778338639));
#132390=CARTESIAN_POINT('Ctrl Pts',(21.5740214249876,-0.207796009962646,
-6.84162885472508));
#132391=CARTESIAN_POINT('Ctrl Pts',(21.5740052540952,-0.207790975805693,
-6.84162992607682));
#132392=CARTESIAN_POINT('Ctrl Pts',(21.5301887526272,-0.194150470342384,
-6.84453285090531));
#132393=CARTESIAN_POINT('Ctrl Pts',(21.4870600614421,-0.178042935966803,
-6.84753884171575));
#132394=CARTESIAN_POINT('Ctrl Pts',(21.4448958919887,-0.159584333445583,
-6.85058879476411));
#132395=CARTESIAN_POINT('Ctrl Pts',(21.4403540045181,-0.157595988919839,
-6.85091733303999));
#132396=CARTESIAN_POINT('Ctrl Pts',(21.4358233375632,-0.155580404652721,
-6.85124638142775));
#132397=CARTESIAN_POINT('Ctrl Pts',(21.4313042568956,-0.153537755545344,
-6.85157586605306));
#132398=CARTESIAN_POINT('Ctrl Pts',(21.3861311093499,-0.133119246495114,
-6.85486942478502));
#132399=CARTESIAN_POINT('Ctrl Pts',(21.3421117789209,-0.10999206023659,
-6.85820602282507));
#132400=CARTESIAN_POINT('Ctrl Pts',(21.2995639830833,-0.0843384566189006,
-6.86152689828285));
#132401=CARTESIAN_POINT('Ctrl Pts',(21.2570558557206,-0.0587087705581764,
-6.86484467759752));
#132402=CARTESIAN_POINT('Ctrl Pts',(21.2160163016383,-0.0305576030157111,
-6.86814647008664));
#132403=CARTESIAN_POINT('Ctrl Pts',(21.1767369068999,-9.51095119867129E-5,
-6.87139508591847));
#132404=CARTESIAN_POINT('Ctrl Pts',(21.1374777418491,0.030351695187625,
-6.87464202864704));
#132405=CARTESIAN_POINT('Ctrl Pts',(21.0999768602153,0.0631073930715781,
-6.87783575437138));
#132406=CARTESIAN_POINT('Ctrl Pts',(21.0645022911954,0.0979357489692311,
-6.88096336386761));
#132407=CARTESIAN_POINT('Ctrl Pts',(21.0271682715109,0.134589683339287,
-6.88425491152339));
#132408=CARTESIAN_POINT('Ctrl Pts',(20.9920788931084,0.173539570838059,
-6.88747304910112));
#132409=CARTESIAN_POINT('Ctrl Pts',(20.9595186796348,0.214478450135798,
-6.89063209350199));
#132410=CARTESIAN_POINT('Ctrl Pts',(20.928552990418,0.253412488889815,-6.89363643458897));
#132411=CARTESIAN_POINT('Ctrl Pts',(20.8998748503192,0.294145362371813,
-6.89658775113724));
#132412=CARTESIAN_POINT('Ctrl Pts',(20.8737024166744,0.336384547288791,
-6.89952161411312));
#132413=CARTESIAN_POINT('Ctrl Pts',(20.8475141232985,0.378649327919265,
-6.90245725492435));
#132414=CARTESIAN_POINT('Ctrl Pts',(20.8238350245176,0.422422397756516,
-6.90537583380583));
#132415=CARTESIAN_POINT('Ctrl Pts',(20.802852535304,0.467380785622911,-6.90833104940879));
#132416=CARTESIAN_POINT('Ctrl Pts',(20.7834786740189,0.508892427128444,
-6.91105970264801));
#132417=CARTESIAN_POINT('Ctrl Pts',(20.7664038099828,0.551415116425624,
-6.91382017768355));
#132418=CARTESIAN_POINT('Ctrl Pts',(20.7517458282314,0.594668391099852,
-6.9166624960234));
#132419=CARTESIAN_POINT('Ctrl Pts',(20.7505025216512,0.598337182747256,
-6.91690358467768));
#132420=CARTESIAN_POINT('Ctrl Pts',(20.7492765785363,0.602011249014336,
-6.91714526216378));
#132421=CARTESIAN_POINT('Ctrl Pts',(20.7480680571252,0.605690429331247,
-6.91738755900762));
#132422=CARTESIAN_POINT('Ctrl Pts',(20.7457352261486,0.612792418367502,
-6.91785526903547));
#132423=CARTESIAN_POINT('Ctrl Pts',(20.7434673324641,0.619913322422839,
-6.91832529279064));
#132424=CARTESIAN_POINT('Ctrl Pts',(20.7412647880579,0.627051853772677,
-6.9187978518838));
#132425=CARTESIAN_POINT('Ctrl Pts',(20.7412597946966,0.627068037449193,
-6.9187989232167));
#132426=CARTESIAN_POINT('Ctrl Pts',(20.7412548016711,0.627084221216311,
-6.91879999456263));
#132427=CARTESIAN_POINT('Ctrl Pts',(20.7412498089815,0.627100405074025,
-6.91880106592159));
#132428=CARTESIAN_POINT('Ctrl Pts',(20.7269381749478,0.673491722735542,
-6.92187213556098));
#132429=CARTESIAN_POINT('Ctrl Pts',(20.7153550167606,0.720746816475562,
-6.92505507810059));
#132430=CARTESIAN_POINT('Ctrl Pts',(20.7065458452856,0.768570366770981,
-6.92828331058919));
#132431=CARTESIAN_POINT('Ctrl Pts',(20.7046661143239,0.778775118539138,
-6.92897216181401));
#132432=CARTESIAN_POINT('Ctrl Pts',(20.7029127089235,0.789005565373911,
-6.92966307520232));
#132433=CARTESIAN_POINT('Ctrl Pts',(20.7012860861758,0.799258531203285,
-6.93035540384252));
#132434=CARTESIAN_POINT('Ctrl Pts',(20.6932986460189,0.849605147289468,
-6.93375504496431));
#132435=CARTESIAN_POINT('Ctrl Pts',(20.6883673085457,0.900501158509976,
-6.93718806872723));
#132436=CARTESIAN_POINT('Ctrl Pts',(20.6865206510876,0.951614527893218,
-6.94059901766862));
#132437=CARTESIAN_POINT('Ctrl Pts',(20.6862523792291,0.959039986546106,
-6.94109454086807));
#132438=CARTESIAN_POINT('Ctrl Pts',(20.6860492463712,0.966469951088698,
-6.94158959818679));
#132439=CARTESIAN_POINT('Ctrl Pts',(20.6859113746941,0.973903318693967,
-6.94208401959448));
#132440=CARTESIAN_POINT('Ctrl Pts',(20.6857558836499,0.982286636539075,
-6.94264162578728));
#132441=CARTESIAN_POINT('Ctrl Pts',(20.6856832995832,0.990674430511361,
-6.943198488816));
#132442=CARTESIAN_POINT('Ctrl Pts',(20.6856937166151,0.999065229854251,
-6.94375443275022));
#132443=CARTESIAN_POINT('Ctrl Pts',(20.685693716616,0.999065230477396,-6.94375443279149));
#132444=CARTESIAN_POINT('Ctrl Pts',(20.6857551278917,1.0485312865077,-6.94703187426906));
#132445=CARTESIAN_POINT('Ctrl Pts',(20.6887020793451,1.09803110754432,-6.95027188392369));
#132446=CARTESIAN_POINT('Ctrl Pts',(20.6945091701822,1.14721024717709,-6.95344961851266));
#132447=CARTESIAN_POINT('Ctrl Pts',(20.7003144327648,1.19637390367318,-6.95662635265104));
#132448=CARTESIAN_POINT('Ctrl Pts',(20.7089780416456,1.24521705585266,-6.95974083149961));
#132449=CARTESIAN_POINT('Ctrl Pts',(20.7204397803494,1.29338962554135,-6.96279253068962));
#132450=CARTESIAN_POINT('Ctrl Pts',(20.7319109841211,1.34160197598738,-6.96584674996327));
#132451=CARTESIAN_POINT('Ctrl Pts',(20.7461850959508,1.38914253792151,-6.9688382028184));
#132452=CARTESIAN_POINT('Ctrl Pts',(20.7631656009654,1.43566531597457,-6.97178998233388));
#132453=CARTESIAN_POINT('Ctrl Pts',(20.7801530496552,1.48220711814135,-6.97474296889227));
#132454=CARTESIAN_POINT('Ctrl Pts',(20.7998493943831,1.52773010249413,-6.97765653747682));
#132455=CARTESIAN_POINT('Ctrl Pts',(20.8221185135132,1.57189499446312,-6.98057444667909));
#132456=CARTESIAN_POINT('Ctrl Pts',(20.8444291451012,1.61614221538313,-6.98349779523359));
#132457=CARTESIAN_POINT('Ctrl Pts',(20.869322573561,1.65902587372874,-6.98642602058845));
#132458=CARTESIAN_POINT('Ctrl Pts',(20.8966168887807,1.7002163716426,-6.98941784958919));
#132459=CARTESIAN_POINT('Ctrl Pts',(20.9161665316061,1.72971920091432,-6.99156075692679));
#132460=CARTESIAN_POINT('Ctrl Pts',(20.9369469521193,1.7583535746909,-6.9937366703361));
#132461=CARTESIAN_POINT('Ctrl Pts',(20.9588752605237,1.78600436831953,-6.99596900134297));
#132462=CARTESIAN_POINT('Ctrl Pts',(20.958885784244,1.7860176383454,-6.99597007267172));
#132463=CARTESIAN_POINT('Ctrl Pts',(20.9588963082288,1.78603090814513,-6.99597114401347));
#132464=CARTESIAN_POINT('Ctrl Pts',(20.9589068324779,1.78604417771874,-6.99597221536821));
#132465=CARTESIAN_POINT('Ctrl Pts',(20.9874231821028,1.82199921804461,-6.99887514232692));
#132466=CARTESIAN_POINT('Ctrl Pts',(21.0179928358731,1.85642349262579,-7.00188113528414));
#132467=CARTESIAN_POINT('Ctrl Pts',(21.0504078929258,1.8891006848048,-7.00493109083005));
#132468=CARTESIAN_POINT('Ctrl Pts',(21.0538996320004,1.89262066098736,-7.0052596310186));
#132469=CARTESIAN_POINT('Ctrl Pts',(21.0574127359555,1.89612035267063,-7.00558868132818));
#132470=CARTESIAN_POINT('Ctrl Pts',(21.0609469098073,1.89959948170392,-7.00591816788382));
#132471=CARTESIAN_POINT('Ctrl Pts',(21.0962747177362,1.93437705841731,-7.00921173470899));
#132472=CARTESIAN_POINT('Ctrl Pts',(21.1337132810345,1.96710208179375,-7.01254834138308));
#132473=CARTESIAN_POINT('Ctrl Pts',(21.1729780749988,1.99754388043512,-7.01586922582333));
#132474=CARTESIAN_POINT('Ctrl Pts',(21.2122062616413,2.02795729760271,-7.01918701413921));
#132475=CARTESIAN_POINT('Ctrl Pts',(21.2532571421861,2.05609203131309,-7.02248881597173));
#132476=CARTESIAN_POINT('Ctrl Pts',(21.2958295897617,2.08175183975354,-7.02573744114571));
#132477=CARTESIAN_POINT('Ctrl Pts',(21.3383801118927,2.10739843301043,-7.02898439322933));
#132478=CARTESIAN_POINT('Ctrl Pts',(21.3824506079409,2.13057272766119,-7.03217812830337));
#132479=CARTESIAN_POINT('Ctrl Pts',(21.4277241149225,2.15110985535873,-7.03530574671623));
#132480=CARTESIAN_POINT('Ctrl Pts',(21.4753706061152,2.17272342451209,-7.03859729740664));
#132481=CARTESIAN_POINT('Ctrl Pts',(21.5243496983534,2.19141570151684,-7.04181543782941));
#132482=CARTESIAN_POINT('Ctrl Pts',(21.5742725134357,2.20703192480476,-7.04497448422916));
#132483=CARTESIAN_POINT('Ctrl Pts',(21.6217506221013,2.22188342596689,-7.04797883300236));
#132484=CARTESIAN_POINT('Ctrl Pts',(21.6700821660592,2.23395277606183,-7.0509301562539));
#132485=CARTESIAN_POINT('Ctrl Pts',(21.7189156529662,2.24314191431671,-7.05386402443837));
#132486=CARTESIAN_POINT('Ctrl Pts',(21.7677787313942,2.25233662089355,-7.05679967045252));
#132487=CARTESIAN_POINT('Ctrl Pts',(21.8171443403872,2.25864714910988,-7.05971825303604));
#132488=CARTESIAN_POINT('Ctrl Pts',(21.8666436667313,2.2620150884441,-7.06267347039033));
#132489=CARTESIAN_POINT('Ctrl Pts',(21.9123482058553,2.26512483005954,-7.06540213070079));
#132490=CARTESIAN_POINT('Ctrl Pts',(21.9581672161228,2.26572567292485,-7.06816261126618));
#132491=CARTESIAN_POINT('Ctrl Pts',(22.0037965948361,2.26380874167111,-7.07100493365448));
#132492=CARTESIAN_POINT('Ctrl Pts',(22.0076668306934,2.26364614958058,-7.07124601644665));
#132493=CARTESIAN_POINT('Ctrl Pts',(22.0115357284369,2.26346546078326,-7.07148768802967));
#132494=CARTESIAN_POINT('Ctrl Pts',(22.0154031173103,2.26326667882846,-7.07172997892714));
#132495=CARTESIAN_POINT('Ctrl Pts',(22.0228682888261,2.26288297255133,-7.07219766996248));
#132496=CARTESIAN_POINT('Ctrl Pts',(22.0303276993002,2.26243188135987,-7.07266767448959));
#132497=CARTESIAN_POINT('Ctrl Pts',(22.0377799992292,2.26191348507893,-7.07314021409209));
#132498=CARTESIAN_POINT('Ctrl Pts',(22.0377968933154,2.26191230989388,-7.07314128532176));
#132499=CARTESIAN_POINT('Ctrl Pts',(22.0378137873651,2.26191113436296,-7.07314235656445));
#132500=CARTESIAN_POINT('Ctrl Pts',(22.0378306813782,2.26190995848617,-7.07314342782018));
#132501=CARTESIAN_POINT('Ctrl Pts',(22.08361093453,2.25872350796018,-7.07604637089033));
#132502=CARTESIAN_POINT('Ctrl Pts',(22.1292898167375,2.25297790701657,-7.07905237820387));
#132503=CARTESIAN_POINT('Ctrl Pts',(22.1745713474598,2.24472229803669,-7.08210234591501));
#132504=CARTESIAN_POINT('Ctrl Pts',(22.1794486211828,2.24383308638455,-7.08243085794047));
#132505=CARTESIAN_POINT('Ctrl Pts',(22.1843212476966,2.24291478795741,-7.08275987997004));
#132506=CARTESIAN_POINT('Ctrl Pts',(22.1891888308828,2.24196748872918,-7.08308933814804));
#132507=CARTESIAN_POINT('Ctrl Pts',(22.2378496331668,2.23249742141138,-7.08638290266398));
#132508=CARTESIAN_POINT('Ctrl Pts',(22.2860112071759,2.22012577175817,-7.08971950473026));
#132509=CARTESIAN_POINT('Ctrl Pts',(22.3333224062371,2.20495675917564,-7.09304038328605));
#132510=CARTESIAN_POINT('Ctrl Pts',(22.3805894975061,2.18980188852287,-7.09635816581756));
#132511=CARTESIAN_POINT('Ctrl Pts',(22.4270079592013,2.17185513983666,-7.09965996060118));
#132512=CARTESIAN_POINT('Ctrl Pts',(22.4722456518536,2.15125389476901,-7.10290857893874));
#132513=CARTESIAN_POINT('Ctrl Pts',(22.5174600471837,2.13066325930182,-7.10615552424428));
#132514=CARTESIAN_POINT('Ctrl Pts',(22.5614949388929,2.10742092666226,-7.10934925276055));
#132515=CARTESIAN_POINT('Ctrl Pts',(22.604035107296,2.08169508090793,-7.11247686661958));
#132516=CARTESIAN_POINT('Ctrl Pts',(22.6488046503027,2.05462103768905,-7.11576838727938));
#132517=CARTESIAN_POINT('Ctrl Pts',(22.6919184439548,2.02479597004318,-7.11898650106652));
#132518=CARTESIAN_POINT('Ctrl Pts',(22.7330289434229,1.99245308442595,-7.12214552604287));
#132519=CARTESIAN_POINT('Ctrl Pts',(22.7721265717464,1.9616937860196,-7.12514987738834));
#132520=CARTESIAN_POINT('Ctrl Pts',(22.8094122162172,1.92865729892989,-7.12810120709323));
#132521=CARTESIAN_POINT('Ctrl Pts',(22.8446062298037,1.8935780652595,-7.13103508730942));
#132522=CARTESIAN_POINT('Ctrl Pts',(22.8798215691838,1.85847757534628,-7.13397074530875));
#132523=CARTESIAN_POINT('Ctrl Pts',(22.9129423386157,1.82133161119038,-7.13688934548987));
#132524=CARTESIAN_POINT('Ctrl Pts',(22.9437117976406,1.78241132324634,-7.13984458737692));
#132525=CARTESIAN_POINT('Ctrl Pts',(22.9721220955032,1.74647513819684,-7.1425732444586));
#132526=CARTESIAN_POINT('Ctrl Pts',(22.9985279273012,1.70902578404918,-7.14533372713626));
#132527=CARTESIAN_POINT('Ctrl Pts',(23.0227500061312,1.67030904664563,-7.148176055919));
#132528=CARTESIAN_POINT('Ctrl Pts',(23.02480474488,1.66702473809689,-7.14841716829948));
#132529=CARTESIAN_POINT('Ctrl Pts',(23.0268437980163,1.66373129740975,-7.14865886964349));
#132530=CARTESIAN_POINT('Ctrl Pts',(23.0288670718732,1.66042886747209,-7.14890119048505));
#132531=CARTESIAN_POINT('Ctrl Pts',(23.0327715173278,1.65405594987828,-7.14936881304894));
#132532=CARTESIAN_POINT('Ctrl Pts',(23.0366171472399,1.64764968808478,-7.14983874853652));
#132533=CARTESIAN_POINT('Ctrl Pts',(23.0404032646256,1.64121123969717,-7.15031121842487));
#132534=CARTESIAN_POINT('Ctrl Pts',(23.0404118505076,1.64119663905169,-7.15031228985776));
#132535=CARTESIAN_POINT('Ctrl Pts',(23.0404204360835,1.64118203824067,-7.15031336130368));
#132536=CARTESIAN_POINT('Ctrl Pts',(23.0404290213534,1.64116743726415,-7.15031443276264));
#132537=CARTESIAN_POINT('Ctrl Pts',(23.0636891555693,1.60160890523665,-7.15321734431571));
#132538=CARTESIAN_POINT('Ctrl Pts',(23.0847813867873,1.5606868188613,-7.15622332121024));
#132539=CARTESIAN_POINT('Ctrl Pts',(23.1035788700111,1.51867306745788,-7.15927325930162));
#132540=CARTESIAN_POINT('Ctrl Pts',(23.1056039194408,1.51414693370333,-7.15960182857439));
#132541=CARTESIAN_POINT('Ctrl Pts',(23.1076023427295,1.50960817985568,-7.15993090804821));
#132542=CARTESIAN_POINT('Ctrl Pts',(23.1095739866974,1.50505718142626,-7.16026042382627));
#132543=CARTESIAN_POINT('Ctrl Pts',(23.1292807058241,1.45956963435734,-7.16355395703598));
#132544=CARTESIAN_POINT('Ctrl Pts',(23.1463121274894,1.41285302083312,-7.16689052733892));
#132545=CARTESIAN_POINT('Ctrl Pts',(23.160555635742,1.36525587302037,-7.17021137308667));
#132546=CARTESIAN_POINT('Ctrl Pts',(23.1747858651263,1.3177030988439,-7.17352912289258));
#132547=CARTESIAN_POINT('Ctrl Pts',(23.1862336914812,1.26927145254509,-7.17683088390998));
#132548=CARTESIAN_POINT('Ctrl Pts',(23.1948245979885,1.22031254384211,-7.18007946634394));
#132549=CARTESIAN_POINT('Ctrl Pts',(23.2034110807242,1.17137884587059,-7.18332637596407));
#132550=CARTESIAN_POINT('Ctrl Pts',(23.2091436674003,1.12191842475156,-7.18652006664586));
#132551=CARTESIAN_POINT('Ctrl Pts',(23.2119828137938,1.07228635432059,-7.18964763895261));
#132552=CARTESIAN_POINT('Ctrl Pts',(23.2149708425993,1.02005162050749,-7.19293921847983));
#132553=CARTESIAN_POINT('Ctrl Pts',(23.2147535520184,0.967626754614273,
-7.19615738227058));
#132554=CARTESIAN_POINT('Ctrl Pts',(23.2113267459532,0.915430297146576,
-7.19931644801464));
#132555=CARTESIAN_POINT('Ctrl Pts',(23.2080678248899,0.86579103205804,-7.20232074580628));
#132556=CARTESIAN_POINT('Ctrl Pts',(23.201906219855,0.816358453725433,-7.20527201699764));
#132557=CARTESIAN_POINT('Ctrl Pts',(23.1928771501315,0.767495764724232,
-7.20820583271065));
#132558=CARTESIAN_POINT('Ctrl Pts',(23.1838426076001,0.71860345848436,-7.21114142670319));
#132559=CARTESIAN_POINT('Ctrl Pts',(23.1719366878453,0.670281923275512,
-7.2140599568284));
#132560=CARTESIAN_POINT('Ctrl Pts',(23.1572378379234,0.62289622656633,-7.21701512218833));
#132561=CARTESIAN_POINT('Ctrl Pts',(23.1436658154371,0.579143161212322,
-7.21974374183739));
#132562=CARTESIAN_POINT('Ctrl Pts',(23.1277123164478,0.536187580615072,
-7.22250418228607));
#132563=CARTESIAN_POINT('Ctrl Pts',(23.1094786702379,0.494316340902381,
-7.22534646665043));
#132564=CARTESIAN_POINT('Ctrl Pts',(23.1079321580124,0.490764973097593,
-7.22558753897723));
#132565=CARTESIAN_POINT('Ctrl Pts',(23.1063692490606,0.487221375408037,
-7.22582920007457));
#132566=CARTESIAN_POINT('Ctrl Pts',(23.1047900082331,0.483685705815835,
-7.22607148046424));
#132567=CARTESIAN_POINT('Ctrl Pts',(23.101740083699,0.476857408797344,-7.22653938687329));
#132568=CARTESIAN_POINT('Ctrl Pts',(23.0986293235844,0.470058800527314,
-7.22700960902506));
#132569=CARTESIAN_POINT('Ctrl Pts',(23.0954582895556,0.46329111275518,-7.22748236882627));
#132570=CARTESIAN_POINT('Ctrl Pts',(23.0954511030209,0.463275775101049,
-7.22748344024484));
#132571=CARTESIAN_POINT('Ctrl Pts',(23.0954439161766,0.463260437605711,
-7.22748451167644));
#132572=CARTESIAN_POINT('Ctrl Pts',(23.0954367290228,0.463245100269174,
-7.22748558312107));
#132573=CARTESIAN_POINT('Ctrl Pts',(23.0759885435365,0.421742807111391,
-7.23038487461292));
#132574=CARTESIAN_POINT('Ctrl Pts',(23.0541955748594,0.381254633016138,
-7.2333870240812));
#132575=CARTESIAN_POINT('Ctrl Pts',(23.0302100424038,0.342038699230848,
-7.2364330315869));
#132576=CARTESIAN_POINT('Ctrl Pts',(23.0282976945341,0.338912043294594,
-7.23667588739907));
#132577=CARTESIAN_POINT('Ctrl Pts',(23.0263714334915,0.335793487179436,
-7.23691902200578));
#132578=CARTESIAN_POINT('Ctrl Pts',(23.0244313492434,0.332683167846775,
-7.23716240550476));
#132579=CARTESIAN_POINT('Ctrl Pts',(22.9981951656695,0.29062163929907,-7.24045373378824));
#132580=CARTESIAN_POINT('Ctrl Pts',(22.9694263119232,0.250063447762252,
-7.24378997834366));
#132581=CARTESIAN_POINT('Ctrl Pts',(22.9383478845116,0.211299474319808,
-7.24711185102367));
#132582=CARTESIAN_POINT('Ctrl Pts',(22.9073006248753,0.172574376294066,
-7.25043039228088));
#132583=CARTESIAN_POINT('Ctrl Pts',(22.8739486232003,0.13563964686214,-7.25373429046647));
#132584=CARTESIAN_POINT('Ctrl Pts',(22.8385390936182,0.100756320054096,
-7.25698571893782));
#132585=CARTESIAN_POINT('Ctrl Pts',(22.8031397311405,0.0658830092623621,
-7.26023621382961));
#132586=CARTESIAN_POINT('Ctrl Pts',(22.7656840675728,0.0330598495998048,
-7.26343416853049));
#132587=CARTESIAN_POINT('Ctrl Pts',(22.7264421556169,0.00252111828283075,
-7.26656599894528));
#132588=CARTESIAN_POINT('Ctrl Pts',(22.6872079281136,-0.0280116328608765,
-7.26969721607694));
#132589=CARTESIAN_POINT('Ctrl Pts',(22.6461881210261,-0.0562607641338967,
-7.27276238169854));
#132590=CARTESIAN_POINT('Ctrl Pts',(22.6036756059344,-0.082018775347772,
-7.27577250159465));
#132591=CARTESIAN_POINT('Ctrl Pts',(22.5611291330222,-0.107797361348121,
-7.27878502589123));
#132592=CARTESIAN_POINT('Ctrl Pts',(22.5170874833382,-0.13108059782982,
-7.28174260914648));
#132593=CARTESIAN_POINT('Ctrl Pts',(22.4718681260937,-0.151689667592821,
-7.28467914380461));
#132594=CARTESIAN_POINT('Ctrl Pts',(22.4451788861354,-0.163853493921597,
-7.28641233690846));
#132595=CARTESIAN_POINT('Ctrl Pts',(22.4180798423309,-0.175086317613026,
-7.28813862593899));
#132596=CARTESIAN_POINT('Ctrl Pts',(22.3906403691454,-0.185356836028299,
-7.28986813301021));
#132597=CARTESIAN_POINT('Ctrl Pts',(22.3906127227906,-0.185251306681596,
-7.15421791561113));
#132598=CARTESIAN_POINT('Ctrl Pts',(22.3963865089124,-0.183104923268248,
-7.15381305253448));
#132599=CARTESIAN_POINT('Ctrl Pts',(22.4021446040177,-0.180916353269807,
-7.15340651779141));
#132600=CARTESIAN_POINT('Ctrl Pts',(22.4974886487836,-0.143877849688105,
-7.1466312728536));
#132601=CARTESIAN_POINT('Ctrl Pts',(22.5828282425092,-0.0989673465778473,
-7.13995318145344));
#132602=CARTESIAN_POINT('Ctrl Pts',(22.7055482856947,-0.0153089157280206,
-7.12993909527289));
#132603=CARTESIAN_POINT('Ctrl Pts',(22.7469681914671,0.0168681629758805,
-7.12646807965307));
#132604=CARTESIAN_POINT('Ctrl Pts',(22.8082537735905,0.0709040978539566,
-7.12119935494327));
#132605=CARTESIAN_POINT('Ctrl Pts',(22.8295525623377,0.0910411210818873,
-7.11933950438369));
#132606=CARTESIAN_POINT('Ctrl Pts',(22.871585102151,0.133643274251094,-7.11560107051006));
#132607=CARTESIAN_POINT('Ctrl Pts',(22.8922427104079,0.15615642476928,-7.11372630343523));
#132608=CARTESIAN_POINT('Ctrl Pts',(22.9574869606839,0.232648087821485,
-7.10764917212118));
#132609=CARTESIAN_POINT('Ctrl Pts',(22.9984101846094,0.289580172405581,
-7.10358548663138));
#132610=CARTESIAN_POINT('Ctrl Pts',(23.072345242098,0.412854521249262,-7.09529103843624));
#132611=CARTESIAN_POINT('Ctrl Pts',(23.1046673072505,0.479288879500483,
-7.09107723958861));
#132612=CARTESIAN_POINT('Ctrl Pts',(23.1389392649683,0.56886719174341,-7.08529140007046));
#132613=CARTESIAN_POINT('Ctrl Pts',(23.1463173960146,0.589784659058625,
-7.08393279762197));
#132614=CARTESIAN_POINT('Ctrl Pts',(23.158206153192,0.626544511255371,-7.08151495742629));
#132615=CARTESIAN_POINT('Ctrl Pts',(23.1629640934315,0.642300241452674,
-7.08046809863432));
#132616=CARTESIAN_POINT('Ctrl Pts',(23.1749718169935,0.685061957637121,
-7.07760142930103));
#132617=CARTESIAN_POINT('Ctrl Pts',(23.1816351708149,0.712221459791249,
-7.07575535289521));
#132618=CARTESIAN_POINT('Ctrl Pts',(23.203857975858,0.817812575233972,-7.06853396277475));
#132619=CARTESIAN_POINT('Ctrl Pts',(23.2128665995165,0.897432126960158,
-7.0630090361043));
#132620=CARTESIAN_POINT('Ctrl Pts',(23.215019269856,1.01769492812765,-7.05486999779951));
#132621=CARTESIAN_POINT('Ctrl Pts',(23.2138114256659,1.05803438076521,-7.05217190181311));
#132622=CARTESIAN_POINT('Ctrl Pts',(23.2079990946158,1.13261433088414,-7.04725922220962));
#132623=CARTESIAN_POINT('Ctrl Pts',(23.2039167964405,1.1668571285292,-7.04503324036443));
#132624=CARTESIAN_POINT('Ctrl Pts',(23.1939624687753,1.22871782296008,-7.04106150457622));
#132625=CARTESIAN_POINT('Ctrl Pts',(23.1885558222564,1.25638668499816,-7.03930323746905));
#132626=CARTESIAN_POINT('Ctrl Pts',(23.1734549661269,1.32194059829662,-7.0351692499306));
#132627=CARTESIAN_POINT('Ctrl Pts',(23.1629196905066,1.35960261735808,-7.03282040298909));
#132628=CARTESIAN_POINT('Ctrl Pts',(23.1223165566055,1.48248658654174,-7.0251667183367));
#132629=CARTESIAN_POINT('Ctrl Pts',(23.0848703744882,1.56496751080769,-7.02006338298117));
#132630=CARTESIAN_POINT('Ctrl Pts',(23.018098585617,1.67809252021458,-7.01239182177738));
#132631=CARTESIAN_POINT('Ctrl Pts',(22.99553433456,1.71239133048874,-7.00996088770126));
#132632=CARTESIAN_POINT('Ctrl Pts',(22.9608713578482,1.75987821054881,-7.00635347643586));
#132633=CARTESIAN_POINT('Ctrl Pts',(22.9500967330442,1.77400404954302,-7.00524755386539));
#132634=CARTESIAN_POINT('Ctrl Pts',(22.9273605293499,1.80254424848222,-7.00293425551295));
#132635=CARTESIAN_POINT('Ctrl Pts',(22.9153693172436,1.81692892310139,-7.00172542550888));
#132636=CARTESIAN_POINT('Ctrl Pts',(22.866589267801,1.87287141437836,-6.99686839863679));
#132637=CARTESIAN_POINT('Ctrl Pts',(22.8274031403086,1.91225166181806,-6.99309977126369));
#132638=CARTESIAN_POINT('Ctrl Pts',(22.7131658491625,2.01286537602583,-6.98271086244623));
#132639=CARTESIAN_POINT('Ctrl Pts',(22.6334605288347,2.06827231163822,-6.97611228950282));
#132640=CARTESIAN_POINT('Ctrl Pts',(22.5213521311855,2.12847068837013,-6.96785931357987));
#132641=CARTESIAN_POINT('Ctrl Pts',(22.4939830176899,2.14191596731054,-6.96591374833515));
#132642=CARTESIAN_POINT('Ctrl Pts',(22.4393668850518,2.16633666194278,-6.96215815956609));
#132643=CARTESIAN_POINT('Ctrl Pts',(22.4121708293295,2.17737822759954,-6.96034692672753));
#132644=CARTESIAN_POINT('Ctrl Pts',(22.3349542145218,2.20563961126037,-6.95534762334885));
#132645=CARTESIAN_POINT('Ctrl Pts',(22.2842010377944,2.22068304692898,-6.95222759534592));
#132646=CARTESIAN_POINT('Ctrl Pts',(22.1371485266208,2.25440663767665,-6.94345124070746));
#132647=CARTESIAN_POINT('Ctrl Pts',(22.0394357345041,2.26513154795565,-6.93794718681885));
#132648=CARTESIAN_POINT('Ctrl Pts',(21.9199669069424,2.26432629184898,-6.93072511192586));
#132649=CARTESIAN_POINT('Ctrl Pts',(21.8984654055484,2.26363247000938,-6.92940483284868));
#132650=CARTESIAN_POINT('Ctrl Pts',(21.8604483318462,2.26143387185808,-6.92701816159079));
#132651=CARTESIAN_POINT('Ctrl Pts',(21.8439259107583,2.26015201157404,-6.92596228362889));
#132652=CARTESIAN_POINT('Ctrl Pts',(21.7982629451956,2.25570504719778,-6.92299679427486));
#132653=CARTESIAN_POINT('Ctrl Pts',(21.7692012973077,2.25185097393195,-6.92105736487237));
#132654=CARTESIAN_POINT('Ctrl Pts',(21.696613600545,2.23964441021518,-6.9161212406612));
#132655=CARTESIAN_POINT('Ctrl Pts',(21.6533428573753,2.23000698680476,-6.91309542446328));
#132656=CARTESIAN_POINT('Ctrl Pts',(21.5317557998315,2.19613651961983,-6.90447520369459));
#132657=CARTESIAN_POINT('Ctrl Pts',(21.4551553100821,2.16653458018866,-6.89891502349031));
#132658=CARTESIAN_POINT('Ctrl Pts',(21.3536001712636,2.11547050081701,-6.89150827998112));
#132659=CARTESIAN_POINT('Ctrl Pts',(21.3257951654428,2.10015262423619,-6.88947397030077));
#132660=CARTESIAN_POINT('Ctrl Pts',(21.2739805442903,2.06901012222855,-6.8856647425911));
#132661=CARTESIAN_POINT('Ctrl Pts',(21.2498769318876,2.05338161859388,-6.88388462258408));
#132662=CARTESIAN_POINT('Ctrl Pts',(21.1887028702218,2.01068875622358,-6.8793296808101));
#132663=CARTESIAN_POINT('Ctrl Pts',(21.1525354679066,1.98240317723918,-6.87660049088308));
#132664=CARTESIAN_POINT('Ctrl Pts',(21.0660967739793,1.90687536981503,-6.86987776175335));
#132665=CARTESIAN_POINT('Ctrl Pts',(21.0180038698156,1.85737451268228,-6.86595206847186));
#132666=CARTESIAN_POINT('Ctrl Pts',(20.9445941419729,1.76829934022167,-6.85924854932783));
#132667=CARTESIAN_POINT('Ctrl Pts',(20.9170119033821,1.73079383200894,-6.85651503189649));
#132668=CARTESIAN_POINT('Ctrl Pts',(20.8812538929564,1.67608944724294,-6.85252525943183));
#132669=CARTESIAN_POINT('Ctrl Pts',(20.8713009601347,1.66009353286491,-6.85135820117931));
#132670=CARTESIAN_POINT('Ctrl Pts',(20.8527068172351,1.6286657019775,-6.8490526053752));
#132671=CARTESIAN_POINT('Ctrl Pts',(20.8440248971968,1.61326328403275,-6.8479165160438));
#132672=CARTESIAN_POINT('Ctrl Pts',(20.8166975525861,1.56231390591735,-6.84415034578213));
#132673=CARTESIAN_POINT('Ctrl Pts',(20.7994221081287,1.52606210176704,-6.84145871909278));
#132674=CARTESIAN_POINT('Ctrl Pts',(20.7509371966222,1.41045475984126,-6.83295770041728));
#132675=CARTESIAN_POINT('Ctrl Pts',(20.7260013998426,1.32871605246627,-6.82708106795391));
#132676=CARTESIAN_POINT('Ctrl Pts',(20.7012940701894,1.20365947452558,-6.8185858665388));
#132677=CARTESIAN_POINT('Ctrl Pts',(20.6951888115559,1.16184306796678,-6.8158209408496));
#132678=CARTESIAN_POINT('Ctrl Pts',(20.6884970714627,1.09152628403947,-6.81129810265361));
#132679=CARTESIAN_POINT('Ctrl Pts',(20.6867596803886,1.06317272302595,-6.80950804890915));
#132680=CARTESIAN_POINT('Ctrl Pts',(20.6850738156102,1.00190778767717,-6.80570397500247));
#132681=CARTESIAN_POINT('Ctrl Pts',(20.685451990105,0.969008127792423,-6.80370086054496));
#132682=CARTESIAN_POINT('Ctrl Pts',(20.6889935345336,0.898950803247316,
-6.79949479316228));
#132683=CARTESIAN_POINT('Ctrl Pts',(20.6925179295186,0.861842986321424,
-6.7973028541908));
#132684=CARTESIAN_POINT('Ctrl Pts',(20.7104488830827,0.733568411109644,
-6.78976070684839));
#132685=CARTESIAN_POINT('Ctrl Pts',(20.7331824769302,0.643874770766013,
-6.78456552064773));
#132686=CARTESIAN_POINT('Ctrl Pts',(20.7743138370979,0.533779686459548,
-6.77753390829196));
#132687=CARTESIAN_POINT('Ctrl Pts',(20.7838683191025,0.51037151850517,-6.77599745183441));
#132688=CARTESIAN_POINT('Ctrl Pts',(20.8007334967601,0.472351385461223,
-6.77340899431203));
#132689=CARTESIAN_POINT('Ctrl Pts',(20.8076369258322,0.457567420316831,
-6.77237783259001));
#132690=CARTESIAN_POINT('Ctrl Pts',(20.8254131762144,0.421344301150035,
-6.7697876802359));
#132691=CARTESIAN_POINT('Ctrl Pts',(20.836613790816,0.400075902066019,-6.76821255840321));
#132692=CARTESIAN_POINT('Ctrl Pts',(20.8641128378357,0.351284455593395,
-6.76449142200549));
#132693=CARTESIAN_POINT('Ctrl Pts',(20.8808632207748,0.32403467279011,-6.76233025450739));
#132694=CARTESIAN_POINT('Ctrl Pts',(20.9474008643691,0.224460394373303,
-6.7541831645393));
#132695=CARTESIAN_POINT('Ctrl Pts',(21.0036489697528,0.156738807302235,
-6.74814774155795));
#132696=CARTESIAN_POINT('Ctrl Pts',(21.0933645015358,0.0691133248970699,
-6.73985523634111));
#132697=CARTESIAN_POINT('Ctrl Pts',(21.1214269165456,0.0440494411410075,
-6.73741120008417));
#132698=CARTESIAN_POINT('Ctrl Pts',(21.1723565606275,0.00249218114765082,
-6.73322401034571));
#132699=CARTESIAN_POINT('Ctrl Pts',(21.1947341116024,-0.0145564527277919,
-6.73146054951477));
#132700=CARTESIAN_POINT('Ctrl Pts',(21.2466254174067,-0.0514212512889634,
-6.72752940875522));
#132701=CARTESIAN_POINT('Ctrl Pts',(21.2764436592025,-0.0707682455996173,
-6.72537950856607));
#132702=CARTESIAN_POINT('Ctrl Pts',(21.3436034248488,-0.110426309120024,
-6.72073426415478));
#132703=CARTESIAN_POINT('Ctrl Pts',(21.38123348881,-0.130162987160132,-6.71825671179315));
#132704=CARTESIAN_POINT('Ctrl Pts',(21.4924773583885,-0.181543219386842,
-6.71116278146636));
#132705=CARTESIAN_POINT('Ctrl Pts',(21.5681861558721,-0.208133907758561,
-6.70661885548462));
#132706=CARTESIAN_POINT('Ctrl Pts',(21.6703019322688,-0.233434882759522,
-6.70032254202073));
#132707=CARTESIAN_POINT('Ctrl Pts',(21.694883819683,-0.238752666230422,
-6.69879366072573));
#132708=CARTESIAN_POINT('Ctrl Pts',(21.7356526564801,-0.246307270359711,
-6.69621274823031));
#132709=CARTESIAN_POINT('Ctrl Pts',(21.7517528162549,-0.248969410577584,
-6.6951811815374));
#132710=CARTESIAN_POINT('Ctrl Pts',(21.7918239997672,-0.254800802836197,
-6.69258130711573));
#132711=CARTESIAN_POINT('Ctrl Pts',(21.8158405486243,-0.25759523402539,
-6.69099652089502));
#132712=CARTESIAN_POINT('Ctrl Pts',(21.8720660704988,-0.262508526584901,
-6.68724567675781));
#132713=CARTESIAN_POINT('Ctrl Pts',(21.9043057432556,-0.264085953687192,
-6.68506416753593));
#132714=CARTESIAN_POINT('Ctrl Pts',(22.0243936500095,-0.265361582990704,
-6.67689295696047));
#132715=CARTESIAN_POINT('Ctrl Pts',(22.1120879124508,-0.257141564761878,
-6.67085666184916));
#132716=CARTESIAN_POINT('Ctrl Pts',(22.2348177933554,-0.232571167358713,
-6.66258516992038));
#132717=CARTESIAN_POINT('Ctrl Pts',(22.2710698533072,-0.223628801507223,
-6.66016111164593));
#132718=CARTESIAN_POINT('Ctrl Pts',(22.3338561783121,-0.205157907870959,
-6.65599388783242));
#132719=CARTESIAN_POINT('Ctrl Pts',(22.3605652756198,-0.196322487082332,
-6.65423114745454));
#132720=CARTESIAN_POINT('Ctrl Pts',(22.3881777505251,-0.186154364635265,
-6.65241463787186));
#132721=CARTESIAN_POINT('Ctrl Pts',(22.3893955932103,-0.185703770054698,
-6.65233453257165));
#132722=CARTESIAN_POINT('Ctrl Pts',(22.3906127229569,-0.185251306619802,
-6.65225448505536));
#132723=CARTESIAN_POINT('Origin',(21.9499999789786,0.999999999999992,-6.00000000000001));
#132724=CARTESIAN_POINT('',(22.3906127230461,-0.185251306586623,-6.15441073460198));
#132725=CARTESIAN_POINT('',(22.3906686070801,-0.185465307370993,-6.2896766972819));
#132726=CARTESIAN_POINT('',(22.3906127231008,-0.185251306566283,-6.00000000000001));
#132727=CARTESIAN_POINT('',(22.908116131701,1.82521129893649,-6.00000000000001));
#132728=CARTESIAN_POINT('Ctrl Pts',(22.3906127229914,-0.185251306606962,
-6.15441073460198));
#132729=CARTESIAN_POINT('Ctrl Pts',(22.4057011923799,-0.179642224496554,
-6.15337585754839));
#132730=CARTESIAN_POINT('Ctrl Pts',(22.4206806463947,-0.173745732741962,
-6.15232558575311));
#132731=CARTESIAN_POINT('Ctrl Pts',(22.4576526446442,-0.158370580821461,
-6.14968303259365));
#132732=CARTESIAN_POINT('Ctrl Pts',(22.4794955608251,-0.148550359902258,
-6.1480767831395));
#132733=CARTESIAN_POINT('Ctrl Pts',(22.5513072346985,-0.113781092920369,
-6.14267246581676));
#132734=CARTESIAN_POINT('Ctrl Pts',(22.5999008878328,-0.0861433318381266,
-6.13881400970775));
#132735=CARTESIAN_POINT('Ctrl Pts',(22.7063613905894,-0.015884069010359,
-6.13006915257598));
#132736=CARTESIAN_POINT('Ctrl Pts',(22.7627535715962,0.0286415226550085,
-6.12522290339564));
#132737=CARTESIAN_POINT('Ctrl Pts',(22.8368763351462,0.0981661737317596,
-6.11860992756174));
#132738=CARTESIAN_POINT('Ctrl Pts',(22.8579495235599,0.119385561944241,
-6.11669608585324));
#132739=CARTESIAN_POINT('Ctrl Pts',(22.8970511659868,0.161655977368502,
-6.11307156243022));
#132740=CARTESIAN_POINT('Ctrl Pts',(22.9151786762439,0.18259134058388,-6.11135729054517));
#132741=CARTESIAN_POINT('Ctrl Pts',(22.9607684632705,0.238876208560583,
-6.10693888225787));
#132742=CARTESIAN_POINT('Ctrl Pts',(22.9870677755454,0.275118416270965,
-6.10427981671326));
#132743=CARTESIAN_POINT('Ctrl Pts',(23.0478711257816,0.369014067598781,
-6.09773532268297));
#132744=CARTESIAN_POINT('Ctrl Pts',(23.0798069369696,0.428160380031941,
-6.09391526460624));
#132745=CARTESIAN_POINT('Ctrl Pts',(23.1259659390328,0.532778844877155,
-6.08728611650922));
#132746=CARTESIAN_POINT('Ctrl Pts',(23.1425955202437,0.577026498993845,
-6.08451587356466));
#132747=CARTESIAN_POINT('Ctrl Pts',(23.1622512866886,0.639790576151933,
-6.08050092457355));
#132748=CARTESIAN_POINT('Ctrl Pts',(23.1674025017133,0.657603928892554,
-6.07935201345799));
#132749=CARTESIAN_POINT('Ctrl Pts',(23.1766212926487,0.692326984305418,
-6.07708267067493));
#132750=CARTESIAN_POINT('Ctrl Pts',(23.1807353231366,0.709220090239246,
-6.07596501277343));
#132751=CARTESIAN_POINT('Ctrl Pts',(23.1922838535727,0.761288044280355,
-6.07248866640026));
#132752=CARTESIAN_POINT('Ctrl Pts',(23.1985673161203,0.796697812072016,
-6.07008113187139));
#132753=CARTESIAN_POINT('Ctrl Pts',(23.2116825207765,0.894730342318195,
-6.06336937998488));
#132754=CARTESIAN_POINT('Ctrl Pts',(23.2153587510691,0.957672476655,-6.05901261864392));
#132755=CARTESIAN_POINT('Ctrl Pts',(23.2131961310744,1.09023716025245,-6.04994062542701));
#132756=CARTESIAN_POINT('Ctrl Pts',(23.2063134732515,1.15964331065296,-6.04525385919441));
#132757=CARTESIAN_POINT('Ctrl Pts',(23.1877691925515,1.26074208526004,-6.03856247798658));
#132758=CARTESIAN_POINT('Ctrl Pts',(23.1805085603149,1.29310064875821,-6.03644018423112));
#132759=CARTESIAN_POINT('Ctrl Pts',(23.1635107776574,1.356984199452,-6.0322773043734));
#132760=CARTESIAN_POINT('Ctrl Pts',(23.1537954632829,1.38848792858206,-6.03023791503399));
#132761=CARTESIAN_POINT('Ctrl Pts',(23.1310276328374,1.45321682865112,-6.02605223181921));
#132762=CARTESIAN_POINT('Ctrl Pts',(23.1177774201401,1.48634133539319,-6.02391286682768));
#132763=CARTESIAN_POINT('Ctrl Pts',(23.0616144632079,1.61116036503629,-6.01577950387353));
#132764=CARTESIAN_POINT('Ctrl Pts',(23.0091579730641,1.69812949140097,-6.00997918615594));
#132765=CARTESIAN_POINT('Ctrl Pts',(22.9343556261016,1.79399011384819,-6.00254541175663));
#132766=CARTESIAN_POINT('Ctrl Pts',(22.9214265697249,1.80975714108992,-6.00128356337885));
#132767=CARTESIAN_POINT('Ctrl Pts',(22.9081161317008,1.82521129893667,-6.));
#132768=CARTESIAN_POINT('',(20.9988875029867,1.83390743487766,-6.00000965788105));
#132769=CARTESIAN_POINT('Origin',(21.9499999789786,0.999999999999992,-6.00000000000001));
#132770=CARTESIAN_POINT('Ctrl Pts',(20.9988875029867,1.83390743487766,-6.00000965788105));
#132771=CARTESIAN_POINT('Ctrl Pts',(21.0286901916504,1.86779465086861,-6.00298051266928));
#132772=CARTESIAN_POINT('Ctrl Pts',(21.0603844609322,1.90012375983217,-6.00600667165696));
#132773=CARTESIAN_POINT('Ctrl Pts',(21.09376706437,1.9306946394671,-6.00903840021643));
#132774=CARTESIAN_POINT('Ctrl Pts',(21.1299596154473,1.96383879267031,-6.01232532152996));
#132775=CARTESIAN_POINT('Ctrl Pts',(21.1681370950843,1.99491683397022,-6.01561839937007));
#132776=CARTESIAN_POINT('Ctrl Pts',(21.2080211602335,2.02370881328864,-6.01887262241129));
#132777=CARTESIAN_POINT('Ctrl Pts',(21.2478716347671,2.0524765438174,-6.022124104725));
#132778=CARTESIAN_POINT('Ctrl Pts',(21.2894257342513,2.0789621813169,-6.0253366302436));
#132779=CARTESIAN_POINT('Ctrl Pts',(21.3323868181518,2.10297735669125,-6.02848774538209));
#132780=CARTESIAN_POINT('Ctrl Pts',(21.3753306942387,2.12698291292599,-6.03163759835963));
#132781=CARTESIAN_POINT('Ctrl Pts',(21.4196803982476,2.1485199368721,-6.03472607855688));
#132782=CARTESIAN_POINT('Ctrl Pts',(21.46512147125,2.16743080065149,-6.03775449719176));
#132783=CARTESIAN_POINT('Ctrl Pts',(21.5105945642123,2.18635498993266,-6.04078504979568));
#132784=CARTESIAN_POINT('Ctrl Pts',(21.5571605595361,2.20264911447047,-6.04375558047421));
#132785=CARTESIAN_POINT('Ctrl Pts',(21.6044863659149,2.2161876712167,-6.04669034846989));
#132786=CARTESIAN_POINT('Ctrl Pts',(21.6518292233586,2.22973110578392,-6.04962617383625));
#132787=CARTESIAN_POINT('Ctrl Pts',(21.6999324250985,2.24051662077448,-6.05252650726871));
#132788=CARTESIAN_POINT('Ctrl Pts',(21.7484446496936,2.2484552726454,-6.05543547749697));
#132789=CARTESIAN_POINT('Ctrl Pts',(21.7970413041404,2.25640774081118,-6.05834951044759));
#132790=CARTESIAN_POINT('Ctrl Pts',(21.8460482988538,2.26150284578719,-6.06127273889257));
#132791=CARTESIAN_POINT('Ctrl Pts',(21.8950953201096,2.26369509549222,-6.06426330924486));
#132792=CARTESIAN_POINT('Ctrl Pts',(21.9256270201211,2.26505976777263,-6.0661249349771));
#132793=CARTESIAN_POINT('Ctrl Pts',(21.9561738762397,2.2653004590272,-6.06801291925003));
#132794=CARTESIAN_POINT('Ctrl Pts',(21.986643756937,2.26441650318461,-6.06994229671044));
#132795=CARTESIAN_POINT('Ctrl Pts',(21.986660132454,2.26441602811763,-6.06994333362141));
#132796=CARTESIAN_POINT('Ctrl Pts',(21.9866765079491,2.264415552726,-6.06994437054433));
#132797=CARTESIAN_POINT('Ctrl Pts',(21.9866928834221,2.26441507700973,-6.06994540747922));
#132798=CARTESIAN_POINT('Ctrl Pts',(22.0326809237129,2.2630790997727,-6.07285748232858));
#132799=CARTESIAN_POINT('Ctrl Pts',(22.0786682668699,2.25916991357468,-6.07587157755844));
#132800=CARTESIAN_POINT('Ctrl Pts',(22.1243556678835,2.25272547701368,-6.07892867334182));
#132801=CARTESIAN_POINT('Ctrl Pts',(22.1291582634149,2.2520480468788,-6.07925003096389));
#132802=CARTESIAN_POINT('Ctrl Pts',(22.133957507768,2.25134263235827,-6.07957186373863));
#132803=CARTESIAN_POINT('Ctrl Pts',(22.1387530280941,2.25060929931715,-6.07989410311142));
#132804=CARTESIAN_POINT('Ctrl Pts',(22.1878297144056,2.24310447123295,-6.08319185591832));
#132805=CARTESIAN_POINT('Ctrl Pts',(22.2365212677171,2.23267260072574,-6.08653164154161));
#132806=CARTESIAN_POINT('Ctrl Pts',(22.2844718942759,2.21940438098023,-6.08985504759089));
#132807=CARTESIAN_POINT('Ctrl Pts',(22.3323791486108,2.20614816258353,-6.09317544755826));
#132808=CARTESIAN_POINT('Ctrl Pts',(22.3795469665926,2.19006100091275,-6.09647920494974));
#132809=CARTESIAN_POINT('Ctrl Pts',(22.4256372421703,2.17126745842227,-6.09972950322665));
#132810=CARTESIAN_POINT('Ctrl Pts',(22.4717048879636,2.15248314334057,-6.10297820564525));
#132811=CARTESIAN_POINT('Ctrl Pts',(22.516696097646,2.13099517083427,-6.10617340736871));
#132812=CARTESIAN_POINT('Ctrl Pts',(22.5602884459666,2.10695954641308,-6.1093025953749));
#132813=CARTESIAN_POINT('Ctrl Pts',(22.6060509761539,2.08172734327377,-6.11258756546968));
#132814=CARTESIAN_POINT('Ctrl Pts',(22.6502716692536,2.05368713042489,-6.11579961957646));
#132815=CARTESIAN_POINT('Ctrl Pts',(22.6925957272256,2.02305700606354,-6.11895337160971));
#132816=CARTESIAN_POINT('Ctrl Pts',(22.7329495418233,1.99385275631031,-6.12196031212854));
#132817=CARTESIAN_POINT('Ctrl Pts',(22.7715791222734,1.96229419772647,-6.12491466625996));
#132818=CARTESIAN_POINT('Ctrl Pts',(22.8081948530333,1.92860496734828,-6.1278522924454));
#132819=CARTESIAN_POINT('Ctrl Pts',(22.8448331350749,1.89489498809229,-6.13079172788697));
#132820=CARTESIAN_POINT('Ctrl Pts',(22.8794546905557,1.85905144030258,-6.1337148321294));
#132821=CARTESIAN_POINT('Ctrl Pts',(22.9117913162614,1.82133568321041,-6.13667550720105));
#132822=CARTESIAN_POINT('Ctrl Pts',(22.9415978529287,1.78657089028073,-6.13940453251391));
#132823=CARTESIAN_POINT('Ctrl Pts',(22.9694631685719,1.75021490169197,-6.14216607008642));
#132824=CARTESIAN_POINT('Ctrl Pts',(22.9951985991147,1.7125056088617,-6.14500991311024));
#132825=CARTESIAN_POINT('Ctrl Pts',(22.9974292928614,1.70923704556444,-6.1452564115257));
#132826=CARTESIAN_POINT('Ctrl Pts',(22.9996440150743,1.70595830355076,-6.1455035283072));
#132827=CARTESIAN_POINT('Ctrl Pts',(23.0018426600711,1.70266953085443,-6.14575129588088));
#132828=CARTESIAN_POINT('Ctrl Pts',(23.0057821587272,1.69677675797102,-6.14619524204998));
#132829=CARTESIAN_POINT('Ctrl Pts',(23.0096699883344,1.69085189810752,-6.14664128249749));
#132830=CARTESIAN_POINT('Ctrl Pts',(23.0135055153554,1.68489591262325,-6.14708960513326));
#132831=CARTESIAN_POINT('Ctrl Pts',(23.013514654098,1.68488172155684,-6.14709067333202));
#132832=CARTESIAN_POINT('Ctrl Pts',(23.0135237925438,1.68486753031373,-6.14709174154373));
#132833=CARTESIAN_POINT('Ctrl Pts',(23.0135329306927,1.68485333889393,-6.14709280976841));
#132834=CARTESIAN_POINT('Ctrl Pts',(23.0383604653831,1.64629651813792,-6.14999508084554));
#132835=CARTESIAN_POINT('Ctrl Pts',(23.0610808588401,1.60628993946131,-6.15300039228515));
#132836=CARTESIAN_POINT('Ctrl Pts',(23.0815561499041,1.56509966304113,-6.15604955149147));
#132837=CARTESIAN_POINT('Ctrl Pts',(23.0837750031228,1.56063598156621,-6.15637998082204));
#132838=CARTESIAN_POINT('Ctrl Pts',(23.0859674949999,1.55615844960958,-6.15671092507817));
#132839=CARTESIAN_POINT('Ctrl Pts',(23.0881334539325,1.55166744219402,-6.15704230893076));
#132840=CARTESIAN_POINT('Ctrl Pts',(23.1096475742327,1.50705899078141,-6.16033389122385));
#132841=CARTESIAN_POINT('Ctrl Pts',(23.1285441657354,1.46111522005574,-6.16366829876123));
#132842=CARTESIAN_POINT('Ctrl Pts',(23.1446964210521,1.41417901002546,-6.16698677355879));
#132843=CARTESIAN_POINT('Ctrl Pts',(23.1608334138497,1.36728715075519,-6.17030211267753));
#132844=CARTESIAN_POINT('Ctrl Pts',(23.1742315647608,1.31940476171366,-6.17360125719417));
#132845=CARTESIAN_POINT('Ctrl Pts',(23.1848019649728,1.27087942969894,-6.1768470231628));
#132846=CARTESIAN_POINT('Ctrl Pts',(23.195366813583,1.22237958331531,-6.18009108444666));
#132847=CARTESIAN_POINT('Ctrl Pts',(23.2031069616019,1.17323747086701,-6.18328172876644));
#132848=CARTESIAN_POINT('Ctrl Pts',(23.2079682928694,1.12380562289868,-6.18640604697854));
#132849=CARTESIAN_POINT('Ctrl Pts',(23.2128291111351,1.07437899132607,-6.18953003549064));
#132850=CARTESIAN_POINT('Ctrl Pts',(23.2148116257186,1.02466270822257,-6.19258776206157));
#132851=CARTESIAN_POINT('Ctrl Pts',(23.2138965373217,0.975014523593003,
-6.1955908500668));
#132852=CARTESIAN_POINT('Ctrl Pts',(23.2129805785505,0.925319116745311,
-6.19859679441971));
#132853=CARTESIAN_POINT('Ctrl Pts',(23.209161243197,0.875692002999865,-6.20154819210288));
#132854=CARTESIAN_POINT('Ctrl Pts',(23.2024566986069,0.826496664179489,
-6.20447946551915));
#132855=CARTESIAN_POINT('Ctrl Pts',(23.195748241031,0.777272613392309,-6.20741244971995));
#132856=CARTESIAN_POINT('Ctrl Pts',(23.1861507743226,0.728481007109299,
-6.21032568483769));
#132857=CARTESIAN_POINT('Ctrl Pts',(23.1737252053094,0.680489037516421,
-6.21327203773247));
#132858=CARTESIAN_POINT('Ctrl Pts',(23.1621874248703,0.635926023346594,
-6.21600787805978));
#132859=CARTESIAN_POINT('Ctrl Pts',(23.1482108799797,0.592052120796729,
-6.21877285073307));
#132860=CARTESIAN_POINT('Ctrl Pts',(23.1318842122252,0.549162471506275,
-6.22161761851486));
#132861=CARTESIAN_POINT('Ctrl Pts',(23.1305985213221,0.545785001421174,
-6.22184163802168));
#132862=CARTESIAN_POINT('Ctrl Pts',(23.1292982629967,0.542413608841275,
-6.22206615235655));
#132863=CARTESIAN_POINT('Ctrl Pts',(23.1279834833797,0.539048424415133,
-6.22229118625981));
#132864=CARTESIAN_POINT('Ctrl Pts',(23.124196597574,0.529355872924713,-6.22293933875854));
#132865=CARTESIAN_POINT('Ctrl Pts',(23.1202893850572,0.519715057120877,
-6.22359181589556));
#132866=CARTESIAN_POINT('Ctrl Pts',(23.1162632099014,0.510129357139251,
-6.22424921766053));
#132867=CARTESIAN_POINT('Ctrl Pts',(23.1162565869514,0.510113588920277,
-6.22425029906877));
#132868=CARTESIAN_POINT('Ctrl Pts',(23.1162499636796,0.510097820850403,
-6.22425138049034));
#132869=CARTESIAN_POINT('Ctrl Pts',(23.1162433400858,0.510082052929644,
-6.22425246192524));
#132870=CARTESIAN_POINT('Ctrl Pts',(23.0984965463045,0.467834588966754,
-6.22714998294805));
#132871=CARTESIAN_POINT('Ctrl Pts',(23.0783667308209,0.426505274501597,
-6.23015061953357));
#132872=CARTESIAN_POINT('Ctrl Pts',(23.0559954974735,0.386357985883809,
-6.23319539900638));
#132873=CARTESIAN_POINT('Ctrl Pts',(23.0542030444861,0.38314125990796,-6.23343935623384));
#132874=CARTESIAN_POINT('Ctrl Pts',(23.0523962263639,0.37993213579517,-6.23368359684601));
#132875=CARTESIAN_POINT('Ctrl Pts',(23.0505751287022,0.376730756018156,
-6.23392809050927));
#132876=CARTESIAN_POINT('Ctrl Pts',(23.0260598235902,0.333634329250968,
-6.23721942236857));
#132877=CARTESIAN_POINT('Ctrl Pts',(22.9989521667812,0.291938164542877,
-6.24055601012744));
#132878=CARTESIAN_POINT('Ctrl Pts',(22.9694634631529,0.251942012917784,
-6.24387848847534));
#132879=CARTESIAN_POINT('Ctrl Pts',(22.940003946175,0.211985447763226,-6.24719767837709));
#132880=CARTESIAN_POINT('Ctrl Pts',(22.9081683055633,0.173725286597264,
-6.25050248569246));
#132881=CARTESIAN_POINT('Ctrl Pts',(22.8741931459292,0.137432405205992,
-6.25375499851268));
#132882=CARTESIAN_POINT('Ctrl Pts',(22.8402243688189,0.101146341742298,
-6.25700690032059));
#132883=CARTESIAN_POINT('Ctrl Pts',(22.8041169244941,0.0668267464994518,
-6.26020642568044));
#132884=CARTESIAN_POINT('Ctrl Pts',(22.7661313802783,0.0347187356368984,
-6.26333990837154));
#132885=CARTESIAN_POINT('Ctrl Pts',(22.7281530948429,0.00261686039791348,
-6.2664727922753));
#132886=CARTESIAN_POINT('Ctrl Pts',(22.6882973927823,-0.0272741915223843,
-6.26953970530947));
#132887=CARTESIAN_POINT('Ctrl Pts',(22.6468487220025,-0.0547351490927038,
-6.27255159353335));
#132888=CARTESIAN_POINT('Ctrl Pts',(22.6053564963114,-0.0822249630666226,
-6.27556664669647));
#132889=CARTESIAN_POINT('Ctrl Pts',(22.562267857641,-0.107279327169208,
-6.27852675107654));
#132890=CARTESIAN_POINT('Ctrl Pts',(22.5178932287369,-0.129706502125296,
-6.2814657934101));
#132891=CARTESIAN_POINT('Ctrl Pts',(22.4765123176448,-0.150620636075763,
-6.28420655434724));
#132892=CARTESIAN_POINT('Ctrl Pts',(22.434013247025,-0.169250079969709,
-6.28692948158993));
#132893=CARTESIAN_POINT('Ctrl Pts',(22.3906686070801,-0.185465307370996,
-6.2896766972819));
#132894=CARTESIAN_POINT('Origin',(21.9499999789786,0.999999999999992,-4.89578827641128));
#132895=CARTESIAN_POINT('',(22.8894915957587,2.22401164291841,-7.78024830238043));
#132896=CARTESIAN_POINT('',(22.889491610182,2.22401163184779,-7.82252261963806));
#132897=CARTESIAN_POINT('',(22.8894916101512,2.22401163187148,-4.89578827641128));
#132898=CARTESIAN_POINT('',(22.3485138208359,-0.490649428218508,-8.00000000000001));
#132899=CARTESIAN_POINT('Ctrl Pts',(22.889491610182,2.22401163184779,-7.82252261963806));
#132900=CARTESIAN_POINT('Ctrl Pts',(22.8898635485898,2.22372615006616,-7.82254904469854));
#132901=CARTESIAN_POINT('Ctrl Pts',(22.8902353594378,2.22344049679263,-7.82257547297005));
#132902=CARTESIAN_POINT('Ctrl Pts',(22.9584420387731,2.17098949790154,-7.82742584661769));
#132903=CARTESIAN_POINT('Ctrl Pts',(23.0218183424636,2.11327304613071,-7.83235239300052));
#132904=CARTESIAN_POINT('Ctrl Pts',(23.1068674277578,2.02178972213453,-7.83935303997649));
#132905=CARTESIAN_POINT('Ctrl Pts',(23.1325426168569,1.99196261873962,-7.84152587714254));
#132906=CARTESIAN_POINT('Ctrl Pts',(23.1683716943707,1.94696864979136,-7.84461104845634));
#132907=CARTESIAN_POINT('Ctrl Pts',(23.1794407656144,1.93255277116917,-7.84557223559737));
#132908=CARTESIAN_POINT('Ctrl Pts',(23.2000218049921,1.90474530731534,-7.84736979107497));
#132909=CARTESIAN_POINT('Ctrl Pts',(23.2095790772173,1.89139168657683,-7.84820843300643));
#132910=CARTESIAN_POINT('Ctrl Pts',(23.2361293666813,1.85301520523579,-7.85055550327267));
#132911=CARTESIAN_POINT('Ctrl Pts',(23.2526030596146,1.82764072472637,-7.85203360653475));
#132912=CARTESIAN_POINT('Ctrl Pts',(23.2911235882287,1.76430495959742,-7.85558658151277));
#132913=CARTESIAN_POINT('Ctrl Pts',(23.3123173991765,1.72585549298537,-7.85762877496279));
#132914=CARTESIAN_POINT('Ctrl Pts',(23.3846576998291,1.58025425398773,-7.8651233531947));
#132915=CARTESIAN_POINT('Ctrl Pts',(23.4250265827451,1.46822364563206,-7.87046371008796));
#132916=CARTESIAN_POINT('Ctrl Pts',(23.4599090754759,1.31964723972354,-7.8778737839146));
#132917=CARTESIAN_POINT('Ctrl Pts',(23.4665712002994,1.28637624954946,-7.87955029503946));
#132918=CARTESIAN_POINT('Ctrl Pts',(23.4765429513912,1.22636255077981,-7.88261868401024));
#132919=CARTESIAN_POINT('Ctrl Pts',(23.4802590236487,1.19970125063584,-7.88399722774642));
#132920=CARTESIAN_POINT('Ctrl Pts',(23.4870124430072,1.13983186497366,-7.88713193073266));
#132921=CARTESIAN_POINT('Ctrl Pts',(23.4896744184964,1.10659578293834,-7.88889896610823));
#132922=CARTESIAN_POINT('Ctrl Pts',(23.4949036162639,0.996644662793407,
-7.89483554001359));
#132923=CARTESIAN_POINT('Ctrl Pts',(23.4928250647758,0.919830638399253,
-7.89913529926684));
#132924=CARTESIAN_POINT('Ctrl Pts',(23.4750586052286,0.745570115913723,
-7.90909402318625));
#132925=CARTESIAN_POINT('Ctrl Pts',(23.4557265847982,0.648820166733901,
-7.91477608861073));
#132926=CARTESIAN_POINT('Ctrl Pts',(23.4214552654331,0.535156542065498,
-7.92121807243912));
#132927=CARTESIAN_POINT('Ctrl Pts',(23.4152197841016,0.51586045315267,-7.92230257536467));
#132928=CARTESIAN_POINT('Ctrl Pts',(23.4033404750406,0.481433768169408,
-7.92421382447387));
#132929=CARTESIAN_POINT('Ctrl Pts',(23.397836830251,0.466260367432381,-7.92504717392675));
#132930=CARTESIAN_POINT('Ctrl Pts',(23.3831498789931,0.427668883517724,
-7.92714785785703));
#132931=CARTESIAN_POINT('Ctrl Pts',(23.3736303738123,0.40438420925236,-7.9283978513551));
#132932=CARTESIAN_POINT('Ctrl Pts',(23.3505507784266,0.351650659952187,
-7.93120874318343));
#132933=CARTESIAN_POINT('Ctrl Pts',(23.3366233219783,0.322375256239287,
-7.9327546230739));
#132934=CARTESIAN_POINT('Ctrl Pts',(23.279694037837,0.211828629361794,-7.93860553967999));
#132935=CARTESIAN_POINT('Ctrl Pts',(23.2303838546479,0.134021665293877,
-7.94276242087797));
#132936=CARTESIAN_POINT('Ctrl Pts',(23.1338177743768,0.00809238171863846,
-7.95015372417362));
#132937=CARTESIAN_POINT('Ctrl Pts',(23.0898044425818,-0.0421852376196696,
-7.95331877871642));
#132938=CARTESIAN_POINT('Ctrl Pts',(23.0183295296939,-0.113871633295997,
-7.95829426390745));
#132939=CARTESIAN_POINT('Ctrl Pts',(22.9931722255307,-0.137466264300778,
-7.96001769657505));
#132940=CARTESIAN_POINT('Ctrl Pts',(22.9434664337016,-0.181047686565909,
-7.9633821547244));
#132941=CARTESIAN_POINT('Ctrl Pts',(22.9190518222137,-0.201160936123177,
-7.96501734641841));
#132942=CARTESIAN_POINT('Ctrl Pts',(22.8545967442228,-0.251015550072751,
-7.96929485261125));
#132943=CARTESIAN_POINT('Ctrl Pts',(22.8137030758859,-0.279590405128052,
-7.97197238475304));
#132944=CARTESIAN_POINT('Ctrl Pts',(22.6679253088973,-0.371278140795948,
-7.98137216582847));
#132945=CARTESIAN_POINT('Ctrl Pts',(22.5569746768909,-0.423868254770818,
-7.98831317868678));
#132946=CARTESIAN_POINT('Ctrl Pts',(22.423651150773,-0.468617633822337,
-7.99588534263564));
#132947=CARTESIAN_POINT('Ctrl Pts',(22.4062179835011,-0.474126304133557,
-7.99686039556757));
#132948=CARTESIAN_POINT('Ctrl Pts',(22.3753503458647,-0.483280039559475,
-7.99855641085894));
#132949=CARTESIAN_POINT('Ctrl Pts',(22.3619568853333,-0.487055526676146,
-7.99928234965091));
#132950=CARTESIAN_POINT('Ctrl Pts',(22.3485138208359,-0.490649428218505,
-8.));
#132951=CARTESIAN_POINT('',(21.5504184355883,-0.491444307170665,-7.99938271504714));
#132952=CARTESIAN_POINT('Origin',(21.9499999789786,0.999999999999992,-8.00000000000001));
#132953=CARTESIAN_POINT('Ctrl Pts',(21.5507417872889,-0.49045023277154,
-7.99877818246404));
#132954=CARTESIAN_POINT('Ctrl Pts',(21.684483670055,-0.526276683794352,
-7.99205016521409));
#132955=CARTESIAN_POINT('Ctrl Pts',(21.8224480500903,-0.543942214410516,
-7.98592091362909));
#132956=CARTESIAN_POINT('Ctrl Pts',(22.0076445340552,-0.542630388429268,
-7.97709993740197));
#132957=CARTESIAN_POINT('Ctrl Pts',(22.0543175938958,-0.540178169116188,
-7.97483282718998));
#132958=CARTESIAN_POINT('Ctrl Pts',(22.1300476144749,-0.532741075226077,
-7.97104119923413));
#132959=CARTESIAN_POINT('Ctrl Pts',(22.1592005200333,-0.529034776397013,
-7.96955425248215));
#132960=CARTESIAN_POINT('Ctrl Pts',(22.2185250141901,-0.519764318499925,
-7.96646495803174));
#132961=CARTESIAN_POINT('Ctrl Pts',(22.2486719472076,-0.514128187063365,
-7.96486109129298));
#132962=CARTESIAN_POINT('Ctrl Pts',(22.3349526873501,-0.495320509388373,
-7.96016768204963));
#132963=CARTESIAN_POINT('Ctrl Pts',(22.3905386526835,-0.47989753293824,
-7.95701473113232));
#132964=CARTESIAN_POINT('Ctrl Pts',(22.5298702510011,-0.432691552635531,
-7.94881084346073));
#132965=CARTESIAN_POINT('Ctrl Pts',(22.6119540851012,-0.396664012856216,
-7.94368124252772));
#132966=CARTESIAN_POINT('Ctrl Pts',(22.7178990892324,-0.338715415524575,
-7.93690452528127));
#132967=CARTESIAN_POINT('Ctrl Pts',(22.7448882674401,-0.322868389504563,
-7.93516484143859));
#132968=CARTESIAN_POINT('Ctrl Pts',(22.7920362356633,-0.293220577486188,
-7.93212352032235));
#132969=CARTESIAN_POINT('Ctrl Pts',(22.8123845719503,-0.279741166603724,
-7.93081020265514));
#132970=CARTESIAN_POINT('Ctrl Pts',(22.8458680156909,-0.256399130905018,
-7.92865873181386));
#132971=CARTESIAN_POINT('Ctrl Pts',(22.8591798284966,-0.2468000552734,-7.92780650899487));
#132972=CARTESIAN_POINT('Ctrl Pts',(22.8904231188431,-0.223504089348374,
-7.92581458781756));
#132973=CARTESIAN_POINT('Ctrl Pts',(22.9082116631827,-0.209623248594206,
-7.92468586685922));
#132974=CARTESIAN_POINT('Ctrl Pts',(22.9815050389257,-0.149798734799642,
-7.92002979168096));
#132975=CARTESIAN_POINT('Ctrl Pts',(23.034064820614,-0.100383923271257,
-7.91667454246241));
#132976=CARTESIAN_POINT('Ctrl Pts',(23.1475970402999,0.0224162361659275,
-7.90891702684744));
#132977=CARTESIAN_POINT('Ctrl Pts',(23.2056052200213,0.0981335695832763,
-7.90453139757395));
#132978=CARTESIAN_POINT('Ctrl Pts',(23.2755930363982,0.209449138652271,
-7.89814265424258));
#132979=CARTESIAN_POINT('Ctrl Pts',(23.2938290078715,0.24086172682944,-7.89634763221282));
#132980=CARTESIAN_POINT('Ctrl Pts',(23.324084694423,0.297491370902265,-7.89310749174407));
#132981=CARTESIAN_POINT('Ctrl Pts',(23.336559926694,0.322446632448505,-7.89167838397129));
#132982=CARTESIAN_POINT('Ctrl Pts',(23.3628895160827,0.378892212641739,
-7.8884373539397));
#132983=CARTESIAN_POINT('Ctrl Pts',(23.3763807425985,0.410534641874167,
-7.88661461070158));
#132984=CARTESIAN_POINT('Ctrl Pts',(23.4145875705298,0.509156971457689,
-7.88091183326549));
#132985=CARTESIAN_POINT('Ctrl Pts',(23.4357205178586,0.577416881690707,
-7.87693014128697));
#132986=CARTESIAN_POINT('Ctrl Pts',(23.473692996158,0.738942701068894,-7.86752949903149));
#132987=CARTESIAN_POINT('Ctrl Pts',(23.4868258235285,0.832792439124259,
-7.86207848972414));
#132988=CARTESIAN_POINT('Ctrl Pts',(23.4925210920485,0.953460837313003,
-7.85543830034237));
#132989=CARTESIAN_POINT('Ctrl Pts',(23.4930894613947,0.979695454057876,
-7.85401775081592));
#132990=CARTESIAN_POINT('Ctrl Pts',(23.4929258171609,1.02225335893383,-7.85176374258021));
#132991=CARTESIAN_POINT('Ctrl Pts',(23.4926041471341,1.0385721741514,-7.85091175838352));
#132992=CARTESIAN_POINT('Ctrl Pts',(23.4912966068882,1.07530848984636,-7.84902399298244));
#132993=CARTESIAN_POINT('Ctrl Pts',(23.490163938166,1.09571686872353,-7.84799522589264));
#132994=CARTESIAN_POINT('Ctrl Pts',(23.4844035555486,1.17205844097231,-7.84420258776438));
#132995=CARTESIAN_POINT('Ctrl Pts',(23.4771308214474,1.22775148193488,-7.84154707939638));
#132996=CARTESIAN_POINT('Ctrl Pts',(23.4515938273841,1.3646610016949,-7.83504905181641));
#132997=CARTESIAN_POINT('Ctrl Pts',(23.4297677109401,1.44502724139663,-7.83125538581598));
#132998=CARTESIAN_POINT('Ctrl Pts',(23.3835267062311,1.57330813667429,-7.82481894732443));
#132999=CARTESIAN_POINT('Ctrl Pts',(23.3629035441215,1.62240179620157,-7.82225978846643));
#133000=CARTESIAN_POINT('Ctrl Pts',(23.3268218294822,1.69720958368327,-7.81814280302905));
#133001=CARTESIAN_POINT('Ctrl Pts',(23.3130805107826,1.72370638247791,-7.81664007640385));
#133002=CARTESIAN_POINT('Ctrl Pts',(23.2844661838071,1.77517261073433,-7.8136237035442));
#133003=CARTESIAN_POINT('Ctrl Pts',(23.269638969942,1.80015337106273,-7.81211204137438));
#133004=CARTESIAN_POINT('Ctrl Pts',(23.2290208064344,1.86438378038673,-7.80809379194539));
#133005=CARTESIAN_POINT('Ctrl Pts',(23.2021289864727,1.90289864861316,-7.80554994523843));
#133006=CARTESIAN_POINT('Ctrl Pts',(23.1339596224093,1.99161757948425,-7.79936801720477));
#133007=CARTESIAN_POINT('Ctrl Pts',(23.0911854309392,2.04055788104414,-7.79568842927852));
#133008=CARTESIAN_POINT('Ctrl Pts',(22.9966083279801,2.13590115824035,-7.78803989644304));
#133009=CARTESIAN_POINT('Ctrl Pts',(22.9445002796644,2.18178966106186,-7.78407766963962));
#133010=CARTESIAN_POINT('Ctrl Pts',(22.8894915957587,2.22401164291842,-7.78024830238043));
#133011=CARTESIAN_POINT('Origin',(21.9499999789786,0.999999999999992,-4.89578827641128));
#133012=CARTESIAN_POINT('',(22.8894915988056,2.22401164057975,-7.28231538991333));
#133013=CARTESIAN_POINT('',(22.889491673488,2.22401158325724,-7.32301705809308));
#133014=CARTESIAN_POINT('',(22.8894916101512,2.22401163187148,-4.89578827641128));
#133015=CARTESIAN_POINT('',(20.4070000765807,0.999451182879079,-7.64468155021554));
#133016=CARTESIAN_POINT('Ctrl Pts',(22.889491673488,2.22401158325724,-7.32301705809308));
#133017=CARTESIAN_POINT('Ctrl Pts',(22.9174806528591,2.20252860546791,-7.32465069545391));
#133018=CARTESIAN_POINT('Ctrl Pts',(22.9447372388077,2.18008218588996,-7.32628495168413));
#133019=CARTESIAN_POINT('Ctrl Pts',(23.0197626922916,2.11384526528419,-7.33096307828763));
#133020=CARTESIAN_POINT('Ctrl Pts',(23.0655639624875,2.06796984703058,-7.3340413964136));
#133021=CARTESIAN_POINT('Ctrl Pts',(23.1289816116115,1.99590515951898,-7.33877506694343));
#133022=CARTESIAN_POINT('Ctrl Pts',(23.1489002156125,1.97183477725879,-7.34034038117292));
#133023=CARTESIAN_POINT('Ctrl Pts',(23.1856445951545,1.92458136313975,-7.34339398889923));
#133024=CARTESIAN_POINT('Ctrl Pts',(23.2025823945152,1.90150178568562,-7.34487714599291));
#133025=CARTESIAN_POINT('Ctrl Pts',(23.2430084589554,1.8430765515422,-7.34861675317297));
#133026=CARTESIAN_POINT('Ctrl Pts',(23.2656981967317,1.80720924795092,-7.35089993945748));
#133027=CARTESIAN_POINT('Ctrl Pts',(23.343388625699,1.67240211298067,-7.35943294626908));
#133028=CARTESIAN_POINT('Ctrl Pts',(23.3889349482176,1.56843495398951,-7.36595299097858));
#133029=CARTESIAN_POINT('Ctrl Pts',(23.4328651501621,1.42792563815277,-7.37426533489055));
#133030=CARTESIAN_POINT('Ctrl Pts',(23.4419514411839,1.39508289850369,-7.37617185478681));
#133031=CARTESIAN_POINT('Ctrl Pts',(23.4559961654803,1.33688310572054,-7.3794593624945));
#133032=CARTESIAN_POINT('Ctrl Pts',(23.4614191737601,1.31165188862252,-7.38085507067608));
#133033=CARTESIAN_POINT('Ctrl Pts',(23.469205645451,1.27041507889937,-7.38307596209645));
#133034=CARTESIAN_POINT('Ctrl Pts',(23.4719546191998,1.25448834457933,-7.38391895058142));
#133035=CARTESIAN_POINT('Ctrl Pts',(23.4776546813915,1.21805746436626,-7.38581159163521));
#133036=CARTESIAN_POINT('Ctrl Pts',(23.4804440729965,1.19753202611035,-7.38685345524712));
#133037=CARTESIAN_POINT('Ctrl Pts',(23.4895700144441,1.11848163026228,-7.39079267040249));
#133038=CARTESIAN_POINT('Ctrl Pts',(23.4929694967009,1.05966462694489,-7.39357090071966));
#133039=CARTESIAN_POINT('Ctrl Pts',(23.4930614715204,0.880834542133844,
-7.40190366196691));
#133040=CARTESIAN_POINT('Ctrl Pts',(23.4791348666175,0.761284932770572,
-7.40735185444612));
#133041=CARTESIAN_POINT('Ctrl Pts',(23.4437488052126,0.611803904543438,
-7.41486325513049));
#133042=CARTESIAN_POINT('Ctrl Pts',(23.4349265867479,0.579316586949283,
-7.41653677307096));
#133043=CARTESIAN_POINT('Ctrl Pts',(23.4168013484243,0.520278644999048,
-7.41966737658068));
#133044=CARTESIAN_POINT('Ctrl Pts',(23.407821005861,0.493643840414046,-7.42111398176074));
#133045=CARTESIAN_POINT('Ctrl Pts',(23.3852925784078,0.432404852236581,
-7.42452567038954));
#133046=CARTESIAN_POINT('Ctrl Pts',(23.3712122651412,0.398016246501824,
-7.42650678676884));
#133047=CARTESIAN_POINT('Ctrl Pts',(23.337797951035,0.324132601264742,-7.43090906588496));
#133048=CARTESIAN_POINT('Ctrl Pts',(23.3179893484773,0.28488837636492,-7.43334264362142));
#133049=CARTESIAN_POINT('Ctrl Pts',(23.236198919598,0.138716953140601,-7.44274398069557));
#133050=CARTESIAN_POINT('Ctrl Pts',(23.1631330001449,0.0385303398521764,
-7.44994267268712));
#133051=CARTESIAN_POINT('Ctrl Pts',(23.0643556210841,-0.0674810929042513,
-7.45781349628265));
#133052=CARTESIAN_POINT('Ctrl Pts',(23.0494852719459,-0.0827910963252965,
-7.4589561060049));
#133053=CARTESIAN_POINT('Ctrl Pts',(23.0227871258641,-0.109161240994213,
-7.46092699576836));
#133054=CARTESIAN_POINT('Ctrl Pts',(23.0110954006843,-0.120351487063606,
-7.46176363932748));
#133055=CARTESIAN_POINT('Ctrl Pts',(22.981368965395,-0.147919990082372,
-7.46382778665516));
#133056=CARTESIAN_POINT('Ctrl Pts',(22.9631189616701,-0.164058561511551,
-7.46503989993721));
#133057=CARTESIAN_POINT('Ctrl Pts',(22.9205753568766,-0.199921262072684,
-7.46776183320603));
#133058=CARTESIAN_POINT('Ctrl Pts',(22.8960484320435,-0.219352322342665,
-7.46925776557148));
#133059=CARTESIAN_POINT('Ctrl Pts',(22.7994993422812,-0.291173631194641,
-7.4749384043586));
#133060=CARTESIAN_POINT('Ctrl Pts',(22.7235842798912,-0.33803835266542,
-7.47898627597311));
#133061=CARTESIAN_POINT('Ctrl Pts',(22.5901404182338,-0.405244647338239,
-7.4859933365481));
#133062=CARTESIAN_POINT('Ctrl Pts',(22.5346883073623,-0.42920643891053,
-7.48887462363873));
#133063=CARTESIAN_POINT('Ctrl Pts',(22.4490338252202,-0.46039827214964,
-7.4933776447817));
#133064=CARTESIAN_POINT('Ctrl Pts',(22.4197814008684,-0.470069096749479,
-7.49492378896884));
#133065=CARTESIAN_POINT('Ctrl Pts',(22.3626510756701,-0.487076964808972,
-7.49796886546628));
#133066=CARTESIAN_POINT('Ctrl Pts',(22.334818380678,-0.494521155600971,
-7.49946373531877));
#133067=CARTESIAN_POINT('Ctrl Pts',(22.2640441314933,-0.511342491691904,
-7.50329856917447));
#133068=CARTESIAN_POINT('Ctrl Pts',(22.220881979117,-0.519671781551221,
-7.50566853636649));
#133069=CARTESIAN_POINT('Ctrl Pts',(22.0689622849165,-0.542310778490602,
-7.51411276100414));
#133070=CARTESIAN_POINT('Ctrl Pts',(21.959089791038,-0.546863974449758,
-7.52042763261872));
#133071=CARTESIAN_POINT('Ctrl Pts',(21.8040087556298,-0.536759606479476,
-7.52920406591462));
#133072=CARTESIAN_POINT('Ctrl Pts',(21.7584916095135,-0.531753435522759,
-7.53175848313519));
#133073=CARTESIAN_POINT('Ctrl Pts',(21.6929704889091,-0.521580267026578,
-7.53534778085406));
#133074=CARTESIAN_POINT('Ctrl Pts',(21.6727430030873,-0.518024807557795,
-7.53644348220558));
#133075=CARTESIAN_POINT('Ctrl Pts',(21.6364961700584,-0.510904835171577,
-7.53837748730586));
#133076=CARTESIAN_POINT('Ctrl Pts',(21.6204535767768,-0.507487061365945,
-7.53922228011786));
#133077=CARTESIAN_POINT('Ctrl Pts',(21.5786297080394,-0.497877137387341,
-7.54139966970917));
#133078=CARTESIAN_POINT('Ctrl Pts',(21.5529485722373,-0.49127533430978,
-7.5427123542691));
#133079=CARTESIAN_POINT('Ctrl Pts',(21.49333990079,-0.474302659211232,-7.54572781863924));
#133080=CARTESIAN_POINT('Ctrl Pts',(21.4595742432316,-0.463417085448077,
-7.5474118348925));
#133081=CARTESIAN_POINT('Ctrl Pts',(21.3059050064523,-0.407959393115651,
-7.55507887264987));
#133082=CARTESIAN_POINT('Ctrl Pts',(21.1914675442868,-0.349754408263219,
-7.56084381663139));
#133083=CARTESIAN_POINT('Ctrl Pts',(21.0567624245766,-0.25864260638842,
-7.56877479948666));
#133084=CARTESIAN_POINT('Ctrl Pts',(21.0286687306386,-0.238225768625484,
-7.57049700206357));
#133085=CARTESIAN_POINT('Ctrl Pts',(20.9791109395356,-0.199589215092315,
-7.5736763646391));
#133086=CARTESIAN_POINT('Ctrl Pts',(20.9574109658991,-0.181696549192534,
-7.5751210249888));
#133087=CARTESIAN_POINT('Ctrl Pts',(20.9090664583786,-0.139562669637341,
-7.57846754215476));
#133088=CARTESIAN_POINT('Ctrl Pts',(20.8827581931345,-0.114962049900615,
-7.58038305171594));
#133089=CARTESIAN_POINT('Ctrl Pts',(20.8278163997992,-0.0598589172470465,
-7.58459582033289));
#133090=CARTESIAN_POINT('Ctrl Pts',(20.7995141819669,-0.0290670452530772,
-7.58690328428394));
#133091=CARTESIAN_POINT('Ctrl Pts',(20.7048788467948,0.0826829521462757,
-7.59509720996102));
#133092=CARTESIAN_POINT('Ctrl Pts',(20.6455600305647,0.169197788408244,
-7.60114996977033));
#133093=CARTESIAN_POINT('Ctrl Pts',(20.5787194885078,0.291720585798969,
-7.60893121394299));
#133094=CARTESIAN_POINT('Ctrl Pts',(20.5630314206416,0.322956109743386,
-7.61085024488963));
#133095=CARTESIAN_POINT('Ctrl Pts',(20.5410739466015,0.370647397965778,
-7.61365723245521));
#133096=CARTESIAN_POINT('Ctrl Pts',(20.5340036243639,0.38672058250917,-7.61458287806887));
#133097=CARTESIAN_POINT('Ctrl Pts',(20.520303458396,0.419366463448125,-7.61641708828457));
#133098=CARTESIAN_POINT('Ctrl Pts',(20.5136837186262,0.435940517543099,
-7.61732503682478));
#133099=CARTESIAN_POINT('Ctrl Pts',(20.4941171895752,0.487509680540059,
-7.62008920803211));
#133100=CARTESIAN_POINT('Ctrl Pts',(20.4821503907886,0.522863799232232,
-7.62189887160568));
#133101=CARTESIAN_POINT('Ctrl Pts',(20.4287708368372,0.701672871395411,
-7.63078168924784));
#133102=CARTESIAN_POINT('Ctrl Pts',(20.4070531773116,0.850158423141492,
-7.6373883095844));
#133103=CARTESIAN_POINT('Ctrl Pts',(20.4070000765807,0.999451182879078,
-7.64468155021554));
#133104=CARTESIAN_POINT('Ctrl Pts',(20.4070000761094,0.999452509765842,
-7.64468161503654));
#133105=CARTESIAN_POINT('Ctrl Pts',(20.4069914884943,1.02365511365021,-7.64586395966915));
#133106=CARTESIAN_POINT('Ctrl Pts',(20.4075523420559,1.0478539923095,-7.64706070389743));
#133107=CARTESIAN_POINT('Ctrl Pts',(20.4098303397597,1.09659975623545,-7.6495067341467));
#133108=CARTESIAN_POINT('Ctrl Pts',(20.4115658938258,1.12113839695251,-7.65075618920184));
#133109=CARTESIAN_POINT('Ctrl Pts',(20.4167554741822,1.17588051974584,-7.65358872521351));
#133110=CARTESIAN_POINT('Ctrl Pts',(20.4205169287147,1.20604393197918,-7.65518047584784));
#133111=CARTESIAN_POINT('Ctrl Pts',(20.4334913207319,1.28984679235276,-7.65969431087745));
#133112=CARTESIAN_POINT('Ctrl Pts',(20.4446539627764,1.3431358168734,-7.66267158712686));
#133113=CARTESIAN_POINT('Ctrl Pts',(20.4842124700803,1.49222414245962,-7.67127933065706));
#133114=CARTESIAN_POINT('Ctrl Pts',(20.5191225231289,1.58600828362626,-7.67704303295215));
#133115=CARTESIAN_POINT('Ctrl Pts',(20.5757445171939,1.70223815246044,-7.68430550542341));
#133116=CARTESIAN_POINT('Ctrl Pts',(20.5893997189086,1.72834303462435,-7.68594337704621));
#133117=CARTESIAN_POINT('Ctrl Pts',(20.6152059849074,1.77441545386583,-7.68882741006617));
#133118=CARTESIAN_POINT('Ctrl Pts',(20.6270792470567,1.79452825563682,-7.69008402747835));
#133119=CARTESIAN_POINT('Ctrl Pts',(20.6479170113864,1.82806343534428,-7.69216538973155));
#133120=CARTESIAN_POINT('Ctrl Pts',(20.6566429198552,1.84162739480979,-7.69300271689554));
#133121=CARTESIAN_POINT('Ctrl Pts',(20.6780538700932,1.873789856518,-7.69497760930347));
#133122=CARTESIAN_POINT('Ctrl Pts',(20.6909358458058,1.89225177079883,-7.69610370305999));
#133123=CARTESIAN_POINT('Ctrl Pts',(20.7487534790556,1.97136657519879,-7.70092546515341));
#133124=CARTESIAN_POINT('Ctrl Pts',(20.7977043778059,2.02896198846566,-7.70442897853137));
#133125=CARTESIAN_POINT('Ctrl Pts',(20.898527760055,2.13132889495774,-7.71108426465713));
#133126=CARTESIAN_POINT('Ctrl Pts',(20.9495448845472,2.17668522573863,-7.71423041094079));
#133127=CARTESIAN_POINT('Ctrl Pts',(21.0415676646499,2.24817327739315,-7.71976850765597));
#133128=CARTESIAN_POINT('Ctrl Pts',(21.081112541018,2.27601721332088,-7.72210935365691));
#133129=CARTESIAN_POINT('Ctrl Pts',(21.1467554493328,2.31776900427268,-7.72598116723772));
#133130=CARTESIAN_POINT('Ctrl Pts',(21.1720603481634,2.33286410094567,-7.72747033571417));
#133131=CARTESIAN_POINT('Ctrl Pts',(21.2240474592773,2.36189095116137,-7.73053078079335));
#133132=CARTESIAN_POINT('Ctrl Pts',(21.2507360896607,2.37578482245284,-7.73210246767179));
#133133=CARTESIAN_POINT('Ctrl Pts',(21.3258391274469,2.41213279801038,-7.73653177117818));
#133134=CARTESIAN_POINT('Ctrl Pts',(21.3750349785873,2.43286784019779,-7.73944173894915));
#133135=CARTESIAN_POINT('Ctrl Pts',(21.5164731889253,2.48402276129025,-7.74780912558417));
#133136=CARTESIAN_POINT('Ctrl Pts',(21.6106532633793,2.50834714407414,-7.75339476799625));
#133137=CARTESIAN_POINT('Ctrl Pts',(21.738434647399,2.52876942832236,-7.76068203807632));
#133138=CARTESIAN_POINT('Ctrl Pts',(21.7705384172451,2.53286971983794,-7.76248719636736));
#133139=CARTESIAN_POINT('Ctrl Pts',(21.8275932519181,2.53833953472043,-7.76562606886156));
#133140=CARTESIAN_POINT('Ctrl Pts',(21.852493391881,2.54011834796466,-7.76697271342015));
#133141=CARTESIAN_POINT('Ctrl Pts',(21.8938578065908,2.54206602592885,-7.76915985300163));
#133142=CARTESIAN_POINT('Ctrl Pts',(21.9102997637596,2.54257690982044,-7.77001565020145));
#133143=CARTESIAN_POINT('Ctrl Pts',(21.9485699524295,2.54315366347932,-7.77197567170477));
#133144=CARTESIAN_POINT('Ctrl Pts',(21.9703967204295,2.54301955099044,-7.7730705618745));
#133145=CARTESIAN_POINT('Ctrl Pts',(22.0924079379571,2.53968024761724,-7.77909704930489));
#133146=CARTESIAN_POINT('Ctrl Pts',(22.192104685531,2.52718175694384,-7.78367956488091));
#133147=CARTESIAN_POINT('Ctrl Pts',(22.3415418178797,2.49343491596646,-7.79082096802479));
#133148=CARTESIAN_POINT('Ctrl Pts',(22.3925562044891,2.47912017361101,-7.79330709691478));
#133149=CARTESIAN_POINT('Ctrl Pts',(22.4822656362566,2.44889014326399,-7.79786208085157));
#133150=CARTESIAN_POINT('Ctrl Pts',(22.5212404332267,2.43397119329344,-7.79990532598986));
#133151=CARTESIAN_POINT('Ctrl Pts',(22.5860208528212,2.40611380343839,-7.80344086774118));
#133152=CARTESIAN_POINT('Ctrl Pts',(22.6121555307083,2.39399729967823,-7.80490705909161));
#133153=CARTESIAN_POINT('Ctrl Pts',(22.6667068889749,2.36682603588452,-7.80805986555164));
#133154=CARTESIAN_POINT('Ctrl Pts',(22.6950226131164,2.35160026961135,-7.8097515732248));
#133155=CARTESIAN_POINT('Ctrl Pts',(22.7807550611733,2.3019878029393,-7.81505186375773));
#133156=CARTESIAN_POINT('Ctrl Pts',(22.836421930236,2.26474532986395,-7.81875218487559));
#133157=CARTESIAN_POINT('Ctrl Pts',(22.889491610182,2.22401163184779,-7.82252261963806));
#133158=CARTESIAN_POINT('',(20.4070004000582,1.00121065507753,-7.60402771031333));
#133159=CARTESIAN_POINT('Ctrl Pts',(22.8894915957587,2.22401164291842,-7.78024830238043));
#133160=CARTESIAN_POINT('Ctrl Pts',(22.880257682641,2.23109914409893,-7.77960549397171));
#133161=CARTESIAN_POINT('Ctrl Pts',(22.8709420309963,2.23808333424448,-7.77896653901388));
#133162=CARTESIAN_POINT('Ctrl Pts',(22.8435437238085,2.25814403624021,-7.77711690966168));
#133163=CARTESIAN_POINT('Ctrl Pts',(22.8252564149561,2.27093395165168,-7.77591928997979));
#133164=CARTESIAN_POINT('Ctrl Pts',(22.793323012972,2.29225146272404,-7.77389927352338));
#133165=CARTESIAN_POINT('Ctrl Pts',(22.7798107599659,2.30096951712248,-7.7730663387722));
#133166=CARTESIAN_POINT('Ctrl Pts',(22.7463339099439,2.32183478920938,-7.7710542050887));
#133167=CARTESIAN_POINT('Ctrl Pts',(22.7262256245581,2.33374240125316,-7.76988840332241));
#133168=CARTESIAN_POINT('Ctrl Pts',(22.6801787966661,2.35961583585793,-7.76729710652219));
#133169=CARTESIAN_POINT('Ctrl Pts',(22.6540950310548,2.37330500137809,-7.76588352073751));
#133170=CARTESIAN_POINT('Ctrl Pts',(22.5586012495163,2.41998515159651,-7.760848482913));
#133171=CARTESIAN_POINT('Ctrl Pts',(22.4871420125279,2.44852769964705,-7.7573364284221));
#133172=CARTESIAN_POINT('Ctrl Pts',(22.3462507685608,2.4929361219175,-7.75046208951894));
#133173=CARTESIAN_POINT('Ctrl Pts',(22.2772657339821,2.50955920336922,-7.74711737841442));
#133174=CARTESIAN_POINT('Ctrl Pts',(22.1755363456467,2.52676973305955,-7.74204962671551));
#133175=CARTESIAN_POINT('Ctrl Pts',(22.1435263310517,2.53115637404756,-7.74043681604782));
#133176=CARTESIAN_POINT('Ctrl Pts',(22.0832329886062,2.53749807259431,-7.73735346166105));
#133177=CARTESIAN_POINT('Ctrl Pts',(22.0549874927621,2.5396846585077,-7.73589047344871));
#133178=CARTESIAN_POINT('Ctrl Pts',(21.9870832276432,2.54306419921142,-7.73232370777881));
#133179=CARTESIAN_POINT('Ctrl Pts',(21.9474087683684,2.54350744100091,-7.73019897156096));
#133180=CARTESIAN_POINT('Ctrl Pts',(21.8590267161619,2.54108724920566,-7.72537508504436));
#133181=CARTESIAN_POINT('Ctrl Pts',(21.8103835658148,2.53744359000075,-7.72265822272179));
#133182=CARTESIAN_POINT('Ctrl Pts',(21.6762829786785,2.52098179466736,-7.71503687152916));
#133183=CARTESIAN_POINT('Ctrl Pts',(21.5916049749986,2.50328291115702,-7.71006754088825));
#133184=CARTESIAN_POINT('Ctrl Pts',(21.4740633261771,2.46821365983889,-7.70321950518927));
#133185=CARTESIAN_POINT('Ctrl Pts',(21.4396487033743,2.45660871563313,-7.70122249865693));
#133186=CARTESIAN_POINT('Ctrl Pts',(21.3890485483809,2.43753197216848,-7.69832881259261));
#133187=CARTESIAN_POINT('Ctrl Pts',(21.3725322363799,2.43097719747414,-7.69739125950921));
#133188=CARTESIAN_POINT('Ctrl Pts',(21.3397321112258,2.41729949552865,-7.69554858472773));
#133189=CARTESIAN_POINT('Ctrl Pts',(21.3234507545024,2.41017759603771,-7.69464362410134));
#133190=CARTESIAN_POINT('Ctrl Pts',(21.2741719712013,2.38759971781135,-7.69192417094538));
#133191=CARTESIAN_POINT('Ctrl Pts',(21.241594383403,2.37125428239819,-7.6901534763187));
#133192=CARTESIAN_POINT('Ctrl Pts',(21.1572101034558,2.32510458212038,-7.68556538245284));
#133193=CARTESIAN_POINT('Ctrl Pts',(21.1065029389211,2.29341842461624,-7.68280539233803));
#133194=CARTESIAN_POINT('Ctrl Pts',(20.9870503155218,2.20875486251205,-7.67602597713628));
#133195=CARTESIAN_POINT('Ctrl Pts',(20.9206922636456,2.15277262916053,-7.6720045182926));
#133196=CARTESIAN_POINT('Ctrl Pts',(20.8346040841136,2.06675605876907,-7.66607649630674));
#133197=CARTESIAN_POINT('Ctrl Pts',(20.8106717726939,2.04115681254455,-7.66434053421702));
#133198=CARTESIAN_POINT('Ctrl Pts',(20.7692000002589,1.99365282861371,-7.66115272455574));
#133199=CARTESIAN_POINT('Ctrl Pts',(20.7513470825887,1.97204199505773,-7.65971416377032));
#133200=CARTESIAN_POINT('Ctrl Pts',(20.7122980387137,1.92206083279264,-7.65640720418107));
#133201=CARTESIAN_POINT('Ctrl Pts',(20.6914706019602,1.8934236519855,-7.65452618947099));
#133202=CARTESIAN_POINT('Ctrl Pts',(20.648816414946,1.83032067502098,-7.65040791663656));
#133203=CARTESIAN_POINT('Ctrl Pts',(20.6273343520704,1.79565469516914,-7.64816138106526));
#133204=CARTESIAN_POINT('Ctrl Pts',(20.559384708497,1.67563148217609,-7.64045517225515));
#133205=CARTESIAN_POINT('Ctrl Pts',(20.5196136451572,1.58675573281389,-7.6348516282934));
#133206=CARTESIAN_POINT('Ctrl Pts',(20.4755583497264,1.45660814296849,-7.62713291457989));
#133207=CARTESIAN_POINT('Ctrl Pts',(20.4641486580224,1.41798967558686,-7.62490234084615));
#133208=CARTESIAN_POINT('Ctrl Pts',(20.4495810968905,1.36049322952509,-7.62170857570756));
#133209=CARTESIAN_POINT('Ctrl Pts',(20.44524292523,1.3419334220221,-7.62069684308843));
#133210=CARTESIAN_POINT('Ctrl Pts',(20.43773241531,1.30688367478168,-7.61882817541303));
#133211=CARTESIAN_POINT('Ctrl Pts',(20.4344833899312,1.29041393168936,-7.61796791226469));
#133212=CARTESIAN_POINT('Ctrl Pts',(20.4262000145396,1.24449007017566,-7.61561161196411));
#133213=CARTESIAN_POINT('Ctrl Pts',(20.421751238443,1.21493652510305,-7.61414308772383));
#133214=CARTESIAN_POINT('Ctrl Pts',(20.4107765321421,1.12419665233873,-7.60973178671522));
#133215=CARTESIAN_POINT('Ctrl Pts',(20.4070487067959,1.0627332925579,-7.60687691375844));
#133216=CARTESIAN_POINT('Ctrl Pts',(20.4070004535616,1.00121019123005,-7.60402759549201));
#133217=CARTESIAN_POINT('Ctrl Pts',(20.4070004539288,1.00121065934862,-7.60402761717198));
#133218=CARTESIAN_POINT('Ctrl Pts',(20.4069404364847,0.924717723665204,
-7.60048500117601));
#133219=CARTESIAN_POINT('Ctrl Pts',(20.4125686362602,0.848325809332539,
-7.59695636083124));
#133220=CARTESIAN_POINT('Ctrl Pts',(20.4302233931201,0.72980335152939,-7.5912204783422));
#133221=CARTESIAN_POINT('Ctrl Pts',(20.4384109065201,0.687229799530118,
-7.58910750751098));
#133222=CARTESIAN_POINT('Ctrl Pts',(20.4549766894986,0.617146204419026,
-7.58550847460207));
#133223=CARTESIAN_POINT('Ctrl Pts',(20.4623512340671,0.589423888569778,
-7.58405290486925));
#133224=CARTESIAN_POINT('Ctrl Pts',(20.4792543043622,0.532337421372184,
-7.58098187890168));
#133225=CARTESIAN_POINT('Ctrl Pts',(20.4888999288707,0.503021531856045,
-7.57936334978893));
#133226=CARTESIAN_POINT('Ctrl Pts',(20.5203199021808,0.416370147408416,
-7.57444937714896));
#133227=CARTESIAN_POINT('Ctrl Pts',(20.5446380078088,0.360026980332973,
-7.57107803141705));
#133228=CARTESIAN_POINT('Ctrl Pts',(20.6118260550235,0.226779847925846,
-7.56270836534051));
#133229=CARTESIAN_POINT('Ctrl Pts',(20.6580460495585,0.151805988023286,
-7.55764830584345));
#133230=CARTESIAN_POINT('Ctrl Pts',(20.7289220841007,0.0561856460658383,
-7.55094967865945));
#133231=CARTESIAN_POINT('Ctrl Pts',(20.7481991027466,0.0317585128412778,
-7.54921574637432));
#133232=CARTESIAN_POINT('Ctrl Pts',(20.7837969757221,-0.0106472506195487,
-7.54618603170542));
#133233=CARTESIAN_POINT('Ctrl Pts',(20.7998284621887,-0.0288551467130027,
-7.5448783394791));
#133234=CARTESIAN_POINT('Ctrl Pts',(20.8272428352801,-0.0585492067619242,
-7.54274480337316));
#133235=CARTESIAN_POINT('Ctrl Pts',(20.8383879952986,-0.0702471134814875,
-7.54190452179177));
#133236=CARTESIAN_POINT('Ctrl Pts',(20.8646837503652,-0.0969929233667788,
-7.53998452909802));
#133237=CARTESIAN_POINT('Ctrl Pts',(20.8799663594014,-0.111905089105901,
-7.53891383043223));
#133238=CARTESIAN_POINT('Ctrl Pts',(20.9613090366144,-0.18804512502939,
-7.53341560865051));
#133239=CARTESIAN_POINT('Ctrl Pts',(21.0323325260271,-0.243724353494565,
-7.529278107026));
#133240=CARTESIAN_POINT('Ctrl Pts',(21.1585262692755,-0.325926637475304,
-7.52230364504257));
#133241=CARTESIAN_POINT('Ctrl Pts',(21.2111375683254,-0.355947642740331,
-7.51949311520841));
#133242=CARTESIAN_POINT('Ctrl Pts',(21.3058427372353,-0.402836267948401,
-7.51444913056078));
#133243=CARTESIAN_POINT('Ctrl Pts',(21.3471688605105,-0.42108492783576,
-7.512253396365));
#133244=CARTESIAN_POINT('Ctrl Pts',(21.4161840954563,-0.448007752659545,
-7.50855748603983));
#133245=CARTESIAN_POINT('Ctrl Pts',(21.4434235211971,-0.457760613261931,
-7.50709185163064));
#133246=CARTESIAN_POINT('Ctrl Pts',(21.4998620271572,-0.476195052972779,
-7.50403386720214));
#133247=CARTESIAN_POINT('Ctrl Pts',(21.5290761485654,-0.48478920164567,
-7.50243957182671));
#133248=CARTESIAN_POINT('Ctrl Pts',(21.6140286215346,-0.507071644878461,
-7.49776590108286));
#133249=CARTESIAN_POINT('Ctrl Pts',(21.6702971976674,-0.51852133889621,
-7.49462252480263));
#133250=CARTESIAN_POINT('Ctrl Pts',(21.8184258495567,-0.540149775638676,
-7.48625613057676));
#133251=CARTESIAN_POINT('Ctrl Pts',(21.9107950335803,-0.545262059290152,
-7.48094034631308));
#133252=CARTESIAN_POINT('Ctrl Pts',(22.0347432075985,-0.540997279014519,
-7.47395608308751));
#133253=CARTESIAN_POINT('Ctrl Pts',(22.0663869261323,-0.53893088758926,
-7.47218768193824));
#133254=CARTESIAN_POINT('Ctrl Pts',(22.1224052819572,-0.533534881598952,
-7.46910604169119));
#133255=CARTESIAN_POINT('Ctrl Pts',(22.1468063855873,-0.530594716047843,
-7.46778035822661));
#133256=CARTESIAN_POINT('Ctrl Pts',(22.1871447371499,-0.524753513699698,
-7.46562754772565));
#133257=CARTESIAN_POINT('Ctrl Pts',(22.2031239743921,-0.522182387121726,
-7.46478535310051));
#133258=CARTESIAN_POINT('Ctrl Pts',(22.2398899888756,-0.515671535944335,
-7.46287308136835));
#133259=CARTESIAN_POINT('Ctrl Pts',(22.2606412090513,-0.51155500434557,
-7.46181157540772));
#133260=CARTESIAN_POINT('Ctrl Pts',(22.402259150928,-0.480421673714395,
-7.45465113225172));
#133261=CARTESIAN_POINT('Ctrl Pts',(22.5195860978097,-0.439362599838922,
-7.44910884886831));
#133262=CARTESIAN_POINT('Ctrl Pts',(22.6866857263994,-0.357213365843605,
-7.44039011852325));
#133263=CARTESIAN_POINT('Ctrl Pts',(22.7409003166773,-0.326352063248985,
-7.43742069907414));
#133264=CARTESIAN_POINT('Ctrl Pts',(22.8190349341517,-0.275376948805524,
-7.43281614404673));
#133265=CARTESIAN_POINT('Ctrl Pts',(22.8444561289702,-0.257678873593203,
-7.43126296786823));
#133266=CARTESIAN_POINT('Ctrl Pts',(22.8920837958749,-0.222346100866249,
-7.42823567730313));
#133267=CARTESIAN_POINT('Ctrl Pts',(22.9143705766032,-0.204840705467908,
-7.42676667744416));
#133268=CARTESIAN_POINT('Ctrl Pts',(22.9690042151343,-0.159440733914313,
-7.4230264266045));
#133269=CARTESIAN_POINT('Ctrl Pts',(23.0006972133969,-0.130799421437278,
-7.42072732038427));
#133270=CARTESIAN_POINT('Ctrl Pts',(23.106417467474,-0.0269731518823635,
-7.41259669149464));
#133271=CARTESIAN_POINT('Ctrl Pts',(23.1738932938146,0.0544542401824089,
-7.40654052091814));
#133272=CARTESIAN_POINT('Ctrl Pts',(23.2535312802292,0.173512248879439,
-7.39842681675134));
#133273=CARTESIAN_POINT('Ctrl Pts',(23.2733737991496,0.20567146503963,-7.39630328286484));
#133274=CARTESIAN_POINT('Ctrl Pts',(23.3056473382805,0.262550262435295,
-7.39269874334556));
#133275=CARTESIAN_POINT('Ctrl Pts',(23.3186312646397,0.286935872596983,
-7.39119919578614));
#133276=CARTESIAN_POINT('Ctrl Pts',(23.3383081643222,0.326411748991351,
-7.38885869998939));
#133277=CARTESIAN_POINT('Ctrl Pts',(23.3454256109164,0.341282960369145,
-7.38799636940707));
#133278=CARTESIAN_POINT('Ctrl Pts',(23.3605946106287,0.374327014451219,
-7.38612570290247));
#133279=CARTESIAN_POINT('Ctrl Pts',(23.368535872225,0.392546388425967,-7.38512302140777));
#133280=CARTESIAN_POINT('Ctrl Pts',(23.3959012989305,0.45879568257635,-7.38156294166614));
#133281=CARTESIAN_POINT('Ctrl Pts',(23.4132568690596,0.507645691789587,
-7.37909772323242));
#133282=CARTESIAN_POINT('Ctrl Pts',(23.4586594830442,0.659232550490287,
-7.37168572094013));
#133283=CARTESIAN_POINT('Ctrl Pts',(23.4785655803018,0.764069051469471,
-7.36686324167786));
#133284=CARTESIAN_POINT('Ctrl Pts',(23.4911695183809,0.913275743994522,
-7.35969503151058));
#133285=CARTESIAN_POINT('Ctrl Pts',(23.4929962386157,0.9565625538337,-7.35758324507889));
#133286=CARTESIAN_POINT('Ctrl Pts',(23.4930024230829,1.02827377338184,-7.35399914715059));
#133287=CARTESIAN_POINT('Ctrl Pts',(23.4922204160075,1.05667400551033,-7.3525576714625));
#133288=CARTESIAN_POINT('Ctrl Pts',(23.488957872469,1.11578414100086,-7.34950475898091));
#133289=CARTESIAN_POINT('Ctrl Pts',(23.4863406531038,1.14647363838399,-7.34788989712755));
#133290=CARTESIAN_POINT('Ctrl Pts',(23.4758491210652,1.23729722655133,-7.34301712938948));
#133291=CARTESIAN_POINT('Ctrl Pts',(23.4653473529279,1.29706356196314,-7.33968549298856));
#133292=CARTESIAN_POINT('Ctrl Pts',(23.4248616387608,1.46777859122865,-7.32985116481224));
#133293=CARTESIAN_POINT('Ctrl Pts',(23.3859786537944,1.57619262085885,-7.32318266929766));
#133294=CARTESIAN_POINT('Ctrl Pts',(23.3235480041885,1.7035220866657,-7.31537606907888));
#133295=CARTESIAN_POINT('Ctrl Pts',(23.3110311094961,1.72744204167632,-7.31391246444009));
#133296=CARTESIAN_POINT('Ctrl Pts',(23.2899057577224,1.7653566217664,-7.31161137532962));
#133297=CARTESIAN_POINT('Ctrl Pts',(23.2816905682516,1.77956302467632,-7.31075382499874));
#133298=CARTESIAN_POINT('Ctrl Pts',(23.262884807307,1.81091830023135,-7.30887427813815));
#133299=CARTESIAN_POINT('Ctrl Pts',(23.2521822061575,1.82799552098128,-7.30785857812452));
#133300=CARTESIAN_POINT('Ctrl Pts',(23.2077044960095,1.89596816201364,-7.30382859710218));
#133301=CARTESIAN_POINT('Ctrl Pts',(23.1712534058312,1.94505068856687,-7.30094689308019));
#133302=CARTESIAN_POINT('Ctrl Pts',(23.059824766865,2.07784054179424,-7.29287211099152));
#133303=CARTESIAN_POINT('Ctrl Pts',(22.9785112118013,2.15568452861694,-7.28776613946278));
#133304=CARTESIAN_POINT('Ctrl Pts',(22.8894915988056,2.22401164057974,-7.28231538991333));
#133305=CARTESIAN_POINT('Origin',(21.9499999789786,0.999999999999992,-4.89578827641128));
#133306=CARTESIAN_POINT('',(22.8894916066884,2.22401163452936,-6.78051560659813));
#133307=CARTESIAN_POINT('',(22.8894530727892,2.22394970963619,-6.82271760993144));
#133308=CARTESIAN_POINT('',(22.8894916101512,2.22401163187148,-4.89578827641128));
#133309=CARTESIAN_POINT('',(20.406507169633,1.00049669003439,-7.14664979013704));
#133310=CARTESIAN_POINT('Ctrl Pts',(22.8894530727892,2.22394970963619,-6.82271760993144));
#133311=CARTESIAN_POINT('Ctrl Pts',(22.9353005742457,2.18892258955494,-6.82591636290728));
#133312=CARTESIAN_POINT('Ctrl Pts',(22.9791500519513,2.15135845546692,-6.829135128161));
#133313=CARTESIAN_POINT('Ctrl Pts',(23.0207002168903,2.11149723851871,-6.83231403385656));
#133314=CARTESIAN_POINT('Ctrl Pts',(23.059743469323,2.07404103207845,-6.83530114155428));
#133315=CARTESIAN_POINT('Ctrl Pts',(23.0967567332383,2.03455601206123,-6.83825257867589));
#133316=CARTESIAN_POINT('Ctrl Pts',(23.1315058091072,1.99327445448767,-6.8411059364984));
#133317=CARTESIAN_POINT('Ctrl Pts',(23.1337965278077,1.99055310338541,-6.84129403474158));
#133318=CARTESIAN_POINT('Ctrl Pts',(23.1360774251152,1.98782393969824,-6.84148170676424));
#133319=CARTESIAN_POINT('Ctrl Pts',(23.1383484415223,1.98508702747687,-6.84166893468789));
#133320=CARTESIAN_POINT('Ctrl Pts',(23.1454578829252,1.97651909419329,-6.84225505372602));
#133321=CARTESIAN_POINT('Ctrl Pts',(23.1524703651171,1.9678754174032,-6.84283679013381));
#133322=CARTESIAN_POINT('Ctrl Pts',(23.1593839597114,1.95915822782426,-6.84341356061474));
#133323=CARTESIAN_POINT('Ctrl Pts',(23.1593944945009,1.95914494475483,-6.84341443948542));
#133324=CARTESIAN_POINT('Ctrl Pts',(23.1594050290725,1.95913166150046,-6.84341531834532));
#133325=CARTESIAN_POINT('Ctrl Pts',(23.1594155634263,1.95911837806115,-6.84341619719443));
#133326=CARTESIAN_POINT('Ctrl Pts',(23.1918413993482,1.91823057129339,-6.84612138611208));
#133327=CARTESIAN_POINT('Ctrl Pts',(23.2222034754519,1.8755861315841,-6.84872442054874));
#133328=CARTESIAN_POINT('Ctrl Pts',(23.2503299501565,1.83143439238815,-6.85127679550709));
#133329=CARTESIAN_POINT('Ctrl Pts',(23.2531698104295,1.826976500973,-6.85153450246546));
#133330=CARTESIAN_POINT('Ctrl Pts',(23.2559868805442,1.82250328730227,-6.85179169297886));
#133331=CARTESIAN_POINT('Ctrl Pts',(23.2587809847565,1.81801503743372,-6.85204842005146));
#133332=CARTESIAN_POINT('Ctrl Pts',(23.2892065310885,1.76914160826103,-6.85484397127236));
#133333=CARTESIAN_POINT('Ctrl Pts',(23.3169092064515,1.71847955854335,-6.85758527374401));
#133334=CARTESIAN_POINT('Ctrl Pts',(23.3417102552614,1.66638007405639,-6.86033245303685));
#133335=CARTESIAN_POINT('Ctrl Pts',(23.3664883206591,1.61432887075016,-6.8630770864876));
#133336=CARTESIAN_POINT('Ctrl Pts',(23.3883705234435,1.56084319642377,-6.8658280233161));
#133337=CARTESIAN_POINT('Ctrl Pts',(23.4072216783572,1.5062830451516,-6.86862842195339));
#133338=CARTESIAN_POINT('Ctrl Pts',(23.4260624850877,1.45175284421613,-6.87142728333537));
#133339=CARTESIAN_POINT('Ctrl Pts',(23.4418758252863,1.39614949199035,-6.87427578780015));
#133340=CARTESIAN_POINT('Ctrl Pts',(23.4545649487095,1.33983891959706,-6.87719525329033));
#133341=CARTESIAN_POINT('Ctrl Pts',(23.4672518996907,1.28353798785837,-6.88011421895326));
#133342=CARTESIAN_POINT('Ctrl Pts',(23.4768158231066,1.22653014248622,-6.88310421089122));
#133343=CARTESIAN_POINT('Ctrl Pts',(23.48319543489,1.16918611634482,-6.88616236731445));
#133344=CARTESIAN_POINT('Ctrl Pts',(23.4895806266956,1.11179193340039,-6.88922319859956));
#133345=CARTESIAN_POINT('Ctrl Pts',(23.4927759120905,1.0540609865502,-6.8923522795552));
#133346=CARTESIAN_POINT('Ctrl Pts',(23.4927545859088,0.996369469660129,
-6.8955221021616));
#133347=CARTESIAN_POINT('Ctrl Pts',(23.4927332500643,0.938651813220718,
-6.89869336098843));
#133348=CARTESIAN_POINT('Ctrl Pts',(23.4894921934945,0.880973587000663,
-6.90190520900859));
#133349=CARTESIAN_POINT('Ctrl Pts',(23.4830409884787,0.823716243544801,
-6.90510708351915));
#133350=CARTESIAN_POINT('Ctrl Pts',(23.4765785699948,0.76635937552023,-6.90831452351985));
#133351=CARTESIAN_POINT('Ctrl Pts',(23.4668943892679,0.709424848678099,
-6.91151154679704));
#133352=CARTESIAN_POINT('Ctrl Pts',(23.4540392373995,0.653301300146426,
-6.91462863265755));
#133353=CARTESIAN_POINT('Ctrl Pts',(23.4456805697153,0.616808686427064,
-6.9166554220038));
#133354=CARTESIAN_POINT('Ctrl Pts',(23.4359820907259,0.580659069910008,
-6.91864801976249));
#133355=CARTESIAN_POINT('Ctrl Pts',(23.4249687810269,0.544960262964138,
-6.92058471113213));
#133356=CARTESIAN_POINT('Ctrl Pts',(23.4249637831682,0.544944062784526,
-6.92058559000599));
#133357=CARTESIAN_POINT('Ctrl Pts',(23.4249587850337,0.544927862679981,
-6.92058646886906));
#133358=CARTESIAN_POINT('Ctrl Pts',(23.4249537866235,0.544911662650505,
-6.92058734772135));
#133359=CARTESIAN_POINT('Ctrl Pts',(23.409568224219,0.495046494521923,-6.92329253521352));
#133360=CARTESIAN_POINT('Ctrl Pts',(23.3915668267523,0.445890046649582,
-6.92589556871675));
#133361=CARTESIAN_POINT('Ctrl Pts',(23.3710580569309,0.397725042837229,
-6.92844794313227));
#133362=CARTESIAN_POINT('Ctrl Pts',(23.3689873456662,0.392861961490763,
-6.92870564900639));
#133363=CARTESIAN_POINT('Ctrl Pts',(23.3668911097967,0.388009011609156,
-6.92896283844364));
#133364=CARTESIAN_POINT('Ctrl Pts',(23.364769485865,0.383166499898504,-6.92921956444747));
#133365=CARTESIAN_POINT('Ctrl Pts',(23.3416666234825,0.33043525004452,-6.93201511433164));
#133366=CARTESIAN_POINT('Ctrl Pts',(23.3155488213821,0.278938233791786,
-6.93475641593523));
#133367=CARTESIAN_POINT('Ctrl Pts',(23.2866046352174,0.229021473990792,
-6.9375035946566));
#133368=CARTESIAN_POINT('Ctrl Pts',(23.2576872709693,0.179150970911703,
-6.94024822763016));
#133369=CARTESIAN_POINT('Ctrl Pts',(23.225949226306,0.130857646564572,-6.94299916427836));
#133370=CARTESIAN_POINT('Ctrl Pts',(23.1916109603711,0.0844565701330748,
-6.94579956288904));
#133371=CARTESIAN_POINT('Ctrl Pts',(23.1572915429672,0.0380809635996349,
-6.94859842433997));
#133372=CARTESIAN_POINT('Ctrl Pts',(23.1203750226841,-0.00640459895006078,
-6.95144692903123));
#133373=CARTESIAN_POINT('Ctrl Pts',(23.0811084900701,-0.0487133903317922,
-6.95436639478018));
#133374=CARTESIAN_POINT('Ctrl Pts',(23.0418486787455,-0.0910149396779262,
-6.95728536080143));
#133375=CARTESIAN_POINT('Ctrl Pts',(23.0002397802386,-0.131140525167259,
-6.96027535313538));
#133376=CARTESIAN_POINT('Ctrl Pts',(22.9565529012732,-0.168829955070649,
-6.9633335098726));
#133377=CARTESIAN_POINT('Ctrl Pts',(22.9128278086591,-0.206552352553033,
-6.96639434163101));
#133378=CARTESIAN_POINT('Ctrl Pts',(22.8670210906049,-0.241834309659026,
-6.96952342298557));
#133379=CARTESIAN_POINT('Ctrl Pts',(22.8194279119882,-0.274441065500062,
-6.97269324578701));
#133380=CARTESIAN_POINT('Ctrl Pts',(22.7718131679043,-0.307062596145898,
-6.97586450490162));
#133381=CARTESIAN_POINT('Ctrl Pts',(22.7224102051567,-0.337006360951613,
-6.9790763530086));
#133382=CARTESIAN_POINT('Ctrl Pts',(22.6715390404077,-0.364064545154381,
-6.9822782272528));
#133383=CARTESIAN_POINT('Ctrl Pts',(22.6205794492212,-0.391169763051821,
-6.98548566713195));
#133384=CARTESIAN_POINT('Ctrl Pts',(22.5681462911772,-0.41537899686547,
-6.98868268993298));
#133385=CARTESIAN_POINT('Ctrl Pts',(22.5145888174665,-0.436514364241684,
-6.99179977477122));
#133386=CARTESIAN_POINT('Ctrl Pts',(22.479764718626,-0.45025698635479,-6.99382656324685));
#133387=CARTESIAN_POINT('Ctrl Pts',(22.44446584951,-0.462700634545866,-6.99581915991031));
#133388=CARTESIAN_POINT('Ctrl Pts',(22.4087952549026,-0.473804944237803,
-6.99775584990608));
#133389=CARTESIAN_POINT('Ctrl Pts',(22.408779067629,-0.473809983360409,
-6.99775672877371));
#133390=CARTESIAN_POINT('Ctrl Pts',(22.4087628802613,-0.473815022213182,
-6.99775760763055));
#133391=CARTESIAN_POINT('Ctrl Pts',(22.4087466927996,-0.47382006079611,
-6.99775848647662));
#133392=CARTESIAN_POINT('Ctrl Pts',(22.3589199269531,-0.48932936652176,
-7.0004636701555));
#133393=CARTESIAN_POINT('Ctrl Pts',(22.3081984348818,-0.502280486332587,
-7.00306669948927));
#133394=CARTESIAN_POINT('Ctrl Pts',(22.2568767273539,-0.512602995713214,
-7.00561906908348));
#133395=CARTESIAN_POINT('Ctrl Pts',(22.2516948146702,-0.513645251414825,
-7.00587677984586));
#133396=CARTESIAN_POINT('Ctrl Pts',(22.2465068235975,-0.514660725305008,
-7.0061339741432));
#133397=CARTESIAN_POINT('Ctrl Pts',(22.2413130843257,-0.515649356552682,
-7.00639070498193));
#133398=CARTESIAN_POINT('Ctrl Pts',(22.1847583086682,-0.526414590518925,
-7.00918625443655));
#133399=CARTESIAN_POINT('Ctrl Pts',(22.127516529053,-0.533995289840677,
-7.01192755471752));
#133400=CARTESIAN_POINT('Ctrl Pts',(22.0699797563789,-0.538351291058253,
-7.01467473145523));
#133401=CARTESIAN_POINT('Ctrl Pts',(22.0124963031947,-0.542703255557179,
-7.01741936237649));
#133402=CARTESIAN_POINT('Ctrl Pts',(21.9547185440105,-0.543836966660925,
-7.02017029631679));
#133403=CARTESIAN_POINT('Ctrl Pts',(21.8970310019311,-0.541756077642057,
-7.02297069195622));
#133404=CARTESIAN_POINT('Ctrl Pts',(21.8393751265965,-0.539676330897219,
-7.02576955035883));
#133405=CARTESIAN_POINT('Ctrl Pts',(21.7818094141064,-0.534385802431919,
-7.02861805173894));
#133406=CARTESIAN_POINT('Ctrl Pts',(21.7247100723998,-0.525926137154944,
-7.0315375144116));
#133407=CARTESIAN_POINT('Ctrl Pts',(21.6676205061858,-0.517467920185284,
-7.03445647726788));
#133408=CARTESIAN_POINT('Ctrl Pts',(21.6109971680635,-0.505841786149631,
-7.03744646666923));
#133409=CARTESIAN_POINT('Ctrl Pts',(21.5552079618626,-0.491124193051166,
-7.04050462127644));
#133410=CARTESIAN_POINT('Ctrl Pts',(21.4993699590489,-0.476393727055949,
-7.04356545073055));
#133411=CARTESIAN_POINT('Ctrl Pts',(21.4443675607246,-0.45856637310289,
-7.04669453057846));
#133412=CARTESIAN_POINT('Ctrl Pts',(21.3905613013614,-0.437752812222422,
-7.04986435329719));
#133413=CARTESIAN_POINT('Ctrl Pts',(21.3367306628793,-0.416929820909862,
-7.05303561223331));
#133414=CARTESIAN_POINT('Ctrl Pts',(21.2840972842237,-0.393117722594224,
-7.05624746158659));
#133415=CARTESIAN_POINT('Ctrl Pts',(21.233013529593,-0.366462932744109,
-7.05944933916246));
#133416=CARTESIAN_POINT('Ctrl Pts',(21.1818409821029,-0.339761812019858,
-7.06265678218408));
#133417=CARTESIAN_POINT('Ctrl Pts',(21.1322236049285,-0.310207692293406,
-7.06585381022509));
#133418=CARTESIAN_POINT('Ctrl Pts',(21.0845056074429,-0.277988026804604,
-7.06897090306744));
#133419=CARTESIAN_POINT('Ctrl Pts',(21.0534789061002,-0.25703849012744,
-7.07099766684156));
#133420=CARTESIAN_POINT('Ctrl Pts',(21.0232550309494,-0.234962852301261,
-7.07299024097854));
#133421=CARTESIAN_POINT('Ctrl Pts',(20.9939255402615,-0.21182327068612,
-7.07492691175894));
#133422=CARTESIAN_POINT('Ctrl Pts',(20.9939122314531,-0.211812770665437,
-7.07492779055976));
#133423=CARTESIAN_POINT('Ctrl Pts',(20.9938989228132,-0.211802270414054,
-7.07492866934983));
#133424=CARTESIAN_POINT('Ctrl Pts',(20.9938856143419,-0.211791769931971,
-7.07492954812917));
#133425=CARTESIAN_POINT('Ctrl Pts',(20.9531641999186,-0.179662273484807,
-7.07761844729391));
#133426=CARTESIAN_POINT('Ctrl Pts',(20.9140198227237,-0.145368622016484,
-7.0802067852082));
#133427=CARTESIAN_POINT('Ctrl Pts',(20.876677017731,-0.109110200271477,
-7.08274496610853));
#133428=CARTESIAN_POINT('Ctrl Pts',(20.8724589226394,-0.105014592809239,
-7.0830316689526));
#133429=CARTESIAN_POINT('Ctrl Pts',(20.8682638249325,-0.100893970305654,
-7.08331773184006));
#133430=CARTESIAN_POINT('Ctrl Pts',(20.8640920555125,-0.0967486611347506,
-7.08360322741416));
#133431=CARTESIAN_POINT('Ctrl Pts',(20.8236204324131,-0.0565337370805138,
-7.08637290812002));
#133432=CARTESIAN_POINT('Ctrl Pts',(20.7853427847753,-0.0139899011780043,
-7.08908987158476));
#133433=CARTESIAN_POINT('Ctrl Pts',(20.7495112547215,0.0305884202616647,
-7.09181249410042));
#133434=CARTESIAN_POINT('Ctrl Pts',(20.7137122859447,0.0751262319305429,
-7.09453264248044));
#133435=CARTESIAN_POINT('Ctrl Pts',(20.6803547176496,0.12169444025125,-7.09725886511378));
#133436=CARTESIAN_POINT('Ctrl Pts',(20.6496504682484,0.169979289696589,
-7.10003321935231));
#133437=CARTESIAN_POINT('Ctrl Pts',(20.6189619168207,0.218239452842812,
-7.10280615516375));
#133438=CARTESIAN_POINT('Ctrl Pts',(20.5909237821157,0.26821427989406,-7.10562740367482));
#133439=CARTESIAN_POINT('Ctrl Pts',(20.5657116524017,0.31957489765083,-7.10851795047218));
#133440=CARTESIAN_POINT('Ctrl Pts',(20.5397449316027,0.3724727224869,-7.11149501042289));
#133441=CARTESIAN_POINT('Ctrl Pts',(20.5167759968454,0.4268404724139,-7.11454579998516));
#133442=CARTESIAN_POINT('Ctrl Pts',(20.4969590545714,0.482304349981721,
-7.117667332509));
#133443=CARTESIAN_POINT('Ctrl Pts',(20.4777036213231,0.536196669867898,
-7.12070041704414));
#133444=CARTESIAN_POINT('Ctrl Pts',(20.4614239473617,0.591123785151236,
-7.1238001322834));
#133445=CARTESIAN_POINT('Ctrl Pts',(20.4482274795238,0.646730635327404,
-7.1269396055833));
#133446=CARTESIAN_POINT('Ctrl Pts',(20.4344537770139,0.704769818331229,
-7.13021640448148));
#133447=CARTESIAN_POINT('Ctrl Pts',(20.4240393927185,0.763549646139969,
-7.13353646981584));
#133448=CARTESIAN_POINT('Ctrl Pts',(20.4170658700461,0.822652418007863,
-7.1368436453435));
#133449=CARTESIAN_POINT('Ctrl Pts',(20.4105353527739,0.878000581433825,
-7.13994072667823));
#133450=CARTESIAN_POINT('Ctrl Pts',(20.4070225510227,0.9336325600701,-7.14302605898205));
#133451=CARTESIAN_POINT('Ctrl Pts',(20.4065569725966,0.989191189421772,
-7.14603652038649));
#133452=CARTESIAN_POINT('Ctrl Pts',(20.4065253895308,0.992960075069953,
-7.1462407386135));
#133453=CARTESIAN_POINT('Ctrl Pts',(20.4065078194293,0.996728640647018,
-7.14644461230347));
#133454=CARTESIAN_POINT('Ctrl Pts',(20.4065042675225,1.00049678240474,-7.14664812175195));
#133455=CARTESIAN_POINT('Ctrl Pts',(20.4070000539504,1.00048100217607,-7.14693314283738));
#133456=CARTESIAN_POINT('Ctrl Pts',(20.4070043911558,1.01439426051975,-7.1476949496416));
#133457=CARTESIAN_POINT('Ctrl Pts',(20.407196912604,1.02830727097016,-7.14845039496485));
#133458=CARTESIAN_POINT('Ctrl Pts',(20.4079245187433,1.05489128412844,-7.14987943904459));
#133459=CARTESIAN_POINT('Ctrl Pts',(20.4084276730568,1.06756199170956,-7.15055429935513));
#133460=CARTESIAN_POINT('Ctrl Pts',(20.4098781160518,1.09542107250405,-7.15202227234891));
#133461=CARTESIAN_POINT('Ctrl Pts',(20.4108939396218,1.11060366610524,-7.15281144404058));
#133462=CARTESIAN_POINT('Ctrl Pts',(20.4139675239172,1.1481860864981,-7.15473853162009));
#133463=CARTESIAN_POINT('Ctrl Pts',(20.4162906839258,1.17056000144823,-7.15586353571352));
#133464=CARTESIAN_POINT('Ctrl Pts',(20.428221908484,1.26526058343634,-7.16055938457115));
#133465=CARTESIAN_POINT('Ctrl Pts',(20.4424645642558,1.33691282787775,-7.16395161044413));
#133466=CARTESIAN_POINT('Ctrl Pts',(20.486812221479,1.49896218641207,-7.171735707453));
#133467=CARTESIAN_POINT('Ctrl Pts',(20.5203145467133,1.58811568222157,-7.17611228865077));
#133468=CARTESIAN_POINT('Ctrl Pts',(20.5775637714579,1.70609576792949,-7.18248265732038));
#133469=CARTESIAN_POINT('Ctrl Pts',(20.5944589210291,1.73801123191433,-7.18426702960988));
#133470=CARTESIAN_POINT('Ctrl Pts',(20.6264530411218,1.79363753481879,-7.18750492596221));
#133471=CARTESIAN_POINT('Ctrl Pts',(20.641109876985,1.81758400588174,-7.18894307646896));
#133472=CARTESIAN_POINT('Ctrl Pts',(20.6752139039797,1.87003404101473,-7.19219913200481));
#133473=CARTESIAN_POINT('Ctrl Pts',(20.6949799735352,1.89831136945066,-7.19402780813477));
#133474=CARTESIAN_POINT('Ctrl Pts',(20.760025369074,1.98502373309913,-7.19987446489188));
#133475=CARTESIAN_POINT('Ctrl Pts',(20.8085610868534,2.04087786893519,-7.20400382444038));
#133476=CARTESIAN_POINT('Ctrl Pts',(20.9260377573493,2.15793083873767,-7.21340732637559));
#133477=CARTESIAN_POINT('Ctrl Pts',(20.996839496075,2.21687649802452,-7.21869957929475));
#133478=CARTESIAN_POINT('Ctrl Pts',(21.093578709451,2.28376409378472,-7.22515581461593));
#133479=CARTESIAN_POINT('Ctrl Pts',(21.1150501889081,2.29783150945306,-7.22654367599907));
#133480=CARTESIAN_POINT('Ctrl Pts',(21.1507059531751,2.31994065801378,-7.22876351807761));
#133481=CARTESIAN_POINT('Ctrl Pts',(21.1646835567014,2.32830435881413,-7.22961279108647));
#133482=CARTESIAN_POINT('Ctrl Pts',(21.1968941645141,2.34689175921865,-7.23152070578121));
#133483=CARTESIAN_POINT('Ctrl Pts',(21.2152069359682,2.3569690649454,-7.23257141180791));
#133484=CARTESIAN_POINT('Ctrl Pts',(21.330729481491,2.4175150867158,-7.23902375517673));
#133485=CARTESIAN_POINT('Ctrl Pts',(21.4328864049288,2.45789000708564,-7.24398205208198));
#133486=CARTESIAN_POINT('Ctrl Pts',(21.5877825352006,2.50075510905614,-7.25145444036878));
#133487=CARTESIAN_POINT('Ctrl Pts',(21.6377455394643,2.51194053415837,-7.25385495133468));
#133488=CARTESIAN_POINT('Ctrl Pts',(21.7284574103357,2.52755984617057,-7.25828065783118));
#133489=CARTESIAN_POINT('Ctrl Pts',(21.7690022432529,2.5328925879683,-7.26028219069691));
#133490=CARTESIAN_POINT('Ctrl Pts',(21.8380335002001,2.5391950696334,-7.26375619811298));
#133491=CARTESIAN_POINT('Ctrl Pts',(21.8664226439939,2.54099729167704,-7.26520356024424));
#133492=CARTESIAN_POINT('Ctrl Pts',(21.9265847735143,2.5431492069447,-7.26831680433476));
#133493=CARTESIAN_POINT('Ctrl Pts',(21.9583510938058,2.54330418833115,-7.26998775709018));
#133494=CARTESIAN_POINT('Ctrl Pts',(22.0531076809942,2.54084090078519,-7.27505765183627));
#133495=CARTESIAN_POINT('Ctrl Pts',(22.1159519210039,2.53534379580097,-7.27853586058876));
#133496=CARTESIAN_POINT('Ctrl Pts',(22.2756294975527,2.5114574332279,-7.28761557897988));
#133497=CARTESIAN_POINT('Ctrl Pts',(22.3713598290015,2.4876133666492,-7.2933017009994));
#133498=CARTESIAN_POINT('Ctrl Pts',(22.4954884057359,2.44374342304794,-7.30062487629376));
#133499=CARTESIAN_POINT('Ctrl Pts',(22.5264478703202,2.43166364364086,-7.30244512223817));
#133500=CARTESIAN_POINT('Ctrl Pts',(22.5728997393109,2.41178757881728,-7.30514245397109));
#133501=CARTESIAN_POINT('Ctrl Pts',(22.5886900177701,2.40471470046022,-7.30605319238636));
#133502=CARTESIAN_POINT('Ctrl Pts',(22.6209306996614,2.3896171445202,-7.30789516424898));
#133503=CARTESIAN_POINT('Ctrl Pts',(22.6373637520081,2.38156250015455,-7.30882474280428));
#133504=CARTESIAN_POINT('Ctrl Pts',(22.6894322662673,2.35488206608178,-7.31175195686221));
#133505=CARTESIAN_POINT('Ctrl Pts',(22.7244862699264,2.33515426687521,-7.31369512460448));
#133506=CARTESIAN_POINT('Ctrl Pts',(22.8038542486379,2.2863083304854,-7.31811685197965));
#133507=CARTESIAN_POINT('Ctrl Pts',(22.847497344002,2.25624438587793,-7.32056596815938));
#133508=CARTESIAN_POINT('Ctrl Pts',(22.889491673488,2.22401158325724,-7.32301705809308));
#133509=CARTESIAN_POINT('',(20.4070004162552,0.998856448297238,-7.10475668005849));
#133510=CARTESIAN_POINT('Ctrl Pts',(22.8894915988056,2.22401164057974,-7.28231538991332));
#133511=CARTESIAN_POINT('Ctrl Pts',(22.8845521534573,2.22780291784992,-7.28201294331082));
#133512=CARTESIAN_POINT('Ctrl Pts',(22.8795889774586,2.23156489550419,-7.2817095323024));
#133513=CARTESIAN_POINT('Ctrl Pts',(22.847518386252,2.25556927291874,-7.27975172234917));
#133514=CARTESIAN_POINT('Ctrl Pts',(22.8197764516961,2.27494398920208,-7.27807039357847));
#133515=CARTESIAN_POINT('Ctrl Pts',(22.7678965287784,2.30869471919725,-7.27493424659343));
#133516=CARTESIAN_POINT('Ctrl Pts',(22.7439596224551,2.32335353945117,-7.27349029773104));
#133517=CARTESIAN_POINT('Ctrl Pts',(22.6877197826458,2.35571922192614,-7.2700991669245));
#133518=CARTESIAN_POINT('Ctrl Pts',(22.6551569074382,2.37293792112831,-7.26813656518618));
#133519=CARTESIAN_POINT('Ctrl Pts',(22.5829802384274,2.40785829621056,-7.26378668078137));
#133520=CARTESIAN_POINT('Ctrl Pts',(22.5431731816798,2.42508741940847,-7.2613875777753));
#133521=CARTESIAN_POINT('Ctrl Pts',(22.3918745258154,2.48313345571084,-7.25229932018913));
#133522=CARTESIAN_POINT('Ctrl Pts',(22.2765227071108,2.51271940634196,-7.24539632296005));
#133523=CARTESIAN_POINT('Ctrl Pts',(22.1346929324414,2.53210167666293,-7.23755978498624));
#133524=CARTESIAN_POINT('Ctrl Pts',(22.1103868020574,2.53483654670601,-7.2362407854107));
#133525=CARTESIAN_POINT('Ctrl Pts',(22.0699147763377,2.53841834537676,-7.23409516525903));
#133526=CARTESIAN_POINT('Ctrl Pts',(22.0537834117036,2.5395907328649,-7.2332537102185));
#133527=CARTESIAN_POINT('Ctrl Pts',(22.0160523422047,2.54173713380429,-7.23131853736766));
#133528=CARTESIAN_POINT('Ctrl Pts',(21.9944455685431,2.54251125812968,-7.23023437542709));
#133529=CARTESIAN_POINT('Ctrl Pts',(21.9465009345402,2.54322067734371,-7.22786853579623));
#133530=CARTESIAN_POINT('Ctrl Pts',(21.9201664354746,2.54293628292467,-7.22659568585361));
#133531=CARTESIAN_POINT('Ctrl Pts',(21.8337807617944,2.53979067647612,-7.22247311583009));
#133532=CARTESIAN_POINT('Ctrl Pts',(21.7738872481558,2.53409487411891,-7.21969710898256));
#133533=CARTESIAN_POINT('Ctrl Pts',(21.6293358048462,2.51176897379883,-7.2129251630867));
#133534=CARTESIAN_POINT('Ctrl Pts',(21.5454489901307,2.49151204561127,-7.20892673403416));
#133535=CARTESIAN_POINT('Ctrl Pts',(21.4304439485781,2.45331970299062,-7.20302424726479));
#133536=CARTESIAN_POINT('Ctrl Pts',(21.3975795635323,2.44114818497966,-7.20128829740587));
#133537=CARTESIAN_POINT('Ctrl Pts',(21.339229658987,2.41724865750151,-7.1981009189788));
#133538=CARTESIAN_POINT('Ctrl Pts',(21.3135952965397,2.40592428453362,-7.19666279535045));
#133539=CARTESIAN_POINT('Ctrl Pts',(21.2563222745226,2.37873566840239,-7.19335746594781));
#133540=CARTESIAN_POINT('Ctrl Pts',(21.2248932823828,2.3624686500678,-7.19147767220279));
#133541=CARTESIAN_POINT('Ctrl Pts',(21.1585368424642,2.32517729039153,-7.18736236635965));
#133542=CARTESIAN_POINT('Ctrl Pts',(21.1238274549572,2.30382029918256,-7.18511759622543));
#133543=CARTESIAN_POINT('Ctrl Pts',(21.0094425457237,2.2270353756561,-7.17742075223178));
#133544=CARTESIAN_POINT('Ctrl Pts',(20.9341652709363,2.16547954528211,-7.17182521054017));
#133545=CARTESIAN_POINT('Ctrl Pts',(20.8365114712754,2.06893233229076,-7.16411099494136));
#133546=CARTESIAN_POINT('Ctrl Pts',(20.8089731332872,2.03948599251083,-7.16187772940895));
#133547=CARTESIAN_POINT('Ctrl Pts',(20.7701502146398,1.99456877543557,-7.15868092404283));
#133548=CARTESIAN_POINT('Ctrl Pts',(20.7579504382081,1.97991350308562,-7.15766873883154));
#133549=CARTESIAN_POINT('Ctrl Pts',(20.7355219492455,1.95193178733353,-7.15579926067446));
#133550=CARTESIAN_POINT('Ctrl Pts',(20.7252336620435,1.93865781349616,-7.15493863562881));
#133551=CARTESIAN_POINT('Ctrl Pts',(20.6972397547846,1.90129594063933,-7.15258127533428));
#133552=CARTESIAN_POINT('Ctrl Pts',(20.6800135590714,1.87685645464419,-7.15111206340992));
#133553=CARTESIAN_POINT('Ctrl Pts',(20.6399169138774,1.81630688266772,-7.14760704139548));
#133554=CARTESIAN_POINT('Ctrl Pts',(20.6178152417466,1.77971706097726,-7.14559999690437));
#133555=CARTESIAN_POINT('Ctrl Pts',(20.5412923362039,1.6402562397643,-7.1381936448793));
#133556=CARTESIAN_POINT('Ctrl Pts',(20.4970433166301,1.53226058919941,-7.13289999536883));
#133557=CARTESIAN_POINT('Ctrl Pts',(20.4560352108718,1.38741181727617,-7.12555046086082));
#133558=CARTESIAN_POINT('Ctrl Pts',(20.4478160809911,1.35420611659052,-7.12385242583675));
#133559=CARTESIAN_POINT('Ctrl Pts',(20.4349336714764,1.29358895426854,-7.12071470938939));
#133560=CARTESIAN_POINT('Ctrl Pts',(20.4298948956972,1.26627204453838,-7.11928706560123));
#133561=CARTESIAN_POINT('Ctrl Pts',(20.4214036547572,1.21207531645098,-7.11642319191832));
#133562=CARTESIAN_POINT('Ctrl Pts',(20.4179166107863,1.18521095877565,-7.11498855704211));
#133563=CARTESIAN_POINT('Ctrl Pts',(20.4096768020266,1.10530330344337,-7.11067492792935));
#133564=CARTESIAN_POINT('Ctrl Pts',(20.4069609369192,1.05209452824687,-7.10774097361327));
#133565=CARTESIAN_POINT('Ctrl Pts',(20.4070004029467,0.998856162050184,
-7.10475668494137));
#133566=CARTESIAN_POINT('Ctrl Pts',(20.4070004027354,0.998856447117781,
-7.1047567009209));
#133567=CARTESIAN_POINT('Ctrl Pts',(20.4070509525418,0.9306494309019,-7.1009333413968));
#133568=CARTESIAN_POINT('Ctrl Pts',(20.4116240317839,0.862522408636186,
-7.09703298057708));
#133569=CARTESIAN_POINT('Ctrl Pts',(20.4262633056739,0.753352816772122,
-7.09077819504367));
#133570=CARTESIAN_POINT('Ctrl Pts',(20.4335309269496,0.712024010642907,
-7.08841037679596));
#133571=CARTESIAN_POINT('Ctrl Pts',(20.4487726883061,0.642175256369573,
-7.08445610803221));
#133572=CARTESIAN_POINT('Ctrl Pts',(20.4558997436795,0.613494358933053,
-7.08284653533944));
#133573=CARTESIAN_POINT('Ctrl Pts',(20.468349154306,0.568908175950438,-7.0803843563375));
#133574=CARTESIAN_POINT('Ctrl Pts',(20.4731143669726,0.552855390044602,
-7.07950627917967));
#133575=CARTESIAN_POINT('Ctrl Pts',(20.4838952644542,0.518592061803567,
-7.07765407945101));
#133576=CARTESIAN_POINT('Ctrl Pts',(20.4899908035707,0.500410258706161,
-7.07668394218358));
#133577=CARTESIAN_POINT('Ctrl Pts',(20.510185875544,0.443702353444211,-7.07368512557166));
#133578=CARTESIAN_POINT('Ctrl Pts',(20.5254842771696,0.405620360842853,
-7.071710668315));
#133579=CARTESIAN_POINT('Ctrl Pts',(20.5768797550957,0.291107417325853,
-7.06577414664544));
#133580=CARTESIAN_POINT('Ctrl Pts',(20.617749939527,0.216993945476465,-7.06192599283445));
#133581=CARTESIAN_POINT('Ctrl Pts',(20.7004798554822,0.0923743172461711,
-7.05493606753585));
#133582=CARTESIAN_POINT('Ctrl Pts',(20.7398687909791,0.040486334191363,
-7.0518437130033));
#133583=CARTESIAN_POINT('Ctrl Pts',(20.8028326728216,-0.0323912474073396,
-7.04709530335299));
#133584=CARTESIAN_POINT('Ctrl Pts',(20.8239637528491,-0.0553988669875149,
-7.04553045741632));
#133585=CARTESIAN_POINT('Ctrl Pts',(20.8657220878292,-0.0981829553572622,
-7.04248109803501));
#133586=CARTESIAN_POINT('Ctrl Pts',(20.8862290540689,-0.118058867736983,
-7.04100182502386));
#133587=CARTESIAN_POINT('Ctrl Pts',(20.9383559252877,-0.165848753205058,
-7.03728038176894));
#133588=CARTESIAN_POINT('Ctrl Pts',(20.9705899017304,-0.193055943279883,
-7.03501195960825));
#133589=CARTESIAN_POINT('Ctrl Pts',(21.0936050258876,-0.288539093483138,
-7.02647505636288));
#133590=CARTESIAN_POINT('Ctrl Pts',(21.1907230058785,-0.348050194545007,
-7.01993246464822));
#133591=CARTESIAN_POINT('Ctrl Pts',(21.3243259083336,-0.410866099597751,
-7.011596241665));
#133592=CARTESIAN_POINT('Ctrl Pts',(21.3556506367177,-0.424345550700895,
-7.00968819907164));
#133593=CARTESIAN_POINT('Ctrl Pts',(21.4114278316744,-0.446186380588833,
-7.00639883959606));
#133594=CARTESIAN_POINT('Ctrl Pts',(21.4356919064804,-0.454992217573493,
-7.00500276792051));
#133595=CARTESIAN_POINT('Ctrl Pts',(21.4754759321275,-0.468310787723789,
-7.00278232797752));
#133596=CARTESIAN_POINT('Ctrl Pts',(21.4908650874757,-0.473195460255269,
-7.00194012234738));
#133597=CARTESIAN_POINT('Ctrl Pts',(21.5261146013529,-0.483777916261725,
-7.0000508846564));
#133598=CARTESIAN_POINT('Ctrl Pts',(21.5460175944571,-0.489319988870331,
-6.99901155844509));
#133599=CARTESIAN_POINT('Ctrl Pts',(21.6735683421865,-0.522091719025388,
-6.99249103803639));
#133600=CARTESIAN_POINT('Ctrl Pts',(21.7837887111138,-0.538036552840913,
-6.98746920792789));
#133601=CARTESIAN_POINT('Ctrl Pts',(21.945419728441,-0.543825203860573,
-6.97994681118554));
#133602=CARTESIAN_POINT('Ctrl Pts',(21.9961217408377,-0.543142788714532,
-6.9775679413078));
#133603=CARTESIAN_POINT('Ctrl Pts',(22.0872402683269,-0.537421343486204,
-6.97317628028501));
#133604=CARTESIAN_POINT('Ctrl Pts',(22.1276654537821,-0.533275559687159,
-6.97118650990352));
#133605=CARTESIAN_POINT('Ctrl Pts',(22.195974581872,-0.523532395917599,
-6.96772754909587));
#133606=CARTESIAN_POINT('Ctrl Pts',(22.2239537962885,-0.518750684793128,
-6.96628297967836));
#133607=CARTESIAN_POINT('Ctrl Pts',(22.2829535253383,-0.506984109268314,
-6.96317116043018));
#133608=CARTESIAN_POINT('Ctrl Pts',(22.3139217498944,-0.499806629533253,
-6.96149869766345));
#133609=CARTESIAN_POINT('Ctrl Pts',(22.4094051788206,-0.474545117238194,
-6.95621489133463));
#133610=CARTESIAN_POINT('Ctrl Pts',(22.4729748481352,-0.453214447024215,
-6.95251021870147));
#133611=CARTESIAN_POINT('Ctrl Pts',(22.6098273250283,-0.397148542494041,
-6.94417563933477));
#133612=CARTESIAN_POINT('Ctrl Pts',(22.6821713982143,-0.360632524233955,
-6.93952423402196));
#133613=CARTESIAN_POINT('Ctrl Pts',(22.7875780215223,-0.296577189991489,
-6.93259221955281));
#133614=CARTESIAN_POINT('Ctrl Pts',(22.8229167152729,-0.273053899500617,
-6.93024082535303));
#133615=CARTESIAN_POINT('Ctrl Pts',(22.8722546767471,-0.237190245306591,
-6.92696355518505));
#133616=CARTESIAN_POINT('Ctrl Pts',(22.8870691493192,-0.22600769248049,
-6.92598034644523));
#133617=CARTESIAN_POINT('Ctrl Pts',(22.9151152446012,-0.204031935546696,
-6.9241262809822));
#133618=CARTESIAN_POINT('Ctrl Pts',(22.9283760894639,-0.19328143437829,
-6.92325334198535));
#133619=CARTESIAN_POINT('Ctrl Pts',(22.9658106850263,-0.161889779435671,
-6.92079173926943));
#133620=CARTESIAN_POINT('Ctrl Pts',(22.9895298441754,-0.140717817380733,
-6.91923506165352));
#133621=CARTESIAN_POINT('Ctrl Pts',(23.0911481809923,-0.044208231348577,
-6.91249658121761));
#133622=CARTESIAN_POINT('Ctrl Pts',(23.1616420068988,0.0384822650013561,
-6.90761411827222));
#133623=CARTESIAN_POINT('Ctrl Pts',(23.246756380588,0.162710095104583,-6.9005460540303));
#133624=CARTESIAN_POINT('Ctrl Pts',(23.2691791378977,0.198502881308005,
-6.89853939020893));
#133625=CARTESIAN_POINT('Ctrl Pts',(23.3080501397243,0.266611017828464,
-6.89473105156451));
#133626=CARTESIAN_POINT('Ctrl Pts',(23.324881975976,0.298673476871123,-6.8929422353621));
#133627=CARTESIAN_POINT('Ctrl Pts',(23.3526077823798,0.35632936563645,-6.88971494453106));
#133628=CARTESIAN_POINT('Ctrl Pts',(23.363966873702,0.381681285425901,-6.88829249959763));
#133629=CARTESIAN_POINT('Ctrl Pts',(23.3877593496193,0.438872153847334,
-6.8850705269798));
#133630=CARTESIAN_POINT('Ctrl Pts',(23.3998313437624,0.470844778175845,
-6.88326037270658));
#133631=CARTESIAN_POINT('Ctrl Pts',(23.4481802805556,0.613011181954941,
-6.87516754162936));
#133632=CARTESIAN_POINT('Ctrl Pts',(23.4730219262029,0.726682765747686,
-6.86854534014066));
#133633=CARTESIAN_POINT('Ctrl Pts',(23.4892942074949,0.884804194948909,
-6.8595146124425));
#133634=CARTESIAN_POINT('Ctrl Pts',(23.4919060433311,0.927731286423592,
-6.85708569865248));
#133635=CARTESIAN_POINT('Ctrl Pts',(23.4932915484781,1.00071371423795,-6.85304514358394));
#133636=CARTESIAN_POINT('Ctrl Pts',(23.4929858694857,1.03072662701455,-6.85140919309752));
#133637=CARTESIAN_POINT('Ctrl Pts',(23.4911436940628,1.07750853433028,-6.84891771520969));
#133638=CARTESIAN_POINT('Ctrl Pts',(23.4902078937249,1.09429309963478,-6.84803571898826));
#133639=CARTESIAN_POINT('Ctrl Pts',(23.4876280856383,1.13004226184516,-6.84618660210858));
#133640=CARTESIAN_POINT('Ctrl Pts',(23.4859071600779,1.14899791642161,-6.84522311585918));
#133641=CARTESIAN_POINT('Ctrl Pts',(23.479474269024,1.20775884398913,-6.84227644125621));
#133642=CARTESIAN_POINT('Ctrl Pts',(23.473561702995,1.24741747635017,-6.84034479976302));
#133643=CARTESIAN_POINT('Ctrl Pts',(23.4480334903751,1.38236585902902,-6.8338413094117));
#133644=CARTESIAN_POINT('Ctrl Pts',(23.4209611034105,1.47600689798692,-6.82943545975346));
#133645=CARTESIAN_POINT('Ctrl Pts',(23.3702843743358,1.60440350326869,-6.8229424583509));
#133646=CARTESIAN_POINT('Ctrl Pts',(23.3538191453811,1.64171867508635,-6.82099968666875));
#133647=CARTESIAN_POINT('Ctrl Pts',(23.3203343354426,1.71013082681355,-6.81729327346647));
#133648=CARTESIAN_POINT('Ctrl Pts',(23.3036837939901,1.74137840638692,-6.81554097997366));
#133649=CARTESIAN_POINT('Ctrl Pts',(23.2719551874492,1.79628417773131,-6.81233757809382));
#133650=CARTESIAN_POINT('Ctrl Pts',(23.2572786000605,1.82015641473043,-6.81090049815251));
#133651=CARTESIAN_POINT('Ctrl Pts',(23.2228160068598,1.87293442718122,-6.80761639848175));
#133652=CARTESIAN_POINT('Ctrl Pts',(23.2026797895514,1.90159203501022,-6.80575750412412));
#133653=CARTESIAN_POINT('Ctrl Pts',(23.1310769007845,1.99646190582334,-6.79933729399077));
#133654=CARTESIAN_POINT('Ctrl Pts',(23.0752007641256,2.05915043571072,-6.79462402470615));
#133655=CARTESIAN_POINT('Ctrl Pts',(22.9747719206674,2.15486177791452,-6.7867353945752));
#133656=CARTESIAN_POINT('Ctrl Pts',(22.933037559065,2.19058788550244,-6.78359930739587));
#133657=CARTESIAN_POINT('Ctrl Pts',(22.8894916066884,2.22401163452936,-6.78051560659813));
#133658=CARTESIAN_POINT('Origin',(21.9499999789786,0.999999999999992,-4.89578827641128));
#133659=CARTESIAN_POINT('',(22.8894915905204,2.22401164693913,-6.28210119346687));
#133660=CARTESIAN_POINT('',(22.8895004346677,2.22400481472634,-6.32268402640472));
#133661=CARTESIAN_POINT('',(22.8894916101512,2.22401163187148,-4.89578827641128));
#133662=CARTESIAN_POINT('',(20.4070005050181,0.998725889518171,-6.10421116894535));
#133663=CARTESIAN_POINT('Ctrl Pts',(22.8894915905204,2.22401164693913,-6.28210119346687));
#133664=CARTESIAN_POINT('Ctrl Pts',(22.8600553989009,2.2466054312151,-6.28033339624786));
#133665=CARTESIAN_POINT('Ctrl Pts',(22.8298085810512,2.26813397574543,-6.27853880379917));
#133666=CARTESIAN_POINT('Ctrl Pts',(22.7727444074889,2.30572384812454,-6.27516745510784));
#133667=CARTESIAN_POINT('Ctrl Pts',(22.7461660072385,2.3220978228453,-6.27360266342571));
#133668=CARTESIAN_POINT('Ctrl Pts',(22.6941902911137,2.3519822829555,-6.27054290319535));
#133669=CARTESIAN_POINT('Ctrl Pts',(22.6688757747584,2.36561076662804,-6.26905281247638));
#133670=CARTESIAN_POINT('Ctrl Pts',(22.6048225541322,2.39782019571297,-6.26527767352184));
#133671=CARTESIAN_POINT('Ctrl Pts',(22.565662336875,2.41550461754234,-6.26296501168263));
#133672=CARTESIAN_POINT('Ctrl Pts',(22.428894249053,2.47051806277432,-6.25487651315597));
#133673=CARTESIAN_POINT('Ctrl Pts',(22.3282672992176,2.49955775718204,-6.24888450310819));
#133674=CARTESIAN_POINT('Ctrl Pts',(22.1722764493203,2.52786363154342,-6.23991046985082));
#133675=CARTESIAN_POINT('Ctrl Pts',(22.1185865032598,2.5347160902759,-6.23688159576919));
#133676=CARTESIAN_POINT('Ctrl Pts',(22.0446773188154,2.54022274430607,-6.23287971266383));
#133677=CARTESIAN_POINT('Ctrl Pts',(22.0246821453628,2.5413216889432,-6.23181389362117));
#133678=CARTESIAN_POINT('Ctrl Pts',(21.9878240333186,2.54262843759522,-6.22988690615916));
#133679=CARTESIAN_POINT('Ctrl Pts',(21.9709692550235,2.54294959511889,-6.22902086504839));
#133680=CARTESIAN_POINT('Ctrl Pts',(21.9252084244684,2.54307155076537,-6.22670426894211));
#133681=CARTESIAN_POINT('Ctrl Pts',(21.8963066504455,2.54233642118829,-6.2252782296859));
#133682=CARTESIAN_POINT('Ctrl Pts',(21.8270408353905,2.53862500956103,-6.22191554811223));
#133683=CARTESIAN_POINT('Ctrl Pts',(21.7867395678952,2.53487203895624,-6.22000372970443));
#133684=CARTESIAN_POINT('Ctrl Pts',(21.6235471981066,2.51317382521763,-6.21229659923492));
#133685=CARTESIAN_POINT('Ctrl Pts',(21.502896670471,2.48201357631916,-6.20663635098878));
#133686=CARTESIAN_POINT('Ctrl Pts',(21.3574350097396,2.42504154761335,-6.1989408578269));
#133687=CARTESIAN_POINT('Ctrl Pts',(21.3279587438811,2.41242386796144,-6.19733624205496));
#133688=CARTESIAN_POINT('Ctrl Pts',(21.2728115453115,2.38675619606742,-6.19423587548501));
#133689=CARTESIAN_POINT('Ctrl Pts',(21.2470710311032,2.3738877969212,-6.19274645174937));
#133690=CARTESIAN_POINT('Ctrl Pts',(21.1849736159429,2.3406415323837,-6.18904272977856));
#133691=CARTESIAN_POINT('Ctrl Pts',(21.1490549929924,2.3194967891154,-6.18680390040954));
#133692=CARTESIAN_POINT('Ctrl Pts',(21.0699299863074,2.2684950233314,-6.18164967455186));
#133693=CARTESIAN_POINT('Ctrl Pts',(21.0273037886067,2.2378343807638,-6.17871224587833));
#133694=CARTESIAN_POINT('Ctrl Pts',(20.9029608879772,2.13839881092861,-6.16969916154285));
#133695=CARTESIAN_POINT('Ctrl Pts',(20.8267386383126,2.06326282245282,-6.1635259810367));
#133696=CARTESIAN_POINT('Ctrl Pts',(20.7453009317883,1.96436798655721,-6.15657028512496));
#133697=CARTESIAN_POINT('Ctrl Pts',(20.7320636771059,1.94759519842708,-6.15542705973641));
#133698=CARTESIAN_POINT('Ctrl Pts',(20.7097270652528,1.91805103633547,-6.15348322115078));
#133699=CARTESIAN_POINT('Ctrl Pts',(20.7004668270198,1.90540684845341,-6.15267309604488));
#133700=CARTESIAN_POINT('Ctrl Pts',(20.6782243882741,1.87404493695788,-6.15071697341251));
#133701=CARTESIAN_POINT('Ctrl Pts',(20.6654612999617,1.85517728613556,-6.14958425638012));
#133702=CARTESIAN_POINT('Ctrl Pts',(20.6375599109191,1.81189580118105,-6.14706780939901));
#133703=CARTESIAN_POINT('Ctrl Pts',(20.6226760267317,1.78732775370399,-6.14569614075528));
#133704=CARTESIAN_POINT('Ctrl Pts',(20.5721698227893,1.69845242859358,-6.14088300763944));
#133705=CARTESIAN_POINT('Ctrl Pts',(20.540465224596,1.63203187329078,-6.13755155522816));
#133706=CARTESIAN_POINT('Ctrl Pts',(20.4844006410698,1.48914690638092,-6.13049671404354));
#133707=CARTESIAN_POINT('Ctrl Pts',(20.4610212648567,1.41253730832467,-6.12677259578111));
#133708=CARTESIAN_POINT('Ctrl Pts',(20.436805875047,1.30347994205005,-6.1213120860232));
#133709=CARTESIAN_POINT('Ctrl Pts',(20.4308837375617,1.27229054016978,-6.11973400305116));
#133710=CARTESIAN_POINT('Ctrl Pts',(20.4217173393884,1.21430873009392,-6.11675935037156));
#133711=CARTESIAN_POINT('Ctrl Pts',(20.4182058996628,1.18757088729275,-6.11537175597376));
#133712=CARTESIAN_POINT('Ctrl Pts',(20.4127836711266,1.13580934329507,-6.11265134435453));
#133713=CARTESIAN_POINT('Ctrl Pts',(20.4107792170472,1.11080390447286,-6.11132187629459));
#133714=CARTESIAN_POINT('Ctrl Pts',(20.4077706531801,1.05675830852917,-6.10841482815476));
#133715=CARTESIAN_POINT('Ctrl Pts',(20.4069755445682,1.02771678371464,-6.10683182438699));
#133716=CARTESIAN_POINT('Ctrl Pts',(20.4070005508311,0.998671566178611,
-6.10522917581996));
#133717=CARTESIAN_POINT('',(21.5514861371214,-0.490649428218508,-6.00000000000001));
#133718=CARTESIAN_POINT('Ctrl Pts',(21.5514861371214,-0.490649428218532,
-6.00000000000001));
#133719=CARTESIAN_POINT('Ctrl Pts',(21.4945349590153,-0.475423961817293,
-6.00304030623798));
#133720=CARTESIAN_POINT('Ctrl Pts',(21.4384128966158,-0.456918607184443,
-6.00608061247596));
#133721=CARTESIAN_POINT('Ctrl Pts',(21.38350805469,-0.435247678874912,-6.00912091871394));
#133722=CARTESIAN_POINT('Ctrl Pts',(21.3286309055878,-0.413587680916414,
-6.01215969148671));
#133723=CARTESIAN_POINT('Ctrl Pts',(21.2749702099976,-0.388765455016415,
-6.01519846425949));
#133724=CARTESIAN_POINT('Ctrl Pts',(21.2228965519548,-0.360944380351481,
-6.01823723703227));
#133725=CARTESIAN_POINT('Ctrl Pts',(21.170835959667,-0.333130286247549,
-6.02127524734928));
#133726=CARTESIAN_POINT('Ctrl Pts',(21.1203620422553,-0.302319066725625,
-6.02431325766629));
#133727=CARTESIAN_POINT('Ctrl Pts',(21.0718214599,-0.268720413893039,-6.0273512679833));
#133728=CARTESIAN_POINT('Ctrl Pts',(21.023278430521,-0.235120067288085,
-6.03038943145223));
#133729=CARTESIAN_POINT('Ctrl Pts',(20.976669328728,-0.198732285415966,
-6.03342759492116));
#133730=CARTESIAN_POINT('Ctrl Pts',(20.9323109715251,-0.159809503370445,
-6.03646575839008));
#133731=CARTESIAN_POINT('Ctrl Pts',(20.8879370108942,-0.120873029906427,
-6.03950499055876));
#133732=CARTESIAN_POINT('Ctrl Pts',(20.84581573173,-0.079400106202768,-6.04254422272743));
#133733=CARTESIAN_POINT('Ctrl Pts',(20.8062287260957,-0.035681573206096,
-6.04558345489611));
#133734=CARTESIAN_POINT('Ctrl Pts',(20.7665859145349,0.00809858994418625,
-6.04862697147995));
#133735=CARTESIAN_POINT('Ctrl Pts',(20.7294848338383,0.0541303200353416,
-6.05167048806378));
#133736=CARTESIAN_POINT('Ctrl Pts',(20.6951676387845,0.102088646912787,
-6.05471400464761));
#133737=CARTESIAN_POINT('Ctrl Pts',(20.6608240427085,0.150083869254561,
-6.05775986268005));
#133738=CARTESIAN_POINT('Ctrl Pts',(20.6292688596443,0.200008230956686,
-6.06080572071249));
#133739=CARTESIAN_POINT('Ctrl Pts',(20.6007000136401,0.251509115928909,
-6.06385157874493));
#133740=CARTESIAN_POINT('Ctrl Pts',(20.5720768570487,0.303107906266273,
-6.06690322708258));
#133741=CARTESIAN_POINT('Ctrl Pts',(20.5464515881279,0.356288768094418,
-6.06995487542024));
#133742=CARTESIAN_POINT('Ctrl Pts',(20.5239750856165,0.410676656230577,
-6.07300652375789));
#133743=CARTESIAN_POINT('Ctrl Pts',(20.5137504352638,0.435417922774606,
-6.07439473071918));
#133744=CARTESIAN_POINT('Ctrl Pts',(20.5041767079994,0.460408731288417,
-6.07578293768047));
#133745=CARTESIAN_POINT('Ctrl Pts',(20.4952646815418,0.485612777771825,
-6.07717114464176));
#133746=CARTESIAN_POINT('Ctrl Pts',(20.4737630263397,0.546421474847099,
-6.08052041066706));
#133747=CARTESIAN_POINT('Ctrl Pts',(20.4560483133547,0.60866417772397,-6.08386967669236));
#133748=CARTESIAN_POINT('Ctrl Pts',(20.4422897149553,0.671886056744092,
-6.08721894271766));
#133749=CARTESIAN_POINT('Ctrl Pts',(20.4286352356818,0.734629499910075,
-6.09054286294533));
#133750=CARTESIAN_POINT('Ctrl Pts',(20.4188773539673,0.79833710680527,-6.09386678317299));
#133751=CARTESIAN_POINT('Ctrl Pts',(20.4131347728899,0.862543322046143,
-6.09719070340066));
#133752=CARTESIAN_POINT('Ctrl Pts',(20.4090917965417,0.907746725555561,
-6.09953085858222));
#133753=CARTESIAN_POINT('Ctrl Pts',(20.407038100011,0.953196828097098,-6.10187101376378));
#133754=CARTESIAN_POINT('Ctrl Pts',(20.4070005050181,0.99872588951817,-6.10421116894535));
#133755=CARTESIAN_POINT('',(22.3495840788696,-0.491448861522601,-6.00061432324861));
#133756=CARTESIAN_POINT('Origin',(21.9499999789786,0.999999999999992,-6.00000000000001));
#133757=CARTESIAN_POINT('Ctrl Pts',(22.3492600981242,-0.49044971644798,
-6.00122173936631));
#133758=CARTESIAN_POINT('Ctrl Pts',(22.2389460564105,-0.520000527154304,
-6.00677119856528));
#133759=CARTESIAN_POINT('Ctrl Pts',(22.1256840647128,-0.537215372964368,
-6.01190298829388));
#133760=CARTESIAN_POINT('Ctrl Pts',(21.9677427274376,-0.543520801088802,
-6.01930601480983));
#133761=CARTESIAN_POINT('Ctrl Pts',(21.9238811128887,-0.54340169363555,
-6.0213846758462));
#133762=CARTESIAN_POINT('Ctrl Pts',(21.8428736818116,-0.539727424063985,
-6.02531513175915));
#133763=CARTESIAN_POINT('Ctrl Pts',(21.8057369663867,-0.536692717851297,
-6.02715258783839));
#133764=CARTESIAN_POINT('Ctrl Pts',(21.7405056763577,-0.528976758088233,
-6.03046194549552));
#133765=CARTESIAN_POINT('Ctrl Pts',(21.7123623617402,-0.524856065847814,
-6.03191678715776));
#133766=CARTESIAN_POINT('Ctrl Pts',(21.6503648202652,-0.514020491329616,
-6.03518766512962));
#133767=CARTESIAN_POINT('Ctrl Pts',(21.6165902362738,-0.506942926832763,
-6.03701374319692));
#133768=CARTESIAN_POINT('Ctrl Pts',(21.5117169171735,-0.481268139899593,
-6.04282634549045));
#133769=CARTESIAN_POINT('Ctrl Pts',(21.4416964926351,-0.458723121755922,
-6.0469206074828));
#133770=CARTESIAN_POINT('Ctrl Pts',(21.3106334568717,-0.405937633412248,
-6.05490532750201));
#133771=CARTESIAN_POINT('Ctrl Pts',(21.2494521601919,-0.376474876570989,
-6.05877746229642));
#133772=CARTESIAN_POINT('Ctrl Pts',(21.1661251445168,-0.329348522734971,
-6.06412434161184));
#133773=CARTESIAN_POINT('Ctrl Pts',(21.1422183519377,-0.314958638490253,
-6.06566686852603));
#133774=CARTESIAN_POINT('Ctrl Pts',(21.0997017366622,-0.287769848717985,
-6.06840956690481));
#133775=CARTESIAN_POINT('Ctrl Pts',(21.0809575576242,-0.275195535103139,
-6.06961849079366));
#133776=CARTESIAN_POINT('Ctrl Pts',(21.0490555499635,-0.252764166351627,
-6.07166667355661));
#133777=CARTESIAN_POINT('Ctrl Pts',(21.0357684422469,-0.243100822828799,
-6.0725161757459));
#133778=CARTESIAN_POINT('Ctrl Pts',(21.0063495257877,-0.22097833516864,
-6.07439024599287));
#133779=CARTESIAN_POINT('Ctrl Pts',(20.990305966843,-0.208408766142356,
-6.07540837189322));
#133780=CARTESIAN_POINT('Ctrl Pts',(20.9168587552396,-0.148479743675298,
-6.08007417882351));
#133781=CARTESIAN_POINT('Ctrl Pts',(20.8626762669674,-0.0973218886797023,
-6.08353352830336));
#133782=CARTESIAN_POINT('Ctrl Pts',(20.7497573544803,0.0259043337482767,
-6.09128365314722));
#133783=CARTESIAN_POINT('Ctrl Pts',(20.6934103137738,0.0997633753528193,
-6.09556198197975));
#133784=CARTESIAN_POINT('Ctrl Pts',(20.6246422260201,0.209049987884131,
-6.10183457832132));
#133785=CARTESIAN_POINT('Ctrl Pts',(20.6063461910823,0.240546676970981,
-6.10363440488854));
#133786=CARTESIAN_POINT('Ctrl Pts',(20.576012610059,0.297299312273243,-6.10688156409804));
#133787=CARTESIAN_POINT('Ctrl Pts',(20.5635152670006,0.322290943916612,
-6.10831273841653));
#133788=CARTESIAN_POINT('Ctrl Pts',(20.5371537861922,0.378792418623317,
-6.11155694980618));
#133789=CARTESIAN_POINT('Ctrl Pts',(20.523652016707,0.410454007411718,-6.11338078139074));
#133790=CARTESIAN_POINT('Ctrl Pts',(20.4855010749848,0.508919708531068,
-6.11907447167697));
#133791=CARTESIAN_POINT('Ctrl Pts',(20.4644086054296,0.576994687016685,
-6.12304523881323));
#133792=CARTESIAN_POINT('Ctrl Pts',(20.426371671626,0.738499367635295,-6.13244484822318));
#133793=CARTESIAN_POINT('Ctrl Pts',(20.4131917664023,0.832527525450142,
-6.13790678576824));
#133794=CARTESIAN_POINT('Ctrl Pts',(20.4074799514418,0.953407776264625,
-6.14455885747248));
#133795=CARTESIAN_POINT('Ctrl Pts',(20.4069102795322,0.979672727419416,
-6.14598107986032));
#133796=CARTESIAN_POINT('Ctrl Pts',(20.407074337124,1.0222834328177,-6.14823787442868));
#133797=CARTESIAN_POINT('Ctrl Pts',(20.4073968871114,1.0386246937928,-6.14909100723485));
#133798=CARTESIAN_POINT('Ctrl Pts',(20.4087087238537,1.07543140343511,-6.1509823018051));
#133799=CARTESIAN_POINT('Ctrl Pts',(20.4098460050509,1.09588765886885,-6.15201339257036));
#133800=CARTESIAN_POINT('Ctrl Pts',(20.4160801089225,1.1783513212385,-6.15610974492835));
#133801=CARTESIAN_POINT('Ctrl Pts',(20.4245177640344,1.24005114339434,-6.15903835603049));
#133802=CARTESIAN_POINT('Ctrl Pts',(20.4591147545198,1.41395044292493,-6.16728631434038));
#133803=CARTESIAN_POINT('Ctrl Pts',(20.4941261403144,1.52395053529094,-6.17252368462059));
#133804=CARTESIAN_POINT('Ctrl Pts',(20.5549909095745,1.66027988345722,-6.17980850959296));
#133805=CARTESIAN_POINT('Ctrl Pts',(20.569975055633,1.69105052649164,-6.18150656486357));
#133806=CARTESIAN_POINT('Ctrl Pts',(20.5990244616489,1.74598534889885,-6.18465173205501));
#133807=CARTESIAN_POINT('Ctrl Pts',(20.6127472285442,1.77031418507078,-6.18608696454662));
#133808=CARTESIAN_POINT('Ctrl Pts',(20.6456358647184,1.82509203036845,-6.18942227251122));
#133809=CARTESIAN_POINT('Ctrl Pts',(20.6652210329991,1.8552691916005,-6.19133632453058));
#133810=CARTESIAN_POINT('Ctrl Pts',(20.7399076036783,1.96198572939441,-6.19839177344126));
#133811=CARTESIAN_POINT('Ctrl Pts',(20.8009359090357,2.03411237170792,-6.20373317207936));
#133812=CARTESIAN_POINT('Ctrl Pts',(20.9211764269764,2.15234553094063,-6.2133402501196));
#133813=CARTESIAN_POINT('Ctrl Pts',(20.9778985205184,2.20058240741101,-6.21757715180105));
#133814=CARTESIAN_POINT('Ctrl Pts',(21.0559785456939,2.25780688078353,-6.22285164873405));
#133815=CARTESIAN_POINT('Ctrl Pts',(21.0743646949676,2.27067518339825,-6.22405636420658));
#133816=CARTESIAN_POINT('Ctrl Pts',(21.1064163536908,2.29208163553281,-6.22608456222704));
#133817=CARTESIAN_POINT('Ctrl Pts',(21.1199452962614,2.30081418536878,-6.22691880436355));
#133818=CARTESIAN_POINT('Ctrl Pts',(21.1533951002631,2.32167064583337,-6.22892986322777));
#133819=CARTESIAN_POINT('Ctrl Pts',(21.1734581438383,2.33355746512882,-6.23009342356617));
#133820=CARTESIAN_POINT('Ctrl Pts',(21.2193653160923,2.35936870536518,-6.23267777615744));
#133821=CARTESIAN_POINT('Ctrl Pts',(21.2453530360858,2.37301970664579,-6.23408677404265));
#133822=CARTESIAN_POINT('Ctrl Pts',(21.3401133532828,2.41939640591508,-6.23908539283991));
#133823=CARTESIAN_POINT('Ctrl Pts',(21.4108974256887,2.44776275967269,-6.24256715351212));
#133824=CARTESIAN_POINT('Ctrl Pts',(21.4885359458098,2.47238853170355,-6.24635610638211));
#133825=CARTESIAN_POINT('Ctrl Pts',(21.4935918018411,2.47396357410221,-6.24660268601106));
#133826=CARTESIAN_POINT('Ctrl Pts',(21.5622279170449,2.49495866560251,-6.24994881050477));
#133827=CARTESIAN_POINT('Ctrl Pts',(21.6269866199216,2.51027481141422,-6.25309455412155));
#133828=CARTESIAN_POINT('Ctrl Pts',(21.7244173001186,2.52676374822183,-6.25794806330741));
#133829=CARTESIAN_POINT('Ctrl Pts',(21.7564673785425,2.53115643878961,-6.2595628771343));
#133830=CARTESIAN_POINT('Ctrl Pts',(21.8168444990354,2.53750559320117,-6.26265054819264));
#133831=CARTESIAN_POINT('Ctrl Pts',(21.8451336436462,2.53969371943589,-6.26411584255606));
#133832=CARTESIAN_POINT('Ctrl Pts',(21.9131739847374,2.5430727347742,-6.26768994805713));
#133833=CARTESIAN_POINT('Ctrl Pts',(21.9529408887972,2.54350918749679,-6.26981984984527));
#133834=CARTESIAN_POINT('Ctrl Pts',(22.0415697650441,2.54105684256572,-6.27465787470543));
#133835=CARTESIAN_POINT('Ctrl Pts',(22.0903664911747,2.53738022209195,-6.27738386990655));
#133836=CARTESIAN_POINT('Ctrl Pts',(22.2265459946849,2.52058191394221,-6.28512499152032));
#133837=CARTESIAN_POINT('Ctrl Pts',(22.3130971043322,2.50226743725145,-6.29020900478887));
#133838=CARTESIAN_POINT('Ctrl Pts',(22.4309242280149,2.46655138514755,-6.29706996368971));
#133839=CARTESIAN_POINT('Ctrl Pts',(22.4638931476742,2.4553264943439,-6.29898122936458));
#133840=CARTESIAN_POINT('Ctrl Pts',(22.5128797035298,2.43677550142827,-6.3017808672692));
#133841=CARTESIAN_POINT('Ctrl Pts',(22.5291970295223,2.43027559174652,-6.30270649612236));
#133842=CARTESIAN_POINT('Ctrl Pts',(22.5620524528981,2.4165332895137,-6.30455107145079));
#133843=CARTESIAN_POINT('Ctrl Pts',(22.5785814608003,2.40927646966181,-6.30546913265023));
#133844=CARTESIAN_POINT('Ctrl Pts',(22.6297832884031,2.38571691547216,-6.30829280364629));
#133845=CARTESIAN_POINT('Ctrl Pts',(22.6639803134744,2.36841118237412,-6.31014945798633));
#133846=CARTESIAN_POINT('Ctrl Pts',(22.7645337602741,2.31272818320848,-6.31561738288569));
#133847=CARTESIAN_POINT('Ctrl Pts',(22.8287116292269,2.27066407013551,-6.31912334298961));
#133848=CARTESIAN_POINT('Ctrl Pts',(22.8895003442092,2.22400492798496,-6.32268395960923));
#133849=CARTESIAN_POINT('Origin',(-21.9500000210213,0.999999999999992,-4.89578827641128));
#133850=CARTESIAN_POINT('',(-21.0105083902185,2.22401163215526,-7.78024815277603));
#133851=CARTESIAN_POINT('',(-21.0105083757967,2.22401162108585,-7.82252260735286));
#133852=CARTESIAN_POINT('',(-21.0105083758276,2.22401162110953,-4.89578827641128));
#133853=CARTESIAN_POINT('',(-21.5514861791641,-0.490649428218508,-8.00000000000001));
#133854=CARTESIAN_POINT('Ctrl Pts',(-21.0105083757967,2.22401162108585,
-7.82252260735286));
#133855=CARTESIAN_POINT('Ctrl Pts',(-21.0101364665912,2.22372616171165,
-7.82254903034026));
#133856=CARTESIAN_POINT('Ctrl Pts',(-21.0097646849254,2.22344053087246,
-7.82257545653808));
#133857=CARTESIAN_POINT('Ctrl Pts',(-20.9415574485498,2.17098911014149,
-7.8274258697074));
#133858=CARTESIAN_POINT('Ctrl Pts',(-20.8781806357393,2.11327211895452,
-7.83235245582535));
#133859=CARTESIAN_POINT('Ctrl Pts',(-20.7931319397805,2.021788962789,-7.83935306760022));
#133860=CARTESIAN_POINT('Ctrl Pts',(-20.7674574930824,1.99196270521193,
-7.84152583818574));
#133861=CARTESIAN_POINT('Ctrl Pts',(-20.7316291236481,1.94696970088399,
-7.84461094125883));
#133862=CARTESIAN_POINT('Ctrl Pts',(-20.7205600831609,1.93255388876716,
-7.84557212336584));
#133863=CARTESIAN_POINT('Ctrl Pts',(-20.6999790583234,1.90474650013823,
-7.84736967305452));
#133864=CARTESIAN_POINT('Ctrl Pts',(-20.6904217720473,1.89139288667088,
-7.84820831404718));
#133865=CARTESIAN_POINT('Ctrl Pts',(-20.6638711720371,1.85301603447934,
-7.85055540520169));
#133866=CARTESIAN_POINT('Ctrl Pts',(-20.6473972055945,1.82764115965349,
-7.85203352878403));
#133867=CARTESIAN_POINT('Ctrl Pts',(-20.6088757422345,1.76430386038195,
-7.85558658163264));
#133868=CARTESIAN_POINT('Ctrl Pts',(-20.5876813430491,1.72585321197464,
-7.8576288300798));
#133869=CARTESIAN_POINT('Ctrl Pts',(-20.5153433346791,1.58025565853965,
-7.86512319148981));
#133870=CARTESIAN_POINT('Ctrl Pts',(-20.4749760545482,1.46823052444739,
-7.87046330075095));
#133871=CARTESIAN_POINT('Ctrl Pts',(-20.4400936045535,1.3196598991621,-7.87787308008542));
#133872=CARTESIAN_POINT('Ctrl Pts',(-20.4334312005787,1.28638896378547,
-7.87954958683943));
#133873=CARTESIAN_POINT('Ctrl Pts',(-20.4234590698477,1.2263760915183,-7.88261793112134));
#133874=CARTESIAN_POINT('Ctrl Pts',(-20.4197428587125,1.19971557253502,
-7.88399643310594));
#133875=CARTESIAN_POINT('Ctrl Pts',(-20.4129891727275,1.13984911668774,
-7.88713097929326));
#133876=CARTESIAN_POINT('Ctrl Pts',(-20.4103269711696,1.10661518845308,
-7.88889789704431));
#133877=CARTESIAN_POINT('Ctrl Pts',(-20.4050970260198,0.996680750127306,
-7.89483355749922));
#133878=CARTESIAN_POINT('Ctrl Pts',(-20.4071730285304,0.919881221640968,
-7.89913247009676));
#133879=CARTESIAN_POINT('Ctrl Pts',(-20.4249337908562,0.745603808065916,
-7.90909211026956));
#133880=CARTESIAN_POINT('Ctrl Pts',(-20.4442706781516,0.648823289085554,
-7.91477605849206));
#133881=CARTESIAN_POINT('Ctrl Pts',(-20.478551910376,0.535133969891604,
-7.9212194892826));
#133882=CARTESIAN_POINT('Ctrl Pts',(-20.4847866649622,0.515841072379941,
-7.92230381076316));
#133883=CARTESIAN_POINT('Ctrl Pts',(-20.4966653771655,0.4814173590333,-7.9242148922779));
#133884=CARTESIAN_POINT('Ctrl Pts',(-20.5021692818573,0.466243780132118,
-7.92504824956178));
#133885=CARTESIAN_POINT('Ctrl Pts',(-20.5168580125421,0.427648969840413,
-7.92714911191537));
#133886=CARTESIAN_POINT('Ctrl Pts',(-20.5263791873653,0.404361209544981,
-7.92839926840572));
#133887=CARTESIAN_POINT('Ctrl Pts',(-20.549463745622,0.351618962859086,
-7.93121062067599));
#133888=CARTESIAN_POINT('Ctrl Pts',(-20.563394706907,0.322338055432545,
-7.93275679063243));
#133889=CARTESIAN_POINT('Ctrl Pts',(-20.6203510831758,0.211747237138487,
-7.93861007554522));
#133890=CARTESIAN_POINT('Ctrl Pts',(-20.6696914423677,0.133905544782897,
-7.94276892681729));
#133891=CARTESIAN_POINT('Ctrl Pts',(-20.7662759191897,0.00798323245494448,
-7.95016071945355));
#133892=CARTESIAN_POINT('Ctrl Pts',(-20.8102671522517,-0.0422610010400515,
-7.95332402361043));
#133893=CARTESIAN_POINT('Ctrl Pts',(-20.8817143842222,-0.113913629167302,
-7.9582974566318));
#133894=CARTESIAN_POINT('Ctrl Pts',(-20.9068697361912,-0.137504627672249,
-7.96002072079728));
#133895=CARTESIAN_POINT('Ctrl Pts',(-20.9565760612962,-0.18108350126588,
-7.96338515672788));
#133896=CARTESIAN_POINT('Ctrl Pts',(-20.9809934423874,-0.201197521638292,
-7.96502050629124));
#133897=CARTESIAN_POINT('Ctrl Pts',(-21.0454698315142,-0.251064557923271,
-7.96929935346712));
#133898=CARTESIAN_POINT('Ctrl Pts',(-21.0863831581526,-0.279649458108628,
-7.97197811452552));
#133899=CARTESIAN_POINT('Ctrl Pts',(-21.2322368052158,-0.371368263218477,
-7.98138249353394));
#133900=CARTESIAN_POINT('Ctrl Pts',(-21.3432485853337,-0.423968475974452,
-7.98832698880254));
#133901=CARTESIAN_POINT('Ctrl Pts',(-21.4765752288491,-0.468689818554702,
-7.99589803576898));
#133902=CARTESIAN_POINT('Ctrl Pts',(-21.4939471892734,-0.47417660831274,
-7.99686953981591));
#133903=CARTESIAN_POINT('Ctrl Pts',(-21.5247187777658,-0.483299523563084,
-7.99856015766123));
#133904=CARTESIAN_POINT('Ctrl Pts',(-21.5380778050746,-0.487064800894149,
-7.99928420157857));
#133905=CARTESIAN_POINT('Ctrl Pts',(-21.5514861791641,-0.490649428218531,
-7.99999999999997));
#133906=CARTESIAN_POINT('',(-22.3495836570369,-0.491450109733673,-7.99938619261749));
#133907=CARTESIAN_POINT('Origin',(-21.9500000210213,0.999999999999992,-8.00000000000001));
#133908=CARTESIAN_POINT('Ctrl Pts',(-22.3492583994676,-0.490450182743604,
-7.99877810051043));
#133909=CARTESIAN_POINT('Ctrl Pts',(-22.2384388820329,-0.520136261046303,
-7.99320323557973));
#133910=CARTESIAN_POINT('Ctrl Pts',(-22.1246459944166,-0.537372637890604,
-7.98804968162678));
#133911=CARTESIAN_POINT('Ctrl Pts',(-21.9664146949985,-0.543528710254337,
-7.98063115457279));
#133912=CARTESIAN_POINT('Ctrl Pts',(-21.9227930458819,-0.543376110631364,
-7.97856310091227));
#133913=CARTESIAN_POINT('Ctrl Pts',(-21.8421707043095,-0.539674874830167,
-7.9746501645128));
#133914=CARTESIAN_POINT('Ctrl Pts',(-21.8051788113476,-0.536636731148366,
-7.97281937567373));
#133915=CARTESIAN_POINT('Ctrl Pts',(-21.7401379958302,-0.528925477980793,
-7.96951906637576));
#133916=CARTESIAN_POINT('Ctrl Pts',(-21.7120409465171,-0.524805081106625,
-7.96806637484147));
#133917=CARTESIAN_POINT('Ctrl Pts',(-21.650086568324,-0.513965478821969,
-7.96479733085237));
#133918=CARTESIAN_POINT('Ctrl Pts',(-21.6163094102781,-0.506880848368754,
-7.96297085456803));
#133919=CARTESIAN_POINT('Ctrl Pts',(-21.5110114463801,-0.481081012433662,
-7.95713388664677));
#133920=CARTESIAN_POINT('Ctrl Pts',(-21.4405862735911,-0.458357903949134,
-7.95301400344654));
#133921=CARTESIAN_POINT('Ctrl Pts',(-21.3095237292062,-0.405414164595004,
-7.94502466825928));
#133922=CARTESIAN_POINT('Ctrl Pts',(-21.2487049862821,-0.376075685144217,
-7.94117463103428));
#133923=CARTESIAN_POINT('Ctrl Pts',(-21.1657927426782,-0.329150740126245,
-7.9358540260567));
#133924=CARTESIAN_POINT('Ctrl Pts',(-21.1419585008929,-0.314797236550457,
-7.93431615194845));
#133925=CARTESIAN_POINT('Ctrl Pts',(-21.0995576879271,-0.287673787591833,
-7.93158091869557));
#133926=CARTESIAN_POINT('Ctrl Pts',(-21.0808578105156,-0.275126605941027,
-7.9303748663119));
#133927=CARTESIAN_POINT('Ctrl Pts',(-21.04901952846,-0.252737905173928,
-7.92833078870972));
#133928=CARTESIAN_POINT('Ctrl Pts',(-21.0357526680659,-0.243088863336784,
-7.92748258443072));
#133929=CARTESIAN_POINT('Ctrl Pts',(-21.0063770126725,-0.220999055005691,
-7.92561126463514));
#133930=CARTESIAN_POINT('Ctrl Pts',(-20.9903562287209,-0.208448152004266,
-7.92459457615832));
#133931=CARTESIAN_POINT('Ctrl Pts',(-20.9160165047158,-0.147798369704182,
-7.91987207901798));
#133932=CARTESIAN_POINT('Ctrl Pts',(-20.861031231293,-0.0957699230770892,
-7.91636116260214));
#133933=CARTESIAN_POINT('Ctrl Pts',(-20.7482389106577,0.027869189716978,
-7.90860196020264));
#133934=CARTESIAN_POINT('Ctrl Pts',(-20.692570999941,0.101034389439105,
-7.90436462058109));
#133935=CARTESIAN_POINT('Ctrl Pts',(-20.6244066672067,0.209449570851663,
-7.89814236080197));
#133936=CARTESIAN_POINT('Ctrl Pts',(-20.6061700119408,0.240863394503106,
-7.89634727513816));
#133937=CARTESIAN_POINT('Ctrl Pts',(-20.5759137041703,0.29749449652976,
-7.89310706347015));
#133938=CARTESIAN_POINT('Ctrl Pts',(-20.5634384547691,0.322449937740252,
-7.89167795074537));
#133939=CARTESIAN_POINT('Ctrl Pts',(-20.5371092778647,0.378895001071782,
-7.88843696223817));
#133940=CARTESIAN_POINT('Ctrl Pts',(-20.5236184236341,0.41053670672039,
-7.88661426736097));
#133941=CARTESIAN_POINT('Ctrl Pts',(-20.4854206959021,0.509135814754278,
-7.88091285356935));
#133942=CARTESIAN_POINT('Ctrl Pts',(-20.4642933731975,0.577372119177006,
-7.87693256769951));
#133943=CARTESIAN_POINT('Ctrl Pts',(-20.4263143282665,0.738892566900184,
-7.86753224324677));
#133944=CARTESIAN_POINT('Ctrl Pts',(-20.4131762028146,0.832762284156119,
-7.8620800221764));
#133945=CARTESIAN_POINT('Ctrl Pts',(-20.4074791168623,0.953452867454163,
-7.85543859438069));
#133946=CARTESIAN_POINT('Ctrl Pts',(-20.4069105875293,0.979689338170266,
-7.85401794089713));
#133947=CARTESIAN_POINT('Ctrl Pts',(-20.407074122763,1.02224945059713,-7.85176381209117));
#133948=CARTESIAN_POINT('Ctrl Pts',(-20.4073957602307,1.0385686178664,-7.85091180793199));
#133949=CARTESIAN_POINT('Ctrl Pts',(-20.4087032216148,1.07530486524538,
-7.84902404313319));
#133950=CARTESIAN_POINT('Ctrl Pts',(-20.4098358161491,1.09571282519011,
-7.84799529516952));
#133951=CARTESIAN_POINT('Ctrl Pts',(-20.4155956852066,1.17205054070338,
-7.84420284070168));
#133952=CARTESIAN_POINT('Ctrl Pts',(-20.4228676212515,1.22774018619161,
-7.8415474830042));
#133953=CARTESIAN_POINT('Ctrl Pts',(-20.4484032470428,1.36464968149549,
-7.83504944595518));
#133954=CARTESIAN_POINT('Ctrl Pts',(-20.4702296781954,1.445019155653,-7.83125563776568));
#133955=CARTESIAN_POINT('Ctrl Pts',(-20.5164716674808,1.57330416441257,
-7.82481900236634));
#133956=CARTESIAN_POINT('Ctrl Pts',(-20.5370951030455,1.6223988119019,-7.82225979576069));
#133957=CARTESIAN_POINT('Ctrl Pts',(-20.5731772706048,1.69720781856102,
-7.81814274628359));
#133958=CARTESIAN_POINT('Ctrl Pts',(-20.5869186867565,1.72370488261534,
-7.81664000558087));
#133959=CARTESIAN_POINT('Ctrl Pts',(-20.6155331988979,1.77517155548965,
-7.81362360810701));
#133960=CARTESIAN_POINT('Ctrl Pts',(-20.6303604959109,1.80015249733067,
-7.81211193555699));
#133961=CARTESIAN_POINT('Ctrl Pts',(-20.6709788817185,1.86438333425773,
-7.80809366056266));
#133962=CARTESIAN_POINT('Ctrl Pts',(-20.6978708531977,1.90289844092202,
-7.80554979851484));
#133963=CARTESIAN_POINT('Ctrl Pts',(-20.7660407117086,1.99161801298054,
-7.7993678259325));
#133964=CARTESIAN_POINT('Ctrl Pts',(-20.8088152773384,2.04055869075717,
-7.79568820833976));
#133965=CARTESIAN_POINT('Ctrl Pts',(-20.9033924699419,2.13590186039225,
-7.78803967956329));
#133966=CARTESIAN_POINT('Ctrl Pts',(-20.9555001348351,2.18178997821006,
-7.78407748728989));
#133967=CARTESIAN_POINT('Ctrl Pts',(-21.0105083902185,2.22401163215526,
-7.78024815277603));
#133968=CARTESIAN_POINT('Origin',(-21.9500000210213,0.999999999999992,-4.89578827641128));
#133969=CARTESIAN_POINT('',(-21.0105083871506,2.22401162980051,-7.28231522554091));
#133970=CARTESIAN_POINT('',(-21.0105083124886,2.22401157249358,-7.32301699234766));
#133971=CARTESIAN_POINT('',(-21.0105083758276,2.22401162110953,-4.89578827641128));
#133972=CARTESIAN_POINT('',(-23.4929999234274,0.999451206005362,-7.64468148481327));
#133973=CARTESIAN_POINT('Ctrl Pts',(-21.0105083124886,2.22401157249359,
-7.32301699234766));
#133974=CARTESIAN_POINT('Ctrl Pts',(-20.9825174099087,2.20252711803328,
-7.32465074210701));
#133975=CARTESIAN_POINT('Ctrl Pts',(-20.9552590027711,2.18007909040033,
-7.32628511078963));
#133976=CARTESIAN_POINT('Ctrl Pts',(-20.8802334173451,2.11384142226394,
-7.33096327137465));
#133977=CARTESIAN_POINT('Ctrl Pts',(-20.8344335815339,2.06796717042893,
-7.33404150784907));
#133978=CARTESIAN_POINT('Ctrl Pts',(-20.7710173471336,1.99590392117325,
-7.33877508236544));
#133979=CARTESIAN_POINT('Ctrl Pts',(-20.7510988824047,1.9718336587144,-7.34034038852786));
#133980=CARTESIAN_POINT('Ctrl Pts',(-20.7143546234119,1.92458032026418,
-7.34339399104344));
#133981=CARTESIAN_POINT('Ctrl Pts',(-20.6974168159423,1.90150069016189,
-7.34487715139806));
#133982=CARTESIAN_POINT('Ctrl Pts',(-20.6569904945918,1.84307497164331,
-7.34861678929152));
#133983=CARTESIAN_POINT('Ctrl Pts',(-20.6343005404688,1.80720721579581,
-7.35090000409829));
#133984=CARTESIAN_POINT('Ctrl Pts',(-20.556610532312,1.67240022770003,-7.35943299964571));
#133985=CARTESIAN_POINT('Ctrl Pts',(-20.5110646580972,1.56843379141645,
-7.36595299644807));
#133986=CARTESIAN_POINT('Ctrl Pts',(-20.4671347665531,1.42792534268164,
-7.37426528765962));
#133987=CARTESIAN_POINT('Ctrl Pts',(-20.4580485041753,1.39508268472228,
-7.37617180250815));
#133988=CARTESIAN_POINT('Ctrl Pts',(-20.444003816196,1.33688302021406,-7.37945930259372));
#133989=CARTESIAN_POINT('Ctrl Pts',(-20.4385808188261,1.31165184878328,
-7.38085500811797));
#133990=CARTESIAN_POINT('Ctrl Pts',(-20.4307943588022,1.27041510178611,
-7.38307589604204));
#133991=CARTESIAN_POINT('Ctrl Pts',(-20.4280453875969,1.25448838415569,
-7.38391888361165));
#133992=CARTESIAN_POINT('Ctrl Pts',(-20.4223453296819,1.21805754009262,
-7.38581152273993));
#133993=CARTESIAN_POINT('Ctrl Pts',(-20.4195559395557,1.19753212131848,
-7.38685338534983));
#133994=CARTESIAN_POINT('Ctrl Pts',(-20.4104299899328,1.11848170660292,
-7.39079260141721));
#133995=CARTESIAN_POINT('Ctrl Pts',(-20.4070305032439,1.05966466419257,
-7.39357083336393));
#133996=CARTESIAN_POINT('Ctrl Pts',(-20.4069385286596,0.880834598077489,
-7.40190359308587));
#133997=CARTESIAN_POINT('Ctrl Pts',(-20.4208651202421,0.761285046035383,
-7.40735178265562));
#133998=CARTESIAN_POINT('Ctrl Pts',(-20.456251147579,0.611804087759982,
-7.41486317912615));
#133999=CARTESIAN_POINT('Ctrl Pts',(-20.4650733571445,0.579316786439152,
-7.41653669605546));
#134000=CARTESIAN_POINT('Ctrl Pts',(-20.4831985698121,0.52027889734565,
-7.41966729640507));
#134001=CARTESIAN_POINT('Ctrl Pts',(-20.4921788946539,0.49364412905756,
-7.42111389940446));
#134002=CARTESIAN_POINT('Ctrl Pts',(-20.5147072589758,0.432405270198859,
-7.42452558022747));
#134003=CARTESIAN_POINT('Ctrl Pts',(-20.5287875219883,0.398016755426616,
-7.42650669084278));
#134004=CARTESIAN_POINT('Ctrl Pts',(-20.5622016925475,0.324133344117312,
-7.4309089545039));
#134005=CARTESIAN_POINT('Ctrl Pts',(-20.5820101956731,0.284889258787158,
-7.43334252240344));
#134006=CARTESIAN_POINT('Ctrl Pts',(-20.6637999857438,0.138718718927442,
-7.44274379721125));
#134007=CARTESIAN_POINT('Ctrl Pts',(-20.7368651968496,0.0385327322597062,
-7.44994243427988));
#134008=CARTESIAN_POINT('Ctrl Pts',(-20.8356420516684,-0.0674786742026878,
-7.45781325123887));
#134009=CARTESIAN_POINT('Ctrl Pts',(-20.8505127447654,-0.0827890930495645,
-7.45895589166271));
#134010=CARTESIAN_POINT('Ctrl Pts',(-20.8772111809303,-0.109159602219511,
-7.46092680846376));
#134011=CARTESIAN_POINT('Ctrl Pts',(-20.88890283473,-0.120349814725715,
-7.46176344954001));
#134012=CARTESIAN_POINT('Ctrl Pts',(-20.9186285316735,-0.147917722788811,
-7.463827551843));
#134013=CARTESIAN_POINT('Ctrl Pts',(-20.9368778425727,-0.164055761895932,
-7.46503962438934));
#134014=CARTESIAN_POINT('Ctrl Pts',(-20.9794194152348,-0.199916990876399,
-7.46776144170377));
#134015=CARTESIAN_POINT('Ctrl Pts',(-21.0039449655319,-0.219347157900796,
-7.46925730064342));
#134016=CARTESIAN_POINT('Ctrl Pts',(-21.1004826953953,-0.291160989232186,
-7.4749373138021));
#134017=CARTESIAN_POINT('Ctrl Pts',(-21.1763866890077,-0.338020772946308,
-7.47898466000172));
#134018=CARTESIAN_POINT('Ctrl Pts',(-21.3098275538653,-0.40523052196344,
-7.48599160329124));
#134019=CARTESIAN_POINT('Ctrl Pts',(-21.3652891660476,-0.429197680117652,
-7.4888733748211));
#134020=CARTESIAN_POINT('Ctrl Pts',(-21.4509546007336,-0.460394340771098,
-7.49337696367223));
#134021=CARTESIAN_POINT('Ctrl Pts',(-21.4802080171293,-0.47006573856716,
-7.49492315699789));
#134022=CARTESIAN_POINT('Ctrl Pts',(-21.5373387453146,-0.487074128834837,
-7.49796824884198));
#134023=CARTESIAN_POINT('Ctrl Pts',(-21.56517082176,-0.494518364049688,
-7.49946308194927));
#134024=CARTESIAN_POINT('Ctrl Pts',(-21.6359399645652,-0.511339055157261,
-7.50329762925914));
#134025=CARTESIAN_POINT('Ctrl Pts',(-21.679097562047,-0.519668003638882,
-7.50566733676152));
#134026=CARTESIAN_POINT('Ctrl Pts',(-21.8309885556989,-0.542305271731283,
-7.51410992656871));
#134027=CARTESIAN_POINT('Ctrl Pts',(-21.9408365684424,-0.546861831239269,
-7.52042331398859));
#134028=CARTESIAN_POINT('Ctrl Pts',(-22.0958932938982,-0.53676888202514,
-7.52919847845896));
#134029=CARTESIAN_POINT('Ctrl Pts',(-22.1414098711509,-0.531765722993547,
-7.53175292081958));
#134030=CARTESIAN_POINT('Ctrl Pts',(-22.2069442455781,-0.521594851987155,
-7.53534307517313));
#134031=CARTESIAN_POINT('Ctrl Pts',(-22.2271853538923,-0.518038075534597,
-7.53643955310714));
#134032=CARTESIAN_POINT('Ctrl Pts',(-22.2634430446844,-0.51091741548571,
-7.53837419482939));
#134033=CARTESIAN_POINT('Ctrl Pts',(-22.279482987493,-0.507500896406463,
-7.53921887770395));
#134034=CARTESIAN_POINT('Ctrl Pts',(-22.3212785846377,-0.497899401140471,
-7.54139486311327));
#134035=CARTESIAN_POINT('Ctrl Pts',(-22.3469344129687,-0.491306011968331,
-7.54270631114527));
#134036=CARTESIAN_POINT('Ctrl Pts',(-22.4064675711735,-0.474360991844471,
-7.54571807414151));
#134037=CARTESIAN_POINT('Ctrl Pts',(-22.4401837662657,-0.463496861682668,
-7.54739969250235));
#134038=CARTESIAN_POINT('Ctrl Pts',(-22.5934123338542,-0.408232804815731,
-7.5550447355139));
#134039=CARTESIAN_POINT('Ctrl Pts',(-22.7075008109141,-0.350293314109797,
-7.56079061806701));
#134040=CARTESIAN_POINT('Ctrl Pts',(-22.8421048301696,-0.259451035805984,
-7.56870602408927));
#134041=CARTESIAN_POINT('Ctrl Pts',(-22.8703711059668,-0.238945014554024,
-7.57043691824677));
#134042=CARTESIAN_POINT('Ctrl Pts',(-22.920102126338,-0.200225593617103,
-7.5736245937489));
#134043=CARTESIAN_POINT('Ctrl Pts',(-22.9418105371418,-0.18234992364591,
-7.57506848978076));
#134044=CARTESIAN_POINT('Ctrl Pts',(-22.9900174503622,-0.140392028154088,
-7.57840233260295));
#134045=CARTESIAN_POINT('Ctrl Pts',(-23.0161897903214,-0.11596117382787,
-7.58030550933155));
#134046=CARTESIAN_POINT('Ctrl Pts',(-23.0707648472802,-0.061343877884279,
-7.58448345814335));
#134047=CARTESIAN_POINT('Ctrl Pts',(-23.0988486391809,-0.0308788126267512,
-7.58676806107228));
#134048=CARTESIAN_POINT('Ctrl Pts',(-23.1914998655966,0.0781224522796942,
-7.59476820294255));
#134049=CARTESIAN_POINT('Ctrl Pts',(-23.2495112925459,0.161877582365277,
-7.60064078391186));
#134050=CARTESIAN_POINT('Ctrl Pts',(-23.3171212636818,0.283590941131213,
-7.60842788628872));
#134051=CARTESIAN_POINT('Ctrl Pts',(-23.3341714951037,0.317114857107446,
-7.61049976047697));
#134052=CARTESIAN_POINT('Ctrl Pts',(-23.3575265775445,0.367512801829775,
-7.6134753723346));
#134053=CARTESIAN_POINT('Ctrl Pts',(-23.3647878991279,0.383926644308552,
-7.61442335329552));
#134054=CARTESIAN_POINT('Ctrl Pts',(-23.3785471106268,0.416555746178902,
-7.6162611971365));
#134055=CARTESIAN_POINT('Ctrl Pts',(-23.3850592199905,0.432761853411496,
-7.61715156911495));
#134056=CARTESIAN_POINT('Ctrl Pts',(-23.4036813872892,0.481480027026735,
-7.61977108682102));
#134057=CARTESIAN_POINT('Ctrl Pts',(-23.4149722010192,0.514295073396851,
-7.62146071096474));
#134058=CARTESIAN_POINT('Ctrl Pts',(-23.4567647225752,0.650527847038154,
-7.62827219534873));
#134059=CARTESIAN_POINT('Ctrl Pts',(-23.4774950477446,0.756623954743234,
-7.63312464040482));
#134060=CARTESIAN_POINT('Ctrl Pts',(-23.4909810007103,0.909055911904548,
-7.64031701852787));
#134061=CARTESIAN_POINT('Ctrl Pts',(-23.4929838445311,0.954243467532069,
-7.64247299936936));
#134062=CARTESIAN_POINT('Ctrl Pts',(-23.4929999234274,0.999451206005372,
-7.64468148481327));
#134063=CARTESIAN_POINT('Ctrl Pts',(-23.4929999238988,0.999452532970484,
-7.6446815496381));
#134064=CARTESIAN_POINT('Ctrl Pts',(-23.4930085114816,1.02365607183503,
-7.64586393984481));
#134065=CARTESIAN_POINT('Ctrl Pts',(-23.4924476138905,1.0478558850477,-7.64706073081155));
#134066=CARTESIAN_POINT('Ctrl Pts',(-23.4901694298798,1.09660371989079,
-7.64950686770363));
#134067=CARTESIAN_POINT('Ctrl Pts',(-23.4884337229621,1.12114349549346,
-7.65075638292366));
#134068=CARTESIAN_POINT('Ctrl Pts',(-23.4832437590197,1.17588730286728,
-7.6535890139563));
#134069=CARTESIAN_POINT('Ctrl Pts',(-23.4794820947881,1.20605126467252,
-7.65518079881767));
#134070=CARTESIAN_POINT('Ctrl Pts',(-23.4665063553662,1.28985996614385,
-7.65969496515285));
#134071=CARTESIAN_POINT('Ctrl Pts',(-23.4553420473108,1.34315417741164,
-7.66267255350303));
#134072=CARTESIAN_POINT('Ctrl Pts',(-23.4157813897991,1.49224118326177,
-7.67128030487612));
#134073=CARTESIAN_POINT('Ctrl Pts',(-23.3808725778652,1.58601920182374,
-7.67704365154786));
#134074=CARTESIAN_POINT('Ctrl Pts',(-23.32425325355,1.70224247422789,-7.68430571723315));
#134075=CARTESIAN_POINT('Ctrl Pts',(-23.310598428907,1.7283464552991,-7.68594353260486));
#134076=CARTESIAN_POINT('Ctrl Pts',(-23.284792819778,1.77441749754843,-7.68882747927395));
#134077=CARTESIAN_POINT('Ctrl Pts',(-23.2729198099333,1.79452980962327,
-7.69008406577255));
#134078=CARTESIAN_POINT('Ctrl Pts',(-23.2520823567405,1.82806442713746,
-7.69216539256959));
#134079=CARTESIAN_POINT('Ctrl Pts',(-23.2433564881602,1.84162830276682,
-7.69300271423055));
#134080=CARTESIAN_POINT('Ctrl Pts',(-23.2219454670272,1.87379082615475,
-7.69497760974999));
#134081=CARTESIAN_POINT('Ctrl Pts',(-23.2090633715712,1.89225287977395,
-7.69610371153933));
#134082=CARTESIAN_POINT('Ctrl Pts',(-23.151252659042,1.97135804848215,-7.70092488448967));
#134083=CARTESIAN_POINT('Ctrl Pts',(-23.1023102094883,2.02894476856537,
-7.70442786783079));
#134084=CARTESIAN_POINT('Ctrl Pts',(-23.001492262045,2.13131074214869,-7.71108294872847));
#134085=CARTESIAN_POINT('Ctrl Pts',(-22.9504701430702,2.17667288738263,
-7.71422942256887));
#134086=CARTESIAN_POINT('Ctrl Pts',(-22.8584396223527,2.24816808717301,
-7.71976799293735));
#134087=CARTESIAN_POINT('Ctrl Pts',(-22.8188924839979,2.27601390244584,
-7.72210897050593));
#134088=CARTESIAN_POINT('Ctrl Pts',(-22.753246906146,2.31776757601064,-7.72598093632391));
#134089=CARTESIAN_POINT('Ctrl Pts',(-22.7279417435769,2.33286288751146,
-7.72747011811387));
#134090=CARTESIAN_POINT('Ctrl Pts',(-22.6759548820214,2.36188969038298,
-7.73053054398033));
#134091=CARTESIAN_POINT('Ctrl Pts',(-22.649266790528,2.37578334592831,-7.73210219678114));
#134092=CARTESIAN_POINT('Ctrl Pts',(-22.574168254494,2.41212937179847,-7.73653122830441));
#134093=CARTESIAN_POINT('Ctrl Pts',(-22.5249765339493,2.43286305957033,
-7.73944094679471));
#134094=CARTESIAN_POINT('Ctrl Pts',(-22.3835381759353,2.48401977293374,
-7.74780833457134));
#134095=CARTESIAN_POINT('Ctrl Pts',(-22.289353304043,2.50834599267184,-7.7533942681113));
#134096=CARTESIAN_POINT('Ctrl Pts',(-22.1615663346598,2.52876930529932,
-7.76068186047944));
#134097=CARTESIAN_POINT('Ctrl Pts',(-22.129461962326,2.53286968825049,-7.76248705373911));
#134098=CARTESIAN_POINT('Ctrl Pts',(-22.0724061986856,2.53833958368692,
-7.76562597878474));
#134099=CARTESIAN_POINT('Ctrl Pts',(-22.0475057349244,2.54011840849329,
-7.76697264145341));
#134100=CARTESIAN_POINT('Ctrl Pts',(-22.006140838668,2.54206607692399,-7.76915980717778));
#134101=CARTESIAN_POINT('Ctrl Pts',(-21.9896987243607,2.54257695040143,
-7.77001561273912));
#134102=CARTESIAN_POINT('Ctrl Pts',(-21.9514280502855,2.54315366996898,
-7.77197565979465));
#134103=CARTESIAN_POINT('Ctrl Pts',(-21.9296009542589,2.54301952489229,
-7.7730705668631));
#134104=CARTESIAN_POINT('Ctrl Pts',(-21.8075920309032,2.53968007434948,
-7.77909694454067));
#134105=CARTESIAN_POINT('Ctrl Pts',(-21.7078978891598,2.52718199321523,
-7.78367936087284));
#134106=CARTESIAN_POINT('Ctrl Pts',(-21.5584628593292,2.49343615451053,
-7.79082067555691));
#134107=CARTESIAN_POINT('Ctrl Pts',(-21.5074480946691,2.47912147234658,
-7.79330682532593));
#134108=CARTESIAN_POINT('Ctrl Pts',(-21.4177380503691,2.44889150373347,
-7.79786184300392));
#134109=CARTESIAN_POINT('Ctrl Pts',(-21.3787630166346,2.43397257380083,
-7.79990510100624));
#134110=CARTESIAN_POINT('Ctrl Pts',(-21.3139820648928,2.4061151292695,-7.80344067170145));
#134111=CARTESIAN_POINT('Ctrl Pts',(-21.2878470936279,2.39399855237854,
-7.80490687943469));
#134112=CARTESIAN_POINT('Ctrl Pts',(-21.2332948943076,2.36682698487295,
-7.8080597344432));
#134113=CARTESIAN_POINT('Ctrl Pts',(-21.204978631849,2.35160096991859,-7.80975147477486));
#134114=CARTESIAN_POINT('Ctrl Pts',(-21.119245398269,2.30198811074357,-7.8150518172889));
#134115=CARTESIAN_POINT('Ctrl Pts',(-21.0635782815461,2.26474549338369,
-7.81875215631224));
#134116=CARTESIAN_POINT('Ctrl Pts',(-21.0105083757967,2.22401162108585,
-7.82252260735286));
#134117=CARTESIAN_POINT('',(-23.4929996000016,1.00121063888742,-7.60402754881385));
#134118=CARTESIAN_POINT('Ctrl Pts',(-21.0105083902185,2.22401163215526,
-7.78024815277603));
#134119=CARTESIAN_POINT('Ctrl Pts',(-21.0197419184587,2.23109883809076,
-7.7796053716493));
#134120=CARTESIAN_POINT('Ctrl Pts',(-21.0290571784149,2.23808274160231,
-7.77896644365765));
#134121=CARTESIAN_POINT('Ctrl Pts',(-21.0564551693885,2.25814325226005,
-7.77711683465143));
#134122=CARTESIAN_POINT('Ctrl Pts',(-21.0747425636672,2.27093325031787,
-7.77591920883034));
#134123=CARTESIAN_POINT('Ctrl Pts',(-21.1066760886153,2.29225087703121,
-7.77389918387178));
#134124=CARTESIAN_POINT('Ctrl Pts',(-21.1201883770866,2.30096896730836,
-7.77306624663121));
#134125=CARTESIAN_POINT('Ctrl Pts',(-21.1536653251659,2.32183432985019,
-7.77105410660961));
#134126=CARTESIAN_POINT('Ctrl Pts',(-21.1737736744045,2.33374199468929,
-7.76988830108668));
#134127=CARTESIAN_POINT('Ctrl Pts',(-21.2198207051163,2.35961557186169,
-7.76729699303873));
#134128=CARTESIAN_POINT('Ctrl Pts',(-21.245904612514,2.37330482217105,-7.76588339996987));
#134129=CARTESIAN_POINT('Ctrl Pts',(-21.3413995460949,2.41998555348903,
-7.76084830321388));
#134130=CARTESIAN_POINT('Ctrl Pts',(-21.4128598593125,2.44852845345996,
-7.75733619977407));
#134131=CARTESIAN_POINT('Ctrl Pts',(-21.5537504719334,2.49293636181643,
-7.75046189238699));
#134132=CARTESIAN_POINT('Ctrl Pts',(-21.6227336739363,2.50955898666401,
-7.74711726701255));
#134133=CARTESIAN_POINT('Ctrl Pts',(-21.7244611107527,2.52676935584913,
-7.74204961207007));
#134134=CARTESIAN_POINT('Ctrl Pts',(-21.7564710493216,2.53115604148476,
-7.74043680514408));
#134135=CARTESIAN_POINT('Ctrl Pts',(-21.8167641829495,2.53749782510377,
-7.73735346131916));
#134136=CARTESIAN_POINT('Ctrl Pts',(-21.8450095454325,2.53968445416299,
-7.73589048002731));
#134137=CARTESIAN_POINT('Ctrl Pts',(-21.9129133037364,2.54306410630991,
-7.73232374112381));
#134138=CARTESIAN_POINT('Ctrl Pts',(-21.9525873905057,2.54350743791063,
-7.73019902524178));
#134139=CARTESIAN_POINT('Ctrl Pts',(-22.0409683647097,2.54108751699568,
-7.72537519877531));
#134140=CARTESIAN_POINT('Ctrl Pts',(-22.0896108143746,2.53744407769253,
-7.72265837686186));
#134141=CARTESIAN_POINT('Ctrl Pts',(-22.2237099944816,2.52098301537759,
-7.71503710853011));
#134142=CARTESIAN_POINT('Ctrl Pts',(-22.3083873242692,2.50328470266827,
-7.71006781788095));
#134143=CARTESIAN_POINT('Ctrl Pts',(-22.4259304090191,2.46821574170422,
-7.70321968796503));
#134144=CARTESIAN_POINT('Ctrl Pts',(-22.4603470330766,2.45661026094603,
-7.70122256125562));
#134145=CARTESIAN_POINT('Ctrl Pts',(-22.5109493811257,2.43753278314046,
-7.69832874573481));
#134146=CARTESIAN_POINT('Ctrl Pts',(-22.5274659299164,2.4309779405036,-7.69739117791553));
#134147=CARTESIAN_POINT('Ctrl Pts',(-22.5602659327625,2.41730033281319,
-7.69554850763487));
#134148=CARTESIAN_POINT('Ctrl Pts',(-22.5765469386756,2.41017861599385,
-7.69464356527523));
#134149=CARTESIAN_POINT('Ctrl Pts',(-22.6258229610287,2.38760211544239,
-7.6919242610315));
#134150=CARTESIAN_POINT('Ctrl Pts',(-22.6583982163992,2.37125803393056,
-7.69015368986645));
#134151=CARTESIAN_POINT('Ctrl Pts',(-22.742773382217,2.32511409832406,-7.68556609088079));
#134152=CARTESIAN_POINT('Ctrl Pts',(-22.7934741572237,2.29343298809316,
-7.68280645716952));
#134153=CARTESIAN_POINT('Ctrl Pts',(-22.9129322814421,2.20876961904608,
-7.67602684285459));
#134154=CARTESIAN_POINT('Ctrl Pts',(-22.9793004999558,2.15278002644172,
-7.67200483924843));
#134155=CARTESIAN_POINT('Ctrl Pts',(-23.0653973436928,2.06675456468141,
-7.66607621203001));
#134156=CARTESIAN_POINT('Ctrl Pts',(-23.0893295966423,2.04115531288518,
-7.66434025154041));
#134157=CARTESIAN_POINT('Ctrl Pts',(-23.1308013119013,1.99365127050742,
-7.6611524413116));
#134158=CARTESIAN_POINT('Ctrl Pts',(-23.148654227675,1.97204038054973,-7.65971387821901));
#134159=CARTESIAN_POINT('Ctrl Pts',(-23.1877033287463,1.92205900344857,
-7.65640690763637));
#134160=CARTESIAN_POINT('Ctrl Pts',(-23.2085308171283,1.89342165939779,
-7.65452588400141));
#134161=CARTESIAN_POINT('Ctrl Pts',(-23.2511851465789,1.830318241846,-7.65040758639692));
#134162=CARTESIAN_POINT('Ctrl Pts',(-23.2726672903487,1.79565197934347,
-7.64816103474137));
#134163=CARTESIAN_POINT('Ctrl Pts',(-23.3406178280417,1.67562656014211,
-7.6404546928881));
#134164=CARTESIAN_POINT('Ctrl Pts',(-23.3803893676498,1.58674873226413,
-7.63485102634545));
#134165=CARTESIAN_POINT('Ctrl Pts',(-23.4244437981223,1.45660101062369,
-7.62713234020692));
#134166=CARTESIAN_POINT('Ctrl Pts',(-23.4358526985855,1.41798463828813,
-7.62490189634416));
#134167=CARTESIAN_POINT('Ctrl Pts',(-23.4504195209111,1.36049064100476,
-7.62170827403076));
#134168=CARTESIAN_POINT('Ctrl Pts',(-23.4547575886915,1.34193114230808,
-7.62069656021869));
#134169=CARTESIAN_POINT('Ctrl Pts',(-23.4622680333557,1.30688147646575,
-7.6188279000062));
#134170=CARTESIAN_POINT('Ctrl Pts',(-23.4655170783054,1.29041150155825,
-7.61796762642306));
#134171=CARTESIAN_POINT('Ctrl Pts',(-23.4738006666381,1.24448599846408,
-7.61561124648096));
#134172=CARTESIAN_POINT('Ctrl Pts',(-23.4782495619118,1.21493103208098,
-7.61414265623193));
#134173=CARTESIAN_POINT('Ctrl Pts',(-23.4892237504235,1.12419200102315,
-7.6097314109794));
#134174=CARTESIAN_POINT('Ctrl Pts',(-23.4929512956989,1.06273095523487,
-7.60687664523302));
#134175=CARTESIAN_POINT('Ctrl Pts',(-23.4929995464514,1.00121017463365,
-7.6040274338919));
#134176=CARTESIAN_POINT('Ctrl Pts',(-23.4929995460838,1.00121064316225,
-7.60402745559086));
#134177=CARTESIAN_POINT('Ctrl Pts',(-23.4930596419354,0.924616752090264,
-7.60048016335937));
#134178=CARTESIAN_POINT('Ctrl Pts',(-23.4874164958633,0.848124290790459,
-7.59694687164609));
#134179=CARTESIAN_POINT('Ctrl Pts',(-23.4697312634755,0.729556736793429,
-7.59120813810576));
#134180=CARTESIAN_POINT('Ctrl Pts',(-23.4615473628301,0.687035361430817,
-7.58909752211753));
#134181=CARTESIAN_POINT('Ctrl Pts',(-23.4449882882033,0.617009942846924,
-7.58550120388002));
#134182=CARTESIAN_POINT('Ctrl Pts',(-23.4376128968803,0.589294386240042,
-7.5840458793293));
#134183=CARTESIAN_POINT('Ctrl Pts',(-23.4207027905572,0.532201560820202,
-7.58097429083855));
#134184=CARTESIAN_POINT('Ctrl Pts',(-23.4110498168629,0.502872916424515,
-7.57935491829063));
#134185=CARTESIAN_POINT('Ctrl Pts',(-23.3795675010402,0.416079660239683,
-7.57443241543105));
#134186=CARTESIAN_POINT('Ctrl Pts',(-23.3551797296148,0.359613451613856,
-7.57105294541982));
#134187=CARTESIAN_POINT('Ctrl Pts',(-23.2879466423569,0.226404038537122,
-7.56268307598321));
#134188=CARTESIAN_POINT('Ctrl Pts',(-23.2417901228115,0.151572394266637,
-7.55763195629812));
#134189=CARTESIAN_POINT('Ctrl Pts',(-23.1710100165528,0.0560985072348075,
-7.55094334657079));
#134190=CARTESIAN_POINT('Ctrl Pts',(-23.1517446042031,0.0316893280978903,
-7.54921065594732));
#134191=CARTESIAN_POINT('Ctrl Pts',(-23.1161658143576,-0.0106899147818895,
-7.5461828076401));
#134192=CARTESIAN_POINT('Ctrl Pts',(-23.1001412057038,-0.0288887877254895,
-7.54487575978468));
#134193=CARTESIAN_POINT('Ctrl Pts',(-23.0727342685971,-0.0585734818121564,
-7.54274289611917));
#134194=CARTESIAN_POINT('Ctrl Pts',(-23.0615892832405,-0.0702707033213201,
-7.54190266586779));
#134195=CARTESIAN_POINT('Ctrl Pts',(-23.0352876493887,-0.0970213781877094,
-7.53998232383929));
#134196=CARTESIAN_POINT('Ctrl Pts',(-23.0199987346164,-0.111938837198471,
-7.53891124202531));
#134197=CARTESIAN_POINT('Ctrl Pts',(-22.9387089639375,-0.188023740955705,
-7.53341694542624));
#134198=CARTESIAN_POINT('Ctrl Pts',(-22.8677548878983,-0.243653730995503,
-7.52928309846972));
#134199=CARTESIAN_POINT('Ctrl Pts',(-22.7416118789101,-0.325845829355833,
-7.5223109031778));
#134200=CARTESIAN_POINT('Ctrl Pts',(-22.6889715804988,-0.355889789636206,
-7.5194987778821));
#134201=CARTESIAN_POINT('Ctrl Pts',(-22.5942224235777,-0.402806846620529,
-7.51445243134997));
#134202=CARTESIAN_POINT('Ctrl Pts',(-22.5528827945077,-0.421063509037571,
-7.51225599094274));
#134203=CARTESIAN_POINT('Ctrl Pts',(-22.483851918244,-0.447994515079917,
-7.50855925863481));
#134204=CARTESIAN_POINT('Ctrl Pts',(-22.4566108628926,-0.457748703528487,
-7.50709354417815));
#134205=CARTESIAN_POINT('Ctrl Pts',(-22.4001741632374,-0.476183945786,-7.50403567366152));
#134206=CARTESIAN_POINT('Ctrl Pts',(-22.3709635723084,-0.484777869885602,
-7.50244158152876));
#134207=CARTESIAN_POINT('Ctrl Pts',(-22.2860445492342,-0.507054171364554,
-7.49776978629059));
#134208=CARTESIAN_POINT('Ctrl Pts',(-22.2298065628716,-0.518501072663407,
-7.49462817013797));
#134209=CARTESIAN_POINT('Ctrl Pts',(-22.0816744032439,-0.54014336215404,
-7.48626170914276));
#134210=CARTESIAN_POINT('Ctrl Pts',(-21.9892694060592,-0.545262569073013,
-7.48094383685638));
#134211=CARTESIAN_POINT('Ctrl Pts',(-21.8652805946514,-0.540998683831635,
-7.47395724803011));
#134212=CARTESIAN_POINT('Ctrl Pts',(-21.833632184854,-0.538932429006236,
-7.47218857410449));
#134213=CARTESIAN_POINT('Ctrl Pts',(-21.7776066803395,-0.533536265839936,
-7.46910652516652));
#134214=CARTESIAN_POINT('Ctrl Pts',(-21.753203110952,-0.530595976630233,
-7.46778070139841));
#134215=CARTESIAN_POINT('Ctrl Pts',(-21.7128621329344,-0.524754583934963,
-7.46562774297288));
#134216=CARTESIAN_POINT('Ctrl Pts',(-21.6968827208267,-0.52218350221434,
-7.46478553566933));
#134217=CARTESIAN_POINT('Ctrl Pts',(-21.6601181541629,-0.515673070150711,
-7.46287333248927));
#134218=CARTESIAN_POINT('Ctrl Pts',(-21.6393685425915,-0.511556985091568,
-7.46181190417512));
#134219=CARTESIAN_POINT('Ctrl Pts',(-21.4977492012223,-0.48042446424839,
-7.4546513588263));
#134220=CARTESIAN_POINT('Ctrl Pts',(-21.3804193312323,-0.439364994380878,
-7.44910895372614));
#134221=CARTESIAN_POINT('Ctrl Pts',(-21.2133162502117,-0.357214475686276,
-7.44039005712894));
#134222=CARTESIAN_POINT('Ctrl Pts',(-21.159100921515,-0.326352839384203,
-7.43742060166912));
#134223=CARTESIAN_POINT('Ctrl Pts',(-21.0809655232895,-0.27537726297433,
-7.43281600339389));
#134224=CARTESIAN_POINT('Ctrl Pts',(-21.0555442391294,-0.257679137889282,
-7.43126282256385));
#134225=CARTESIAN_POINT('Ctrl Pts',(-21.0079164800827,-0.222346313620481,
-7.42823552736711));
#134226=CARTESIAN_POINT('Ctrl Pts',(-20.9856296930827,-0.204840921398022,
-7.42676652770496));
#134227=CARTESIAN_POINT('Ctrl Pts',(-20.9309961724158,-0.159441068286679,
-7.42302628650033));
#134228=CARTESIAN_POINT('Ctrl Pts',(-20.8993032888504,-0.130799881715213,
-7.42072719012891));
#134229=CARTESIAN_POINT('Ctrl Pts',(-20.7935830929418,-0.0269737837130934,
-7.41259657298036));
#134230=CARTESIAN_POINT('Ctrl Pts',(-20.7261072175214,0.0544535774880694,
-7.40654040341755));
#134231=CARTESIAN_POINT('Ctrl Pts',(-20.6464690772227,0.173511678049652,
-7.39842668985596));
#134232=CARTESIAN_POINT('Ctrl Pts',(-20.6266264646943,0.205671018122708,
-7.39630314709043));
#134233=CARTESIAN_POINT('Ctrl Pts',(-20.5943527970144,0.26255001077216,
-7.39269859444294));
#134234=CARTESIAN_POINT('Ctrl Pts',(-20.5813688297038,0.286935688463927,
-7.39119904248992));
#134235=CARTESIAN_POINT('Ctrl Pts',(-20.5616918804516,0.326411656098937,
-7.38885854109423));
#134236=CARTESIAN_POINT('Ctrl Pts',(-20.5545744222045,0.341282889580845,
-7.38799620917483));
#134237=CARTESIAN_POINT('Ctrl Pts',(-20.5394054038096,0.374326981356683,
-7.38612554047329));
#134238=CARTESIAN_POINT('Ctrl Pts',(-20.531464135058,0.392546370859086,
-7.38512285810854));
#134239=CARTESIAN_POINT('Ctrl Pts',(-20.5040987168699,0.458795644155141,
-7.38156277947558));
#134240=CARTESIAN_POINT('Ctrl Pts',(-20.4867431580902,0.507645615271635,
-7.37909756278097));
#134241=CARTESIAN_POINT('Ctrl Pts',(-20.4413405371832,0.659232453935692,
-7.37168556082397));
#134242=CARTESIAN_POINT('Ctrl Pts',(-20.4214344297855,0.764068975997816,
-7.3668630803487));
#134243=CARTESIAN_POINT('Ctrl Pts',(-20.4088304832659,0.91327570661631,
-7.3596948681011));
#134244=CARTESIAN_POINT('Ctrl Pts',(-20.4070037615243,0.956562532668586,
-7.35758308081218));
#134245=CARTESIAN_POINT('Ctrl Pts',(-20.4069975768245,1.02827379355278,
-7.35399898070112));
#134246=CARTESIAN_POINT('Ctrl Pts',(-20.4077795851932,1.05667405076351,
-7.35255750368066));
#134247=CARTESIAN_POINT('Ctrl Pts',(-20.4110421353416,1.11578425703944,
-7.34950458738404));
#134248=CARTESIAN_POINT('Ctrl Pts',(-20.4136593613833,1.1464737999966,-7.34788972301113));
#134249=CARTESIAN_POINT('Ctrl Pts',(-20.4241509379542,1.23729766619312,
-7.34301693987845));
#134250=CARTESIAN_POINT('Ctrl Pts',(-20.4346527686506,1.29706423016573,
-7.3396852899364));
#134251=CARTESIAN_POINT('Ctrl Pts',(-20.4751389248404,1.4677806731414,-7.32985087727042));
#134252=CARTESIAN_POINT('Ctrl Pts',(-20.5140225278048,1.57619581321561,
-7.32318230675));
#134253=CARTESIAN_POINT('Ctrl Pts',(-20.5764537348811,1.70352544961722,
-7.31537569807187));
#134254=CARTESIAN_POINT('Ctrl Pts',(-20.5889702902008,1.72744462915774,
-7.31391214165409));
#134255=CARTESIAN_POINT('Ctrl Pts',(-20.6100952404935,1.76535836747691,
-7.31161110467496));
#134256=CARTESIAN_POINT('Ctrl Pts',(-20.6183104045863,1.77956468469998,
-7.31075356003251));
#134257=CARTESIAN_POINT('Ctrl Pts',(-20.6371163776265,1.81092022924765,
-7.3088739979586));
#134258=CARTESIAN_POINT('Ctrl Pts',(-20.6478192327962,1.82799779439238,
-7.30785827798668));
#134259=CARTESIAN_POINT('Ctrl Pts',(-20.6923015762068,1.89597721645553,
-7.30382789631088));
#134260=CARTESIAN_POINT('Ctrl Pts',(-20.7287577906987,1.94506566056608,
-7.300945846947));
#134261=CARTESIAN_POINT('Ctrl Pts',(-20.840188010109,2.0778527740842,-7.29287114832312));
#134262=CARTESIAN_POINT('Ctrl Pts',(-20.921495780058,2.15568989360413,-7.28776554622509));
#134263=CARTESIAN_POINT('Ctrl Pts',(-21.0105083871506,2.22401162980051,
-7.28231522554091));
#134264=CARTESIAN_POINT('Origin',(-21.9500000210213,0.999999999999992,-4.89578827641128));
#134265=CARTESIAN_POINT('',(-21.010508379234,2.22401162372414,-6.7805154429392));
#134266=CARTESIAN_POINT('',(-21.0105469284169,2.2239496744092,-6.82271756118853));
#134267=CARTESIAN_POINT('',(-21.0105083758276,2.22401162110953,-4.89578827641128));
#134268=CARTESIAN_POINT('',(-23.4934928036937,1.00049669217445,-7.14664973949428));
#134269=CARTESIAN_POINT('Ctrl Pts',(-21.0105469284169,2.2239496744092,-6.82271756118853));
#134270=CARTESIAN_POINT('Ctrl Pts',(-20.9646994282928,2.18892255442207,
-6.82591631418018));
#134271=CARTESIAN_POINT('Ctrl Pts',(-20.9208499519301,2.15135842051501,
-6.82913507944199));
#134272=CARTESIAN_POINT('Ctrl Pts',(-20.8792997883414,2.11149720384009,
-6.83231398513469));
#134273=CARTESIAN_POINT('Ctrl Pts',(-20.8402565375944,2.07404099805647,
-6.83530109279786));
#134274=CARTESIAN_POINT('Ctrl Pts',(-20.8032432753279,2.03455597882077,
-6.838252529876));
#134275=CARTESIAN_POINT('Ctrl Pts',(-20.7684942010589,1.99327442215102,
-6.84110588764712));
#134276=CARTESIAN_POINT('Ctrl Pts',(-20.7662034820682,1.99055307063837,
-6.8412939859194));
#134277=CARTESIAN_POINT('Ctrl Pts',(-20.7639225844739,1.98782390653865,
-6.84148165797097));
#134278=CARTESIAN_POINT('Ctrl Pts',(-20.7616515677829,1.98508699390259,
-6.84166888592334));
#134279=CARTESIAN_POINT('Ctrl Pts',(-20.7545421303374,1.97651906516054,
-6.84225500465191));
#134280=CARTESIAN_POINT('Ctrl Pts',(-20.7475296520023,1.96787539299453,
-6.8428367407542));
#134281=CARTESIAN_POINT('Ctrl Pts',(-20.7406160611608,1.95915820811847,
-6.84341351093467));
#134282=CARTESIAN_POINT('Ctrl Pts',(-20.740605526905,1.95914492572187,-6.84341438976085));
#134283=CARTESIAN_POINT('Ctrl Pts',(-20.740594992867,1.95913164314035,-6.84341526857625));
#134284=CARTESIAN_POINT('Ctrl Pts',(-20.7405844590468,1.9591183603739,-6.84341614738087));
#134285=CARTESIAN_POINT('Ctrl Pts',(-20.7081586236352,1.91823055425673,
-6.84612133631287));
#134286=CARTESIAN_POINT('Ctrl Pts',(-20.6777965480067,1.87558611519414,
-6.84872437076239));
#134287=CARTESIAN_POINT('Ctrl Pts',(-20.6496700737443,1.83143437663984,
-6.85127674573291));
#134288=CARTESIAN_POINT('Ctrl Pts',(-20.6468302132197,1.82697648482437,
-6.8515344527194));
#134289=CARTESIAN_POINT('Ctrl Pts',(-20.6440131428578,1.82250327075007,
-6.8517916432608));
#134290=CARTESIAN_POINT('Ctrl Pts',(-20.6412190384027,1.81801502047479,
-6.85204837036131));
#134291=CARTESIAN_POINT('Ctrl Pts',(-20.6107934927671,1.7691415922377,-6.85484392157923));
#134292=CARTESIAN_POINT('Ctrl Pts',(-20.5830908180337,1.71847954347281,
-6.8575852240484));
#134293=CARTESIAN_POINT('Ctrl Pts',(-20.5582897697873,1.6663800599524,-6.8603324033392));
#134294=CARTESIAN_POINT('Ctrl Pts',(-20.5335117049533,1.61432885761366,
-6.86307703678782));
#134295=CARTESIAN_POINT('Ctrl Pts',(-20.5116295026666,1.56084318426877,
-6.86582797361469));
#134296=CARTESIAN_POINT('Ctrl Pts',(-20.4927783481858,1.5062830339907,-6.86862837225068));
#134297=CARTESIAN_POINT('Ctrl Pts',(-20.4739375418887,1.45175283405081,
-6.87142723363127));
#134298=CARTESIAN_POINT('Ctrl Pts',(-20.4581242020584,1.39614948283325,
-6.87427573809505));
#134299=CARTESIAN_POINT('Ctrl Pts',(-20.4454350789399,1.33983891146091,
-6.87719520358442));
#134300=CARTESIAN_POINT('Ctrl Pts',(-20.4327481282639,1.2835379807448,-6.88011416924645));
#134301=CARTESIAN_POINT('Ctrl Pts',(-20.4231842050893,1.22653013640785,
-6.88310416118364));
#134302=CARTESIAN_POINT('Ctrl Pts',(-20.4168045934839,1.16918611131505,
-6.88616231760585));
#134303=CARTESIAN_POINT('Ctrl Pts',(-20.4104194018568,1.11179192942249,
-6.8892231488898));
#134304=CARTESIAN_POINT('Ctrl Pts',(-20.4072241165769,1.05406098363771,
-6.89235222984401));
#134305=CARTESIAN_POINT('Ctrl Pts',(-20.4072454428099,0.996369467827194,
-6.89552205244813));
#134306=CARTESIAN_POINT('Ctrl Pts',(-20.4072667787057,0.938651812469348,
-6.89869331127257));
#134307=CARTESIAN_POINT('Ctrl Pts',(-20.410507835263,0.880973587345166,
-6.90190515928954));
#134308=CARTESIAN_POINT('Ctrl Pts',(-20.4169590402013,0.823716245000039,
-6.90510703379557));
#134309=CARTESIAN_POINT('Ctrl Pts',(-20.4234214586073,0.766359378089729,
-6.90831447379162));
#134310=CARTESIAN_POINT('Ctrl Pts',(-20.433105639191,0.709424852376949,
-6.91151149706294));
#134311=CARTESIAN_POINT('Ctrl Pts',(-20.4459607908488,0.653301304988339,
-6.91462858291627));
#134312=CARTESIAN_POINT('Ctrl Pts',(-20.4543194584833,0.616808691631712,
-6.91665537227897));
#134313=CARTESIAN_POINT('Ctrl Pts',(-20.4640179374223,0.580659075490424,
-6.91864797005291));
#134314=CARTESIAN_POINT('Ctrl Pts',(-20.4750312470688,0.544960268935724,
-6.92058466143602));
#134315=CARTESIAN_POINT('Ctrl Pts',(-20.4750362446744,0.544944069577026,
-6.92058554026535));
#134316=CARTESIAN_POINT('Ctrl Pts',(-20.4750412425556,0.544927870293381,
-6.9205864190839));
#134317=CARTESIAN_POINT('Ctrl Pts',(-20.4750462407125,0.544911671084798,
-6.92058729789167));
#134318=CARTESIAN_POINT('Ctrl Pts',(-20.4904318029095,0.495046503635593,
-6.92329248539754));
#134319=CARTESIAN_POINT('Ctrl Pts',(-20.5084332001617,0.445890056417994,
-6.92589551891448));
#134320=CARTESIAN_POINT('Ctrl Pts',(-20.5289419697622,0.397725053238161,
-6.92844789334448));
#134321=CARTESIAN_POINT('Ctrl Pts',(-20.5310126811773,0.392861971549898,
-6.92870559924156));
#134322=CARTESIAN_POINT('Ctrl Pts',(-20.5331089172014,0.388009021327957,
-6.92896278870169));
#134323=CARTESIAN_POINT('Ctrl Pts',(-20.5352305412919,0.383166509278513,
-6.92921951472834));
#134324=CARTESIAN_POINT('Ctrl Pts',(-20.5583334033085,0.330435260516698,
-6.93201506460749));
#134325=CARTESIAN_POINT('Ctrl Pts',(-20.58445120499,0.278938245314851,-6.93475636620834));
#134326=CARTESIAN_POINT('Ctrl Pts',(-20.6133953906851,0.229021486521721,
-6.93750354492877));
#134327=CARTESIAN_POINT('Ctrl Pts',(-20.6423127544647,0.179150984448229,
-6.94024817790147));
#134328=CARTESIAN_POINT('Ctrl Pts',(-20.674050798609,0.130857661063998,
-6.94299911455059));
#134329=CARTESIAN_POINT('Ctrl Pts',(-20.7083890639754,0.0844565855523038,
-6.94579951316334));
#134330=CARTESIAN_POINT('Ctrl Pts',(-20.742708480812,0.0380809799369405,
-6.94859837461641));
#134331=CARTESIAN_POINT('Ctrl Pts',(-20.7796250004785,-0.0064045817375827,
-6.95144687931098));
#134332=CARTESIAN_POINT('Ctrl Pts',(-20.8188915324266,-0.0487133722867088,
-6.95436634506362));
#134333=CARTESIAN_POINT('Ctrl Pts',(-20.8581513430867,-0.0910149208016234,
-6.95728531108864));
#134334=CARTESIAN_POINT('Ctrl Pts',(-20.8997602408799,-0.13114050550213,
-6.96027530342673));
#134335=CARTESIAN_POINT('Ctrl Pts',(-20.9434471190817,-0.168829934658833,
-6.96333346016748));
#134336=CARTESIAN_POINT('Ctrl Pts',(-20.9871722109337,-0.206552331395789,
-6.96639429192958));
#134337=CARTESIAN_POINT('Ctrl Pts',(-21.0329789281761,-0.241834287798403,
-6.96952337328719));
#134338=CARTESIAN_POINT('Ctrl Pts',(-21.0805721059298,-0.274441042978287,
-6.97269319608993));
#134339=CARTESIAN_POINT('Ctrl Pts',(-21.1281868491517,-0.307062572963616,
-6.97586445520593));
#134340=CARTESIAN_POINT('Ctrl Pts',(-21.1775898109862,-0.337006337150968,
-6.97907630331255));
#134341=CARTESIAN_POINT('Ctrl Pts',(-21.2284609747694,-0.364064520778986,
-6.98227817755357));
#134342=CARTESIAN_POINT('Ctrl Pts',(-21.2794205649908,-0.391169738102013,
-6.98548561742969));
#134343=CARTESIAN_POINT('Ctrl Pts',(-21.331853722017,-0.415378971384698,
-6.98868264022486));
#134344=CARTESIAN_POINT('Ctrl Pts',(-21.3854111946562,-0.436514338276396,
-6.99179972505387));
#134345=CARTESIAN_POINT('Ctrl Pts',(-21.4202352931566,-0.450256960215189,
-6.99382651354427));
#134346=CARTESIAN_POINT('Ctrl Pts',(-21.4555341619196,-0.462700608224986,
-6.9958191102204));
#134347=CARTESIAN_POINT('Ctrl Pts',(-21.491204756158,-0.473804917728884,
-6.99775580022609));
#134348=CARTESIAN_POINT('Ctrl Pts',(-21.4912209426116,-0.473809956596179,
-6.99775667904921));
#134349=CARTESIAN_POINT('Ctrl Pts',(-21.4912371291592,-0.47381499519367,
-6.99775755786155));
#134350=CARTESIAN_POINT('Ctrl Pts',(-21.4912533158008,-0.473820033521343,
-6.99775843666311));
#134351=CARTESIAN_POINT('Ctrl Pts',(-21.5410800807606,-0.489329338961987,
-7.00046362034064));
#134352=CARTESIAN_POINT('Ctrl Pts',(-21.5918015719565,-0.502280458528975,
-7.00306664967207));
#134353=CARTESIAN_POINT('Ctrl Pts',(-21.6431232786224,-0.512602967705018,
-7.00561901926318));
#134354=CARTESIAN_POINT('Ctrl Pts',(-21.6483051918672,-0.513645223516332,
-7.00587673005749));
#134355=CARTESIAN_POINT('Ctrl Pts',(-21.6534931835026,-0.514660697509918,
-7.0061339243866));
#134356=CARTESIAN_POINT('Ctrl Pts',(-21.6586869233386,-0.515649328854675,
-7.00639065525699));
#134357=CARTESIAN_POINT('Ctrl Pts',(-21.7152416978683,-0.526414562493791,
-7.00918620469696));
#134358=CARTESIAN_POINT('Ctrl Pts',(-21.7724834763618,-0.533995261557184,
-7.01192750496353));
#134359=CARTESIAN_POINT('Ctrl Pts',(-21.8300202479235,-0.53835126258365,
-7.01467468168719));
#134360=CARTESIAN_POINT('Ctrl Pts',(-21.8875036999948,-0.542703226891542,
-7.01741931259434));
#134361=CARTESIAN_POINT('Ctrl Pts',(-21.9452814580753,-0.543836937871541,
-7.02017024652085));
#134362=CARTESIAN_POINT('Ctrl Pts',(-22.0029689990605,-0.541756048795133,
-7.0229706421471));
#134363=CARTESIAN_POINT('Ctrl Pts',(-22.0606248733005,-0.539676301992831,
-7.02576950053649));
#134364=CARTESIAN_POINT('Ctrl Pts',(-22.1181905847057,-0.534385773536387,
-7.02861800190396));
#134365=CARTESIAN_POINT('Ctrl Pts',(-22.1752899253371,-0.525926108334006,
-7.03153746456503));
#134366=CARTESIAN_POINT('Ctrl Pts',(-22.2323794904752,-0.51746789143909,
-7.03445642740968));
#134367=CARTESIAN_POINT('Ctrl Pts',(-22.2890028275311,-0.505841757544152,
-7.03744641680038));
#134368=CARTESIAN_POINT('Ctrl Pts',(-22.3447920326749,-0.491124164652751,
-7.04050457139828));
#134369=CARTESIAN_POINT('Ctrl Pts',(-22.4006300344293,-0.476393698865109,
-7.04356540084301));
#134370=CARTESIAN_POINT('Ctrl Pts',(-22.4556324317036,-0.458566345186209,
-7.0466944806829));
#134371=CARTESIAN_POINT('Ctrl Pts',(-22.509438690026,-0.437752784647632,
-7.0498643033953));
#134372=CARTESIAN_POINT('Ctrl Pts',(-22.563269327466,-0.416929793677423,
-7.05303556232504));
#134373=CARTESIAN_POINT('Ctrl Pts',(-22.6159027050888,-0.393117695772129,
-7.05624741167359));
#134374=CARTESIAN_POINT('Ctrl Pts',(-22.6669864586967,-0.366462906402016,
-7.05944928924691));
#134375=CARTESIAN_POINT('Ctrl Pts',(-22.7181590051619,-0.339761786158799,
-7.06265673226596));
#134376=CARTESIAN_POINT('Ctrl Pts',(-22.7677763813216,-0.310207666983498,
-7.06585376030648));
#134377=CARTESIAN_POINT('Ctrl Pts',(-22.8154943778053,-0.277988002117594,
-7.06897085315136));
#134378=CARTESIAN_POINT('Ctrl Pts',(-22.8465210788424,-0.257038465612008,
-7.07099761694971));
#134379=CARTESIAN_POINT('Ctrl Pts',(-22.8767449536752,-0.234962827962764,
-7.07299019111136));
#134380=CARTESIAN_POINT('Ctrl Pts',(-22.9060744440312,-0.211823246532039,
-7.07492686191659));
#134381=CARTESIAN_POINT('Ctrl Pts',(-22.9060877521632,-0.21181274704497,
-7.07492774067277));
#134382=CARTESIAN_POINT('Ctrl Pts',(-22.9061010601267,-0.211802247327223,
-7.0749286194182));
#134383=CARTESIAN_POINT('Ctrl Pts',(-22.9061143679217,-0.211791747378802,
-7.07492949815289));
#134384=CARTESIAN_POINT('Ctrl Pts',(-22.9468357822309,-0.179662251027165,
-7.07761839737488));
#134385=CARTESIAN_POINT('Ctrl Pts',(-22.9859801592963,-0.145368599613194,
-7.08020673534755));
#134386=CARTESIAN_POINT('Ctrl Pts',(-23.0233229641384,-0.10911017788726,
-7.08274491630824));
#134387=CARTESIAN_POINT('Ctrl Pts',(-23.0275410591066,-0.105014570530441,
-7.0830316191519));
#134388=CARTESIAN_POINT('Ctrl Pts',(-23.0317361566911,-0.100893948133087,
-7.083317682039));
#134389=CARTESIAN_POINT('Ctrl Pts',(-23.0359079259895,-0.0967486390692106,
-7.08360317761281));
#134390=CARTESIAN_POINT('Ctrl Pts',(-23.0763795485599,-0.0565337154069281,
-7.08637285836026));
#134391=CARTESIAN_POINT('Ctrl Pts',(-23.1146571956832,-0.0139898798970523,
-7.08908982186985));
#134392=CARTESIAN_POINT('Ctrl Pts',(-23.150488725235,0.0305884411469265,
-7.09181244443254));
#134393=CARTESIAN_POINT('Ctrl Pts',(-23.1862876935111,0.0751262524214138,
-7.09453259285961));
#134394=CARTESIAN_POINT('Ctrl Pts',(-23.2196452613176,0.121694460344611,
-7.09725881554214));
#134395=CARTESIAN_POINT('Ctrl Pts',(-23.2503495102397,0.169979309385704,
-7.10003316983043));
#134396=CARTESIAN_POINT('Ctrl Pts',(-23.2810380611888,0.218239472128002,
-7.10280610569161));
#134397=CARTESIAN_POINT('Ctrl Pts',(-23.3090761954244,0.268214298768575,
-7.10562735425302));
#134398=CARTESIAN_POINT('Ctrl Pts',(-23.3342883246752,0.319574916103118,
-7.10851790109925));
#134399=CARTESIAN_POINT('Ctrl Pts',(-23.3602550446221,0.372472739740242,
-7.11149496105729));
#134400=CARTESIAN_POINT('Ctrl Pts',(-23.3832239786204,0.426840488413619,
-7.11454575062313));
#134401=CARTESIAN_POINT('Ctrl Pts',(-23.4030409202316,0.482304364683225,
-7.11766728314441));
#134402=CARTESIAN_POINT('Ctrl Pts',(-23.4222963531123,0.536196684081849,
-7.12070036772061));
#134403=CARTESIAN_POINT('Ctrl Pts',(-23.4385760267113,0.591123798865315,
-7.12380008299715));
#134404=CARTESIAN_POINT('Ctrl Pts',(-23.4517724941886,0.646730648522823,
-7.12693955632812));
#134405=CARTESIAN_POINT('Ctrl Pts',(-23.4655461960298,0.704769829752706,
-7.13021635518913));
#134406=CARTESIAN_POINT('Ctrl Pts',(-23.4759605798014,0.763549655735676,
-7.13353642047766));
#134407=CARTESIAN_POINT('Ctrl Pts',(-23.4829341020971,0.822652425744619,
-7.13684359595235));
#134408=CARTESIAN_POINT('Ctrl Pts',(-23.4894646191262,0.878000588358255,
-7.13994067728945));
#134409=CARTESIAN_POINT('Ctrl Pts',(-23.4929774206621,0.933632566162483,
-7.14302600958895));
#134410=CARTESIAN_POINT('Ctrl Pts',(-23.4934429988996,0.989191194661555,
-7.14603647098282));
#134411=CARTESIAN_POINT('Ctrl Pts',(-23.4934745819443,0.992960079256549,
-7.14624068915519));
#134412=CARTESIAN_POINT('Ctrl Pts',(-23.4934921520323,0.996728643780493,
-7.14644456279066));
#134413=CARTESIAN_POINT('Ctrl Pts',(-23.4934957039329,1.00049678448525,
-7.14664807218481));
#134414=CARTESIAN_POINT('Ctrl Pts',(-23.4929999460485,1.00048100516412,
-7.1469330768822));
#134415=CARTESIAN_POINT('Ctrl Pts',(-23.492995606971,1.01440018264177,-7.14769520777935));
#134416=CARTESIAN_POINT('Ctrl Pts',(-23.4928029234977,1.02831911176174,
-7.14845097177061));
#134417=CARTESIAN_POINT('Ctrl Pts',(-23.4920747206752,1.05491373269753,
-7.14988057379478));
#134418=CARTESIAN_POINT('Ctrl Pts',(-23.4915711760172,1.06758912955807,
-7.15055567525103));
#134419=CARTESIAN_POINT('Ctrl Pts',(-23.4901195877529,1.09545912419696,
-7.15202419674145));
#134420=CARTESIAN_POINT('Ctrl Pts',(-23.4891029406518,1.11064793043558,
-7.15281367016478));
#134421=CARTESIAN_POINT('Ctrl Pts',(-23.4860264450462,1.14825076246317,
-7.15474174833385));
#134422=CARTESIAN_POINT('Ctrl Pts',(-23.4837007584413,1.17063882517362,
-7.15586742123826));
#134423=CARTESIAN_POINT('Ctrl Pts',(-23.4718381460451,1.2647487847365,-7.16053380107808));
#134424=CARTESIAN_POINT('Ctrl Pts',(-23.4577523504494,1.33580899914792,
-7.16389923987488));
#134425=CARTESIAN_POINT('Ctrl Pts',(-23.4136240420131,1.49777028144667,
-7.17167745885749));
#134426=CARTESIAN_POINT('Ctrl Pts',(-23.3800166044622,1.58738566658417,
-7.17607379939565));
#134427=CARTESIAN_POINT('Ctrl Pts',(-23.3225703197009,1.70583732246154,
-7.18246826192759));
#134428=CARTESIAN_POINT('Ctrl Pts',(-23.3056601762985,1.73779458812649,
-7.18425462770703));
#134429=CARTESIAN_POINT('Ctrl Pts',(-23.273650854959,1.79346428721037,-7.18749456285743));
#134430=CARTESIAN_POINT('Ctrl Pts',(-23.2589964753055,1.8174137632315,-7.18893267095306));
#134431=CARTESIAN_POINT('Ctrl Pts',(-23.2249186609308,1.86983830929628,
-7.19218663482361));
#134432=CARTESIAN_POINT('Ctrl Pts',(-23.2051784341818,1.89808860119427,
-7.19401318830177));
#134433=CARTESIAN_POINT('Ctrl Pts',(-23.1404516046374,1.98441242923143,
-7.1998321920315));
#134434=CARTESIAN_POINT('Ctrl Pts',(-23.0922582773881,2.03994570306167,
-7.20393429709599));
#134435=CARTESIAN_POINT('Ctrl Pts',(-22.9748421830628,2.15719689916491,
-7.21334160530327));
#134436=CARTESIAN_POINT('Ctrl Pts',(-22.9036391416837,2.21654403609204,
-7.21866748139473));
#134437=CARTESIAN_POINT('Ctrl Pts',(-22.8064356547726,2.28375458395037,
-7.22515481445023));
#134438=CARTESIAN_POINT('Ctrl Pts',(-22.784961263876,2.29782421345522,-7.22654288378816));
#134439=CARTESIAN_POINT('Ctrl Pts',(-22.7493022659349,2.31993568488509,
-7.22876294875351));
#134440=CARTESIAN_POINT('Ctrl Pts',(-22.7353244335586,2.32829963880074,
-7.22961224423531));
#134441=CARTESIAN_POINT('Ctrl Pts',(-22.7031155255575,2.34688630745489,
-7.23152007551862));
#134442=CARTESIAN_POINT('Ctrl Pts',(-22.6848047304287,2.35696271424021,
-7.23257068044111));
#134443=CARTESIAN_POINT('Ctrl Pts',(-22.5692719180702,2.41751559109791,
-7.23902368287473));
#134444=CARTESIAN_POINT('Ctrl Pts',(-22.4671012880312,2.45789545795415,
-7.24398258813654));
#134445=CARTESIAN_POINT('Ctrl Pts',(-22.3121948561576,2.50076041021326,
-7.25145546034124));
#134446=CARTESIAN_POINT('Ctrl Pts',(-22.2622361565879,2.51194416002773,
-7.25385577103448));
#134447=CARTESIAN_POINT('Ctrl Pts',(-22.1715308460596,2.52756148926621,
-7.25828116903142));
#134448=CARTESIAN_POINT('Ctrl Pts',(-22.1309882027902,2.53289365621636,
-7.26028259981875));
#134449=CARTESIAN_POINT('Ctrl Pts',(-22.0619594124097,2.53919558030227,
-7.26375649074289));
#134450=CARTESIAN_POINT('Ctrl Pts',(-22.0335705239765,2.54099765733307,
-7.26520384315705));
#134451=CARTESIAN_POINT('Ctrl Pts',(-21.9734078333471,2.54314933590617,
-7.26831712319099));
#134452=CARTESIAN_POINT('Ctrl Pts',(-21.9416406956213,2.54330416067235,
-7.26998812350956));
#134453=CARTESIAN_POINT('Ctrl Pts',(-21.8468753336334,2.54084009038898,
-7.2750585036591));
#134454=CARTESIAN_POINT('Ctrl Pts',(-21.7840232013831,2.53534143395902,
-7.27853717554386));
#134455=CARTESIAN_POINT('Ctrl Pts',(-21.6243468563648,2.51145177189216,
-7.28761690548862));
#134456=CARTESIAN_POINT('Ctrl Pts',(-21.5286253330284,2.48760858816982,
-7.29330251109865));
#134457=CARTESIAN_POINT('Ctrl Pts',(-21.4045065326495,2.44374147697707,
-7.3006251062374));
#134458=CARTESIAN_POINT('Ctrl Pts',(-21.3735484677153,2.43166213524614,
-7.30244526827081));
#134459=CARTESIAN_POINT('Ctrl Pts',(-21.3270981830507,2.41178665936046,
-7.30514250636572));
#134460=CARTESIAN_POINT('Ctrl Pts',(-21.3113081209796,2.40471385140882,
-7.30605323168097));
#134461=CARTESIAN_POINT('Ctrl Pts',(-21.2790674065393,2.38961623386901,
-7.30789520428164));
#134462=CARTESIAN_POINT('Ctrl Pts',(-21.2626341129214,2.38156144162985,
-7.30882479588518));
#134463=CARTESIAN_POINT('Ctrl Pts',(-21.2105634331301,2.35487978438863,
-7.31175213004992));
#134464=CARTESIAN_POINT('Ctrl Pts',(-21.175507583218,2.33515076760792,-7.31369539834519));
#134465=CARTESIAN_POINT('Ctrl Pts',(-21.0961406510116,2.2863048176587,-7.31811707110993));
#134466=CARTESIAN_POINT('Ctrl Pts',(-21.0525001934093,2.25624249647932,
-7.32056604511031));
#134467=CARTESIAN_POINT('Ctrl Pts',(-21.0105083124886,2.22401157249359,
-7.32301699234766));
#134468=CARTESIAN_POINT('',(-23.4929995837554,0.998856457160122,-7.10475651497821));
#134469=CARTESIAN_POINT('Ctrl Pts',(-21.0105083871506,2.22401162980051,
-7.28231522554091));
#134470=CARTESIAN_POINT('Ctrl Pts',(-21.0154433030097,2.22779943054572,
-7.2820130562768));
#134471=CARTESIAN_POINT('Ctrl Pts',(-21.0204019059921,2.23155798536614,
-7.28170992437689));
#134472=CARTESIAN_POINT('Ctrl Pts',(-21.0524692318098,2.25556047488597,
-7.27975230871523));
#134473=CARTESIAN_POINT('Ctrl Pts',(-21.0802126029924,2.27493657437935,
-7.27807089094534));
#134474=CARTESIAN_POINT('Ctrl Pts',(-21.1320938352773,2.3086886945479,-7.27493466288154));
#134475=CARTESIAN_POINT('Ctrl Pts',(-21.1560305371592,2.32334763317577,
-7.27349072591619));
#134476=CARTESIAN_POINT('Ctrl Pts',(-21.2122677539476,2.35571236830967,
-7.27009975274404));
#134477=CARTESIAN_POINT('Ctrl Pts',(-21.2448281257554,2.37293016328562,
-7.26813730194881));
#134478=CARTESIAN_POINT('Ctrl Pts',(-21.3169976092341,2.40784818654129,
-7.26378785011317));
#134479=CARTESIAN_POINT('Ctrl Pts',(-21.3567999017545,2.42507606764693,
-7.26138903369756));
#134480=CARTESIAN_POINT('Ctrl Pts',(-21.5080480798264,2.48310656762016,
-7.25230379096701));
#134481=CARTESIAN_POINT('Ctrl Pts',(-21.6233510767689,2.51268840343621,
-7.24540369428604));
#134482=CARTESIAN_POINT('Ctrl Pts',(-21.7651606672024,2.53208449585394,
-7.23756759266639));
#134483=CARTESIAN_POINT('Ctrl Pts',(-21.7894961107612,2.53482478079956,
-7.23624690026639));
#134484=CARTESIAN_POINT('Ctrl Pts',(-21.8299994154273,2.53841167427614,
-7.23409950048903));
#134485=CARTESIAN_POINT('Ctrl Pts',(-21.8461326030543,2.53958508900774,
-7.23325789768662));
#134486=CARTESIAN_POINT('Ctrl Pts',(-21.8838441270495,2.54173239551484,
-7.23132362071633));
#134487=CARTESIAN_POINT('Ctrl Pts',(-21.9054294949286,2.54250735399395,
-7.23024045598921));
#134488=CARTESIAN_POINT('Ctrl Pts',(-21.9533154410427,2.54322044730049,
-7.22787733247796));
#134489=CARTESIAN_POINT('Ctrl Pts',(-21.9796126886395,2.54293990217794,
-7.22660616669071));
#134490=CARTESIAN_POINT('Ctrl Pts',(-22.0657856888371,2.53981647523319,
-7.22249340032146));
#134491=CARTESIAN_POINT('Ctrl Pts',(-22.1255053989186,2.53415758684263,
-7.21972515361034));
#134492=CARTESIAN_POINT('Ctrl Pts',(-22.2701556811391,2.5118918462487,-7.21294916558321));
#134493=CARTESIAN_POINT('Ctrl Pts',(-22.3543061852121,2.49159373334547,
-7.20893914798103));
#134494=CARTESIAN_POINT('Ctrl Pts',(-22.4695614278901,2.45331776208942,
-7.20302379902626));
#134495=CARTESIAN_POINT('Ctrl Pts',(-22.5024250381675,2.44114640207076,
-7.20128788444688));
#134496=CARTESIAN_POINT('Ctrl Pts',(-22.5607741855221,2.41724700131708,
-7.19810053903254));
#134497=CARTESIAN_POINT('Ctrl Pts',(-22.586408546388,2.40592254562723,-7.19666241153334));
#134498=CARTESIAN_POINT('Ctrl Pts',(-22.6436823226993,2.37873337814514,
-7.19335702924423));
#134499=CARTESIAN_POINT('Ctrl Pts',(-22.6751120434059,2.36246583866492,
-7.19147718478864));
#134500=CARTESIAN_POINT('Ctrl Pts',(-22.7414704559497,2.32517297960324,
-7.18736173738413));
#134501=CARTESIAN_POINT('Ctrl Pts',(-22.7761810526608,2.30381495724719,
-7.1851168749434));
#134502=CARTESIAN_POINT('Ctrl Pts',(-22.8905757391552,2.22702222184579,
-7.17741931534524));
#134503=CARTESIAN_POINT('Ctrl Pts',(-22.9658603965422,2.16545808079784,
-7.17182311867539));
#134504=CARTESIAN_POINT('Ctrl Pts',(-23.0635118593128,2.06890764052073,
-7.16410894451162));
#134505=CARTESIAN_POINT('Ctrl Pts',(-23.0910426054437,2.0394683168284,-7.16187627565383));
#134506=CARTESIAN_POINT('Ctrl Pts',(-23.1298573577239,1.99455976175702,
-7.15868013171908));
#134507=CARTESIAN_POINT('Ctrl Pts',(-23.1420560093701,1.97990562862154,
-7.15766803758976));
#134508=CARTESIAN_POINT('Ctrl Pts',(-23.1644838315487,1.95192442584678,
-7.15579861238001));
#134509=CARTESIAN_POINT('Ctrl Pts',(-23.174772511727,1.93864977178774,-7.15493795306817));
#134510=CARTESIAN_POINT('Ctrl Pts',(-23.2027698489291,1.90128277031755,
-7.15258029688543));
#134511=CARTESIAN_POINT('Ctrl Pts',(-23.2199988473526,1.8768386692303,-7.15111083575362));
#134512=CARTESIAN_POINT('Ctrl Pts',(-23.2601041473455,1.81627372022938,
-7.1476050035486));
#134513=CARTESIAN_POINT('Ctrl Pts',(-23.2822110673174,1.77967277852856,
-7.14559741607967));
#134514=CARTESIAN_POINT('Ctrl Pts',(-23.3587185524053,1.64022641179758,
-7.13819206927601));
#134515=CARTESIAN_POINT('Ctrl Pts',(-23.4029541298363,1.53226049804071,
-7.13289979707267));
#134516=CARTESIAN_POINT('Ctrl Pts',(-23.4439575791163,1.38743996206328,
-7.125551731529));
#134517=CARTESIAN_POINT('Ctrl Pts',(-23.4521782242363,1.35423064126585,
-7.1238535211426));
#134518=CARTESIAN_POINT('Ctrl Pts',(-23.4650622428798,1.29361002239718,
-7.12071564115976));
#134519=CARTESIAN_POINT('Ctrl Pts',(-23.4701013710537,1.26629333959326,
-7.11928801698951));
#134520=CARTESIAN_POINT('Ctrl Pts',(-23.478593183246,1.21209796685664,-7.11642423113787));
#134521=CARTESIAN_POINT('Ctrl Pts',(-23.4820804942635,1.18523474495591,
-7.11498966588192));
#134522=CARTESIAN_POINT('Ctrl Pts',(-23.4903223452944,1.10531999917952,
-7.11067568228148));
#134523=CARTESIAN_POINT('Ctrl Pts',(-23.4930390689691,1.05210288801396,
-7.10774127659502));
#134524=CARTESIAN_POINT('Ctrl Pts',(-23.4929995970599,0.998856170999325,
-7.10475651985954));
#134525=CARTESIAN_POINT('Ctrl Pts',(-23.4929995972711,0.998856455981027,
-7.10475653583426));
#134526=CARTESIAN_POINT('Ctrl Pts',(-23.4929235684559,0.896269736323447,
-7.09900601444055));
#134527=CARTESIAN_POINT('Ctrl Pts',(-23.4826173632919,0.793951174046108,
-7.09307389240344));
#134528=CARTESIAN_POINT('Ctrl Pts',(-23.4554216638391,0.659808150190311,
-7.08544914418858));
#134529=CARTESIAN_POINT('Ctrl Pts',(-23.447489592033,0.626435965649716,
-7.08356747181471));
#134530=CARTESIAN_POINT('Ctrl Pts',(-23.4338545668414,0.576527510145044,
-7.08080277447794));
#134531=CARTESIAN_POINT('Ctrl Pts',(-23.4289723050001,0.5597792430666,-7.07988358165846));
#134532=CARTESIAN_POINT('Ctrl Pts',(-23.4184651421447,0.525885426277317,
-7.07804590384003));
#134533=CARTESIAN_POINT('Ctrl Pts',(-23.4128214830959,0.508748672184849,
-7.07712845262034));
#134534=CARTESIAN_POINT('Ctrl Pts',(-23.3942266054438,0.4554509610844,-7.07430080697578));
#134535=CARTESIAN_POINT('Ctrl Pts',(-23.3802245111786,0.419670474931517,
-7.07243990595309));
#134536=CARTESIAN_POINT('Ctrl Pts',(-23.3247344473096,0.29212168199213,
-7.06582440446269));
#134537=CARTESIAN_POINT('Ctrl Pts',(-23.2756269513529,0.203946453300423,
-7.06127103180419));
#134538=CARTESIAN_POINT('Ctrl Pts',(-23.1947847243802,0.0872780304448506,
-7.0545992842203));
#134539=CARTESIAN_POINT('Ctrl Pts',(-23.1699431365536,0.0543315104024122,
-7.052635529525));
#134540=CARTESIAN_POINT('Ctrl Pts',(-23.1212172601452,-0.00517217496151634,
-7.0488955805939));
#134541=CARTESIAN_POINT('Ctrl Pts',(-23.0976733738544,-0.031972173152881,
-7.04713122248206));
#134542=CARTESIAN_POINT('Ctrl Pts',(-23.0540091024304,-0.0783312500188815,
-7.04391566112988));
#134543=CARTESIAN_POINT('Ctrl Pts',(-23.0342437025603,-0.0982030088020824,
-7.04247901301624));
#134544=CARTESIAN_POINT('Ctrl Pts',(-22.9887646089028,-0.141501763314325,
-7.03920886218204));
#134545=CARTESIAN_POINT('Ctrl Pts',(-22.9627783967539,-0.164619191730893,
-7.03736396896967));
#134546=CARTESIAN_POINT('Ctrl Pts',(-22.8759567370481,-0.236751334806526,
-7.03127076068956));
#134547=CARTESIAN_POINT('Ctrl Pts',(-22.8121812656029,-0.282026159689912,
-7.02689484245253));
#134548=CARTESIAN_POINT('Ctrl Pts',(-22.6885981218585,-0.356353052293743,
-7.01870584870337));
#134549=CARTESIAN_POINT('Ctrl Pts',(-22.6298048411199,-0.386753904916288,
-7.0149198752483));
#134550=CARTESIAN_POINT('Ctrl Pts',(-22.5440146711127,-0.424343430091305,
-7.00967619214999));
#134551=CARTESIAN_POINT('Ctrl Pts',(-22.5184945792665,-0.434720068827819,
-7.00815027324963));
#134552=CARTESIAN_POINT('Ctrl Pts',(-22.4718291636836,-0.452253724291736,
-7.00543646442907));
#134553=CARTESIAN_POINT('Ctrl Pts',(-22.4507802083443,-0.459645791147558,
-7.00423981184371));
#134554=CARTESIAN_POINT('Ctrl Pts',(-22.4142449426568,-0.471592971785797,
-7.00221832953674));
#134555=CARTESIAN_POINT('Ctrl Pts',(-22.3988356394484,-0.476365755844768,
-7.00138309921836));
#134556=CARTESIAN_POINT('Ctrl Pts',(-22.3607207743651,-0.487519248761599,
-6.99935827975823));
#134557=CARTESIAN_POINT('Ctrl Pts',(-22.3379391289771,-0.493622579457318,
-6.99818245163965));
#134558=CARTESIAN_POINT('Ctrl Pts',(-22.2089740258507,-0.525022989092951,
-6.99167488196766));
#134559=CARTESIAN_POINT('Ctrl Pts',(-22.1004735716382,-0.539520866665173,
-6.98674407773248));
#134560=CARTESIAN_POINT('Ctrl Pts',(-21.9429128893289,-0.543744164116973,
-6.97939961816967));
#134561=CARTESIAN_POINT('Ctrl Pts',(-21.8944492667416,-0.542760529498119,
-6.97711872041165));
#134562=CARTESIAN_POINT('Ctrl Pts',(-21.8066980210038,-0.536839038377313,
-6.97287877274052));
#134563=CARTESIAN_POINT('Ctrl Pts',(-21.767400942394,-0.532666620530167,
-6.97093984339362));
#134564=CARTESIAN_POINT('Ctrl Pts',(-21.7003350912236,-0.522929891555131,
-6.96753784741619));
#134565=CARTESIAN_POINT('Ctrl Pts',(-21.6724793484114,-0.518100846150755,
-6.96609707798743));
#134566=CARTESIAN_POINT('Ctrl Pts',(-21.6131465058929,-0.506127377859396,
-6.96296223021407));
#134567=CARTESIAN_POINT('Ctrl Pts',(-21.5817296271079,-0.498755046429045,
-6.96126188238585));
#134568=CARTESIAN_POINT('Ctrl Pts',(-21.4826261628817,-0.472195084465676,
-6.9557639991729));
#134569=CARTESIAN_POINT('Ctrl Pts',(-21.4160151938523,-0.449363720947438,
-6.95186191620282));
#134570=CARTESIAN_POINT('Ctrl Pts',(-21.2800805401054,-0.39212482982534,
-6.94353064191551));
#134571=CARTESIAN_POINT('Ctrl Pts',(-21.2113095914403,-0.356886132052856,
-6.93909812875738));
#134572=CARTESIAN_POINT('Ctrl Pts',(-21.1100450799699,-0.295008716368494,
-6.93243413491605));
#134573=CARTESIAN_POINT('Ctrl Pts',(-21.0755116954913,-0.271944376227107,
-6.93013619706407));
#134574=CARTESIAN_POINT('Ctrl Pts',(-21.0270350840932,-0.236658793809985,
-6.92691624399505));
#134575=CARTESIAN_POINT('Ctrl Pts',(-21.0123168573177,-0.225536450728647,
-6.92593950089538));
#134576=CARTESIAN_POINT('Ctrl Pts',(-20.9843119570395,-0.203573606993106,
-6.92408833559616));
#134577=CARTESIAN_POINT('Ctrl Pts',(-20.9709999790984,-0.192770641257813,
-6.9232121190002));
#134578=CARTESIAN_POINT('Ctrl Pts',(-20.9331534224597,-0.160996785684957,
-6.92072351297379));
#134579=CARTESIAN_POINT('Ctrl Pts',(-20.909092004255,-0.139474124473975,
-6.91914429441138));
#134580=CARTESIAN_POINT('Ctrl Pts',(-20.8077072639397,-0.0428929965425517,
-6.91241776664495));
#134581=CARTESIAN_POINT('Ctrl Pts',(-20.7376880684383,0.0393955660242851,
-6.90756134962266));
#134582=CARTESIAN_POINT('Ctrl Pts',(-20.6530010058874,0.163089637464466,
-6.90052454657455));
#134583=CARTESIAN_POINT('Ctrl Pts',(-20.6306265776347,0.198826577730289,
-6.898521096522));
#134584=CARTESIAN_POINT('Ctrl Pts',(-20.5918250272167,0.266844205188268,
-6.89471787182838));
#134585=CARTESIAN_POINT('Ctrl Pts',(-20.5750169378145,0.298873752970388,
-6.89293087809891));
#134586=CARTESIAN_POINT('Ctrl Pts',(-20.547316080813,0.356495366945819,
-6.88970547296704));
#134587=CARTESIAN_POINT('Ctrl Pts',(-20.5359606161303,0.38184719788406,
-6.88828301164002));
#134588=CARTESIAN_POINT('Ctrl Pts',(-20.5121629580809,0.43906928953469,
-6.88505922553819));
#134589=CARTESIAN_POINT('Ctrl Pts',(-20.5000842471488,0.471074015530362,
-6.88324720963607));
#134590=CARTESIAN_POINT('Ctrl Pts',(-20.4518269416484,0.61305446837943,
-6.8751647374586));
#134591=CARTESIAN_POINT('Ctrl Pts',(-20.4270307385083,0.726490167276728,
-6.86855659908311));
#134592=CARTESIAN_POINT('Ctrl Pts',(-20.4107297270828,0.884453665080072,
-6.85953431059122));
#134593=CARTESIAN_POINT('Ctrl Pts',(-20.4081041812435,0.927463828955015,
-6.85710049262177));
#134594=CARTESIAN_POINT('Ctrl Pts',(-20.4067076773825,1.00056636344053,
-6.85305303151891));
#134595=CARTESIAN_POINT('Ctrl Pts',(-20.4070112176528,1.03061597687359,
-6.85141498321165));
#134596=CARTESIAN_POINT('Ctrl Pts',(-20.4088527960233,1.0774398547753,-6.84892117341234));
#134597=CARTESIAN_POINT('Ctrl Pts',(-20.4097881696222,1.0942297131862,-6.84803886342712));
#134598=CARTESIAN_POINT('Ctrl Pts',(-20.4123662245766,1.12997337732766,
-6.84618996558625));
#134599=CARTESIAN_POINT('Ctrl Pts',(-20.4140852520832,1.1489182898307,-6.84522698511415));
#134600=CARTESIAN_POINT('Ctrl Pts',(-20.42050610887,1.20760122916372,-6.84228409368999));
#134601=CARTESIAN_POINT('Ctrl Pts',(-20.4264036946116,1.24719329182546,
-6.84035554010008));
#134602=CARTESIAN_POINT('Ctrl Pts',(-20.4519070219309,1.38215124775166,
-6.83385124108246));
#134603=CARTESIAN_POINT('Ctrl Pts',(-20.4789884718184,1.4758659320459,-6.82944225733426));
#134604=CARTESIAN_POINT('Ctrl Pts',(-20.5296893367747,1.60434242310546,
-6.82294545066961));
#134605=CARTESIAN_POINT('Ctrl Pts',(-20.5461572741502,1.6416677470014,-6.82100222148694));
#134606=CARTESIAN_POINT('Ctrl Pts',(-20.5796471676462,1.71009542190057,
-6.81729507665812));
#134607=CARTESIAN_POINT('Ctrl Pts',(-20.5962996928161,1.74134853143709,
-6.81554251962331));
#134608=CARTESIAN_POINT('Ctrl Pts',(-20.6280302337796,1.79625997677209,
-6.81233885406098));
#134609=CARTESIAN_POINT('Ctrl Pts',(-20.642706422861,1.82013254419814,-6.81090178551949));
#134610=CARTESIAN_POINT('Ctrl Pts',(-20.6771650920889,1.87290664683747,
-6.80761800174241));
#134611=CARTESIAN_POINT('Ctrl Pts',(-20.6972974748007,1.90156023183691,
-6.8057594227486));
#134612=CARTESIAN_POINT('Ctrl Pts',(-20.7687254420368,1.99620402690321,
-6.79935474250027));
#134613=CARTESIAN_POINT('Ctrl Pts',(-20.8243953407901,2.05869903584125,
-6.79465794669617));
#134614=CARTESIAN_POINT('Ctrl Pts',(-20.9247799203756,2.15447800779839,
-6.78676889289815));
#134615=CARTESIAN_POINT('Ctrl Pts',(-20.9667284900612,2.19040831542292,
-6.78361570988936));
#134616=CARTESIAN_POINT('Ctrl Pts',(-21.010508379234,2.22401162372414,-6.7805154429392));
#134617=CARTESIAN_POINT('Origin',(-21.9500000210213,0.999999999999992,-4.89578827641128));
#134618=CARTESIAN_POINT('',(-21.0105083954618,2.22401163617983,-6.28210099484077));
#134619=CARTESIAN_POINT('',(-21.0104995485061,2.22400480179726,-6.32268395191223));
#134620=CARTESIAN_POINT('',(-21.0105083758276,2.22401162110953,-4.89578827641128));
#134621=CARTESIAN_POINT('',(-23.4929994962299,0.998727401813637,-6.10421116902006));
#134622=CARTESIAN_POINT('Ctrl Pts',(-21.0105083954618,2.22401163617983,
-6.28210099484077));
#134623=CARTESIAN_POINT('Ctrl Pts',(-21.0399420576368,2.24660347951331,
-6.28033334307814));
#134624=CARTESIAN_POINT('Ctrl Pts',(-21.0701862087003,2.26813026764285,
-6.27853890030681));
#134625=CARTESIAN_POINT('Ctrl Pts',(-21.1272476034273,2.30571881745943,
-6.27516770049963));
#134626=CARTESIAN_POINT('Ctrl Pts',(-21.1538260232459,2.32209302687499,
-6.27360290129919));
#134627=CARTESIAN_POINT('Ctrl Pts',(-21.2058017969316,2.35197793063193,
-6.27054312625838));
#134628=CARTESIAN_POINT('Ctrl Pts',(-21.2311163498558,2.36560662365534,
-6.26905302826995));
#134629=CARTESIAN_POINT('Ctrl Pts',(-21.2951697405236,2.39781659414886,
-6.26527786714295));
#134630=CARTESIAN_POINT('Ctrl Pts',(-21.3343301025341,2.41550133710155,
-6.26296519001372));
#134631=CARTESIAN_POINT('Ctrl Pts',(-21.4710988065573,2.4705158514446,-6.25487663302854));
#134632=CARTESIAN_POINT('Ctrl Pts',(-21.5717263105529,2.49955619443129,
-6.24888457579755));
#134633=CARTESIAN_POINT('Ctrl Pts',(-21.7277180933228,2.52786285000555,
-6.23991047362025));
#134634=CARTESIAN_POINT('Ctrl Pts',(-21.7814083644928,2.53471553886673,
-6.2368815771936));
#134635=CARTESIAN_POINT('Ctrl Pts',(-21.8553177804522,2.54022244172986,
-6.23287967914589));
#134636=CARTESIAN_POINT('Ctrl Pts',(-21.8753128488886,2.5413214450698,-6.23181386516449));
#134637=CARTESIAN_POINT('Ctrl Pts',(-21.9121701837277,2.54262828845049,
-6.2298869175179));
#134638=CARTESIAN_POINT('Ctrl Pts',(-21.9290242886329,2.54294950002155,
-6.22902091033235));
#134639=CARTESIAN_POINT('Ctrl Pts',(-21.974782136117,2.54307165911276,-6.22670446443604));
#134640=CARTESIAN_POINT('Ctrl Pts',(-22.0036816037231,2.54233678673989,
-6.22527853767758));
#134641=CARTESIAN_POINT('Ctrl Pts',(-22.0729403217914,2.53862638826864,
-6.22191620035668));
#134642=CARTESIAN_POINT('Ctrl Pts',(-22.113236826147,2.53487442235251,-6.22000460833268));
#134643=CARTESIAN_POINT('Ctrl Pts',(-22.2764385706084,2.51317803463437,
-6.21229706939189));
#134644=CARTESIAN_POINT('Ctrl Pts',(-22.3971028428975,2.48201488658762,
-6.20663628045763));
#134645=CARTESIAN_POINT('Ctrl Pts',(-22.5425760708672,2.42503691862949,
-6.19894016248278));
#134646=CARTESIAN_POINT('Ctrl Pts',(-22.5720513687978,2.41241939267394,
-6.19733559635578));
#134647=CARTESIAN_POINT('Ctrl Pts',(-22.6271966893725,2.38675215540171,
-6.19423532974995));
#134648=CARTESIAN_POINT('Ctrl Pts',(-22.6529362929851,2.37388403002961,
-6.19274595625672));
#134649=CARTESIAN_POINT('Ctrl Pts',(-22.7150309651085,2.34063885617738,
-6.18904239299203));
#134650=CARTESIAN_POINT('Ctrl Pts',(-22.7509478063943,2.31949502682848,
-6.18680367436301));
#134651=CARTESIAN_POINT('Ctrl Pts',(-22.8300682175276,2.26849612803417,
-6.18164975339245));
#134652=CARTESIAN_POINT('Ctrl Pts',(-22.8726917097609,2.23783759138832,
-6.17871252205881));
#134653=CARTESIAN_POINT('Ctrl Pts',(-22.9970391372201,2.13839958269721,
-6.16969915852561));
#134654=CARTESIAN_POINT('Ctrl Pts',(-23.0732672897155,2.06325741091267,
-6.16352545379134));
#134655=CARTESIAN_POINT('Ctrl Pts',(-23.1547083221331,1.96435639115255,
-6.15656940289705));
#134656=CARTESIAN_POINT('Ctrl Pts',(-23.1679444396728,1.94758473008388,
-6.15542626544825));
#134657=CARTESIAN_POINT('Ctrl Pts',(-23.1902798871168,1.91804164419559,
-6.15348251238319));
#134658=CARTESIAN_POINT('Ctrl Pts',(-23.1995400452213,1.90539736460431,
-6.1526723881803));
#134659=CARTESIAN_POINT('Ctrl Pts',(-23.2217834688439,1.87403355879309,
-6.15071616183161));
#134660=CARTESIAN_POINT('Ctrl Pts',(-23.2345475457967,1.85516405463928,
-6.14958334449216));
#134661=CARTESIAN_POINT('Ctrl Pts',(-23.2624514573597,1.81187754770932,
-6.14706663325803));
#134662=CARTESIAN_POINT('Ctrl Pts',(-23.2773367856322,1.78730628113049,
-6.14569480397432));
#134663=CARTESIAN_POINT('Ctrl Pts',(-23.3278520552486,1.69841118107881,
-6.14088067068674));
#134664=CARTESIAN_POINT('Ctrl Pts',(-23.3595621120084,1.63197301865059,
-6.13754841931213));
#134665=CARTESIAN_POINT('Ctrl Pts',(-23.4156185653712,1.48908618307238,
-6.13049356446041));
#134666=CARTESIAN_POINT('Ctrl Pts',(-23.438989578096,1.4124944097765,-6.1267702769421));
#134667=CARTESIAN_POINT('Ctrl Pts',(-23.4631992388391,1.30345455377153,
-6.12131064098858));
#134668=CARTESIAN_POINT('Ctrl Pts',(-23.469121040962,1.2722640034517,-6.1197324987456));
#134669=CARTESIAN_POINT('Ctrl Pts',(-23.4782868704816,1.21427896280653,
-6.11675767833993));
#134670=CARTESIAN_POINT('Ctrl Pts',(-23.4817980370255,1.18753902847286,
-6.11536997386869));
#134671=CARTESIAN_POINT('Ctrl Pts',(-23.4872188284534,1.1357801535101,-6.11264969886424));
#134672=CARTESIAN_POINT('Ctrl Pts',(-23.4892224601812,1.11077950719954,
-6.1113204876626));
#134673=CARTESIAN_POINT('Ctrl Pts',(-23.492229676773,1.05674573773822,-6.10841408928787));
#134674=CARTESIAN_POINT('Ctrl Pts',(-23.4930244222693,1.0277112516658,-6.10683148327199));
#134675=CARTESIAN_POINT('Ctrl Pts',(-23.4929994504673,0.998673075206048,
-6.10522924338513));
#134676=CARTESIAN_POINT('',(-22.3485138628786,-0.490649428218508,-6.00000000000001));
#134677=CARTESIAN_POINT('Ctrl Pts',(-22.3485138628786,-0.490649428218505,
-6.00000000000001));
#134678=CARTESIAN_POINT('Ctrl Pts',(-22.4054645488374,-0.475424093389119,
-6.00304027996498));
#134679=CARTESIAN_POINT('Ctrl Pts',(-22.4615861511829,-0.456918922190118,
-6.00608055992995));
#134680=CARTESIAN_POINT('Ctrl Pts',(-22.5164905695608,-0.435248221882018,
-6.00912083989493));
#134681=CARTESIAN_POINT('Ctrl Pts',(-22.5713672765413,-0.413588459225288,
-6.01215958536762));
#134682=CARTESIAN_POINT('Ctrl Pts',(-22.6250275672966,-0.388766515308164,
-6.01519833084031));
#134683=CARTESIAN_POINT('Ctrl Pts',(-22.6771008615109,-0.360945762240122,
-6.01823707631301));
#134684=CARTESIAN_POINT('Ctrl Pts',(-22.7291610802877,-0.333131994874129,
-6.02127505876644));
#134685=CARTESIAN_POINT('Ctrl Pts',(-22.7796346657544,-0.302321142806013,
-6.02431304121987));
#134686=CARTESIAN_POINT('Ctrl Pts',(-22.8281749607985,-0.268722891394062,
-6.0273510236733));
#134687=CARTESIAN_POINT('Ctrl Pts',(-22.8767176954887,-0.235122951326502,
-6.0303891588164));
#134688=CARTESIAN_POINT('Ctrl Pts',(-22.9233265478032,-0.198735610807954,
-6.03342729395951));
#134689=CARTESIAN_POINT('Ctrl Pts',(-22.9676847033286,-0.159813298508449,
-6.03646542910262));
#134690=CARTESIAN_POINT('Ctrl Pts',(-23.0120584570753,-0.120877299462252,
-6.03950463258375));
#134691=CARTESIAN_POINT('Ctrl Pts',(-23.0541795776982,-0.0794048791799065,
-6.04254383606487));
#134692=CARTESIAN_POINT('Ctrl Pts',(-23.093766475409,-0.0356868724751493,
-6.045583039546));
#134693=CARTESIAN_POINT('Ctrl Pts',(-23.1334091763913,0.00809276087724915,
-6.04862652720969));
#134694=CARTESIAN_POINT('Ctrl Pts',(-23.1705101975796,0.0541239379441578,
-6.05167001487339));
#134695=CARTESIAN_POINT('Ctrl Pts',(-23.204827386285,0.102081694481424,
-6.05471350253708));
#134696=CARTESIAN_POINT('Ctrl Pts',(-23.2391709747928,0.150076344346653,
-6.05775933151939));
#134697=CARTESIAN_POINT('Ctrl Pts',(-23.2707262037194,0.200000116083609,
-6.06080516050171));
#134698=CARTESIAN_POINT('Ctrl Pts',(-23.2992951510333,0.25150039938155,
-6.06385098948403));
#134699=CARTESIAN_POINT('Ctrl Pts',(-23.3279184112935,0.303098590806417,
-6.06690260894732));
#134700=CARTESIAN_POINT('Ctrl Pts',(-23.353543839082,0.356278842196677,
-6.06995422841061));
#134701=CARTESIAN_POINT('Ctrl Pts',(-23.3760205576544,0.41066611407408,
-6.07300584787389));
#134702=CARTESIAN_POINT('Ctrl Pts',(-23.3862470624495,0.435411349676536,
-6.07439428012985));
#134703=CARTESIAN_POINT('Ctrl Pts',(-23.3958224323161,0.46040621178625,
-6.07578271238581));
#134704=CARTESIAN_POINT('Ctrl Pts',(-23.4047358843596,0.485614378197155,
-6.07717114464177));
#134705=CARTESIAN_POINT('Ctrl Pts',(-23.4262377242088,0.546423810324719,
-6.0805204472311));
#134706=CARTESIAN_POINT('Ctrl Pts',(-23.4439525213542,0.608667248297671,
-6.08386974982044));
#134707=CARTESIAN_POINT('Ctrl Pts',(-23.4577111099897,0.671889847457075,
-6.08721905240977));
#134708=CARTESIAN_POINT('Ctrl Pts',(-23.4713655900064,0.734634053254386,
-6.09054301146455));
#134709=CARTESIAN_POINT('Ctrl Pts',(-23.481123374027,0.798342409543584,
-6.09386697051933));
#134710=CARTESIAN_POINT('Ctrl Pts',(-23.4868657659852,0.862549347195262,
-6.09719092957411));
#134711=CARTESIAN_POINT('Ctrl Pts',(-23.4909084317617,0.907751275475867,
-6.09953100938943));
#134712=CARTESIAN_POINT('Ctrl Pts',(-23.4929619471197,0.953199867774789,
-6.10187108920474));
#134713=CARTESIAN_POINT('Ctrl Pts',(-23.4929994962299,0.998727401813637,
-6.10421116902006));
#134714=CARTESIAN_POINT('',(-21.5504160121885,-0.491448856702306,-6.00061430725121));
#134715=CARTESIAN_POINT('Origin',(-21.9500000210213,0.999999999999992,-6.00000000000001));
#134716=CARTESIAN_POINT('Ctrl Pts',(-21.5507399893082,-0.490449739869315,
-6.00122170731199));
#134717=CARTESIAN_POINT('Ctrl Pts',(-21.6610500159688,-0.519999468092027,
-6.00677097255486));
#134718=CARTESIAN_POINT('Ctrl Pts',(-21.7743077902558,-0.537214133001513,
-6.01190259476999));
#134719=CARTESIAN_POINT('Ctrl Pts',(-21.9322474019439,-0.543520758127318,
-6.01930552493555));
#134720=CARTESIAN_POINT('Ctrl Pts',(-21.9761115034942,-0.543401889099155,
-6.02138429714415));
#134721=CARTESIAN_POINT('Ctrl Pts',(-22.0571228967315,-0.539727697711485,
-6.02531493526066));
#134722=CARTESIAN_POINT('Ctrl Pts',(-22.0942610855388,-0.536692936399459,
-6.02715245989659));
#134723=CARTESIAN_POINT('Ctrl Pts',(-22.1594942207025,-0.528976779336596,
-6.0304619058166));
#134724=CARTESIAN_POINT('Ctrl Pts',(-22.1876379153144,-0.524856029833001,
-6.03191676485581));
#134725=CARTESIAN_POINT('Ctrl Pts',(-22.2496355964202,-0.514020403450957,
-6.03518764553848));
#134726=CARTESIAN_POINT('Ctrl Pts',(-22.2834099463349,-0.50694288099423,
-6.03701370772975));
#134727=CARTESIAN_POINT('Ctrl Pts',(-22.3882782086187,-0.481269335601699,
-6.04282601778578));
#134728=CARTESIAN_POINT('Ctrl Pts',(-22.4582939949709,-0.458726186211478,
-6.04691998350428));
#134729=CARTESIAN_POINT('Ctrl Pts',(-22.5893559603307,-0.405942603454932,
-6.05490457723179));
#134730=CARTESIAN_POINT('Ctrl Pts',(-22.6505403979752,-0.376478824792641,
-6.05877689367356));
#134731=CARTESIAN_POINT('Ctrl Pts',(-22.7338709781122,-0.329350822765226,
-6.06412398750824));
#134732=CARTESIAN_POINT('Ctrl Pts',(-22.7577783682896,-0.314960667081059,
-6.06566654975089));
#134733=CARTESIAN_POINT('Ctrl Pts',(-22.8002959396778,-0.287771390292826,
-6.06840930513845));
#134734=CARTESIAN_POINT('Ctrl Pts',(-22.8190404855472,-0.275196876042019,
-6.06961825102237));
#134735=CARTESIAN_POINT('Ctrl Pts',(-22.8509429893663,-0.252765218852784,
-6.07166646327611));
#134736=CARTESIAN_POINT('Ctrl Pts',(-22.8642302338089,-0.243101798573084,
-6.07251597341895));
#134737=CARTESIAN_POINT('Ctrl Pts',(-22.8936494233844,-0.220979149973743,
-6.07439005923984));
#134738=CARTESIAN_POINT('Ctrl Pts',(-22.9096931179497,-0.208409495667832,
-6.07540819278686));
#134739=CARTESIAN_POINT('Ctrl Pts',(-22.9831314129292,-0.148487828845703,
-6.08007342936211));
#134740=CARTESIAN_POINT('Ctrl Pts',(-23.0373059617777,-0.0973387028306494,
-6.08353226615008));
#134741=CARTESIAN_POINT('Ctrl Pts',(-23.1502278023002,0.0258849230818559,
-6.09128240976901));
#134742=CARTESIAN_POINT('Ctrl Pts',(-23.2065829199942,0.0997527170754831,
-6.09556125321762));
#134743=CARTESIAN_POINT('Ctrl Pts',(-23.2753571201417,0.2090489116262,-6.10183440883477));
#134744=CARTESIAN_POINT('Ctrl Pts',(-23.293652973816,0.240545219623791,
-6.10363421644827));
#134745=CARTESIAN_POINT('Ctrl Pts',(-23.3239863983212,0.297297376375765,
-6.10688135315738));
#134746=CARTESIAN_POINT('Ctrl Pts',(-23.336483743355,0.322288922384821,
-6.10831252467071));
#134747=CARTESIAN_POINT('Ctrl Pts',(-23.3628453486188,0.378790441542916,
-6.11155674323206));
#134748=CARTESIAN_POINT('Ctrl Pts',(-23.3763472268142,0.410452167354132,
-6.11338058526193));
#134749=CARTESIAN_POINT('Ctrl Pts',(-23.4145000719108,0.508922436110657,
-6.1190745475602));
#134750=CARTESIAN_POINT('Ctrl Pts',(-23.4355937249144,0.577002067434984,
-6.12304559436128));
#134751=CARTESIAN_POINT('Ctrl Pts',(-23.4736296145518,0.738508175634958,
-6.13244529422364));
#134752=CARTESIAN_POINT('Ctrl Pts',(-23.486808582738,0.832532780455595,
-6.13790701918962));
#134753=CARTESIAN_POINT('Ctrl Pts',(-23.4925200820875,0.953409077433793,
-6.14455887250051));
#134754=CARTESIAN_POINT('Ctrl Pts',(-23.493089727375,0.979673689909002,
-6.14598107634226));
#134755=CARTESIAN_POINT('Ctrl Pts',(-23.4929256542696,1.02228395308811,
-6.14823784741868));
#134756=CARTESIAN_POINT('Ctrl Pts',(-23.4926031013543,1.03862511078824,
-6.14909097477935));
#134757=CARTESIAN_POINT('Ctrl Pts',(-23.4912912630949,1.07543165259509,
-6.15098226069784));
#134758=CARTESIAN_POINT('Ctrl Pts',(-23.4901539825997,1.09588784344058,
-6.15201334818872));
#134759=CARTESIAN_POINT('Ctrl Pts',(-23.4839198812159,1.17835138725323,
-6.15610969450251));
#134760=CARTESIAN_POINT('Ctrl Pts',(-23.4754822318377,1.240051155664,-6.1590383024477));
#134761=CARTESIAN_POINT('Ctrl Pts',(-23.4408852249599,1.41395056175007,
-6.16728626316443));
#134762=CARTESIAN_POINT('Ctrl Pts',(-23.405873775418,1.5239508049406,-6.17252363801508));
#134763=CARTESIAN_POINT('Ctrl Pts',(-23.3450089343391,1.66028020901609,
-6.17980846545791));
#134764=CARTESIAN_POINT('Ctrl Pts',(-23.3300248175135,1.69105077579272,
-6.18150651637506));
#134765=CARTESIAN_POINT('Ctrl Pts',(-23.3009754905653,1.74598543158371,
-6.18465167366141));
#134766=CARTESIAN_POINT('Ctrl Pts',(-23.287252773586,1.77031417764042,-6.18608690057584));
#134767=CARTESIAN_POINT('Ctrl Pts',(-23.2543643062361,1.82509175063418,
-6.18942219110806));
#134768=CARTESIAN_POINT('Ctrl Pts',(-23.2347792649466,1.85526873488805,
-6.1913362310384));
#134769=CARTESIAN_POINT('Ctrl Pts',(-23.1600938155023,1.96198378283801,
-6.1983915769134));
#134770=CARTESIAN_POINT('Ctrl Pts',(-23.099066730903,2.03410928827497,-6.20373287736962));
#134771=CARTESIAN_POINT('Ctrl Pts',(-22.9788263056844,2.15234322845604,
-6.21333998477113));
#134772=CARTESIAN_POINT('Ctrl Pts',(-22.9221026636113,2.20058158039932,
-6.21757701323441));
#134773=CARTESIAN_POINT('Ctrl Pts',(-22.8440209512564,2.25780723714646,
-6.22285162256179));
#134774=CARTESIAN_POINT('Ctrl Pts',(-22.8256348519561,2.27067549443591,
-6.22405633446677));
#134775=CARTESIAN_POINT('Ctrl Pts',(-22.7935832655446,2.29208188377887,
-6.22608452755371));
#134776=CARTESIAN_POINT('Ctrl Pts',(-22.7800543441279,2.30081441448915,
-6.22691876824615));
#134777=CARTESIAN_POINT('Ctrl Pts',(-22.7466045939436,2.3216708294086,-6.22892982368272));
#134778=CARTESIAN_POINT('Ctrl Pts',(-22.7265415836033,2.333557623114,-6.2300933820803));
#134779=CARTESIAN_POINT('Ctrl Pts',(-22.680634511015,2.35936879660854,-6.23267772917099));
#134780=CARTESIAN_POINT('Ctrl Pts',(-22.6546468587024,2.3730197589747,-6.23408672358884));
#134781=CARTESIAN_POINT('Ctrl Pts',(-22.5598870564335,2.41939620322339,
-6.23908531612044));
#134782=CARTESIAN_POINT('Ctrl Pts',(-22.489103459848,2.44776240380153,-6.24256705516795));
#134783=CARTESIAN_POINT('Ctrl Pts',(-22.4114565320771,2.47239092282788,
-6.24635641860603));
#134784=CARTESIAN_POINT('Ctrl Pts',(-22.4063917444806,2.47396870242068,
-6.24660343356632));
#134785=CARTESIAN_POINT('Ctrl Pts',(-22.3377292321456,2.49497057530267,
-6.24995084027072));
#134786=CARTESIAN_POINT('Ctrl Pts',(-22.2729525430773,2.51028860883495,
-6.25309746792029));
#134787=CARTESIAN_POINT('Ctrl Pts',(-22.1755111153672,2.52677415703778,
-6.25795160199854));
#134788=CARTESIAN_POINT('Ctrl Pts',(-22.1434686229847,2.53116436088038,
-6.25956606450709));
#134789=CARTESIAN_POINT('Ctrl Pts',(-22.0830973930617,2.53751065570492,
-6.26265348577708));
#134790=CARTESIAN_POINT('Ctrl Pts',(-22.0548064789168,2.5396978275622,-6.26411889894446));
#134791=CARTESIAN_POINT('Ctrl Pts',(-21.9867470944211,2.54307506056329,
-6.26769407499894));
#134792=CARTESIAN_POINT('Ctrl Pts',(-21.9469629074188,2.54350944526434,
-6.2698249634293));
#134793=CARTESIAN_POINT('Ctrl Pts',(-21.8582828737924,2.54104916253855,
-6.2746659497019));
#134794=CARTESIAN_POINT('Ctrl Pts',(-21.8094524622411,2.53736476695281,
-6.27739396025025));
#134795=CARTESIAN_POINT('Ctrl Pts',(-21.6731460597477,2.52053146119447,
-6.28514267612558));
#134796=CARTESIAN_POINT('Ctrl Pts',(-21.5865046564124,2.50217678250399,
-6.29023233649642));
#134797=CARTESIAN_POINT('Ctrl Pts',(-21.4687029736605,2.46642646096579,
-6.29709151426721));
#134798=CARTESIAN_POINT('Ctrl Pts',(-21.4358412537486,2.45523003967735,
-6.29899642453891));
#134799=CARTESIAN_POINT('Ctrl Pts',(-21.3869755296177,2.43671857752933,
-6.30178902130684));
#134800=CARTESIAN_POINT('Ctrl Pts',(-21.3706740825828,2.43022318980088,
-6.30271370133179));
#134801=CARTESIAN_POINT('Ctrl Pts',(-21.337817154416,2.41647718771444,-6.30455827205078));
#134802=CARTESIAN_POINT('Ctrl Pts',(-21.3212712525374,2.40921101237725,
-6.30547722344926));
#134803=CARTESIAN_POINT('Ctrl Pts',(-21.2699277666166,2.38557900306318,
-6.30830857008338));
#134804=CARTESIAN_POINT('Ctrl Pts',(-21.2356102976186,2.36820142370269,
-6.3101716146859));
#134805=CARTESIAN_POINT('Ctrl Pts',(-21.1351312428264,2.3125085960954,-6.31563558238665));
#134806=CARTESIAN_POINT('Ctrl Pts',(-21.0711295876697,2.27054219549131,
-6.31913256746625));
#134807=CARTESIAN_POINT('Ctrl Pts',(-21.0104996389931,2.22400491509179,
-6.32268388509548));
#134808=CARTESIAN_POINT('Origin',(-21.9500000210213,0.999999999999992,-4.89578827641128));
#134809=CARTESIAN_POINT('Ctrl Pts',(-21.0104995251143,2.22400482768268,
-6.32268389176578));
#134810=CARTESIAN_POINT('Ctrl Pts',(-20.9562341136017,2.18235271988569,
-6.32586241547408));
#134811=CARTESIAN_POINT('Ctrl Pts',(-20.904801326001,2.13714005071609,-6.32907692812556));
#134812=CARTESIAN_POINT('Ctrl Pts',(-20.836886846209,2.0689265576077,-6.33377202520786));
#134813=CARTESIAN_POINT('Ctrl Pts',(-20.8177723087817,2.04865877321731,
-6.3351494024185));
#134814=CARTESIAN_POINT('Ctrl Pts',(-20.7803819362632,2.00679789242068,
-6.33796867069634));
#134815=CARTESIAN_POINT('Ctrl Pts',(-20.7621304569972,1.98519755889625,
-6.33941067971846));
#134816=CARTESIAN_POINT('Ctrl Pts',(-20.7241763881389,1.93769071429974,
-6.34256173010129));
#134817=CARTESIAN_POINT('Ctrl Pts',(-20.7046794530676,1.91163805099431,
-6.34427751992109));
#134818=CARTESIAN_POINT('Ctrl Pts',(-20.6422571075561,1.82248390314033,
-6.35011409126985));
#134819=CARTESIAN_POINT('Ctrl Pts',(-20.6031940448469,1.75682417900575,
-6.35436279536965));
#134820=CARTESIAN_POINT('Ctrl Pts',(-20.5269466097512,1.60391434667756,
-6.36404044954824));
#134821=CARTESIAN_POINT('Ctrl Pts',(-20.4926133630438,1.51557577547159,
-6.36949173509087));
#134822=CARTESIAN_POINT('Ctrl Pts',(-20.4593701503564,1.39944800184883,
-6.37613068745714));
#134823=CARTESIAN_POINT('Ctrl Pts',(-20.4527990439309,1.37406616908951,
-6.37754990006557));
#134824=CARTESIAN_POINT('Ctrl Pts',(-20.4431870672623,1.33261188094062,
-6.37980343335026));
#134825=CARTESIAN_POINT('Ctrl Pts',(-20.4397495176974,1.3166377024717,-6.38065619165817));
#134826=CARTESIAN_POINT('Ctrl Pts',(-20.4325568901538,1.2804261259711,-6.3825518739719));
#134827=CARTESIAN_POINT('Ctrl Pts',(-20.4289517763339,1.26016299182771,
-6.38358756660748));
#134828=CARTESIAN_POINT('Ctrl Pts',(-20.408399779469,1.12954571381993,-6.39013654082707));
#134829=CARTESIAN_POINT('Ctrl Pts',(-20.4030657857814,1.01769003896382,
-6.39518362391348));
#134830=CARTESIAN_POINT('Ctrl Pts',(-20.4129206373538,0.855827210789566,
-6.40272654629885));
#134831=CARTESIAN_POINT('Ctrl Pts',(-20.4184615460036,0.805607689584953,
-6.40509731095146));
#134832=CARTESIAN_POINT('Ctrl Pts',(-20.4328717565922,0.715721109269101,
-6.4094769056059));
#134833=CARTESIAN_POINT('Ctrl Pts',(-20.4408641619389,0.675960963588054,
-6.41146296055267));
#134834=CARTESIAN_POINT('Ctrl Pts',(-20.4571000342257,0.608969604186957,
-6.41491880669847));
#134835=CARTESIAN_POINT('Ctrl Pts',(-20.4645476519412,0.581566887249796,
-6.41636416598429));
#134836=CARTESIAN_POINT('Ctrl Pts',(-20.4819485838035,0.523881088261651,
-6.419481160704));
#134837=CARTESIAN_POINT('Ctrl Pts',(-20.4920926772242,0.493669843337177,
-6.42115813565528));
#134838=CARTESIAN_POINT('Ctrl Pts',(-20.5257524393385,0.402845995000081,
-6.4263410428713));
#134839=CARTESIAN_POINT('Ctrl Pts',(-20.5521672900069,0.343390251564348,
-6.4299329195472));
#134840=CARTESIAN_POINT('Ctrl Pts',(-20.6203403434113,0.212836742300793,
-6.43822622212054));
#134841=CARTESIAN_POINT('Ctrl Pts',(-20.6642042133427,0.143058002541596,
-6.44295830203225));
#134842=CARTESIAN_POINT('Ctrl Pts',(-20.7315494102603,0.0528222783889909,
-6.44928846053436));
#134843=CARTESIAN_POINT('Ctrl Pts',(-20.7503890387456,0.0290720038810077,
-6.45097557899787));
#134844=CARTESIAN_POINT('Ctrl Pts',(-20.7852712951851,-0.0123359045356564,
-6.45393509006294));
#134845=CARTESIAN_POINT('Ctrl Pts',(-20.8010469073053,-0.030205730246653,
-6.4552186523618));
#134846=CARTESIAN_POINT('Ctrl Pts',(-20.8282025812767,-0.0595662316240952,
-6.45732825101379));
#134847=CARTESIAN_POINT('Ctrl Pts',(-20.8393596816521,-0.0712554251554742,
-6.45816782161908));
#134848=CARTESIAN_POINT('Ctrl Pts',(-20.8662483195728,-0.0985545988870662,
-6.46012755899386));
#134849=CARTESIAN_POINT('Ctrl Pts',(-20.88213590301,-0.114004612038738,
-6.46123703413011));
#134850=CARTESIAN_POINT('Ctrl Pts',(-20.9598138514844,-0.186353685959237,
-6.46646524650204));
#134851=CARTESIAN_POINT('Ctrl Pts',(-21.0258530758953,-0.238490394082511,
-6.47033902180352));
#134852=CARTESIAN_POINT('Ctrl Pts',(-21.1484797236972,-0.320005204140976,
-6.47715631456662));
#134853=CARTESIAN_POINT('Ctrl Pts',(-21.2032481408839,-0.351743225870034,
-6.48008573476119));
#134854=CARTESIAN_POINT('Ctrl Pts',(-21.3012246596113,-0.400744078161206,
-6.48530548313974));
#134855=CARTESIAN_POINT('Ctrl Pts',(-21.3435506834406,-0.419581698746345,
-6.48755350984637));
#134856=CARTESIAN_POINT('Ctrl Pts',(-21.4137553273215,-0.447113623230408,
-6.49131200715453));
#134857=CARTESIAN_POINT('Ctrl Pts',(-21.441146992811,-0.45697105924249,
-6.49278530721232));
#134858=CARTESIAN_POINT('Ctrl Pts',(-21.4975619518885,-0.475488111564677,
-6.49584095296535));
#134859=CARTESIAN_POINT('Ctrl Pts',(-21.5265940810974,-0.484079721875075,
-6.49742464029722));
#134860=CARTESIAN_POINT('Ctrl Pts',(-21.6096220131408,-0.506015952451806,
-6.50199026825619));
#134861=CARTESIAN_POINT('Ctrl Pts',(-21.6641091384797,-0.517302451331485,
-6.50503113072352));
#134862=CARTESIAN_POINT('Ctrl Pts',(-21.812480326198,-0.539759817998222,
-6.51340318009745));
#134863=CARTESIAN_POINT('Ctrl Pts',(-21.9069774850213,-0.545289479571833,
-6.5188429419793));
#134864=CARTESIAN_POINT('Ctrl Pts',(-22.033347344027,-0.541079278017493,
-6.52596573887694));
#134865=CARTESIAN_POINT('Ctrl Pts',(-22.0652763800405,-0.539020354314514,
-6.52775069597113));
#134866=CARTESIAN_POINT('Ctrl Pts',(-22.1217359591999,-0.533612498204303,
-6.53085747415398));
#134867=CARTESIAN_POINT('Ctrl Pts',(-22.1462934541628,-0.530663105383828,
-6.5321919993967));
#134868=CARTESIAN_POINT('Ctrl Pts',(-22.1868194492482,-0.524804415545166,
-6.53435520691601));
#134869=CARTESIAN_POINT('Ctrl Pts',(-22.2028307423267,-0.52223146657294,
-6.53519924511303));
#134870=CARTESIAN_POINT('Ctrl Pts',(-22.2395951150924,-0.515727427956221,
-6.53711169458104));
#134871=CARTESIAN_POINT('Ctrl Pts',(-22.2603130945794,-0.511621921228222,
-6.53817165515519));
#134872=CARTESIAN_POINT('Ctrl Pts',(-22.3713839177443,-0.487231968747643,
-6.54378835514993));
#134873=CARTESIAN_POINT('Ctrl Pts',(-22.4598635700684,-0.459268836868039,
-6.5480350907299));
#134874=CARTESIAN_POINT('Ctrl Pts',(-22.6001469429997,-0.400603907158095,
-6.55507815490046));
#134875=CARTESIAN_POINT('Ctrl Pts',(-22.6536139325846,-0.374521509609291,
-6.55784135482481));
#134876=CARTESIAN_POINT('Ctrl Pts',(-22.7444188811032,-0.323535381443718,
-6.56281563063614));
#134877=CARTESIAN_POINT('Ctrl Pts',(-22.7824246651095,-0.299967705704365,
-6.56499076557906));
#134878=CARTESIAN_POINT('Ctrl Pts',(-22.8432256142893,-0.258503891876072,
-6.5686640702641));
#134879=CARTESIAN_POINT('Ctrl Pts',(-22.8666359666912,-0.241556447839582,
-6.57012876868565));
#134880=CARTESIAN_POINT('Ctrl Pts',(-22.9138325744578,-0.205326702411308,
-6.57319460310958));
#134881=CARTESIAN_POINT('Ctrl Pts',(-22.9375483131362,-0.185973798882371,
-6.57479801190376));
#134882=CARTESIAN_POINT('Ctrl Pts',(-23.004930141621,-0.127564667818754,
-6.57954616177047));
#134883=CARTESIAN_POINT('Ctrl Pts',(-23.0469641398496,-0.086714456729049,
-6.58275836341238));
#134884=CARTESIAN_POINT('Ctrl Pts',(-23.1569796139188,0.0331046437758653,
-6.59185970446722));
#134885=CARTESIAN_POINT('Ctrl Pts',(-23.2194426880718,0.116710483508204,
-6.59788077953576));
#134886=CARTESIAN_POINT('Ctrl Pts',(-23.2912070633835,0.236283472400158,
-6.60566010455058));
#134887=CARTESIAN_POINT('Ctrl Pts',(-23.308356659545,0.267219804178711,
-6.60760322519845));
#134888=CARTESIAN_POINT('Ctrl Pts',(-23.3324356887674,0.314411950420515,
-6.61043673716491));
#134889=CARTESIAN_POINT('Ctrl Pts',(-23.3401734202136,0.330240840590128,
-6.6113658409607));
#134890=CARTESIAN_POINT('Ctrl Pts',(-23.3552233444543,0.362413282298291,
-6.6132065810141));
#134891=CARTESIAN_POINT('Ctrl Pts',(-23.3625255688187,0.378758466336531,
-6.61411765569486));
#134892=CARTESIAN_POINT('Ctrl Pts',(-23.3841632059582,0.429547060338007,
-6.61688541096149));
#134893=CARTESIAN_POINT('Ctrl Pts',(-23.3975359418104,0.464387549600414,
-6.61869588756311));
#134894=CARTESIAN_POINT('Ctrl Pts',(-23.4298625914804,0.558697394457863,
-6.62344517255297));
#134895=CARTESIAN_POINT('Ctrl Pts',(-23.4464946628616,0.618889023904732,
-6.62632150302345));
#134896=CARTESIAN_POINT('Ctrl Pts',(-23.4766331346268,0.761018215989604,
-6.63304958114686));
#134897=CARTESIAN_POINT('Ctrl Pts',(-23.487265281678,0.843362629562132,
-6.63690547217981));
#134898=CARTESIAN_POINT('Ctrl Pts',(-23.4929082668566,0.961142564865192,
-6.64264947334773));
#134899=CARTESIAN_POINT('Ctrl Pts',(-23.4933926753148,0.996172631423811,
-6.64438499317861));
#134900=CARTESIAN_POINT('Ctrl Pts',(-23.4921176458459,1.05924199535909,
-6.64757409183285));
#134901=CARTESIAN_POINT('Ctrl Pts',(-23.4907853367835,1.08727465647435,
-6.64901444994649));
#134902=CARTESIAN_POINT('Ctrl Pts',(-23.4860372889687,1.15066291194352,
-6.65232896858211));
#134903=CARTESIAN_POINT('Ctrl Pts',(-23.4821637489637,1.18596734259516,
-6.6542159044333));
#134904=CARTESIAN_POINT('Ctrl Pts',(-23.4712090913378,1.26162638613013,
-6.65835012692968));
#134905=CARTESIAN_POINT('Ctrl Pts',(-23.463731816284,1.30189586599952,-6.66060684148032));
#134906=CARTESIAN_POINT('Ctrl Pts',(-23.4328736456791,1.43773153290873,
-6.66839145727455));
#134907=CARTESIAN_POINT('Ctrl Pts',(-23.4019655431347,1.53133589721564,
-6.67406668466317));
#134908=CARTESIAN_POINT('Ctrl Pts',(-23.3466214656947,1.65713401311009,
-6.68177779194508));
#134909=CARTESIAN_POINT('Ctrl Pts',(-23.3295278391368,1.69230047404541,
-6.68394064536241));
#134910=CARTESIAN_POINT('Ctrl Pts',(-23.3022236472745,1.74343573844717,
-6.68705933762911));
#134911=CARTESIAN_POINT('Ctrl Pts',(-23.2930257710599,1.7599258723455,-6.68806077676556));
#134912=CARTESIAN_POINT('Ctrl Pts',(-23.2750108856074,1.79087406184402,
-6.68992616830943));
#134913=CARTESIAN_POINT('Ctrl Pts',(-23.2662544151352,1.80536324413174,
-6.69079293623079));
#134914=CARTESIAN_POINT('Ctrl Pts',(-23.2409432436152,1.84572932969834,
-6.69319651652667));
#134915=CARTESIAN_POINT('Ctrl Pts',(-23.223850985873,1.871261403476,-6.69470390459601));
#134916=CARTESIAN_POINT('Ctrl Pts',(-23.1800957449363,1.93257890810397,
-6.69833351932767));
#134917=CARTESIAN_POINT('Ctrl Pts',(-23.1526208887644,1.96775115043998,
-6.70042416658543));
#134918=CARTESIAN_POINT('Ctrl Pts',(-23.0466673251364,2.09189542188605,
-6.70801287965762));
#134919=CARTESIAN_POINT('Ctrl Pts',(-22.9595373433578,2.17292280288611,
-6.71342011846344));
#134920=CARTESIAN_POINT('Ctrl Pts',(-22.8378521767939,2.26238657448279,
-6.72083474224028));
#134921=CARTESIAN_POINT('Ctrl Pts',(-22.8111180778296,2.28077196420455,
-6.72245361893247));
#134922=CARTESIAN_POINT('Ctrl Pts',(-22.7600259350867,2.31358557905283,
-6.72554074265786));
#134923=CARTESIAN_POINT('Ctrl Pts',(-22.7358116511044,2.32821271073992,
-6.72700110516213));
#134924=CARTESIAN_POINT('Ctrl Pts',(-22.6770094243654,2.36156242814138,
-6.73054636689619));
#134925=CARTESIAN_POINT('Ctrl Pts',(-22.6420821221952,2.37964377137921,
-6.7326515817394));
#134926=CARTESIAN_POINT('Ctrl Pts',(-22.5630159106784,2.41681678509703,
-6.73741613417258));
#134927=CARTESIAN_POINT('Ctrl Pts',(-22.5185986794014,2.43521892210959,
-6.74009239767715));
#134928=CARTESIAN_POINT('Ctrl Pts',(-22.3926152074019,2.48064685103347,
-6.7476444945669));
#134929=CARTESIAN_POINT('Ctrl Pts',(-22.3095438413971,2.50298080889107,
-6.75258775007764));
#134930=CARTESIAN_POINT('Ctrl Pts',(-22.1877083790675,2.52505201268467,
-6.75951568622415));
#134931=CARTESIAN_POINT('Ctrl Pts',(-22.1501307279146,2.53043685570049,
-6.76160781875572));
#134932=CARTESIAN_POINT('Ctrl Pts',(-22.0944990680934,2.53632441820255,
-6.76460540963081));
#134933=CARTESIAN_POINT('Ctrl Pts',(-22.0765749744832,2.53790491596644,
-6.76555602527367));
#134934=CARTESIAN_POINT('Ctrl Pts',(-22.041131350066,2.5404063387539,-6.76740053378691));
#134935=CARTESIAN_POINT('Ctrl Pts',(-22.0236157812493,2.54134271564379,
-6.76829494186236));
#134936=CARTESIAN_POINT('Ctrl Pts',(-21.9712829415989,2.5432462528985,-6.77092580964335));
#134937=CARTESIAN_POINT('Ctrl Pts',(-21.9364433604481,2.54333355593785,
-6.77262268627803));
#134938=CARTESIAN_POINT('Ctrl Pts',(-21.7931234648943,2.53883843510636,
-6.77948017284892));
#134939=CARTESIAN_POINT('Ctrl Pts',(-21.6852768798642,2.52399407466373,
-6.78437055207333));
#134940=CARTESIAN_POINT('Ctrl Pts',(-21.5254125865281,2.4844938621063,-6.79212364309885));
#134941=CARTESIAN_POINT('Ctrl Pts',(-21.471726072942,2.46807692340225,-6.79481389497106));
#134942=CARTESIAN_POINT('Ctrl Pts',(-21.3905822328316,2.43833943454232,
-6.79909201940464));
#134943=CARTESIAN_POINT('Ctrl Pts',(-21.3624244324847,2.42706810112698,
-6.80061711419488));
#134944=CARTESIAN_POINT('Ctrl Pts',(-21.3079700030568,2.40338551053759,
-6.80365574010498));
#134945=CARTESIAN_POINT('Ctrl Pts',(-21.2816558843548,2.39104615530282,
-6.80516647060912));
#134946=CARTESIAN_POINT('Ctrl Pts',(-21.2234565369133,2.36172232622214,
-6.80860841085151));
#134947=CARTESIAN_POINT('Ctrl Pts',(-21.1917884061643,2.34434668504245,
-6.81055170629451));
#134948=CARTESIAN_POINT('Ctrl Pts',(-21.108714593042,2.29489629144899,-6.81583981531629));
#134949=CARTESIAN_POINT('Ctrl Pts',(-21.0585416696014,2.26088010595229,
-6.81923971945315));
#134950=CARTESIAN_POINT('Ctrl Pts',(-21.010500834247,2.22400583252304,-6.82267576524316));
#134951=CARTESIAN_POINT('Ctrl Pts',(-21.010508379234,2.22401162372414,-6.7805154429392));
#134952=CARTESIAN_POINT('Ctrl Pts',(-21.0158319840829,2.22809776323681,
-6.78013845257946));
#134953=CARTESIAN_POINT('Ctrl Pts',(-21.0211826687174,2.23214949563438,
-6.779762270056));
#134954=CARTESIAN_POINT('Ctrl Pts',(-21.0479546426187,2.25214866918077,
-6.77789414648241));
#134955=CARTESIAN_POINT('Ctrl Pts',(-21.069761413228,2.2675733773478,-6.77641700861394));
#134956=CARTESIAN_POINT('Ctrl Pts',(-21.1101024866793,2.29456468137134,
-6.77377829641301));
#134957=CARTESIAN_POINT('Ctrl Pts',(-21.1285030699195,2.30631865728353,
-6.77260864865622));
#134958=CARTESIAN_POINT('Ctrl Pts',(-21.1609438262069,2.32608457938309,
-6.77061298461235));
#134959=CARTESIAN_POINT('Ctrl Pts',(-21.1748701643254,2.33427273249087,
-6.76977756093891));
#134960=CARTESIAN_POINT('Ctrl Pts',(-21.2099411322835,2.35415861960067,
-6.76772428237199));
#134961=CARTESIAN_POINT('Ctrl Pts',(-21.231236115858,2.36558093497895,-6.76652142220933));
#134962=CARTESIAN_POINT('Ctrl Pts',(-21.3591082537511,2.43034926128059,
-6.7595058326914));
#134963=CARTESIAN_POINT('Ctrl Pts',(-21.4713137061134,2.47170531252301,
-6.75416210594382));
#134964=CARTESIAN_POINT('Ctrl Pts',(-21.6293616921906,2.50994187462362,
-6.74654261423925));
#134965=CARTESIAN_POINT('Ctrl Pts',(-21.6719644205224,2.51836403026559,
-6.74448354629973));
#134966=CARTESIAN_POINT('Ctrl Pts',(-21.7512869548835,2.53059475126771,
-6.74059197164442));
#134967=CARTESIAN_POINT('Ctrl Pts',(-21.7878975289414,2.53490380989219,
-6.73877361598536));
#134968=CARTESIAN_POINT('Ctrl Pts',(-21.8525981064449,2.54017840620371,
-6.73550244069011));
#134969=CARTESIAN_POINT('Ctrl Pts',(-21.8806262774467,2.54169511006505,
-6.73406654873934));
#134970=CARTESIAN_POINT('Ctrl Pts',(-21.9424740070872,2.54335195946797,
-6.73085074675524));
#134971=CARTESIAN_POINT('Ctrl Pts',(-21.9762876254071,2.54314634694285,
-6.72906136890564));
#134972=CARTESIAN_POINT('Ctrl Pts',(-22.1286348797819,2.53721130201981,
-6.72085287407357));
#134973=CARTESIAN_POINT('Ctrl Pts',(-22.2462637612988,2.51893051234446,
-6.71407324563384));
#134974=CARTESIAN_POINT('Ctrl Pts',(-22.4011572741826,2.4761690198959,-6.70494802028667));
#134975=CARTESIAN_POINT('Ctrl Pts',(-22.4412254382283,2.46332351396336,
-6.70257354827352));
#134976=CARTESIAN_POINT('Ctrl Pts',(-22.508510626299,2.43867676985224,-6.69860984269868));
#134977=CARTESIAN_POINT('Ctrl Pts',(-22.5360042181797,2.42769892636964,
-6.69699735988813));
#134978=CARTESIAN_POINT('Ctrl Pts',(-22.5785388779167,2.4092794372668,-6.69453185836545));
#134979=CARTESIAN_POINT('Ctrl Pts',(-22.5938028425612,2.40237214751335,
-6.69365326401092));
#134980=CARTESIAN_POINT('Ctrl Pts',(-22.6262850837856,2.38703097935296,
-6.69180079736924));
#134981=CARTESIAN_POINT('Ctrl Pts',(-22.6434642433958,2.37852234693594,
-6.69083088443239));
#134982=CARTESIAN_POINT('Ctrl Pts',(-22.696841661751,2.35083469734678,-6.68783513167605));
#134983=CARTESIAN_POINT('Ctrl Pts',(-22.7324390925866,2.33053234822254,
-6.68586331655349));
#134984=CARTESIAN_POINT('Ctrl Pts',(-22.8388756668371,2.26407733948411,
-6.6799278788393));
#134985=CARTESIAN_POINT('Ctrl Pts',(-22.9067659995775,2.21350364864761,
-6.67607848618741));
#134986=CARTESIAN_POINT('Ctrl Pts',(-23.0190125075856,2.11458458275668,
-6.66908665964202));
#134987=CARTESIAN_POINT('Ctrl Pts',(-23.0650746359817,2.06850088429555,
-6.66599363517545));
#134988=CARTESIAN_POINT('Ctrl Pts',(-23.1287298590071,1.99620320124634,
-6.66124424824113));
#134989=CARTESIAN_POINT('Ctrl Pts',(-23.1486552774172,1.97213695556005,
-6.6596791010701));
#134990=CARTESIAN_POINT('Ctrl Pts',(-23.1853751846258,1.92493949450979,
-6.6566289499626));
#134991=CARTESIAN_POINT('Ctrl Pts',(-23.2022843990128,1.9019138338186,-6.65514918052333));
#134992=CARTESIAN_POINT('Ctrl Pts',(-23.2425644188,1.84374550446447,-6.6514258184822));
#134993=CARTESIAN_POINT('Ctrl Pts',(-23.2651501614679,1.80808965011639,
-6.64915593455419));
#134994=CARTESIAN_POINT('Ctrl Pts',(-23.3430156744391,1.67323548699643,
-6.64061895435643));
#134995=CARTESIAN_POINT('Ctrl Pts',(-23.3887578541548,1.56895524816671,
-6.63407810995863));
#134996=CARTESIAN_POINT('Ctrl Pts',(-23.4328202632318,1.42808318778802,
-6.62574372398752));
#134997=CARTESIAN_POINT('Ctrl Pts',(-23.4419161280397,1.39521843421883,
-6.62383579116251));
#134998=CARTESIAN_POINT('Ctrl Pts',(-23.4559719691841,1.33699181962598,
-6.6205465618877));
#134999=CARTESIAN_POINT('Ctrl Pts',(-23.4613977951412,1.31175616257833,
-6.61915051412952));
#135000=CARTESIAN_POINT('Ctrl Pts',(-23.4691843926443,1.27053356069065,
-6.61693023044573));
#135001=CARTESIAN_POINT('Ctrl Pts',(-23.4719314972308,1.25462564032951,
-6.61608815137605));
#135002=CARTESIAN_POINT('Ctrl Pts',(-23.4776218601947,1.21828113336301,
-6.61419977605289));
#135003=CARTESIAN_POINT('Ctrl Pts',(-23.4804055428535,1.19782354118241,
-6.61316116608744));
#135004=CARTESIAN_POINT('Ctrl Pts',(-23.4896298994907,1.11808486546197,
-6.60918679118317));
#135005=CARTESIAN_POINT('Ctrl Pts',(-23.4930433496661,1.05850239208585,
-6.60637398081075));
#135006=CARTESIAN_POINT('Ctrl Pts',(-23.4929123977605,0.879980588466109,
-6.59805811834505));
#135007=CARTESIAN_POINT('Ctrl Pts',(-23.4790861453881,0.761508781866254,
-6.59265560430452));
#135008=CARTESIAN_POINT('Ctrl Pts',(-23.4440436444851,0.612930062110029,
-6.58519421624484));
#135009=CARTESIAN_POINT('Ctrl Pts',(-23.4352147740766,0.58032581523435,
-6.58351569085597));
#135010=CARTESIAN_POINT('Ctrl Pts',(-23.4171075627419,0.521218975455224,
-6.58038309620043));
#135011=CARTESIAN_POINT('Ctrl Pts',(-23.4081619541454,0.494629386536749,
-6.57893981051724));
#135012=CARTESIAN_POINT('Ctrl Pts',(-23.3857994507276,0.433707849286491,
-6.57554803580583));
#135013=CARTESIAN_POINT('Ctrl Pts',(-23.3718676369664,0.399584314033827,
-6.57358404660376));
#135014=CARTESIAN_POINT('Ctrl Pts',(-23.3388913280474,0.32641670775893,
-6.56922966389112));
#135015=CARTESIAN_POINT('Ctrl Pts',(-23.3193928864519,0.28761225208465,
-6.56682737888396));
#135016=CARTESIAN_POINT('Ctrl Pts',(-23.2402869771439,0.145462469034467,
-6.55770283807279));
#135017=CARTESIAN_POINT('Ctrl Pts',(-23.1704028363531,0.0483220371332482,
-6.55076448196625));
#135018=CARTESIAN_POINT('Ctrl Pts',(-23.0737893992558,-0.0576044878973603,
-6.54292216097589));
#135019=CARTESIAN_POINT('Ctrl Pts',(-23.0571329308987,-0.0750286779057241,
-6.54162328574241));
#135020=CARTESIAN_POINT('Ctrl Pts',(-23.028646468382,-0.103463437826083,
-6.53949900737956));
#135021=CARTESIAN_POINT('Ctrl Pts',(-23.0170404137433,-0.114690349423836,
-6.53865948264827));
#135022=CARTESIAN_POINT('Ctrl Pts',(-22.989310460399,-0.140684296004001,
-6.53671437571113));
#135023=CARTESIAN_POINT('Ctrl Pts',(-22.9730454101688,-0.155294366914331,
-6.53561888994776));
#135024=CARTESIAN_POINT('Ctrl Pts',(-22.9361953473105,-0.18700614455315,
-6.53322219475524));
#135025=CARTESIAN_POINT('Ctrl Pts',(-22.9154647302448,-0.203928078952855,
-6.53193021308359));
#135026=CARTESIAN_POINT('Ctrl Pts',(-22.8451633437883,-0.258329209796937,
-6.52769522621964));
#135027=CARTESIAN_POINT('Ctrl Pts',(-22.7937690425955,-0.293353850330553,
-6.52483012745152));
#135028=CARTESIAN_POINT('Ctrl Pts',(-22.6688317874341,-0.367872169940582,
-6.51809418198171));
#135029=CARTESIAN_POINT('Ctrl Pts',(-22.5939250372128,-0.404689552146031,
-6.51421928011043));
#135030=CARTESIAN_POINT('Ctrl Pts',(-22.4838396276065,-0.448133563824942,
-6.50845448975972));
#135031=CARTESIAN_POINT('Ctrl Pts',(-22.4508360134639,-0.459876238515879,
-6.50671921363529));
#135032=CARTESIAN_POINT('Ctrl Pts',(-22.3907525256212,-0.478976595796365,
-6.5035321224017));
#135033=CARTESIAN_POINT('Ctrl Pts',(-22.3638169944941,-0.486738015358892,
-6.50209356883858));
#135034=CARTESIAN_POINT('Ctrl Pts',(-22.3024003776073,-0.502636772834646,
-6.49878590246613));
#135035=CARTESIAN_POINT('Ctrl Pts',(-22.2678212487443,-0.510328670147802,
-6.49690414862591));
#135036=CARTESIAN_POINT('Ctrl Pts',(-22.1929004767861,-0.524307426316777,
-6.49278341043077));
#135037=CARTESIAN_POINT('Ctrl Pts',(-22.1525123664644,-0.530196776520286,
-6.4905351174371));
#135038=CARTESIAN_POINT('Ctrl Pts',(-22.0150094238882,-0.544708068951087,
-6.48281006598786));
#135039=CARTESIAN_POINT('Ctrl Pts',(-21.9173332026759,-0.545729844303109,
-6.47718870666442));
#135040=CARTESIAN_POINT('Ctrl Pts',(-21.7805028360202,-0.534179947045099,
-6.46947870034317));
#135041=CARTESIAN_POINT('Ctrl Pts',(-21.7409314524311,-0.529290074618025,
-6.46727129671209));
#135042=CARTESIAN_POINT('Ctrl Pts',(-21.6828321060616,-0.519813011305401,
-6.46410260838279));
#135043=CARTESIAN_POINT('Ctrl Pts',(-21.6641298431269,-0.516406472774023,
-6.46309385846568));
#135044=CARTESIAN_POINT('Ctrl Pts',(-21.6289448336819,-0.509323542847642,
-6.46122336014601));
#135045=CARTESIAN_POINT('Ctrl Pts',(-21.6124509880453,-0.50572064195062,
-6.46035850839637));
#135046=CARTESIAN_POINT('Ctrl Pts',(-21.5665004722398,-0.494890250556752,
-6.45797549455699));
#135047=CARTESIAN_POINT('Ctrl Pts',(-21.537191549784,-0.487063594733397,
-6.45648575672324));
#135048=CARTESIAN_POINT('Ctrl Pts',(-21.4662484252342,-0.46585955517807,
-6.45291414954621));
#135049=CARTESIAN_POINT('Ctrl Pts',(-21.4249150449788,-0.451566714662723,
-6.45086240355508));
#135050=CARTESIAN_POINT('Ctrl Pts',(-21.2786382340742,-0.393917821786189,
-6.44354382177873));
#135051=CARTESIAN_POINT('Ctrl Pts',(-21.1779548297279,-0.34077544946403,
-6.43836818824263));
#135052=CARTESIAN_POINT('Ctrl Pts',(-21.0554792722513,-0.257724145329528,
-6.43114710654988));
#135053=CARTESIAN_POINT('Ctrl Pts',(-21.0276052634691,-0.237426803901148,
-6.42943627318962));
#135054=CARTESIAN_POINT('Ctrl Pts',(-20.9782974621631,-0.198929513972592,
-6.42626996190927));
#135055=CARTESIAN_POINT('Ctrl Pts',(-20.9566364666845,-0.1810446913926,
-6.42482654959232));
#135056=CARTESIAN_POINT('Ctrl Pts',(-20.9082215771356,-0.138795493085473,
-6.42147212821899));
#135057=CARTESIAN_POINT('Ctrl Pts',(-20.881813112811,-0.114061917786863,
-6.41954708107062));
#135058=CARTESIAN_POINT('Ctrl Pts',(-20.7888175167438,-0.0206155256541241,
-6.41240637985316));
#135059=CARTESIAN_POINT('Ctrl Pts',(-20.727794450089,0.053315868740702,
-6.40698564829393));
#135060=CARTESIAN_POINT('Ctrl Pts',(-20.6333894536693,0.192159711004867,
-6.3974279864016));
#135061=CARTESIAN_POINT('Ctrl Pts',(-20.5970086062709,0.254691521244603,
-6.39331852025902));
#135062=CARTESIAN_POINT('Ctrl Pts',(-20.5552227476554,0.339733896410683,
-6.38815766930478));
#135063=CARTESIAN_POINT('Ctrl Pts',(-20.5457452578314,0.360137804077088,
-6.38695033880945));
#135064=CARTESIAN_POINT('Ctrl Pts',(-20.5302659605582,0.395465004514892,
-6.38492122329409));
#135065=CARTESIAN_POINT('Ctrl Pts',(-20.5240457433938,0.410286677399196,
-6.38408853577244));
#135066=CARTESIAN_POINT('Ctrl Pts',(-20.509425406014,0.446709175401514,
-6.38208667830427));
#135067=CARTESIAN_POINT('Ctrl Pts',(-20.5012783785832,0.468406484994799,
-6.38093053177392));
#135068=CARTESIAN_POINT('Ctrl Pts',(-20.4839962705789,0.517785110231488,
-6.37836406239133));
#135069=CARTESIAN_POINT('Ctrl Pts',(-20.4751504511113,0.545558494229956,
-6.37696543244));
#135070=CARTESIAN_POINT('Ctrl Pts',(-20.446333687969,0.645767596038787,
-6.37202730282894));
#135071=CARTESIAN_POINT('Ctrl Pts',(-20.4308713361058,0.719390317600381,
-6.36859432163417));
#135072=CARTESIAN_POINT('Ctrl Pts',(-20.4109184264138,0.867394565708439,
-6.36165839645302));
#135073=CARTESIAN_POINT('Ctrl Pts',(-20.4063227858988,0.941555743434317,
-6.35816487654251));
#135074=CARTESIAN_POINT('Ctrl Pts',(-20.4074069935842,1.04773290587426,
-6.35294860163666));
#135075=CARTESIAN_POINT('Ctrl Pts',(-20.4087275525422,1.07969115724474,
-6.35135169440429));
#135076=CARTESIAN_POINT('Ctrl Pts',(-20.4130748840943,1.13964928531475,
-6.3482940066114));
#135077=CARTESIAN_POINT('Ctrl Pts',(-20.4158770275671,1.16765234748434,
-6.34684051975046));
#135078=CARTESIAN_POINT('Ctrl Pts',(-20.4244449069659,1.2347084391863,-6.34329366542665));
#135079=CARTESIAN_POINT('Ctrl Pts',(-20.4309463814792,1.27364602089609,
-6.34117932056259));
#135080=CARTESIAN_POINT('Ctrl Pts',(-20.4487420770081,1.35975358654683,
-6.33638099729633));
#135081=CARTESIAN_POINT('Ctrl Pts',(-20.4607816699277,1.40672626384451,
-6.33367939842577));
#135082=CARTESIAN_POINT('Ctrl Pts',(-20.5083340076015,1.56154109862775,
-6.32453935669608));
#135083=CARTESIAN_POINT('Ctrl Pts',(-20.553524172263,1.66602185052851,-6.31795301443009));
#135084=CARTESIAN_POINT('Ctrl Pts',(-20.6202965149974,1.78306409743752,
-6.31063225522325));
#135085=CARTESIAN_POINT('Ctrl Pts',(-20.6312101018548,1.80130769991334,
-6.30949396333953));
#135086=CARTESIAN_POINT('Ctrl Pts',(-20.6510730153479,1.83300566999782,
-6.30752892301034));
#135087=CARTESIAN_POINT('Ctrl Pts',(-20.659862053185,1.84655411008623,-6.30669390780339));
#135088=CARTESIAN_POINT('Ctrl Pts',(-20.6823976207191,1.88012662696967,
-6.30463470947974));
#135089=CARTESIAN_POINT('Ctrl Pts',(-20.6964068100095,1.89996827884071,
-6.3034258014671));
#135090=CARTESIAN_POINT('Ctrl Pts',(-20.7294275208484,1.94446844244388,
-6.30071397204598));
#135091=CARTESIAN_POINT('Ctrl Pts',(-20.7487287696739,1.96889907006515,
-6.29922472929941));
#135092=CARTESIAN_POINT('Ctrl Pts',(-20.8251818558492,2.05987013461749,
-6.29361229556627));
#135093=CARTESIAN_POINT('Ctrl Pts',(-20.8872293570132,2.12207838838893,
-6.28962278864746));
#135094=CARTESIAN_POINT('Ctrl Pts',(-20.9726354167221,2.19423119567501,
-6.28438479964871));
#135095=CARTESIAN_POINT('Ctrl Pts',(-20.9914011279391,2.20934582966756,
-6.28324849034829));
#135096=CARTESIAN_POINT('Ctrl Pts',(-21.0105083954618,2.22401163617983,
-6.28210099484077));
#135097=CARTESIAN_POINT('Origin',(21.9499999789786,0.999999999999992,-4.89578827641128));
#135098=CARTESIAN_POINT('Ctrl Pts',(22.889500458052,2.22400484060351,-6.32268396627741));
#135099=CARTESIAN_POINT('Ctrl Pts',(22.9437643008469,2.18235393808173,-6.32586239762496));
#135100=CARTESIAN_POINT('Ctrl Pts',(22.9951956853828,2.13714267871505,-6.32907681541136));
#135101=CARTESIAN_POINT('Ctrl Pts',(23.0631093143957,2.0689305661042,-6.33377182508186));
#135102=CARTESIAN_POINT('Ctrl Pts',(23.0822241961862,2.04866255736481,-6.33514921903181));
#135103=CARTESIAN_POINT('Ctrl Pts',(23.1196150714722,2.00680137313515,-6.33796850987336));
#135104=CARTESIAN_POINT('Ctrl Pts',(23.1378667184438,1.98520096915314,-6.33941052433828));
#135105=CARTESIAN_POINT('Ctrl Pts',(23.175820593364,1.93769463660604,-6.34256154195298));
#135106=CARTESIAN_POINT('Ctrl Pts',(23.1953172082192,1.9116425873736,-6.34427729204013));
#135107=CARTESIAN_POINT('Ctrl Pts',(23.2577255716203,1.82250918564089,-6.35011250822171));
#135108=CARTESIAN_POINT('Ctrl Pts',(23.2967779641055,1.75687153698208,-6.35435979606607));
#135109=CARTESIAN_POINT('Ctrl Pts',(23.3730325216872,1.60396707328758,-6.36403726486672));
#135110=CARTESIAN_POINT('Ctrl Pts',(23.4073766301252,1.5156082237948,-6.36948991197114));
#135111=CARTESIAN_POINT('Ctrl Pts',(23.44062749298,1.39945692921207,-6.37613025049715));
#135112=CARTESIAN_POINT('Ctrl Pts',(23.447199243024,1.37407316760549,-6.37754957858955));
#135113=CARTESIAN_POINT('Ctrl Pts',(23.4568118692577,1.33261671013395,-6.37980323811566));
#135114=CARTESIAN_POINT('Ctrl Pts',(23.4602495177829,1.31664231485889,-6.38065601132625));
#135115=CARTESIAN_POINT('Ctrl Pts',(23.4674421017827,1.2804315076925,-6.38255165984801));
#135116=CARTESIAN_POINT('Ctrl Pts',(23.4710471195632,1.26016936813628,-6.38358730609421));
#135117=CARTESIAN_POINT('Ctrl Pts',(23.4916006802992,1.12954626747083,-6.3901366029481));
#135118=CARTESIAN_POINT('Ctrl Pts',(23.496934793451,1.01768353663625,-6.39518397990132));
#135119=CARTESIAN_POINT('Ctrl Pts',(23.487078239273,0.855816002836622,-6.40272713885022));
#135120=CARTESIAN_POINT('Ctrl Pts',(23.4815372409517,0.805598702475043,
-6.40509780733745));
#135121=CARTESIAN_POINT('Ctrl Pts',(23.4671271473542,0.715715413179718,
-6.40947725420946));
#135122=CARTESIAN_POINT('Ctrl Pts',(23.4591348184108,0.675956349232925,
-6.41146326048851));
#135123=CARTESIAN_POINT('Ctrl Pts',(23.4428990601418,0.608966152625854,
-6.41491905342869));
#135124=CARTESIAN_POINT('Ctrl Pts',(23.4354514014897,0.581563532518983,
-6.41636441048629));
#135125=CARTESIAN_POINT('Ctrl Pts',(23.4180502203203,0.523877367121495,
-6.41948143109962));
#135126=CARTESIAN_POINT('Ctrl Pts',(23.4079058844485,0.49366567009403,-6.42115843521622));
#135127=CARTESIAN_POINT('Ctrl Pts',(23.374247668214,0.402846881396846,-6.42634106846));
#135128=CARTESIAN_POINT('Ctrl Pts',(23.3478353183392,0.34339637697697,-6.42993261983137));
#135129=CARTESIAN_POINT('Ctrl Pts',(23.2796645464399,0.21284467531784,-6.43822575523003));
#135130=CARTESIAN_POINT('Ctrl Pts',(23.2357993549451,0.143063056448227,
-6.44295801734837));
#135131=CARTESIAN_POINT('Ctrl Pts',(23.1684521806485,0.0528243095948877,
-6.44928838236166));
#135132=CARTESIAN_POINT('Ctrl Pts',(23.1496122899442,0.0290736305479866,
-6.45097552873429));
#135133=CARTESIAN_POINT('Ctrl Pts',(23.1147295976499,-0.0123348835206993,
-6.45393508227006));
#135134=CARTESIAN_POINT('Ctrl Pts',(23.0989538246302,-0.0302049200618226,
-6.45521865955291));
#135135=CARTESIAN_POINT('Ctrl Pts',(23.0717979693521,-0.0595656490477214,
-6.45732827442608));
#135136=CARTESIAN_POINT('Ctrl Pts',(23.0606408571012,-0.0712548669842761,
-6.45816784678587));
#135137=CARTESIAN_POINT('Ctrl Pts',(23.0337523306823,-0.0985539540488167,
-6.46012757782062));
#135138=CARTESIAN_POINT('Ctrl Pts',(23.0178648761823,-0.114003861819678,
-6.46123704524837));
#135139=CARTESIAN_POINT('Ctrl Pts',(22.9401855826268,-0.186354305817296,
-6.46646535512513));
#135140=CARTESIAN_POINT('Ctrl Pts',(22.8741446509117,-0.238492231703882,
-6.47033922117249));
#135141=CARTESIAN_POINT('Ctrl Pts',(22.751516819588,-0.320007256122885,
-6.47715656516353));
#135142=CARTESIAN_POINT('Ctrl Pts',(22.6967491804622,-0.351744659790034,
-6.48008594248547));
#135143=CARTESIAN_POINT('Ctrl Pts',(22.5987738286207,-0.400744765220158,
-6.48530562827809));
#135144=CARTESIAN_POINT('Ctrl Pts',(22.5564481505334,-0.419582183915144,
-6.48755363697606));
#135145=CARTESIAN_POINT('Ctrl Pts',(22.4862438984667,-0.44711390931647,
-6.49131211381761));
#135146=CARTESIAN_POINT('Ctrl Pts',(22.4588522655957,-0.456971317445483,
-6.49278541236058));
#135147=CARTESIAN_POINT('Ctrl Pts',(22.4024372406223,-0.475488361222527,
-6.49584106219699));
#135148=CARTESIAN_POINT('Ctrl Pts',(22.3734050104377,-0.484079983098811,
-6.49742475536692));
#135149=CARTESIAN_POINT('Ctrl Pts',(22.2903762349551,-0.506016376353173,
-6.50199043079261));
#135150=CARTESIAN_POINT('Ctrl Pts',(22.2358883509165,-0.517302952110055,
-6.50503133700028));
#135151=CARTESIAN_POINT('Ctrl Pts',(22.0875172306779,-0.539759982591068,
-6.51340338646219));
#135152=CARTESIAN_POINT('Ctrl Pts',(21.9930209423237,-0.545289469972139,
-6.51884309799928));
#135153=CARTESIAN_POINT('Ctrl Pts',(21.8666520621711,-0.541079243741303,
-6.52596583927362));
#135154=CARTESIAN_POINT('Ctrl Pts',(21.8347231308639,-0.539020315515715,
-6.52775079035233));
#135155=CARTESIAN_POINT('Ctrl Pts',(21.7782637085599,-0.533612460159687,
-6.53085755966035));
#135156=CARTESIAN_POINT('Ctrl Pts',(21.7537062659276,-0.530663068646278,
-6.53219208194916));
#135157=CARTESIAN_POINT('Ctrl Pts',(21.7131803188534,-0.524804379576196,
-6.53435528675913));
#135158=CARTESIAN_POINT('Ctrl Pts',(21.6971690217876,-0.522231427441526,
-6.53519932508586));
#135159=CARTESIAN_POINT('Ctrl Pts',(21.660404585231,-0.515727371555119,
-6.5371117777072));
#135160=CARTESIAN_POINT('Ctrl Pts',(21.6396865464047,-0.511621848385371,
-6.53817174118872));
#135161=CARTESIAN_POINT('Ctrl Pts',(21.5286161950409,-0.487231967237438,
-6.54378841661526));
#135162=CARTESIAN_POINT('Ctrl Pts',(21.4401370515953,-0.459269019950006,
-6.54803512904835));
#135163=CARTESIAN_POINT('Ctrl Pts',(21.299853908761,-0.400604312704793,
-6.5550781790296));
#135164=CARTESIAN_POINT('Ctrl Pts',(21.2463866893962,-0.374521838360011,
-6.55784138945292));
#135165=CARTESIAN_POINT('Ctrl Pts',(21.1555814175104,-0.323535564518975,
-6.56281568134926));
#135166=CARTESIAN_POINT('Ctrl Pts',(21.1175755322744,-0.29996783600625,
-6.56499082150684));
#135167=CARTESIAN_POINT('Ctrl Pts',(21.0567744575371,-0.258503943642658,
-6.56866413327037));
#135168=CARTESIAN_POINT('Ctrl Pts',(21.0333640765504,-0.241556480562992,
-6.57012883332864));
#135169=CARTESIAN_POINT('Ctrl Pts',(20.9861674288754,-0.205326705468321,
-6.57319467015804));
#135170=CARTESIAN_POINT('Ctrl Pts',(20.9624516782821,-0.185973792134488,
-6.5747980796891));
#135171=CARTESIAN_POINT('Ctrl Pts',(20.895069857232,-0.127564665502109,
-6.57954622892622));
#135172=CARTESIAN_POINT('Ctrl Pts',(20.8530358759571,-0.0867144713952817,
-6.58275842908974));
#135173=CARTESIAN_POINT('Ctrl Pts',(20.7430205123819,0.0331045016887321,
-6.59185976021977));
#135174=CARTESIAN_POINT('Ctrl Pts',(20.680557511281,0.116710214052071,-6.59788082635173));
#135175=CARTESIAN_POINT('Ctrl Pts',(20.6087931150197,0.236283153847814,
-6.60566015045069));
#135176=CARTESIAN_POINT('Ctrl Pts',(20.591643457666,0.267219581433107,-6.60760327755508));
#135177=CARTESIAN_POINT('Ctrl Pts',(20.5675643604903,0.314411850406251,
-6.61043679718368));
#135178=CARTESIAN_POINT('Ctrl Pts',(20.5598266162508,0.330240764197565,
-6.61136590244031));
#135179=CARTESIAN_POINT('Ctrl Pts',(20.5447766746547,0.362413239865487,
-6.61320664452485));
#135180=CARTESIAN_POINT('Ctrl Pts',(20.5374744452525,0.378758434017095,
-6.61411771979798));
#135181=CARTESIAN_POINT('Ctrl Pts',(20.5158367981773,0.429547049152643,
-6.61688547626871));
#135182=CARTESIAN_POINT('Ctrl Pts',(20.5024640578692,0.464387549626548,
-6.61869595346582));
#135183=CARTESIAN_POINT('Ctrl Pts',(20.4701373990076,0.558697423726744,
-6.62344523994509));
#135184=CARTESIAN_POINT('Ctrl Pts',(20.4535053242237,0.618889071572606,
-6.62632157129356));
#135185=CARTESIAN_POINT('Ctrl Pts',(20.4233668602429,0.761018257768411,
-6.63304964922663));
#135186=CARTESIAN_POINT('Ctrl Pts',(20.4127347180812,0.843362645664008,
-6.63690553919466));
#135187=CARTESIAN_POINT('Ctrl Pts',(20.407091732587,0.961142571795386,-6.64264953999652));
#135188=CARTESIAN_POINT('Ctrl Pts',(20.4066073242446,0.996172655188285,
-6.64438506069481));
#135189=CARTESIAN_POINT('Ctrl Pts',(20.4078823562372,1.05924206190599,-6.6475741616009));
#135190=CARTESIAN_POINT('Ctrl Pts',(20.4092146679806,1.08727474894511,-6.64901452110638));
#135191=CARTESIAN_POINT('Ctrl Pts',(20.4139627268901,1.15066308713468,-6.65232904425536));
#135192=CARTESIAN_POINT('Ctrl Pts',(20.4178362778303,1.18596757428787,-6.6542159832979));
#135193=CARTESIAN_POINT('Ctrl Pts',(20.4287909704093,1.26162675880698,-6.65835021399949));
#135194=CARTESIAN_POINT('Ctrl Pts',(20.4362682724006,1.30189632250002,-6.66060693363008));
#135195=CARTESIAN_POINT('Ctrl Pts',(20.4671266317164,1.43773259514078,-6.66839158565604));
#135196=CARTESIAN_POINT('Ctrl Pts',(20.4980349893845,1.53133745335054,-6.67406684576527));
#135197=CARTESIAN_POINT('Ctrl Pts',(20.5533792694773,1.6571355467828,-6.68177795249405));
#135198=CARTESIAN_POINT('Ctrl Pts',(20.5704727173108,1.69230155551479,-6.68394077780806));
#135199=CARTESIAN_POINT('Ctrl Pts',(20.5977766696573,1.74343631298846,-6.6870594387879));
#135200=CARTESIAN_POINT('Ctrl Pts',(20.6069745156197,1.75992637711794,-6.68806087354461));
#135201=CARTESIAN_POINT('Ctrl Pts',(20.6249894061157,1.7908745519929,-6.68992626393878));
#135202=CARTESIAN_POINT('Ctrl Pts',(20.6337459161862,1.80536378700923,-6.6907930348651));
#135203=CARTESIAN_POINT('Ctrl Pts',(20.6590573462398,1.84573024410616,-6.6931966369645));
#135204=CARTESIAN_POINT('Ctrl Pts',(20.6761498403642,1.8712626251278,-6.69470404293512));
#135205=CARTESIAN_POINT('Ctrl Pts',(20.7199058994271,1.93258111984863,-6.69833371665423));
#135206=CARTESIAN_POINT('Ctrl Pts',(20.7473813800819,1.96775401116228,-6.70042440363885));
#135207=CARTESIAN_POINT('Ctrl Pts',(20.8533343207297,2.09189681237628,-6.70801304148536));
#135208=CARTESIAN_POINT('Ctrl Pts',(20.9404625637073,2.17292247844536,-6.71342017695837));
#135209=CARTESIAN_POINT('Ctrl Pts',(21.0621458576958,2.26238519948046,-6.72083468934783));
#135210=CARTESIAN_POINT('Ctrl Pts',(21.0888801661886,2.2807707908411,-6.72245357899984));
#135211=CARTESIAN_POINT('Ctrl Pts',(21.139972488864,2.31358460660175,-6.72554071388244));
#135212=CARTESIAN_POINT('Ctrl Pts',(21.1641867323002,2.32821175374242,-6.72700107400664));
#135213=CARTESIAN_POINT('Ctrl Pts',(21.2229884635093,2.36156128605233,-6.73054630594845));
#135214=CARTESIAN_POINT('Ctrl Pts',(21.2579152940554,2.37964246114793,-6.7326514923484));
#135215=CARTESIAN_POINT('Ctrl Pts',(21.3369800858114,2.41681501954508,-6.73741595938099));
#135216=CARTESIAN_POINT('Ctrl Pts',(21.3813963494781,2.43521691975713,-6.74009216476792));
#135217=CARTESIAN_POINT('Ctrl Pts',(21.5073782212088,2.48064485645767,-6.74764416940453));
#135218=CARTESIAN_POINT('Ctrl Pts',(21.5904489791571,2.50297906165908,-6.75258739415442));
#135219=CARTESIAN_POINT('Ctrl Pts',(21.7122856226903,2.5250511234118,-6.75951541783196));
#135220=CARTESIAN_POINT('Ctrl Pts',(21.7498650751572,2.53043635240697,-6.76160765623574));
#135221=CARTESIAN_POINT('Ctrl Pts',(21.8054988143049,2.5363242221215,-6.76460536335205));
#135222=CARTESIAN_POINT('Ctrl Pts',(21.823423168918,2.53790476624975,-6.76555599408177));
#135223=CARTESIAN_POINT('Ctrl Pts',(21.8588668545299,2.54040623025768,-6.76740050787923));
#135224=CARTESIAN_POINT('Ctrl Pts',(21.8763822221601,2.54134261800288,-6.76829490683412));
#135225=CARTESIAN_POINT('Ctrl Pts',(21.9287134532859,2.54324617143663,-6.77092569723392));
#135226=CARTESIAN_POINT('Ctrl Pts',(21.9635516264176,2.54333356821809,-6.77262250926825));
#135227=CARTESIAN_POINT('Ctrl Pts',(22.1068607274314,2.53883938259562,-6.77947949458667));
#135228=CARTESIAN_POINT('Ctrl Pts',(22.2146981090058,2.52399774847878,-6.78436947284413));
#135229=CARTESIAN_POINT('Ctrl Pts',(22.3745615522837,2.48450154673247,-6.79212242091079));
#135230=CARTESIAN_POINT('Ctrl Pts',(22.4282556192527,2.4680831789754,-6.79481301565766));
#135231=CARTESIAN_POINT('Ctrl Pts',(22.5094076935878,2.43834337153749,-6.79909154459208));
#135232=CARTESIAN_POINT('Ctrl Pts',(22.5375664105778,2.42707189056893,-6.8006166790024));
#135233=CARTESIAN_POINT('Ctrl Pts',(22.5920213244423,2.40338946713281,-6.80365531411678));
#135234=CARTESIAN_POINT('Ctrl Pts',(22.6183350435291,2.39105050305001,-6.80516601174385));
#135235=CARTESIAN_POINT('Ctrl Pts',(22.6765353482745,2.36172669227281,-6.80860798388125));
#135236=CARTESIAN_POINT('Ctrl Pts',(22.708204780748,2.3443505645048,-6.81055134782412));
#135237=CARTESIAN_POINT('Ctrl Pts',(22.7912818291088,2.29489871651529,-6.81583963967357));
#135238=CARTESIAN_POINT('Ctrl Pts',(22.8414566079082,2.26088142700837,-6.81923966280967));
#135239=CARTESIAN_POINT('Ctrl Pts',(22.8894991487533,2.22400584557124,-6.82267583049642));
#135240=CARTESIAN_POINT('Ctrl Pts',(22.8894916066884,2.22401163452936,-6.78051560659813));
#135241=CARTESIAN_POINT('Ctrl Pts',(22.8840931829709,2.22815520125885,-6.78013331794407));
#135242=CARTESIAN_POINT('Ctrl Pts',(22.8786669161915,2.23226338446389,-6.77975186021311));
#135243=CARTESIAN_POINT('Ctrl Pts',(22.8518487668555,2.2522893892527,-6.77788090947732));
#135244=CARTESIAN_POINT('Ctrl Pts',(22.830073521286,2.2676871181595,-6.77640617520325));
#135245=CARTESIAN_POINT('Ctrl Pts',(22.7897835548849,2.29463821236672,-6.77377117239461));
#135246=CARTESIAN_POINT('Ctrl Pts',(22.7714018742259,2.30637803644346,-6.77260286395183));
#135247=CARTESIAN_POINT('Ctrl Pts',(22.7389786896359,2.3261307014459,-6.77060845819639));
#135248=CARTESIAN_POINT('Ctrl Pts',(22.7250504636334,2.33431885929378,-6.76977300307344));
#135249=CARTESIAN_POINT('Ctrl Pts',(22.6899501003446,2.35421860565912,-6.76771819252665));
#135250=CARTESIAN_POINT('Ctrl Pts',(22.6686269459659,2.36565354765244,-6.76651389728743));
#135251=CARTESIAN_POINT('Ctrl Pts',(22.5407643180451,2.43039771643578,-6.75949987971156));
#135252=CARTESIAN_POINT('Ctrl Pts',(22.4286034762515,2.47172818012277,-6.75415828547375));
#135253=CARTESIAN_POINT('Ctrl Pts',(22.2706083637621,2.5099480869076,-6.74654133461936));
#135254=CARTESIAN_POINT('Ctrl Pts',(22.2280104735494,2.51836848209117,-6.74448249074873));
#135255=CARTESIAN_POINT('Ctrl Pts',(22.1486955342246,2.53059695792077,-6.74059127163562));
#135256=CARTESIAN_POINT('Ctrl Pts',(22.1120876658938,2.53490530697078,-6.73877304185693));
#135257=CARTESIAN_POINT('Ctrl Pts',(22.0473899727701,2.54017915697149,-6.73550200032558));
#135258=CARTESIAN_POINT('Ctrl Pts',(22.0193619581218,2.54169563633919,-6.73406611077397));
#135259=CARTESIAN_POINT('Ctrl Pts',(21.9575124536453,2.5433520677348,-6.73085020387539));
#135260=CARTESIAN_POINT('Ctrl Pts',(21.9236969047742,2.54314612563261,-6.72906071477139));
#135261=CARTESIAN_POINT('Ctrl Pts',(21.7713623908797,2.53720985684749,-6.72085285723711));
#135262=CARTESIAN_POINT('Ctrl Pts',(21.6537480387357,2.51893167321256,-6.71407409434332));
#135263=CARTESIAN_POINT('Ctrl Pts',(21.498863030427,2.47617536862273,-6.70494939127576));
#135264=CARTESIAN_POINT('Ctrl Pts',(21.458789916911,2.46332881297855,-6.7025746245593));
#135265=CARTESIAN_POINT('Ctrl Pts',(21.3914977318376,2.43868006049563,-6.69861050217562));
#135266=CARTESIAN_POINT('Ctrl Pts',(21.3640020083109,2.42770152835382,-6.6969978915552));
#135267=CARTESIAN_POINT('Ctrl Pts',(21.3214649612704,2.40928115321159,-6.69453224843813));
#135268=CARTESIAN_POINT('Ctrl Pts',(21.306200696785,2.40237377604644,-6.69365363547436));
#135269=CARTESIAN_POINT('Ctrl Pts',(21.2737187776936,2.38703285237926,-6.69180118471747));
#135270=CARTESIAN_POINT('Ctrl Pts',(21.256540224098,2.37852458449533,-6.69083130454782));
#135271=CARTESIAN_POINT('Ctrl Pts',(21.2031676882277,2.35083971776745,-6.68783582185984));
#135272=CARTESIAN_POINT('Ctrl Pts',(21.1675743567698,2.33054010600596,-6.6858642297926));
#135273=CARTESIAN_POINT('Ctrl Pts',(21.0611400029486,2.26408844206428,-6.67992892815794));
#135274=CARTESIAN_POINT('Ctrl Pts',(20.9932480484945,2.21351481213039,-6.67607947826741));
#135275=CARTESIAN_POINT('Ctrl Pts',(20.8809964866106,2.1145934459105,-6.6690874217422));
#135276=CARTESIAN_POINT('Ctrl Pts',(20.8349311676575,2.068507187801,-6.66599421617396));
#135277=CARTESIAN_POINT('Ctrl Pts',(20.7712728118056,1.99620637292017,-6.66124461787238));
#135278=CARTESIAN_POINT('Ctrl Pts',(20.7513470972283,1.97213989531612,-6.6596794543379));
#135279=CARTESIAN_POINT('Ctrl Pts',(20.7146269435313,1.92494233273732,-6.65662929477761));
#135280=CARTESIAN_POINT('Ctrl Pts',(20.6977177555909,1.90191682112566,-6.65514953412702));
#135281=CARTESIAN_POINT('Ctrl Pts',(20.6574383238106,1.84374964845012,-6.65142624429221));
#135282=CARTESIAN_POINT('Ctrl Pts',(20.6348530691273,1.80809484780244,-6.64915642623132));
#135283=CARTESIAN_POINT('Ctrl Pts',(20.5569865088252,1.6732403373715,-6.64061941759587));
#135284=CARTESIAN_POINT('Ctrl Pts',(20.5112432376026,1.56895840254702,-6.63407846001082));
#135285=CARTESIAN_POINT('Ctrl Pts',(20.467180058202,1.42808431637099,-6.62574395041717));
#135286=CARTESIAN_POINT('Ctrl Pts',(20.4580841195376,1.39521938524899,-6.62383600647422));
#135287=CARTESIAN_POINT('Ctrl Pts',(20.4440281814812,1.33699250020193,-6.62054676086045));
#135288=CARTESIAN_POINT('Ctrl Pts',(20.438602324927,1.31175675253409,-6.61915070769246));
#135289=CARTESIAN_POINT('Ctrl Pts',(20.4308156970049,1.27053406387355,-6.6169304188676));
#135290=CARTESIAN_POINT('Ctrl Pts',(20.428068587813,1.25462614839134,-6.61608833984631));
#135291=CARTESIAN_POINT('Ctrl Pts',(20.4223782303219,1.21828175639506,-6.61419997008572));
#135292=CARTESIAN_POINT('Ctrl Pts',(20.4195945534745,1.19782427487334,-6.61316136543443));
#135293=CARTESIAN_POINT('Ctrl Pts',(20.4103699967504,1.11808425446866,-6.6091869222361));
#135294=CARTESIAN_POINT('Ctrl Pts',(20.4069565145037,1.05850030743707,-6.60637404577534));
#135295=CARTESIAN_POINT('Ctrl Pts',(20.4070878771545,0.879979125521468,
-6.59805821849222));
#135296=CARTESIAN_POINT('Ctrl Pts',(20.4209139176431,0.761509420213065,
-6.59265579470078));
#135297=CARTESIAN_POINT('Ctrl Pts',(20.4559557337416,0.612932441158596,
-6.58519450407706));
#135298=CARTESIAN_POINT('Ctrl Pts',(20.4647846174834,0.580327949192161,
-6.58351596820535));
#135299=CARTESIAN_POINT('Ctrl Pts',(20.4828917995404,0.521220934336388,
-6.5803833676819));
#135300=CARTESIAN_POINT('Ctrl Pts',(20.4918373460953,0.494631410075126,
-6.57894008721395));
#135301=CARTESIAN_POINT('Ctrl Pts',(20.5141995513575,0.433710413910999,
-6.57554834688385));
#135302=CARTESIAN_POINT('Ctrl Pts',(20.5281310980393,0.399587342221404,
-6.5735843877792));
#135303=CARTESIAN_POINT('Ctrl Pts',(20.5611066216066,0.326420996188346,
-6.56923008950995));
#135304=CARTESIAN_POINT('Ctrl Pts',(20.5806045083557,0.287617317350972,
-6.56682785975829));
#135305=CARTESIAN_POINT('Ctrl Pts',(20.6597049123616,0.1454759886516,-6.55770389375578));
#135306=CARTESIAN_POINT('Ctrl Pts',(20.7295823956875,0.0483421189603384,
-6.55076608976156));
#135307=CARTESIAN_POINT('Ctrl Pts',(20.8261911071129,-0.0575839008484547,
-6.54292385490149));
#135308=CARTESIAN_POINT('Ctrl Pts',(20.8428511354534,-0.0750123930301116,
-6.54162466241861));
#135309=CARTESIAN_POINT('Ctrl Pts',(20.8713413936361,-0.103451576259399,
-6.53950005581383));
#135310=CARTESIAN_POINT('Ctrl Pts',(20.882947502136,-0.114678785293956,
-6.53866050857244));
#135311=CARTESIAN_POINT('Ctrl Pts',(20.9106741103289,-0.140670152489015,
-6.53671559668221));
#135312=CARTESIAN_POINT('Ctrl Pts',(20.9269356295874,-0.15527749260217,
-6.53562031896456));
#135313=CARTESIAN_POINT('Ctrl Pts',(20.963775794222,-0.186981991820656,
-6.53322419177594));
#135314=CARTESIAN_POINT('Ctrl Pts',(20.9844999103353,-0.203899549018343,
-6.53193256269565));
#135315=CARTESIAN_POINT('Ctrl Pts',(21.054763183386,-0.258275061804536,
-6.52769968262103));
#135316=CARTESIAN_POINT('Ctrl Pts',(21.1061234807423,-0.293281901160238,
-6.5248362596312));
#135317=CARTESIAN_POINT('Ctrl Pts',(21.2310655043174,-0.367821419251677,
-6.51809965527141));
#135318=CARTESIAN_POINT('Ctrl Pts',(21.3060179359046,-0.404666552556696,
-6.51422243412655));
#135319=CARTESIAN_POINT('Ctrl Pts',(21.416153512383,-0.448131064296362,
-6.50845502411498));
#135320=CARTESIAN_POINT('Ctrl Pts',(21.4491582203328,-0.459874289426101,
-6.50671969329122));
#135321=CARTESIAN_POINT('Ctrl Pts',(21.5092427555379,-0.478975188539539,
-6.50353255105917));
#135322=CARTESIAN_POINT('Ctrl Pts',(21.5361782121453,-0.48673668019922,
-6.50209400370346));
#135323=CARTESIAN_POINT('Ctrl Pts',(21.5975933806693,-0.502635276219801,
-6.498786420574));
#135324=CARTESIAN_POINT('Ctrl Pts',(21.6321711152116,-0.510327030653523,
-6.49690474642806));
#135325=CARTESIAN_POINT('Ctrl Pts',(21.7070880248085,-0.524305528313742,
-6.49278423021513));
#135326=CARTESIAN_POINT('Ctrl Pts',(21.7474736554734,-0.530194861139748,
-6.49053608178524));
#135327=CARTESIAN_POINT('Ctrl Pts',(21.8849570246883,-0.544705579414959,
-6.48281215151114));
#135328=CARTESIAN_POINT('Ctrl Pts',(21.9826160321093,-0.545729839865223,
-6.47719181880399));
#135329=CARTESIAN_POINT('Ctrl Pts',(22.119445509224,-0.53418606024692,-6.46948177352854));
#135330=CARTESIAN_POINT('Ctrl Pts',(22.1590326063599,-0.529295396342859,
-6.46727346182807));
#135331=CARTESIAN_POINT('Ctrl Pts',(22.2171500931561,-0.51981617261752,
-6.46410375767297));
#135332=CARTESIAN_POINT('Ctrl Pts',(22.2358549284144,-0.516409375835991,
-6.46309486077475));
#135333=CARTESIAN_POINT('Ctrl Pts',(22.2710413790207,-0.509326462490085,
-6.46122427240631));
#135334=CARTESIAN_POINT('Ctrl Pts',(22.2875341176328,-0.505723967756331,
-6.46035947151717));
#135335=CARTESIAN_POINT('Ctrl Pts',(22.3334753671109,-0.494896276698613,
-6.45797691954056));
#135336=CARTESIAN_POINT('Ctrl Pts',(22.3627762470728,-0.487072361160386,
-6.45648757275791));
#135337=CARTESIAN_POINT('Ctrl Pts',(22.4336930571506,-0.465878281295291,
-6.45291725494369));
#135338=CARTESIAN_POINT('Ctrl Pts',(22.4750085545412,-0.451593759290283,
-6.45086637768186));
#135339=CARTESIAN_POINT('Ctrl Pts',(22.6213211387481,-0.393941787310652,
-6.44354608404348));
#135340=CARTESIAN_POINT('Ctrl Pts',(22.7220534181049,-0.340775273734657,
-6.43836812109678));
#135341=CARTESIAN_POINT('Ctrl Pts',(22.8445642454575,-0.257692989729819,
-6.43114461131943));
#135342=CARTESIAN_POINT('Ctrl Pts',(22.8724315858372,-0.237399128054494,
-6.42943411332381));
#135343=CARTESIAN_POINT('Ctrl Pts',(22.921732874008,-0.198904935814554,
-6.42626810994936));
#135344=CARTESIAN_POINT('Ctrl Pts',(22.9433937173593,-0.181019312596473,
-6.42482465495505));
#135345=CARTESIAN_POINT('Ctrl Pts',(22.9918147952299,-0.138762512766051,
-6.4214696779132));
#135346=CARTESIAN_POINT('Ctrl Pts',(23.0182291685037,-0.114021676901523,
-6.41954409982678));
#135347=CARTESIAN_POINT('Ctrl Pts',(23.1112963858827,-0.0204951197811365,
-6.41239742905592));
#135348=CARTESIAN_POINT('Ctrl Pts',(23.1723720004862,0.0535208882474469,
-6.40697078512297));
#135349=CARTESIAN_POINT('Ctrl Pts',(23.266729171269,0.192364277332073,-6.39741470329425));
#135350=CARTESIAN_POINT('Ctrl Pts',(23.3030397516549,0.254791455240788,
-6.39331263114128));
#135351=CARTESIAN_POINT('Ctrl Pts',(23.3447720161121,0.33972276701939,-6.38815846847536));
#135352=CARTESIAN_POINT('Ctrl Pts',(23.3542504995107,0.360128422700714,
-6.38695102416488));
#135353=CARTESIAN_POINT('Ctrl Pts',(23.3697307558064,0.395457295352428,
-6.38492179943724));
#135354=CARTESIAN_POINT('Ctrl Pts',(23.3759510206594,0.410278855129356,
-6.38408911225237));
#135355=CARTESIAN_POINT('Ctrl Pts',(23.3905706399993,0.446698980537339,
-6.38208737200271));
#135356=CARTESIAN_POINT('Ctrl Pts',(23.3987169996827,0.468393993728911,
-6.38093133740976));
#135357=CARTESIAN_POINT('Ctrl Pts',(23.4159974082986,0.517766152213794,
-6.37836517799455));
#135358=CARTESIAN_POINT('Ctrl Pts',(23.424842325753,0.545535327396278,-6.3769667417294));
#135359=CARTESIAN_POINT('Ctrl Pts',(23.4536527927569,0.645715557503674,
-6.3720299703545));
#135360=CARTESIAN_POINT('Ctrl Pts',(23.4691131058387,0.719312849991645,
-6.36859809863064));
#135361=CARTESIAN_POINT('Ctrl Pts',(23.4890770279367,0.867323398095032,
-6.36166190593236));
#135362=CARTESIAN_POINT('Ctrl Pts',(23.493677344455,0.941517396790919,-6.35816691881182));
#135363=CARTESIAN_POINT('Ctrl Pts',(23.492593171557,1.04772775196917,-6.35294902417737));
#135364=CARTESIAN_POINT('Ctrl Pts',(23.491272705243,1.07968628112634,-6.35135210632943));
#135365=CARTESIAN_POINT('Ctrl Pts',(23.4869255573007,1.13964435966628,-6.34829442666829));
#135366=CARTESIAN_POINT('Ctrl Pts',(23.4841235401043,1.16764709644041,-6.34684095963345));
#135367=CARTESIAN_POINT('Ctrl Pts',(23.4755561461554,1.23470133033093,-6.34329421128866));
#135368=CARTESIAN_POINT('Ctrl Pts',(23.4690551312463,1.27363739727861,-6.34117995530574));
#135369=CARTESIAN_POINT('Ctrl Pts',(23.4512609260417,1.35974065703618,-6.33638189067511));
#135370=CARTESIAN_POINT('Ctrl Pts',(23.4392225156365,1.40671058667802,-6.33368046478458));
#135371=CARTESIAN_POINT('Ctrl Pts',(23.3916706808293,1.56153063553269,-6.32454017074507));
#135372=CARTESIAN_POINT('Ctrl Pts',(23.3464779068928,1.66601881761278,-6.31795334965074));
#135373=CARTESIAN_POINT('Ctrl Pts',(23.2797017797471,1.78306697197067,-6.31063222170074));
#135374=CARTESIAN_POINT('Ctrl Pts',(23.2687885574923,1.8013098857123,-6.30949397324053));
#135375=CARTESIAN_POINT('Ctrl Pts',(23.248926102489,1.83300704257971,-6.30752898423778));
#135376=CARTESIAN_POINT('Ctrl Pts',(23.2401371351826,1.84655534405131,-6.30669397812446));
#135377=CARTESIAN_POINT('Ctrl Pts',(23.2176015009986,1.8801278980579,-6.30463477886682));
#135378=CARTESIAN_POINT('Ctrl Pts',(23.2035921619174,1.89996971688336,-6.30342586172547));
#135379=CARTESIAN_POINT('Ctrl Pts',(23.1705709844292,1.94447038942134,-6.30071400387885));
#135380=CARTESIAN_POINT('Ctrl Pts',(23.151269405167,1.96890134786215,-6.29922474256441));
#135381=CARTESIAN_POINT('Ctrl Pts',(23.0748138740875,2.05987491672823,-6.29361215898745));
#135382=CARTESIAN_POINT('Ctrl Pts',(23.0127639054047,2.12208500635517,-6.2896225304504));
#135383=CARTESIAN_POINT('Ctrl Pts',(22.9273581178032,2.19423640340638,-6.28438459941712));
#135384=CARTESIAN_POINT('Ctrl Pts',(22.9085955731876,2.20934836206942,-6.28324848751454));
#135385=CARTESIAN_POINT('Ctrl Pts',(22.8894915905204,2.22401164693913,-6.28210119346687));
#135386=CARTESIAN_POINT('Origin',(21.9499999789786,0.999999999999992,-6.00000000000001));
#135387=CARTESIAN_POINT('',(20.6853192846384,1.00091784636197,-6.44310594448828));
#135388=CARTESIAN_POINT('Ctrl Pts',(22.3906686064029,-0.185465307624328,
-6.28967669732482));
#135389=CARTESIAN_POINT('Ctrl Pts',(22.3471104093517,-0.201760426698602,
-6.29243744842554));
#135390=CARTESIAN_POINT('Ctrl Pts',(22.3026975844951,-0.215616979717695,
-6.29522313617549));
#135391=CARTESIAN_POINT('Ctrl Pts',(22.2577300141014,-0.226935083304443,
-6.29808537729643));
#135392=CARTESIAN_POINT('Ctrl Pts',(22.2546229511194,-0.227717114896844,
-6.29828314567384));
#135393=CARTESIAN_POINT('Ctrl Pts',(22.2515132255729,-0.228487042529604,
-6.2984812795329));
#135394=CARTESIAN_POINT('Ctrl Pts',(22.2484009299199,-0.229244839827862,
-6.29867979590079));
#135395=CARTESIAN_POINT('Ctrl Pts',(22.234150207789,-0.232714676865598,
-6.29958877175418));
#135396=CARTESIAN_POINT('Ctrl Pts',(22.2198461265754,-0.23593014822109,
-6.3005058046491));
#135397=CARTESIAN_POINT('Ctrl Pts',(22.2054985961248,-0.238888984456219,
-6.30143257033421));
#135398=CARTESIAN_POINT('Ctrl Pts',(22.20548208595,-0.238892389286325,-6.30143363679394));
#135399=CARTESIAN_POINT('Ctrl Pts',(22.2054655757175,-0.238895793776658,
-6.30143470326657));
#135400=CARTESIAN_POINT('Ctrl Pts',(22.2054490654275,-0.238899197927225,
-6.30143576975208));
#135401=CARTESIAN_POINT('Ctrl Pts',(22.1604907218272,-0.24816886980053,
-6.30433986302597));
#135402=CARTESIAN_POINT('Ctrl Pts',(22.1149403822828,-0.254945368919111,
-6.30734688179163));
#135403=CARTESIAN_POINT('Ctrl Pts',(22.0690965134344,-0.259196302886019,
-6.31039772755901));
#135404=CARTESIAN_POINT('Ctrl Pts',(22.0641721363121,-0.259652922331561,
-6.3107254380136));
#135405=CARTESIAN_POINT('Ctrl Pts',(22.0592444169884,-0.260080422701723,
-6.31105365415526));
#135406=CARTESIAN_POINT('Ctrl Pts',(22.0543137570268,-0.260478780285977,
-6.31138230273755));
#135407=CARTESIAN_POINT('Ctrl Pts',(22.0048946868554,-0.264471442842854,
-6.31467628518133));
#135408=CARTESIAN_POINT('Ctrl Pts',(21.9551747105688,-0.265534638531312,
-6.31801315904949));
#135409=CARTESIAN_POINT('Ctrl Pts',(21.905520136309,-0.263674160723438,
-6.3213342091162));
#135410=CARTESIAN_POINT('Ctrl Pts',(21.8559117159873,-0.261815412230112,
-6.32465217226612));
#135411=CARTESIAN_POINT('Ctrl Pts',(21.8063684946944,-0.257038727270444,
-6.32795404769888));
#135412=CARTESIAN_POINT('Ctrl Pts',(21.7572474127023,-0.249386952654866,
-6.33120269555329));
#135413=CARTESIAN_POINT('Ctrl Pts',(21.7081515065201,-0.241739099769335,
-6.33444967839266));
#135414=CARTESIAN_POINT('Ctrl Pts',(21.6594772769829,-0.231219180125691,
-6.3376433932741));
#135415=CARTESIAN_POINT('Ctrl Pts',(21.611573671104,-0.217904261974882,
-6.34077099162547));
#135416=CARTESIAN_POINT('Ctrl Pts',(21.5611704791935,-0.203894578100078,
-6.34406178648382));
#135417=CARTESIAN_POINT('Ctrl Pts',(21.5116205713624,-0.18679016275,-6.34727920537245));
#135418=CARTESIAN_POINT('Ctrl Pts',(21.4633212996666,-0.166721911367082,
-6.35043760878328));
#135419=CARTESIAN_POINT('Ctrl Pts',(21.4173767827947,-0.147632055932856,
-6.35344202921658));
#135420=CARTESIAN_POINT('Ctrl Pts',(21.3725640158992,-0.125860400443001,
-6.35639347018246));
#135421=CARTESIAN_POINT('Ctrl Pts',(21.3292155495703,-0.101557407831931,
-6.35932754013549));
#135422=CARTESIAN_POINT('Ctrl Pts',(21.2858407634226,-0.0772396592117836,
-6.36226339156306));
#135423=CARTESIAN_POINT('Ctrl Pts',(21.243932377574,-0.0503871474844555,
-6.36518226420441));
#135424=CARTESIAN_POINT('Ctrl Pts',(21.2038107755342,-0.0211918718241275,
-6.36813788253618));
#135425=CARTESIAN_POINT('Ctrl Pts',(21.1667726819221,0.00575962806526852,
-6.37086634956861));
#135426=CARTESIAN_POINT('Ctrl Pts',(21.1312570442013,0.0347080777191685,
-6.37362671885412));
#135427=CARTESIAN_POINT('Ctrl Pts',(21.0975026667503,0.0654651437902246,
-6.37646898484549));
#135428=CARTESIAN_POINT('Ctrl Pts',(21.0946320745128,0.0680808340140638,
-6.37671070124815));
#135429=CARTESIAN_POINT('Ctrl Pts',(21.0917741894305,0.0707096087900683,
-6.37695300996106));
#135430=CARTESIAN_POINT('Ctrl Pts',(21.0889291411323,0.0733513549243375,
-6.37719594173426));
#135431=CARTESIAN_POINT('Ctrl Pts',(21.0834768458455,0.0784140387480052,
-6.37766150000366));
#135432=CARTESIAN_POINT('Ctrl Pts',(21.0780717819019,0.083524250400563,
-6.37812935236638));
#135433=CARTESIAN_POINT('Ctrl Pts',(21.0727149191585,0.088681075410001,
-6.37859971721835));
#135434=CARTESIAN_POINT('Ctrl Pts',(21.0727027152255,0.0886928236197154,
-6.37860078879726));
#135435=CARTESIAN_POINT('Ctrl Pts',(21.0726905115426,0.0887045720713643,
-6.37860186038921));
#135436=CARTESIAN_POINT('Ctrl Pts',(21.0726783081099,0.088716320764919,
-6.3786029319942));
#135437=CARTESIAN_POINT('Ctrl Pts',(21.0400053868558,0.120171743909859,
-6.38147199895402));
#135438=CARTESIAN_POINT('Ctrl Pts',(21.0090029359217,0.15349050789987,-6.38444249757833));
#135439=CARTESIAN_POINT('Ctrl Pts',(20.9798665486039,0.188451002708149,
-6.387456984648));
#135440=CARTESIAN_POINT('Ctrl Pts',(20.9776674710995,0.191089656458805,
-6.38768450395676));
#135441=CARTESIAN_POINT('Ctrl Pts',(20.9754790263654,0.193737637925406,
-6.3879122738466));
#135442=CARTESIAN_POINT('Ctrl Pts',(20.9733012995092,0.196394839864987,
-6.38814026962001));
#135443=CARTESIAN_POINT('Ctrl Pts',(20.9423131839197,0.234205679463701,
-6.39138455131693));
#135444=CARTESIAN_POINT('Ctrl Pts',(20.913494205518,0.273888825683377,-6.3946739912619));
#135445=CARTESIAN_POINT('Ctrl Pts',(20.887045626256,0.315148386127671,-6.39795100572697));
#135446=CARTESIAN_POINT('Ctrl Pts',(20.8606219175173,0.356369148765442,
-6.40122493870083));
#135447=CARTESIAN_POINT('Ctrl Pts',(20.8365638887051,0.399163211076456,
-6.40448617352742));
#135448=CARTESIAN_POINT('Ctrl Pts',(20.815036381223,0.443220424278687,-6.40769730950366));
#135449=CARTESIAN_POINT('Ctrl Pts',(20.79350913539,0.487277102001824,-6.41090840645119));
#135450=CARTESIAN_POINT('Ctrl Pts',(20.7745122829039,0.532596833091644,
-6.41406930190269));
#135451=CARTESIAN_POINT('Ctrl Pts',(20.7581772244235,0.578855915145535,
-6.41716555815408));
#135452=CARTESIAN_POINT('Ctrl Pts',(20.7418437351398,0.625110553407703,
-6.42026151696944));
#135453=CARTESIAN_POINT('Ctrl Pts',(20.7281716171061,0.672304312036179,
-6.42329289035936));
#135454=CARTESIAN_POINT('Ctrl Pts',(20.7172586082588,0.720100864105695,
-6.42626864486285));
#135455=CARTESIAN_POINT('Ctrl Pts',(20.7063314001507,0.767959605779906,
-6.42924827121457));
#135456=CARTESIAN_POINT('Ctrl Pts',(20.6981707252607,0.816422655751023,
-6.43217231323709));
#135457=CARTESIAN_POINT('Ctrl Pts',(20.6928385219224,0.86514038307293,-6.43507160755436));
#135458=CARTESIAN_POINT('Ctrl Pts',(20.6878983206692,0.91027657955696,-6.43775775744604));
#135459=CARTESIAN_POINT('Ctrl Pts',(20.6853858878954,0.955631193610204,
-6.44042312323611));
#135460=CARTESIAN_POINT('Ctrl Pts',(20.6853192846385,1.00091784626045,-6.44310594448226));
#135461=CARTESIAN_POINT('Ctrl Pts',(20.6853192846374,1.00091784701293,-6.44310594452685));
#135462=CARTESIAN_POINT('Ctrl Pts',(20.6852476706139,1.04961157282125,-6.44599060379221));
#135463=CARTESIAN_POINT('Ctrl Pts',(20.6880029641633,1.09822147251094,-6.44889478139007));
#135464=CARTESIAN_POINT('Ctrl Pts',(20.693576975525,1.14645852421811,-6.45188204245391));
#135465=CARTESIAN_POINT('Ctrl Pts',(20.6959637507833,1.16711348777554,-6.45316117884858));
#135466=CARTESIAN_POINT('Ctrl Pts',(20.6988674365921,1.18770073386852,-6.45445554882266));
#135467=CARTESIAN_POINT('Ctrl Pts',(20.7022881168209,1.20820041042418,-6.45577014294436));
#135468=CARTESIAN_POINT('Ctrl Pts',(20.7022909071302,1.20821713237236,-6.455771215282));
#135469=CARTESIAN_POINT('Ctrl Pts',(20.7022936977835,1.20823385426237,-6.45577228763309));
#135470=CARTESIAN_POINT('Ctrl Pts',(20.7022964887809,1.20825057609418,-6.45577335999765));
#135471=CARTESIAN_POINT('Ctrl Pts',(20.7098513922171,1.25351461943438,-6.45867612545473));
#135472=CARTESIAN_POINT('Ctrl Pts',(20.719943901946,1.29843270002029,-6.46168198209947));
#135473=CARTESIAN_POINT('Ctrl Pts',(20.7324967565363,1.34271492383747,-6.46473183056348));
#135474=CARTESIAN_POINT('Ctrl Pts',(20.7338491123666,1.34748557764594,-6.46506039968074));
#135475=CARTESIAN_POINT('Ctrl Pts',(20.7352299875163,1.35224881741516,-6.46538947938398));
#135476=CARTESIAN_POINT('Ctrl Pts',(20.7366392583893,1.3570042568621,-6.46571899577594));
#135477=CARTESIAN_POINT('Ctrl Pts',(20.7507252931146,1.40453613058896,-6.46901259917654));
#135478=CARTESIAN_POINT('Ctrl Pts',(20.7676519490923,1.45129316637296,-6.47234927943961));
#135479=CARTESIAN_POINT('Ctrl Pts',(20.7872818407009,1.4969357915126,-6.47567026653761));
#135480=CARTESIAN_POINT('Ctrl Pts',(20.8068934362007,1.54253587528487,-6.47898815829804));
#135481=CARTESIAN_POINT('Ctrl Pts',(20.8292029756259,1.58702381075725,-6.48229009245401));
#135482=CARTESIAN_POINT('Ctrl Pts',(20.8540418840448,1.63008212614013,-6.48553887032211));
#135483=CARTESIAN_POINT('Ctrl Pts',(20.8788680045907,1.67311827371008,-6.48878597561432));
#135484=CARTESIAN_POINT('Ctrl Pts',(20.9062208296114,1.71472632860985,-6.49197988416206));
#135485=CARTESIAN_POINT('Ctrl Pts',(20.9359027452407,1.75460861385274,-6.49510768867772));
#135486=CARTESIAN_POINT('Ctrl Pts',(20.9671387033798,1.79657899770192,-6.49839925422688));
#135487=CARTESIAN_POINT('Ctrl Pts',(21.0009543832482,1.83663788006493,-6.5016174317813));
#135488=CARTESIAN_POINT('Ctrl Pts',(21.0370843899636,1.87446167891545,-6.50477652742008));
#135489=CARTESIAN_POINT('Ctrl Pts',(21.0714470076843,1.91043523272293,-6.50778108805117));
#135490=CARTESIAN_POINT('Ctrl Pts',(21.107902955075,1.94438697496761,-6.51073262798619));
#135491=CARTESIAN_POINT('Ctrl Pts',(21.146192076393,1.97606098262062,-6.51366671243432));
#135492=CARTESIAN_POINT('Ctrl Pts',(21.1845043966793,2.00775418121552,-6.51660257461279));
#135493=CARTESIAN_POINT('Ctrl Pts',(21.2246523245406,2.03716645867982,-6.51952137292581));
#135494=CARTESIAN_POINT('Ctrl Pts',(21.266341359226,2.06406820693224,-6.52247680275527));
#135495=CARTESIAN_POINT('Ctrl Pts',(21.3048348640832,2.08890789403071,-6.52520569425767));
#135496=CARTESIAN_POINT('Ctrl Pts',(21.344642779175,2.11160723173152,-6.52796640405794));
#135497=CARTESIAN_POINT('Ctrl Pts',(21.3855032537724,2.13201127186824,-6.53080895545953));
#135498=CARTESIAN_POINT('Ctrl Pts',(21.388968410253,2.13374162846853,-6.53105001691336));
#135499=CARTESIAN_POINT('Ctrl Pts',(21.3924411512998,2.13545550504126,-6.53129166695737));
#135500=CARTESIAN_POINT('Ctrl Pts',(21.3959213258287,2.13715282208749,-6.53153393610074));
#135501=CARTESIAN_POINT('Ctrl Pts',(21.4026324497046,2.14042590648584,-6.53200112480608));
#135502=CARTESIAN_POINT('Ctrl Pts',(21.4093710802883,2.14363737076525,-6.53247062165335));
#135503=CARTESIAN_POINT('Ctrl Pts',(21.4161360021069,2.14678663364116,-6.53294264747405));
#135504=CARTESIAN_POINT('Ctrl Pts',(21.4161513468401,2.14679377704944,-6.53294371816052));
#135505=CARTESIAN_POINT('Ctrl Pts',(21.4161666917085,2.14680092013772,-6.53294478886));
#135506=CARTESIAN_POINT('Ctrl Pts',(21.4161820367122,2.14680806290598,-6.5329458595725));
#135507=CARTESIAN_POINT('Ctrl Pts',(21.4577876250457,2.16617456689952,-6.53584892979829));
#135508=CARTESIAN_POINT('Ctrl Pts',(21.5005429917933,2.18325238011408,-6.53885504780126));
#135509=CARTESIAN_POINT('Ctrl Pts',(21.5441653242742,2.19794127035611,-6.54190510997097));
#135510=CARTESIAN_POINT('Ctrl Pts',(21.5488627923362,2.1995230425552,-6.54223355571915));
#135511=CARTESIAN_POINT('Ctrl Pts',(21.5535702651596,2.2010771234395,-6.54256251104589));
#135512=CARTESIAN_POINT('Ctrl Pts',(21.5582873547441,2.20260339662812,-6.54289190214734));
#135513=CARTESIAN_POINT('Ctrl Pts',(21.6054538032502,2.21786468952239,-6.54618550260735));
#135514=CARTESIAN_POINT('Ctrl Pts',(21.6535875340928,2.23034517524371,-6.54952212201841));
#135515=CARTESIAN_POINT('Ctrl Pts',(21.7023308204948,2.23996612765215,-6.55284300448456));
#135516=CARTESIAN_POINT('Ctrl Pts',(21.7510286760591,2.2495781129195,-6.55616079174554));
#135517=CARTESIAN_POINT('Ctrl Pts',(21.8003349605609,2.25633620796331,-6.55946257787524));
#135518=CARTESIAN_POINT('Ctrl Pts',(21.8498925316008,2.26019990474393,-6.56271117944452));
#135519=CARTESIAN_POINT('Ctrl Pts',(21.8994245922865,2.26406161264029,-6.56595810875717));
#135520=CARTESIAN_POINT('Ctrl Pts',(21.9492076923783,2.26503198288817,-6.56915181316977));
#135521=CARTESIAN_POINT('Ctrl Pts',(21.9988845893612,2.26310565079043,-6.57227939982553));
#135522=CARTESIAN_POINT('Ctrl Pts',(22.0511644406077,2.2610783833555,-6.57557086477311));
#135523=CARTESIAN_POINT('Ctrl Pts',(22.1033266316716,2.25584243778223,-6.57878892069119));
#135524=CARTESIAN_POINT('Ctrl Pts',(22.1549541755633,2.2474337071581,-6.58194789038805));
#135525=CARTESIAN_POINT('Ctrl Pts',(22.2040543373295,2.23943661872874,-6.58495221543314));
#135526=CARTESIAN_POINT('Ctrl Pts',(22.2526708125535,2.22856984937452,-6.58790352022602));
#135527=CARTESIAN_POINT('Ctrl Pts',(22.3004454236137,2.21490323255278,-6.59083738040785));
#135528=CARTESIAN_POINT('Ctrl Pts',(22.3482489917486,2.201228332142,-6.59377301885657));
#135529=CARTESIAN_POINT('Ctrl Pts',(22.3952094434081,2.18474977396774,-6.59669160440083));
#135530=CARTESIAN_POINT('Ctrl Pts',(22.4409708823338,2.16558060137129,-6.59964683883878));
#135531=CARTESIAN_POINT('Ctrl Pts',(22.4832230133281,2.14788145530833,-6.60237544518339));
#135532=CARTESIAN_POINT('Ctrl Pts',(22.5244533118351,2.12788815848536,-6.60513588226684));
#135533=CARTESIAN_POINT('Ctrl Pts',(22.5643859502812,2.10572903376187,-6.60797816851481));
#135534=CARTESIAN_POINT('Ctrl Pts',(22.5677741073003,2.10384890269889,-6.60821932743834));
#135535=CARTESIAN_POINT('Ctrl Pts',(22.5711529534085,2.10195318318941,-6.60846107559247));
#135536=CARTESIAN_POINT('Ctrl Pts',(22.5745223374019,2.10004195499564,-6.608703443529));
#135537=CARTESIAN_POINT('Ctrl Pts',(22.5810220036043,2.09635512520112,-6.60917098023264));
#135538=CARTESIAN_POINT('Ctrl Pts',(22.5874863489624,2.09261067408924,-6.60964082917019));
#135539=CARTESIAN_POINT('Ctrl Pts',(22.5939142039863,2.08880927703164,-6.61011321169221));
#135540=CARTESIAN_POINT('Ctrl Pts',(22.5939287831095,2.08880065502077,-6.61011428311074));
#135541=CARTESIAN_POINT('Ctrl Pts',(22.593943362045,2.08879203271695,-6.6101153545423));
#135542=CARTESIAN_POINT('Ctrl Pts',(22.5939579407927,2.0887834101202,-6.6101164259869));
#135543=CARTESIAN_POINT('Ctrl Pts',(22.6334564898289,2.06542200309203,-6.61301931639274));
#135544=CARTESIAN_POINT('Ctrl Pts',(22.6717177856026,2.03981823663042,-6.61602527589385));
#135545=CARTESIAN_POINT('Ctrl Pts',(22.7084992502895,2.01214865355727,-6.61907519982099));
#135546=CARTESIAN_POINT('Ctrl Pts',(22.7124618255038,2.00916772810996,-6.61940377708299));
#135547=CARTESIAN_POINT('Ctrl Pts',(22.7164072065831,2.00616287220831,-6.61973286461307));
#135548=CARTESIAN_POINT('Ctrl Pts',(22.7203350777303,2.00313434035199,-6.62006238850735));
#135549=CARTESIAN_POINT('Ctrl Pts',(22.7595934208316,1.97286472654529,-6.62335591867085));
#135550=CARTESIAN_POINT('Ctrl Pts',(22.7971053959507,1.94022488047618,-6.62669248968518));
#135551=CARTESIAN_POINT('Ctrl Pts',(22.8326037837931,1.90546530295001,-6.63001333856003));
#135552=CARTESIAN_POINT('Ctrl Pts',(22.8680690690358,1.87073813907568,-6.63333109071027));
#135553=CARTESIAN_POINT('Ctrl Pts',(22.9015247857167,1.83389536597084,-6.63663285649171));
#135554=CARTESIAN_POINT('Ctrl Pts',(22.9327355656196,1.79520861528196,-6.63988144488369));
#135555=CARTESIAN_POINT('Ctrl Pts',(22.9639302666225,1.75654179489907,-6.64312835969597));
#135556=CARTESIAN_POINT('Ctrl Pts',(22.9928824170569,1.71603293301656,-6.64632205678973));
#135557=CARTESIAN_POINT('Ctrl Pts',(23.0193855766467,1.67397361748084,-6.64944963556714));
#135558=CARTESIAN_POINT('Ctrl Pts',(23.0472785290064,1.62970876367932,-6.65274122069094));
#135559=CARTESIAN_POINT('Ctrl Pts',(23.0724585106709,1.58372635331601,-6.6559593902003));
#135560=CARTESIAN_POINT('Ctrl Pts',(23.0947193002865,1.53639062033585,-6.65911846042949));
#135561=CARTESIAN_POINT('Ctrl Pts',(23.1158894916827,1.49137395451329,-6.66212276182855));
#135562=CARTESIAN_POINT('Ctrl Pts',(23.1344195132852,1.44513344505979,-6.66507403553562));
#135563=CARTESIAN_POINT('Ctrl Pts',(23.150164416456,1.39800397460386,-6.66800785145195));
#135564=CARTESIAN_POINT('Ctrl Pts',(23.1659188599464,1.35084594695641,-6.67094344505731));
#135565=CARTESIAN_POINT('Ctrl Pts',(23.1788843355623,1.30279783682696,-6.67386197248567));
#135566=CARTESIAN_POINT('Ctrl Pts',(23.1889528208304,1.25421707858004,-6.67681713154628));
#135567=CARTESIAN_POINT('Ctrl Pts',(23.198249482924,1.20936039143749,-6.67954575601039));
#135568=CARTESIAN_POINT('Ctrl Pts',(23.2050761545052,1.1640490966972,-6.68230619844614));
#135569=CARTESIAN_POINT('Ctrl Pts',(23.2093826866129,1.11858326311822,-6.68514848154152));
#135570=CARTESIAN_POINT('Ctrl Pts',(23.2097479316627,1.11472722066174,-6.68538954089151));
#135571=CARTESIAN_POINT('Ctrl Pts',(23.210095069409,1.11087004298659,-6.68563118892575));
#135572=CARTESIAN_POINT('Ctrl Pts',(23.2104240801512,1.1070118997018,-6.6858734561609));
#135573=CARTESIAN_POINT('Ctrl Pts',(23.211059522753,1.09956038431777,-6.68634136465898));
#135574=CARTESIAN_POINT('Ctrl Pts',(23.2116273591245,1.09210540896253,-6.68681158883039));
#135575=CARTESIAN_POINT('Ctrl Pts',(23.2121274846818,1.08464832339169,-6.68728435058385));
#135576=CARTESIAN_POINT('Ctrl Pts',(23.2121286181064,1.08463142354659,-6.68728542199443));
#135577=CARTESIAN_POINT('Ctrl Pts',(23.2121297511833,1.08461452369063,-6.68728649341805));
#135578=CARTESIAN_POINT('Ctrl Pts',(23.2121308839124,1.08459762382385,-6.6872875648547));
#135579=CARTESIAN_POINT('Ctrl Pts',(23.2151998645702,1.03880965703489,-6.69019048157388));
#135580=CARTESIAN_POINT('Ctrl Pts',(23.2157197162104,0.992774095079383,
-6.69319646598462));
#135581=CARTESIAN_POINT('Ctrl Pts',(23.2136988736089,0.946790846383176,
-6.69624641501267));
#135582=CARTESIAN_POINT('Ctrl Pts',(23.2134811925711,0.941837624747483,
-6.69657494929291));
#135583=CARTESIAN_POINT('Ctrl Pts',(23.2132340590177,0.936885051607219,
-6.69690399370157));
#135584=CARTESIAN_POINT('Ctrl Pts',(23.2129575042627,0.931933531175082,
-6.69723347436758));
#135585=CARTESIAN_POINT('Ctrl Pts',(23.2101929952465,0.882436921082219,
-6.70052704374327));
#135586=CARTESIAN_POINT('Ctrl Pts',(23.2044859647048,0.833040306351522,
-6.70386365569681));
#135587=CARTESIAN_POINT('Ctrl Pts',(23.1958919117608,0.784105745232262,
-6.70718454778575));
#135588=CARTESIAN_POINT('Ctrl Pts',(23.1873058706464,0.73521680349227,-6.7105023439639));
#135589=CARTESIAN_POINT('Ctrl Pts',(23.1758384782386,0.686788932139672,
-6.71380415601139));
#135590=CARTESIAN_POINT('Ctrl Pts',(23.1615806728929,0.639169867944375,
-6.71705279346231));
#135591=CARTESIAN_POINT('Ctrl Pts',(23.1473302097475,0.591575325664848,
-6.72029975799473));
#135592=CARTESIAN_POINT('Ctrl Pts',(23.1302922787626,0.54478871760092,-6.72349350756752));
#135593=CARTESIAN_POINT('Ctrl Pts',(23.1105906354368,0.499145206274198,
-6.72662114241718));
#135594=CARTESIAN_POINT('Ctrl Pts',(23.0898564998218,0.451109682630735,
-6.72991268536387));
#135595=CARTESIAN_POINT('Ctrl Pts',(23.0661717270767,0.40434040629928,-6.73313082134135));
#135596=CARTESIAN_POINT('Ctrl Pts',(23.0397200949546,0.359213406650139,
-6.73628986628034));
#135597=CARTESIAN_POINT('Ctrl Pts',(23.0145635988948,0.316295934351077,
-6.73929423671743));
#135598=CARTESIAN_POINT('Ctrl Pts',(22.9869046538028,0.274863929787187,
-6.74224558348198));
#135599=CARTESIAN_POINT('Ctrl Pts',(22.9569374945045,0.235226323224293,
-6.74517947716699));
#135600=CARTESIAN_POINT('Ctrl Pts',(22.9269521756465,0.195564696984603,
-6.74811514873881));
#135601=CARTESIAN_POINT('Ctrl Pts',(22.8946555404327,0.157700009658192,
-6.75103375887565));
#135602=CARTESIAN_POINT('Ctrl Pts',(22.8602813054491,0.121923489755126,
-6.75398900607447));
#135603=CARTESIAN_POINT('Ctrl Pts',(22.8285423804401,0.088889786377389,
-6.75671768845158));
#135604=CARTESIAN_POINT('Ctrl Pts',(22.795031725813,0.0576361706875381,
-6.75947819291928));
#135605=CARTESIAN_POINT('Ctrl Pts',(22.7599684665536,0.0283736927536179,
-6.76232054099184));
#135606=CARTESIAN_POINT('Ctrl Pts',(22.7569943620507,0.0258916169504828,
-6.76256163210487));
#135607=CARTESIAN_POINT('Ctrl Pts',(22.7540090790911,0.0234238366124944,
-6.76280331205156));
#135608=CARTESIAN_POINT('Ctrl Pts',(22.7510127464627,0.0209704639387167,
-6.76304561135783));
#135609=CARTESIAN_POINT('Ctrl Pts',(22.7452300253659,0.0162356191540649,
-6.76351323277503));
#135610=CARTESIAN_POINT('Ctrl Pts',(22.7394062714582,0.0115545087102523,
-6.76398316700287));
#135611=CARTESIAN_POINT('Ctrl Pts',(22.7335425367983,0.0069279805368398,
-6.76445563551957));
#135612=CARTESIAN_POINT('Ctrl Pts',(22.7335292417718,0.00691749066676322,
-6.76445670676202));
#135613=CARTESIAN_POINT('Ctrl Pts',(22.7335159465398,0.00690700107725976,
-6.76445777801749));
#135614=CARTESIAN_POINT('Ctrl Pts',(22.7335026511022,0.00689651176833514,
-6.76445884928599));
#135615=CARTESIAN_POINT('Ctrl Pts',(22.6975191189874,-0.0214923534050475,
-6.76735819159388));
#135616=CARTESIAN_POINT('Ctrl Pts',(22.6598937213588,-0.0479238910441021,
-6.77036038496798));
#135617=CARTESIAN_POINT('Ctrl Pts',(22.6208782113788,-0.0722355422069828,
-6.77340642694032));
#135618=CARTESIAN_POINT('Ctrl Pts',(22.6177634576589,-0.0741764320207257,
-6.77364960383508));
#135619=CARTESIAN_POINT('Ctrl Pts',(22.6146398716569,-0.0761038106475597,
-6.77389306019558));
#135620=CARTESIAN_POINT('Ctrl Pts',(22.6115075957382,-0.0780175956295496,
-6.77413676600051));
#135621=CARTESIAN_POINT('Ctrl Pts',(22.5692067673493,-0.103862920944605,
-6.77742796948936));
#135622=CARTESIAN_POINT('Ctrl Pts',(22.5253155148886,-0.127229590285433,
-6.78076406660601));
#135623=CARTESIAN_POINT('Ctrl Pts',(22.4801635910675,-0.147957541694851,
-6.78408577953313));
#135624=CARTESIAN_POINT('Ctrl Pts',(22.4507965966687,-0.16143908536842,
-6.78624623509449));
#135625=CARTESIAN_POINT('Ctrl Pts',(22.4208965137197,-0.173805229005387,
-6.78840095258332));
#135626=CARTESIAN_POINT('Ctrl Pts',(22.3905561784951,-0.185020462416371,
-6.79053837538029));
#135627=CARTESIAN_POINT('Ctrl Pts',(22.3906127229569,-0.185251306619802,
-6.65225448505536));
#135628=CARTESIAN_POINT('Ctrl Pts',(22.4229418914661,-0.173233059039878,
-6.65012827817395));
#135629=CARTESIAN_POINT('Ctrl Pts',(22.4547681000435,-0.159896281965281,
-6.64804342440638));
#135630=CARTESIAN_POINT('Ctrl Pts',(22.5249542668526,-0.127047699454832,
-6.64343073834645));
#135631=CARTESIAN_POINT('Ctrl Pts',(22.562943450965,-0.106846685042448,
-6.64092390595764));
#135632=CARTESIAN_POINT('Ctrl Pts',(22.6682338942969,-0.043771221167721,
-6.63382131291894));
#135633=CARTESIAN_POINT('Ctrl Pts',(22.7326014297101,0.00358078292254316,
-6.62929400300919));
#135634=CARTESIAN_POINT('Ctrl Pts',(22.810506713512,0.0731242077139838,
-6.62303729769182));
#135635=CARTESIAN_POINT('Ctrl Pts',(22.8284492585354,0.0901114018485893,
-6.62153374253444));
#135636=CARTESIAN_POINT('Ctrl Pts',(22.8573897587429,0.119165192594868,
-6.61897932643687));
#135637=CARTESIAN_POINT('Ctrl Pts',(22.8686716815253,0.130938202508655,
-6.61794774962455));
#135638=CARTESIAN_POINT('Ctrl Pts',(22.8963653551783,0.160979326106974,
-6.61532267287721));
#135639=CARTESIAN_POINT('Ctrl Pts',(22.9124770022823,0.179511779669976,
-6.61371169143372));
#135640=CARTESIAN_POINT('Ctrl Pts',(22.9489990013632,0.224078087098607,
-6.60987908201856));
#135641=CARTESIAN_POINT('Ctrl Pts',(22.9689477287969,0.250467396070868,
-6.60764112847349));
#135642=CARTESIAN_POINT('Ctrl Pts',(23.049927730056,0.366808645854362,-6.59799017465999));
#135643=CARTESIAN_POINT('Ctrl Pts',(23.1002705280125,0.463662450552342,
-6.59053615369726));
#135644=CARTESIAN_POINT('Ctrl Pts',(23.1478751937892,0.593860023580723,
-6.58156746065694));
#135645=CARTESIAN_POINT('Ctrl Pts',(23.1571462844445,0.622306021973822,
-6.579663061484));
#135646=CARTESIAN_POINT('Ctrl Pts',(23.173616779965,0.679674107861699,-6.57592415435642));
#135647=CARTESIAN_POINT('Ctrl Pts',(23.1808202093669,0.708575003392693,
-6.57409055540309));
#135648=CARTESIAN_POINT('Ctrl Pts',(23.1991670030157,0.795099497046015,
-6.56872598676445));
#135649=CARTESIAN_POINT('Ctrl Pts',(23.2073284953621,0.853274167238784,
-6.56528446753947));
#135650=CARTESIAN_POINT('Ctrl Pts',(23.2172708468426,0.99548442344696,-6.55702394678011));
#135651=CARTESIAN_POINT('Ctrl Pts',(23.2147802828762,1.07952552150498,-6.5522740699562));
#135652=CARTESIAN_POINT('Ctrl Pts',(23.2008467656394,1.18692093023769,-6.54578160592033));
#135653=CARTESIAN_POINT('Ctrl Pts',(23.1970021781084,1.21105084973372,-6.5442938038775));
#135654=CARTESIAN_POINT('Ctrl Pts',(23.189430441389,1.25107421682301,-6.54175542394405));
#135655=CARTESIAN_POINT('Ctrl Pts',(23.1860903008329,1.26703329452856,-6.5407233980417));
#135656=CARTESIAN_POINT('Ctrl Pts',(23.1768890529206,1.30711479257385,-6.53808015883207));
#135657=CARTESIAN_POINT('Ctrl Pts',(23.1706250219677,1.33113534840014,-6.5364507715613));
#135658=CARTESIAN_POINT('Ctrl Pts',(23.1542184221563,1.38723277235453,-6.53256099081813));
#135659=CARTESIAN_POINT('Ctrl Pts',(23.1434945033475,1.41912035655433,-6.53028367481263));
#135660=CARTESIAN_POINT('Ctrl Pts',(23.0932344276081,1.55092402255907,-6.52067607673287));
#135661=CARTESIAN_POINT('Ctrl Pts',(23.0423104011212,1.64604017452173,-6.51331219644281));
#135662=CARTESIAN_POINT('Ctrl Pts',(22.9625696372737,1.75799863612506,-6.50441697182777));
#135663=CARTESIAN_POINT('Ctrl Pts',(22.9443112688797,1.78179571422997,-6.50250723217336));
#135664=CARTESIAN_POINT('Ctrl Pts',(22.9062836969719,1.8278688999728,-6.49876402185259));
#135665=CARTESIAN_POINT('Ctrl Pts',(22.8865396142467,1.85014068913675,-6.49693125825614));
#135666=CARTESIAN_POINT('Ctrl Pts',(22.8259593021182,1.91380182455314,-6.49159971436625));
#135667=CARTESIAN_POINT('Ctrl Pts',(22.7830343684834,1.95309663528567,-6.48818815045933));
#135668=CARTESIAN_POINT('Ctrl Pts',(22.6744986427988,2.03949877468062,-6.48014601181487));
#135669=CARTESIAN_POINT('Ctrl Pts',(22.6067931185085,2.08354831775119,-6.47557668954084));
#135670=CARTESIAN_POINT('Ctrl Pts',(22.5117677518244,2.13317508698441,-6.46918173980384));
#135671=CARTESIAN_POINT('Ctrl Pts',(22.4877914023894,2.14474843587869,-6.46756850683698));
#135672=CARTESIAN_POINT('Ctrl Pts',(22.44848385361,2.16221469264991,-6.46489678218574));
#135673=CARTESIAN_POINT('Ctrl Pts',(22.4333723103359,2.16858046688527,-6.46386270623205));
#135674=CARTESIAN_POINT('Ctrl Pts',(22.3966486341831,2.18321615882464,-6.46132958118678));
#135675=CARTESIAN_POINT('Ctrl Pts',(22.3749275231949,2.19118929205379,-6.4598168478667));
#135676=CARTESIAN_POINT('Ctrl Pts',(22.3244422896744,2.20816433163066,-6.45628627200453));
#135677=CARTESIAN_POINT('Ctrl Pts',(22.2955503129036,2.21674273094702,-6.45425524132634));
#135678=CARTESIAN_POINT('Ctrl Pts',(22.1694415427855,2.24933203011163,-6.4454114212588));
#135679=CARTESIAN_POINT('Ctrl Pts',(22.0698531090616,2.26278477941171,-6.43851841280116));
#135680=CARTESIAN_POINT('Ctrl Pts',(21.9357225270067,2.264876368253,-6.42972147512304));
#135681=CARTESIAN_POINT('Ctrl Pts',(21.9017195179265,2.2640353659169,-6.4275288580805));
#135682=CARTESIAN_POINT('Ctrl Pts',(21.8395584929326,2.25998542815719,-6.4235844331879));
#135683=CARTESIAN_POINT('Ctrl Pts',(21.8113960304349,2.25719916417087,-6.42182145704969));
#135684=CARTESIAN_POINT('Ctrl Pts',(21.743574011528,2.24818211048376,-6.4176216835447));
#135685=CARTESIAN_POINT('Ctrl Pts',(21.7040710336316,2.2410034873884,-6.41521436637669));
#135686=CARTESIAN_POINT('Ctrl Pts',(21.5560739308449,2.20676277512529,-6.40624580782625));
#135687=CARTESIAN_POINT('Ctrl Pts',(21.4510083410748,2.16724351259546,-6.40002393137641));
#135688=CARTESIAN_POINT('Ctrl Pts',(21.3299869840087,2.10235993287699,-6.39181347945772));
#135689=CARTESIAN_POINT('Ctrl Pts',(21.307833745662,2.08960353908267,-6.3902609318516));
#135690=CARTESIAN_POINT('Ctrl Pts',(21.2722277399349,2.06763762816172,-6.3876583929243));
#135691=CARTESIAN_POINT('Ctrl Pts',(21.2585401188699,2.05882412293911,-6.38663011554596));
#135692=CARTESIAN_POINT('Ctrl Pts',(21.2254481470396,2.03660070931656,-6.38407229850616));
#135693=CARTESIAN_POINT('Ctrl Pts',(21.2062436324016,2.02290895194047,-6.38252763448191));
#135694=CARTESIAN_POINT('Ctrl Pts',(21.1626349070214,1.98994091823309,-6.37889727310592));
#135695=CARTESIAN_POINT('Ctrl Pts',(21.1385363406133,1.97028518491145,-6.37679723784216));
#135696=CARTESIAN_POINT('Ctrl Pts',(21.0493634331188,1.89190494460368,-6.36872172455945));
#135697=CARTESIAN_POINT('Ctrl Pts',(20.9897243191032,1.82735369292184,-6.36268736375753));
#135698=CARTESIAN_POINT('Ctrl Pts',(20.9141747344568,1.72629889302598,-6.35432593481205));
#135699=CARTESIAN_POINT('Ctrl Pts',(20.892530192544,1.69440776998183,-6.35181739378952));
#135700=CARTESIAN_POINT('Ctrl Pts',(20.85771431513,1.63769691624951,-6.34757219712827));
#135701=CARTESIAN_POINT('Ctrl Pts',(20.8438517915657,1.61333653622235,-6.34581255880034));
#135702=CARTESIAN_POINT('Ctrl Pts',(20.8147824893943,1.55805665696229,-6.34194964543567));
#135703=CARTESIAN_POINT('Ctrl Pts',(20.8000064289279,1.52693559631412,-6.33986172053459));
#135704=CARTESIAN_POINT('Ctrl Pts',(20.7707062881251,1.45810102891156,-6.33539696595839));
#135705=CARTESIAN_POINT('Ctrl Pts',(20.756681700617,1.4202165588794,-6.33303522280747));
#135706=CARTESIAN_POINT('Ctrl Pts',(20.7204004420713,1.30563828213752,-6.32606691087302));
#135707=CARTESIAN_POINT('Ctrl Pts',(20.7035668400059,1.22744791854381,-6.32154485298269));
#135708=CARTESIAN_POINT('Ctrl Pts',(20.690949349893,1.12053172370471,-6.31514163156302));
#135709=CARTESIAN_POINT('Ctrl Pts',(20.6885997400898,1.0927662796998,-6.31345795749804));
#135710=CARTESIAN_POINT('Ctrl Pts',(20.6863252941211,1.04854268290466,-6.31071233581132));
#135711=CARTESIAN_POINT('Ctrl Pts',(20.6858013954468,1.03212484759911,-6.30967847347548));
#135712=CARTESIAN_POINT('Ctrl Pts',(20.6853222615321,0.993537912993814,
-6.30720972031712));
#135713=CARTESIAN_POINT('Ctrl Pts',(20.6856298223234,0.971373844165684,
-6.30576351673096));
#135714=CARTESIAN_POINT('Ctrl Pts',(20.6894531847861,0.876222513690097,
-6.29946400872126));
#135715=CARTESIAN_POINT('Ctrl Pts',(20.6987090850081,0.803609462986055,
-6.29443513129044));
#135716=CARTESIAN_POINT('Ctrl Pts',(20.7292486581001,0.662675292926393,
-6.28460518109254));
#135717=CARTESIAN_POINT('Ctrl Pts',(20.7501582003088,0.594532485565407,
-6.2798197683935));
#135718=CARTESIAN_POINT('Ctrl Pts',(20.7881329708965,0.500033280715777,
-6.27321078514778));
#135719=CARTESIAN_POINT('Ctrl Pts',(20.800606706807,0.471987669378895,-6.27125137703142));
#135720=CARTESIAN_POINT('Ctrl Pts',(20.8270225246117,0.417979067579286,
-6.26747542497142));
#135721=CARTESIAN_POINT('Ctrl Pts',(20.8408757780864,0.391994699817149,
-6.26565746122949));
#135722=CARTESIAN_POINT('Ctrl Pts',(20.8821316750368,0.320723060396655,
-6.26064793415078));
#135723=CARTESIAN_POINT('Ctrl Pts',(20.9114885204447,0.276636580457099,
-6.25752406661893));
#135724=CARTESIAN_POINT('Ctrl Pts',(21.0028151189924,0.156558306110455,
-6.24874156481803));
#135725=CARTESIAN_POINT('Ctrl Pts',(21.0709557507471,0.0857624279732416,
-6.24323398612785));
#135726=CARTESIAN_POINT('Ctrl Pts',(21.1631953468981,0.00986762333587077,
-6.23600949412291));
#135727=CARTESIAN_POINT('Ctrl Pts',(21.1801639077479,-0.00338225527553693,
-6.23468766683016));
#135728=CARTESIAN_POINT('Ctrl Pts',(21.211099032642,-0.0262912028573803,
-6.23227438584376));
#135729=CARTESIAN_POINT('Ctrl Pts',(21.2249369620469,-0.036113769134416,
-6.23119260707361));
#135730=CARTESIAN_POINT('Ctrl Pts',(21.2648901438327,-0.0632814662434411,
-6.22806889240433));
#135731=CARTESIAN_POINT('Ctrl Pts',(21.2914575813583,-0.0799372974997237,
-6.22599268088905));
#135732=CARTESIAN_POINT('Ctrl Pts',(21.361958077986,-0.120566655890619,
-6.22053434867788));
#135733=CARTESIAN_POINT('Ctrl Pts',(21.4067450842764,-0.142950912770123,
-6.21711749014903));
#135734=CARTESIAN_POINT('Ctrl Pts',(21.5218832653832,-0.192196230705459,
-6.20860017259085));
#135735=CARTESIAN_POINT('Ctrl Pts',(21.593536129904,-0.215546003688449,
-6.20354251225363));
#135736=CARTESIAN_POINT('Ctrl Pts',(21.6967487534954,-0.239259994538608,
-6.1966837584893));
#135737=CARTESIAN_POINT('Ctrl Pts',(21.7268916389409,-0.245039932475306,
-6.19472805494932));
#135738=CARTESIAN_POINT('Ctrl Pts',(21.7867340547998,-0.254271292050343,
-6.19093171914911));
#135739=CARTESIAN_POINT('Ctrl Pts',(21.8164046932406,-0.257777703760111,
-6.18909060702583));
#135740=CARTESIAN_POINT('Ctrl Pts',(21.9020793423433,-0.264836167150757,
-6.18387153716627));
#135741=CARTESIAN_POINT('Ctrl Pts',(21.9582325827962,-0.265717211201952,
-6.18057226940304));
#135742=CARTESIAN_POINT('Ctrl Pts',(22.0935696736252,-0.25883031456539,
-6.17270785144827));
#135743=CARTESIAN_POINT('Ctrl Pts',(22.1723140692175,-0.247333554259472,
-6.16820851151158));
#135744=CARTESIAN_POINT('Ctrl Pts',(22.2780889139525,-0.221550862167308,
-6.16175186234005));
#135745=CARTESIAN_POINT('Ctrl Pts',(22.3064677635747,-0.213572949850973,
-6.1599758759125));
#135746=CARTESIAN_POINT('Ctrl Pts',(22.349977044977,-0.199683788943705,
-6.15714914733171));
#135747=CARTESIAN_POINT('Ctrl Pts',(22.3653177106432,-0.194459712317254,
-6.15613187305958));
#135748=CARTESIAN_POINT('Ctrl Pts',(22.3839119206128,-0.187726161438603,
-6.15486919788211));
#135749=CARTESIAN_POINT('Ctrl Pts',(22.3872650050902,-0.186495808226498,
-6.15464034546235));
#135750=CARTESIAN_POINT('Ctrl Pts',(22.3906127229914,-0.185251306606962,
-6.15441073460198));
#135751=CARTESIAN_POINT('Origin',(-21.9500000210213,0.999999999999992,-6.00000000000001));
#135752=CARTESIAN_POINT('',(-23.2146807734794,1.00091784938516,-6.44310584370542));
#135753=CARTESIAN_POINT('Ctrl Pts',(-21.5093309148108,-0.185465194729169,
-6.28967656068295));
#135754=CARTESIAN_POINT('Ctrl Pts',(-21.5528890708403,-0.20176031886336,
-6.29243730725128));
#135755=CARTESIAN_POINT('Ctrl Pts',(-21.5973018538419,-0.215616881063163,
-6.29522299047107));
#135756=CARTESIAN_POINT('Ctrl Pts',(-21.6422693820371,-0.22693499812517,
-6.29808522706224));
#135757=CARTESIAN_POINT('Ctrl Pts',(-21.6453764473183,-0.227717031961227,
-6.2982829954586));
#135758=CARTESIAN_POINT('Ctrl Pts',(-21.6484861751713,-0.228486961817531,
-6.29848112933784));
#135759=CARTESIAN_POINT('Ctrl Pts',(-21.6515984731377,-0.22924476131915,
-6.29867964572721));
#135760=CARTESIAN_POINT('Ctrl Pts',(-21.6658493874608,-0.232714652662521,
-6.29958863326223));
#135761=CARTESIAN_POINT('Ctrl Pts',(-21.6801536623721,-0.235930171416049,
-6.30050567807171));
#135762=CARTESIAN_POINT('Ctrl Pts',(-21.6945013876115,-0.238889048051699,
-6.30143245597623));
#135763=CARTESIAN_POINT('Ctrl Pts',(-21.6945179001323,-0.238892453365868,
-6.30143352258708));
#135764=CARTESIAN_POINT('Ctrl Pts',(-21.6945344127108,-0.238895858340165,
-6.30143458921083));
#135765=CARTESIAN_POINT('Ctrl Pts',(-21.6945509253467,-0.238899262974601,
-6.30143565584746));
#135766=CARTESIAN_POINT('Ctrl Pts',(-21.7395092457333,-0.248168930510011,
-6.30433974649248));
#135767=CARTESIAN_POINT('Ctrl Pts',(-21.7850595616849,-0.254945427799025,
-6.30734676297183));
#135768=CARTESIAN_POINT('Ctrl Pts',(-21.8309034069721,-0.259196362451375,
-6.31039760680955));
#135769=CARTESIAN_POINT('Ctrl Pts',(-21.8358278096666,-0.259652984576445,
-6.31072531892709));
#135770=CARTESIAN_POINT('Ctrl Pts',(-21.8407555546012,-0.260080487322827,
-6.31105353674159));
#135771=CARTESIAN_POINT('Ctrl Pts',(-21.8456862402058,-0.260478846979626,
-6.31138218700536));
#135772=CARTESIAN_POINT('Ctrl Pts',(-21.8951053083839,-0.264471509383489,
-6.31467616903842));
#135773=CARTESIAN_POINT('Ctrl Pts',(-21.9448252828204,-0.265534705092938,
-6.31801304290788));
#135774=CARTESIAN_POINT('Ctrl Pts',(-21.9944798553753,-0.263674227481021,
-6.32133409327276));
#135775=CARTESIAN_POINT('Ctrl Pts',(-22.0440882738254,-0.261815479189773,
-6.32465205670931));
#135776=CARTESIAN_POINT('Ctrl Pts',(-22.0936314933926,-0.25703879462773,
-6.32795393272415));
#135777=CARTESIAN_POINT('Ctrl Pts',(-22.1427525738362,-0.249387020616709,
-6.33120258133066));
#135778=CARTESIAN_POINT('Ctrl Pts',(-22.1918484783148,-0.241739168359695,
-6.33444956491144));
#135779=CARTESIAN_POINT('Ctrl Pts',(-22.2405227063286,-0.231219249570335,
-6.33764328070394));
#135780=CARTESIAN_POINT('Ctrl Pts',(-22.2884263109151,-0.2179043325076,
-6.34077088001125));
#135781=CARTESIAN_POINT('Ctrl Pts',(-22.3388295094863,-0.203894647548285,
-6.34406167639909));
#135782=CARTESIAN_POINT('Ctrl Pts',(-22.3883794239626,-0.186790230387356,
-6.34727909684211));
#135783=CARTESIAN_POINT('Ctrl Pts',(-22.4366787021697,-0.166721976528897,
-6.35043750170706));
#135784=CARTESIAN_POINT('Ctrl Pts',(-22.4826232176231,-0.147632121902707,
-6.35344192302581));
#135785=CARTESIAN_POINT('Ctrl Pts',(-22.5274359833547,-0.125860467509555,
-6.35639336480415));
#135786=CARTESIAN_POINT('Ctrl Pts',(-22.570784448847,-0.101557476263163,
-6.35932743540377));
#135787=CARTESIAN_POINT('Ctrl Pts',(-22.6141592340666,-0.0772397290595335,
-6.36226328747218));
#135788=CARTESIAN_POINT('Ctrl Pts',(-22.6560676193217,-0.0503872190281829,
-6.36518216058722));
#135789=CARTESIAN_POINT('Ctrl Pts',(-22.6961892211718,-0.0211919452919621,
-6.36813777916461));
#135790=CARTESIAN_POINT('Ctrl Pts',(-22.7332273305202,0.00575956439951002,
-6.37086624759594));
#135791=CARTESIAN_POINT('Ctrl Pts',(-22.7687429830093,0.0347080253773226,
-6.37362661811217));
#135792=CARTESIAN_POINT('Ctrl Pts',(-22.8024973740039,0.0654651041167603,
-6.37646888522295));
#135793=CARTESIAN_POINT('Ctrl Pts',(-22.8053679515819,0.0680807810107938,
-6.37671060038944));
#135794=CARTESIAN_POINT('Ctrl Pts',(-22.808225822136,0.0707095423226226,
-6.37695290785885));
#135795=CARTESIAN_POINT('Ctrl Pts',(-22.811070856039,0.0733512748601315,
-6.37719583838075));
#135796=CARTESIAN_POINT('Ctrl Pts',(-22.8165231690677,0.078413974716596,
-6.37766139812267));
#135797=CARTESIAN_POINT('Ctrl Pts',(-22.8219282504577,0.0835242027064733,
-6.37812925196743));
#135798=CARTESIAN_POINT('Ctrl Pts',(-22.8272851303427,0.0886810443488697,
-6.37859961831321));
#135799=CARTESIAN_POINT('Ctrl Pts',(-22.827297335773,0.0886927940002537,
-6.37860069002357));
#135800=CARTESIAN_POINT('Ctrl Pts',(-22.8273095409531,0.0887045438936312,
-6.37860176174696));
#135801=CARTESIAN_POINT('Ctrl Pts',(-22.8273217458829,0.0887162940289741,
-6.37860283348341));
#135802=CARTESIAN_POINT('Ctrl Pts',(-22.8599946799189,0.12017173059851,
-6.3814719015195));
#135803=CARTESIAN_POINT('Ctrl Pts',(-22.8909971419964,0.153490508933891,
-6.38444240110765));
#135804=CARTESIAN_POINT('Ctrl Pts',(-22.9201335387744,0.188451018775665,
-6.3874568890493));
#135805=CARTESIAN_POINT('Ctrl Pts',(-22.9223326145792,0.191089670764765,
-6.38768440817415));
#135806=CARTESIAN_POINT('Ctrl Pts',(-22.9245210576273,0.193737650453255,
-6.387912177879));
#135807=CARTESIAN_POINT('Ctrl Pts',(-22.9266987828115,0.196394850598419,
-6.38814017346644));
#135808=CARTESIAN_POINT('Ctrl Pts',(-22.9576869063787,0.234205703426636,
-6.39138445584307));
#135809=CARTESIAN_POINT('Ctrl Pts',(-22.9865058911464,0.273888863401147,
-6.39467389636256));
#135810=CARTESIAN_POINT('Ctrl Pts',(-23.0129544751761,0.315148437923321,
-6.39795091134187));
#135811=CARTESIAN_POINT('Ctrl Pts',(-23.0393781887874,0.356369214796404,
-6.40122484484302));
#135812=CARTESIAN_POINT('Ctrl Pts',(-23.0634362208576,0.399163291678379,
-6.40448608013678));
#135813=CARTESIAN_POINT('Ctrl Pts',(-23.0849637300028,0.443220519601541,
-6.40769721656754));
#135814=CARTESIAN_POINT('Ctrl Pts',(-23.1064909775948,0.487277212241604,
-6.41090831398387));
#135815=CARTESIAN_POINT('Ctrl Pts',(-23.1254878302226,0.532596958409967,
-6.41406920989122));
#135816=CARTESIAN_POINT('Ctrl Pts',(-23.1418228872495,0.578856055528787,
-6.4171654666348));
#135817=CARTESIAN_POINT('Ctrl Pts',(-23.1581563751267,0.625110708986886,
-6.42026142595116));
#135818=CARTESIAN_POINT('Ctrl Pts',(-23.1718284901437,0.672304482803547,
-6.42329279987827));
#135819=CARTESIAN_POINT('Ctrl Pts',(-23.1827414943878,0.720101049882449,
-6.42626855500388));
#135820=CARTESIAN_POINT('Ctrl Pts',(-23.1936686979045,0.767959806663703,
-6.4292481819834));
#135821=CARTESIAN_POINT('Ctrl Pts',(-23.2018293666031,0.816422871565319,
-6.43217222471905));
#135822=CARTESIAN_POINT('Ctrl Pts',(-23.2071615621788,0.865140613466418,
-6.43507151987879));
#135823=CARTESIAN_POINT('Ctrl Pts',(-23.2121017465369,0.910276734805267,
-6.43775766527513));
#135824=CARTESIAN_POINT('Ctrl Pts',(-23.214614170614,0.955631272551833,
-6.44042302676632));
#135825=CARTESIAN_POINT('Ctrl Pts',(-23.2146807734792,1.00091784928355,
-6.44310584369939));
#135826=CARTESIAN_POINT('Ctrl Pts',(-23.2146807734804,1.00091785003632,
-6.443105843744));
#135827=CARTESIAN_POINT('Ctrl Pts',(-23.2147523872175,1.04961158575364,
-6.4459905037947));
#135828=CARTESIAN_POINT('Ctrl Pts',(-23.211997092343,1.09822149555741,-6.44889468223683));
#135829=CARTESIAN_POINT('Ctrl Pts',(-23.2064230785462,1.14645855753,-6.45188194418482));
#135830=CARTESIAN_POINT('Ctrl Pts',(-23.2040363039612,1.16711351063344,
-6.45316108003847));
#135831=CARTESIAN_POINT('Ctrl Pts',(-23.2011326193651,1.18770074639772,
-6.45445544945693));
#135832=CARTESIAN_POINT('Ctrl Pts',(-23.1977119408825,1.20820041278777,
-6.45577004299616));
#135833=CARTESIAN_POINT('Ctrl Pts',(-23.1977091502273,1.20821713680927,
-6.45577111546681));
#135834=CARTESIAN_POINT('Ctrl Pts',(-23.197706359228,1.20823386077257,-6.45577218795093));
#135835=CARTESIAN_POINT('Ctrl Pts',(-23.1977035678845,1.20825058467767,
-6.4557732604485));
#135836=CARTESIAN_POINT('Ctrl Pts',(-23.1901486642958,1.2535146281704,-6.45867602608016));
#135837=CARTESIAN_POINT('Ctrl Pts',(-23.180056154529,1.29843270908024,-6.46168188285201));
#135838=CARTESIAN_POINT('Ctrl Pts',(-23.167503299968,1.34271493338495,-6.46473173138053));
#135839=CARTESIAN_POINT('Ctrl Pts',(-23.1661509436738,1.34748558889334,
-6.46506030061821));
#135840=CARTESIAN_POINT('Ctrl Pts',(-23.1647700680414,1.35224883035924,
-6.46538938044148));
#135841=CARTESIAN_POINT('Ctrl Pts',(-23.1633607966667,1.3570042714992,-6.46571889695301));
#135842=CARTESIAN_POINT('Ctrl Pts',(-23.1492747632291,1.4045361408835,-6.46901250007524));
#135843=CARTESIAN_POINT('Ctrl Pts',(-23.1323481091942,1.45129317265826,
-6.47234917997492));
#135844=CARTESIAN_POINT('Ctrl Pts',(-23.1127182200878,1.49693579420182,
-6.47567016663973));
#135845=CARTESIAN_POINT('Ctrl Pts',(-23.0931066271162,1.54253587431553,
-6.47898805796259));
#135846=CARTESIAN_POINT('Ctrl Pts',(-23.0707970907848,1.58702380654452,
-6.48228999161174));
#135847=CARTESIAN_POINT('Ctrl Pts',(-23.0459581859298,1.63008211916181,
-6.48553876892156));
#135848=CARTESIAN_POINT('Ctrl Pts',(-23.0211320689732,1.67311826392066,
-6.48878587365224));
#135849=CARTESIAN_POINT('Ctrl Pts',(-22.9937792480166,1.71472631648939,
-6.4919797815873));
#135850=CARTESIAN_POINT('Ctrl Pts',(-22.9640973368353,1.75460859993243,
-6.49510758545456));
#135851=CARTESIAN_POINT('Ctrl Pts',(-22.9328613760098,1.79657899178639,
-6.49839915109771));
#135852=CARTESIAN_POINT('Ctrl Pts',(-22.8990456926618,1.83663788183948,
-6.50161732867082));
#135853=CARTESIAN_POINT('Ctrl Pts',(-22.8629156817652,1.87446168789097,
-6.50477642427912));
#135854=CARTESIAN_POINT('Ctrl Pts',(-22.828553068191,1.91043524004335,-6.50778098417097));
#135855=CARTESIAN_POINT('Ctrl Pts',(-22.7920971253035,1.94438698114695,
-6.51073252334852));
#135856=CARTESIAN_POINT('Ctrl Pts',(-22.7538080087705,1.97606098822029,
-6.51366660703195));
#135857=CARTESIAN_POINT('Ctrl Pts',(-22.7154956932696,2.00775418623713,
-6.51660246844543));
#135858=CARTESIAN_POINT('Ctrl Pts',(-22.6753477704758,2.03716646368514,
-6.5195212659862));
#135859=CARTESIAN_POINT('Ctrl Pts',(-22.6336587410667,2.06406821252966,
-6.52247669504206));
#135860=CARTESIAN_POINT('Ctrl Pts',(-22.595165241663,2.08890789979943,-6.52520558578889));
#135861=CARTESIAN_POINT('Ctrl Pts',(-22.5553573322426,2.11160723825521,
-6.52796629483141));
#135862=CARTESIAN_POINT('Ctrl Pts',(-22.5144968634658,2.13201127977266,
-6.53080884547288));
#135863=CARTESIAN_POINT('Ctrl Pts',(-22.5110317067516,2.13374163685317,
-6.53104990691283));
#135864=CARTESIAN_POINT('Ctrl Pts',(-22.5075589654691,2.13545551390369,
-6.5312915569432));
#135865=CARTESIAN_POINT('Ctrl Pts',(-22.5040787907026,2.13715283142528,
-6.53153382607317));
#135866=CARTESIAN_POINT('Ctrl Pts',(-22.4973676365808,2.14042593126798,
-6.53200101682631));
#135867=CARTESIAN_POINT('Ctrl Pts',(-22.4906289754993,2.14363741043556,
-6.53247051574278));
#135868=CARTESIAN_POINT('Ctrl Pts',(-22.4838640229481,2.14678668763567,
-6.53294254365717));
#135869=CARTESIAN_POINT('Ctrl Pts',(-22.4838486762386,2.146793831964,-6.53294361448142));
#135870=CARTESIAN_POINT('Ctrl Pts',(-22.4838333293938,2.14680097597224,
-6.53294468531869));
#135871=CARTESIAN_POINT('Ctrl Pts',(-22.4838179824138,2.14680811966039,
-6.53294575616898));
#135872=CARTESIAN_POINT('Ctrl Pts',(-22.4422123954647,2.16617462284804,
-6.5358488259889));
#135873=CARTESIAN_POINT('Ctrl Pts',(-22.3994570302705,2.1832524354923,-6.53885494363662));
#135874=CARTESIAN_POINT('Ctrl Pts',(-22.3558346994545,2.19794132542384,
-6.54190500550471));
#135875=CARTESIAN_POINT('Ctrl Pts',(-22.3511372275183,2.1995230989544,-6.54223345150383));
#135876=CARTESIAN_POINT('Ctrl Pts',(-22.3464297508048,2.20107718112541,
-6.542562407083));
#135877=CARTESIAN_POINT('Ctrl Pts',(-22.3417126573151,2.20260345555568,
-6.54289179843821));
#135878=CARTESIAN_POINT('Ctrl Pts',(-22.2945462066872,2.21786474891735,
-6.54618539885695));
#135879=CARTESIAN_POINT('Ctrl Pts',(-22.2464124737228,2.23034523495559,
-6.54952201828973));
#135880=CARTESIAN_POINT('Ctrl Pts',(-22.1976691852061,2.2399661875372,-6.55284290082326));
#135881=CARTESIAN_POINT('Ctrl Pts',(-22.1489713275507,2.24957817297327,
-6.55616068815007));
#135882=CARTESIAN_POINT('Ctrl Pts',(-22.0996650409653,2.25633626804522,
-6.55946247439116));
#135883=CARTESIAN_POINT('Ctrl Pts',(-22.0501074678495,2.26019996472128,
-6.5627110760994));
#135884=CARTESIAN_POINT('Ctrl Pts',(-22.0005754051105,2.26406167251145,
-6.56595800554953));
#135885=CARTESIAN_POINT('Ctrl Pts',(-21.950792302973,2.26503204252326,-6.5691517101272));
#135886=CARTESIAN_POINT('Ctrl Pts',(-21.9011154039486,2.26310571006556,
-6.5722792969579));
#135887=CARTESIAN_POINT('Ctrl Pts',(-21.8488355501432,2.26107844223591,
-6.57557076211541));
#135888=CARTESIAN_POINT('Ctrl Pts',(-21.7966733565268,2.2558424960804,-6.57878881825307));
#135889=CARTESIAN_POINT('Ctrl Pts',(-21.7450458100928,2.2474337646913,-6.58194778816075));
#135890=CARTESIAN_POINT('Ctrl Pts',(-21.6959456463445,2.23943667560541,
-6.58495211337968));
#135891=CARTESIAN_POINT('Ctrl Pts',(-21.6473291691393,2.22856990548032,
-6.58790341833928));
#135892=CARTESIAN_POINT('Ctrl Pts',(-21.5995545560935,2.21490328777289,
-6.59083727866739));
#135893=CARTESIAN_POINT('Ctrl Pts',(-21.5517509859884,2.20122838648063,
-6.59377291726144));
#135894=CARTESIAN_POINT('Ctrl Pts',(-21.5047905323539,2.18474982731193,
-6.59669150293038));
#135895=CARTESIAN_POINT('Ctrl Pts',(-21.4590290914463,2.16558065360346,
-6.59964673746386));
#135896=CARTESIAN_POINT('Ctrl Pts',(-21.4167769564816,2.14788150561707,
-6.6023753440349));
#135897=CARTESIAN_POINT('Ctrl Pts',(-21.3755466541024,2.12788820653758,
-6.60513578132295));
#135898=CARTESIAN_POINT('Ctrl Pts',(-21.3356140119275,2.10572907923901,
-6.60797806776067));
#135899=CARTESIAN_POINT('Ctrl Pts',(-21.3322258568059,2.10384894918605,
-6.60821922654272));
#135900=CARTESIAN_POINT('Ctrl Pts',(-21.328847012584,2.10195323070465,-6.6084609745545));
#135901=CARTESIAN_POINT('Ctrl Pts',(-21.3254776304655,2.10004200355688,
-6.60870334234774));
#135902=CARTESIAN_POINT('Ctrl Pts',(-21.3189779645595,2.09635517389664,
-6.60917087901383));
#135903=CARTESIAN_POINT('Ctrl Pts',(-21.3125136194912,2.09261072292676,
-6.60964072791275));
#135904=CARTESIAN_POINT('Ctrl Pts',(-21.3060857647504,2.08880932601868,
-6.61011311039498));
#135905=CARTESIAN_POINT('Ctrl Pts',(-21.3060711837952,2.08880070292431,
-6.6101141819481));
#135906=CARTESIAN_POINT('Ctrl Pts',(-21.3060566030277,2.08879207953692,
-6.61011525351425));
#135907=CARTESIAN_POINT('Ctrl Pts',(-21.306042022448,2.08878345585653,-6.61011632509345));
#135908=CARTESIAN_POINT('Ctrl Pts',(-21.2665434693734,2.06542204605492,
-6.61301921569763));
#135909=CARTESIAN_POINT('Ctrl Pts',(-21.2282821698809,2.03981827656591,
-6.6160251753714));
#135910=CARTESIAN_POINT('Ctrl Pts',(-21.1915007018088,2.0121486902521,-6.6190750994482));
#135911=CARTESIAN_POINT('Ctrl Pts',(-21.1875381283282,2.00916776603422,
-6.61940367655232));
#135912=CARTESIAN_POINT('Ctrl Pts',(-21.1835927489682,2.00616291138487,
-6.61973276392372));
#135913=CARTESIAN_POINT('Ctrl Pts',(-21.1796648795256,2.00313438080335,
-6.62006228765863));
#135914=CARTESIAN_POINT('Ctrl Pts',(-21.1404065330904,1.97286476403174,
-6.62335581793822));
#135915=CARTESIAN_POINT('Ctrl Pts',(-21.1028945549724,1.94022491479254,
-6.62669238904534));
#135916=CARTESIAN_POINT('Ctrl Pts',(-21.067396164469,1.90546533392439,-6.63001323799809));
#135917=CARTESIAN_POINT('Ctrl Pts',(-21.0319308765439,1.87073816668763,
-6.63333099022841));
#135918=CARTESIAN_POINT('Ctrl Pts',(-20.9984751575207,1.83389539004587,
-6.63663275607506));
#135919=CARTESIAN_POINT('Ctrl Pts',(-20.967264375618,1.79520863567327,-6.63988134452721));
#135920=CARTESIAN_POINT('Ctrl Pts',(-20.9360696725984,1.75654181158648,
-6.64312825940148));
#135921=CARTESIAN_POINT('Ctrl Pts',(-20.9071175204923,1.71603294585134,
-6.64632195655213));
#135922=CARTESIAN_POINT('Ctrl Pts',(-20.8806143595794,1.67397362633977,
-6.64944953539169));
#135923=CARTESIAN_POINT('Ctrl Pts',(-20.852721407826,1.62970877152585,-6.65274112034504));
#135924=CARTESIAN_POINT('Ctrl Pts',(-20.8275414267647,1.58372636025973,
-6.65595928970062));
#135925=CARTESIAN_POINT('Ctrl Pts',(-20.8052806377126,1.53639062643641,
-6.65911835980036));
#135926=CARTESIAN_POINT('Ctrl Pts',(-20.7841104453188,1.49137395655138,
-6.66212266129391));
#135927=CARTESIAN_POINT('Ctrl Pts',(-20.7655804230656,1.44513344291141,
-6.66507393510946));
#135928=CARTESIAN_POINT('Ctrl Pts',(-20.749835519601,1.39800396817185,-6.66800775115554));
#135929=CARTESIAN_POINT('Ctrl Pts',(-20.7340810758135,1.35084593622912,
-6.67094334489131));
#135930=CARTESIAN_POINT('Ctrl Pts',(-20.721115600259,1.30279782170665,-6.67386187247146));
#135931=CARTESIAN_POINT('Ctrl Pts',(-20.7110471154209,1.25421705900154,
-6.67681703171073));
#135932=CARTESIAN_POINT('Ctrl Pts',(-20.7017504542369,1.2093603702151,-6.67954565618941));
#135933=CARTESIAN_POINT('Ctrl Pts',(-20.6949237836073,1.16404907382507,
-6.68230609865919));
#135934=CARTESIAN_POINT('Ctrl Pts',(-20.690617252492,1.11858323857537,-6.68514838180113));
#135935=CARTESIAN_POINT('Ctrl Pts',(-20.6902520072694,1.11472719326355,
-6.68538944132471));
#135936=CARTESIAN_POINT('Ctrl Pts',(-20.689904869376,1.1108700127313,-6.68563108953346));
#135937=CARTESIAN_POINT('Ctrl Pts',(-20.6895758585126,1.10701186658802,
-6.6858733569441));
#135938=CARTESIAN_POINT('Ctrl Pts',(-20.6889404172309,1.09956036391026,
-6.68634126463657));
#135939=CARTESIAN_POINT('Ctrl Pts',(-20.6883725819451,1.09210540127322,
-6.68681148799471));
#135940=CARTESIAN_POINT('Ctrl Pts',(-20.6878724572385,1.08464832842542,
-6.68728424892598));
#135941=CARTESIAN_POINT('Ctrl Pts',(-20.687871323671,1.0846314264489,-6.68728532047166));
#135942=CARTESIAN_POINT('Ctrl Pts',(-20.6878701904512,1.08461452446153,
-6.68728639203037));
#135943=CARTESIAN_POINT('Ctrl Pts',(-20.6878690575793,1.08459762246331,
-6.68728746360212));
#135944=CARTESIAN_POINT('Ctrl Pts',(-20.6848000770319,1.03880965400266,
-6.69019038034012));
#135945=CARTESIAN_POINT('Ctrl Pts',(-20.6842802255432,0.992774090407304,
-6.69319636476006));
#135946=CARTESIAN_POINT('Ctrl Pts',(-20.6863010683395,0.946790840098534,
-6.69624631378546));
#135947=CARTESIAN_POINT('Ctrl Pts',(-20.6865187494249,0.941837617682455,
-6.69657484810565));
#135948=CARTESIAN_POINT('Ctrl Pts',(-20.6867658830337,0.936885043762289,
-6.69690389255425));
#135949=CARTESIAN_POINT('Ctrl Pts',(-20.6870424378518,0.931933522550874,
-6.69723337326016));
#135950=CARTESIAN_POINT('Ctrl Pts',(-20.6898069471317,0.882436911237792,
-6.70052694259754));
#135951=CARTESIAN_POINT('Ctrl Pts',(-20.6955139779276,0.833040295320728,
-6.70386355449708));
#135952=CARTESIAN_POINT('Ctrl Pts',(-20.704108031124,0.784105733031032,
-6.70718444651916));
#135953=CARTESIAN_POINT('Ctrl Pts',(-20.7126940724883,0.735216790134869,
-6.71050224262962));
#135954=CARTESIAN_POINT('Ctrl Pts',(-20.7241614651429,0.686788917641545,
-6.71380405459674));
#135955=CARTESIAN_POINT('Ctrl Pts',(-20.7384192707434,0.639169852304406,
-6.71705269195841));
#135956=CARTESIAN_POINT('Ctrl Pts',(-20.7526697341407,0.59157530889364,
-6.72029965640093));
#135957=CARTESIAN_POINT('Ctrl Pts',(-20.7697076653843,0.544788699697114,
-6.72349340587503));
#135958=CARTESIAN_POINT('Ctrl Pts',(-20.7894093089887,0.499145187221971,
-6.72662104062077));
#135959=CARTESIAN_POINT('Ctrl Pts',(-20.8101434456976,0.451109660515009,
-6.72991258358517));
#135960=CARTESIAN_POINT('Ctrl Pts',(-20.8338282197867,0.404340381200418,
-6.73313071956871));
#135961=CARTESIAN_POINT('Ctrl Pts',(-20.8602798534964,0.359213378678562,
-6.73628976450706));
#135962=CARTESIAN_POINT('Ctrl Pts',(-20.8854363500905,0.316295905311972,
-6.73929413482702));
#135963=CARTESIAN_POINT('Ctrl Pts',(-20.9130952957426,0.274863899665037,
-6.74224548147274));
#135964=CARTESIAN_POINT('Ctrl Pts',(-20.9430624556387,0.235226291994243,
-6.74517937503937));
#135965=CARTESIAN_POINT('Ctrl Pts',(-20.9730477750942,0.195564664646751,
-6.74811504649268));
#135966=CARTESIAN_POINT('Ctrl Pts',(-21.0053444109433,0.157699976187537,
-6.75103365651137));
#135967=CARTESIAN_POINT('Ctrl Pts',(-21.0397186466094,0.121923455120705,
-6.75398890359384));
#135968=CARTESIAN_POINT('Ctrl Pts',(-21.0714575718499,0.0888897510833839,
-6.75671758582924));
#135969=CARTESIAN_POINT('Ctrl Pts',(-21.1049682267046,0.0576361346627014,
-6.75947809015584));
#135970=CARTESIAN_POINT('Ctrl Pts',(-21.1400314862003,0.0283736559177723,
-6.76232043808688));
#135971=CARTESIAN_POINT('Ctrl Pts',(-21.1430055912075,0.0258915796416098,
-6.76256152922717));
#135972=CARTESIAN_POINT('Ctrl Pts',(-21.1459908746752,0.0234237988346693,
-6.76280320920131));
#135973=CARTESIAN_POINT('Ctrl Pts',(-21.1489872078154,0.0209704256960743,
-6.76304550853523));
#135974=CARTESIAN_POINT('Ctrl Pts',(-21.1547699320427,0.0162355782598507,
-6.76351313017908));
#135975=CARTESIAN_POINT('Ctrl Pts',(-21.1605936891247,0.0115544652196716,
-6.76398306463605));
#135976=CARTESIAN_POINT('Ctrl Pts',(-21.1664574270013,0.00692793450649951,
-6.76445553338469));
#135977=CARTESIAN_POINT('Ctrl Pts',(-21.1664707237123,0.00691744330732976,
-6.7644566047628));
#135978=CARTESIAN_POINT('Ctrl Pts',(-21.1664840206289,0.00690695238880424,
-6.76445767615394));
#135979=CARTESIAN_POINT('Ctrl Pts',(-21.1664973177511,0.00689646175092878,
-6.76445874755812));
#135980=CARTESIAN_POINT('Ctrl Pts',(-21.2024808513942,-0.0214924043354978,
-6.76735808981954));
#135981=CARTESIAN_POINT('Ctrl Pts',(-21.2401062505285,-0.0479239427983001,
-6.77036028314935));
#135982=CARTESIAN_POINT('Ctrl Pts',(-21.279121761994,-0.0722355947060704,
-6.77340632508014));
#135983=CARTESIAN_POINT('Ctrl Pts',(-21.2822365164627,-0.0741764849719107,
-6.77364950202077));
#135984=CARTESIAN_POINT('Ctrl Pts',(-21.2853601032168,-0.0761038640448651,
-6.77389295842728));
#135985=CARTESIAN_POINT('Ctrl Pts',(-21.288492379891,-0.0780176494669613,
-6.77413666427833));
#135986=CARTESIAN_POINT('Ctrl Pts',(-21.3307932105313,-0.103862975867311,
-6.77742786777135));
#135987=CARTESIAN_POINT('Ctrl Pts',(-21.3746844652608,-0.127229646128756,
-6.78076396489562));
#135988=CARTESIAN_POINT('Ctrl Pts',(-21.4198363913639,-0.147957598299775,
-6.78408567783295));
#135989=CARTESIAN_POINT('Ctrl Pts',(-21.4492032374382,-0.161439073695795,
-6.7862461223799));
#135990=CARTESIAN_POINT('Ctrl Pts',(-21.4791031666279,-0.1738051603732,
-6.78840082891751));
#135991=CARTESIAN_POINT('Ctrl Pts',(-21.5094433440835,-0.185020348671025,
-6.79053824099259));
#135992=CARTESIAN_POINT('Ctrl Pts',(-21.5093868170662,-0.185251135625031,
-6.6522544014516));
#135993=CARTESIAN_POINT('Ctrl Pts',(-21.4970021902249,-0.180647191407368,
-6.65143989621879));
#135994=CARTESIAN_POINT('Ctrl Pts',(-21.4846892091089,-0.175848947059488,
-6.65063124382325));
#135995=CARTESIAN_POINT('Ctrl Pts',(-21.4228283175852,-0.150618288101447,
-6.64657067847646));
#135996=CARTESIAN_POINT('Ctrl Pts',(-21.3745383918806,-0.12724318529751,
-6.64341097068174));
#135997=CARTESIAN_POINT('Ctrl Pts',(-21.2403132319356,-0.0513896722782414,
-6.63444713150408));
#135998=CARTESIAN_POINT('Ctrl Pts',(-21.158980200687,0.00835566288177159,
-6.62880279875395));
#135999=CARTESIAN_POINT('Ctrl Pts',(-21.0710275547414,0.0907333471529403,
-6.62147891500746));
#136000=CARTESIAN_POINT('Ctrl Pts',(-21.0567892706854,0.104716306006347,
-6.62024791148091));
#136001=CARTESIAN_POINT('Ctrl Pts',(-21.0310187702787,0.131251481673118,
-6.61792044664163));
#136002=CARTESIAN_POINT('Ctrl Pts',(-21.0193984880813,0.143710801499513,
-6.61682998867927));
#136003=CARTESIAN_POINT('Ctrl Pts',(-20.9853955898538,0.18167850615026,
-6.61352208669295));
#136004=CARTESIAN_POINT('Ctrl Pts',(-20.9637852400462,0.207856197129783,
-6.61126205115897));
#136005=CARTESIAN_POINT('Ctrl Pts',(-20.9079975393363,0.28126054778753,
-6.60504335474356));
#136006=CARTESIAN_POINT('Ctrl Pts',(-20.8759888639061,0.330033209153253,
-6.60103926331554));
#136007=CARTESIAN_POINT('Ctrl Pts',(-20.8152027207198,0.438275255375555,
-6.59259353366974));
#136008=CARTESIAN_POINT('Ctrl Pts',(-20.7874817405927,0.498150565786792,
-6.58817795239542));
#136009=CARTESIAN_POINT('Ctrl Pts',(-20.7539781127685,0.588399833319446,
-6.5819365895114));
#136010=CARTESIAN_POINT('Ctrl Pts',(-20.7444346797864,0.617252623269691,
-6.57999827978544));
#136011=CARTESIAN_POINT('Ctrl Pts',(-20.727723115405,0.67463437518271,-6.57624768814011));
#136012=CARTESIAN_POINT('Ctrl Pts',(-20.7204924025503,0.703124860166806,
-6.5744345002805));
#136013=CARTESIAN_POINT('Ctrl Pts',(-20.7029092879162,0.784152653289509,
-6.56939514297486));
#136014=CARTESIAN_POINT('Ctrl Pts',(-20.6948902639548,0.837132860561267,
-6.5662393159371));
#136015=CARTESIAN_POINT('Ctrl Pts',(-20.6815577796816,0.990469720607132,
-6.55729075366656));
#136016=CARTESIAN_POINT('Ctrl Pts',(-20.6848022537679,1.09113985981767,
-6.55165734920069));
#136017=CARTESIAN_POINT('Ctrl Pts',(-20.7029290791665,1.21018232131975,
-6.54434215780434));
#136018=CARTESIAN_POINT('Ctrl Pts',(-20.7064195791314,1.22993503473715,
-6.54310532642317));
#136019=CARTESIAN_POINT('Ctrl Pts',(-20.7137321490241,1.26625315219018,
-6.54077498739096));
#136020=CARTESIAN_POINT('Ctrl Pts',(-20.7174212348531,1.28283989428573,
-6.53968780408896));
#136021=CARTESIAN_POINT('Ctrl Pts',(-20.7293704513592,1.33188114774661,
-6.53641291504399));
#136022=CARTESIAN_POINT('Ctrl Pts',(-20.7385865838009,1.3640861994133,-6.53418390452247));
#136023=CARTESIAN_POINT('Ctrl Pts',(-20.7668278921536,1.44975726022328,
-6.52810247375362));
#136024=CARTESIAN_POINT('Ctrl Pts',(-20.7881913990345,1.50237282705595,
-6.52420636252505));
#136025=CARTESIAN_POINT('Ctrl Pts',(-20.8426835133907,1.61433427157042,
-6.5157285708729));
#136026=CARTESIAN_POINT('Ctrl Pts',(-20.8772098222052,1.67281483091745,
-6.51117820991828));
#136027=CARTESIAN_POINT('Ctrl Pts',(-20.9338196190595,1.75317121262564,
-6.50480300606975));
#136028=CARTESIAN_POINT('Ctrl Pts',(-20.9522720193142,1.77745004081163,
-6.50285730414519));
#136029=CARTESIAN_POINT('Ctrl Pts',(-20.9901798717367,1.8237518588822,-6.49910083611303));
#136030=CARTESIAN_POINT('Ctrl Pts',(-21.0095606392189,1.84581074791794,
-6.49728888167223));
#136031=CARTESIAN_POINT('Ctrl Pts',(-21.0660112356979,1.90571999077067,
-6.49228408434947));
#136032=CARTESIAN_POINT('Ctrl Pts',(-21.1047170012583,1.94194602072816,
-6.48915952161548));
#136033=CARTESIAN_POINT('Ctrl Pts',(-21.2214056149115,2.03815581941333,
-6.48036169293891));
#136034=CARTESIAN_POINT('Ctrl Pts',(-21.3042471389755,2.09161185924171,
-6.47484143699861));
#136035=CARTESIAN_POINT('Ctrl Pts',(-21.4115689812116,2.14433692125753,
-6.46760842362708));
#136036=CARTESIAN_POINT('Ctrl Pts',(-21.4309417711391,2.15325339096281,
-6.46629878194238));
#136037=CARTESIAN_POINT('Ctrl Pts',(-21.4658365575232,2.16825665692896,
-6.46391709360524));
#136038=CARTESIAN_POINT('Ctrl Pts',(-21.4812701598006,2.17453398374778,
-6.46285492664888));
#136039=CARTESIAN_POINT('Ctrl Pts',(-21.524815411337,2.19125034860985,-6.45983860796339));
#136040=CARTESIAN_POINT('Ctrl Pts',(-21.5531798186893,2.20099658192033,
-6.45785296301066));
#136041=CARTESIAN_POINT('Ctrl Pts',(-21.6769200678191,2.23865272427844,
-6.4491735438664));
#136042=CARTESIAN_POINT('Ctrl Pts',(-21.7750595854177,2.25627697119716,
-6.44228095537805));
#136043=CARTESIAN_POINT('Ctrl Pts',(-21.9165692210142,2.26476848774623,
-6.43283376779055));
#136044=CARTESIAN_POINT('Ctrl Pts',(-21.9589846805841,2.26517858140536,
-6.43005853257355));
#136045=CARTESIAN_POINT('Ctrl Pts',(-22.029775093487,2.2623017950378,-6.42552209856486));
#136046=CARTESIAN_POINT('Ctrl Pts',(-22.0581601695301,2.26018707563593,
-6.42372849983404));
#136047=CARTESIAN_POINT('Ctrl Pts',(-22.1192118056452,2.25356032943692,
-6.41991696570142));
#136048=CARTESIAN_POINT('Ctrl Pts',(-22.1518223336909,2.24872501247293,
-6.41790996584829));
#136049=CARTESIAN_POINT('Ctrl Pts',(-22.220899121435,2.23570543425117,-6.41369533146793));
#136050=CARTESIAN_POINT('Ctrl Pts',(-22.2572665399047,2.22716820459328,
-6.41149876216713));
#136051=CARTESIAN_POINT('Ctrl Pts',(-22.3824485176305,2.1918667567163,-6.40392538894816));
#136052=CARTESIAN_POINT('Ctrl Pts',(-22.4686448810944,2.15696274461396,
-6.39870509394675));
#136053=CARTESIAN_POINT('Ctrl Pts',(-22.5722422474158,2.10109017614784,
-6.39165795826604));
#136054=CARTESIAN_POINT('Ctrl Pts',(-22.5938828845439,2.08857688778398,
-6.39013778916279));
#136055=CARTESIAN_POINT('Ctrl Pts',(-22.6289704645237,2.06687579206379,
-6.38756910176284));
#136056=CARTESIAN_POINT('Ctrl Pts',(-22.6426354602233,2.05805524863577,
-6.38654076399397));
#136057=CARTESIAN_POINT('Ctrl Pts',(-22.6760951616742,2.03553150371386,
-6.38395047645573));
#136058=CARTESIAN_POINT('Ctrl Pts',(-22.6956738591022,2.0215233755612,-6.3823721386644));
#136059=CARTESIAN_POINT('Ctrl Pts',(-22.7403970504793,1.98755395507167,
-6.3786386253462));
#136060=CARTESIAN_POINT('Ctrl Pts',(-22.7652051100249,1.9671766794096,-6.37646805421133));
#136061=CARTESIAN_POINT('Ctrl Pts',(-22.8549911663522,1.88751602877188,
-6.36829710044216));
#136062=CARTESIAN_POINT('Ctrl Pts',(-22.9145128670383,1.82244252281694,
-6.36224766542795));
#136063=CARTESIAN_POINT('Ctrl Pts',(-22.989086276843,1.72157137713819,-6.35395080733568));
#136064=CARTESIAN_POINT('Ctrl Pts',(-23.0100213250107,1.69044969438836,
-6.35151397885211));
#136065=CARTESIAN_POINT('Ctrl Pts',(-23.0441127035126,1.63455532280189,
-6.34734289030684));
#136066=CARTESIAN_POINT('Ctrl Pts',(-23.0578852617868,1.61019136543082,
-6.34558822531375));
#136067=CARTESIAN_POINT('Ctrl Pts',(-23.0871268986927,1.55420266516301,
-6.34168662776561));
#136068=CARTESIAN_POINT('Ctrl Pts',(-23.1021070341037,1.52234843119303,
-6.33955695681918));
#136069=CARTESIAN_POINT('Ctrl Pts',(-23.1319632385754,1.45130543625157,
-6.33496610105155));
#136070=CARTESIAN_POINT('Ctrl Pts',(-23.1462596107942,1.41191863480103,
-6.33252203161919));
#136071=CARTESIAN_POINT('Ctrl Pts',(-23.182207903786,1.29509416136878,-6.32544540608318));
#136072=CARTESIAN_POINT('Ctrl Pts',(-23.1984639498658,1.2162237043578,-6.32088955103311));
#136073=CARTESIAN_POINT('Ctrl Pts',(-23.2098865673701,1.1109099850932,-6.31455818574808));
#136074=CARTESIAN_POINT('Ctrl Pts',(-23.2118728653557,1.08539242329968,
-6.31300424434368));
#136075=CARTESIAN_POINT('Ctrl Pts',(-23.2138550976213,1.04354800777466,
-6.31039881337899));
#136076=CARTESIAN_POINT('Ctrl Pts',(-23.2143114567595,1.0272510540721,-6.30936911836072));
#136077=CARTESIAN_POINT('Ctrl Pts',(-23.2146576302375,0.98727302373077,
-6.30680415675638));
#136078=CARTESIAN_POINT('Ctrl Pts',(-23.2141976115936,0.963597598331454,
-6.30525361561269));
#136079=CARTESIAN_POINT('Ctrl Pts',(-23.2115916996031,0.908784870456056,
-6.30161036620721));
#136080=CARTESIAN_POINT('Ctrl Pts',(-23.2089570647934,0.87768596553925,
-6.29950334034772));
#136081=CARTESIAN_POINT('Ctrl Pts',(-23.1945338626333,0.759579094743743,
-6.29141267589574));
#136082=CARTESIAN_POINT('Ctrl Pts',(-23.1748455365704,0.67377459892076,
-6.28537099253779));
#136083=CARTESIAN_POINT('Ctrl Pts',(-23.1339265523788,0.554164623880316,
-6.27699618822844));
#136084=CARTESIAN_POINT('Ctrl Pts',(-23.1197603227409,0.518219415416183,
-6.27448223154372));
#136085=CARTESIAN_POINT('Ctrl Pts',(-23.0924083533556,0.457171300286188,
-6.27021532486726));
#136086=CARTESIAN_POINT('Ctrl Pts',(-23.0799839556492,0.431760352740889,
-6.26843986115372));
#136087=CARTESIAN_POINT('Ctrl Pts',(-23.0502495411082,0.375785753884799,
-6.26452035056393));
#136088=CARTESIAN_POINT('Ctrl Pts',(-23.0324973490981,0.34548316596362,
-6.26239268909699));
#136089=CARTESIAN_POINT('Ctrl Pts',(-22.991038177419,0.281025173994651,
-6.25782025231511));
#136090=CARTESIAN_POINT('Ctrl Pts',(-22.9668621667606,0.247220524323781,
-6.25539186112436));
#136091=CARTESIAN_POINT('Ctrl Pts',(-22.8910336525855,0.151527541332093,
-6.24831199079154));
#136092=CARTESIAN_POINT('Ctrl Pts',(-22.8350872144647,0.0933200213287932,
-6.24373967145049));
#136093=CARTESIAN_POINT('Ctrl Pts',(-22.7542397875024,0.0238665009735284,
-6.23737024999725));
#136094=CARTESIAN_POINT('Ctrl Pts',(-22.733971408656,0.00751479920781506,
-6.23578962104664));
#136095=CARTESIAN_POINT('Ctrl Pts',(-22.6999867559428,-0.0182118570375911,
-6.23313925031822));
#136096=CARTESIAN_POINT('Ctrl Pts',(-22.68656546832,-0.0279624341031814,
-6.23209166121726));
#136097=CARTESIAN_POINT('Ctrl Pts',(-22.6527815928084,-0.0515050878096002,
-6.22945063463704));
#136098=CARTESIAN_POINT('Ctrl Pts',(-22.6322030976972,-0.064971209058915,
-6.22784051876266));
#136099=CARTESIAN_POINT('Ctrl Pts',(-22.583066427279,-0.0951165239884055,
-6.22401479469022));
#136100=CARTESIAN_POINT('Ctrl Pts',(-22.5542202376943,-0.111292487676677,
-6.22178335526167));
#136101=CARTESIAN_POINT('Ctrl Pts',(-22.4299148142328,-0.174727142567352,
-6.21230976520936));
#136102=CARTESIAN_POINT('Ctrl Pts',(-22.3292998411566,-0.210966985010121,
-6.20503261708783));
#136103=CARTESIAN_POINT('Ctrl Pts',(-22.1959551179931,-0.240714213003921,
-6.19620797740491));
#136104=CARTESIAN_POINT('Ctrl Pts',(-22.1663606706167,-0.246215860613299,
-6.19429483274812));
#136105=CARTESIAN_POINT('Ctrl Pts',(-22.1065187448456,-0.255144184014924,
-6.19051003223404));
#136106=CARTESIAN_POINT('Ctrl Pts',(-22.076287695335,-0.258545463157658,
-6.1886402899011));
#136107=CARTESIAN_POINT('Ctrl Pts',(-21.9815568978915,-0.265755262406095,
-6.18288797933221));
#136108=CARTESIAN_POINT('Ctrl Pts',(-21.9168684953216,-0.265715493425707,
-6.17911856337654));
#136109=CARTESIAN_POINT('Ctrl Pts',(-21.7648057862798,-0.253950863845791,
-6.17030528920132));
#136110=CARTESIAN_POINT('Ctrl Pts',(-21.6781073295134,-0.238047029935697,
-6.16532090699785));
#136111=CARTESIAN_POINT('Ctrl Pts',(-21.5750936585617,-0.207801460718238,
-6.15878424981587));
#136112=CARTESIAN_POINT('Ctrl Pts',(-21.5565470372811,-0.201887598518051,
-6.1575814016423));
#136113=CARTESIAN_POINT('Ctrl Pts',(-21.5285172000524,-0.192231600010188,
-6.15571343033484));
#136114=CARTESIAN_POINT('Ctrl Pts',(-21.518930357273,-0.188798915329577,
-6.15506523016673));
#136115=CARTESIAN_POINT('Ctrl Pts',(-21.5093868082137,-0.185251132334142,
-6.15441066307283));
#136116=CARTESIAN_POINT('Ctrl Pts',(-20.9936430045563,1.82409301376269,
-6.00117192218052));
#136117=CARTESIAN_POINT('Ctrl Pts',(-20.7271798796497,1.51487473521959,
-6.02690195485214));
#136118=CARTESIAN_POINT('Ctrl Pts',(-20.5209353847399,0.623305030710792,
-6.07835570240434));
#136119=CARTESIAN_POINT('Ctrl Pts',(-21.4536811939941,-0.39338969715931,
-6.15553316483713));
#136120=CARTESIAN_POINT('Ctrl Pts',(-22.8180405859452,-0.196442644913706,
-6.23270430947889));
#136121=CARTESIAN_POINT('Ctrl Pts',(-23.4278797311105,1.03891461924669,
-6.30987545412066));
#136122=CARTESIAN_POINT('Ctrl Pts',(-22.7535238523448,2.24109353052079,
-6.38704659876242));
#136123=CARTESIAN_POINT('Ctrl Pts',(-21.3808545992212,2.36444027989689,
-6.46421774340418));
#136124=CARTESIAN_POINT('Ctrl Pts',(-20.5027990432502,1.30223244993389,
-6.54138888804594));
#136125=CARTESIAN_POINT('Ctrl Pts',(-20.8823603280752,-0.0226928241682067,
-6.6185600326877));
#136126=CARTESIAN_POINT('Ctrl Pts',(-22.1897133690524,-0.458853923907108,
-6.69573117732946));
#136127=CARTESIAN_POINT('Ctrl Pts',(-23.2887511850415,0.372721156485589,
-6.77290232197122));
#136128=CARTESIAN_POINT('Ctrl Pts',(-23.2244061652798,1.74941481466079,
-6.85007346661298));
#136129=CARTESIAN_POINT('Ctrl Pts',(-22.052592595292,2.47485743098409,-6.92724461125474));
#136130=CARTESIAN_POINT('Ctrl Pts',(-20.7916257543038,1.91864064422539,
-7.00441575589651));
#136131=CARTESIAN_POINT('Ctrl Pts',(-20.5372939483187,0.56411783578739,
-7.08158690053826));
#136132=CARTESIAN_POINT('Ctrl Pts',(-21.5106140510918,-0.411620184201609,
-7.15875804518003));
#136133=CARTESIAN_POINT('Ctrl Pts',(-22.8657628892087,-0.160649838355007,
-7.23592918982179));
#136134=CARTESIAN_POINT('Ctrl Pts',(-23.4251088531142,1.09893188787309,
-7.31310033446354));
#136135=CARTESIAN_POINT('Ctrl Pts',(-22.7025719108783,2.27254429285729,
-7.39027147910531));
#136136=CARTESIAN_POINT('Ctrl Pts',(-21.3260507987151,2.34030020089029,
-7.46744262374707));
#136137=CARTESIAN_POINT('Ctrl Pts',(-20.4917335473499,1.24333930698749,
-7.54461376838883));
#136138=CARTESIAN_POINT('Ctrl Pts',(-20.9246853421692,-0.0651126387312084,
-7.62178491303059));
#136139=CARTESIAN_POINT('Ctrl Pts',(-22.2485912883136,-0.447918175746809,
-7.69895605767235));
#136140=CARTESIAN_POINT('Ctrl Pts',(-23.3131243221307,0.427413029548789,
-7.77612720231412));
#136141=CARTESIAN_POINT('Ctrl Pts',(-23.1928787033875,1.80055940816669,
-7.85329834695587));
#136142=CARTESIAN_POINT('Ctrl Pts',(-21.9929993552513,2.47753865674549,
-7.93046949159765));
#136143=CARTESIAN_POINT('Ctrl Pts',(-20.7548625344256,1.87150078275659,
-8.00764063623939));
#136144=CARTESIAN_POINT('Ctrl Pts',(-20.5571190900327,0.505939988512289,
-8.08482166293017));
#136145=CARTESIAN_POINT('Ctrl Pts',(-21.2299640074188,-0.114446298241111,
-8.13627897474035));
#136146=CARTESIAN_POINT('Ctrl Pts',(-21.6244020672167,-0.219727019003528,
-8.16201257166996));
#136147=CARTESIAN_POINT('Ctrl Pts',(-20.9215174516537,1.88624361572157,
-5.9462028619613));
#136148=CARTESIAN_POINT('Ctrl Pts',(-20.6349584840009,1.5537050300928,-5.97193289463292));
#136149=CARTESIAN_POINT('Ctrl Pts',(-20.413159653239,0.594895835747109,
-6.02338664218513));
#136150=CARTESIAN_POINT('Ctrl Pts',(-21.4162503295794,-0.498474932679462,
-6.10056410461792));
#136151=CARTESIAN_POINT('Ctrl Pts',(-22.8835055792575,-0.286674729579892,
-6.17773524925968));
#136152=CARTESIAN_POINT('Ctrl Pts',(-23.5393369477972,1.0418494421014,-6.25490639390145));
#136153=CARTESIAN_POINT('Ctrl Pts',(-22.8141231887923,2.33469304989657,
-6.3320775385432));
#136154=CARTESIAN_POINT('Ctrl Pts',(-21.3379313733521,2.4673422379482,-6.40924868318497));
#136155=CARTESIAN_POINT('Ctrl Pts',(-20.3936555237423,1.32502590696021,
-6.48641982782672));
#136156=CARTESIAN_POINT('Ctrl Pts',(-20.8018421723771,-0.0998212230013129,
-6.56359097246849));
#136157=CARTESIAN_POINT('Ctrl Pts',(-22.2077918245531,-0.568876273358851,
-6.64076211711025));
#136158=CARTESIAN_POINT('Ctrl Pts',(-23.389715747691,0.325413683822369,
-6.71793326175202));
#136159=CARTESIAN_POINT('Ctrl Pts',(-23.3205180212025,1.80593341276833,
-6.79510440639377));
#136160=CARTESIAN_POINT('Ctrl Pts',(-22.060329816869,2.58608671652385,-6.87227555103553));
#136161=CARTESIAN_POINT('Ctrl Pts',(-20.7042646715523,1.98792174243761,
-6.94944669567729));
#136162=CARTESIAN_POINT('Ctrl Pts',(-20.4307519301931,0.531244921642298,
-7.02661784031905));
#136163=CARTESIAN_POINT('Ctrl Pts',(-21.4774768905197,-0.518080307901676,
-7.10378898496081));
#136164=CARTESIAN_POINT('Ctrl Pts',(-22.9348269542584,-0.248182537834989,
-7.18096012960258));
#136165=CARTESIAN_POINT('Ctrl Pts',(-23.5363570985653,1.10639303155661,
-7.25813127424434));
#136166=CARTESIAN_POINT('Ctrl Pts',(-22.7593286060459,2.36851573358007,
-7.3353024188861));
#136167=CARTESIAN_POINT('Ctrl Pts',(-21.2789944360103,2.44138158721428,
-7.41247356352786));
#136168=CARTESIAN_POINT('Ctrl Pts',(-20.3817555016178,1.26169122134304,
-7.48964470816962));
#136169=CARTESIAN_POINT('Ctrl Pts',(-20.8473592109878,-0.145440211645416,
-7.56681585281138));
#136170=CARTESIAN_POINT('Ctrl Pts',(-22.2711101383608,-0.557115784156377,
-7.64398699745315));
#136171=CARTESIAN_POINT('Ctrl Pts',(-23.4159270330431,0.384230252492084,
-7.7211581420949));
#136172=CARTESIAN_POINT('Ctrl Pts',(-23.2866128535148,1.86093517678805,
-7.79832928673667));
#136173=CARTESIAN_POINT('Ctrl Pts',(-21.9962422349526,2.58897015222068,
-7.87550043137843));
#136174=CARTESIAN_POINT('Ctrl Pts',(-20.6647288808513,1.93722673522966,
-7.95267157602019));
#136175=CARTESIAN_POINT('Ctrl Pts',(-20.4520722241179,0.468679477131948,
-8.02985260271096));
#136176=CARTESIAN_POINT('Ctrl Pts',(-21.1756610696071,-0.198494466505865,
-8.08130991452115));
#136177=CARTESIAN_POINT('Ctrl Pts',(-21.5998464545764,-0.311715140721045,
-8.10704351145075));
#136178=CARTESIAN_POINT('Ctrl Pts',(-20.8493918987509,1.94839421768056,
-5.89123380174209));
#136179=CARTESIAN_POINT('Ctrl Pts',(-20.542737088352,1.59253532496602,-5.91696383441371));
#136180=CARTESIAN_POINT('Ctrl Pts',(-20.305383921738,0.566486640783421,
-5.96841758196591));
#136181=CARTESIAN_POINT('Ctrl Pts',(-21.3788194651646,-0.603560168199624,
-6.04559504439872));
#136182=CARTESIAN_POINT('Ctrl Pts',(-22.9489705725699,-0.376906814246074,
-6.12276618904047));
#136183=CARTESIAN_POINT('Ctrl Pts',(-23.6507941644838,1.04478426495611,
-6.19993733368224));
#136184=CARTESIAN_POINT('Ctrl Pts',(-22.8747225252399,2.42829256927247,
-6.27710847832399));
#136185=CARTESIAN_POINT('Ctrl Pts',(-21.2950081474827,2.57024419599943,
-6.35427962296576));
#136186=CARTESIAN_POINT('Ctrl Pts',(-20.2845120042343,1.34781936398652,
-6.43145076760751));
#136187=CARTESIAN_POINT('Ctrl Pts',(-20.7213240166791,-0.176949621834419,
-6.50862191224927));
#136188=CARTESIAN_POINT('Ctrl Pts',(-22.2258702800536,-0.678898622810493,
-6.58579305689104));
#136189=CARTESIAN_POINT('Ctrl Pts',(-23.4906803103405,0.278106211159241,
-6.6629642015328));
#136190=CARTESIAN_POINT('Ctrl Pts',(-23.4166298771255,1.86245201087587,
-6.74013534617456));
#136191=CARTESIAN_POINT('Ctrl Pts',(-22.0680670384458,2.69731600206373,
-6.81730649081632));
#136192=CARTESIAN_POINT('Ctrl Pts',(-20.6169035888008,2.05720284064994,
-6.89447763545808));
#136193=CARTESIAN_POINT('Ctrl Pts',(-20.3242099120676,0.498372007497316,
-6.97164878009984));
#136194=CARTESIAN_POINT('Ctrl Pts',(-21.4443397299475,-0.624540431601641,
-7.04881992474161));
#136195=CARTESIAN_POINT('Ctrl Pts',(-23.003891019308,-0.335715237314962,
-7.12599106938337));
#136196=CARTESIAN_POINT('Ctrl Pts',(-23.647605344016,1.11385417524012,-7.20316221402513));
#136197=CARTESIAN_POINT('Ctrl Pts',(-22.8160853012138,2.46448717430285,
-7.28033335866689));
#136198=CARTESIAN_POINT('Ctrl Pts',(-21.2319380733055,2.54246297353816,
-7.35750450330865));
#136199=CARTESIAN_POINT('Ctrl Pts',(-20.2717774558857,1.28004313569848,
-7.43467564795041));
#136200=CARTESIAN_POINT('Ctrl Pts',(-20.7700330798062,-0.225767784559823,
-7.51184679259217));
#136201=CARTESIAN_POINT('Ctrl Pts',(-22.293628988408,-0.666313392565936,
-7.58901793723394));
#136202=CARTESIAN_POINT('Ctrl Pts',(-23.5187297439555,0.341047475435277,
-7.66618908187569));
#136203=CARTESIAN_POINT('Ctrl Pts',(-23.3803470036423,1.92131094540931,
-7.74336022651746));
#136204=CARTESIAN_POINT('Ctrl Pts',(-21.9994851146537,2.70040164769598,
-7.82053137115922));
#136205=CARTESIAN_POINT('Ctrl Pts',(-20.5745952272768,2.00295268770264,
-7.89770251580098));
#136206=CARTESIAN_POINT('Ctrl Pts',(-20.3470253582032,0.431418965751602,
-7.97488354249176));
#136207=CARTESIAN_POINT('Ctrl Pts',(-21.1213581317953,-0.282542634770624,
-8.02634085430194));
#136208=CARTESIAN_POINT('Ctrl Pts',(-21.5752908419361,-0.403703262438664,
-8.05207445123154));
#136209=CARTESIAN_POINT('Ctrl Pts',(-20.7772663458482,2.01054481963934,
-5.83626474152288));
#136210=CARTESIAN_POINT('Ctrl Pts',(-20.4505156927031,1.63136561983912,
-5.8619947741945));
#136211=CARTESIAN_POINT('Ctrl Pts',(-20.1976081902372,0.538077445819645,
-5.9134485217467));
#136212=CARTESIAN_POINT('Ctrl Pts',(-21.3413886007498,-0.708645403719883,
-5.9906259841795));
#136213=CARTESIAN_POINT('Ctrl Pts',(-23.0144355658823,-0.467138898912465,
-6.06779712882125));
#136214=CARTESIAN_POINT('Ctrl Pts',(-23.7622513811704,1.04771908781081,
-6.14496827346302));
#136215=CARTESIAN_POINT('Ctrl Pts',(-22.9353218616875,2.52189208864826,
-6.22213941810477));
#136216=CARTESIAN_POINT('Ctrl Pts',(-21.2520849216134,2.67314615405075,
-6.29931056274654));
#136217=CARTESIAN_POINT('Ctrl Pts',(-20.1753684847264,1.37061282101294,
-6.37648170738831));
#136218=CARTESIAN_POINT('Ctrl Pts',(-20.640805860981,-0.254078020667521,
-6.45365285203007));
#136219=CARTESIAN_POINT('Ctrl Pts',(-22.2439487355543,-0.788920972262233,
-6.53082399667182));
#136220=CARTESIAN_POINT('Ctrl Pts',(-23.5916448729899,0.230798738496012,
-6.60799514131358));
#136221=CARTESIAN_POINT('Ctrl Pts',(-23.5127417330482,1.9189706089834,-6.68516628595534));
#136222=CARTESIAN_POINT('Ctrl Pts',(-22.0758042600227,2.8085452876036,-6.76233743059711));
#136223=CARTESIAN_POINT('Ctrl Pts',(-20.5295425060494,2.12648393886206,
-6.83950857523886));
#136224=CARTESIAN_POINT('Ctrl Pts',(-20.217667893942,0.465499093352224,
-6.91667971988063));
#136225=CARTESIAN_POINT('Ctrl Pts',(-21.4112025693755,-0.731000555301602,
-6.99385086452238));
#136226=CARTESIAN_POINT('Ctrl Pts',(-23.0729550843577,-0.423247936795041,
-7.07102200916415));
#136227=CARTESIAN_POINT('Ctrl Pts',(-23.758853589467,1.12131531892362,-7.14819315380591));
#136228=CARTESIAN_POINT('Ctrl Pts',(-22.8728419963814,2.56045861502574,
-7.22536429844767));
#136229=CARTESIAN_POINT('Ctrl Pts',(-21.1848817106007,2.64354435986205,
-7.30253544308943));
#136230=CARTESIAN_POINT('Ctrl Pts',(-20.1617994101534,1.29839505005402,
-7.37970658773119));
#136231=CARTESIAN_POINT('Ctrl Pts',(-20.6927069486246,-0.30609535747403,
-7.45687773237295));
#136232=CARTESIAN_POINT('Ctrl Pts',(-22.3161478384553,-0.775511000975397,
-7.53404887701472));
#136233=CARTESIAN_POINT('Ctrl Pts',(-23.6215324548678,0.297864698378567,
-7.61122002165647));
#136234=CARTESIAN_POINT('Ctrl Pts',(-23.4740811537695,1.98168671403077,
-7.68839116629823));
#136235=CARTESIAN_POINT('Ctrl Pts',(-22.0027279943549,2.81183314317116,
-7.76556231094));
#136236=CARTESIAN_POINT('Ctrl Pts',(-20.4844615737024,2.06867864017571,
-7.84273345558175));
#136237=CARTESIAN_POINT('Ctrl Pts',(-20.2419784922884,0.394158454371154,
-7.91991448227254));
#136238=CARTESIAN_POINT('Ctrl Pts',(-21.0670551939834,-0.366590803035485,
-7.97137179408272));
#136239=CARTESIAN_POINT('Ctrl Pts',(-21.5507352292958,-0.495691384156185,
-7.99710539101233));
#136240=CARTESIAN_POINT('Ctrl Pts',(-21.5514861791641,-0.490649428218476,
-8.00000000000001));
#136241=CARTESIAN_POINT('Ctrl Pts',(-21.4053161238347,-0.437239491620633,
-8.00000000000001));
#136242=CARTESIAN_POINT('Ctrl Pts',(-21.2682206866264,-0.360071395527733,
-8.));
#136243=CARTESIAN_POINT('Ctrl Pts',(-21.0263626032413,-0.171118288369296,
-8.));
#136244=CARTESIAN_POINT('Ctrl Pts',(-20.9206285329538,-0.0601882408216436,
-8.));
#136245=CARTESIAN_POINT('Ctrl Pts',(-20.7358892338651,0.203461517749917,
-8.));
#136246=CARTESIAN_POINT('Ctrl Pts',(-20.6619493872077,0.35988357861727,
-8.));
#136247=CARTESIAN_POINT('Ctrl Pts',(-20.5805393518183,0.685725923832186,
-8.));
#136248=CARTESIAN_POINT('Ctrl Pts',(-20.5715184850394,0.853392047783976,
-8.));
#136249=CARTESIAN_POINT('Ctrl Pts',(-20.6100559739075,1.17524495044367,
-8.));
#136250=CARTESIAN_POINT('Ctrl Pts',(-20.6557618690624,1.33069459916174,
-8.));
#136251=CARTESIAN_POINT('Ctrl Pts',(-20.8004717406764,1.61978786133916,
-8.));
#136252=CARTESIAN_POINT('Ctrl Pts',(-20.8928208619793,1.73842020633026,
-8.00000000000001));
#136253=CARTESIAN_POINT('Ctrl Pts',(-21.001487092682,1.83623171117383,-8.00000000000001));
#136254=CARTESIAN_POINT('Ctrl Pts',(-20.9918838682989,1.82521129893649,
-6.00000000000001));
#136255=CARTESIAN_POINT('Ctrl Pts',(-20.9541736575533,1.7899949737847,-6.00000000000002));
#136256=CARTESIAN_POINT('Ctrl Pts',(-20.9189421950651,1.75244099022259,
-6.));
#136257=CARTESIAN_POINT('Ctrl Pts',(-20.8861950831707,1.71288999786489,
-6.00000000000001));
#136258=CARTESIAN_POINT('Ctrl Pts',(-20.8534479712762,1.67333900550718,
-6.00000000000002));
#136259=CARTESIAN_POINT('Ctrl Pts',(-20.8231848002971,1.63179022769739,
-6.00000000000002));
#136260=CARTESIAN_POINT('Ctrl Pts',(-20.7954373175153,1.58853787365536,
-6.00000000000003));
#136261=CARTESIAN_POINT('Ctrl Pts',(-20.7732296613486,1.55392091706439,
-6.00000000000004));
#136262=CARTESIAN_POINT('Ctrl Pts',(-20.7526338659112,1.51821167100359,
-6.00000000000001));
#136263=CARTESIAN_POINT('Ctrl Pts',(-20.7336809691674,1.48154464880145,
-6.00000000000003));
#136264=CARTESIAN_POINT('Ctrl Pts',(-20.7265367050108,1.46772307334569,
-6.00000000000004));
#136265=CARTESIAN_POINT('Ctrl Pts',(-20.7196260261576,1.45376528333739,
-6.00000000000004));
#136266=CARTESIAN_POINT('Ctrl Pts',(-20.7129511478733,1.43967807833951,
-6.00000000000002));
#136267=CARTESIAN_POINT('Ctrl Pts',(-20.7070329743969,1.42718788459759,
-6.00000000000001));
#136268=CARTESIAN_POINT('Ctrl Pts',(-20.7012980994116,1.4145908100944,-6.00000000000002));
#136269=CARTESIAN_POINT('Ctrl Pts',(-20.6957608152527,1.40192135070849,
-6.00000000000002));
#136270=CARTESIAN_POINT('Ctrl Pts',(-20.6737369136607,1.3515300544102,-6.00000000000005));
#136271=CARTESIAN_POINT('Ctrl Pts',(-20.6547985766653,1.2999241035713,-6.00000000000003));
#136272=CARTESIAN_POINT('Ctrl Pts',(-20.638977977284,1.24744397487004,-6.00000000000003));
#136273=CARTESIAN_POINT('Ctrl Pts',(-20.6231888036185,1.19506809162579,
-6.00000000000002));
#136274=CARTESIAN_POINT('Ctrl Pts',(-20.610504532974,1.14182048266499,-6.00000000000001));
#136275=CARTESIAN_POINT('Ctrl Pts',(-20.6009967006508,1.08800620437009,
-6.));
#136276=CARTESIAN_POINT('Ctrl Pts',(-20.5944877417198,1.05116553286749,
-5.99999999999999));
#136277=CARTESIAN_POINT('Ctrl Pts',(-20.5894682777219,1.0140585905501,-6.00000000000001));
#136278=CARTESIAN_POINT('Ctrl Pts',(-20.5859737043841,0.976777961364623,
-6.));
#136279=CARTESIAN_POINT('Ctrl Pts',(-20.5845817085914,0.961927942790997,
-6.));
#136280=CARTESIAN_POINT('Ctrl Pts',(-20.5834317834929,0.947050334331592,
-6.00000000000002));
#136281=CARTESIAN_POINT('Ctrl Pts',(-20.5825266608602,0.932150896779572,
-6.00000000000001));
#136282=CARTESIAN_POINT('Ctrl Pts',(-20.5818018340487,0.92021935134809,
-5.99999999999999));
#136283=CARTESIAN_POINT('Ctrl Pts',(-20.5812340735239,0.908271702282496,
-5.99999999999999));
#136284=CARTESIAN_POINT('Ctrl Pts',(-20.5808252608828,0.896333462267451,
-5.99999999999998));
#136285=CARTESIAN_POINT('Ctrl Pts',(-20.5788807239938,0.839548652388208,
-5.99999999999997));
#136286=CARTESIAN_POINT('Ctrl Pts',(-20.5805204587098,0.782868892275996,
-6.00000000000001));
#136287=CARTESIAN_POINT('Ctrl Pts',(-20.5858064535069,0.726625924331545,
-6.00000000000003));
#136288=CARTESIAN_POINT('Ctrl Pts',(-20.5884730759742,0.698253069701404,
-6.00000000000004));
#136289=CARTESIAN_POINT('Ctrl Pts',(-20.5920683585492,0.669990976519162,
-6.00000000000004));
#136290=CARTESIAN_POINT('Ctrl Pts',(-20.596605014284,0.641880555611109,
-6.00000000000004));
#136291=CARTESIAN_POINT('Ctrl Pts',(-20.6053457226608,0.587720618010693,
-6.00000000000002));
#136292=CARTESIAN_POINT('Ctrl Pts',(-20.6175775576439,0.534123432324477,
-6.00000000000002));
#136293=CARTESIAN_POINT('Ctrl Pts',(-20.6330757343097,0.481297854682912,
-6.00000000000002));
#136294=CARTESIAN_POINT('Ctrl Pts',(-20.641649315731,0.452074778910586,
-6.00000000000002));
#136295=CARTESIAN_POINT('Ctrl Pts',(-20.6512234402395,0.423087837825986,
-5.99999999999999));
#136296=CARTESIAN_POINT('Ctrl Pts',(-20.6617666141062,0.394373265917769,
-6.00000000000002));
#136297=CARTESIAN_POINT('Ctrl Pts',(-20.6648813824875,0.385890123953785,
-6.00000000000002));
#136298=CARTESIAN_POINT('Ctrl Pts',(-20.6680800797172,0.377432774733792,
-6.00000000000001));
#136299=CARTESIAN_POINT('Ctrl Pts',(-20.671358423858,0.369010458514467,
-6.00000000000001));
#136300=CARTESIAN_POINT('Ctrl Pts',(-20.6919756536175,0.31604322226919,
-6.00000000000001));
#136301=CARTESIAN_POINT('Ctrl Pts',(-20.7157726857117,0.26436761155119,
-6.00000000000002));
#136302=CARTESIAN_POINT('Ctrl Pts',(-20.7424735625905,0.21420120207078,
-6.00000000000001));
#136303=CARTESIAN_POINT('Ctrl Pts',(-20.7697924963213,0.162873568812587,
-6.00000000000001));
#136304=CARTESIAN_POINT('Ctrl Pts',(-20.8001515955868,0.113124889015486,
-6.));
#136305=CARTESIAN_POINT('Ctrl Pts',(-20.8333103098429,0.0651935718726574,
-6.00000000000003));
#136306=CARTESIAN_POINT('Ctrl Pts',(-20.8552521517862,0.0334763775098842,
-6.00000000000005));
#136307=CARTESIAN_POINT('Ctrl Pts',(-20.878421006149,0.002555091943291,
-5.99999999999998));
#136308=CARTESIAN_POINT('Ctrl Pts',(-20.9027587660785,-0.0274968485461307,
-6.00000000000002));
#136309=CARTESIAN_POINT('Ctrl Pts',(-20.9161338002876,-0.044012161921713,
-6.00000000000003));
#136310=CARTESIAN_POINT('Ctrl Pts',(-20.9298620146726,-0.0602648435553045,
-5.99999999999998));
#136311=CARTESIAN_POINT('Ctrl Pts',(-20.9439348110724,-0.0762420159595881,
-5.99999999999999));
#136312=CARTESIAN_POINT('Ctrl Pts',(-20.9530636035687,-0.0866061459742095,
-5.99999999999999));
#136313=CARTESIAN_POINT('Ctrl Pts',(-20.9623391710389,-0.0968560195668169,
-6.00000000000001));
#136314=CARTESIAN_POINT('Ctrl Pts',(-20.9717431138342,-0.106971189160145,
-6.00000000000001));
#136315=CARTESIAN_POINT('Ctrl Pts',(-21.0128363116122,-0.151172294346014,
-6.00000000000001));
#136316=CARTESIAN_POINT('Ctrl Pts',(-21.0564377688707,-0.192874028286213,
-6.00000000000002));
#136317=CARTESIAN_POINT('Ctrl Pts',(-21.1023016041767,-0.231816412469469,
-6.00000000000002));
#136318=CARTESIAN_POINT('Ctrl Pts',(-21.1275553688095,-0.25325905453901,
-6.00000000000003));
#136319=CARTESIAN_POINT('Ctrl Pts',(-21.1534959236055,-0.273864748872313,
-6.00000000000004));
#136320=CARTESIAN_POINT('Ctrl Pts',(-21.1800879138415,-0.293586475167077,
-6.00000000000003));
#136321=CARTESIAN_POINT('Ctrl Pts',(-21.1924609844341,-0.302762859089012,
-6.00000000000002));
#136322=CARTESIAN_POINT('Ctrl Pts',(-21.2049751417566,-0.311747822082119,
-6.00000000000005));
#136323=CARTESIAN_POINT('Ctrl Pts',(-21.2176270836379,-0.3205363747662,
-6.00000000000002));
#136324=CARTESIAN_POINT('Ctrl Pts',(-21.2273289074436,-0.327275655617109,
-6.00000000000001));
#136325=CARTESIAN_POINT('Ctrl Pts',(-21.2371108740145,-0.333898730182812,
-6.00000000000006));
#136326=CARTESIAN_POINT('Ctrl Pts',(-21.2469630024738,-0.340398020720054,
-6.00000000000005));
#136327=CARTESIAN_POINT('Ctrl Pts',(-21.2977187567768,-0.373880774727412,
-6.00000000000003));
#136328=CARTESIAN_POINT('Ctrl Pts',(-21.3503919444321,-0.404121965629313,
-6.));
#136329=CARTESIAN_POINT('Ctrl Pts',(-21.4047548111353,-0.43084736906057,
-6.00000000000003));
#136330=CARTESIAN_POINT('Ctrl Pts',(-21.4148035193166,-0.435787428266307,
-6.00000000000003));
#136331=CARTESIAN_POINT('Ctrl Pts',(-21.4249100656712,-0.44060726441391,
-6.00000000000002));
#136332=CARTESIAN_POINT('Ctrl Pts',(-21.4350731491762,-0.445305004100473,
-6.00000000000002));
#136333=CARTESIAN_POINT('Ctrl Pts',(-21.4726735185508,-0.462685235932125,
-6.00000000000001));
#136334=CARTESIAN_POINT('Ctrl Pts',(-21.5110472512579,-0.478395093363263,
-6.00000000000004));
#136335=CARTESIAN_POINT('Ctrl Pts',(-21.5500883508879,-0.492459335223598,
-6.00000000000006));
#136336=CARTESIAN_POINT('Ctrl Pts',(-22.3494288790946,-0.495721457493081,
-6.00294356625675));
#136337=CARTESIAN_POINT('Ctrl Pts',(-22.8330683941797,-0.366577429477468,
-6.02867458008192));
#136338=CARTESIAN_POINT('Ctrl Pts',(-23.6580915401405,0.394190827129925,
-6.08012930878768));
#136339=CARTESIAN_POINT('Ctrl Pts',(-23.4156065885705,2.06872657277341,
-6.15730775237402));
#136340=CARTESIAN_POINT('Ctrl Pts',(-21.8972695958558,2.81191799254906,
-6.23447889701578));
#136341=CARTESIAN_POINT('Ctrl Pts',(-20.4258482304807,1.98173169021987,
-6.31165004165755));
#136342=CARTESIAN_POINT('Ctrl Pts',(-20.2783902012899,0.2978324463073,-6.3888211862993));
#136343=CARTESIAN_POINT('Ctrl Pts',(-21.5838352020395,-0.775593405817618,
-6.46599233094107));
#136344=CARTESIAN_POINT('Ctrl Pts',(-23.207351366242,-0.306155785057727,
-6.54316347558283));
#136345=CARTESIAN_POINT('Ctrl Pts',(-23.7382834590338,1.29840883098511,
-6.62033462022458));
#136346=CARTESIAN_POINT('Ctrl Pts',(-22.7151537867526,2.64362052392713,
-6.69750576486635));
#136347=CARTESIAN_POINT('Ctrl Pts',(-21.0271152873712,2.56053089525116,
-6.77467690950811));
#136348=CARTESIAN_POINT('Ctrl Pts',(-20.1410626558735,1.1213209453176,-6.85184805414987));
#136349=CARTESIAN_POINT('Ctrl Pts',(-20.8269929323425,-0.423313875344182,
-6.92901919879164));
#136350=CARTESIAN_POINT('Ctrl Pts',(-22.4888224346674,-0.731080747060635,
-7.0061903434334));
#136351=CARTESIAN_POINT('Ctrl Pts',(-23.6824124023475,0.465474331375493,
-7.08336148807515));
#136352=CARTESIAN_POINT('Ctrl Pts',(-23.3705233422915,2.12653612459561,
-7.16053263271692));
#136353=CARTESIAN_POINT('Ctrl Pts',(-21.8241899541753,2.80862907641399,
-7.23770377735867));
#136354=CARTESIAN_POINT('Ctrl Pts',(-20.3871859100543,1.91901317583765,
-7.31487492200044));
#136355=CARTESIAN_POINT('Ctrl Pts',(-20.3082791180656,0.23076311617535,
-7.3920460666422));
#136356=CARTESIAN_POINT('Ctrl Pts',(-21.6560376834298,-0.789003872540381,
-7.46921721128396));
#136357=CARTESIAN_POINT('Ctrl Pts',(-23.2592548439766,-0.254136074614078,
-7.54638835592573));
#136358=CARTESIAN_POINT('Ctrl Pts',(-23.724713747306,1.37062990962013,-7.62355950056747));
#136359=CARTESIAN_POINT('Ctrl Pts',(-22.6479475054437,2.67322381241457,
-7.70073064520925));
#136360=CARTESIAN_POINT('Ctrl Pts',(-20.9646324202764,2.5219623366835,-7.77790178985101));
#136361=CARTESIAN_POINT('Ctrl Pts',(-20.137664945086,1.04772174268297,-7.85507293449276));
#136362=CARTESIAN_POINT('Ctrl Pts',(-20.8855146423405,-0.467207615859468,
-7.93224407913453));
#136363=CARTESIAN_POINT('Ctrl Pts',(-22.5586407113732,-0.708723385526007,
-8.00941522377629));
#136364=CARTESIAN_POINT('Ctrl Pts',(-23.7023760809268,0.537950929960438,
-8.08658636841805));
#136365=CARTESIAN_POINT('Ctrl Pts',(-23.4496155782475,1.63112624023658,
-8.13803379817922));
#136366=CARTESIAN_POINT('Ctrl Pts',(-23.123028433054,2.01031205541452,-8.16375751305981));
#136367=CARTESIAN_POINT('Ctrl Pts',(-22.3249001525792,-0.403869950441567,
-5.94805471546504));
#136368=CARTESIAN_POINT('Ctrl Pts',(-22.7788396067957,-0.282656592632247,
-5.97378572929022));
#136369=CARTESIAN_POINT('Ctrl Pts',(-23.5531984937602,0.43139326561541,
-6.02524045799597));
#136370=CARTESIAN_POINT('Ctrl Pts',(-23.3256044218573,2.0030966081544,-6.10241890158232));
#136371=CARTESIAN_POINT('Ctrl Pts',(-21.9005077449073,2.70064901433409,
-6.17959004622408));
#136372=CARTESIAN_POINT('Ctrl Pts',(-20.5194456300734,1.92144403785305,
-6.25676119086584));
#136373=CARTESIAN_POINT('Ctrl Pts',(-20.3810429247468,0.340952204793195,
-6.33393233550761));
#136374=CARTESIAN_POINT('Ctrl Pts',(-21.6063212005416,-0.666555102316617,
-6.41110348014935));
#136375=CARTESIAN_POINT('Ctrl Pts',(-23.1301380486332,-0.225945411193953,
-6.48827462479113));
#136376=CARTESIAN_POINT('Ctrl Pts',(-23.6284658669989,1.28008369383731,
-6.56544576943288));
#136377=CARTESIAN_POINT('Ctrl Pts',(-22.6681660764697,2.54268660913492,
-6.64261691407464));
#136378=CARTESIAN_POINT('Ctrl Pts',(-21.0837891775504,2.46469947302274,
-6.71978805871641));
#136379=CARTESIAN_POINT('Ctrl Pts',(-20.2521485952495,1.11387068670934,
-6.79695920335817));
#136380=CARTESIAN_POINT('Ctrl Pts',(-20.8959562363107,-0.335908881718829,
-6.87413034799992));
#136381=CARTESIAN_POINT('Ctrl Pts',(-22.4557336195818,-0.624775943683584,
-6.95130149264168));
#136382=CARTESIAN_POINT('Ctrl Pts',(-23.576025823976,0.498299285497095,
-7.02847263728345));
#136383=CARTESIAN_POINT('Ctrl Pts',(-23.2832897151967,2.05735610429587,
-7.10564378192521));
#136384=CARTESIAN_POINT('Ctrl Pts',(-21.8319158874927,2.69756206889499,
-7.18281492656696));
#136385=CARTESIAN_POINT('Ctrl Pts',(-20.4831575434186,1.8625770360886,-7.25998607120874));
#136386=CARTESIAN_POINT('Ctrl Pts',(-20.4090963780835,0.278001568699366,
-7.3371572158505));
#136387=CARTESIAN_POINT('Ctrl Pts',(-21.674089763641,-0.679142038981393,
-7.41432836049225));
#136388=CARTESIAN_POINT('Ctrl Pts',(-23.1788541597446,-0.177120205165915,
-7.49149950513402));
#136389=CARTESIAN_POINT('Ctrl Pts',(-23.6157294644854,1.34786971213385,
-7.56867064977578));
#136390=CARTESIAN_POINT('Ctrl Pts',(-22.6050868993022,2.57047197447387,
-7.64584179441754));
#136391=CARTESIAN_POINT('Ctrl Pts',(-21.0251433520911,2.42849939035783,
-7.72301293905929));
#136392=CARTESIAN_POINT('Ctrl Pts',(-20.2489595361832,1.04479117431909,
-7.80018408370107));
#136393=CARTESIAN_POINT('Ctrl Pts',(-20.9508841573504,-0.377107129569758,
-7.87735522834283));
#136394=CARTESIAN_POINT('Ctrl Pts',(-22.5212643908144,-0.603791536545408,
-7.95452637298458));
#136395=CARTESIAN_POINT('Ctrl Pts',(-23.5947635430329,0.566325132391112,
-8.03169751762634));
#136396=CARTESIAN_POINT('Ctrl Pts',(-23.3575249364778,1.59236909329918,
-8.08314494738751));
#136397=CARTESIAN_POINT('Ctrl Pts',(-23.0509933446224,1.94826929710738,
-8.1088686622681));
#136398=CARTESIAN_POINT('Ctrl Pts',(-22.300371426064,-0.312018443390052,
-5.89316586467334));
#136399=CARTESIAN_POINT('Ctrl Pts',(-22.7246108194117,-0.198735755787229,
-5.91889687849851));
#136400=CARTESIAN_POINT('Ctrl Pts',(-23.4483054473798,0.468595704100783,
-5.97035160720427));
#136401=CARTESIAN_POINT('Ctrl Pts',(-23.2356022551438,1.9374666435354,-6.04753005079061));
#136402=CARTESIAN_POINT('Ctrl Pts',(-21.9037458939589,2.58938003611924,
-6.12470119543238));
#136403=CARTESIAN_POINT('Ctrl Pts',(-20.6130430296662,1.86115638548621,
-6.20187234007413));
#136404=CARTESIAN_POINT('Ctrl Pts',(-20.4836956482035,0.3840719632792,-6.2790434847159));
#136405=CARTESIAN_POINT('Ctrl Pts',(-21.6288071990437,-0.557516798815514,
-6.35621462935766));
#136406=CARTESIAN_POINT('Ctrl Pts',(-23.0529247310244,-0.145735037330184,
-6.43338577399942));
#136407=CARTESIAN_POINT('Ctrl Pts',(-23.5186482749642,1.2617585566895,-6.51055691864117));
#136408=CARTESIAN_POINT('Ctrl Pts',(-22.6211783661869,2.4417526943427,-6.58772806328294));
#136409=CARTESIAN_POINT('Ctrl Pts',(-21.1404630677295,2.36886805079411,
-6.6648992079247));
#136410=CARTESIAN_POINT('Ctrl Pts',(-20.3632345346257,1.10642042810096,
-6.74207035256646));
#136411=CARTESIAN_POINT('Ctrl Pts',(-20.9649195402789,-0.248503888093268,
-6.81924149720822));
#136412=CARTESIAN_POINT('Ctrl Pts',(-22.4226448044962,-0.518471140306853,
-6.89641264184999));
#136413=CARTESIAN_POINT('Ctrl Pts',(-23.4696392456045,0.531124239618692,
-6.97358378649174));
#136414=CARTESIAN_POINT('Ctrl Pts',(-23.1960560881021,1.98817608399623,
-7.05075493113352));
#136415=CARTESIAN_POINT('Ctrl Pts',(-21.8396418208102,2.586495061376,-7.12792607577527));
#136416=CARTESIAN_POINT('Ctrl Pts',(-20.579129176783,1.80614089633934,-7.20509722041702));
#136417=CARTESIAN_POINT('Ctrl Pts',(-20.5099136381014,0.325240021223374,
-7.2822683650588));
#136418=CARTESIAN_POINT('Ctrl Pts',(-21.6921418438521,-0.569280205422404,
-7.35943950970054));
#136419=CARTESIAN_POINT('Ctrl Pts',(-23.0984534755126,-0.100104335717859,
-7.43661065434232));
#136420=CARTESIAN_POINT('Ctrl Pts',(-23.5067451816648,1.32510951464757,
-7.51378179898406));
#136421=CARTESIAN_POINT('Ctrl Pts',(-22.5622262931607,2.46772013653318,
-7.59095294362584));
#136422=CARTESIAN_POINT('Ctrl Pts',(-21.0856542839059,2.33503644403196,
-7.66812408826759));
#136423=CARTESIAN_POINT('Ctrl Pts',(-20.3602541272804,1.04186060595509,
-7.74529523290936));
#136424=CARTESIAN_POINT('Ctrl Pts',(-21.0162536723602,-0.287006643279932,
-7.82246637755112));
#136425=CARTESIAN_POINT('Ctrl Pts',(-22.4838880702559,-0.49885968756481,
-7.89963752219288));
#136426=CARTESIAN_POINT('Ctrl Pts',(-23.4871510051389,0.594699334821902,
-7.97680866683464));
#136427=CARTESIAN_POINT('Ctrl Pts',(-23.2654342947082,1.55361194636178,
-8.02825609659581));
#136428=CARTESIAN_POINT('Ctrl Pts',(-22.978958256191,1.88622653880024,-8.0539798114764));
#136429=CARTESIAN_POINT('Ctrl Pts',(-22.2758426995487,-0.220166936338542,
-5.83827701388163));
#136430=CARTESIAN_POINT('Ctrl Pts',(-22.6703820320277,-0.114814918942012,
-5.86400802770681));
#136431=CARTESIAN_POINT('Ctrl Pts',(-23.3434124009993,0.505798142586267,
-5.91546275641256));
#136432=CARTESIAN_POINT('Ctrl Pts',(-23.1456000884306,1.87183667891629,
-5.99264119999891));
#136433=CARTESIAN_POINT('Ctrl Pts',(-21.9069840430104,2.47811105790429,
-6.06981234464067));
#136434=CARTESIAN_POINT('Ctrl Pts',(-20.706640429259,1.80086873311939,-6.14698348928243));
#136435=CARTESIAN_POINT('Ctrl Pts',(-20.5863483716603,0.427191721765094,
-6.2241546339242));
#136436=CARTESIAN_POINT('Ctrl Pts',(-21.6512931975458,-0.44847849531461,
-6.30132577856596));
#136437=CARTESIAN_POINT('Ctrl Pts',(-22.9757114134156,-0.0655246634663076,
-6.37849692320771));
#136438=CARTESIAN_POINT('Ctrl Pts',(-23.4088306829294,1.24343341954179,
-6.45566806784948));
#136439=CARTESIAN_POINT('Ctrl Pts',(-22.574190655904,2.34081877955049,-6.53283921249123));
#136440=CARTESIAN_POINT('Ctrl Pts',(-21.1971369579087,2.27303662856569,
-6.610010357133));
#136441=CARTESIAN_POINT('Ctrl Pts',(-20.4743204740017,1.09897016949269,
-6.68718150177476));
#136442=CARTESIAN_POINT('Ctrl Pts',(-21.0338828442468,-0.161098894467706,
-6.76435264641652));
#136443=CARTESIAN_POINT('Ctrl Pts',(-22.3895559894107,-0.412166336930007,
-6.84152379105829));
#136444=CARTESIAN_POINT('Ctrl Pts',(-23.3632526672331,0.56394919374029,
-6.91869493570004));
#136445=CARTESIAN_POINT('Ctrl Pts',(-23.1088224610074,1.91899606369649,
-6.99586608034181));
#136446=CARTESIAN_POINT('Ctrl Pts',(-21.8473677541276,2.47542805385689,
-7.07303722498357));
#136447=CARTESIAN_POINT('Ctrl Pts',(-20.6751008101473,1.74970475659019,
-7.15020836962532));
#136448=CARTESIAN_POINT('Ctrl Pts',(-20.6107308981193,0.372478473747391,
-7.22737951426709));
#136449=CARTESIAN_POINT('Ctrl Pts',(-21.7101939240631,-0.459418371863309,
-7.30455065890885));
#136450=CARTESIAN_POINT('Ctrl Pts',(-23.0180527912807,-0.0230884662698116,
-7.38172180355061));
#136451=CARTESIAN_POINT('Ctrl Pts',(-23.3977608988442,1.30234931716139,
-7.45889294819237));
#136452=CARTESIAN_POINT('Ctrl Pts',(-22.5193656870193,2.36496829859259,
-7.53606409283414));
#136453=CARTESIAN_POINT('Ctrl Pts',(-21.1461652157205,2.24157349770619,
-7.61323523747589));
#136454=CARTESIAN_POINT('Ctrl Pts',(-20.4715487183776,1.03893003759129,
-7.69040638211766));
#136455=CARTESIAN_POINT('Ctrl Pts',(-21.0816231873701,-0.196906156990209,
-7.76757752675942));
#136456=CARTESIAN_POINT('Ctrl Pts',(-22.4465117496972,-0.393927838584109,
-7.84474867140118));
#136457=CARTESIAN_POINT('Ctrl Pts',(-23.3795384672449,0.623073537252594,
-7.92191981604294));
#136458=CARTESIAN_POINT('Ctrl Pts',(-23.1733436529386,1.51485479942439,
-7.97336724580411));
#136459=CARTESIAN_POINT('Ctrl Pts',(-22.9069231677594,1.82418378049299,
-7.9990909606847));
#136460=CARTESIAN_POINT('Ctrl Pts',(-22.9081161737437,1.8252112989365,-8.));
#136461=CARTESIAN_POINT('Ctrl Pts',(-22.9458263014938,1.7899950512915,-8.));
#136462=CARTESIAN_POINT('Ctrl Pts',(-22.9810576730778,1.7524411352478,-8.));
#136463=CARTESIAN_POINT('Ctrl Pts',(-23.0138046909494,1.71289020318495,
-8.));
#136464=CARTESIAN_POINT('Ctrl Pts',(-23.046551708821,1.67333927112209,-8.));
#136465=CARTESIAN_POINT('Ctrl Pts',(-23.0768147826443,1.63179054638159,
-8.00000000000002));
#136466=CARTESIAN_POINT('Ctrl Pts',(-23.1045621698079,1.58853824094364,
-8.00000000000001));
#136467=CARTESIAN_POINT('Ctrl Pts',(-23.1267698135901,1.55392122326679,
-8.00000000000001));
#136468=CARTESIAN_POINT('Ctrl Pts',(-23.1473655883184,1.51821190695519,
-8.));
#136469=CARTESIAN_POINT('Ctrl Pts',(-23.1663184581739,1.48154480791058,
-8.));
#136470=CARTESIAN_POINT('Ctrl Pts',(-23.1734626007625,1.46772341907179,
-8.));
#136471=CARTESIAN_POINT('Ctrl Pts',(-23.1803731644546,1.45376581899129,
-8.00000000000001));
#136472=CARTESIAN_POINT('Ctrl Pts',(-23.1870479342029,1.43967880704949,
-8.00000000000001));
#136473=CARTESIAN_POINT('Ctrl Pts',(-23.1929663010849,1.4271881732021,-8.00000000000001));
#136474=CARTESIAN_POINT('Ctrl Pts',(-23.1987013567933,1.41459065047149,
-8.00000000000002));
#136475=CARTESIAN_POINT('Ctrl Pts',(-23.2042388080911,1.40192073735314,
-8.00000000000001));
#136476=CARTESIAN_POINT('Ctrl Pts',(-23.2260392040861,1.35204054728949,
-8.));
#136477=CARTESIAN_POINT('Ctrl Pts',(-23.2448162561212,1.30097015180589,
-8.00000000000002));
#136478=CARTESIAN_POINT('Ctrl Pts',(-23.2605389470064,1.24903997091589,
-8.00000000000001));
#136479=CARTESIAN_POINT('Ctrl Pts',(-23.2765523292268,1.19614967106579,
-8.));
#136480=CARTESIAN_POINT('Ctrl Pts',(-23.289397971074,1.14236657698248,-8.00000000000001));
#136481=CARTESIAN_POINT('Ctrl Pts',(-23.2990023606596,1.08800528941673,
-8.));
#136482=CARTESIAN_POINT('Ctrl Pts',(-23.305511272655,1.05116454763219,-8.));
#136483=CARTESIAN_POINT('Ctrl Pts',(-23.3105306914628,1.0140575372159,-7.99999999999998));
#136484=CARTESIAN_POINT('Ctrl Pts',(-23.3140252228657,0.976776843801469,
-8.));
#136485=CARTESIAN_POINT('Ctrl Pts',(-23.315417198095,0.961926840816698,
-8.00000000000001));
#136486=CARTESIAN_POINT('Ctrl Pts',(-23.3165671044889,0.947049248713289,
-7.99999999999999));
#136487=CARTESIAN_POINT('Ctrl Pts',(-23.3174722103952,0.932149828344294,
-7.99999999999999));
#136488=CARTESIAN_POINT('Ctrl Pts',(-23.3181970285803,0.920218218178783,
-8.));
#136489=CARTESIAN_POINT('Ctrl Pts',(-23.3187647796848,0.908270504603085,
-8.00000000000002));
#136490=CARTESIAN_POINT('Ctrl Pts',(-23.3191735821551,0.896332200675252,
-8.00000000000001));
#136491=CARTESIAN_POINT('Ctrl Pts',(-23.3211180629428,0.839547312335889,
-8.));
#136492=CARTESIAN_POINT('Ctrl Pts',(-23.3194782836048,0.782867486104685,
-7.99999999999999));
#136493=CARTESIAN_POINT('Ctrl Pts',(-23.3141922606772,0.726624469789134,
-7.99999999999999));
#136494=CARTESIAN_POINT('Ctrl Pts',(-23.3115256230824,0.698251580794284,
-7.99999999999999));
#136495=CARTESIAN_POINT('Ctrl Pts',(-23.3079303289237,0.66998945784058,
-8.00000000000002));
#136496=CARTESIAN_POINT('Ctrl Pts',(-23.3033936657804,0.641879012493639,
-8.00000000000001));
#136497=CARTESIAN_POINT('Ctrl Pts',(-23.294652936409,0.587718986164878,
-7.99999999999998));
#136498=CARTESIAN_POINT('Ctrl Pts',(-23.2824210905532,0.534121732388085,
-8.));
#136499=CARTESIAN_POINT('Ctrl Pts',(-23.2669229101663,0.481296104319126,
-8.00000000000001));
#136500=CARTESIAN_POINT('Ctrl Pts',(-23.258349314679,0.452072959722687,
-8.00000000000001));
#136501=CARTESIAN_POINT('Ctrl Pts',(-23.2487751754921,0.423085955886089,
-7.99999999999999));
#136502=CARTESIAN_POINT('Ctrl Pts',(-23.2382319859601,0.394371326985252,
-8.));
#136503=CARTESIAN_POINT('Ctrl Pts',(-23.2351171946824,0.385888118429588,
-8.00000000000001));
#136504=CARTESIAN_POINT('Ctrl Pts',(-23.2319184736363,0.377430703827278,
-8.));
#136505=CARTESIAN_POINT('Ctrl Pts',(-23.2286401046448,0.369008323085798,
-8.));
#136506=CARTESIAN_POINT('Ctrl Pts',(-23.2080228662233,0.316041060317681,
-8.00000000000002));
#136507=CARTESIAN_POINT('Ctrl Pts',(-23.1842258309568,0.264365440852388,
-7.99999999999999));
#136508=CARTESIAN_POINT('Ctrl Pts',(-23.1575249531342,0.214199037169825,
-8.));
#136509=CARTESIAN_POINT('Ctrl Pts',(-23.1301428741228,0.162752772425961,
-8.00000000000002));
#136510=CARTESIAN_POINT('Ctrl Pts',(-23.0997065813885,0.112892778633516,
-8.00000000000004));
#136511=CARTESIAN_POINT('Ctrl Pts',(-23.066458234878,0.0648591349457721,
-8.00000000000002));
#136512=CARTESIAN_POINT('Ctrl Pts',(-23.0445846382061,0.0332585093815861,
-8.00000000000001));
#136513=CARTESIAN_POINT('Ctrl Pts',(-23.0214928135711,0.00244848622698404,
-8.00000000000001));
#136514=CARTESIAN_POINT('Ctrl Pts',(-22.9972402439659,-0.0274982596333189,
-7.99999999999999));
#136515=CARTESIAN_POINT('Ctrl Pts',(-22.9838653736619,-0.0440133691011212,
-7.99999999999998));
#136516=CARTESIAN_POINT('Ctrl Pts',(-22.9701373308597,-0.060265851750123,
-8.00000000000002));
#136517=CARTESIAN_POINT('Ctrl Pts',(-22.9560647132586,-0.0762428306815151,
-8.00000000000001));
#136518=CARTESIAN_POINT('Ctrl Pts',(-22.9469359143498,-0.0866069741528238,
-8.));
#136519=CARTESIAN_POINT('Ctrl Pts',(-22.9376603395824,-0.0968568604488173,
-8.));
#136520=CARTESIAN_POINT('Ctrl Pts',(-22.928256388654,-0.106972041920554,
-8.));
#136521=CARTESIAN_POINT('Ctrl Pts',(-22.8871632797553,-0.151173065183216,
-8.00000000000001));
#136522=CARTESIAN_POINT('Ctrl Pts',(-22.8435619105751,-0.19287471672912,
-7.99999999999999));
#136523=CARTESIAN_POINT('Ctrl Pts',(-22.7976981582322,-0.231817022324734,
-8.));
#136524=CARTESIAN_POINT('Ctrl Pts',(-22.7724444422472,-0.25325961860342,
-8.));
#136525=CARTESIAN_POINT('Ctrl Pts',(-22.7465039347115,-0.273865268493912,
-7.99999999999998));
#136526=CARTESIAN_POINT('Ctrl Pts',(-22.71991198962,-0.293586952417093,
-7.99999999999999));
#136527=CARTESIAN_POINT('Ctrl Pts',(-22.7075388639141,-0.302763373076619,
-7.99999999999999));
#136528=CARTESIAN_POINT('Ctrl Pts',(-22.6950246492845,-0.311748370900717,
-7.99999999999998));
#136529=CARTESIAN_POINT('Ctrl Pts',(-22.6823726478889,-0.32053695648976,
-8.));
#136530=CARTESIAN_POINT('Ctrl Pts',(-22.6726708307602,-0.327276226233617,
-8.00000000000001));
#136531=CARTESIAN_POINT('Ctrl Pts',(-22.6628888705827,-0.333899289710013,
-8.00000000000002));
#136532=CARTESIAN_POINT('Ctrl Pts',(-22.6530367480453,-0.340398569322225,
-8.00000000000002));
#136533=CARTESIAN_POINT('Ctrl Pts',(-22.6022810630418,-0.373881241456408,
-8.00000000000001));
#136534=CARTESIAN_POINT('Ctrl Pts',(-22.5496079356719,-0.404122359348019,
-7.99999999999998));
#136535=CARTESIAN_POINT('Ctrl Pts',(-22.4952451157902,-0.430847702929976,
-8.00000000000002));
#136536=CARTESIAN_POINT('Ctrl Pts',(-22.4851965086495,-0.435787705655013,
-8.00000000000002));
#136537=CARTESIAN_POINT('Ctrl Pts',(-22.4750900639388,-0.440607487982115,
-8.00000000000002));
#136538=CARTESIAN_POINT('Ctrl Pts',(-22.4649270826171,-0.445305176587642,
-8.00000000000002));
#136539=CARTESIAN_POINT('Ctrl Pts',(-22.4273267498864,-0.46268537724355,
-8.00000000000001));
#136540=CARTESIAN_POINT('Ctrl Pts',(-22.3889530471574,-0.4783952106442,
-8.));
#136541=CARTESIAN_POINT('Ctrl Pts',(-22.3499119716047,-0.492459434737854,
-8.00000000000002));
#136542=CARTESIAN_POINT('',(-22.9090732202108,1.8254401058412,-5.99954788385073));
#136543=CARTESIAN_POINT('Ctrl Pts',(-22.900798095226,1.8336325761921,-6.00000000000001));
#136544=CARTESIAN_POINT('Ctrl Pts',(-22.9033489063661,1.83072325332144,
-5.99984929461692));
#136545=CARTESIAN_POINT('Ctrl Pts',(-22.9058863641674,1.8278022226256,-5.99969858923382));
#136546=CARTESIAN_POINT('Ctrl Pts',(-22.9084103617212,1.82486960717409,
-5.99954788385073));
#136547=CARTESIAN_POINT('Ctrl Pts',(-22.3485138628787,-0.490649428218507,
-6.));
#136548=CARTESIAN_POINT('Ctrl Pts',(-22.4044028679726,-0.470227815790022,
-6.));
#136549=CARTESIAN_POINT('Ctrl Pts',(-22.4588173702241,-0.446392867385509,
-6.00000000000003));
#136550=CARTESIAN_POINT('Ctrl Pts',(-22.5115730856902,-0.419418969216882,
-6.00000000000002));
#136551=CARTESIAN_POINT('Ctrl Pts',(-22.565456234803,-0.39186861634361,
-6.00000000000001));
#136552=CARTESIAN_POINT('Ctrl Pts',(-22.6176097455121,-0.361042932611707,
-6.));
#136553=CARTESIAN_POINT('Ctrl Pts',(-22.6678060374361,-0.327189985610635,
-6.00000000000003));
#136554=CARTESIAN_POINT('Ctrl Pts',(-22.7055462084096,-0.301737587459099,
-6.00000000000005));
#136555=CARTESIAN_POINT('Ctrl Pts',(-22.7421794219536,-0.274572932256311,
-6.00000000000003));
#136556=CARTESIAN_POINT('Ctrl Pts',(-22.7775935489668,-0.245789659304715,
-6.));
#136557=CARTESIAN_POINT('Ctrl Pts',(-22.79478021356,-0.231820983529406,
-5.99999999999999));
#136558=CARTESIAN_POINT('Ctrl Pts',(-22.8116795392235,-0.217470962941808,
-6.00000000000005));
#136559=CARTESIAN_POINT('Ctrl Pts',(-22.8282773830848,-0.202749708172314,
-6.00000000000002));
#136560=CARTESIAN_POINT('Ctrl Pts',(-22.8358955754876,-0.195992845523012,
-6.00000000000001));
#136561=CARTESIAN_POINT('Ctrl Pts',(-22.8434519976646,-0.189156144639804,
-6.00000000000003));
#136562=CARTESIAN_POINT('Ctrl Pts',(-22.8509394373616,-0.182245914402203,
-6.00000000000003));
#136563=CARTESIAN_POINT('Ctrl Pts',(-22.8944102507364,-0.142126281898408,
-6.00000000000003));
#136564=CARTESIAN_POINT('Ctrl Pts',(-22.9354415666047,-0.0996417229512457,
-6.00000000000002));
#136565=CARTESIAN_POINT('Ctrl Pts',(-22.9738282935603,-0.0550316376893066,
-6.00000000000001));
#136566=CARTESIAN_POINT('Ctrl Pts',(-23.0115902613443,-0.0111475992181314,
-6.00000000000001));
#136567=CARTESIAN_POINT('Ctrl Pts',(-23.0467935106165,0.03479427217587,
-6.00000000000001));
#136568=CARTESIAN_POINT('Ctrl Pts',(-23.0792001586263,0.082590657958306,
-6.00000000000003));
#136569=CARTESIAN_POINT('Ctrl Pts',(-23.1022939499262,0.116651562924882,
-6.00000000000003));
#136570=CARTESIAN_POINT('Ctrl Pts',(-23.1239666670789,0.151654784425088,
-6.00000000000001));
#136571=CARTESIAN_POINT('Ctrl Pts',(-23.144116612275,0.187530760613085,
-6.00000000000002));
#136572=CARTESIAN_POINT('Ctrl Pts',(-23.1568808693999,0.210256886178785,
-6.00000000000003));
#136573=CARTESIAN_POINT('Ctrl Pts',(-23.1690338052687,0.23333328147849,
-5.99999999999999));
#136574=CARTESIAN_POINT('Ctrl Pts',(-23.1805465357337,0.256742489999805,
-6.00000000000001));
#136575=CARTESIAN_POINT('Ctrl Pts',(-23.1851137868955,0.266029230025591,
-6.00000000000002));
#136576=CARTESIAN_POINT('Ctrl Pts',(-23.1895802294321,0.275368546163185,
-6.00000000000001));
#136577=CARTESIAN_POINT('Ctrl Pts',(-23.1939379823001,0.284745750340967,
-6.00000000000001));
#136578=CARTESIAN_POINT('Ctrl Pts',(-23.2174796042975,0.335403647389285,
-6.));
#136579=CARTESIAN_POINT('Ctrl Pts',(-23.2379015456237,0.387262745342791,
-6.00000000000002));
#136580=CARTESIAN_POINT('Ctrl Pts',(-23.254989552808,0.440133962889093,
-6.00000000000001));
#136581=CARTESIAN_POINT('Ctrl Pts',(-23.2645258105778,0.469639659702598,
-6.00000000000001));
#136582=CARTESIAN_POINT('Ctrl Pts',(-23.2730228982952,0.499460843070488,
-6.00000000000003));
#136583=CARTESIAN_POINT('Ctrl Pts',(-23.2804365582016,0.529565852679068,
-6.00000000000002));
#136584=CARTESIAN_POINT('Ctrl Pts',(-23.2933860024121,0.582150291040888,
-6.));
#136585=CARTESIAN_POINT('Ctrl Pts',(-23.3030321297007,0.635601394376387,
-5.99999999999998));
#136586=CARTESIAN_POINT('Ctrl Pts',(-23.3094241819638,0.689622624956746,
-5.99999999999999));
#136587=CARTESIAN_POINT('Ctrl Pts',(-23.3124570061112,0.715253969293792,
-6.));
#136588=CARTESIAN_POINT('Ctrl Pts',(-23.3147566567809,0.741013543589083,
-6.00000000000002));
#136589=CARTESIAN_POINT('Ctrl Pts',(-23.3163252005774,0.766868579593576,
-6.00000000000001));
#136590=CARTESIAN_POINT('Ctrl Pts',(-23.3172283381346,0.781755415466084,
-6.00000000000001));
#136591=CARTESIAN_POINT('Ctrl Pts',(-23.3178890663563,0.79668034899549,
-6.00000000000002));
#136592=CARTESIAN_POINT('Ctrl Pts',(-23.3183070192964,0.811601449950553,
-6.00000000000001));
#136593=CARTESIAN_POINT('Ctrl Pts',(-23.3198670669725,0.867295827560084,
-5.99999999999998));
#136594=CARTESIAN_POINT('Ctrl Pts',(-23.3180563498196,0.923011937479286,
-5.99999999999999));
#136595=CARTESIAN_POINT('Ctrl Pts',(-23.3129681477124,0.978431297783051,
-6.));
#136596=CARTESIAN_POINT('Ctrl Pts',(-23.3078908445592,1.03373194954259,
-6.00000000000002));
#136597=CARTESIAN_POINT('Ctrl Pts',(-23.2995496495147,1.08873825785068,
-6.));
#136598=CARTESIAN_POINT('Ctrl Pts',(-23.2879882369054,1.14311837677537,
-6.));
#136599=CARTESIAN_POINT('Ctrl Pts',(-23.2803755700282,1.17892522357717,
-6.));
#136600=CARTESIAN_POINT('Ctrl Pts',(-23.2713657489019,1.21446022763029,
-6.00000000000002));
#136601=CARTESIAN_POINT('Ctrl Pts',(-23.2609609427906,1.24962142831958,
-5.99999999999999));
#136602=CARTESIAN_POINT('Ctrl Pts',(-23.2551733467015,1.26917958494658,
-5.99999999999997));
#136603=CARTESIAN_POINT('Ctrl Pts',(-23.2489539947974,1.28862196500248,
-5.99999999999997));
#136604=CARTESIAN_POINT('Ctrl Pts',(-23.2423022650395,1.30792997183709,
-6.));
#136605=CARTESIAN_POINT('Ctrl Pts',(-23.2386072618587,1.31865547471599,
-6.00000000000001));
#136606=CARTESIAN_POINT('Ctrl Pts',(-23.2347819386265,1.32933040930559,
-6.00000000000001));
#136607=CARTESIAN_POINT('Ctrl Pts',(-23.2308275153244,1.33994985949573,
-6.00000000000001));
#136608=CARTESIAN_POINT('Ctrl Pts',(-23.2121715534761,1.39004972045208,
-6.));
#136609=CARTESIAN_POINT('Ctrl Pts',(-23.1906400792063,1.43893237474899,
-6.00000000000003));
#136610=CARTESIAN_POINT('Ctrl Pts',(-23.1662615812377,1.48628287293513,
-6.00000000000002));
#136611=CARTESIAN_POINT('Ctrl Pts',(-23.1528667473223,1.5122997366416,-6.00000000000001));
#136612=CARTESIAN_POINT('Ctrl Pts',(-23.138611706844,1.53785350946739,-6.));
#136613=CARTESIAN_POINT('Ctrl Pts',(-23.1234964888878,1.56288705326999,
-5.99999999999999));
#136614=CARTESIAN_POINT('Ctrl Pts',(-23.1168576664729,1.57388214789589,
-5.99999999999999));
#136615=CARTESIAN_POINT('Ctrl Pts',(-23.1100516986934,1.58477863417229,
-5.99999999999999));
#136616=CARTESIAN_POINT('Ctrl Pts',(-23.1030821447323,1.59556564650599,
-5.99999999999999));
#136617=CARTESIAN_POINT('Ctrl Pts',(-23.0751444036478,1.6388058250503,-5.99999999999998));
#136618=CARTESIAN_POINT('Ctrl Pts',(-23.0446406097003,1.68019930939369,
-5.99999999999999));
#136619=CARTESIAN_POINT('Ctrl Pts',(-23.0115864199713,1.7194450443779,-5.99999999999999));
#136620=CARTESIAN_POINT('Ctrl Pts',(-23.0020837523893,1.73072770405349,
-5.99999999999998));
#136621=CARTESIAN_POINT('Ctrl Pts',(-22.9923700884712,1.7418326038274,-6.00000000000002));
#136622=CARTESIAN_POINT('Ctrl Pts',(-22.9824453147852,1.75275193981372,
-6.00000000000001));
#136623=CARTESIAN_POINT('Ctrl Pts',(-22.9593362153627,1.77817680378731,
-5.99999999999997));
#136624=CARTESIAN_POINT('Ctrl Pts',(-22.9350827358701,1.8025961952395,-5.99999999999997));
#136625=CARTESIAN_POINT('Ctrl Pts',(-22.9097689137086,1.8259702051831,-6.00000000000002));
#136626=CARTESIAN_POINT('Origin',(-21.3427505978759,0.999999999999992,-8.00000000000001));
#136627=CARTESIAN_POINT('',(-17.5765008460949,-4.73438257217951,-8.00000000000001));
#136628=CARTESIAN_POINT('',(-17.2475487670954,-4.96527972955151,-8.00000000000001));
#136629=CARTESIAN_POINT('Origin',(-18.0333567745876,-5.73502369695961,-8.00000000000001));
#136630=CARTESIAN_POINT('',(-23.3621001638699,-2.09289074983501,-8.00000000000001));
#136631=CARTESIAN_POINT('',(-20.026783119352,-3.61567382106381,-8.00000000000001));
#136632=CARTESIAN_POINT('',(-23.3621001638699,4.09289074983499,-8.00000000000001));
#136633=CARTESIAN_POINT('Origin',(-21.9500000210213,0.999999999999992,-8.00000000000001));
#136634=CARTESIAN_POINT('',(-17.5765008460949,6.73438257217959,-8.00000000000001));
#136635=CARTESIAN_POINT('',(-23.1108487927725,4.20760288347129,-8.00000000000001));
#136636=CARTESIAN_POINT('',(-17.2475487670954,6.96527972955149,-8.00000000000001));
#136637=CARTESIAN_POINT('Origin',(-18.0333567745876,7.73502369695969,-8.00000000000001));
#136638=CARTESIAN_POINT('Origin',(-2.10213452200837E-8,0.999999999999992,
-8.00000000000001));
#136639=CARTESIAN_POINT('Ctrl Pts',(22.9063568733139,1.82409293608429,-6.00117200355571));
#136640=CARTESIAN_POINT('Ctrl Pts',(23.1728199782998,1.51487469222179,-6.02690203666603));
#136641=CARTESIAN_POINT('Ctrl Pts',(23.3790636548542,0.62330421389329,-6.07835578465692));
#136642=CARTESIAN_POINT('Ctrl Pts',(22.4463190818302,-0.39338932020661,
-6.1555332475284));
#136643=CARTESIAN_POINT('Ctrl Pts',(21.0819593047411,-0.196442803679409,
-6.23270439217017));
#136644=CARTESIAN_POINT('Ctrl Pts',(20.4721203926454,1.03891473966289,-6.30987553681192));
#136645=CARTESIAN_POINT('Ctrl Pts',(21.1464761479847,2.24109341156569,-6.38704668145369));
#136646=CARTESIAN_POINT('Ctrl Pts',(22.5191453930256,2.36444026682549,-6.46421782609544));
#136647=CARTESIAN_POINT('Ctrl Pts',(23.3972008937867,1.30223241594259,-6.54138897073721));
#136648=CARTESIAN_POINT('Ctrl Pts',(23.0176396334798,-0.0226927722025083,
-6.61856011537897));
#136649=CARTESIAN_POINT('Ctrl Pts',(21.7102866388558,-0.45885387376241,
-6.69573126002073));
#136650=CARTESIAN_POINT('Ctrl Pts',(20.6112488676729,0.37272118441749,-6.77290240466248));
#136651=CARTESIAN_POINT('Ctrl Pts',(20.6755938840128,1.74941478365189,-6.85007354930426));
#136652=CARTESIAN_POINT('Ctrl Pts',(21.8474074087956,2.47485737455439,-6.92724469394601));
#136653=CARTESIAN_POINT('Ctrl Pts',(23.1083742006497,1.91864060809139,-7.00441583858777));
#136654=CARTESIAN_POINT('Ctrl Pts',(23.3627059966256,0.564117852774593,
-7.08158698322954));
#136655=CARTESIAN_POINT('Ctrl Pts',(22.3893859320526,-0.411620128968209,
-7.1587581278713));
#136656=CARTESIAN_POINT('Ctrl Pts',(21.0342371459635,-0.16064979403871,
-7.23592927251305));
#136657=CARTESIAN_POINT('Ctrl Pts',(20.4748912050807,1.09893188571729,-7.31310041715483));
#136658=CARTESIAN_POINT('Ctrl Pts',(21.1974281169335,2.27254424007929,-7.39027156179657));
#136659=CARTESIAN_POINT('Ctrl Pts',(22.5739491795643,2.34030015500749,-7.46744270643835));
#136660=CARTESIAN_POINT('Ctrl Pts',(23.4082663916087,1.24333928571779,-7.5446138510801));
#136661=CARTESIAN_POINT('Ctrl Pts',(22.9753146249661,-0.0651125751728099,
-7.62178499572186));
#136662=CARTESIAN_POINT('Ctrl Pts',(21.6514087126462,-0.447918160579306,
-7.69895614036363));
#136663=CARTESIAN_POINT('Ctrl Pts',(20.5868757451666,0.42741312763809,-7.77612728500538));
#136664=CARTESIAN_POINT('Ctrl Pts',(20.7071213310053,1.80055923895449,-7.85329842964714));
#136665=CARTESIAN_POINT('Ctrl Pts',(21.9070006438952,2.47753884950259,-7.9304695742889));
#136666=CARTESIAN_POINT('Ctrl Pts',(23.1451374810536,1.87150031592389,-8.00764071893066));
#136667=CARTESIAN_POINT('Ctrl Pts',(23.3428805758158,0.505941210960477,
-8.08482174569748));
#136668=CARTESIAN_POINT('Ctrl Pts',(22.6700359089709,-0.114446174087646,
-8.13627905758372));
#136669=CARTESIAN_POINT('Ctrl Pts',(22.2755978923469,-0.219726881556652,
-8.16201265458937));
#136670=CARTESIAN_POINT('Ctrl Pts',(22.9784824811563,1.88624358746325,-5.94620290068195));
#136671=CARTESIAN_POINT('Ctrl Pts',(23.2650414452598,1.55370501838886,-5.97193293379227));
#136672=CARTESIAN_POINT('Ctrl Pts',(23.4868394097826,0.594894932059846,
-6.02338668178316));
#136673=CARTESIAN_POINT('Ctrl Pts',(22.4837500003388,-0.498474620763636,
-6.10056414465465));
#136674=CARTESIAN_POINT('Ctrl Pts',(21.0164942449583,-0.286674980573953,
-6.17773528929641));
#136675=CARTESIAN_POINT('Ctrl Pts',(20.3606630861593,1.04184957420938,-6.25490643393818));
#136676=CARTESIAN_POINT('Ctrl Pts',(21.0858767576635,2.33469300522009,-6.33207757857993));
#136677=CARTESIAN_POINT('Ctrl Pts',(22.5620686564872,2.46734231541453,-6.4092487232217));
#136678=CARTESIAN_POINT('Ctrl Pts',(23.5063445056212,1.32502589067852,-6.48641986786346));
#136679=CARTESIAN_POINT('Ctrl Pts',(23.0981578578932,-0.0998212357164752,
-6.5635910125052));
#136680=CARTESIAN_POINT('Ctrl Pts',(21.6922081678721,-0.568876317289018,
-6.64076215714698));
#136681=CARTESIAN_POINT('Ctrl Pts',(20.5102842191986,0.325413671784407,
-6.71793330178873));
#136682=CARTESIAN_POINT('Ctrl Pts',(20.5794819463231,1.80593342968993,-6.79510444643051));
#136683=CARTESIAN_POINT('Ctrl Pts',(21.8396701806453,2.58608675476861,-6.87227559107226));
#136684=CARTESIAN_POINT('Ctrl Pts',(23.1957353577051,1.98792176519896,-6.94944673571402));
#136685=CARTESIAN_POINT('Ctrl Pts',(23.4692481053602,0.531244910672686,
-7.02661788035579));
#136686=CARTESIAN_POINT('Ctrl Pts',(22.4225231208266,-0.518080343191016,
-7.10378902499754));
#136687=CARTESIAN_POINT('Ctrl Pts',(20.9651730221392,-0.248182568030355,
-7.18096016963931));
#136688=CARTESIAN_POINT('Ctrl Pts',(20.3636428650717,1.10639303587442,-7.25813131428107));
#136689=CARTESIAN_POINT('Ctrl Pts',(21.1406713733825,2.3685157621811,-7.33530245892283));
#136690=CARTESIAN_POINT('Ctrl Pts',(22.6210055824841,2.44138162777535,-7.41247360356459));
#136691=CARTESIAN_POINT('Ctrl Pts',(23.5182445305545,1.26169121479189,-7.48964474820635));
#136692=CARTESIAN_POINT('Ctrl Pts',(23.0526408224449,-0.145440214739043,
-7.56681589284811));
#136693=CARTESIAN_POINT('Ctrl Pts',(21.6288898426426,-0.557115864968094,
-7.64398703748988));
#136694=CARTESIAN_POINT('Ctrl Pts',(20.4840729478942,0.384230319571,-7.72115818213162));
#136695=CARTESIAN_POINT('Ctrl Pts',(20.6133871001022,1.86093504851414,-7.79832932677341));
#136696=CARTESIAN_POINT('Ctrl Pts',(21.9037577612453,2.58897045862498,-7.87550047141513));
#136697=CARTESIAN_POINT('Ctrl Pts',(23.2352712159626,1.93722629164813,-7.95267161605693));
#136698=CARTESIAN_POINT('Ctrl Pts',(23.4479275099613,0.468680758633138,
-8.02985264282373));
#136699=CARTESIAN_POINT('Ctrl Pts',(22.7243388887756,-0.198494407743786,
-8.08130995470997));
#136700=CARTESIAN_POINT('Ctrl Pts',(22.3001535237779,-0.311715074725019,
-8.10704355171562));
#136701=CARTESIAN_POINT('Ctrl Pts',(23.0506080889988,1.94839423884221,-5.8912337978082));
#136702=CARTESIAN_POINT('Ctrl Pts',(23.3572629122198,1.59253534455582,-5.91696383091851));
#136703=CARTESIAN_POINT('Ctrl Pts',(23.5946151647109,0.5664856502263,-5.96841757890941));
#136704=CARTESIAN_POINT('Ctrl Pts',(22.5211809188473,-0.603559921320658,
-6.04559504178089));
#136705=CARTESIAN_POINT('Ctrl Pts',(20.9510291851757,-0.376907157468498,
-6.12276618642265));
#136706=CARTESIAN_POINT('Ctrl Pts',(20.249205779673,1.04478440875577,-6.19993733106441));
#136707=CARTESIAN_POINT('Ctrl Pts',(21.0252773673422,2.42829259887449,-6.27710847570617));
#136708=CARTESIAN_POINT('Ctrl Pts',(22.6049919199487,2.57024436400366,-6.35427962034794));
#136709=CARTESIAN_POINT('Ctrl Pts',(23.6154881174555,1.34781936541443,-6.43145076498969));
#136710=CARTESIAN_POINT('Ctrl Pts',(23.1786760823068,-0.176949699230544,
-6.50862190963147));
#136711=CARTESIAN_POINT('Ctrl Pts',(21.6741296968885,-0.678898760815727,
-6.58579305427322));
#136712=CARTESIAN_POINT('Ctrl Pts',(20.4093195707243,0.27810615915123,-6.66296419891498));
#136713=CARTESIAN_POINT('Ctrl Pts',(20.4833700086334,1.86245207572798,-6.74013534355674));
#136714=CARTESIAN_POINT('Ctrl Pts',(21.8319329524951,2.69731613498273,-6.8173064881985));
#136715=CARTESIAN_POINT('Ctrl Pts',(23.2830965147605,2.05720292230642,-6.89447763284026));
#136716=CARTESIAN_POINT('Ctrl Pts',(23.5757902140948,0.498371968570677,
-6.97164877748203));
#136717=CARTESIAN_POINT('Ctrl Pts',(22.4556603096006,-0.624540557413726,
-7.04881992212377));
#136718=CARTESIAN_POINT('Ctrl Pts',(20.8961088983147,-0.335715342022009,
-7.12599106676556));
#136719=CARTESIAN_POINT('Ctrl Pts',(20.2523945250627,1.11385418603145,-7.2031622114073));
#136720=CARTESIAN_POINT('Ctrl Pts',(21.0839146298315,2.46448728428302,-7.28033335604907));
#136721=CARTESIAN_POINT('Ctrl Pts',(22.668061985404,2.54246310054321,-7.35750450069083));
#136722=CARTESIAN_POINT('Ctrl Pts',(23.6282226695004,1.28004314386601,-7.43467564533259));
#136723=CARTESIAN_POINT('Ctrl Pts',(23.1299670199237,-0.225767854305383,
-7.51184678997435));
#136724=CARTESIAN_POINT('Ctrl Pts',(21.606370972639,-0.666313569356887,
-7.58901793461611));
#136725=CARTESIAN_POINT('Ctrl Pts',(20.3812701506218,0.341047511504016,
-7.66618907925788));
#136726=CARTESIAN_POINT('Ctrl Pts',(20.5196528691991,1.92131085807378,-7.74336022389963));
#136727=CARTESIAN_POINT('Ctrl Pts',(21.9005148785954,2.70040206774737,-7.8205313685414));
#136728=CARTESIAN_POINT('Ctrl Pts',(23.3254049508715,2.00295226737237,-7.89770251318316));
#136729=CARTESIAN_POINT('Ctrl Pts',(23.5529744441067,0.431420306305785,
-7.97488353994999));
#136730=CARTESIAN_POINT('Ctrl Pts',(22.7786418685801,-0.282542641399823,
-8.02634085183622));
#136731=CARTESIAN_POINT('Ctrl Pts',(22.3247091552089,-0.403703267893301,
-8.05207444884186));
#136732=CARTESIAN_POINT('Ctrl Pts',(23.122733696841,2.01054489022106,-5.83626469493445));
#136733=CARTESIAN_POINT('Ctrl Pts',(23.4494843791796,1.63136567072288,-5.86199472804476));
#136734=CARTESIAN_POINT('Ctrl Pts',(23.7023909196395,0.538076368392755,
-5.91344847603567));
#136735=CARTESIAN_POINT('Ctrl Pts',(22.5586118373558,-0.708645221877573,
-5.99062593890713));
#136736=CARTESIAN_POINT('Ctrl Pts',(20.885564125393,-0.467139334363051,
-6.06779708354891));
#136737=CARTESIAN_POINT('Ctrl Pts',(20.1377484731868,1.04771924330226,-6.14496822819066));
#136738=CARTESIAN_POINT('Ctrl Pts',(20.964677977021,2.52189219252879,-6.22213937283243));
#136739=CARTESIAN_POINT('Ctrl Pts',(22.6479151834103,2.6731464125927,-6.29931051747418));
#136740=CARTESIAN_POINT('Ctrl Pts',(23.72463172929,1.37061284015026,-6.37648166211595));
#136741=CARTESIAN_POINT('Ctrl Pts',(23.2591943067203,-0.254078162744511,
-6.4536528067577));
#136742=CARTESIAN_POINT('Ctrl Pts',(21.6560512259048,-0.78892120434233,
-6.53082395139948));
#136743=CARTESIAN_POINT('Ctrl Pts',(20.3083549222499,0.230798646518151,
-6.60799509604123));
#136744=CARTESIAN_POINT('Ctrl Pts',(20.3872580709438,1.91897072176602,-6.685166240683));
#136745=CARTESIAN_POINT('Ctrl Pts',(21.8241957243447,2.80854551519707,-6.76233738532475));
#136746=CARTESIAN_POINT('Ctrl Pts',(23.3704576718158,2.12648407941399,-6.83950852996651));
#136747=CARTESIAN_POINT('Ctrl Pts',(23.6823323228293,0.465499026468774,
-6.91667967460828));
#136748=CARTESIAN_POINT('Ctrl Pts',(22.4887974983745,-0.731000771636436,
-6.99385081925003));
#136749=CARTESIAN_POINT('Ctrl Pts',(20.8270447744904,-0.423248116013548,
-7.0710219638918));
#136750=CARTESIAN_POINT('Ctrl Pts',(20.1411461850536,1.12131533618847,-7.14819310853356));
#136751=CARTESIAN_POINT('Ctrl Pts',(21.0271578862804,2.56045880638504,-7.22536425317532));
#136752=CARTESIAN_POINT('Ctrl Pts',(22.7151183883238,2.64354457331116,-7.30253539781708));
#136753=CARTESIAN_POINT('Ctrl Pts',(23.7382008084462,1.29839507294001,-7.37970654245884));
#136754=CARTESIAN_POINT('Ctrl Pts',(23.2072932174024,-0.306095493871621,
-7.4568776871006));
#136755=CARTESIAN_POINT('Ctrl Pts',(21.5838521026352,-0.775511273745666,
-7.53404883174237));
#136756=CARTESIAN_POINT('Ctrl Pts',(20.2784673533496,0.297864703436921,
-7.61121997638412));
#136757=CARTESIAN_POINT('Ctrl Pts',(20.4259186382961,1.98168666763342,-7.68839112102589));
#136758=CARTESIAN_POINT('Ctrl Pts',(21.8972719959456,2.81183367686976,-7.76556226566763));
#136759=CARTESIAN_POINT('Ctrl Pts',(23.4155386857805,2.06867824309672,-7.84273341030942));
#136760=CARTESIAN_POINT('Ctrl Pts',(23.658021378252,0.394159853978335,-7.91991443707622));
#136761=CARTESIAN_POINT('Ctrl Pts',(22.8329448483847,-0.36659087505587,
-7.97137174896246));
#136762=CARTESIAN_POINT('Ctrl Pts',(22.3492647866401,-0.495691461061565,
-7.99710534596811));
#136763=CARTESIAN_POINT('Ctrl Pts',(22.3485138208359,-0.490649428218493,
-8.00000000000001));
#136764=CARTESIAN_POINT('Ctrl Pts',(22.4946838404348,-0.4372395046764,-8.00000000000001));
#136765=CARTESIAN_POINT('Ctrl Pts',(22.6317792133684,-0.360071372937282,
-8.));
#136766=CARTESIAN_POINT('Ctrl Pts',(22.8736371924913,-0.171118184548593,
-8.));
#136767=CARTESIAN_POINT('Ctrl Pts',(22.9793712212907,-0.060188077426786,
-7.99999999999999));
#136768=CARTESIAN_POINT('Ctrl Pts',(23.1641105979564,0.203461914247813,
-7.99999999999999));
#136769=CARTESIAN_POINT('Ctrl Pts',(23.238050538628,0.3598842296734,-8.));
#136770=CARTESIAN_POINT('Ctrl Pts',(23.3194606150182,0.685726918729976,
-8.));
#136771=CARTESIAN_POINT('Ctrl Pts',(23.3284814781232,0.853393148949051,
-7.99999999999999));
#136772=CARTESIAN_POINT('Ctrl Pts',(23.2899438559561,1.17524600463165,-7.99999999999999));
#136773=CARTESIAN_POINT('Ctrl Pts',(23.2442379373553,1.33069545188236,-7.99999999999999));
#136774=CARTESIAN_POINT('Ctrl Pts',(23.0995280621159,1.61978829999637,-7.99999999999999));
#136775=CARTESIAN_POINT('Ctrl Pts',(23.0071789540993,1.73842050470344,-8.00000000000001));
#136776=CARTESIAN_POINT('Ctrl Pts',(22.8985126966394,1.83623195014015,-8.00000000000001));
#136777=CARTESIAN_POINT('Ctrl Pts',(22.908116131701,1.82521129893649,-6.));
#136778=CARTESIAN_POINT('Ctrl Pts',(22.9450075044187,1.79075965967929,-5.99999999999999));
#136779=CARTESIAN_POINT('Ctrl Pts',(22.9795265199656,1.75407059764649,-5.99999999999999));
#136780=CARTESIAN_POINT('Ctrl Pts',(23.0116681749775,1.71546357193199,-6.));
#136781=CARTESIAN_POINT('Ctrl Pts',(23.045222326383,1.67515992279949,-6.00000000000001));
#136782=CARTESIAN_POINT('Ctrl Pts',(23.0761861970359,1.63276557070519,-6.00000000000003));
#136783=CARTESIAN_POINT('Ctrl Pts',(23.1045263085396,1.58859440245256,-6.));
#136784=CARTESIAN_POINT('Ctrl Pts',(23.1267477757339,1.55395981161368,-5.99999999999998));
#136785=CARTESIAN_POINT('Ctrl Pts',(23.1473556422849,1.51823166591899,-5.99999999999999));
#136786=CARTESIAN_POINT('Ctrl Pts',(23.1663188241877,1.48154470230262,-5.99999999999999));
#136787=CARTESIAN_POINT('Ctrl Pts',(23.1734630474769,1.46772318958289,-5.99999999999999));
#136788=CARTESIAN_POINT('Ctrl Pts',(23.1803736876164,1.45376546342369,-6.00000000000003));
#136789=CARTESIAN_POINT('Ctrl Pts',(23.1870485294143,1.43967832332659,-6.00000000000002));
#136790=CARTESIAN_POINT('Ctrl Pts',(23.1929667679057,1.42718798164059,-6.00000000000001));
#136791=CARTESIAN_POINT('Ctrl Pts',(23.1987017036428,1.41459075646318,-5.99999999999998));
#136792=CARTESIAN_POINT('Ctrl Pts',(23.2042390439871,1.40192114455257,-5.99999999999998));
#136793=CARTESIAN_POINT('Ctrl Pts',(23.2260395195741,1.35204095876289,-5.99999999999999));
#136794=CARTESIAN_POINT('Ctrl Pts',(23.2448166472336,1.3009705679638,-6.00000000000002));
#136795=CARTESIAN_POINT('Ctrl Pts',(23.2605394064777,1.24904038991027,-6.00000000000002));
#136796=CARTESIAN_POINT('Ctrl Pts',(23.2765528398699,1.19615015389059,-6.00000000000003));
#136797=CARTESIAN_POINT('Ctrl Pts',(23.2893985326549,1.14236712377669,-6.));
#136798=CARTESIAN_POINT('Ctrl Pts',(23.2990029696711,1.0880058968445,-6.));
#136799=CARTESIAN_POINT('Ctrl Pts',(23.3055119128261,1.05116520172179,-6.));
#136800=CARTESIAN_POINT('Ctrl Pts',(23.3105313616353,1.01405823651869,-6.00000000000003));
#136801=CARTESIAN_POINT('Ctrl Pts',(23.3140259208794,0.976777585749033,
-6.00000000000001));
#136802=CARTESIAN_POINT('Ctrl Pts',(23.315417909761,0.96192757241519,-6.));
#136803=CARTESIAN_POINT('Ctrl Pts',(23.3165678285733,0.947049969453592,
-6.));
#136804=CARTESIAN_POINT('Ctrl Pts',(23.3174729455847,0.932150537677407,
-6.));
#136805=CARTESIAN_POINT('Ctrl Pts',(23.3181977694971,0.920218970493191,
-5.99999999999999));
#136806=CARTESIAN_POINT('Ctrl Pts',(23.318765526856,0.90827129975029,-6.00000000000003));
#136807=CARTESIAN_POINT('Ctrl Pts',(23.3191743360792,0.89633303825873,-6.00000000000003));
#136808=CARTESIAN_POINT('Ctrl Pts',(23.321118854114,0.839548202064488,-6.00000000000002));
#136809=CARTESIAN_POINT('Ctrl Pts',(23.3194791044103,0.78286841978709,-6.));
#136810=CARTESIAN_POINT('Ctrl Pts',(23.3141931001774,0.726625435644048,
-6.));
#136811=CARTESIAN_POINT('Ctrl Pts',(23.3115264726282,0.69825256941879,-6.));
#136812=CARTESIAN_POINT('Ctrl Pts',(23.3079311861598,0.669990466186293,
-5.99999999999998));
#136813=CARTESIAN_POINT('Ctrl Pts',(23.3033945279323,0.641880037021434,
-5.99999999999999));
#136814=CARTESIAN_POINT('Ctrl Pts',(23.294653812508,0.587720069603197,-5.99999999999998));
#136815=CARTESIAN_POINT('Ctrl Pts',(23.2824219738809,0.534122861038484,
-6.));
#136816=CARTESIAN_POINT('Ctrl Pts',(23.2669237959758,0.481297266457223,
-6.));
#136817=CARTESIAN_POINT('Ctrl Pts',(23.2583502098308,0.45207416755008,-5.99999999999999));
#136818=CARTESIAN_POINT('Ctrl Pts',(23.2487760803925,0.423087205372294,
-6.));
#136819=CARTESIAN_POINT('Ctrl Pts',(23.238232901264,0.394372614307267,-6.));
#136820=CARTESIAN_POINT('Ctrl Pts',(23.2351181252019,0.385889449998696,
-6.));
#136821=CARTESIAN_POINT('Ctrl Pts',(23.2319194199829,0.377432078840496,
-6.));
#136822=CARTESIAN_POINT('Ctrl Pts',(23.2286410675058,0.369009740971795,
-6.));
#136823=CARTESIAN_POINT('Ctrl Pts',(23.2077852194334,0.315429474593194,
-5.99999999999999));
#136824=CARTESIAN_POINT('Ctrl Pts',(23.1836756483089,0.263170910526294,
-6.00000000000001));
#136825=CARTESIAN_POINT('Ctrl Pts',(23.1565976811258,0.212459265016296,
-5.99999999999999));
#136826=CARTESIAN_POINT('Ctrl Pts',(23.1295197139427,0.161747619506298,
-5.99999999999998));
#136827=CARTESIAN_POINT('Ctrl Pts',(23.0994728236393,0.112582008396492,
-6.00000000000002));
#136828=CARTESIAN_POINT('Ctrl Pts',(23.0666892022875,0.0651929005834847,
-6.));
#136829=CARTESIAN_POINT('Ctrl Pts',(23.0447474031548,0.0334757734987984,
-5.99999999999999));
#136830=CARTESIAN_POINT('Ctrl Pts',(23.0215785960864,0.00255455394179094,
-5.99999999999999));
#136831=CARTESIAN_POINT('Ctrl Pts',(22.9972408872701,-0.0274973225056871,
-6.));
#136832=CARTESIAN_POINT('Ctrl Pts',(22.9838659081576,-0.0440125673387116,
-6.00000000000001));
#136833=CARTESIAN_POINT('Ctrl Pts',(22.9701377514496,-0.0602651820845042,
-5.99999999999998));
#136834=CARTESIAN_POINT('Ctrl Pts',(22.956065015152,-0.0762422894537602,
-5.99999999999998));
#136835=CARTESIAN_POINT('Ctrl Pts',(22.9469362204977,-0.0866064239944117,
-5.99999999999998));
#136836=CARTESIAN_POINT('Ctrl Pts',(22.9376606505719,-0.0968563018597042,
-6.));
#136837=CARTESIAN_POINT('Ctrl Pts',(22.9282567050398,-0.106971475448321,
-6.));
#136838=CARTESIAN_POINT('Ctrl Pts',(22.8871635371534,-0.151172553076501,
-6.));
#136839=CARTESIAN_POINT('Ctrl Pts',(22.8435621095159,-0.192874259302599,
-6.));
#136840=CARTESIAN_POINT('Ctrl Pts',(22.7976983021094,-0.231816617053861,
-6.));
#136841=CARTESIAN_POINT('Ctrl Pts',(22.7724445538394,-0.253259243719703,
-6.));
#136842=CARTESIAN_POINT('Ctrl Pts',(22.7465040149394,-0.273864923103498,
-5.99999999999998));
#136843=CARTESIAN_POINT('Ctrl Pts',(22.7199120398876,-0.293586635146076,
-5.99999999999999));
#136844=CARTESIAN_POINT('Ctrl Pts',(22.7075389507337,-0.302763031442103,
-5.99999999999999));
#136845=CARTESIAN_POINT('Ctrl Pts',(22.6950247741115,-0.311748006167511,
-6.));
#136846=CARTESIAN_POINT('Ctrl Pts',(22.6823728121875,-0.320536569935376,
-6.00000000000001));
#136847=CARTESIAN_POINT('Ctrl Pts',(22.6726709906612,-0.327275847026208,
-6.00000000000002));
#136848=CARTESIAN_POINT('Ctrl Pts',(22.6628890262749,-0.333898917838801,
-6.));
#136849=CARTESIAN_POINT('Ctrl Pts',(22.653036899842,-0.340398204679071,
-6.));
#136850=CARTESIAN_POINT('Ctrl Pts',(22.6022811687816,-0.373880931194739,
-5.99999999999999));
#136851=CARTESIAN_POINT('Ctrl Pts',(22.5496080013315,-0.404122097580018,
-6.00000000000001));
#136852=CARTESIAN_POINT('Ctrl Pts',(22.4952451503003,-0.430847480914457,
-6.));
#136853=CARTESIAN_POINT('Ctrl Pts',(22.4851964761634,-0.435787521092942,
-6.));
#136854=CARTESIAN_POINT('Ctrl Pts',(22.4750899640567,-0.440607339109571,
-6.));
#136855=CARTESIAN_POINT('Ctrl Pts',(22.4649269149819,-0.445305061588132,
-6.));
#136856=CARTESIAN_POINT('Ctrl Pts',(22.4273265579104,-0.462685282948391,
-6.00000000000001));
#136857=CARTESIAN_POINT('Ctrl Pts',(22.3889528352634,-0.478395132310893,
-5.99999999999998));
#136858=CARTESIAN_POINT('Ctrl Pts',(22.3499117437079,-0.492459368208522,
-6.));
#136859=CARTESIAN_POINT('Ctrl Pts',(21.5505711827703,-0.495721263066522,
-6.00294344809566));
#136860=CARTESIAN_POINT('Ctrl Pts',(21.0669317275038,-0.366577253429168,
-6.02867446208544));
#136861=CARTESIAN_POINT('Ctrl Pts',(20.2419081461725,0.39418733824399,-6.0801291909558));
#136862=CARTESIAN_POINT('Ctrl Pts',(20.4843940653702,2.0687275523926,-6.15730763470675));
#136863=CARTESIAN_POINT('Ctrl Pts',(22.0027303798341,2.8119166544984,-6.23447877934852));
#136864=CARTESIAN_POINT('Ctrl Pts',(23.474151242975,1.98173179924762,-6.31164992399027));
#136865=CARTESIAN_POINT('Ctrl Pts',(23.6216093115122,0.297832438268553,
-6.38882106863204));
#136866=CARTESIAN_POINT('Ctrl Pts',(22.3161646492079,-0.775592716702653,
-6.4659922132738));
#136867=CARTESIAN_POINT('Ctrl Pts',(20.6926490543717,-0.306155437729512,
-6.54316335791556));
#136868=CARTESIAN_POINT('Ctrl Pts',(20.161717095599,1.29840877217903,-6.62033450255732));
#136869=CARTESIAN_POINT('Ctrl Pts',(21.1848464639594,2.64361998303321,-6.69750564719908));
#136870=CARTESIAN_POINT('Ctrl Pts',(22.872884415153,2.56053040974976,-6.77467679184084));
#136871=CARTESIAN_POINT('Ctrl Pts',(23.7589367722621,1.12132090164701,-6.8518479364826));
#136872=CARTESIAN_POINT('Ctrl Pts',(23.0730067097267,-0.423313420904212,
-6.92901908112437));
#136873=CARTESIAN_POINT('Ctrl Pts',(21.4111777371304,-0.731080198416203,
-7.00619022576612));
#136874=CARTESIAN_POINT('Ctrl Pts',(20.2175881473881,0.465474500993284,
-7.08336137040789));
#136875=CARTESIAN_POINT('Ctrl Pts',(20.5294771087722,2.12653576813143,-7.16053251504964));
#136876=CARTESIAN_POINT('Ctrl Pts',(22.0758100061732,2.80862849930232,-7.23770365969141));
#136877=CARTESIAN_POINT('Ctrl Pts',(23.5128135928929,1.91901288970015,-7.31487480433317));
#136878=CARTESIAN_POINT('Ctrl Pts',(23.5917203626195,0.230763349660865,
-7.39204594897493));
#136879=CARTESIAN_POINT('Ctrl Pts',(22.2439622189305,-0.789003284417116,
-7.46921709361669));
#136880=CARTESIAN_POINT('Ctrl Pts',(20.6407455810999,-0.254135713524417,
-7.54638823825845));
#136881=CARTESIAN_POINT('Ctrl Pts',(20.1752867958861,1.37062985966854,-7.62355938290021));
#136882=CARTESIAN_POINT('Ctrl Pts',(21.2520527599446,2.67322315928684,-7.70073052754197));
#136883=CARTESIAN_POINT('Ctrl Pts',(22.9353671726951,2.521962068814,-7.77790167218374));
#136884=CARTESIAN_POINT('Ctrl Pts',(23.7623346813402,1.04772135592905,-7.85507281682549));
#136885=CARTESIAN_POINT('Ctrl Pts',(23.0144845836534,-0.467206524124539,
-7.93224396146726));
#136886=CARTESIAN_POINT('Ctrl Pts',(21.3413603808458,-0.708723826378064,
-8.00941510610901));
#136887=CARTESIAN_POINT('Ctrl Pts',(20.1976216968665,0.537953632605372,
-8.08658625075078));
#136888=CARTESIAN_POINT('Ctrl Pts',(20.4503846191707,1.63112615715144,-8.13803368051195));
#136889=CARTESIAN_POINT('Ctrl Pts',(20.7769717213703,2.01031192241115,-8.16375739539253));
#136890=CARTESIAN_POINT('Ctrl Pts',(21.575099891413,-0.403869820655514,
-5.94805463602293));
#136891=CARTESIAN_POINT('Ctrl Pts',(21.121160476301,-0.282656475545542,
-5.97378565001271));
#136892=CARTESIAN_POINT('Ctrl Pts',(20.3468011516327,0.43138996963465,-6.02524037888307));
#136893=CARTESIAN_POINT('Ctrl Pts',(20.5743961402856,2.0030975652717,-6.10241882263404));
#136894=CARTESIAN_POINT('Ctrl Pts',(21.9994922341333,2.70064782229422,-6.17958996727579));
#136895=CARTESIAN_POINT('Ctrl Pts',(23.3805539294197,1.92144417477625,-6.25676111191756));
#136896=CARTESIAN_POINT('Ctrl Pts',(23.5189566768722,0.3409521725077,-6.3339322565593));
#136897=CARTESIAN_POINT('Ctrl Pts',(22.2936786727421,-0.666554518081695,
-6.41110340120108));
#136898=CARTESIAN_POINT('Ctrl Pts',(20.7698623018489,-0.225945131216578,
-6.48827454584284));
#136899=CARTESIAN_POINT('Ctrl Pts',(20.2715345905649,1.28008364915676,-6.5654456904846));
#136900=CARTESIAN_POINT('Ctrl Pts',(21.2318341318864,2.54268615936893,-6.64261683512636));
#136901=CARTESIAN_POINT('Ctrl Pts',(22.816210575759,2.46469907232,-6.71978797976812));
#136902=CARTESIAN_POINT('Ctrl Pts',(23.6478509317407,1.11387064999528,-6.79695912440989));
#136903=CARTESIAN_POINT('Ctrl Pts',(23.0040434673074,-0.335908505335176,
-6.87413026905164));
#136904=CARTESIAN_POINT('Ctrl Pts',(21.4442665226809,-0.624775489724847,
-6.9513014136934));
#136905=CARTESIAN_POINT('Ctrl Pts',(20.3239746309601,0.498299425864994,
-7.02847255833517));
#136906=CARTESIAN_POINT('Ctrl Pts',(20.616710658116,2.05735580941485,-7.10564370297692));
#136907=CARTESIAN_POINT('Ctrl Pts',(22.0680840797235,2.69756159094942,-7.18281484761869));
#136908=CARTESIAN_POINT('Ctrl Pts',(23.4168420451171,1.86257679990351,-7.25998599226045));
#136909=CARTESIAN_POINT('Ctrl Pts',(23.4909031923374,0.278001760743005,
-7.33715713690221));
#136910=CARTESIAN_POINT('Ctrl Pts',(22.225910155073,-0.67914155000885,-7.41432828154396));
#136911=CARTESIAN_POINT('Ctrl Pts',(20.7211461930974,-0.177119910439378,
-7.49149942618573));
#136912=CARTESIAN_POINT('Ctrl Pts',(20.2842709828186,1.34786967830866,-7.56867057082749));
#136913=CARTESIAN_POINT('Ctrl Pts',(21.2949133251971,2.57047142040939,-7.64584171546925));
#136914=CARTESIAN_POINT('Ctrl Pts',(22.8748563005945,2.42849919256336,-7.72301286011102));
#136915=CARTESIAN_POINT('Ctrl Pts',(23.6510401770406,1.04479081299699,-7.80018400475277));
#136916=CARTESIAN_POINT('Ctrl Pts',(22.9491151536813,-0.377106156573719,
-7.87735514939454));
#136917=CARTESIAN_POINT('Ctrl Pts',(21.3787366128868,-0.603792010530775,
-7.95452629403629));
#136918=CARTESIAN_POINT('Ctrl Pts',(20.3052343094811,0.566327652788141,
-8.03169743867806));
#136919=CARTESIAN_POINT('Ctrl Pts',(20.5424751959788,1.59236903755359,-8.08314486843923));
#136920=CARTESIAN_POINT('Ctrl Pts',(20.8490067589877,1.94826920786929,-8.10886858331982));
#136921=CARTESIAN_POINT('Ctrl Pts',(21.5996286000554,-0.312018378244399,
-5.89316582395021));
#136922=CARTESIAN_POINT('Ctrl Pts',(21.1753892250981,-0.198735697662014,
-5.91889683793999));
#136923=CARTESIAN_POINT('Ctrl Pts',(20.4516941570929,0.468592601025395,
-5.97035156681035));
#136924=CARTESIAN_POINT('Ctrl Pts',(20.664398215201,1.9374675781506,-6.0475300105613));
#136925=CARTESIAN_POINT('Ctrl Pts',(21.9962540884326,2.58937899009016,-6.12470115520306));
#136926=CARTESIAN_POINT('Ctrl Pts',(23.2869566158643,1.86115655030477,-6.20187229984482));
#136927=CARTESIAN_POINT('Ctrl Pts',(23.4163040422321,0.384071906746946,
-6.27904344448659));
#136928=CARTESIAN_POINT('Ctrl Pts',(22.2711926962766,-0.557516319460856,
-6.35621458912835));
#136929=CARTESIAN_POINT('Ctrl Pts',(20.847075549326,-0.145734824703645,
-6.43338573377011));
#136930=CARTESIAN_POINT('Ctrl Pts',(20.3813520855311,1.26175852613438,-6.51055687841187));
#136931=CARTESIAN_POINT('Ctrl Pts',(21.2788217998135,2.44175233570476,-6.58772802305363));
#136932=CARTESIAN_POINT('Ctrl Pts',(22.7595367363648,2.36886773489025,-6.66489916769539));
#136933=CARTESIAN_POINT('Ctrl Pts',(23.5367650912192,1.10642039834334,-6.74207031233716));
#136934=CARTESIAN_POINT('Ctrl Pts',(22.9350802248881,-0.248503589766242,
-6.81924145697891));
#136935=CARTESIAN_POINT('Ctrl Pts',(21.4773553082314,-0.518470781033478,
-6.89641260162068));
#136936=CARTESIAN_POINT('Ctrl Pts',(20.4303611145322,0.531124350736794,
-6.97358374626243));
#136937=CARTESIAN_POINT('Ctrl Pts',(20.70394420746,1.98817585069818,-7.0507548909042));
#136938=CARTESIAN_POINT('Ctrl Pts',(22.0603581532739,2.5864946825963,-7.12792603554596));
#136939=CARTESIAN_POINT('Ctrl Pts',(23.3208704973414,1.80614071010675,-7.20509718018772));
#136940=CARTESIAN_POINT('Ctrl Pts',(23.3900860220554,0.325240171825252,
-7.28226832482948));
#136941=CARTESIAN_POINT('Ctrl Pts',(22.2078580912154,-0.569279815600576,
-7.35943946947124));
#136942=CARTESIAN_POINT('Ctrl Pts',(20.8015468050948,-0.100104107354348,
-7.43661061411301));
#136943=CARTESIAN_POINT('Ctrl Pts',(20.3932551697511,1.32510949694877,-7.51378175875476));
#136944=CARTESIAN_POINT('Ctrl Pts',(21.3377738904494,2.46771968153194,-7.59095290339653));
#136945=CARTESIAN_POINT('Ctrl Pts',(22.8143454284941,2.33503631631273,-7.66812404803829));
#136946=CARTESIAN_POINT('Ctrl Pts',(23.5397456727409,1.04186027006484,-7.74529519268004));
#136947=CARTESIAN_POINT('Ctrl Pts',(22.8837457237093,-0.287005789023116,
-7.82246633732181));
#136948=CARTESIAN_POINT('Ctrl Pts',(21.4161128449277,-0.498860194683393,
-7.89963748196357));
#136949=CARTESIAN_POINT('Ctrl Pts',(20.4128469220958,0.594701672970821,
-7.97680862660533));
#136950=CARTESIAN_POINT('Ctrl Pts',(20.6345657727871,1.55361191795564,-8.0282560563665));
#136951=CARTESIAN_POINT('Ctrl Pts',(20.9210417966052,1.88622649332765,-8.05397977124709));
#136952=CARTESIAN_POINT('Ctrl Pts',(21.6241573086981,-0.220166935833395,
-5.83827701187748));
#136953=CARTESIAN_POINT('Ctrl Pts',(21.2296179738952,-0.11481491977837,
-5.86400802586726));
#136954=CARTESIAN_POINT('Ctrl Pts',(20.556587162553,0.505795232416153,-5.91546275473762));
#136955=CARTESIAN_POINT('Ctrl Pts',(20.7544002901164,1.87183759102959,-5.99264119848858));
#136956=CARTESIAN_POINT('Ctrl Pts',(21.9930159427319,2.47811015788609,-6.06981234313035));
#136957=CARTESIAN_POINT('Ctrl Pts',(23.1933593023089,1.80086892583339,-6.1469834877721));
#136958=CARTESIAN_POINT('Ctrl Pts',(23.3136514075921,0.427191640986089,
-6.22415463241387));
#136959=CARTESIAN_POINT('Ctrl Pts',(22.2487067198108,-0.44847812084011,
-6.30132577705563));
#136960=CARTESIAN_POINT('Ctrl Pts',(20.9242887968032,-0.0655245181906094,
-6.37849692169738));
#136961=CARTESIAN_POINT('Ctrl Pts',(20.4911695804971,1.24343340311209,-6.45566806633915));
#136962=CARTESIAN_POINT('Ctrl Pts',(21.3258094677405,2.34081851204049,-6.5328392109809));
#136963=CARTESIAN_POINT('Ctrl Pts',(22.7028628969708,2.27303639746039,-6.61001035562267));
#136964=CARTESIAN_POINT('Ctrl Pts',(23.4256792506978,1.09897014669149,-6.68718150026444));
#136965=CARTESIAN_POINT('Ctrl Pts',(22.8661169824689,-0.161098674197309,
-6.76435264490619));
#136966=CARTESIAN_POINT('Ctrl Pts',(21.5104440937819,-0.412166072342206,
-6.84152378954795));
#136967=CARTESIAN_POINT('Ctrl Pts',(20.5367475981041,0.563949275608491,
-6.91869493418971));
#136968=CARTESIAN_POINT('Ctrl Pts',(20.7911777568038,1.91899589198159,-6.99586607883148));
#136969=CARTESIAN_POINT('Ctrl Pts',(22.0526322268242,2.47542777424339,-7.07303722347324));
#136970=CARTESIAN_POINT('Ctrl Pts',(23.2248989495656,1.74970462031009,-7.150208368115));
#136971=CARTESIAN_POINT('Ctrl Pts',(23.2892688517734,0.372478582907392,
-7.22737951275675));
#136972=CARTESIAN_POINT('Ctrl Pts',(22.1898060273579,-0.459418081192311,
-7.30455065739853));
#136973=CARTESIAN_POINT('Ctrl Pts',(20.8819474170923,-0.023088304269212,
-7.38172180204028));
#136974=CARTESIAN_POINT('Ctrl Pts',(20.5022393566836,1.30234931558909,-7.45889294668204));
#136975=CARTESIAN_POINT('Ctrl Pts',(21.3806344557018,2.36496794265449,-7.53606409132381));
#136976=CARTESIAN_POINT('Ctrl Pts',(22.7538345563936,2.24157344006209,-7.61323523596556));
#136977=CARTESIAN_POINT('Ctrl Pts',(23.4284511684412,1.03892972713279,-7.69040638060732));
#136978=CARTESIAN_POINT('Ctrl Pts',(22.8183762937372,-0.196905421472411,
-7.76757752524909));
#136979=CARTESIAN_POINT('Ctrl Pts',(21.4534890769687,-0.39392837883621,
-7.84474866989084));
#136980=CARTESIAN_POINT('Ctrl Pts',(20.5204595347103,0.623075693153492,
-7.92191981453261));
#136981=CARTESIAN_POINT('Ctrl Pts',(20.7266563495953,1.51485479835789,-7.97336724429378));
#136982=CARTESIAN_POINT('Ctrl Pts',(20.9930768342227,1.82418377878579,-7.99909095917437));
#136983=CARTESIAN_POINT('Ctrl Pts',(20.9918838262563,1.82521129893647,-8.));
#136984=CARTESIAN_POINT('Ctrl Pts',(20.9541736290457,1.7899949864246,-7.99999999999999));
#136985=CARTESIAN_POINT('Ctrl Pts',(20.9189421813825,1.75244101387378,-8.00000000000001));
#136986=CARTESIAN_POINT('Ctrl Pts',(20.8861950848217,1.71289003134968,-8.));
#136987=CARTESIAN_POINT('Ctrl Pts',(20.853447988261,1.67333904882559,-7.99999999999999));
#136988=CARTESIAN_POINT('Ctrl Pts',(20.8231848331265,1.6317902796713,-7.99999999999998));
#136989=CARTESIAN_POINT('Ctrl Pts',(20.7954373659385,1.58853793355712,-8.00000000000001));
#136990=CARTESIAN_POINT('Ctrl Pts',(20.7732297117916,1.55392096700529,-8.00000000000003));
#136991=CARTESIAN_POINT('Ctrl Pts',(20.7526339197316,1.51821170948909,-8.));
#136992=CARTESIAN_POINT('Ctrl Pts',(20.7336810273727,1.48154467475702,-8.00000000000002));
#136993=CARTESIAN_POINT('Ctrl Pts',(20.726536783042,1.46772312973639,-8.00000000000003));
#136994=CARTESIAN_POINT('Ctrl Pts',(20.7196261229699,1.45376537070319,-7.99999999999999));
#136995=CARTESIAN_POINT('Ctrl Pts',(20.7129512623861,1.43967819719058,-7.99999999999998));
#136996=CARTESIAN_POINT('Ctrl Pts',(20.7070330573699,1.42718793167859,-7.99999999999997));
#136997=CARTESIAN_POINT('Ctrl Pts',(20.7012981529128,1.41459078408099,-8.00000000000003));
#136998=CARTESIAN_POINT('Ctrl Pts',(20.6957608414974,1.40192125070293,-8.00000000000002));
#136999=CARTESIAN_POINT('Ctrl Pts',(20.6737369579797,1.35152994950819,-7.99999999999999));
#137000=CARTESIAN_POINT('Ctrl Pts',(20.6547986385331,1.2999239934859,-8.00000000000001));
#137001=CARTESIAN_POINT('Ctrl Pts',(20.6389780553483,1.24744385996292,-8.00000000000001));
#137002=CARTESIAN_POINT('Ctrl Pts',(20.6231888957401,1.19506796491689,-8.00000000000001));
#137003=CARTESIAN_POINT('Ctrl Pts',(20.6105046386363,1.14182034428139,-8.00000000000002));
#137004=CARTESIAN_POINT('Ctrl Pts',(20.6009968185427,1.0880060551986,-7.99999999999999));
#137005=CARTESIAN_POINT('Ctrl Pts',(20.5944878672644,1.05116537223739,-7.99999999999998));
#137006=CARTESIAN_POINT('Ctrl Pts',(20.5894684106341,1.01405841881779,-8.00000000000001));
#137007=CARTESIAN_POINT('Ctrl Pts',(20.5859738441328,0.976777779161468,
-8.00000000000002));
#137008=CARTESIAN_POINT('Ctrl Pts',(20.5845818516926,0.961927763130589,
-8.00000000000002));
#137009=CARTESIAN_POINT('Ctrl Pts',(20.5834319296435,0.947050157339097,
-7.99999999999998));
#137010=CARTESIAN_POINT('Ctrl Pts',(20.5825268097375,0.932150722589904,
-7.99999999999999));
#137011=CARTESIAN_POINT('Ctrl Pts',(20.5818019843319,0.920219166600302,
-8.));
#137012=CARTESIAN_POINT('Ctrl Pts',(20.5812342253425,0.90827150701319,-7.99999999999999));
#137013=CARTESIAN_POINT('Ctrl Pts',(20.5808254143592,0.896333256574007,
-7.99999999999999));
#137014=CARTESIAN_POINT('Ctrl Pts',(20.5788808866177,0.839548433971287,
-8.00000000000002));
#137015=CARTESIAN_POINT('Ctrl Pts',(20.5805206286002,0.782868663148789,
-8.00000000000002));
#137016=CARTESIAN_POINT('Ctrl Pts',(20.5858066279648,0.726625687387986,
-8.00000000000003));
#137017=CARTESIAN_POINT('Ctrl Pts',(20.5884732528979,0.698252827095684,
-8.00000000000003));
#137018=CARTESIAN_POINT('Ctrl Pts',(20.5920685373646,0.66999072900109,-8.00000000000001));
#137019=CARTESIAN_POINT('Ctrl Pts',(20.5966051943139,0.64188030405106,-8.));
#137020=CARTESIAN_POINT('Ctrl Pts',(20.6053459061087,0.587720351984889,
-7.99999999999999));
#137021=CARTESIAN_POINT('Ctrl Pts',(20.6175777428586,0.534123155199587,
-8.00000000000002));
#137022=CARTESIAN_POINT('Ctrl Pts',(20.6330759201249,0.481297569340178,
-8.00000000000001));
#137023=CARTESIAN_POINT('Ctrl Pts',(20.6416495038376,0.45207448234359,-8.00000000000001));
#137024=CARTESIAN_POINT('Ctrl Pts',(20.6512236307377,0.423087531025189,
-7.99999999999999));
#137025=CARTESIAN_POINT('Ctrl Pts',(20.6617668071571,0.394372949822668,
-8.00000000000001));
#137026=CARTESIAN_POINT('Ctrl Pts',(20.6648815792871,0.385889796957085,
-8.00000000000001));
#137027=CARTESIAN_POINT('Ctrl Pts',(20.6680802804164,0.37743243703309,-8.00000000000001));
#137028=CARTESIAN_POINT('Ctrl Pts',(20.6713586286263,0.369010110250361,
-8.00000000000001));
#137029=CARTESIAN_POINT('Ctrl Pts',(20.6921831588778,0.315510302528568,
-7.99999999999998));
#137030=CARTESIAN_POINT('Ctrl Pts',(20.7162516631977,0.263328227715186,
-8.00000000000001));
#137031=CARTESIAN_POINT('Ctrl Pts',(20.7432800553111,0.212688089663163,
-8.00000000000001));
#137032=CARTESIAN_POINT('Ctrl Pts',(20.7703084474246,0.16204795161114,-8.));
#137033=CARTESIAN_POINT('Ctrl Pts',(20.8002972504436,0.112948872810922,
-8.00000000000002));
#137034=CARTESIAN_POINT('Ctrl Pts',(20.8330152064058,0.0656202583694562,
-7.99999999999999));
#137035=CARTESIAN_POINT('Ctrl Pts',(20.8550444161516,0.033753598492684,
-7.99999999999997));
#137036=CARTESIAN_POINT('Ctrl Pts',(20.8783119487322,0.00268967994438171,
-7.99999999999998));
#137037=CARTESIAN_POINT('Ctrl Pts',(20.9027588922466,-0.0274970785187473,
-7.99999999999999));
#137038=CARTESIAN_POINT('Ctrl Pts',(20.9161338996896,-0.0440123585939095,
-7.99999999999999));
#137039=CARTESIAN_POINT('Ctrl Pts',(20.9298620860546,-0.0602650077312124,
-8.));
#137040=CARTESIAN_POINT('Ctrl Pts',(20.943934853256,-0.076242148539782,
-8.00000000000001));
#137041=CARTESIAN_POINT('Ctrl Pts',(20.9530636468032,-0.0866062807555108,
-8.00000000000002));
#137042=CARTESIAN_POINT('Ctrl Pts',(20.9623392154689,-0.0968561564262098,
-7.99999999999999));
#137043=CARTESIAN_POINT('Ctrl Pts',(20.9717431595962,-0.106971327962954,
-7.99999999999999));
#137044=CARTESIAN_POINT('Ctrl Pts',(21.0128363428694,-0.151172419778212,
-8.00000000000002));
#137045=CARTESIAN_POINT('Ctrl Pts',(21.0564377857545,-0.192874140272209,
-7.99999999999998));
#137046=CARTESIAN_POINT('Ctrl Pts',(21.1023016075224,-0.231816511631777,
-7.99999999999999));
#137047=CARTESIAN_POINT('Ctrl Pts',(21.1275553642185,-0.253259146230811,
-7.99999999999999));
#137048=CARTESIAN_POINT('Ctrl Pts',(21.1534959113046,-0.27386483331401,
-8.00000000000003));
#137049=CARTESIAN_POINT('Ctrl Pts',(21.1800878941763,-0.293586552696765,
-7.99999999999999));
#137050=CARTESIAN_POINT('Ctrl Pts',(21.1924609737589,-0.302762942611214,
-7.99999999999997));
#137051=CARTESIAN_POINT('Ctrl Pts',(21.2049751404292,-0.311747911286012,
-8.00000000000002));
#137052=CARTESIAN_POINT('Ctrl Pts',(21.2176270920186,-0.320536469337559,
-8.));
#137053=CARTESIAN_POINT('Ctrl Pts',(21.2273289146901,-0.327275748345412,
-7.99999999999999));
#137054=CARTESIAN_POINT('Ctrl Pts',(21.2371108801724,-0.333898821072215,
-8.00000000000001));
#137055=CARTESIAN_POINT('Ctrl Pts',(21.2469630076195,-0.340398109798504,
-8.));
#137056=CARTESIAN_POINT('Ctrl Pts',(21.2977187506139,-0.373880850456119,
-7.99999999999999));
#137057=CARTESIAN_POINT('Ctrl Pts',(21.3503919284324,-0.404122029455814,
-7.99999999999999));
#137058=CARTESIAN_POINT('Ctrl Pts',(21.4047547874969,-0.430847423133963,
-7.99999999999997));
#137059=CARTESIAN_POINT('Ctrl Pts',(21.4148034792473,-0.435787473153416,
-7.99999999999997));
#137060=CARTESIAN_POINT('Ctrl Pts',(21.4249100090732,-0.440607300547516,
-7.99999999999999));
#137061=CARTESIAN_POINT('Ctrl Pts',(21.4350730759621,-0.445305031926257,
-7.99999999999999));
#137062=CARTESIAN_POINT('Ctrl Pts',(21.4726734393702,-0.462685258679122,
-7.99999999999997));
#137063=CARTESIAN_POINT('Ctrl Pts',(21.5110471671993,-0.478395112197247,
-7.99999999999998));
#137064=CARTESIAN_POINT('Ctrl Pts',(21.5500882629145,-0.492459351166239,
-7.99999999999999));
#137065=CARTESIAN_POINT('',(20.9909269206557,1.82544017965477,-5.99954793025018));
#137066=CARTESIAN_POINT('Ctrl Pts',(20.9992015084306,1.83363212414324,-6.00000000000001));
#137067=CARTESIAN_POINT('Ctrl Pts',(20.9966508632533,1.83072298777096,-5.9998493100834));
#137068=CARTESIAN_POINT('Ctrl Pts',(20.9941135696973,1.8278021450906,-5.99969862016679));
#137069=CARTESIAN_POINT('Ctrl Pts',(20.9915897346506,1.82486971914787,-5.99954793025018));
#137070=CARTESIAN_POINT('Ctrl Pts',(21.5514861371214,-0.490649428218508,
-5.99999999999999));
#137071=CARTESIAN_POINT('Ctrl Pts',(21.4949834591969,-0.470003582263612,
-6.00000000000002));
#137072=CARTESIAN_POINT('Ctrl Pts',(21.4399877915486,-0.445869143432613,
-6.));
#137073=CARTESIAN_POINT('Ctrl Pts',(21.3866896987483,-0.418529366433886,
-5.99999999999999));
#137074=CARTESIAN_POINT('Ctrl Pts',(21.3328432740675,-0.390908317244221,
-5.99999999999998));
#137075=CARTESIAN_POINT('Ctrl Pts',(21.2807287721543,-0.36001475981561,
-5.99999999999998));
#137076=CARTESIAN_POINT('Ctrl Pts',(21.2305741784146,-0.326096358997265,
-6.));
#137077=CARTESIAN_POINT('Ctrl Pts',(21.1934054239874,-0.300959983311997,
-6.00000000000002));
#137078=CARTESIAN_POINT('Ctrl Pts',(21.1573136603092,-0.27416135946932,
-5.99999999999998));
#137079=CARTESIAN_POINT('Ctrl Pts',(21.1224063705073,-0.245790103209091,
-6.));
#137080=CARTESIAN_POINT('Ctrl Pts',(21.105219694232,-0.231821456555714,
-6.00000000000001));
#137081=CARTESIAN_POINT('Ctrl Pts',(21.0883203569688,-0.217471465991212,
-6.00000000000003));
#137082=CARTESIAN_POINT('Ctrl Pts',(21.0717225016579,-0.202750241854179,
-6.));
#137083=CARTESIAN_POINT('Ctrl Pts',(21.0641043039211,-0.195993393194915,
-5.99999999999999));
#137084=CARTESIAN_POINT('Ctrl Pts',(21.0565478764263,-0.189156706417304,
-6.00000000000002));
#137085=CARTESIAN_POINT('Ctrl Pts',(21.0490604314974,-0.182246490416036,
-6.00000000000002));
#137086=CARTESIAN_POINT('Ctrl Pts',(21.0055579107356,-0.142097705627706,
-6.00000000000003));
#137087=CARTESIAN_POINT('Ctrl Pts',(20.9644984406401,-0.09958055327981,
-6.00000000000001));
#137088=CARTESIAN_POINT('Ctrl Pts',(20.9260875776447,-0.0549349400849231,
-6.));
#137089=CARTESIAN_POINT('Ctrl Pts',(20.8883573993092,-0.0110804984926149,
-5.99999999999999));
#137090=CARTESIAN_POINT('Ctrl Pts',(20.8531823109083,0.0348285706127793,
-6.00000000000002));
#137091=CARTESIAN_POINT('Ctrl Pts',(20.8207996842225,0.0825894135497585,
-6.00000000000004));
#137092=CARTESIAN_POINT('Ctrl Pts',(20.7977058825238,0.116650252605579,
-6.00000000000005));
#137093=CARTESIAN_POINT('Ctrl Pts',(20.7760331558444,0.151653411765795,
-6.00000000000002));
#137094=CARTESIAN_POINT('Ctrl Pts',(20.7558832023643,0.187529331316934,
-6.00000000000003));
#137095=CARTESIAN_POINT('Ctrl Pts',(20.7431189344056,0.210255430951394,
-6.00000000000004));
#137096=CARTESIAN_POINT('Ctrl Pts',(20.7309659887369,0.233331802916497,
-6.00000000000001));
#137097=CARTESIAN_POINT('Ctrl Pts',(20.719453249643,0.256740991241418,-6.));
#137098=CARTESIAN_POINT('Ctrl Pts',(20.7148859970124,0.266027719281294,
-6.));
#137099=CARTESIAN_POINT('Ctrl Pts',(20.7104195531109,0.275367023870494,
-6.));
#137100=CARTESIAN_POINT('Ctrl Pts',(20.7060617989844,0.284744216998827,
-6.));
#137101=CARTESIAN_POINT('Ctrl Pts',(20.6825201841584,0.335402024293288,
-6.00000000000001));
#137102=CARTESIAN_POINT('Ctrl Pts',(20.662098249384,0.387261045497689,-6.00000000000001));
#137103=CARTESIAN_POINT('Ctrl Pts',(20.6450102486691,0.440132204936083,
-6.00000000000001));
#137104=CARTESIAN_POINT('Ctrl Pts',(20.6354739824902,0.469637906510392,
-6.));
#137105=CARTESIAN_POINT('Ctrl Pts',(20.6269768889554,0.499459101243191,
-5.99999999999999));
#137106=CARTESIAN_POINT('Ctrl Pts',(20.6195632260797,0.529564129721978,
-6.));
#137107=CARTESIAN_POINT('Ctrl Pts',(20.6059643035353,0.584785948861191,
-6.00000000000002));
#137108=CARTESIAN_POINT('Ctrl Pts',(20.5960079764508,0.640963673571786,
-6.00000000000001));
#137109=CARTESIAN_POINT('Ctrl Pts',(20.5896384223682,0.697753556830416,
-6.00000000000001));
#137110=CARTESIAN_POINT('Ctrl Pts',(20.587064820506,0.720699362363084,-6.00000000000001));
#137111=CARTESIAN_POINT('Ctrl Pts',(20.5850773566103,0.743744977060889,
-6.00000000000001));
#137112=CARTESIAN_POINT('Ctrl Pts',(20.5836746271151,0.766866927816636,
-5.99999999999999));
#137113=CARTESIAN_POINT('Ctrl Pts',(20.5827714922943,0.781753788699393,
-5.99999999999998));
#137114=CARTESIAN_POINT('Ctrl Pts',(20.5821107673882,0.796678748464092,
-6.));
#137115=CARTESIAN_POINT('Ctrl Pts',(20.5816928183164,0.811599876685016,
-6.));
#137116=CARTESIAN_POINT('Ctrl Pts',(20.5801300585453,0.867391695582489,
-6.));
#137117=CARTESIAN_POINT('Ctrl Pts',(20.581949848881,0.923205339792386,-5.99999999999998));
#137118=CARTESIAN_POINT('Ctrl Pts',(20.5870584639554,0.978720641379529,
-5.99999999999999));
#137119=CARTESIAN_POINT('Ctrl Pts',(20.5921383214789,1.03392343476379,-6.00000000000001));
#137120=CARTESIAN_POINT('Ctrl Pts',(20.60047054055,1.08883235822639,-6.));
#137121=CARTESIAN_POINT('Ctrl Pts',(20.6120117156267,1.1431172831597,-6.));
#137122=CARTESIAN_POINT('Ctrl Pts',(20.6238588849131,1.19884147858242,-6.));
#137123=CARTESIAN_POINT('Ctrl Pts',(20.6390876536583,1.25390950243899,-5.99999999999996));
#137124=CARTESIAN_POINT('Ctrl Pts',(20.6576977119408,1.3079290601828,-6.00000000000001));
#137125=CARTESIAN_POINT('Ctrl Pts',(20.6613927260947,1.31865460587539,-6.00000000000002));
#137126=CARTESIAN_POINT('Ctrl Pts',(20.6652180608678,1.3293295832012,-5.99999999999997));
#137127=CARTESIAN_POINT('Ctrl Pts',(20.6691724961882,1.33994907575922,-5.99999999999997));
#137128=CARTESIAN_POINT('Ctrl Pts',(20.6878284671583,1.39004900882909,-5.99999999999996));
#137129=CARTESIAN_POINT('Ctrl Pts',(20.7093599470678,1.43893173492499,-5.99999999999996));
#137130=CARTESIAN_POINT('Ctrl Pts',(20.7337384463524,1.48628230063181,-5.99999999999997));
#137131=CARTESIAN_POINT('Ctrl Pts',(20.7471332785947,1.51229919678329,-5.99999999999997));
#137132=CARTESIAN_POINT('Ctrl Pts',(20.761388315785,1.53785300092719,-5.99999999999999));
#137133=CARTESIAN_POINT('Ctrl Pts',(20.7765035286841,1.56288657427844,-5.99999999999997));
#137134=CARTESIAN_POINT('Ctrl Pts',(20.7831423587351,1.57388169820809,-5.99999999999996));
#137135=CARTESIAN_POINT('Ctrl Pts',(20.7899483342675,1.58477821309829,-5.99999999999998));
#137136=CARTESIAN_POINT('Ctrl Pts',(20.7969178962072,1.59556525345604,-5.99999999999998));
#137137=CARTESIAN_POINT('Ctrl Pts',(20.824855624804,1.63880547550779,-5.99999999999998));
#137138=CARTESIAN_POINT('Ctrl Pts',(20.8553594001569,1.68019899715349,-5.99999999999999));
#137139=CARTESIAN_POINT('Ctrl Pts',(20.8884135643584,1.71944475979049,-6.));
#137140=CARTESIAN_POINT('Ctrl Pts',(20.8979162936708,1.730727509423,-6.));
#137141=CARTESIAN_POINT('Ctrl Pts',(20.9076300218124,1.74183249577189,-6.00000000000001));
#137142=CARTESIAN_POINT('Ctrl Pts',(20.9175548621962,1.75275191469634,-6.));
#137143=CARTESIAN_POINT('Ctrl Pts',(20.9406639670501,1.7781768068971,-5.99999999999998));
#137144=CARTESIAN_POINT('Ctrl Pts',(20.964917450545,1.8025962199065,-6.));
#137145=CARTESIAN_POINT('Ctrl Pts',(20.9902312754079,1.8259702455601,-6.));
#137146=CARTESIAN_POINT('Origin',(-2.15847961726464E-8,0.999999999999992,
-8.00000000000001));
#137147=CARTESIAN_POINT('',(17.5765008039206,6.73438257216289,-8.00000000000001));
#137148=CARTESIAN_POINT('',(17.2475487250834,6.96527972946289,-8.00000000000001));
#137149=CARTESIAN_POINT('Origin',(18.0333567325795,7.735023696867,-8.00000000000001));
#137150=CARTESIAN_POINT('',(23.3621001218732,4.09289074857519,-8.00000000000001));
#137151=CARTESIAN_POINT('',(11.1961524660154,9.64741492024149,-8.00000000000001));
#137152=CARTESIAN_POINT('',(23.3621001218732,-2.09289074857521,-8.00000000000001));
#137153=CARTESIAN_POINT('Origin',(21.9499999789786,0.999999999999992,-8.00000000000001));
#137154=CARTESIAN_POINT('',(17.5765008039206,-4.73438257216291,-8.00000000000001));
#137155=CARTESIAN_POINT('',(14.2802181394665,-6.23934398201561,-8.00000000000001));
#137156=CARTESIAN_POINT('',(17.2475487250834,-4.96527972946291,-8.00000000000001));
#137157=CARTESIAN_POINT('Origin',(18.0333567325795,-5.73502369686701,-8.00000000000001));
#137158=CARTESIAN_POINT('',(18.2499999789787,0.99999999999999,-8.00000000000001));
#137159=CARTESIAN_POINT('Origin',(-2.10213452200837E-8,0.999999999999992,
-8.00000000000001));
#137160=CARTESIAN_POINT('Origin',(-2.10213452200837E-8,0.999999999999992,
-8.00000000000001));
#137161=CARTESIAN_POINT('Origin',(-2.10213452200837E-8,0.999999999999992,
-4.55000000000001));
#137162=CARTESIAN_POINT('',(7.99999997897866,0.999999999999992,-4.6));
#137163=CARTESIAN_POINT('Origin',(-2.10213452200837E-8,0.999999999999992,
-4.6));
#137164=CARTESIAN_POINT('',(7.89999997897866,0.999999999999992,-4.50000000000001));
#137165=CARTESIAN_POINT('',(7.94999997897866,0.999999999999991,-4.55000000000001));
#137166=CARTESIAN_POINT('Origin',(-2.10213452200837E-8,0.999999999999992,
-4.50000000000001));
#137167=CARTESIAN_POINT('Origin',(-2.10213452200837E-8,0.999999999999992,
-6.00000000000001));
#137168=CARTESIAN_POINT('',(7.99999997897866,0.999999999999992,-6.00000000000001));
#137169=CARTESIAN_POINT('',(7.99999997897866,0.999999999999993,-6.00000000000001));
#137170=CARTESIAN_POINT('Origin',(-2.10213452200837E-8,0.999999999999992,
-6.00000000000001));
#137171=CARTESIAN_POINT('Origin',(-2.10213446649728E-8,0.999999999999992,
-4.50000000000001));
#137172=CARTESIAN_POINT('',(-1.50000000000001,1.00000037997959,-4.50000000000001));
#137173=CARTESIAN_POINT('Origin',(-8.88178376686733E-15,1.00000037997959,
-4.50000000000001));
#137174=CARTESIAN_POINT('Origin',(-2.10213452200837E-8,0.999999999999992,
-9.95000000000001));
#137175=CARTESIAN_POINT('',(18.2499999789787,0.999999999999992,-9.90000000000001));
#137176=CARTESIAN_POINT('',(-18.2500000210213,0.99999999999999,-9.9));
#137177=CARTESIAN_POINT('Origin',(-2.10213452200837E-8,0.999999999999992,
-9.90000000000001));
#137178=CARTESIAN_POINT('',(-18.1500000210213,0.999999999999992,-10.));
#137179=CARTESIAN_POINT('',(-18.2000000210213,0.99999999999999,-9.95000000000001));
#137180=CARTESIAN_POINT('Origin',(-2.10213452200837E-8,0.999999999999992,
-10.));
#137181=CARTESIAN_POINT('Origin',(-2.10213452200837E-8,0.999999999999992,
-9.90000000000001));
#137182=CARTESIAN_POINT('Origin',(-2.10213452200837E-8,0.999999999999992,
-6.00000000000001));
#137183=CARTESIAN_POINT('',(18.2499999789787,0.99999999999999,-6.00000000000001));
#137184=CARTESIAN_POINT('',(17.0965589791457,-5.38515233599081,-7.90000000000001));
#137185=CARTESIAN_POINT('Ctrl Pts',(17.0965589791457,-5.38515233599079,
-7.90000000000003));
#137186=CARTESIAN_POINT('Ctrl Pts',(17.1569700573172,-5.22339870696598,
-7.90000000000003));
#137187=CARTESIAN_POINT('Ctrl Pts',(17.2046206918192,-5.08939852688342,
-7.94381226975377));
#137188=CARTESIAN_POINT('Ctrl Pts',(17.2475487250834,-4.96527972946291,
-8.));
#137189=CARTESIAN_POINT('',(17.0965589791457,-5.38515233599081,-6.1));
#137190=CARTESIAN_POINT('',(17.0965589791457,-5.38515233599081,-6.00000000000001));
#137191=CARTESIAN_POINT('',(-17.0965590211555,-5.38515233607861,-6.1));
#137192=CARTESIAN_POINT('Origin',(-2.10213452200837E-8,0.999999999999992,
-6.1));
#137193=CARTESIAN_POINT('',(-17.0965590211555,-5.38515233607861,-7.90000000000001));
#137194=CARTESIAN_POINT('',(-17.0965590211555,-5.38515233607861,-6.00000000000001));
#137195=CARTESIAN_POINT('Ctrl Pts',(-17.2475487670954,-4.96527972955151,
-7.99999999999999));
#137196=CARTESIAN_POINT('Ctrl Pts',(-17.2046207338306,-5.0893985269718,
-7.94381226975377));
#137197=CARTESIAN_POINT('Ctrl Pts',(-17.1569700993279,-5.2233987070541,
-7.90000000000004));
#137198=CARTESIAN_POINT('Ctrl Pts',(-17.0965590211556,-5.38515233607859,
-7.90000000000004));
#137199=CARTESIAN_POINT('',(-17.0965590211555,7.38515233607859,-7.90000000000001));
#137200=CARTESIAN_POINT('Ctrl Pts',(-17.0965590211555,7.38515233607864,
-7.90000000000007));
#137201=CARTESIAN_POINT('Ctrl Pts',(-17.1569700993279,7.22339870705413,
-7.90000000000008));
#137202=CARTESIAN_POINT('Ctrl Pts',(-17.2046207338306,7.08939852697181,
-7.94381226975381));
#137203=CARTESIAN_POINT('Ctrl Pts',(-17.2475487670954,6.96527972955152,
-8.00000000000005));
#137204=CARTESIAN_POINT('',(-17.0965590211555,7.38515233607859,-6.1));
#137205=CARTESIAN_POINT('',(-17.0965590211555,7.38515233607859,-6.00000000000001));
#137206=CARTESIAN_POINT('',(17.0965589791457,7.38515233599079,-6.1));
#137207=CARTESIAN_POINT('Origin',(-2.10213452200837E-8,0.999999999999992,
-6.1));
#137208=CARTESIAN_POINT('',(17.0965589791457,7.38515233599079,-7.90000000000001));
#137209=CARTESIAN_POINT('',(17.0965589791457,7.38515233599079,-6.00000000000001));
#137210=CARTESIAN_POINT('Ctrl Pts',(17.2475487250834,6.96527972946289,-8.00000000000001));
#137211=CARTESIAN_POINT('Ctrl Pts',(17.2046206918192,7.08939852688341,-7.94381226975377));
#137212=CARTESIAN_POINT('Ctrl Pts',(17.1569700573172,7.22339870696597,-7.90000000000002));
#137213=CARTESIAN_POINT('Ctrl Pts',(17.0965589791457,7.3851523359908,-7.90000000000003));
#137214=CARTESIAN_POINT('Origin',(-8.88178376686733E-15,1.00000037997959,
-10.));
#137215=CARTESIAN_POINT('',(-17.5,1.00000037997959,-10.));
#137216=CARTESIAN_POINT('Origin',(-8.88178376686733E-15,1.00000037997959,
-10.));
#137217=CARTESIAN_POINT('Origin',(-2.10213452200837E-8,0.999999999999992,
-19.05));
#137218=CARTESIAN_POINT('',(18.2499999789787,0.999999999999992,-19.1));
#137219=CARTESIAN_POINT('',(-18.2500000210213,0.999999999999994,-19.1));
#137220=CARTESIAN_POINT('Origin',(-2.10213452200837E-8,0.999999999999992,
-19.1));
#137221=CARTESIAN_POINT('',(-18.1500000210213,0.999999999999992,-19.));
#137222=CARTESIAN_POINT('',(-18.2000000210213,0.999999999999994,-19.05));
#137223=CARTESIAN_POINT('Origin',(-2.10213452200837E-8,0.999999999999992,
-19.));
#137224=CARTESIAN_POINT('Origin',(-2.10213452200837E-8,0.999999999999992,
-19.1));
#137225=CARTESIAN_POINT('Origin',(-2.10213452200837E-8,0.999999999999992,
-6.00000000000001));
#137226=CARTESIAN_POINT('',(18.2499999789787,0.999999999999992,-23.4));
#137227=CARTESIAN_POINT('Origin',(-2.10213452200837E-8,0.999999999999992,
-23.4));
#137228=CARTESIAN_POINT('',(18.2499999789787,0.99999999999999,-6.00000000000001));
#137229=CARTESIAN_POINT('Origin',(-8.88178376686733E-15,1.00000037997959,
-19.));
#137230=CARTESIAN_POINT('',(-17.5,1.00000037997959,-19.));
#137231=CARTESIAN_POINT('Origin',(-8.88178376686733E-15,1.00000037997959,
-19.));
#137232=CARTESIAN_POINT('Origin',(-2.10213452200837E-8,0.999999999999992,
-23.45));
#137233=CARTESIAN_POINT('',(-2.50000002102135,0.999999999999992,-23.4));
#137234=CARTESIAN_POINT('Origin',(-2.10213452200837E-8,0.999999999999992,
-23.4));
#137235=CARTESIAN_POINT('',(-2.60000002102135,0.999999999999992,-23.5));
#137236=CARTESIAN_POINT('',(-2.55000002102135,0.999999999999992,-23.45));
#137237=CARTESIAN_POINT('Origin',(-2.10213452200837E-8,0.999999999999992,
-23.5));
#137238=CARTESIAN_POINT('Origin',(-2.10213446649728E-8,0.999999999999992,
-23.5));
#137239=CARTESIAN_POINT('',(18.1499999789787,0.999999999999992,-23.5));
#137240=CARTESIAN_POINT('Origin',(-2.10213452200837E-8,0.999999999999992,
-23.5));
#137241=CARTESIAN_POINT('Origin',(-2.10213452200837E-8,0.999999999999992,
-6.00000000000001));
#137242=CARTESIAN_POINT('',(-2.50000002102135,0.999999999999992,-23.));
#137243=CARTESIAN_POINT('',(-2.50000002102135,0.999999999999992,-6.00000000000001));
#137244=CARTESIAN_POINT('Origin',(-2.10213452200837E-8,0.999999999999992,
-23.));
#137245=CARTESIAN_POINT('Origin',(-2.10213452200837E-8,0.999999999999992,
-23.45));
#137246=CARTESIAN_POINT('',(18.1999999789787,0.999999999999994,-23.45));
#137247=CARTESIAN_POINT('Origin',(-18.0333567745876,7.73502369695969,-7.95000000000001));
#137248=CARTESIAN_POINT('',(-17.6180332032306,6.82534994715959,-7.90000000000001));
#137249=CARTESIAN_POINT('',(-17.5765008460949,6.73438257217959,-8.00000000000001));
#137250=CARTESIAN_POINT('Origin',(-18.0333567745876,7.73502369695969,-7.90000000000001));
#137251=CARTESIAN_POINT('Origin',(-23.1316149713403,4.25308657096129,-7.95000000000001));
#137252=CARTESIAN_POINT('',(-23.4036325210056,4.18385812481499,-7.90000000000001));
#137253=CARTESIAN_POINT('',(-23.3621001638699,4.09289074983499,-8.00000000000001));
#137254=CARTESIAN_POINT('',(-23.1523811499082,4.29857025845129,-7.90000000000001));
#137255=CARTESIAN_POINT('Origin',(-21.9500000210213,0.999999999999992,-7.95000000000001));
#137256=CARTESIAN_POINT('',(-23.4036325210056,-2.18385812481501,-7.90000000000001));
#137257=CARTESIAN_POINT('',(-23.3621001638699,-2.09289074983501,-8.00000000000001));
#137258=CARTESIAN_POINT('Origin',(-21.9500000210213,0.999999999999992,-7.90000000000001));
#137259=CARTESIAN_POINT('Origin',(-20.0475492979198,-3.66115750855381,-7.95000000000001));
#137260=CARTESIAN_POINT('',(-17.6180332032306,-4.82534994715961,-7.90000000000001));
#137261=CARTESIAN_POINT('',(-17.5765008460949,-4.73438257217951,-8.00000000000001));
#137262=CARTESIAN_POINT('',(-20.0683154764877,-3.70664119604381,-7.90000000000001));
#137263=CARTESIAN_POINT('Origin',(-18.0333567745876,-5.73502369695961,-7.95000000000001));
#137264=CARTESIAN_POINT('Origin',(-18.0333567745876,-5.73502369695961,-7.90000000000001));
#137265=CARTESIAN_POINT('Origin',(18.0333567325795,-5.73502369686701,-7.95000000000001));
#137266=CARTESIAN_POINT('',(17.6180331610714,-4.82534994713601,-7.90000000000001));
#137267=CARTESIAN_POINT('',(17.5765008039206,-4.73438257216291,-8.00000000000001));
#137268=CARTESIAN_POINT('Origin',(18.0333567325795,-5.73502369686701,-7.90000000000001));
#137269=CARTESIAN_POINT('Origin',(14.3009843180419,-6.28482766950221,-7.95000000000001));
#137270=CARTESIAN_POINT('',(23.403632479024,-2.18385812354831,-7.90000000000001));
#137271=CARTESIAN_POINT('',(23.3621001218732,-2.09289074857521,-8.00000000000001));
#137272=CARTESIAN_POINT('',(14.3217504966173,-6.33031135698871,-7.90000000000001));
#137273=CARTESIAN_POINT('Origin',(21.9499999789786,0.999999999999992,-7.95000000000001));
#137274=CARTESIAN_POINT('',(23.403632479024,4.18385812354829,-7.90000000000001));
#137275=CARTESIAN_POINT('',(23.3621001218732,4.09289074857519,-8.00000000000001));
#137276=CARTESIAN_POINT('Origin',(21.9499999789786,0.999999999999992,-7.90000000000001));
#137277=CARTESIAN_POINT('Origin',(11.2169186445908,9.69289860772799,-7.95000000000001));
#137278=CARTESIAN_POINT('',(17.6180331610714,6.82534994713599,-7.90000000000001));
#137279=CARTESIAN_POINT('',(17.5765008039206,6.73438257216289,-8.00000000000001));
#137280=CARTESIAN_POINT('',(11.2376848231662,9.73838229521459,-7.90000000000001));
#137281=CARTESIAN_POINT('Origin',(18.0333567325795,7.735023696867,-7.95000000000001));
#137282=CARTESIAN_POINT('Origin',(18.0333567325795,7.735023696867,-7.90000000000001));
#137283=CARTESIAN_POINT('Origin',(11.2169186448239,9.69289860762159,-6.05000000000001));
#137284=CARTESIAN_POINT('',(23.3621001218732,4.09289074857519,-6.00000000000001));
#137285=CARTESIAN_POINT('',(23.403632479024,4.18385812354829,-6.1));
#137286=CARTESIAN_POINT('',(23.3621001218732,4.09289074857519,-6.00000000000001));
#137287=CARTESIAN_POINT('',(17.6180331610714,6.82534994713599,-6.1));
#137288=CARTESIAN_POINT('',(11.2376848233993,9.73838229510809,-6.1));
#137289=CARTESIAN_POINT('',(17.5765008039206,6.73438257216289,-6.00000000000001));
#137290=CARTESIAN_POINT('',(17.6180331610714,6.82534994713599,-6.1));
#137291=CARTESIAN_POINT('',(11.1961524662485,9.64741492013499,-6.00000000000001));
#137292=CARTESIAN_POINT('Origin',(21.9499999789786,0.999999999999992,-6.05000000000001));
#137293=CARTESIAN_POINT('',(23.3621001218732,-2.09289074857521,-6.00000000000001));
#137294=CARTESIAN_POINT('',(23.403632479024,-2.18385812354831,-6.1));
#137295=CARTESIAN_POINT('',(23.3621001218732,-2.09289074857521,-6.00000000000001));
#137296=CARTESIAN_POINT('Origin',(21.9499999789786,0.999999999999992,-6.1));
#137297=CARTESIAN_POINT('Origin',(21.9499999789786,0.999999999999992,-6.00000000000001));
#137298=CARTESIAN_POINT('Origin',(14.300984318275,-6.28482766939571,-6.05000000000001));
#137299=CARTESIAN_POINT('',(17.5765008039206,-4.73438257216291,-6.00000000000001));
#137300=CARTESIAN_POINT('',(17.6180331610714,-4.82534994713601,-6.1));
#137301=CARTESIAN_POINT('',(17.5765008039206,-4.73438257216291,-6.00000000000001));
#137302=CARTESIAN_POINT('',(14.3217504968504,-6.33031135688231,-6.1));
#137303=CARTESIAN_POINT('',(14.2802181396996,-6.23934398190921,-6.00000000000001));
#137304=CARTESIAN_POINT('Origin',(18.0333567325795,-5.73502369686701,-6.05000000000001));
#137305=CARTESIAN_POINT('',(17.0028792038023,-5.35016519990321,-6.00000000000001));
#137306=CARTESIAN_POINT('',(17.0028792038023,-5.35016519990321,-6.00000000000001));
#137307=CARTESIAN_POINT('Origin',(18.0333567325795,-5.73502369686701,-6.1));
#137308=CARTESIAN_POINT('Origin',(18.0333567325795,-5.73502369686701,-6.00000000000001));
#137309=CARTESIAN_POINT('Origin',(-2.10213452200837E-8,0.999999999999992,
-6.05000000000001));
#137310=CARTESIAN_POINT('',(-17.0028792458123,-5.35016519999051,-6.00000000000001));
#137311=CARTESIAN_POINT('',(-17.0028792458123,-5.35016519999051,-6.00000000000001));
#137312=CARTESIAN_POINT('Origin',(-2.10213452200837E-8,0.999999999999992,
-6.00000000000001));
#137313=CARTESIAN_POINT('Origin',(-18.0333567745876,-5.73502369695961,-6.05000000000001));
#137314=CARTESIAN_POINT('',(-17.576500846095,-4.73438257217951,-6.00000000000001));
#137315=CARTESIAN_POINT('',(-17.6180332032306,-4.82534994715961,-6.1));
#137316=CARTESIAN_POINT('',(-17.576500846095,-4.73438257217951,-6.00000000000001));
#137317=CARTESIAN_POINT('Origin',(-18.0333567745876,-5.73502369695961,-6.1));
#137318=CARTESIAN_POINT('Origin',(-18.0333567745876,-5.73502369695961,-6.00000000000001));
#137319=CARTESIAN_POINT('Origin',(-11.2169186854654,-7.69289860705681,-6.05000000000001));
#137320=CARTESIAN_POINT('',(-23.3621001638699,-2.09289074983501,-6.00000000000001));
#137321=CARTESIAN_POINT('',(-11.1961525068975,-7.64741491956671,-6.00000000000001));
#137322=CARTESIAN_POINT('',(-23.4036325210056,-2.18385812481501,-6.1));
#137323=CARTESIAN_POINT('',(-23.3621001638699,-2.09289074983501,-6.00000000000001));
#137324=CARTESIAN_POINT('',(-11.2376848640332,-7.73838229454681,-6.1));
#137325=CARTESIAN_POINT('Origin',(-21.9500000210213,0.999999999999992,-6.05000000000001));
#137326=CARTESIAN_POINT('',(-23.3621001638699,4.09289074983499,-6.00000000000001));
#137327=CARTESIAN_POINT('',(-23.4036325210056,4.18385812481499,-6.1));
#137328=CARTESIAN_POINT('',(-23.3621001638699,4.09289074983499,-6.00000000000001));
#137329=CARTESIAN_POINT('Origin',(-21.9500000210213,0.999999999999992,-6.1));
#137330=CARTESIAN_POINT('Origin',(-21.9500000210213,0.999999999999992,-6.00000000000001));
#137331=CARTESIAN_POINT('Origin',(-14.3009843588859,8.28482766946429,-6.05000000000001));
#137332=CARTESIAN_POINT('',(-17.5765008460949,6.73438257217959,-6.00000000000001));
#137333=CARTESIAN_POINT('',(-14.280218180318,8.23934398197429,-6.00000000000001));
#137334=CARTESIAN_POINT('',(-17.6180332032306,6.82534994715959,-6.1));
#137335=CARTESIAN_POINT('',(-17.5765008460949,6.73438257217959,-6.00000000000001));
#137336=CARTESIAN_POINT('',(-14.3217505374537,8.33031135695429,-6.1));
#137337=CARTESIAN_POINT('Origin',(-18.0333567745876,7.73502369695969,-6.05000000000001));
#137338=CARTESIAN_POINT('',(-17.0028792458123,7.35016519999049,-6.00000000000001));
#137339=CARTESIAN_POINT('',(-17.0028792458123,7.35016519999049,-6.00000000000001));
#137340=CARTESIAN_POINT('Origin',(-18.0333567745876,7.73502369695969,-6.1));
#137341=CARTESIAN_POINT('Origin',(-18.0333567745876,7.73502369695969,-6.00000000000001));
#137342=CARTESIAN_POINT('Origin',(-2.10213452200837E-8,0.999999999999992,
-6.05000000000001));
#137343=CARTESIAN_POINT('',(17.0028792038023,7.35016519990319,-6.00000000000001));
#137344=CARTESIAN_POINT('',(17.0028792038023,7.35016519990319,-6.00000000000001));
#137345=CARTESIAN_POINT('Origin',(-2.10213452200837E-8,0.999999999999992,
-6.00000000000001));
#137346=CARTESIAN_POINT('Origin',(18.0333567325795,7.735023696867,-6.05000000000001));
#137347=CARTESIAN_POINT('Origin',(18.0333567325795,7.735023696867,-6.1));
#137348=CARTESIAN_POINT('Origin',(18.0333567325795,7.735023696867,-6.00000000000001));
#137349=CARTESIAN_POINT('Origin',(-21.9500000210213,0.999999999999992,-6.00000000000001));
#137350=CARTESIAN_POINT('',(-23.4036325210056,-2.18385812481501,-6.00000000000001));
#137351=CARTESIAN_POINT('',(-23.4036325210056,4.18385812481499,-6.00000000000001));
#137352=CARTESIAN_POINT('Origin',(-23.4036325210056,4.18385812481499,-6.00000000000001));
#137353=CARTESIAN_POINT('',(-17.6180332032306,6.82534994715959,-6.00000000000001));
#137354=CARTESIAN_POINT('Origin',(-18.0333567745876,7.73502369695969,-6.00000000000001));
#137355=CARTESIAN_POINT('Origin',(18.0333567325795,7.735023696867,-6.00000000000001));
#137356=CARTESIAN_POINT('',(17.6180331610714,6.82534994713599,-6.00000000000001));
#137357=CARTESIAN_POINT('Origin',(17.2355011321219,6.99999999999999,-6.00000000000001));
#137358=CARTESIAN_POINT('',(23.403632479024,4.18385812354829,-6.00000000000001));
#137359=CARTESIAN_POINT('Origin',(-2.10213446649728E-8,0.999999999999992,
-6.00000000000001));
#137360=CARTESIAN_POINT('Origin',(-18.0333567745876,-5.73502369695961,-6.00000000000001));
#137361=CARTESIAN_POINT('',(-17.6180332032306,-4.82534994715961,-6.00000000000001));
#137362=CARTESIAN_POINT('Origin',(18.0333567325795,-5.73502369686701,-6.00000000000001));
#137363=CARTESIAN_POINT('',(17.6180331610714,-4.82534994713601,-6.00000000000001));
#137364=CARTESIAN_POINT('Origin',(23.403632479024,-2.18385812354831,-6.00000000000001));
#137365=CARTESIAN_POINT('',(23.403632479024,-2.18385812354831,-6.00000000000001));
#137366=CARTESIAN_POINT('Origin',(-8.88178376686733E-15,1.00000037997959,
-0.150000000000006));
#137367=CARTESIAN_POINT('',(-1.00000000000001,1.00000037997959,-0.300000000000006));
#137368=CARTESIAN_POINT('Origin',(-8.88178376686733E-15,1.00000037997959,
-0.300000000000006));
#137369=CARTESIAN_POINT('',(-1.30000000000001,1.00000037997959,-5.55111512312578E-15));
#137370=CARTESIAN_POINT('',(-1.15000000000001,1.00000037997959,-0.150000000000006));
#137371=CARTESIAN_POINT('Origin',(-8.88178376686733E-15,1.00000037997959,
-5.55111512312578E-15));
#137372=CARTESIAN_POINT('Origin',(-8.88178376686733E-15,1.00000037997959,
-5.55111512312578E-15));
#137373=CARTESIAN_POINT('',(-1.00000000000001,1.00000037997959,-0.500000000000006));
#137374=CARTESIAN_POINT('',(-1.00000000000001,1.00000037997959,-5.55111512312578E-15));
#137375=CARTESIAN_POINT('Origin',(-8.88178376686733E-15,1.00000037997959,
-0.500000000000006));
#137376=CARTESIAN_POINT('Origin',(-8.88178376686733E-15,1.00000037997959,
-5.55111512312578E-15));
#137377=CARTESIAN_POINT('',(1.70199570552156,0.213339323115793,-5.55111512312578E-15));
#137378=CARTESIAN_POINT('',(1.83933121789749,0.63601456862469,-6.66133814775094E-15));
#137379=CARTESIAN_POINT('Origin',(-8.88178376686733E-15,1.00000037997959,
-6.66133814775094E-15));
#137380=CARTESIAN_POINT('',(2.18514148705334,0.567582069807293,-6.66133814775094E-15));
#137381=CARTESIAN_POINT('',(1.74123355294296,0.65542714523029,-6.66133814775094E-15));
#137382=CARTESIAN_POINT('',(2.99888829585913,0.91833650204669,-6.66133814775094E-15));
#137383=CARTESIAN_POINT('Ctrl Pts',(2.18514148705334,0.567582069807293,
-6.66133814775094E-15));
#137384=CARTESIAN_POINT('Ctrl Pts',(2.26527289401707,0.55964143937159,-6.66133814775094E-15));
#137385=CARTESIAN_POINT('Ctrl Pts',(2.44985190263044,0.59248302306639,-1.66533453693774E-14));
#137386=CARTESIAN_POINT('Ctrl Pts',(2.72265593195598,0.710483544687093,
-1.66533453693774E-14));
#137387=CARTESIAN_POINT('Ctrl Pts',(2.89581178365771,0.830373026122091,
-6.66133814775094E-15));
#137388=CARTESIAN_POINT('Ctrl Pts',(2.99888829585914,0.91833650204669,-6.66133814775094E-15));
#137389=CARTESIAN_POINT('',(2.99888829585914,1.08166425791249,-7.21644966006351E-15));
#137390=CARTESIAN_POINT('Origin',(-8.88178376686733E-15,1.00000037997959,
-6.66133814775094E-15));
#137391=CARTESIAN_POINT('',(2.18514148705334,1.43241869015189,-6.66133814775094E-15));
#137392=CARTESIAN_POINT('Ctrl Pts',(2.99888829585914,1.08166425791249,-6.66133814775094E-15));
#137393=CARTESIAN_POINT('Ctrl Pts',(2.88267087431383,1.18084192839999,-6.66133814775094E-15));
#137394=CARTESIAN_POINT('Ctrl Pts',(2.76068287246971,1.26224670259339,1.33226762955019E-14));
#137395=CARTESIAN_POINT('Ctrl Pts',(2.50485018029661,1.38709985462769,-3.66373598126302E-14));
#137396=CARTESIAN_POINT('Ctrl Pts',(2.33008073891961,1.44678146098259,4.32986979603811E-14));
#137397=CARTESIAN_POINT('Ctrl Pts',(2.18514148705334,1.43241869015189,-6.66133814775094E-15));
#137398=CARTESIAN_POINT('',(1.83933121789749,1.36398619133449,-6.66133814775094E-15));
#137399=CARTESIAN_POINT('',(1.74123355294296,1.34457361472889,-6.66133814775094E-15));
#137400=CARTESIAN_POINT('',(1.70199570552156,1.78666143684349,-6.66133814775094E-15));
#137401=CARTESIAN_POINT('Origin',(-8.88178376686733E-15,1.00000037997959,
-6.66133814775094E-15));
#137402=CARTESIAN_POINT('',(2.02198570368039,1.93456055863369,-6.66133814775094E-15));
#137403=CARTESIAN_POINT('',(1.61122260122708,1.74470618047739,-6.66133814775094E-15));
#137404=CARTESIAN_POINT('',(2.47415241867612,2.69663522848389,-6.66133814775094E-15));
#137405=CARTESIAN_POINT('Ctrl Pts',(2.02198570368039,1.93456055863369,-6.66133814775094E-15));
#137406=CARTESIAN_POINT('Ctrl Pts',(2.09148075916129,1.97523651292379,-6.66133814775094E-15));
#137407=CARTESIAN_POINT('Ctrl Pts',(2.22151143449857,2.11031491885179,-2.72004641033164E-14));
#137408=CARTESIAN_POINT('Ctrl Pts',(2.37285866081655,2.36613447758449,-1.66533453693774E-14));
#137409=CARTESIAN_POINT('Ctrl Pts',(2.44246540247316,2.56488442784669,-6.66133814775094E-15));
#137410=CARTESIAN_POINT('Ctrl Pts',(2.47415241867613,2.69663522848389,-6.66133814775094E-15));
#137411=CARTESIAN_POINT('',(2.3781507724882,2.82877015863239,-7.21644966006351E-15));
#137412=CARTESIAN_POINT('Origin',(-8.88178376686733E-15,1.00000037997959,
-6.66133814775094E-15));
#137413=CARTESIAN_POINT('',(1.5136474925994,2.63422808185029,-6.66133814775094E-15));
#137414=CARTESIAN_POINT('Ctrl Pts',(2.3781507724882,2.82877015863239,-6.66133814775094E-15));
#137415=CARTESIAN_POINT('Ctrl Pts',(2.22583373134628,2.84069569307559,-6.66133814775094E-15));
#137416=CARTESIAN_POINT('Ctrl Pts',(2.07929453452094,2.83485055831319,1.33226762955019E-14));
#137417=CARTESIAN_POINT('Ctrl Pts',(1.7989342669203,2.78548400016299,-3.66373598126302E-14));
#137418=CARTESIAN_POINT('Ctrl Pts',(1.62246358563372,2.73104096226529,4.32986979603811E-14));
#137419=CARTESIAN_POINT('Ctrl Pts',(1.5136474925994,2.63422808185029,-6.66133814775094E-15));
#137420=CARTESIAN_POINT('',(1.27410472160532,2.37560285103839,-6.66133814775094E-15));
#137421=CARTESIAN_POINT('',(1.20615246978637,2.30223738591519,-6.66133814775094E-15));
#137422=CARTESIAN_POINT('',(0.914555682342743,2.63683051896609,-5.55111512312578E-15));
#137423=CARTESIAN_POINT('Origin',(-8.88178376686733E-15,1.00000037997959,
-6.66133814775094E-15));
#137424=CARTESIAN_POINT('',(1.08650010626791,2.94456882374649,-5.55111512312578E-15));
#137425=CARTESIAN_POINT('',(0.865779379284463,2.54953291155349,-5.55111512312578E-15));
#137426=CARTESIAN_POINT('',(1.00437441090659,3.82687710928989,-5.55111512312578E-15));
#137427=CARTESIAN_POINT('Ctrl Pts',(1.08650010626791,2.94456882374649,-5.55111512312578E-15));
#137428=CARTESIAN_POINT('Ctrl Pts',(1.11881406112232,3.01832453074849,-5.55111512312578E-15));
#137429=CARTESIAN_POINT('Ctrl Pts',(1.14461503405761,3.20403080265529,-2.60902410786912E-14));
#137430=CARTESIAN_POINT('Ctrl Pts',(1.11669065572569,3.49995129618689,-5.55111512312578E-15));
#137431=CARTESIAN_POINT('Ctrl Pts',(1.05618025388954,3.70166331173879,-5.55111512312578E-15));
#137432=CARTESIAN_POINT('Ctrl Pts',(1.00437441090659,3.82687710928989,-5.55111512312578E-15));
#137433=CARTESIAN_POINT('',(0.849040484398591,3.87734816150549,-6.10622663543835E-15));
#137434=CARTESIAN_POINT('Origin',(-8.88178376686733E-15,1.00000037997959,
-5.55111512312578E-15));
#137435=CARTESIAN_POINT('',(0.263991602958535,3.21181803679069,-5.55111512312578E-15));
#137436=CARTESIAN_POINT('Ctrl Pts',(0.849040484398591,3.87734816150549,
-5.55111512312578E-15));
#137437=CARTESIAN_POINT('Ctrl Pts',(0.71880375631047,3.79746641108109,-5.55111512312578E-15));
#137438=CARTESIAN_POINT('Ctrl Pts',(0.603686786061961,3.70660417322209,
1.4432899320127E-14));
#137439=CARTESIAN_POINT('Ctrl Pts',(0.405887597345406,3.50187433061819,
-3.5527136788005E-14));
#137440=CARTESIAN_POINT('Ctrl Pts',(0.295120488144862,3.35410179701789,
4.44089209850062E-14));
#137441=CARTESIAN_POINT('Ctrl Pts',(0.263991602958535,3.21181803679069,
-5.55111512312578E-15));
#137442=CARTESIAN_POINT('',(0.222213526886636,2.86178612180609,-5.55111512312578E-15));
#137443=CARTESIAN_POINT('',(0.210362138786015,2.76249088224209,-5.55111512312578E-15));
#137444=CARTESIAN_POINT('',(-0.222213526886654,2.86178612180609,-6.66133814775094E-15));
#137445=CARTESIAN_POINT('Origin',(-8.88178376686733E-15,1.00000037997959,
-6.66133814775094E-15));
#137446=CARTESIAN_POINT('',(-0.263991602958553,3.21181803679069,-6.66133814775094E-15));
#137447=CARTESIAN_POINT('',(-0.210362138786033,2.76249088224209,-6.66133814775094E-15));
#137448=CARTESIAN_POINT('',(-0.849040484398609,3.87734816150549,-6.66133814775094E-15));
#137449=CARTESIAN_POINT('Ctrl Pts',(-0.263991602958553,3.21181803679069,
-6.66133814775094E-15));
#137450=CARTESIAN_POINT('Ctrl Pts',(-0.28120158117407,3.29048132329419,
-6.66133814775094E-15));
#137451=CARTESIAN_POINT('Ctrl Pts',(-0.369482464710247,3.45588532446969,
-2.72004641033164E-14));
#137452=CARTESIAN_POINT('Ctrl Pts',(-0.566011153087274,3.67887612480449,
-1.66533453693774E-14));
#137453=CARTESIAN_POINT('Ctrl Pts',(-0.733529853433388,3.80649878184449,
-6.66133814775094E-15));
#137454=CARTESIAN_POINT('Ctrl Pts',(-0.849040484398609,3.87734816150549,
-6.66133814775094E-15));
#137455=CARTESIAN_POINT('',(-1.00437441090661,3.82687710928989,-7.21644966006351E-15));
#137456=CARTESIAN_POINT('Origin',(-8.88178376686733E-15,1.00000037997959,
-6.66133814775094E-15));
#137457=CARTESIAN_POINT('',(-1.08650010626793,2.94456882374649,-6.66133814775094E-15));
#137458=CARTESIAN_POINT('Ctrl Pts',(-1.00437441090661,3.82687710928989,
-6.66133814775094E-15));
#137459=CARTESIAN_POINT('Ctrl Pts',(-1.06278482239486,3.68570018757899,
-6.66133814775094E-15));
#137460=CARTESIAN_POINT('Ctrl Pts',(-1.1025089125507,3.54452700216369,1.33226762955019E-14));
#137461=CARTESIAN_POINT('Ctrl Pts',(-1.14219463053897,3.26263359077969,
-3.66373598126302E-14));
#137462=CARTESIAN_POINT('Ctrl Pts',(-1.14494860503893,3.07797590342699,
4.32986979603811E-14));
#137463=CARTESIAN_POINT('Ctrl Pts',(-1.08650010626793,2.94456882374649,
-6.66133814775094E-15));
#137464=CARTESIAN_POINT('',(-0.914555682342761,2.63683051896609,-6.66133814775094E-15));
#137465=CARTESIAN_POINT('',(-0.86577937928448,2.54953291155349,-6.66133814775094E-15));
#137466=CARTESIAN_POINT('',(-1.27410472160534,2.37560285103839,-6.66133814775094E-15));
#137467=CARTESIAN_POINT('Origin',(-8.88178376686733E-15,1.00000037997959,
-6.66133814775094E-15));
#137468=CARTESIAN_POINT('',(-1.51364749259942,2.63422808185029,-6.66133814775094E-15));
#137469=CARTESIAN_POINT('',(-1.20615246978639,2.30223738591519,-6.66133814775094E-15));
#137470=CARTESIAN_POINT('',(-2.37815077248822,2.82877015863239,-6.66133814775094E-15));
#137471=CARTESIAN_POINT('Ctrl Pts',(-1.51364749259942,2.63422808185029,
-6.66133814775094E-15));
#137472=CARTESIAN_POINT('Ctrl Pts',(-1.57380777715219,2.68775224607759,
-6.66133814775094E-15));
#137473=CARTESIAN_POINT('Ctrl Pts',(-1.74245715676096,2.76967728864719,
-2.72004641033164E-14));
#137474=CARTESIAN_POINT('Ctrl Pts',(-2.03252503861004,2.83456450287859,
-1.66533453693774E-14));
#137475=CARTESIAN_POINT('Ctrl Pts',(-2.2430564885075,2.83934725180989,-6.66133814775094E-15));
#137476=CARTESIAN_POINT('Ctrl Pts',(-2.37815077248822,2.82877015863239,
-6.66133814775094E-15));
#137477=CARTESIAN_POINT('',(-2.47415241867615,2.69663522848389,-7.21644966006351E-15));
#137478=CARTESIAN_POINT('Origin',(-8.88178376686733E-15,1.00000037997959,
-6.66133814775094E-15));
#137479=CARTESIAN_POINT('',(-2.02198570368041,1.93456055863369,-6.66133814775094E-15));
#137480=CARTESIAN_POINT('Ctrl Pts',(-2.47415241867615,2.69663522848389,
-6.66133814775094E-15));
#137481=CARTESIAN_POINT('Ctrl Pts',(-2.43842572167288,2.54808792115299,
-6.66133814775094E-15));
#137482=CARTESIAN_POINT('Ctrl Pts',(-2.38758357586867,2.41052711593049,
1.33226762955019E-14));
#137483=CARTESIAN_POINT('Ctrl Pts',(-2.25399711176357,2.15914377278389,
-3.66373598126302E-14));
#137484=CARTESIAN_POINT('Ctrl Pts',(-2.14768624646963,2.00813398766899,
4.32986979603811E-14));
#137485=CARTESIAN_POINT('Ctrl Pts',(-2.02198570368042,1.93456055863379,
-6.66133814775094E-15));
#137486=CARTESIAN_POINT('',(-1.70199570552158,1.78666143684349,-6.66133814775094E-15));
#137487=CARTESIAN_POINT('',(-1.6112226012271,1.74470618047739,-6.66133814775094E-15));
#137488=CARTESIAN_POINT('',(-1.83933121789751,1.36398619133449,-6.66133814775094E-15));
#137489=CARTESIAN_POINT('Origin',(-8.88178376686733E-15,1.00000037997959,
-6.66133814775094E-15));
#137490=CARTESIAN_POINT('',(-2.18514148705336,1.43241869015189,-6.66133814775094E-15));
#137491=CARTESIAN_POINT('',(-1.74123355294298,1.34457361472889,-6.66133814775094E-15));
#137492=CARTESIAN_POINT('',(-2.99888829585915,1.08166425791249,-6.66133814775094E-15));
#137493=CARTESIAN_POINT('Ctrl Pts',(-2.18514148705336,1.43241869015189,
-6.66133814775094E-15));
#137494=CARTESIAN_POINT('Ctrl Pts',(-2.26527289401709,1.44035932058759,
-6.66133814775094E-15));
#137495=CARTESIAN_POINT('Ctrl Pts',(-2.4498539131878,1.40751653520809,-2.72004641033164E-14));
#137496=CARTESIAN_POINT('Ctrl Pts',(-2.72265866540928,1.28951572275389,
-6.66133814775094E-15));
#137497=CARTESIAN_POINT('Ctrl Pts',(-2.89581178365773,1.16962773383709,
-6.66133814775094E-15));
#137498=CARTESIAN_POINT('Ctrl Pts',(-2.99888829585916,1.08166425791249,
-6.66133814775094E-15));
#137499=CARTESIAN_POINT('',(-2.99888829585916,0.91833650204669,-7.21644966006351E-15));
#137500=CARTESIAN_POINT('Origin',(-8.88178376686733E-15,1.00000037997959,
-6.66133814775094E-15));
#137501=CARTESIAN_POINT('',(-2.18514148705336,0.567582069807293,-6.66133814775094E-15));
#137502=CARTESIAN_POINT('Ctrl Pts',(-2.99888829585916,0.91833650204669,
-6.66133814775094E-15));
#137503=CARTESIAN_POINT('Ctrl Pts',(-2.88267087431385,0.81915883155919,
-6.66133814775094E-15));
#137504=CARTESIAN_POINT('Ctrl Pts',(-2.76068292952053,0.737754056010891,
1.33226762955019E-14));
#137505=CARTESIAN_POINT('Ctrl Pts',(-2.50485030710536,0.61290091813639,
-3.66373598126302E-14));
#137506=CARTESIAN_POINT('Ctrl Pts',(-2.33008073891963,0.553219298973793,
4.32986979603811E-14));
#137507=CARTESIAN_POINT('Ctrl Pts',(-2.18514148705336,0.567582069807391,
-6.66133814775094E-15));
#137508=CARTESIAN_POINT('',(-1.83933121789751,0.63601456862469,-6.66133814775094E-15));
#137509=CARTESIAN_POINT('',(-1.74123355294298,0.65542714523029,-6.66133814775094E-15));
#137510=CARTESIAN_POINT('',(-1.70199570552158,0.213339323115793,-5.55111512312578E-15));
#137511=CARTESIAN_POINT('Origin',(-8.88178376686733E-15,1.00000037997959,
-6.66133814775094E-15));
#137512=CARTESIAN_POINT('',(-2.02198570368041,0.0654402013254929,-5.55111512312578E-15));
#137513=CARTESIAN_POINT('',(-1.6112226012271,0.255294579481791,-5.55111512312578E-15));
#137514=CARTESIAN_POINT('',(-2.47415241867615,-0.696634468524611,-5.55111512312578E-15));
#137515=CARTESIAN_POINT('Ctrl Pts',(-2.02198570368041,0.0654402013254929,
-5.55111512312578E-15));
#137516=CARTESIAN_POINT('Ctrl Pts',(-2.09148075916131,0.0247642470353915,
-5.55111512312578E-15));
#137517=CARTESIAN_POINT('Ctrl Pts',(-2.22149393751475,-0.110273189124808,
-2.60902410786912E-14));
#137518=CARTESIAN_POINT('Ctrl Pts',(-2.37283326403248,-0.366080159665607,
-5.55111512312578E-15));
#137519=CARTESIAN_POINT('Ctrl Pts',(-2.44246540247318,-0.564883667887508,
-5.55111512312578E-15));
#137520=CARTESIAN_POINT('Ctrl Pts',(-2.47415241867615,-0.696634468524611,
-5.55111512312578E-15));
#137521=CARTESIAN_POINT('',(-2.37815077248822,-0.82876939867321,-6.10622663543836E-15));
#137522=CARTESIAN_POINT('Origin',(-8.88178376686733E-15,1.00000037997959,
-5.55111512312578E-15));
#137523=CARTESIAN_POINT('',(-1.51364749259942,-0.634227321891108,-5.55111512312578E-15));
#137524=CARTESIAN_POINT('Ctrl Pts',(-2.37815077248822,-0.82876939867321,
-5.55111512312578E-15));
#137525=CARTESIAN_POINT('Ctrl Pts',(-2.2258337313463,-0.84069493311631,
-5.55111512312578E-15));
#137526=CARTESIAN_POINT('Ctrl Pts',(-2.07929557892755,-0.834850597287109,
1.4432899320127E-14));
#137527=CARTESIAN_POINT('Ctrl Pts',(-1.79893681959492,-0.785484727221708,
-3.5527136788005E-14));
#137528=CARTESIAN_POINT('Ctrl Pts',(-1.62246358563374,-0.731040202306308,
4.44089209850062E-14));
#137529=CARTESIAN_POINT('Ctrl Pts',(-1.51364749259942,-0.634227321891108,
-5.55111512312578E-15));
#137530=CARTESIAN_POINT('',(-1.27410472160534,-0.375602091079212,-5.55111512312578E-15));
#137531=CARTESIAN_POINT('',(-1.20615246978639,-0.302236625956009,-5.55111512312578E-15));
#137532=CARTESIAN_POINT('',(-0.914555682342761,-0.636829759006909,-6.66133814775094E-15));
#137533=CARTESIAN_POINT('Origin',(-8.88178376686733E-15,1.00000037997959,
-6.66133814775094E-15));
#137534=CARTESIAN_POINT('',(-1.08650010626793,-0.944568063787212,-6.66133814775094E-15));
#137535=CARTESIAN_POINT('',(-0.865779379284481,-0.54953215159431,-6.66133814775094E-15));
#137536=CARTESIAN_POINT('',(-1.00437441090661,-1.82687634933071,-6.66133814775094E-15));
#137537=CARTESIAN_POINT('Ctrl Pts',(-1.08650010626793,-0.944568063787212,
-6.66133814775094E-15));
#137538=CARTESIAN_POINT('Ctrl Pts',(-1.11881406112234,-1.01832377078921,
-6.66133814775094E-15));
#137539=CARTESIAN_POINT('Ctrl Pts',(-1.14463100585987,-1.20396029950631,
-2.72004641033164E-14));
#137540=CARTESIAN_POINT('Ctrl Pts',(-1.11670822644255,-1.49985676817681,
-1.66533453693774E-14));
#137541=CARTESIAN_POINT('Ctrl Pts',(-1.05618025388956,-1.70166255177951,
-6.66133814775094E-15));
#137542=CARTESIAN_POINT('Ctrl Pts',(-1.00437441090661,-1.82687634933071,
-6.66133814775094E-15));
#137543=CARTESIAN_POINT('',(-0.849040484398609,-1.87734740154631,-7.21644966006351E-15));
#137544=CARTESIAN_POINT('Origin',(-8.88178376686733E-15,1.00000037997959,
-6.66133814775094E-15));
#137545=CARTESIAN_POINT('',(-0.263991602958553,-1.21181727683151,-6.66133814775094E-15));
#137546=CARTESIAN_POINT('Ctrl Pts',(-0.849040484398609,-1.87734740154631,
-6.66133814775094E-15));
#137547=CARTESIAN_POINT('Ctrl Pts',(-0.718803756310478,-1.79746565112191,
-6.66133814775094E-15));
#137548=CARTESIAN_POINT('Ctrl Pts',(-0.603687404582928,-1.70660550831901,
1.33226762955019E-14));
#137549=CARTESIAN_POINT('Ctrl Pts',(-0.405889607552643,-1.50187812695961,
-3.66373598126302E-14));
#137550=CARTESIAN_POINT('Ctrl Pts',(-0.295120488144882,-1.35410103706051,
4.32986979603811E-14));
#137551=CARTESIAN_POINT('Ctrl Pts',(-0.263991602958552,-1.21181727683151,
-6.66133814775094E-15));
#137552=CARTESIAN_POINT('',(-0.222213526886654,-0.861785361846907,-6.66133814775094E-15));
#137553=CARTESIAN_POINT('',(-0.210362138786033,-0.762490122282808,-6.66133814775094E-15));
#137554=CARTESIAN_POINT('',(0.222213526886635,-0.861785361846907,-6.66133814775094E-15));
#137555=CARTESIAN_POINT('Origin',(-8.88178376686733E-15,1.00000037997959,
-6.66133814775094E-15));
#137556=CARTESIAN_POINT('',(0.263991602958534,-1.21181727683151,-6.66133814775094E-15));
#137557=CARTESIAN_POINT('',(0.210362138786014,-0.762490122282808,-6.66133814775094E-15));
#137558=CARTESIAN_POINT('',(0.849040484398591,-1.87734740154631,-6.66133814775094E-15));
#137559=CARTESIAN_POINT('Ctrl Pts',(0.263991602958534,-1.21181727683151,
-6.66133814775094E-15));
#137560=CARTESIAN_POINT('Ctrl Pts',(0.281201581174052,-1.29048056333501,
-6.66133814775094E-15));
#137561=CARTESIAN_POINT('Ctrl Pts',(0.369415546990755,-1.45582621508241,
-2.72004641033164E-14));
#137562=CARTESIAN_POINT('Ctrl Pts',(0.565925030419526,-1.67879393332191,
-6.66133814775094E-15));
#137563=CARTESIAN_POINT('Ctrl Pts',(0.733529853433378,-1.80649802188531,
-6.66133814775094E-15));
#137564=CARTESIAN_POINT('Ctrl Pts',(0.849040484398591,-1.87734740154631,
-6.66133814775094E-15));
#137565=CARTESIAN_POINT('',(1.00437441090659,-1.82687634933071,-7.21644966006351E-15));
#137566=CARTESIAN_POINT('Origin',(-8.88178376686733E-15,1.00000037997959,
-6.66133814775094E-15));
#137567=CARTESIAN_POINT('',(1.08650010626791,-0.944568063787212,-6.66133814775094E-15));
#137568=CARTESIAN_POINT('Ctrl Pts',(1.00437441090659,-1.82687634933071,
-6.66133814775094E-15));
#137569=CARTESIAN_POINT('Ctrl Pts',(1.06278482239484,-1.68569942761981,
-6.66133814775094E-15));
#137570=CARTESIAN_POINT('Ctrl Pts',(1.10250949831874,-1.54452789700551,
1.33226762955019E-14));
#137571=CARTESIAN_POINT('Ctrl Pts',(1.14219547135593,-1.26263671791611,
-3.66373598126302E-14));
#137572=CARTESIAN_POINT('Ctrl Pts',(1.14494860503891,-1.07797514346901,
4.32986979603811E-14));
#137573=CARTESIAN_POINT('Ctrl Pts',(1.08650010626791,-0.944568063787212,
-6.66133814775094E-15));
#137574=CARTESIAN_POINT('',(0.914555682342743,-0.636829759006909,-6.66133814775094E-15));
#137575=CARTESIAN_POINT('',(0.865779379284462,-0.54953215159431,-6.66133814775094E-15));
#137576=CARTESIAN_POINT('',(1.27410472160532,-0.375602091079212,-5.55111512312578E-15));
#137577=CARTESIAN_POINT('Origin',(-8.88178376686733E-15,1.00000037997959,
-6.66133814775094E-15));
#137578=CARTESIAN_POINT('',(1.5136474925994,-0.634227321891108,-5.55111512312578E-15));
#137579=CARTESIAN_POINT('',(1.20615246978637,-0.302236625956009,-5.55111512312578E-15));
#137580=CARTESIAN_POINT('',(2.3781507724882,-0.82876939867321,-5.55111512312578E-15));
#137581=CARTESIAN_POINT('Ctrl Pts',(1.5136474925994,-0.634227321891108,
-5.55111512312578E-15));
#137582=CARTESIAN_POINT('Ctrl Pts',(1.57380777715217,-0.687751486118411,
-5.55111512312578E-15));
#137583=CARTESIAN_POINT('Ctrl Pts',(1.74240355763935,-0.769671725923708,
-1.55431223447522E-14));
#137584=CARTESIAN_POINT('Ctrl Pts',(2.03245399589892,-0.834554549185307,
-5.55111512312578E-15));
#137585=CARTESIAN_POINT('Ctrl Pts',(2.24305648850748,-0.839346491850712,
-5.55111512312578E-15));
#137586=CARTESIAN_POINT('Ctrl Pts',(2.3781507724882,-0.82876939867321,-5.55111512312578E-15));
#137587=CARTESIAN_POINT('',(2.47415241867613,-0.696634468524611,-6.10622663543836E-15));
#137588=CARTESIAN_POINT('Origin',(-8.88178376686733E-15,1.00000037997959,
-5.55111512312578E-15));
#137589=CARTESIAN_POINT('',(2.02198570368039,0.0654402013254929,-5.55111512312578E-15));
#137590=CARTESIAN_POINT('Ctrl Pts',(2.47415241867613,-0.696634468524611,
-5.55111512312578E-15));
#137591=CARTESIAN_POINT('Ctrl Pts',(2.43842572167286,-0.548087161193807,
-5.55111512312578E-15));
#137592=CARTESIAN_POINT('Ctrl Pts',(2.38758447134345,-0.410526973901209,
1.4432899320127E-14));
#137593=CARTESIAN_POINT('Ctrl Pts',(2.2539989302801,-0.159144637220008,
-3.5527136788005E-14));
#137594=CARTESIAN_POINT('Ctrl Pts',(2.14768624646961,-0.0081332277100099,
4.44089209850062E-14));
#137595=CARTESIAN_POINT('Ctrl Pts',(2.0219857036804,0.0654402013254929,
-5.55111512312578E-15));
#137596=CARTESIAN_POINT('',(1.61122260122708,0.255294579481791,-5.55111512312578E-15));
#137597=CARTESIAN_POINT('Origin',(-8.88178376686733E-15,1.00000037997959,
-0.500000000000006));
#137598=CARTESIAN_POINT('Origin',(-8.88178376686733E-15,1.00000037997959,
-4.00000000000001));
#137599=CARTESIAN_POINT('',(0.914555682342742,-0.636829759006909,-4.00000000000001));
#137600=CARTESIAN_POINT('',(1.27410472160532,-0.375602091079212,-4.00000000000001));
#137601=CARTESIAN_POINT('Origin',(-8.88178376686733E-15,1.00000037997959,
-4.00000000000001));
#137602=CARTESIAN_POINT('',(1.0865001062679,-0.944568063787212,-4.00000000000001));
#137603=CARTESIAN_POINT('',(0.865779379284462,-0.54953215159431,-4.00000000000001));
#137604=CARTESIAN_POINT('',(1.00437441090659,-1.82687634933071,-4.00000000000001));
#137605=CARTESIAN_POINT('Ctrl Pts',(1.00437441090659,-1.82687634933071,
-4.00000000000001));
#137606=CARTESIAN_POINT('Ctrl Pts',(1.06278482239484,-1.68569942761981,
-4.00000000000001));
#137607=CARTESIAN_POINT('Ctrl Pts',(1.10250949831874,-1.54452789700551,
-3.99999999999999));
#137608=CARTESIAN_POINT('Ctrl Pts',(1.14219547135593,-1.26263671791611,
-4.00000000000004));
#137609=CARTESIAN_POINT('Ctrl Pts',(1.14494860503891,-1.07797514346901,
-3.99999999999996));
#137610=CARTESIAN_POINT('Ctrl Pts',(1.08650010626791,-0.944568063787212,
-4.00000000000001));
#137611=CARTESIAN_POINT('',(0.84904048439859,-1.87734740154631,-4.00000000000001));
#137612=CARTESIAN_POINT('Origin',(-8.88178376686733E-15,1.00000037997959,
-4.00000000000001));
#137613=CARTESIAN_POINT('',(0.263991602958534,-1.21181727683151,-4.00000000000001));
#137614=CARTESIAN_POINT('Ctrl Pts',(0.263991602958534,-1.21181727683151,
-4.00000000000001));
#137615=CARTESIAN_POINT('Ctrl Pts',(0.281201581174052,-1.29048056333501,
-4.00000000000001));
#137616=CARTESIAN_POINT('Ctrl Pts',(0.369415546990755,-1.45582621508241,
-4.00000000000003));
#137617=CARTESIAN_POINT('Ctrl Pts',(0.565925030419526,-1.67879393332191,
-4.00000000000001));
#137618=CARTESIAN_POINT('Ctrl Pts',(0.733529853433378,-1.80649802188531,
-4.00000000000001));
#137619=CARTESIAN_POINT('Ctrl Pts',(0.849040484398591,-1.87734740154631,
-4.00000000000001));
#137620=CARTESIAN_POINT('',(0.222213526886635,-0.861785361846907,-4.00000000000001));
#137621=CARTESIAN_POINT('',(0.210362138786014,-0.762490122282808,-4.00000000000001));
#137622=CARTESIAN_POINT('',(-0.222213526886654,-0.861785361846907,-4.00000000000001));
#137623=CARTESIAN_POINT('Origin',(-8.88178376686733E-15,1.00000037997959,
-4.00000000000001));
#137624=CARTESIAN_POINT('',(-0.263991602958553,-1.21181727683151,-4.00000000000001));
#137625=CARTESIAN_POINT('',(-0.210362138786033,-0.762490122282808,-4.00000000000001));
#137626=CARTESIAN_POINT('',(-0.84904048439861,-1.87734740154631,-4.00000000000001));
#137627=CARTESIAN_POINT('Ctrl Pts',(-0.84904048439861,-1.87734740154631,
-4.00000000000001));
#137628=CARTESIAN_POINT('Ctrl Pts',(-0.718803756310479,-1.79746565112191,
-4.00000000000001));
#137629=CARTESIAN_POINT('Ctrl Pts',(-0.603687404582929,-1.70660550831901,
-3.99999999999999));
#137630=CARTESIAN_POINT('Ctrl Pts',(-0.405889607552644,-1.50187812695961,
-4.00000000000004));
#137631=CARTESIAN_POINT('Ctrl Pts',(-0.295120488144883,-1.35410103706051,
-3.99999999999996));
#137632=CARTESIAN_POINT('Ctrl Pts',(-0.263991602958553,-1.21181727683151,
-4.00000000000001));
#137633=CARTESIAN_POINT('',(-1.00437441090661,-1.82687634933071,-4.00000000000001));
#137634=CARTESIAN_POINT('Origin',(-8.88178376686733E-15,1.00000037997959,
-4.00000000000001));
#137635=CARTESIAN_POINT('',(-1.08650010626793,-0.944568063787212,-4.00000000000001));
#137636=CARTESIAN_POINT('Ctrl Pts',(-1.08650010626793,-0.944568063787212,
-4.00000000000001));
#137637=CARTESIAN_POINT('Ctrl Pts',(-1.11881406112234,-1.01832377078921,
-4.00000000000001));
#137638=CARTESIAN_POINT('Ctrl Pts',(-1.14463100585987,-1.20396029950631,
-4.00000000000003));
#137639=CARTESIAN_POINT('Ctrl Pts',(-1.11670822644255,-1.49985676817681,
-4.00000000000002));
#137640=CARTESIAN_POINT('Ctrl Pts',(-1.05618025388956,-1.70166255177951,
-4.00000000000001));
#137641=CARTESIAN_POINT('Ctrl Pts',(-1.00437441090661,-1.82687634933071,
-4.00000000000001));
#137642=CARTESIAN_POINT('',(-0.914555682342761,-0.636829759006909,-4.00000000000001));
#137643=CARTESIAN_POINT('',(-0.865779379284481,-0.54953215159431,-4.00000000000001));
#137644=CARTESIAN_POINT('',(-1.27410472160534,-0.375602091079212,-4.00000000000001));
#137645=CARTESIAN_POINT('Origin',(-8.88178376686733E-15,1.00000037997959,
-4.00000000000001));
#137646=CARTESIAN_POINT('',(-1.51364749259942,-0.634227321891108,-4.00000000000001));
#137647=CARTESIAN_POINT('',(-1.20615246978639,-0.302236625956009,-4.00000000000001));
#137648=CARTESIAN_POINT('',(-2.37815077248822,-0.82876939867321,-4.00000000000001));
#137649=CARTESIAN_POINT('Ctrl Pts',(-2.37815077248822,-0.82876939867321,
-4.00000000000001));
#137650=CARTESIAN_POINT('Ctrl Pts',(-2.2258337313463,-0.84069493311631,
-4.00000000000001));
#137651=CARTESIAN_POINT('Ctrl Pts',(-2.07929557892755,-0.834850597287109,
-3.99999999999999));
#137652=CARTESIAN_POINT('Ctrl Pts',(-1.79893681959492,-0.785484727221708,
-4.00000000000004));
#137653=CARTESIAN_POINT('Ctrl Pts',(-1.62246358563374,-0.731040202306308,
-3.99999999999996));
#137654=CARTESIAN_POINT('Ctrl Pts',(-1.51364749259942,-0.634227321891108,
-4.00000000000001));
#137655=CARTESIAN_POINT('',(-2.47415241867615,-0.696634468524611,-4.00000000000001));
#137656=CARTESIAN_POINT('Origin',(-8.88178376686733E-15,1.00000037997959,
-4.00000000000001));
#137657=CARTESIAN_POINT('',(-2.02198570368041,0.0654402013254929,-4.00000000000001));
#137658=CARTESIAN_POINT('Ctrl Pts',(-2.02198570368041,0.0654402013254929,
-4.00000000000001));
#137659=CARTESIAN_POINT('Ctrl Pts',(-2.09148075916131,0.0247642470353915,
-4.00000000000001));
#137660=CARTESIAN_POINT('Ctrl Pts',(-2.22149393751475,-0.110273189124808,
-4.00000000000003));
#137661=CARTESIAN_POINT('Ctrl Pts',(-2.37283326403248,-0.366080159665607,
-4.00000000000001));
#137662=CARTESIAN_POINT('Ctrl Pts',(-2.44246540247318,-0.564883667887508,
-4.00000000000001));
#137663=CARTESIAN_POINT('Ctrl Pts',(-2.47415241867615,-0.696634468524611,
-4.00000000000001));
#137664=CARTESIAN_POINT('',(-1.70199570552158,0.213339323115793,-4.00000000000001));
#137665=CARTESIAN_POINT('',(-1.6112226012271,0.255294579481791,-4.00000000000001));
#137666=CARTESIAN_POINT('',(-1.83933121789751,0.63601456862469,-4.00000000000001));
#137667=CARTESIAN_POINT('Origin',(-8.88178376686733E-15,1.00000037997959,
-4.00000000000001));
#137668=CARTESIAN_POINT('',(-2.18514148705336,0.567582069807293,-4.00000000000001));
#137669=CARTESIAN_POINT('',(-1.74123355294298,0.65542714523029,-4.00000000000001));
#137670=CARTESIAN_POINT('',(-2.99888829585916,0.91833650204669,-4.00000000000001));
#137671=CARTESIAN_POINT('Ctrl Pts',(-2.99888829585916,0.91833650204669,
-4.00000000000001));
#137672=CARTESIAN_POINT('Ctrl Pts',(-2.88267087431385,0.81915883155919,
-4.00000000000001));
#137673=CARTESIAN_POINT('Ctrl Pts',(-2.76068292952053,0.737754056010891,
-3.99999999999999));
#137674=CARTESIAN_POINT('Ctrl Pts',(-2.50485030710536,0.61290091813639,
-4.00000000000004));
#137675=CARTESIAN_POINT('Ctrl Pts',(-2.33008073891963,0.553219298973793,
-3.99999999999996));
#137676=CARTESIAN_POINT('Ctrl Pts',(-2.18514148705336,0.567582069807391,
-4.00000000000001));
#137677=CARTESIAN_POINT('',(-2.99888829585915,1.08166425791249,-4.00000000000001));
#137678=CARTESIAN_POINT('Origin',(-8.88178376686733E-15,1.00000037997959,
-4.00000000000001));
#137679=CARTESIAN_POINT('',(-2.18514148705336,1.43241869015189,-4.00000000000001));
#137680=CARTESIAN_POINT('Ctrl Pts',(-2.18514148705336,1.43241869015189,
-4.00000000000001));
#137681=CARTESIAN_POINT('Ctrl Pts',(-2.26527289401709,1.44035932058759,
-4.00000000000001));
#137682=CARTESIAN_POINT('Ctrl Pts',(-2.4498539131878,1.40751653520809,-4.00000000000003));
#137683=CARTESIAN_POINT('Ctrl Pts',(-2.72265866540928,1.28951572275389,
-4.00000000000001));
#137684=CARTESIAN_POINT('Ctrl Pts',(-2.89581178365773,1.16962773383709,
-4.00000000000001));
#137685=CARTESIAN_POINT('Ctrl Pts',(-2.99888829585916,1.08166425791249,
-4.00000000000001));
#137686=CARTESIAN_POINT('',(-1.83933121789751,1.36398619133449,-4.00000000000001));
#137687=CARTESIAN_POINT('',(-1.74123355294298,1.34457361472889,-4.00000000000001));
#137688=CARTESIAN_POINT('',(-1.70199570552158,1.78666143684349,-4.00000000000001));
#137689=CARTESIAN_POINT('Origin',(-8.88178376686733E-15,1.00000037997959,
-4.00000000000001));
#137690=CARTESIAN_POINT('',(-2.02198570368041,1.93456055863369,-4.00000000000001));
#137691=CARTESIAN_POINT('',(-1.6112226012271,1.74470618047739,-4.00000000000001));
#137692=CARTESIAN_POINT('',(-2.47415241867615,2.69663522848389,-4.00000000000001));
#137693=CARTESIAN_POINT('Ctrl Pts',(-2.47415241867615,2.69663522848389,
-4.00000000000001));
#137694=CARTESIAN_POINT('Ctrl Pts',(-2.43842572167288,2.54808792115299,
-4.00000000000001));
#137695=CARTESIAN_POINT('Ctrl Pts',(-2.38758357586867,2.41052711593049,
-3.99999999999999));
#137696=CARTESIAN_POINT('Ctrl Pts',(-2.25399711176357,2.15914377278389,
-4.00000000000004));
#137697=CARTESIAN_POINT('Ctrl Pts',(-2.14768624646963,2.00813398766899,
-3.99999999999996));
#137698=CARTESIAN_POINT('Ctrl Pts',(-2.02198570368042,1.93456055863379,
-4.00000000000001));
#137699=CARTESIAN_POINT('',(-2.37815077248822,2.82877015863239,-4.00000000000001));
#137700=CARTESIAN_POINT('Origin',(-8.88178376686733E-15,1.00000037997959,
-4.00000000000001));
#137701=CARTESIAN_POINT('',(-1.51364749259942,2.63422808185029,-4.00000000000001));
#137702=CARTESIAN_POINT('Ctrl Pts',(-1.51364749259942,2.63422808185029,
-4.00000000000001));
#137703=CARTESIAN_POINT('Ctrl Pts',(-1.57380777715219,2.68775224607759,
-4.00000000000001));
#137704=CARTESIAN_POINT('Ctrl Pts',(-1.74245715676096,2.76967728864719,
-4.00000000000003));
#137705=CARTESIAN_POINT('Ctrl Pts',(-2.03252503861004,2.83456450287859,
-4.00000000000002));
#137706=CARTESIAN_POINT('Ctrl Pts',(-2.2430564885075,2.83934725180989,-4.00000000000001));
#137707=CARTESIAN_POINT('Ctrl Pts',(-2.37815077248822,2.82877015863239,
-4.00000000000001));
#137708=CARTESIAN_POINT('',(-1.27410472160534,2.37560285103839,-4.00000000000001));
#137709=CARTESIAN_POINT('',(-1.20615246978639,2.30223738591519,-4.00000000000001));
#137710=CARTESIAN_POINT('',(-0.914555682342761,2.63683051896609,-4.00000000000001));
#137711=CARTESIAN_POINT('Origin',(-8.88178376686733E-15,1.00000037997959,
-4.00000000000001));
#137712=CARTESIAN_POINT('',(-1.08650010626793,2.94456882374649,-4.00000000000001));
#137713=CARTESIAN_POINT('',(-0.86577937928448,2.54953291155349,-4.00000000000001));
#137714=CARTESIAN_POINT('',(-1.00437441090661,3.82687710928989,-4.00000000000001));
#137715=CARTESIAN_POINT('Ctrl Pts',(-1.00437441090661,3.82687710928989,
-4.00000000000001));
#137716=CARTESIAN_POINT('Ctrl Pts',(-1.06278482239486,3.68570018757899,
-4.00000000000001));
#137717=CARTESIAN_POINT('Ctrl Pts',(-1.1025089125507,3.54452700216369,-3.99999999999999));
#137718=CARTESIAN_POINT('Ctrl Pts',(-1.14219463053897,3.26263359077969,
-4.00000000000004));
#137719=CARTESIAN_POINT('Ctrl Pts',(-1.14494860503893,3.07797590342699,
-3.99999999999996));
#137720=CARTESIAN_POINT('Ctrl Pts',(-1.08650010626793,2.94456882374649,
-4.00000000000001));
#137721=CARTESIAN_POINT('',(-0.849040484398609,3.87734816150549,-4.00000000000001));
#137722=CARTESIAN_POINT('Origin',(-8.88178376686733E-15,1.00000037997959,
-4.00000000000001));
#137723=CARTESIAN_POINT('',(-0.263991602958553,3.21181803679069,-4.00000000000001));
#137724=CARTESIAN_POINT('Ctrl Pts',(-0.263991602958553,3.21181803679069,
-4.00000000000001));
#137725=CARTESIAN_POINT('Ctrl Pts',(-0.28120158117407,3.29048132329419,
-4.00000000000001));
#137726=CARTESIAN_POINT('Ctrl Pts',(-0.369482464710247,3.45588532446969,
-4.00000000000003));
#137727=CARTESIAN_POINT('Ctrl Pts',(-0.566011153087274,3.67887612480449,
-4.00000000000002));
#137728=CARTESIAN_POINT('Ctrl Pts',(-0.733529853433388,3.80649878184449,
-4.00000000000001));
#137729=CARTESIAN_POINT('Ctrl Pts',(-0.849040484398609,3.87734816150549,
-4.00000000000001));
#137730=CARTESIAN_POINT('',(-0.222213526886653,2.86178612180609,-4.00000000000001));
#137731=CARTESIAN_POINT('',(-0.210362138786032,2.76249088224209,-4.00000000000001));
#137732=CARTESIAN_POINT('',(0.222213526886636,2.86178612180609,-4.00000000000001));
#137733=CARTESIAN_POINT('Origin',(-8.88178376686733E-15,1.00000037997959,
-4.00000000000001));
#137734=CARTESIAN_POINT('',(0.263991602958535,3.21181803679069,-4.00000000000001));
#137735=CARTESIAN_POINT('',(0.210362138786015,2.76249088224209,-4.00000000000001));
#137736=CARTESIAN_POINT('',(0.849040484398591,3.87734816150549,-4.00000000000001));
#137737=CARTESIAN_POINT('Ctrl Pts',(0.849040484398591,3.87734816150549,
-4.00000000000001));
#137738=CARTESIAN_POINT('Ctrl Pts',(0.71880375631047,3.79746641108109,-4.00000000000001));
#137739=CARTESIAN_POINT('Ctrl Pts',(0.603686786061961,3.70660417322209,
-3.99999999999999));
#137740=CARTESIAN_POINT('Ctrl Pts',(0.405887597345406,3.50187433061819,
-4.00000000000004));
#137741=CARTESIAN_POINT('Ctrl Pts',(0.295120488144862,3.35410179701789,
-3.99999999999996));
#137742=CARTESIAN_POINT('Ctrl Pts',(0.263991602958535,3.21181803679069,
-4.00000000000001));
#137743=CARTESIAN_POINT('',(1.00437441090659,3.82687710928989,-4.00000000000001));
#137744=CARTESIAN_POINT('Origin',(-8.88178376686733E-15,1.00000037997959,
-4.00000000000001));
#137745=CARTESIAN_POINT('',(1.08650010626791,2.94456882374649,-4.00000000000001));
#137746=CARTESIAN_POINT('Ctrl Pts',(1.08650010626791,2.94456882374649,-4.00000000000001));
#137747=CARTESIAN_POINT('Ctrl Pts',(1.11881406112232,3.01832453074849,-4.00000000000001));
#137748=CARTESIAN_POINT('Ctrl Pts',(1.14461503405761,3.20403080265529,-4.00000000000003));
#137749=CARTESIAN_POINT('Ctrl Pts',(1.11669065572569,3.49995129618689,-4.00000000000001));
#137750=CARTESIAN_POINT('Ctrl Pts',(1.05618025388954,3.70166331173879,-4.00000000000001));
#137751=CARTESIAN_POINT('Ctrl Pts',(1.00437441090659,3.82687710928989,-4.00000000000001));
#137752=CARTESIAN_POINT('',(0.914555682342743,2.63683051896609,-4.00000000000001));
#137753=CARTESIAN_POINT('',(0.865779379284463,2.54953291155349,-4.00000000000001));
#137754=CARTESIAN_POINT('',(1.27410472160532,2.37560285103839,-4.00000000000001));
#137755=CARTESIAN_POINT('Origin',(-8.88178376686733E-15,1.00000037997959,
-4.00000000000001));
#137756=CARTESIAN_POINT('',(1.5136474925994,2.63422808185029,-4.00000000000001));
#137757=CARTESIAN_POINT('',(1.20615246978637,2.30223738591519,-4.00000000000001));
#137758=CARTESIAN_POINT('',(2.3781507724882,2.82877015863239,-4.00000000000001));
#137759=CARTESIAN_POINT('Ctrl Pts',(2.3781507724882,2.82877015863239,-4.00000000000001));
#137760=CARTESIAN_POINT('Ctrl Pts',(2.22583373134628,2.84069569307559,-4.00000000000001));
#137761=CARTESIAN_POINT('Ctrl Pts',(2.07929453452094,2.83485055831319,-3.99999999999999));
#137762=CARTESIAN_POINT('Ctrl Pts',(1.7989342669203,2.78548400016299,-4.00000000000004));
#137763=CARTESIAN_POINT('Ctrl Pts',(1.62246358563372,2.73104096226529,-3.99999999999996));
#137764=CARTESIAN_POINT('Ctrl Pts',(1.5136474925994,2.63422808185029,-4.00000000000001));
#137765=CARTESIAN_POINT('',(2.47415241867612,2.69663522848389,-4.00000000000001));
#137766=CARTESIAN_POINT('Origin',(-8.88178376686733E-15,1.00000037997959,
-4.00000000000001));
#137767=CARTESIAN_POINT('',(2.02198570368039,1.93456055863369,-4.00000000000001));
#137768=CARTESIAN_POINT('Ctrl Pts',(2.02198570368039,1.93456055863369,-4.00000000000001));
#137769=CARTESIAN_POINT('Ctrl Pts',(2.09148075916129,1.97523651292379,-4.00000000000001));
#137770=CARTESIAN_POINT('Ctrl Pts',(2.22151143449857,2.11031491885179,-4.00000000000003));
#137771=CARTESIAN_POINT('Ctrl Pts',(2.37285866081655,2.36613447758449,-4.00000000000002));
#137772=CARTESIAN_POINT('Ctrl Pts',(2.44246540247316,2.56488442784669,-4.00000000000001));
#137773=CARTESIAN_POINT('Ctrl Pts',(2.47415241867613,2.69663522848389,-4.00000000000001));
#137774=CARTESIAN_POINT('',(1.70199570552156,1.78666143684349,-4.00000000000001));
#137775=CARTESIAN_POINT('',(1.61122260122708,1.74470618047739,-4.00000000000001));
#137776=CARTESIAN_POINT('',(1.83933121789749,1.36398619133449,-4.00000000000001));
#137777=CARTESIAN_POINT('Origin',(-8.88178376686733E-15,1.00000037997959,
-4.00000000000001));
#137778=CARTESIAN_POINT('',(2.18514148705334,1.43241869015189,-4.00000000000001));
#137779=CARTESIAN_POINT('',(1.74123355294296,1.34457361472889,-4.00000000000001));
#137780=CARTESIAN_POINT('',(2.99888829585914,1.08166425791249,-4.00000000000001));
#137781=CARTESIAN_POINT('Ctrl Pts',(2.99888829585914,1.08166425791249,-4.00000000000001));
#137782=CARTESIAN_POINT('Ctrl Pts',(2.88267087431383,1.18084192839999,-4.00000000000001));
#137783=CARTESIAN_POINT('Ctrl Pts',(2.76068287246971,1.26224670259339,-3.99999999999999));
#137784=CARTESIAN_POINT('Ctrl Pts',(2.50485018029661,1.38709985462769,-4.00000000000004));
#137785=CARTESIAN_POINT('Ctrl Pts',(2.33008073891961,1.44678146098259,-3.99999999999996));
#137786=CARTESIAN_POINT('Ctrl Pts',(2.18514148705334,1.43241869015189,-4.00000000000001));
#137787=CARTESIAN_POINT('',(2.99888829585913,0.91833650204669,-4.00000000000001));
#137788=CARTESIAN_POINT('Origin',(-8.88178376686733E-15,1.00000037997959,
-4.00000000000001));
#137789=CARTESIAN_POINT('',(2.18514148705334,0.567582069807293,-4.00000000000001));
#137790=CARTESIAN_POINT('Ctrl Pts',(2.18514148705334,0.567582069807293,
-4.00000000000001));
#137791=CARTESIAN_POINT('Ctrl Pts',(2.26527289401707,0.55964143937159,-4.00000000000001));
#137792=CARTESIAN_POINT('Ctrl Pts',(2.44985190263044,0.59248302306639,-4.00000000000002));
#137793=CARTESIAN_POINT('Ctrl Pts',(2.72265593195598,0.710483544687093,
-4.00000000000002));
#137794=CARTESIAN_POINT('Ctrl Pts',(2.89581178365771,0.830373026122091,
-4.00000000000001));
#137795=CARTESIAN_POINT('Ctrl Pts',(2.99888829585914,0.91833650204669,-4.00000000000001));
#137796=CARTESIAN_POINT('',(1.83933121789749,0.63601456862469,-4.00000000000001));
#137797=CARTESIAN_POINT('',(1.74123355294296,0.65542714523029,-4.00000000000001));
#137798=CARTESIAN_POINT('',(1.70199570552156,0.213339323115793,-4.00000000000001));
#137799=CARTESIAN_POINT('Origin',(-8.88178376686733E-15,1.00000037997959,
-4.00000000000001));
#137800=CARTESIAN_POINT('',(2.02198570368039,0.0654402013254929,-4.00000000000001));
#137801=CARTESIAN_POINT('',(1.61122260122708,0.255294579481791,-4.00000000000001));
#137802=CARTESIAN_POINT('',(2.47415241867613,-0.696634468524611,-4.00000000000001));
#137803=CARTESIAN_POINT('Ctrl Pts',(2.47415241867613,-0.696634468524611,
-4.00000000000001));
#137804=CARTESIAN_POINT('Ctrl Pts',(2.43842572167286,-0.548087161193807,
-4.00000000000001));
#137805=CARTESIAN_POINT('Ctrl Pts',(2.38758447134345,-0.410526973901209,
-3.99999999999999));
#137806=CARTESIAN_POINT('Ctrl Pts',(2.2539989302801,-0.159144637220008,
-4.00000000000004));
#137807=CARTESIAN_POINT('Ctrl Pts',(2.14768624646961,-0.0081332277100099,
-3.99999999999996));
#137808=CARTESIAN_POINT('Ctrl Pts',(2.0219857036804,0.0654402013254929,
-4.00000000000001));
#137809=CARTESIAN_POINT('',(2.3781507724882,-0.82876939867321,-4.00000000000001));
#137810=CARTESIAN_POINT('Origin',(-8.88178376686733E-15,1.00000037997959,
-4.00000000000001));
#137811=CARTESIAN_POINT('',(1.5136474925994,-0.634227321891108,-4.00000000000001));
#137812=CARTESIAN_POINT('Ctrl Pts',(1.5136474925994,-0.634227321891108,
-4.00000000000001));
#137813=CARTESIAN_POINT('Ctrl Pts',(1.57380777715217,-0.687751486118411,
-4.00000000000001));
#137814=CARTESIAN_POINT('Ctrl Pts',(1.74240355763935,-0.769671725923708,
-4.00000000000002));
#137815=CARTESIAN_POINT('Ctrl Pts',(2.03245399589892,-0.834554549185307,
-4.00000000000001));
#137816=CARTESIAN_POINT('Ctrl Pts',(2.24305648850748,-0.839346491850712,
-4.00000000000001));
#137817=CARTESIAN_POINT('Ctrl Pts',(2.3781507724882,-0.82876939867321,-4.00000000000001));
#137818=CARTESIAN_POINT('',(1.20615246978637,-0.302236625956009,-4.00000000000001));
#137819=CARTESIAN_POINT('',(-1.50000000000001,1.00000037997959,-4.00000000000001));
#137820=CARTESIAN_POINT('Origin',(-8.88178376686733E-15,1.00000037997959,
-4.00000000000001));
#137821=CARTESIAN_POINT('Origin',(1.20615246978637,-0.302236625956009,-4.00000000000001));
#137822=CARTESIAN_POINT('',(1.27410472160532,-0.375602091079212,-4.00000000000001));
#137823=CARTESIAN_POINT('',(1.5136474925994,-0.634227321891108,-4.00000000000001));
#137824=CARTESIAN_POINT('Ctrl Pts',(1.5136474925994,-0.634227321891108,
-4.00000000000001));
#137825=CARTESIAN_POINT('Ctrl Pts',(1.5136474925994,-0.634227321891108,
1.75999999999999));
#137826=CARTESIAN_POINT('Ctrl Pts',(1.57380777715217,-0.687751486118411,
-4.00000000000001));
#137827=CARTESIAN_POINT('Ctrl Pts',(1.57380777715217,-0.687751486118411,
1.75999999999999));
#137828=CARTESIAN_POINT('Ctrl Pts',(1.74240355763935,-0.769671725923708,
-4.00000000000002));
#137829=CARTESIAN_POINT('Ctrl Pts',(1.74240355763935,-0.769671725923708,
1.75999999999998));
#137830=CARTESIAN_POINT('Ctrl Pts',(2.03245399589892,-0.834554549185307,
-4.00000000000001));
#137831=CARTESIAN_POINT('Ctrl Pts',(2.03245399589892,-0.834554549185307,
1.75999999999999));
#137832=CARTESIAN_POINT('Ctrl Pts',(2.24305648850748,-0.839346491850712,
-4.00000000000001));
#137833=CARTESIAN_POINT('Ctrl Pts',(2.24305648850748,-0.839346491850712,
1.75999999999999));
#137834=CARTESIAN_POINT('Ctrl Pts',(2.3781507724882,-0.82876939867321,-4.00000000000001));
#137835=CARTESIAN_POINT('Ctrl Pts',(2.3781507724882,-0.82876939867321,1.75999999999999));
#137836=CARTESIAN_POINT('',(2.3781507724882,-0.82876939867321,-5.55111512312578E-15));
#137837=CARTESIAN_POINT('Origin',(-8.88178376686733E-15,1.00000037997959,
-4.00000000000001));
#137838=CARTESIAN_POINT('',(2.47415241867613,-0.696634468524611,-4.00000000000001));
#137839=CARTESIAN_POINT('Ctrl Pts',(2.47415241867613,-0.696634468524611,
-4.00000000000001));
#137840=CARTESIAN_POINT('Ctrl Pts',(2.47415241867613,-0.696634468524611,
1.76000000000005));
#137841=CARTESIAN_POINT('Ctrl Pts',(2.43842572167286,-0.548087161193807,
-4.00000000000001));
#137842=CARTESIAN_POINT('Ctrl Pts',(2.43842572167286,-0.548087161193807,
1.76000000000005));
#137843=CARTESIAN_POINT('Ctrl Pts',(2.38758447134345,-0.410526973901209,
-3.99999999999999));
#137844=CARTESIAN_POINT('Ctrl Pts',(2.38758447134345,-0.410526973901209,
1.76000000000007));
#137845=CARTESIAN_POINT('Ctrl Pts',(2.2539989302801,-0.159144637220008,
-4.00000000000004));
#137846=CARTESIAN_POINT('Ctrl Pts',(2.2539989302801,-0.159144637220008,
1.76000000000002));
#137847=CARTESIAN_POINT('Ctrl Pts',(2.14768624646961,-0.00813322771000991,
-3.99999999999996));
#137848=CARTESIAN_POINT('Ctrl Pts',(2.14768624646961,-0.00813322771000991,
1.7600000000001));
#137849=CARTESIAN_POINT('Ctrl Pts',(2.0219857036804,0.0654402013254929,
-4.00000000000001));
#137850=CARTESIAN_POINT('Ctrl Pts',(2.0219857036804,0.0654402013254929,
1.76000000000005));
#137851=CARTESIAN_POINT('',(2.02198570368039,0.0654402013254929,-4.00000000000001));
#137852=CARTESIAN_POINT('Origin',(2.02198570368039,0.0654402013254929,-4.00000000000001));
#137853=CARTESIAN_POINT('',(1.70199570552156,0.213339323115793,-4.00000000000001));
#137854=CARTESIAN_POINT('Origin',(-8.88178376686733E-15,1.00000037997959,
-4.00000000000001));
#137855=CARTESIAN_POINT('',(0.914555682342743,-0.636829759006909,-4.00000000000001));
#137856=CARTESIAN_POINT('Origin',(-8.88178376686733E-15,1.00000037997959,
-4.00000000000001));
#137857=CARTESIAN_POINT('',(1.83933121789749,0.63601456862469,-4.00000000000001));
#137858=CARTESIAN_POINT('Origin',(0.210362138786014,-0.762490122282808,
-4.00000000000001));
#137859=CARTESIAN_POINT('',(0.222213526886635,-0.861785361846907,-4.00000000000001));
#137860=CARTESIAN_POINT('',(0.263991602958534,-1.21181727683151,-4.00000000000001));
#137861=CARTESIAN_POINT('Ctrl Pts',(0.263991602958534,-1.21181727683151,
-4.00000000000001));
#137862=CARTESIAN_POINT('Ctrl Pts',(0.263991602958534,-1.21181727683151,
1.75999999999999));
#137863=CARTESIAN_POINT('Ctrl Pts',(0.281201581174052,-1.29048056333501,
-4.00000000000001));
#137864=CARTESIAN_POINT('Ctrl Pts',(0.281201581174052,-1.29048056333501,
1.75999999999999));
#137865=CARTESIAN_POINT('Ctrl Pts',(0.369415546990755,-1.45582621508241,
-4.00000000000003));
#137866=CARTESIAN_POINT('Ctrl Pts',(0.369415546990755,-1.45582621508241,
1.75999999999997));
#137867=CARTESIAN_POINT('Ctrl Pts',(0.565925030419526,-1.67879393332191,
-4.00000000000001));
#137868=CARTESIAN_POINT('Ctrl Pts',(0.565925030419526,-1.67879393332191,
1.75999999999999));
#137869=CARTESIAN_POINT('Ctrl Pts',(0.733529853433378,-1.80649802188531,
-4.00000000000001));
#137870=CARTESIAN_POINT('Ctrl Pts',(0.733529853433378,-1.80649802188531,
1.75999999999999));
#137871=CARTESIAN_POINT('Ctrl Pts',(0.849040484398591,-1.87734740154631,
-4.00000000000001));
#137872=CARTESIAN_POINT('Ctrl Pts',(0.849040484398591,-1.87734740154631,
1.75999999999999));
#137873=CARTESIAN_POINT('',(0.849040484398591,-1.87734740154631,-6.66133814775094E-15));
#137874=CARTESIAN_POINT('Origin',(-8.88178376686733E-15,1.00000037997959,
-4.00000000000001));
#137875=CARTESIAN_POINT('',(1.00437441090659,-1.82687634933071,-4.00000000000001));
#137876=CARTESIAN_POINT('Ctrl Pts',(1.00437441090659,-1.82687634933071,
-4.00000000000001));
#137877=CARTESIAN_POINT('Ctrl Pts',(1.00437441090659,-1.82687634933071,
1.76000000000005));
#137878=CARTESIAN_POINT('Ctrl Pts',(1.06278482239484,-1.68569942761981,
-4.00000000000001));
#137879=CARTESIAN_POINT('Ctrl Pts',(1.06278482239484,-1.68569942761981,
1.76000000000005));
#137880=CARTESIAN_POINT('Ctrl Pts',(1.10250949831874,-1.54452789700551,
-3.99999999999999));
#137881=CARTESIAN_POINT('Ctrl Pts',(1.10250949831874,-1.54452789700551,
1.76000000000007));
#137882=CARTESIAN_POINT('Ctrl Pts',(1.14219547135593,-1.26263671791611,
-4.00000000000004));
#137883=CARTESIAN_POINT('Ctrl Pts',(1.14219547135593,-1.26263671791611,
1.76000000000002));
#137884=CARTESIAN_POINT('Ctrl Pts',(1.14494860503891,-1.07797514346901,
-3.99999999999996));
#137885=CARTESIAN_POINT('Ctrl Pts',(1.14494860503891,-1.07797514346901,
1.7600000000001));
#137886=CARTESIAN_POINT('Ctrl Pts',(1.08650010626791,-0.944568063787212,
-4.00000000000001));
#137887=CARTESIAN_POINT('Ctrl Pts',(1.08650010626791,-0.944568063787212,
1.76000000000005));
#137888=CARTESIAN_POINT('',(1.0865001062679,-0.944568063787212,-4.00000000000001));
#137889=CARTESIAN_POINT('Origin',(1.0865001062679,-0.944568063787212,-4.00000000000001));
#137890=CARTESIAN_POINT('Origin',(-8.88178376686733E-15,1.00000037997959,
-4.00000000000001));
#137891=CARTESIAN_POINT('',(-0.222213526886654,-0.861785361846907,-4.00000000000001));
#137892=CARTESIAN_POINT('Origin',(-0.865779379284481,-0.54953215159431,
-4.00000000000001));
#137893=CARTESIAN_POINT('',(-0.914555682342761,-0.636829759006909,-4.00000000000001));
#137894=CARTESIAN_POINT('',(-1.08650010626793,-0.944568063787212,-4.00000000000001));
#137895=CARTESIAN_POINT('Ctrl Pts',(-1.08650010626793,-0.944568063787212,
-4.00000000000001));
#137896=CARTESIAN_POINT('Ctrl Pts',(-1.08650010626793,-0.944568063787212,
1.75999999999999));
#137897=CARTESIAN_POINT('Ctrl Pts',(-1.11881406112234,-1.01832377078921,
-4.00000000000001));
#137898=CARTESIAN_POINT('Ctrl Pts',(-1.11881406112234,-1.01832377078921,
1.75999999999999));
#137899=CARTESIAN_POINT('Ctrl Pts',(-1.14463100585987,-1.20396029950631,
-4.00000000000003));
#137900=CARTESIAN_POINT('Ctrl Pts',(-1.14463100585987,-1.20396029950631,
1.75999999999997));
#137901=CARTESIAN_POINT('Ctrl Pts',(-1.11670822644255,-1.49985676817681,
-4.00000000000002));
#137902=CARTESIAN_POINT('Ctrl Pts',(-1.11670822644255,-1.49985676817681,
1.75999999999998));
#137903=CARTESIAN_POINT('Ctrl Pts',(-1.05618025388956,-1.70166255177951,
-4.00000000000001));
#137904=CARTESIAN_POINT('Ctrl Pts',(-1.05618025388956,-1.70166255177951,
1.75999999999999));
#137905=CARTESIAN_POINT('Ctrl Pts',(-1.00437441090661,-1.82687634933071,
-4.00000000000001));
#137906=CARTESIAN_POINT('Ctrl Pts',(-1.00437441090661,-1.82687634933071,
1.75999999999999));
#137907=CARTESIAN_POINT('',(-1.00437441090661,-1.82687634933071,-6.66133814775094E-15));
#137908=CARTESIAN_POINT('Origin',(-8.88178376686733E-15,1.00000037997959,
-4.00000000000001));
#137909=CARTESIAN_POINT('',(-0.84904048439861,-1.87734740154631,-4.00000000000001));
#137910=CARTESIAN_POINT('Ctrl Pts',(-0.84904048439861,-1.87734740154631,
-4.00000000000001));
#137911=CARTESIAN_POINT('Ctrl Pts',(-0.849040484398609,-1.87734740154631,
1.76000000000005));
#137912=CARTESIAN_POINT('Ctrl Pts',(-0.718803756310479,-1.79746565112191,
-4.00000000000001));
#137913=CARTESIAN_POINT('Ctrl Pts',(-0.718803756310478,-1.79746565112191,
1.76000000000005));
#137914=CARTESIAN_POINT('Ctrl Pts',(-0.603687404582929,-1.70660550831901,
-3.99999999999999));
#137915=CARTESIAN_POINT('Ctrl Pts',(-0.603687404582928,-1.70660550831901,
1.76000000000007));
#137916=CARTESIAN_POINT('Ctrl Pts',(-0.405889607552644,-1.50187812695961,
-4.00000000000004));
#137917=CARTESIAN_POINT('Ctrl Pts',(-0.405889607552643,-1.50187812695961,
1.76000000000002));
#137918=CARTESIAN_POINT('Ctrl Pts',(-0.295120488144883,-1.35410103706051,
-3.99999999999996));
#137919=CARTESIAN_POINT('Ctrl Pts',(-0.295120488144882,-1.35410103706051,
1.7600000000001));
#137920=CARTESIAN_POINT('Ctrl Pts',(-0.263991602958553,-1.21181727683151,
-4.00000000000001));
#137921=CARTESIAN_POINT('Ctrl Pts',(-0.263991602958552,-1.21181727683151,
1.76000000000005));
#137922=CARTESIAN_POINT('',(-0.263991602958553,-1.21181727683151,-4.00000000000001));
#137923=CARTESIAN_POINT('Origin',(-0.263991602958553,-1.21181727683151,
-4.00000000000001));
#137924=CARTESIAN_POINT('Origin',(-8.88178376686733E-15,1.00000037997959,
-4.00000000000001));
#137925=CARTESIAN_POINT('',(-1.27410472160534,-0.375602091079212,-4.00000000000001));
#137926=CARTESIAN_POINT('Origin',(-1.6112226012271,0.255294579481791,-4.00000000000001));
#137927=CARTESIAN_POINT('',(-1.70199570552158,0.213339323115793,-4.00000000000001));
#137928=CARTESIAN_POINT('',(-2.02198570368041,0.0654402013254929,-4.00000000000001));
#137929=CARTESIAN_POINT('Ctrl Pts',(-2.02198570368041,0.0654402013254929,
-4.00000000000001));
#137930=CARTESIAN_POINT('Ctrl Pts',(-2.02198570368041,0.0654402013254929,
1.75999999999999));
#137931=CARTESIAN_POINT('Ctrl Pts',(-2.09148075916131,0.0247642470353915,
-4.00000000000001));
#137932=CARTESIAN_POINT('Ctrl Pts',(-2.09148075916131,0.0247642470353915,
1.75999999999999));
#137933=CARTESIAN_POINT('Ctrl Pts',(-2.22149393751475,-0.110273189124808,
-4.00000000000003));
#137934=CARTESIAN_POINT('Ctrl Pts',(-2.22149393751475,-0.110273189124808,
1.75999999999997));
#137935=CARTESIAN_POINT('Ctrl Pts',(-2.37283326403248,-0.366080159665607,
-4.00000000000001));
#137936=CARTESIAN_POINT('Ctrl Pts',(-2.37283326403248,-0.366080159665607,
1.75999999999999));
#137937=CARTESIAN_POINT('Ctrl Pts',(-2.44246540247318,-0.564883667887508,
-4.00000000000001));
#137938=CARTESIAN_POINT('Ctrl Pts',(-2.44246540247318,-0.564883667887508,
1.75999999999999));
#137939=CARTESIAN_POINT('Ctrl Pts',(-2.47415241867615,-0.696634468524611,
-4.00000000000001));
#137940=CARTESIAN_POINT('Ctrl Pts',(-2.47415241867615,-0.696634468524611,
1.75999999999999));
#137941=CARTESIAN_POINT('',(-2.47415241867615,-0.696634468524611,-5.55111512312578E-15));
#137942=CARTESIAN_POINT('Origin',(-8.88178376686733E-15,1.00000037997959,
-4.00000000000001));
#137943=CARTESIAN_POINT('',(-2.37815077248822,-0.82876939867321,-4.00000000000001));
#137944=CARTESIAN_POINT('Ctrl Pts',(-2.37815077248822,-0.82876939867321,
-4.00000000000001));
#137945=CARTESIAN_POINT('Ctrl Pts',(-2.37815077248822,-0.82876939867321,
1.76000000000005));
#137946=CARTESIAN_POINT('Ctrl Pts',(-2.2258337313463,-0.84069493311631,
-4.00000000000001));
#137947=CARTESIAN_POINT('Ctrl Pts',(-2.2258337313463,-0.84069493311631,
1.76000000000005));
#137948=CARTESIAN_POINT('Ctrl Pts',(-2.07929557892755,-0.834850597287109,
-3.99999999999999));
#137949=CARTESIAN_POINT('Ctrl Pts',(-2.07929557892755,-0.834850597287109,
1.76000000000007));
#137950=CARTESIAN_POINT('Ctrl Pts',(-1.79893681959492,-0.785484727221708,
-4.00000000000004));
#137951=CARTESIAN_POINT('Ctrl Pts',(-1.79893681959492,-0.785484727221708,
1.76000000000002));
#137952=CARTESIAN_POINT('Ctrl Pts',(-1.62246358563374,-0.731040202306308,
-3.99999999999996));
#137953=CARTESIAN_POINT('Ctrl Pts',(-1.62246358563374,-0.731040202306308,
1.7600000000001));
#137954=CARTESIAN_POINT('Ctrl Pts',(-1.51364749259942,-0.634227321891108,
-4.00000000000001));
#137955=CARTESIAN_POINT('Ctrl Pts',(-1.51364749259942,-0.634227321891108,
1.76000000000005));
#137956=CARTESIAN_POINT('',(-1.51364749259942,-0.634227321891108,-4.00000000000001));
#137957=CARTESIAN_POINT('Origin',(-1.51364749259942,-0.634227321891108,
-4.00000000000001));
#137958=CARTESIAN_POINT('Origin',(-8.88178376686733E-15,1.00000037997959,
-4.00000000000001));
#137959=CARTESIAN_POINT('',(-1.83933121789751,0.63601456862469,-4.00000000000001));
#137960=CARTESIAN_POINT('Origin',(-1.74123355294298,1.34457361472889,-4.00000000000001));
#137961=CARTESIAN_POINT('',(-1.83933121789751,1.36398619133449,-4.00000000000001));
#137962=CARTESIAN_POINT('',(-2.18514148705336,1.43241869015189,-4.00000000000001));
#137963=CARTESIAN_POINT('Ctrl Pts',(-2.18514148705336,1.43241869015189,
-4.00000000000001));
#137964=CARTESIAN_POINT('Ctrl Pts',(-2.18514148705336,1.43241869015189,
1.75999999999999));
#137965=CARTESIAN_POINT('Ctrl Pts',(-2.26527289401709,1.44035932058759,
-4.00000000000001));
#137966=CARTESIAN_POINT('Ctrl Pts',(-2.26527289401709,1.44035932058759,
1.75999999999999));
#137967=CARTESIAN_POINT('Ctrl Pts',(-2.4498539131878,1.40751653520809,-4.00000000000003));
#137968=CARTESIAN_POINT('Ctrl Pts',(-2.4498539131878,1.40751653520809,1.75999999999997));
#137969=CARTESIAN_POINT('Ctrl Pts',(-2.72265866540928,1.28951572275389,
-4.00000000000001));
#137970=CARTESIAN_POINT('Ctrl Pts',(-2.72265866540928,1.28951572275389,
1.75999999999999));
#137971=CARTESIAN_POINT('Ctrl Pts',(-2.89581178365773,1.16962773383709,
-4.00000000000001));
#137972=CARTESIAN_POINT('Ctrl Pts',(-2.89581178365773,1.16962773383709,
1.75999999999999));
#137973=CARTESIAN_POINT('Ctrl Pts',(-2.99888829585916,1.08166425791249,
-4.00000000000001));
#137974=CARTESIAN_POINT('Ctrl Pts',(-2.99888829585916,1.08166425791249,
1.75999999999999));
#137975=CARTESIAN_POINT('',(-2.99888829585915,1.08166425791249,-6.66133814775094E-15));
#137976=CARTESIAN_POINT('Origin',(-8.88178376686733E-15,1.00000037997959,
-4.00000000000001));
#137977=CARTESIAN_POINT('',(-2.99888829585916,0.91833650204669,-4.00000000000001));
#137978=CARTESIAN_POINT('Ctrl Pts',(-2.99888829585916,0.91833650204669,
-4.00000000000001));
#137979=CARTESIAN_POINT('Ctrl Pts',(-2.99888829585916,0.91833650204669,
1.76000000000005));
#137980=CARTESIAN_POINT('Ctrl Pts',(-2.88267087431385,0.81915883155919,
-4.00000000000001));
#137981=CARTESIAN_POINT('Ctrl Pts',(-2.88267087431385,0.81915883155919,
1.76000000000005));
#137982=CARTESIAN_POINT('Ctrl Pts',(-2.76068292952053,0.737754056010891,
-3.99999999999999));
#137983=CARTESIAN_POINT('Ctrl Pts',(-2.76068292952053,0.737754056010891,
1.76000000000007));
#137984=CARTESIAN_POINT('Ctrl Pts',(-2.50485030710536,0.61290091813639,
-4.00000000000004));
#137985=CARTESIAN_POINT('Ctrl Pts',(-2.50485030710536,0.61290091813639,
1.76000000000002));
#137986=CARTESIAN_POINT('Ctrl Pts',(-2.33008073891963,0.553219298973793,
-3.99999999999996));
#137987=CARTESIAN_POINT('Ctrl Pts',(-2.33008073891963,0.553219298973793,
1.7600000000001));
#137988=CARTESIAN_POINT('Ctrl Pts',(-2.18514148705336,0.567582069807391,
-4.00000000000001));
#137989=CARTESIAN_POINT('Ctrl Pts',(-2.18514148705336,0.567582069807391,
1.76000000000005));
#137990=CARTESIAN_POINT('',(-2.18514148705336,0.567582069807293,-4.00000000000001));
#137991=CARTESIAN_POINT('Origin',(-2.18514148705336,0.567582069807293,-4.00000000000001));
#137992=CARTESIAN_POINT('Origin',(-8.88178376686733E-15,1.00000037997959,
-4.00000000000001));
#137993=CARTESIAN_POINT('',(-1.70199570552158,1.78666143684349,-4.00000000000001));
#137994=CARTESIAN_POINT('Origin',(-1.20615246978639,2.30223738591519,-4.00000000000001));
#137995=CARTESIAN_POINT('',(-1.27410472160534,2.37560285103839,-4.00000000000001));
#137996=CARTESIAN_POINT('',(-1.51364749259942,2.63422808185029,-4.00000000000001));
#137997=CARTESIAN_POINT('Ctrl Pts',(-1.51364749259942,2.63422808185029,
-4.00000000000001));
#137998=CARTESIAN_POINT('Ctrl Pts',(-1.51364749259942,2.63422808185029,
1.75999999999999));
#137999=CARTESIAN_POINT('Ctrl Pts',(-1.57380777715219,2.68775224607759,
-4.00000000000001));
#138000=CARTESIAN_POINT('Ctrl Pts',(-1.57380777715219,2.68775224607759,
1.75999999999999));
#138001=CARTESIAN_POINT('Ctrl Pts',(-1.74245715676096,2.76967728864719,
-4.00000000000003));
#138002=CARTESIAN_POINT('Ctrl Pts',(-1.74245715676096,2.76967728864719,
1.75999999999997));
#138003=CARTESIAN_POINT('Ctrl Pts',(-2.03252503861004,2.83456450287859,
-4.00000000000002));
#138004=CARTESIAN_POINT('Ctrl Pts',(-2.03252503861004,2.83456450287859,
1.75999999999998));
#138005=CARTESIAN_POINT('Ctrl Pts',(-2.2430564885075,2.83934725180989,-4.00000000000001));
#138006=CARTESIAN_POINT('Ctrl Pts',(-2.2430564885075,2.83934725180989,1.75999999999999));
#138007=CARTESIAN_POINT('Ctrl Pts',(-2.37815077248822,2.82877015863239,
-4.00000000000001));
#138008=CARTESIAN_POINT('Ctrl Pts',(-2.37815077248822,2.82877015863239,
1.75999999999999));
#138009=CARTESIAN_POINT('',(-2.37815077248822,2.82877015863239,-6.66133814775094E-15));
#138010=CARTESIAN_POINT('Origin',(-8.88178376686733E-15,1.00000037997959,
-4.00000000000001));
#138011=CARTESIAN_POINT('',(-2.47415241867615,2.69663522848389,-4.00000000000001));
#138012=CARTESIAN_POINT('Ctrl Pts',(-2.47415241867615,2.69663522848389,
-4.00000000000001));
#138013=CARTESIAN_POINT('Ctrl Pts',(-2.47415241867615,2.69663522848389,
1.76000000000005));
#138014=CARTESIAN_POINT('Ctrl Pts',(-2.43842572167288,2.54808792115299,
-4.00000000000001));
#138015=CARTESIAN_POINT('Ctrl Pts',(-2.43842572167288,2.54808792115299,
1.76000000000005));
#138016=CARTESIAN_POINT('Ctrl Pts',(-2.38758357586867,2.41052711593049,
-3.99999999999999));
#138017=CARTESIAN_POINT('Ctrl Pts',(-2.38758357586867,2.41052711593049,
1.76000000000007));
#138018=CARTESIAN_POINT('Ctrl Pts',(-2.25399711176357,2.15914377278389,
-4.00000000000004));
#138019=CARTESIAN_POINT('Ctrl Pts',(-2.25399711176357,2.15914377278389,
1.76000000000002));
#138020=CARTESIAN_POINT('Ctrl Pts',(-2.14768624646963,2.00813398766899,
-3.99999999999996));
#138021=CARTESIAN_POINT('Ctrl Pts',(-2.14768624646963,2.00813398766899,
1.7600000000001));
#138022=CARTESIAN_POINT('Ctrl Pts',(-2.02198570368042,1.93456055863379,
-4.00000000000001));
#138023=CARTESIAN_POINT('Ctrl Pts',(-2.02198570368042,1.93456055863379,
1.76000000000005));
#138024=CARTESIAN_POINT('',(-2.02198570368041,1.93456055863369,-4.00000000000001));
#138025=CARTESIAN_POINT('Origin',(-2.02198570368041,1.93456055863369,-4.00000000000001));
#138026=CARTESIAN_POINT('Origin',(-8.88178376686733E-15,1.00000037997959,
-4.00000000000001));
#138027=CARTESIAN_POINT('',(-0.914555682342761,2.63683051896609,-4.00000000000001));
#138028=CARTESIAN_POINT('Origin',(-0.210362138786032,2.76249088224209,-4.00000000000001));
#138029=CARTESIAN_POINT('',(-0.222213526886654,2.86178612180609,-4.00000000000001));
#138030=CARTESIAN_POINT('',(-0.263991602958553,3.21181803679069,-4.00000000000001));
#138031=CARTESIAN_POINT('Ctrl Pts',(-0.263991602958553,3.21181803679069,
-4.00000000000001));
#138032=CARTESIAN_POINT('Ctrl Pts',(-0.263991602958553,3.21181803679069,
1.75999999999999));
#138033=CARTESIAN_POINT('Ctrl Pts',(-0.28120158117407,3.29048132329419,
-4.00000000000001));
#138034=CARTESIAN_POINT('Ctrl Pts',(-0.28120158117407,3.29048132329419,
1.75999999999999));
#138035=CARTESIAN_POINT('Ctrl Pts',(-0.369482464710247,3.45588532446969,
-4.00000000000003));
#138036=CARTESIAN_POINT('Ctrl Pts',(-0.369482464710247,3.45588532446969,
1.75999999999997));
#138037=CARTESIAN_POINT('Ctrl Pts',(-0.566011153087274,3.67887612480449,
-4.00000000000002));
#138038=CARTESIAN_POINT('Ctrl Pts',(-0.566011153087274,3.67887612480449,
1.75999999999998));
#138039=CARTESIAN_POINT('Ctrl Pts',(-0.733529853433388,3.80649878184449,
-4.00000000000001));
#138040=CARTESIAN_POINT('Ctrl Pts',(-0.733529853433388,3.80649878184449,
1.75999999999999));
#138041=CARTESIAN_POINT('Ctrl Pts',(-0.849040484398609,3.87734816150549,
-4.00000000000001));
#138042=CARTESIAN_POINT('Ctrl Pts',(-0.849040484398609,3.87734816150549,
1.75999999999999));
#138043=CARTESIAN_POINT('',(-0.849040484398609,3.87734816150549,-6.66133814775094E-15));
#138044=CARTESIAN_POINT('Origin',(-8.88178376686733E-15,1.00000037997959,
-4.00000000000001));
#138045=CARTESIAN_POINT('',(-1.00437441090661,3.82687710928989,-4.00000000000001));
#138046=CARTESIAN_POINT('Ctrl Pts',(-1.00437441090661,3.82687710928989,
-4.00000000000001));
#138047=CARTESIAN_POINT('Ctrl Pts',(-1.00437441090661,3.82687710928989,
1.76000000000005));
#138048=CARTESIAN_POINT('Ctrl Pts',(-1.06278482239486,3.68570018757899,
-4.00000000000001));
#138049=CARTESIAN_POINT('Ctrl Pts',(-1.06278482239486,3.68570018757899,
1.76000000000005));
#138050=CARTESIAN_POINT('Ctrl Pts',(-1.1025089125507,3.54452700216369,-3.99999999999999));
#138051=CARTESIAN_POINT('Ctrl Pts',(-1.1025089125507,3.54452700216369,1.76000000000007));
#138052=CARTESIAN_POINT('Ctrl Pts',(-1.14219463053897,3.26263359077969,
-4.00000000000004));
#138053=CARTESIAN_POINT('Ctrl Pts',(-1.14219463053897,3.26263359077969,
1.76000000000002));
#138054=CARTESIAN_POINT('Ctrl Pts',(-1.14494860503893,3.07797590342699,
-3.99999999999996));
#138055=CARTESIAN_POINT('Ctrl Pts',(-1.14494860503893,3.07797590342699,
1.7600000000001));
#138056=CARTESIAN_POINT('Ctrl Pts',(-1.08650010626793,2.94456882374649,
-4.00000000000001));
#138057=CARTESIAN_POINT('Ctrl Pts',(-1.08650010626793,2.94456882374649,
1.76000000000005));
#138058=CARTESIAN_POINT('',(-1.08650010626792,2.94456882374639,-4.00000000000001));
#138059=CARTESIAN_POINT('Origin',(-1.08650010626793,2.94456882374649,-4.00000000000001));
#138060=CARTESIAN_POINT('Origin',(-8.88178376686733E-15,1.00000037997959,
-4.00000000000001));
#138061=CARTESIAN_POINT('',(0.222213526886636,2.86178612180609,-4.00000000000001));
#138062=CARTESIAN_POINT('Origin',(0.865779379284463,2.54953291155349,-4.00000000000001));
#138063=CARTESIAN_POINT('',(0.914555682342743,2.63683051896609,-4.00000000000001));
#138064=CARTESIAN_POINT('',(1.08650010626791,2.94456882374639,-4.00000000000001));
#138065=CARTESIAN_POINT('Ctrl Pts',(1.08650010626791,2.94456882374649,-4.00000000000001));
#138066=CARTESIAN_POINT('Ctrl Pts',(1.08650010626791,2.94456882374649,1.75999999999999));
#138067=CARTESIAN_POINT('Ctrl Pts',(1.11881406112232,3.01832453074849,-4.00000000000001));
#138068=CARTESIAN_POINT('Ctrl Pts',(1.11881406112232,3.01832453074849,1.75999999999999));
#138069=CARTESIAN_POINT('Ctrl Pts',(1.14461503405761,3.20403080265529,-4.00000000000003));
#138070=CARTESIAN_POINT('Ctrl Pts',(1.14461503405761,3.20403080265529,1.75999999999997));
#138071=CARTESIAN_POINT('Ctrl Pts',(1.11669065572569,3.49995129618689,-4.00000000000001));
#138072=CARTESIAN_POINT('Ctrl Pts',(1.11669065572569,3.49995129618689,1.75999999999999));
#138073=CARTESIAN_POINT('Ctrl Pts',(1.05618025388954,3.70166331173879,-4.00000000000001));
#138074=CARTESIAN_POINT('Ctrl Pts',(1.05618025388954,3.70166331173879,1.75999999999999));
#138075=CARTESIAN_POINT('Ctrl Pts',(1.00437441090659,3.82687710928989,-4.00000000000001));
#138076=CARTESIAN_POINT('Ctrl Pts',(1.00437441090659,3.82687710928989,1.75999999999999));
#138077=CARTESIAN_POINT('',(1.00437441090659,3.82687710928989,-5.55111512312578E-15));
#138078=CARTESIAN_POINT('Origin',(-8.88178376686733E-15,1.00000037997959,
-4.00000000000001));
#138079=CARTESIAN_POINT('',(0.849040484398591,3.87734816150549,-4.00000000000001));
#138080=CARTESIAN_POINT('Ctrl Pts',(0.849040484398591,3.87734816150549,
-4.00000000000001));
#138081=CARTESIAN_POINT('Ctrl Pts',(0.849040484398591,3.87734816150549,
1.76000000000005));
#138082=CARTESIAN_POINT('Ctrl Pts',(0.71880375631047,3.79746641108109,-4.00000000000001));
#138083=CARTESIAN_POINT('Ctrl Pts',(0.71880375631047,3.79746641108109,1.76000000000005));
#138084=CARTESIAN_POINT('Ctrl Pts',(0.603686786061961,3.70660417322209,
-3.99999999999999));
#138085=CARTESIAN_POINT('Ctrl Pts',(0.603686786061961,3.70660417322209,
1.76000000000007));
#138086=CARTESIAN_POINT('Ctrl Pts',(0.405887597345406,3.50187433061819,
-4.00000000000004));
#138087=CARTESIAN_POINT('Ctrl Pts',(0.405887597345406,3.50187433061819,
1.76000000000002));
#138088=CARTESIAN_POINT('Ctrl Pts',(0.295120488144862,3.35410179701789,
-3.99999999999996));
#138089=CARTESIAN_POINT('Ctrl Pts',(0.295120488144862,3.35410179701789,
1.7600000000001));
#138090=CARTESIAN_POINT('Ctrl Pts',(0.263991602958535,3.21181803679069,
-4.00000000000001));
#138091=CARTESIAN_POINT('Ctrl Pts',(0.263991602958535,3.21181803679069,
1.76000000000005));
#138092=CARTESIAN_POINT('',(0.263991602958535,3.21181803679069,-4.00000000000001));
#138093=CARTESIAN_POINT('Origin',(0.263991602958535,3.21181803679069,-4.00000000000001));
#138094=CARTESIAN_POINT('Origin',(-8.88178376686733E-15,1.00000037997959,
-4.00000000000001));
#138095=CARTESIAN_POINT('',(1.27410472160532,2.37560285103839,-4.00000000000001));
#138096=CARTESIAN_POINT('Origin',(1.61122260122708,1.74470618047739,-4.00000000000001));
#138097=CARTESIAN_POINT('',(1.70199570552156,1.78666143684349,-4.00000000000001));
#138098=CARTESIAN_POINT('',(2.02198570368039,1.93456055863369,-4.00000000000001));
#138099=CARTESIAN_POINT('Ctrl Pts',(2.02198570368039,1.93456055863369,-4.00000000000001));
#138100=CARTESIAN_POINT('Ctrl Pts',(2.02198570368039,1.93456055863369,1.75999999999999));
#138101=CARTESIAN_POINT('Ctrl Pts',(2.09148075916129,1.97523651292379,-4.00000000000001));
#138102=CARTESIAN_POINT('Ctrl Pts',(2.09148075916129,1.97523651292379,1.75999999999999));
#138103=CARTESIAN_POINT('Ctrl Pts',(2.22151143449857,2.11031491885179,-4.00000000000003));
#138104=CARTESIAN_POINT('Ctrl Pts',(2.22151143449857,2.11031491885179,1.75999999999997));
#138105=CARTESIAN_POINT('Ctrl Pts',(2.37285866081655,2.36613447758449,-4.00000000000002));
#138106=CARTESIAN_POINT('Ctrl Pts',(2.37285866081655,2.36613447758449,1.75999999999998));
#138107=CARTESIAN_POINT('Ctrl Pts',(2.44246540247316,2.56488442784669,-4.00000000000001));
#138108=CARTESIAN_POINT('Ctrl Pts',(2.44246540247316,2.56488442784669,1.75999999999999));
#138109=CARTESIAN_POINT('Ctrl Pts',(2.47415241867613,2.69663522848389,-4.00000000000001));
#138110=CARTESIAN_POINT('Ctrl Pts',(2.47415241867613,2.69663522848389,1.75999999999999));
#138111=CARTESIAN_POINT('',(2.47415241867612,2.69663522848389,-6.66133814775094E-15));
#138112=CARTESIAN_POINT('Origin',(-8.88178376686733E-15,1.00000037997959,
-4.00000000000001));
#138113=CARTESIAN_POINT('',(2.3781507724882,2.82877015863239,-4.00000000000001));
#138114=CARTESIAN_POINT('Ctrl Pts',(2.3781507724882,2.82877015863239,-4.00000000000001));
#138115=CARTESIAN_POINT('Ctrl Pts',(2.3781507724882,2.82877015863239,1.76000000000005));
#138116=CARTESIAN_POINT('Ctrl Pts',(2.22583373134628,2.84069569307559,-4.00000000000001));
#138117=CARTESIAN_POINT('Ctrl Pts',(2.22583373134628,2.84069569307559,1.76000000000005));
#138118=CARTESIAN_POINT('Ctrl Pts',(2.07929453452094,2.83485055831319,-3.99999999999999));
#138119=CARTESIAN_POINT('Ctrl Pts',(2.07929453452094,2.83485055831319,1.76000000000007));
#138120=CARTESIAN_POINT('Ctrl Pts',(1.7989342669203,2.78548400016299,-4.00000000000004));
#138121=CARTESIAN_POINT('Ctrl Pts',(1.7989342669203,2.78548400016299,1.76000000000002));
#138122=CARTESIAN_POINT('Ctrl Pts',(1.62246358563372,2.73104096226529,-3.99999999999996));
#138123=CARTESIAN_POINT('Ctrl Pts',(1.62246358563372,2.73104096226529,1.7600000000001));
#138124=CARTESIAN_POINT('Ctrl Pts',(1.5136474925994,2.63422808185029,-4.00000000000001));
#138125=CARTESIAN_POINT('Ctrl Pts',(1.5136474925994,2.63422808185029,1.76000000000005));
#138126=CARTESIAN_POINT('',(1.5136474925994,2.63422808185029,-4.00000000000001));
#138127=CARTESIAN_POINT('Origin',(1.5136474925994,2.63422808185029,-4.00000000000001));
#138128=CARTESIAN_POINT('Origin',(-8.88178376686733E-15,1.00000037997959,
-4.00000000000001));
#138129=CARTESIAN_POINT('',(1.83933121789749,1.36398619133449,-4.00000000000001));
#138130=CARTESIAN_POINT('Origin',(1.74123355294296,0.65542714523029,-4.00000000000001));
#138131=CARTESIAN_POINT('',(2.18514148705334,0.567582069807293,-4.00000000000001));
#138132=CARTESIAN_POINT('Ctrl Pts',(2.18514148705334,0.567582069807293,
-4.00000000000001));
#138133=CARTESIAN_POINT('Ctrl Pts',(2.18514148705334,0.567582069807293,
1.75999999999999));
#138134=CARTESIAN_POINT('Ctrl Pts',(2.26527289401707,0.55964143937159,-4.00000000000001));
#138135=CARTESIAN_POINT('Ctrl Pts',(2.26527289401707,0.55964143937159,1.75999999999999));
#138136=CARTESIAN_POINT('Ctrl Pts',(2.44985190263044,0.59248302306639,-4.00000000000002));
#138137=CARTESIAN_POINT('Ctrl Pts',(2.44985190263044,0.59248302306639,1.75999999999998));
#138138=CARTESIAN_POINT('Ctrl Pts',(2.72265593195598,0.710483544687093,
-4.00000000000002));
#138139=CARTESIAN_POINT('Ctrl Pts',(2.72265593195598,0.710483544687093,
1.75999999999998));
#138140=CARTESIAN_POINT('Ctrl Pts',(2.89581178365771,0.830373026122091,
-4.00000000000001));
#138141=CARTESIAN_POINT('Ctrl Pts',(2.89581178365771,0.830373026122091,
1.75999999999999));
#138142=CARTESIAN_POINT('Ctrl Pts',(2.99888829585914,0.91833650204669,-4.00000000000001));
#138143=CARTESIAN_POINT('Ctrl Pts',(2.99888829585914,0.91833650204669,1.75999999999999));
#138144=CARTESIAN_POINT('',(2.99888829585913,0.91833650204669,-6.66133814775094E-15));
#138145=CARTESIAN_POINT('Origin',(-8.88178376686733E-15,1.00000037997959,
-4.00000000000001));
#138146=CARTESIAN_POINT('',(2.99888829585914,1.08166425791249,-4.00000000000001));
#138147=CARTESIAN_POINT('Ctrl Pts',(2.99888829585914,1.08166425791249,-4.00000000000001));
#138148=CARTESIAN_POINT('Ctrl Pts',(2.99888829585914,1.08166425791249,1.76000000000005));
#138149=CARTESIAN_POINT('Ctrl Pts',(2.88267087431383,1.18084192839999,-4.00000000000001));
#138150=CARTESIAN_POINT('Ctrl Pts',(2.88267087431383,1.18084192839999,1.76000000000005));
#138151=CARTESIAN_POINT('Ctrl Pts',(2.76068287246971,1.26224670259339,-3.99999999999999));
#138152=CARTESIAN_POINT('Ctrl Pts',(2.76068287246971,1.26224670259339,1.76000000000007));
#138153=CARTESIAN_POINT('Ctrl Pts',(2.50485018029661,1.38709985462769,-4.00000000000004));
#138154=CARTESIAN_POINT('Ctrl Pts',(2.50485018029661,1.38709985462769,1.76000000000002));
#138155=CARTESIAN_POINT('Ctrl Pts',(2.33008073891961,1.44678146098259,-3.99999999999996));
#138156=CARTESIAN_POINT('Ctrl Pts',(2.33008073891961,1.44678146098259,1.7600000000001));
#138157=CARTESIAN_POINT('Ctrl Pts',(2.18514148705334,1.43241869015189,-4.00000000000001));
#138158=CARTESIAN_POINT('Ctrl Pts',(2.18514148705334,1.43241869015189,1.76000000000005));
#138159=CARTESIAN_POINT('',(2.18514148705334,1.43241869015189,-4.00000000000001));
#138160=CARTESIAN_POINT('Origin',(2.18514148705334,1.43241869015189,-4.00000000000001));
#138161=CARTESIAN_POINT('Origin',(-8.88178376686733E-15,1.00000037997959,
-18.425));
#138162=CARTESIAN_POINT('',(-17.5,1.00000037997959,-18.4));
#138163=CARTESIAN_POINT('',(8.13264802145921,-14.4954839996407,-18.4));
#138164=CARTESIAN_POINT('Origin',(-8.88178376686733E-15,1.00000037997959,
-18.4));
#138165=CARTESIAN_POINT('',(8.08617574705085,-14.4069383746142,-18.45));
#138166=CARTESIAN_POINT('',(8.10941188425504,-14.4512111871275,-18.425));
#138167=CARTESIAN_POINT('Origin',(4.44089252863457E-15,1.00000037997959,
-18.45));
#138168=CARTESIAN_POINT('Origin',(-8.88178376686733E-15,1.00000037997959,
-18.4));
#138169=CARTESIAN_POINT('Origin',(-8.88178376686733E-15,1.00000037997959,
-18.475));
#138170=CARTESIAN_POINT('',(-17.5,1.00000037997959,-18.5));
#138171=CARTESIAN_POINT('',(8.13264802145921,-14.4954839996407,-18.5));
#138172=CARTESIAN_POINT('Origin',(-8.88178376686733E-15,1.00000037997959,
-18.5));
#138173=CARTESIAN_POINT('',(8.10941188425504,-14.4512111871275,-18.475));
#138174=CARTESIAN_POINT('Origin',(-8.88178376686733E-15,1.00000037997959,
-18.5));
#138175=CARTESIAN_POINT('Origin',(-8.88178376686733E-15,1.00000037997959,
-10.));
#138176=CARTESIAN_POINT('',(-17.5,1.00000037997959,-17.9285714285714));
#138177=CARTESIAN_POINT('',(-17.5,1.00000037997959,-10.));
#138178=CARTESIAN_POINT('',(8.13264802145921,-14.4954839996407,-17.9285714285714));
#138179=CARTESIAN_POINT('Origin',(-8.88178376686733E-15,1.00000037997959,
-17.9285714285714));
#138180=CARTESIAN_POINT('Origin',(-8.88178376686733E-15,1.00000037997959,
-17.9285714285714));
#138181=CARTESIAN_POINT('Origin',(-8.88178376686733E-15,1.00000037997959,
-10.));
#138182=CARTESIAN_POINT('',(-17.5,1.00000037997959,-10.));
#138183=CARTESIAN_POINT('Origin',(-8.88178376686733E-15,1.00000037997959,
-17.8535714285714));
#138184=CARTESIAN_POINT('',(-17.5,1.00000037997959,-17.8285714285714));
#138185=CARTESIAN_POINT('',(8.13264802145921,-14.4954839996407,-17.8285714285714));
#138186=CARTESIAN_POINT('Origin',(-8.88178376686733E-15,1.00000037997959,
-17.8285714285714));
#138187=CARTESIAN_POINT('',(8.08617574705085,-14.4069383746142,-17.8785714285714));
#138188=CARTESIAN_POINT('',(8.10941188425504,-14.4512111871275,-17.8535714285714));
#138189=CARTESIAN_POINT('Origin',(4.44089252863457E-15,1.00000037997959,
-17.8785714285714));
#138190=CARTESIAN_POINT('Origin',(-8.88178376686733E-15,1.00000037997959,
-17.8285714285714));
#138191=CARTESIAN_POINT('Origin',(-8.88178376686733E-15,1.00000037997959,
-17.9035714285714));
#138192=CARTESIAN_POINT('',(8.10941188425504,-14.4512111871275,-17.9035714285714));
#138193=CARTESIAN_POINT('Origin',(-8.88178376686733E-15,1.00000037997959,
-10.));
#138194=CARTESIAN_POINT('',(-17.5,1.00000037997959,-17.3571428571429));
#138195=CARTESIAN_POINT('',(-17.5,1.00000037997959,-10.));
#138196=CARTESIAN_POINT('',(8.13264802145921,-14.4954839996407,-17.3571428571429));
#138197=CARTESIAN_POINT('Origin',(-8.88178376686733E-15,1.00000037997959,
-17.3571428571429));
#138198=CARTESIAN_POINT('Origin',(-8.88178376686733E-15,1.00000037997959,
-17.3571428571429));
#138199=CARTESIAN_POINT('Origin',(-8.88178376686733E-15,1.00000037997959,
-17.2821428571429));
#138200=CARTESIAN_POINT('',(-17.5,1.00000037997959,-17.2571428571429));
#138201=CARTESIAN_POINT('',(8.13264802145921,-14.4954839996407,-17.2571428571429));
#138202=CARTESIAN_POINT('Origin',(-8.88178376686733E-15,1.00000037997959,
-17.2571428571429));
#138203=CARTESIAN_POINT('',(8.08617574705085,-14.4069383746142,-17.3071428571429));
#138204=CARTESIAN_POINT('',(8.10941188425504,-14.4512111871275,-17.2821428571429));
#138205=CARTESIAN_POINT('Origin',(4.44089252863457E-15,1.00000037997959,
-17.3071428571429));
#138206=CARTESIAN_POINT('Origin',(-8.88178376686733E-15,1.00000037997959,
-17.2571428571429));
#138207=CARTESIAN_POINT('Origin',(-8.88178376686733E-15,1.00000037997959,
-17.3321428571429));
#138208=CARTESIAN_POINT('',(8.10941188425504,-14.4512111871275,-17.3321428571429));
#138209=CARTESIAN_POINT('Origin',(-8.88178376686733E-15,1.00000037997959,
-10.));
#138210=CARTESIAN_POINT('',(-17.5,1.00000037997959,-16.7857142857143));
#138211=CARTESIAN_POINT('',(-17.5,1.00000037997959,-10.));
#138212=CARTESIAN_POINT('',(8.13264802145921,-14.4954839996407,-16.7857142857143));
#138213=CARTESIAN_POINT('Origin',(-8.88178376686733E-15,1.00000037997959,
-16.7857142857143));
#138214=CARTESIAN_POINT('Origin',(-8.88178376686733E-15,1.00000037997959,
-16.7857142857143));
#138215=CARTESIAN_POINT('Origin',(-8.88178376686733E-15,1.00000037997959,
-16.7107142857143));
#138216=CARTESIAN_POINT('',(-17.5,1.00000037997959,-16.6857142857143));
#138217=CARTESIAN_POINT('',(8.13264802145921,-14.4954839996407,-16.6857142857143));
#138218=CARTESIAN_POINT('Origin',(-8.88178376686733E-15,1.00000037997959,
-16.6857142857143));
#138219=CARTESIAN_POINT('',(8.08617574705085,-14.4069383746142,-16.7357142857143));
#138220=CARTESIAN_POINT('',(8.10941188425504,-14.4512111871275,-16.7107142857143));
#138221=CARTESIAN_POINT('Origin',(4.44089252863457E-15,1.00000037997959,
-16.7357142857143));
#138222=CARTESIAN_POINT('Origin',(-8.88178376686733E-15,1.00000037997959,
-16.6857142857143));
#138223=CARTESIAN_POINT('Origin',(-8.88178376686733E-15,1.00000037997959,
-16.7607142857143));
#138224=CARTESIAN_POINT('',(8.10941188425504,-14.4512111871275,-16.7607142857143));
#138225=CARTESIAN_POINT('Origin',(-8.88178376686733E-15,1.00000037997959,
-10.));
#138226=CARTESIAN_POINT('',(-17.5,1.00000037997959,-16.2142857142857));
#138227=CARTESIAN_POINT('',(-17.5,1.00000037997959,-10.));
#138228=CARTESIAN_POINT('',(8.13264802145921,-14.4954839996407,-16.2142857142857));
#138229=CARTESIAN_POINT('Origin',(-8.88178376686733E-15,1.00000037997959,
-16.2142857142857));
#138230=CARTESIAN_POINT('Origin',(-8.88178376686733E-15,1.00000037997959,
-16.2142857142857));
#138231=CARTESIAN_POINT('Origin',(-8.88178376686733E-15,1.00000037997959,
-16.1392857142857));
#138232=CARTESIAN_POINT('',(-17.5,1.00000037997959,-16.1142857142857));
#138233=CARTESIAN_POINT('',(8.13264802145921,-14.4954839996407,-16.1142857142857));
#138234=CARTESIAN_POINT('Origin',(-8.88178376686733E-15,1.00000037997959,
-16.1142857142857));
#138235=CARTESIAN_POINT('',(8.08617574705085,-14.4069383746142,-16.1642857142857));
#138236=CARTESIAN_POINT('',(8.10941188425504,-14.4512111871275,-16.1392857142857));
#138237=CARTESIAN_POINT('Origin',(4.44089252863457E-15,1.00000037997959,
-16.1642857142857));
#138238=CARTESIAN_POINT('Origin',(-8.88178376686733E-15,1.00000037997959,
-16.1142857142857));
#138239=CARTESIAN_POINT('Origin',(-8.88178376686733E-15,1.00000037997959,
-16.1892857142857));
#138240=CARTESIAN_POINT('',(8.10941188425504,-14.4512111871275,-16.1892857142857));
#138241=CARTESIAN_POINT('Origin',(-8.88178376686733E-15,1.00000037997959,
-10.));
#138242=CARTESIAN_POINT('',(-17.5,1.00000037997959,-15.6428571428571));
#138243=CARTESIAN_POINT('',(-17.5,1.00000037997959,-10.));
#138244=CARTESIAN_POINT('',(8.13264802145921,-14.4954839996407,-15.6428571428571));
#138245=CARTESIAN_POINT('Origin',(-8.88178376686733E-15,1.00000037997959,
-15.6428571428571));
#138246=CARTESIAN_POINT('Origin',(-8.88178376686733E-15,1.00000037997959,
-15.6428571428571));
#138247=CARTESIAN_POINT('Origin',(-8.88178376686733E-15,1.00000037997959,
-15.5678571428571));
#138248=CARTESIAN_POINT('',(-17.5,1.00000037997959,-15.5428571428571));
#138249=CARTESIAN_POINT('',(8.13264802145921,-14.4954839996407,-15.5428571428571));
#138250=CARTESIAN_POINT('Origin',(-8.88178376686733E-15,1.00000037997959,
-15.5428571428571));
#138251=CARTESIAN_POINT('',(8.08617574705085,-14.4069383746142,-15.5928571428572));
#138252=CARTESIAN_POINT('',(8.10941188425504,-14.4512111871275,-15.5678571428571));
#138253=CARTESIAN_POINT('Origin',(4.44089252863457E-15,1.00000037997959,
-15.5928571428571));
#138254=CARTESIAN_POINT('Origin',(-8.88178376686733E-15,1.00000037997959,
-15.5428571428571));
#138255=CARTESIAN_POINT('Origin',(-8.88178376686733E-15,1.00000037997959,
-15.6178571428571));
#138256=CARTESIAN_POINT('',(8.10941188425504,-14.4512111871275,-15.6178571428571));
#138257=CARTESIAN_POINT('Origin',(-8.88178376686733E-15,1.00000037997959,
-10.));
#138258=CARTESIAN_POINT('',(-17.5,1.00000037997959,-15.0714285714286));
#138259=CARTESIAN_POINT('',(-17.5,1.00000037997959,-10.));
#138260=CARTESIAN_POINT('',(8.13264802145921,-14.4954839996407,-15.0714285714286));
#138261=CARTESIAN_POINT('Origin',(-8.88178376686733E-15,1.00000037997959,
-15.0714285714286));
#138262=CARTESIAN_POINT('Origin',(-8.88178376686733E-15,1.00000037997959,
-15.0714285714286));
#138263=CARTESIAN_POINT('Origin',(-8.88178376686733E-15,1.00000037997959,
-14.9964285714286));
#138264=CARTESIAN_POINT('',(-17.5,1.00000037997959,-14.9714285714286));
#138265=CARTESIAN_POINT('',(8.13264802145921,-14.4954839996407,-14.9714285714286));
#138266=CARTESIAN_POINT('Origin',(-8.88178376686733E-15,1.00000037997959,
-14.9714285714286));
#138267=CARTESIAN_POINT('',(8.08617574705085,-14.4069383746142,-15.0214285714286));
#138268=CARTESIAN_POINT('',(8.10941188425504,-14.4512111871275,-14.9964285714286));
#138269=CARTESIAN_POINT('Origin',(4.44089252863457E-15,1.00000037997959,
-15.0214285714286));
#138270=CARTESIAN_POINT('Origin',(-8.88178376686733E-15,1.00000037997959,
-14.9714285714286));
#138271=CARTESIAN_POINT('Origin',(-8.88178376686733E-15,1.00000037997959,
-15.0464285714286));
#138272=CARTESIAN_POINT('',(8.10941188425504,-14.4512111871275,-15.0464285714286));
#138273=CARTESIAN_POINT('Origin',(-8.88178376686733E-15,1.00000037997959,
-10.));
#138274=CARTESIAN_POINT('',(-17.5,1.00000037997959,-14.5));
#138275=CARTESIAN_POINT('',(-17.5,1.00000037997959,-10.));
#138276=CARTESIAN_POINT('',(8.13264802145921,-14.4954839996407,-14.5));
#138277=CARTESIAN_POINT('Origin',(-8.88178376686733E-15,1.00000037997959,
-14.5));
#138278=CARTESIAN_POINT('Origin',(-8.88178376686733E-15,1.00000037997959,
-14.5));
#138279=CARTESIAN_POINT('Origin',(-8.88178376686733E-15,1.00000037997959,
-14.425));
#138280=CARTESIAN_POINT('',(-17.5,1.00000037997959,-14.4));
#138281=CARTESIAN_POINT('',(8.13264802145921,-14.4954839996407,-14.4));
#138282=CARTESIAN_POINT('Origin',(-8.88178376686733E-15,1.00000037997959,
-14.4));
#138283=CARTESIAN_POINT('',(8.08617574705085,-14.4069383746142,-14.45));
#138284=CARTESIAN_POINT('',(8.10941188425504,-14.4512111871275,-14.425));
#138285=CARTESIAN_POINT('Origin',(4.44089252863457E-15,1.00000037997959,
-14.45));
#138286=CARTESIAN_POINT('Origin',(-8.88178376686733E-15,1.00000037997959,
-14.4));
#138287=CARTESIAN_POINT('Origin',(-8.88178376686733E-15,1.00000037997959,
-14.475));
#138288=CARTESIAN_POINT('',(8.10941188425504,-14.4512111871275,-14.475));
#138289=CARTESIAN_POINT('Origin',(-8.88178376686733E-15,1.00000037997959,
-10.));
#138290=CARTESIAN_POINT('',(-17.5,1.00000037997959,-13.9285714285714));
#138291=CARTESIAN_POINT('',(-17.5,1.00000037997959,-10.));
#138292=CARTESIAN_POINT('',(8.13264802145921,-14.4954839996407,-13.9285714285714));
#138293=CARTESIAN_POINT('Origin',(-8.88178376686733E-15,1.00000037997959,
-13.9285714285714));
#138294=CARTESIAN_POINT('Origin',(-8.88178376686733E-15,1.00000037997959,
-13.9285714285714));
#138295=CARTESIAN_POINT('Origin',(-8.88178376686733E-15,1.00000037997959,
-13.8535714285714));
#138296=CARTESIAN_POINT('',(-17.5,1.00000037997959,-13.8285714285714));
#138297=CARTESIAN_POINT('',(8.13264802145921,-14.4954839996407,-13.8285714285714));
#138298=CARTESIAN_POINT('Origin',(-8.88178376686733E-15,1.00000037997959,
-13.8285714285714));
#138299=CARTESIAN_POINT('',(8.08617574705085,-14.4069383746142,-13.8785714285714));
#138300=CARTESIAN_POINT('',(8.10941188425504,-14.4512111871275,-13.8535714285714));
#138301=CARTESIAN_POINT('Origin',(4.44089252863457E-15,1.00000037997959,
-13.8785714285714));
#138302=CARTESIAN_POINT('Origin',(-8.88178376686733E-15,1.00000037997959,
-13.8285714285714));
#138303=CARTESIAN_POINT('Origin',(-8.88178376686733E-15,1.00000037997959,
-13.9035714285714));
#138304=CARTESIAN_POINT('',(8.10941188425504,-14.4512111871275,-13.9035714285714));
#138305=CARTESIAN_POINT('Origin',(-8.88178376686733E-15,1.00000037997959,
-10.));
#138306=CARTESIAN_POINT('',(-17.5,1.00000037997959,-13.3571428571429));
#138307=CARTESIAN_POINT('',(-17.5,1.00000037997959,-10.));
#138308=CARTESIAN_POINT('',(8.13264802145921,-14.4954839996407,-13.3571428571429));
#138309=CARTESIAN_POINT('Origin',(-8.88178376686733E-15,1.00000037997959,
-13.3571428571429));
#138310=CARTESIAN_POINT('Origin',(-8.88178376686733E-15,1.00000037997959,
-13.3571428571429));
#138311=CARTESIAN_POINT('Origin',(-8.88178376686733E-15,1.00000037997959,
-13.2821428571429));
#138312=CARTESIAN_POINT('',(-17.5,1.00000037997959,-13.2571428571429));
#138313=CARTESIAN_POINT('',(8.13264802145921,-14.4954839996407,-13.2571428571429));
#138314=CARTESIAN_POINT('Origin',(-8.88178376686733E-15,1.00000037997959,
-13.2571428571429));
#138315=CARTESIAN_POINT('',(8.08617574705085,-14.4069383746142,-13.3071428571429));
#138316=CARTESIAN_POINT('',(8.10941188425504,-14.4512111871275,-13.2821428571429));
#138317=CARTESIAN_POINT('Origin',(4.44089252863457E-15,1.00000037997959,
-13.3071428571429));
#138318=CARTESIAN_POINT('Origin',(-8.88178376686733E-15,1.00000037997959,
-13.2571428571429));
#138319=CARTESIAN_POINT('Origin',(-8.88178376686733E-15,1.00000037997959,
-13.3321428571429));
#138320=CARTESIAN_POINT('',(8.10941188425504,-14.4512111871275,-13.3321428571429));
#138321=CARTESIAN_POINT('Origin',(-8.88178376686733E-15,1.00000037997959,
-10.));
#138322=CARTESIAN_POINT('',(-17.5,1.00000037997959,-12.7857142857143));
#138323=CARTESIAN_POINT('',(-17.5,1.00000037997959,-10.));
#138324=CARTESIAN_POINT('',(8.13264802145921,-14.4954839996407,-12.7857142857143));
#138325=CARTESIAN_POINT('Origin',(-8.88178376686733E-15,1.00000037997959,
-12.7857142857143));
#138326=CARTESIAN_POINT('Origin',(-8.88178376686733E-15,1.00000037997959,
-12.7857142857143));
#138327=CARTESIAN_POINT('Origin',(-8.88178376686733E-15,1.00000037997959,
-12.7107142857143));
#138328=CARTESIAN_POINT('',(-17.5,1.00000037997959,-12.6857142857143));
#138329=CARTESIAN_POINT('',(8.13264802145921,-14.4954839996407,-12.6857142857143));
#138330=CARTESIAN_POINT('Origin',(-8.88178376686733E-15,1.00000037997959,
-12.6857142857143));
#138331=CARTESIAN_POINT('',(8.08617574705085,-14.4069383746142,-12.7357142857143));
#138332=CARTESIAN_POINT('',(8.10941188425504,-14.4512111871275,-12.7107142857143));
#138333=CARTESIAN_POINT('Origin',(4.44089252863457E-15,1.00000037997959,
-12.7357142857143));
#138334=CARTESIAN_POINT('Origin',(-8.88178376686733E-15,1.00000037997959,
-12.6857142857143));
#138335=CARTESIAN_POINT('Origin',(-8.88178376686733E-15,1.00000037997959,
-12.7607142857143));
#138336=CARTESIAN_POINT('',(8.10941188425504,-14.4512111871275,-12.7607142857143));
#138337=CARTESIAN_POINT('Origin',(-8.88178376686733E-15,1.00000037997959,
-10.));
#138338=CARTESIAN_POINT('',(-17.5,1.00000037997959,-12.2142857142857));
#138339=CARTESIAN_POINT('',(-17.5,1.00000037997959,-10.));
#138340=CARTESIAN_POINT('',(8.13264802145921,-14.4954839996407,-12.2142857142857));
#138341=CARTESIAN_POINT('Origin',(-8.88178376686733E-15,1.00000037997959,
-12.2142857142857));
#138342=CARTESIAN_POINT('Origin',(-8.88178376686733E-15,1.00000037997959,
-12.2142857142857));
#138343=CARTESIAN_POINT('Origin',(-8.88178376686733E-15,1.00000037997959,
-12.1392857142857));
#138344=CARTESIAN_POINT('',(-17.5,1.00000037997959,-12.1142857142857));
#138345=CARTESIAN_POINT('',(8.13264802145921,-14.4954839996407,-12.1142857142857));
#138346=CARTESIAN_POINT('Origin',(-8.88178376686733E-15,1.00000037997959,
-12.1142857142857));
#138347=CARTESIAN_POINT('',(8.08617574705085,-14.4069383746142,-12.1642857142857));
#138348=CARTESIAN_POINT('',(8.10941188425504,-14.4512111871275,-12.1392857142857));
#138349=CARTESIAN_POINT('Origin',(4.44089252863457E-15,1.00000037997959,
-12.1642857142857));
#138350=CARTESIAN_POINT('Origin',(-8.88178376686733E-15,1.00000037997959,
-12.1142857142857));
#138351=CARTESIAN_POINT('Origin',(-8.88178376686733E-15,1.00000037997959,
-12.1892857142857));
#138352=CARTESIAN_POINT('',(8.10941188425504,-14.4512111871275,-12.1892857142857));
#138353=CARTESIAN_POINT('Origin',(-8.88178376686733E-15,1.00000037997959,
-10.));
#138354=CARTESIAN_POINT('',(-17.5,1.00000037997959,-11.6428571428571));
#138355=CARTESIAN_POINT('',(-17.5,1.00000037997959,-10.));
#138356=CARTESIAN_POINT('',(8.13264802145921,-14.4954839996407,-11.6428571428571));
#138357=CARTESIAN_POINT('Origin',(-8.88178376686733E-15,1.00000037997959,
-11.6428571428571));
#138358=CARTESIAN_POINT('Origin',(-8.88178376686733E-15,1.00000037997959,
-11.6428571428571));
#138359=CARTESIAN_POINT('Origin',(-8.88178376686733E-15,1.00000037997959,
-11.5678571428571));
#138360=CARTESIAN_POINT('',(-17.5,1.00000037997959,-11.5428571428571));
#138361=CARTESIAN_POINT('',(8.13264802145921,-14.4954839996407,-11.5428571428571));
#138362=CARTESIAN_POINT('Origin',(-8.88178376686733E-15,1.00000037997959,
-11.5428571428571));
#138363=CARTESIAN_POINT('',(8.08617574705085,-14.4069383746142,-11.5928571428572));
#138364=CARTESIAN_POINT('',(8.10941188425504,-14.4512111871275,-11.5678571428571));
#138365=CARTESIAN_POINT('Origin',(4.44089252863457E-15,1.00000037997959,
-11.5928571428571));
#138366=CARTESIAN_POINT('Origin',(-8.88178376686733E-15,1.00000037997959,
-11.5428571428571));
#138367=CARTESIAN_POINT('Origin',(-8.88178376686733E-15,1.00000037997959,
-11.6178571428571));
#138368=CARTESIAN_POINT('',(8.10941188425504,-14.4512111871275,-11.6178571428571));
#138369=CARTESIAN_POINT('Origin',(-8.88178376686733E-15,1.00000037997959,
-10.));
#138370=CARTESIAN_POINT('',(-17.5,1.00000037997959,-11.0714285714286));
#138371=CARTESIAN_POINT('',(-17.5,1.00000037997959,-10.));
#138372=CARTESIAN_POINT('',(8.13264802145921,-14.4954839996407,-11.0714285714286));
#138373=CARTESIAN_POINT('Origin',(-8.88178376686733E-15,1.00000037997959,
-11.0714285714286));
#138374=CARTESIAN_POINT('Origin',(-8.88178376686733E-15,1.00000037997959,
-11.0714285714286));
#138375=CARTESIAN_POINT('Origin',(-8.88178376686733E-15,1.00000037997959,
-10.9964285714286));
#138376=CARTESIAN_POINT('',(-17.5,1.00000037997959,-10.9714285714286));
#138377=CARTESIAN_POINT('',(8.13264802145921,-14.4954839996407,-10.9714285714286));
#138378=CARTESIAN_POINT('Origin',(-8.88178376686733E-15,1.00000037997959,
-10.9714285714286));
#138379=CARTESIAN_POINT('',(8.08617574705085,-14.4069383746142,-11.0214285714286));
#138380=CARTESIAN_POINT('',(8.10941188425504,-14.4512111871275,-10.9964285714286));
#138381=CARTESIAN_POINT('Origin',(4.44089252863457E-15,1.00000037997959,
-11.0214285714286));
#138382=CARTESIAN_POINT('Origin',(-8.88178376686733E-15,1.00000037997959,
-10.9714285714286));
#138383=CARTESIAN_POINT('Origin',(-8.88178376686733E-15,1.00000037997959,
-11.0464285714286));
#138384=CARTESIAN_POINT('',(8.10941188425504,-14.4512111871275,-11.0464285714286));
#138385=CARTESIAN_POINT('Origin',(21.9499999789786,0.999999999999992,-6.00000000000001));
#138386=CARTESIAN_POINT('Origin',(-8.88178376686733E-15,1.00000037997959,
-10.));
#138387=CARTESIAN_POINT('',(-17.5,1.00000037997959,-10.5));
#138388=CARTESIAN_POINT('',(-17.5,1.00000037997959,-10.));
#138389=CARTESIAN_POINT('',(8.13264802145921,-14.4954839996407,-10.5));
#138390=CARTESIAN_POINT('Origin',(-8.88178376686733E-15,1.00000037997959,
-10.5));
#138391=CARTESIAN_POINT('Origin',(-8.88178376686733E-15,1.00000037997959,
-10.5));
#138392=CARTESIAN_POINT('Origin',(-8.88178376686733E-15,1.00000037997959,
-10.425));
#138393=CARTESIAN_POINT('',(-17.5,1.00000037997959,-10.4));
#138394=CARTESIAN_POINT('',(8.13264802145921,-14.4954839996407,-10.4));
#138395=CARTESIAN_POINT('Origin',(-8.88178376686733E-15,1.00000037997959,
-10.4));
#138396=CARTESIAN_POINT('Origin',(-8.88178376686733E-15,1.00000037997959,
-10.4));
#138397=CARTESIAN_POINT('',(8.08617574705085,-14.4069383746142,-10.45));
#138398=CARTESIAN_POINT('',(8.10941188425504,-14.4512111871275,-10.425));
#138399=CARTESIAN_POINT('Origin',(4.44089252863457E-15,1.00000037997959,
-10.45));
#138400=CARTESIAN_POINT('Origin',(-8.88178376686733E-15,1.00000037997959,
-10.475));
#138401=CARTESIAN_POINT('',(8.10941188425504,-14.4512111871275,-10.475));
#138402=CARTESIAN_POINT('Origin',(-8.88178376686733E-15,1.00000037997959,
-10.));
#138403=CARTESIAN_POINT('',(-17.5,1.00000037997959,-10.));
#138404=CARTESIAN_POINT('Origin',(-8.88178376686733E-15,1.00000037997959,
-5.55111512312578E-15));
#138405=CARTESIAN_POINT('',(-1.50000000000001,1.00000037997959,-5.55111512312578E-15));
#138406=CARTESIAN_POINT('Origin',(-17.2355011741645,-5.00000000000001,-6.00000000000001));
#138407=CARTESIAN_POINT('Origin',(-2.10213452200843E-8,0.999999999999992,
-23.));
#138408=CARTESIAN_POINT('',(0.,0.,0.));
#138409=CARTESIAN_POINT('Origin',(2.,0.,0.));
#138410=CARTESIAN_POINT('',(-3.44818792991333,0.6,0.));
#138411=CARTESIAN_POINT('',(-1.90787840283389,0.6,0.));
#138412=CARTESIAN_POINT('',(-5.,0.6,0.));
#138413=CARTESIAN_POINT('',(-0.599999999999999,3.44818792991333,0.));
#138414=CARTESIAN_POINT('Origin',(0.,0.,0.));
#138415=CARTESIAN_POINT('',(-0.6,1.90787840283389,0.));
#138416=CARTESIAN_POINT('',(-0.6,1.90787840283389,0.));
#138417=CARTESIAN_POINT('Origin',(0.,0.,0.));
#138418=CARTESIAN_POINT('Origin',(2.,0.,0.));
#138419=CARTESIAN_POINT('',(-1.90787840283389,-0.6,0.));
#138420=CARTESIAN_POINT('',(-3.44818792991333,-0.599999999999999,0.));
#138421=CARTESIAN_POINT('',(-1.90787840283389,-0.6,0.));
#138422=CARTESIAN_POINT('',(-0.6,-1.90787840283389,0.));
#138423=CARTESIAN_POINT('Origin',(0.,0.,0.));
#138424=CARTESIAN_POINT('',(-0.6,-3.44818792991333,0.));
#138425=CARTESIAN_POINT('',(-0.6,-5.,0.));
#138426=CARTESIAN_POINT('Origin',(0.,0.,0.));
#138427=CARTESIAN_POINT('Origin',(2.,0.,0.));
#138428=CARTESIAN_POINT('',(0.6,-1.90787840283389,0.));
#138429=CARTESIAN_POINT('',(0.599999999999999,-3.44818792991333,0.));
#138430=CARTESIAN_POINT('',(0.6,-1.90787840283389,0.));
#138431=CARTESIAN_POINT('',(1.90787840283389,-0.6,0.));
#138432=CARTESIAN_POINT('Origin',(0.,0.,0.));
#138433=CARTESIAN_POINT('',(3.44818792991333,-0.6,0.));
#138434=CARTESIAN_POINT('',(5.,-0.6,0.));
#138435=CARTESIAN_POINT('Origin',(0.,0.,0.));
#138436=CARTESIAN_POINT('Origin',(0.,0.,0.));
#138437=CARTESIAN_POINT('',(-3.95474398665704,0.6,1.5));
#138438=CARTESIAN_POINT('Ctrl Pts',(-3.95474398665705,0.6,1.49999999999998));
#138439=CARTESIAN_POINT('Ctrl Pts',(-3.68458075639299,0.6,0.698680192272979));
#138440=CARTESIAN_POINT('Ctrl Pts',(-3.44818792991332,0.6,-1.17676210180771E-13));
#138441=CARTESIAN_POINT('',(-0.599999999999999,3.95474398665704,1.5));
#138442=CARTESIAN_POINT('Origin',(0.,0.,1.5));
#138443=CARTESIAN_POINT('Ctrl Pts',(-0.6,3.4481879299133,-1.06445473175915E-13));
#138444=CARTESIAN_POINT('Ctrl Pts',(-0.6,3.68458075639367,0.698680192275089));
#138445=CARTESIAN_POINT('Ctrl Pts',(-0.6,3.95474398665703,1.49999999999999));
#138446=CARTESIAN_POINT('Origin',(0.,0.,0.));
#138447=CARTESIAN_POINT('',(-3.95474398665704,-0.599999999999999,1.5));
#138448=CARTESIAN_POINT('Ctrl Pts',(-3.4481879299133,-0.6,-1.05897632346403E-13));
#138449=CARTESIAN_POINT('Ctrl Pts',(-3.68458075639369,-0.6,0.698680192275146));
#138450=CARTESIAN_POINT('Ctrl Pts',(-3.95474398665703,-0.6,1.49999999999999));
#138451=CARTESIAN_POINT('',(-0.6,-3.95474398665704,1.5));
#138452=CARTESIAN_POINT('Ctrl Pts',(-0.6,-3.95474398665703,1.49999999999999));
#138453=CARTESIAN_POINT('Ctrl Pts',(-0.6,-3.68458075639366,0.698680192275045));
#138454=CARTESIAN_POINT('Ctrl Pts',(-0.6,-3.4481879299133,-1.08088995664484E-13));
#138455=CARTESIAN_POINT('Origin',(0.,0.,1.5));
#138456=CARTESIAN_POINT('Origin',(0.,0.,0.));
#138457=CARTESIAN_POINT('',(0.599999999999999,-3.95474398665704,1.5));
#138458=CARTESIAN_POINT('Ctrl Pts',(0.6,-3.4481879299133,-1.06609825424756E-13));
#138459=CARTESIAN_POINT('Ctrl Pts',(0.6,-3.6845807563937,0.698680192275154));
#138460=CARTESIAN_POINT('Ctrl Pts',(0.6,-3.95474398665703,1.49999999999999));
#138461=CARTESIAN_POINT('',(3.95474398665704,-0.6,1.5));
#138462=CARTESIAN_POINT('Ctrl Pts',(3.95474398665703,-0.6,1.49999999999999));
#138463=CARTESIAN_POINT('Ctrl Pts',(3.68458075639368,-0.6,0.698680192275095));
#138464=CARTESIAN_POINT('Ctrl Pts',(3.4481879299133,-0.6,-1.03267996364691E-13));
#138465=CARTESIAN_POINT('Origin',(0.,0.,1.5));
#138466=CARTESIAN_POINT('Origin',(0.,0.,1.5));
#138467=CARTESIAN_POINT('',(-3.44818792991333,0.6,2.3));
#138468=CARTESIAN_POINT('Ctrl Pts',(-3.44818792991347,0.6,2.29999999999978));
#138469=CARTESIAN_POINT('Ctrl Pts',(-3.68458075656704,0.6,1.92737056384667));
#138470=CARTESIAN_POINT('Ctrl Pts',(-3.95474398705481,0.6,1.49999999937077));
#138471=CARTESIAN_POINT('',(-0.599999999999999,3.44818792991333,2.3));
#138472=CARTESIAN_POINT('Origin',(0.,0.,2.3));
#138473=CARTESIAN_POINT('Ctrl Pts',(-0.6,3.95474398665704,1.5));
#138474=CARTESIAN_POINT('Ctrl Pts',(-0.6,3.68458075639373,1.92737056411986));
#138475=CARTESIAN_POINT('Ctrl Pts',(-0.6,3.44818792991333,2.3));
#138476=CARTESIAN_POINT('Origin',(0.,0.,1.5));
#138477=CARTESIAN_POINT('',(-3.44818792991333,-0.599999999999999,2.3));
#138478=CARTESIAN_POINT('Ctrl Pts',(-3.95474398665704,-0.6,1.5));
#138479=CARTESIAN_POINT('Ctrl Pts',(-3.68458075639373,-0.6,1.92737056411986));
#138480=CARTESIAN_POINT('Ctrl Pts',(-3.44818792991333,-0.6,2.3));
#138481=CARTESIAN_POINT('',(-0.6,-3.44818792991333,2.3));
#138482=CARTESIAN_POINT('Ctrl Pts',(-0.600000000000001,-3.44818792991364,
2.2999999999995));
#138483=CARTESIAN_POINT('Ctrl Pts',(-0.600000000000001,-3.68458075656713,
1.92737056384652));
#138484=CARTESIAN_POINT('Ctrl Pts',(-0.600000000000001,-3.95474398705479,
1.49999999937079));
#138485=CARTESIAN_POINT('Origin',(0.,0.,2.3));
#138486=CARTESIAN_POINT('Origin',(0.,0.,1.5));
#138487=CARTESIAN_POINT('',(0.6,-3.44818792991333,2.3));
#138488=CARTESIAN_POINT('Ctrl Pts',(0.6,-3.95474398665704,1.5));
#138489=CARTESIAN_POINT('Ctrl Pts',(0.6,-3.68458075639373,1.92737056411986));
#138490=CARTESIAN_POINT('Ctrl Pts',(0.6,-3.44818792991333,2.3));
#138491=CARTESIAN_POINT('',(3.44818792991333,-0.6,2.3));
#138492=CARTESIAN_POINT('Ctrl Pts',(3.44818792991362,-0.600000000000001,
2.29999999999954));
#138493=CARTESIAN_POINT('Ctrl Pts',(3.68458075656725,-0.600000000000001,
1.92737056384633));
#138494=CARTESIAN_POINT('Ctrl Pts',(3.95474398705511,-0.600000000000001,
1.49999999937029));
#138495=CARTESIAN_POINT('Origin',(0.,0.,2.3));
#138496=CARTESIAN_POINT('Origin',(3.49999999999999,0.,2.3));
#138497=CARTESIAN_POINT('',(-2.93938769133981,0.6,2.3));
#138498=CARTESIAN_POINT('',(3.49999999999999,0.599999999999999,2.3));
#138499=CARTESIAN_POINT('',(-0.6,2.93938769133981,2.3));
#138500=CARTESIAN_POINT('Origin',(0.,0.,2.3));
#138501=CARTESIAN_POINT('',(-0.599999999999999,7.18799175178712E-16,2.3));
#138502=CARTESIAN_POINT('Origin',(3.49999999999999,0.,2.3));
#138503=CARTESIAN_POINT('',(-2.93938769133981,-0.6,2.3));
#138504=CARTESIAN_POINT('',(3.49999999999999,-0.600000000000001,2.3));
#138505=CARTESIAN_POINT('',(-0.6,-2.93938769133981,2.3));
#138506=CARTESIAN_POINT('',(-0.599999999999999,4.31279505107227E-16,2.3));
#138507=CARTESIAN_POINT('Origin',(0.,0.,2.3));
#138508=CARTESIAN_POINT('Origin',(3.49999999999999,0.,2.3));
#138509=CARTESIAN_POINT('',(0.6,-2.93938769133981,2.3));
#138510=CARTESIAN_POINT('',(0.6,5.08418928784942E-16,2.3));
#138511=CARTESIAN_POINT('',(2.93938769133981,-0.6,2.3));
#138512=CARTESIAN_POINT('',(3.49999999999999,-0.6,2.3));
#138513=CARTESIAN_POINT('Origin',(0.,0.,2.3));
#138514=CARTESIAN_POINT('Origin',(0.,0.,0.));
#138515=CARTESIAN_POINT('',(2.,-2.44929359829471E-16,8.));
#138516=CARTESIAN_POINT('Origin',(0.,0.,8.));
#138517=CARTESIAN_POINT('',(2.,-2.44929359829471E-16,6.1));
#138518=CARTESIAN_POINT('',(2.,-2.44929359829471E-16,0.));
#138519=CARTESIAN_POINT('',(1.90787840283389,-0.6,6.1));
#138520=CARTESIAN_POINT('Origin',(0.,0.,6.1));
#138521=CARTESIAN_POINT('',(1.90787840283389,-0.6,6.1));
#138522=CARTESIAN_POINT('',(0.6,-1.90787840283389,6.1));
#138523=CARTESIAN_POINT('',(0.6,-1.90787840283389,6.1));
#138524=CARTESIAN_POINT('',(-0.6,-1.90787840283389,6.1));
#138525=CARTESIAN_POINT('Origin',(0.,0.,6.1));
#138526=CARTESIAN_POINT('',(-0.6,-1.90787840283389,6.1));
#138527=CARTESIAN_POINT('',(-1.90787840283389,-0.6,6.1));
#138528=CARTESIAN_POINT('',(-1.90787840283389,-0.6,6.1));
#138529=CARTESIAN_POINT('',(-1.90787840283389,0.6,6.1));
#138530=CARTESIAN_POINT('Origin',(0.,0.,6.1));
#138531=CARTESIAN_POINT('',(-1.90787840283389,0.6,6.1));
#138532=CARTESIAN_POINT('',(-0.6,1.90787840283389,6.1));
#138533=CARTESIAN_POINT('',(-0.6,1.90787840283389,6.1));
#138534=CARTESIAN_POINT('',(0.6,1.90787840283389,6.1));
#138535=CARTESIAN_POINT('Origin',(0.,0.,6.1));
#138536=CARTESIAN_POINT('',(0.6,1.90787840283389,0.));
#138537=CARTESIAN_POINT('',(0.6,1.90787840283389,6.1));
#138538=CARTESIAN_POINT('',(1.90787840283389,0.6,0.));
#138539=CARTESIAN_POINT('Origin',(0.,0.,0.));
#138540=CARTESIAN_POINT('',(1.90787840283389,0.6,6.1));
#138541=CARTESIAN_POINT('',(1.90787840283389,0.6,6.1));
#138542=CARTESIAN_POINT('Origin',(0.,0.,6.1));
#138543=CARTESIAN_POINT('Origin',(2.,0.,0.));
#138544=CARTESIAN_POINT('',(0.6,3.44818792991333,0.));
#138545=CARTESIAN_POINT('',(0.6,5.,0.));
#138546=CARTESIAN_POINT('',(3.44818792991333,0.599999999999999,0.));
#138547=CARTESIAN_POINT('Origin',(0.,0.,0.));
#138548=CARTESIAN_POINT('',(1.90787840283389,0.6,0.));
#138549=CARTESIAN_POINT('Origin',(0.,0.,0.));
#138550=CARTESIAN_POINT('',(0.6,3.95474398665704,1.5));
#138551=CARTESIAN_POINT('Ctrl Pts',(0.6,3.95474398665705,1.49999999999998));
#138552=CARTESIAN_POINT('Ctrl Pts',(0.6,3.68458075639299,0.698680192272979));
#138553=CARTESIAN_POINT('Ctrl Pts',(0.6,3.44818792991332,-1.17676210180771E-13));
#138554=CARTESIAN_POINT('',(3.95474398665704,0.599999999999999,1.5));
#138555=CARTESIAN_POINT('Origin',(0.,0.,1.5));
#138556=CARTESIAN_POINT('Ctrl Pts',(3.4481879299133,0.6,-1.06445473175915E-13));
#138557=CARTESIAN_POINT('Ctrl Pts',(3.68458075639367,0.6,0.698680192275089));
#138558=CARTESIAN_POINT('Ctrl Pts',(3.95474398665703,0.6,1.49999999999999));
#138559=CARTESIAN_POINT('Origin',(0.,0.,1.5));
#138560=CARTESIAN_POINT('',(0.6,3.44818792991333,2.3));
#138561=CARTESIAN_POINT('Ctrl Pts',(0.600000000000001,3.44818792991352,
2.2999999999997));
#138562=CARTESIAN_POINT('Ctrl Pts',(0.600000000000001,3.68458075656709,
1.92737056384658));
#138563=CARTESIAN_POINT('Ctrl Pts',(0.600000000000001,3.95474398705488,
1.49999999937066));
#138564=CARTESIAN_POINT('',(3.44818792991333,0.599999999999999,2.3));
#138565=CARTESIAN_POINT('Origin',(0.,0.,2.3));
#138566=CARTESIAN_POINT('Ctrl Pts',(3.95474398665705,0.599999999999999,
1.49999999999998));
#138567=CARTESIAN_POINT('Ctrl Pts',(3.68458075639374,0.599999999999999,
1.92737056411985));
#138568=CARTESIAN_POINT('Ctrl Pts',(3.44818792991334,0.599999999999999,
2.29999999999998));
#138569=CARTESIAN_POINT('Origin',(3.49999999999999,0.,2.3));
#138570=CARTESIAN_POINT('',(0.6,2.93938769133981,2.3));
#138571=CARTESIAN_POINT('',(0.6,3.05051357270965E-16,2.3));
#138572=CARTESIAN_POINT('',(2.93938769133981,0.6,2.3));
#138573=CARTESIAN_POINT('Origin',(0.,0.,2.3));
#138574=CARTESIAN_POINT('',(3.49999999999999,0.599999999999999,2.3));
#138575=CARTESIAN_POINT('Origin',(0.,0.,0.));
#138576=CARTESIAN_POINT('',(2.93938769133981,-0.6,6.1));
#138577=CARTESIAN_POINT('',(3.,-3.67394039744206E-16,6.1));
#138578=CARTESIAN_POINT('Origin',(0.,0.,6.1));
#138579=CARTESIAN_POINT('',(3.,-3.67394039744206E-16,6.7));
#138580=CARTESIAN_POINT('',(3.,-3.67394039744206E-16,0.));
#138581=CARTESIAN_POINT('Origin',(0.,0.,6.7));
#138582=CARTESIAN_POINT('',(2.93938769133981,0.6,6.1));
#138583=CARTESIAN_POINT('Origin',(0.,0.,6.1));
#138584=CARTESIAN_POINT('',(2.93938769133981,0.6,0.));
#138585=CARTESIAN_POINT('',(0.6,2.93938769133981,6.1));
#138586=CARTESIAN_POINT('',(0.6,2.93938769133981,0.));
#138587=CARTESIAN_POINT('',(-0.6,2.93938769133981,6.1));
#138588=CARTESIAN_POINT('Origin',(0.,0.,6.1));
#138589=CARTESIAN_POINT('',(-0.6,2.93938769133981,0.));
#138590=CARTESIAN_POINT('',(-2.93938769133981,0.6,6.1));
#138591=CARTESIAN_POINT('',(-2.93938769133981,0.6,0.));
#138592=CARTESIAN_POINT('',(-2.93938769133981,-0.6,6.1));
#138593=CARTESIAN_POINT('Origin',(0.,0.,6.1));
#138594=CARTESIAN_POINT('',(-2.93938769133981,-0.6,0.));
#138595=CARTESIAN_POINT('',(-0.6,-2.93938769133981,6.1));
#138596=CARTESIAN_POINT('',(-0.6,-2.93938769133981,0.));
#138597=CARTESIAN_POINT('',(0.6,-2.93938769133981,6.1));
#138598=CARTESIAN_POINT('Origin',(0.,0.,6.1));
#138599=CARTESIAN_POINT('',(0.6,-2.93938769133981,0.));
#138600=CARTESIAN_POINT('',(2.93938769133981,-0.6,0.));
#138601=CARTESIAN_POINT('Origin',(3.,0.,6.7));
#138602=CARTESIAN_POINT('',(5.,-6.12323399573677E-16,6.7));
#138603=CARTESIAN_POINT('Origin',(0.,0.,6.7));
#138604=CARTESIAN_POINT('Origin',(0.,0.,0.));
#138605=CARTESIAN_POINT('',(5.,-6.12323399573677E-16,8.));
#138606=CARTESIAN_POINT('',(5.,-6.12323399573677E-16,0.));
#138607=CARTESIAN_POINT('Origin',(0.,0.,8.));
#138608=CARTESIAN_POINT('Origin',(5.,0.,8.));
#138609=CARTESIAN_POINT('Origin',(1.90787840283389,0.6,6.1));
#138610=CARTESIAN_POINT('',(1.90787840283389,0.6,6.1));
#138611=CARTESIAN_POINT('Origin',(5.,-0.6,6.1));
#138612=CARTESIAN_POINT('',(5.,-0.6,6.1));
#138613=CARTESIAN_POINT('Origin',(0.,0.,6.1));
#138614=CARTESIAN_POINT('Origin',(-0.6,1.90787840283389,6.1));
#138615=CARTESIAN_POINT('',(-0.6,1.90787840283389,6.1));
#138616=CARTESIAN_POINT('Origin',(0.6,5.,6.1));
#138617=CARTESIAN_POINT('',(0.6,5.,6.1));
#138618=CARTESIAN_POINT('Origin',(0.,0.,6.1));
#138619=CARTESIAN_POINT('Origin',(-0.6,-5.,6.1));
#138620=CARTESIAN_POINT('',(-0.6,-5.,6.1));
#138621=CARTESIAN_POINT('Origin',(0.6,-1.90787840283389,6.1));
#138622=CARTESIAN_POINT('',(0.6,-1.90787840283389,6.1));
#138623=CARTESIAN_POINT('Origin',(0.,0.,6.1));
#138624=CARTESIAN_POINT('Origin',(-5.,0.6,6.1));
#138625=CARTESIAN_POINT('',(-5.,0.6,6.1));
#138626=CARTESIAN_POINT('Origin',(-1.90787840283389,-0.6,6.1));
#138627=CARTESIAN_POINT('',(-1.90787840283389,-0.6,6.1));
#138628=CARTESIAN_POINT('Origin',(0.,0.,6.1));
#138629=CARTESIAN_POINT('Origin',(2.7,1.89736659610103,6.7));
#138630=CARTESIAN_POINT('',(2.3,1.89736659610103,5.2));
#138631=CARTESIAN_POINT('',(2.37272727272727,1.6673827662706,5.2));
#138632=CARTESIAN_POINT('Origin',(2.7,1.89736659610103,5.2));
#138633=CARTESIAN_POINT('',(2.37272727272727,1.6673827662706,6.7));
#138634=CARTESIAN_POINT('',(2.37272727272727,1.6673827662706,6.7));
#138635=CARTESIAN_POINT('',(2.3,1.89736659610103,6.7));
#138636=CARTESIAN_POINT('Origin',(2.7,1.89736659610103,6.7));
#138637=CARTESIAN_POINT('',(2.3,1.89736659610103,6.7));
#138638=CARTESIAN_POINT('Origin',(2.3,1.76635217326557,6.7));
#138639=CARTESIAN_POINT('',(2.3,3.41064510027062,6.7));
#138640=CARTESIAN_POINT('',(2.3,1.76635217326557,6.7));
#138641=CARTESIAN_POINT('',(2.3,3.41064510027062,5.2));
#138642=CARTESIAN_POINT('',(2.3,3.41064510027062,6.7));
#138643=CARTESIAN_POINT('',(2.3,1.76635217326557,5.2));
#138644=CARTESIAN_POINT('Origin',(-3.26886955020535E-16,-1.42199013476836,
6.7));
#138645=CARTESIAN_POINT('',(-2.37272727272727,1.6673827662706,6.7));
#138646=CARTESIAN_POINT('Origin',(-1.534807777198E-23,0.,6.7));
#138647=CARTESIAN_POINT('',(-2.3,1.89736659610103,6.7));
#138648=CARTESIAN_POINT('Origin',(-2.7,1.89736659610103,6.7));
#138649=CARTESIAN_POINT('',(-2.3,3.41064510027062,6.7));
#138650=CARTESIAN_POINT('',(-2.3,1.76635217326557,6.7));
#138651=CARTESIAN_POINT('',(-2.94827586206897,3.72426763822654,6.7));
#138652=CARTESIAN_POINT('Origin',(-2.7,3.41064510027062,6.7));
#138653=CARTESIAN_POINT('',(-2.8,-3.83699100858993,6.7));
#138654=CARTESIAN_POINT('Origin',(-1.534807777198E-23,0.,6.7));
#138655=CARTESIAN_POINT('',(-2.8,-5.2,6.7));
#138656=CARTESIAN_POINT('',(-2.8,-7.,6.7));
#138657=CARTESIAN_POINT('',(2.8,-5.2,6.7));
#138658=CARTESIAN_POINT('',(1.4,-5.2,6.7));
#138659=CARTESIAN_POINT('',(2.8,-3.83699100858994,6.7));
#138660=CARTESIAN_POINT('',(2.8,-7.,6.7));
#138661=CARTESIAN_POINT('',(2.94827586206897,3.72426763822654,6.7));
#138662=CARTESIAN_POINT('Origin',(-1.534807777198E-23,0.,6.7));
#138663=CARTESIAN_POINT('Origin',(2.7,3.41064510027062,6.7));
#138664=CARTESIAN_POINT('Origin',(2.7,3.41064510027062,6.7));
#138665=CARTESIAN_POINT('',(2.94827586206897,3.72426763822654,5.2));
#138666=CARTESIAN_POINT('Origin',(2.7,3.41064510027062,5.2));
#138667=CARTESIAN_POINT('',(2.94827586206897,3.72426763822654,6.7));
#138668=CARTESIAN_POINT('Origin',(-1.534807777198E-23,0.,6.7));
#138669=CARTESIAN_POINT('',(2.8,-3.83699100858994,5.2));
#138670=CARTESIAN_POINT('',(2.8,-3.83699100858994,6.7));
#138671=CARTESIAN_POINT('Origin',(-1.534807777198E-23,0.,5.2));
#138672=CARTESIAN_POINT('Origin',(-2.7,1.89736659610103,6.7));
#138673=CARTESIAN_POINT('',(-2.37272727272727,1.6673827662706,5.2));
#138674=CARTESIAN_POINT('',(-2.3,1.89736659610103,5.2));
#138675=CARTESIAN_POINT('Origin',(-2.7,1.89736659610103,5.2));
#138676=CARTESIAN_POINT('',(-2.3,1.89736659610103,6.7));
#138677=CARTESIAN_POINT('',(-2.37272727272727,1.6673827662706,6.7));
#138678=CARTESIAN_POINT('Origin',(-1.534807777198E-23,0.,6.7));
#138679=CARTESIAN_POINT('Origin',(-1.534807777198E-23,0.,5.2));
#138680=CARTESIAN_POINT('Origin',(-2.7,3.41064510027062,6.7));
#138681=CARTESIAN_POINT('',(-2.3,3.41064510027062,5.2));
#138682=CARTESIAN_POINT('',(-2.94827586206897,3.72426763822654,5.2));
#138683=CARTESIAN_POINT('Origin',(-2.7,3.41064510027062,5.2));
#138684=CARTESIAN_POINT('',(-2.94827586206897,3.72426763822654,6.7));
#138685=CARTESIAN_POINT('',(-2.3,3.41064510027062,6.7));
#138686=CARTESIAN_POINT('Origin',(-1.534807777198E-23,0.,6.7));
#138687=CARTESIAN_POINT('',(-2.8,-3.83699100858993,5.2));
#138688=CARTESIAN_POINT('Origin',(-1.534807777198E-23,0.,5.2));
#138689=CARTESIAN_POINT('',(-2.8,-3.83699100858993,6.7));
#138690=CARTESIAN_POINT('Origin',(2.8,-5.2,6.7));
#138691=CARTESIAN_POINT('',(-2.8,-5.2,8.5));
#138692=CARTESIAN_POINT('',(-2.8,-5.2,6.7));
#138693=CARTESIAN_POINT('',(2.8,-5.2,8.5));
#138694=CARTESIAN_POINT('',(-2.8,-5.2,8.5));
#138695=CARTESIAN_POINT('',(2.8,-5.2,6.7));
#138696=CARTESIAN_POINT('Origin',(-1.84889274661175E-31,-6.1,8.5));
#138697=CARTESIAN_POINT('',(-2.8,-7.,8.5));
#138698=CARTESIAN_POINT('',(-2.8,-7.,8.5));
#138699=CARTESIAN_POINT('',(2.8,-7.,8.5));
#138700=CARTESIAN_POINT('',(-2.8,-7.,8.5));
#138701=CARTESIAN_POINT('',(2.8,-7.,8.5));
#138702=CARTESIAN_POINT('Origin',(2.8,-7.,6.7));
#138703=CARTESIAN_POINT('',(-2.8,-7.,5.2));
#138704=CARTESIAN_POINT('',(-2.8,-7.,6.7));
#138705=CARTESIAN_POINT('',(2.8,-7.,5.2));
#138706=CARTESIAN_POINT('',(-2.8,-7.,5.2));
#138707=CARTESIAN_POINT('',(2.8,-7.,6.7));
#138708=CARTESIAN_POINT('Origin',(2.8,-3.83699100858994,6.7));
#138709=CARTESIAN_POINT('',(2.8,-7.,5.2));
#138710=CARTESIAN_POINT('Origin',(-2.3,4.15601973046327,6.7));
#138711=CARTESIAN_POINT('',(-2.3,1.76635217326557,5.2));
#138712=CARTESIAN_POINT('Origin',(-2.8,-7.,6.7));
#138713=CARTESIAN_POINT('',(-2.8,-7.,5.2));
#138714=CARTESIAN_POINT('Origin',(-3.26886955020535E-16,-1.42199013476836,
5.2));
#138715=CARTESIAN_POINT('',(0.,0.,0.));
#138716=CARTESIAN_POINT('Origin',(-13.5573012957478,-1.4,11.3142715795005));
#138717=CARTESIAN_POINT('',(-14.6656854249453,-1.4,10.771572875254));
#138718=CARTESIAN_POINT('',(-14.3828427124711,-1.,10.4887301627791));
#138719=CARTESIAN_POINT('Origin',(-14.3828427124711,-1.4,10.4887301627791));
#138720=CARTESIAN_POINT('',(-14.2088773290073,-1.,10.6626955462424));
#138721=CARTESIAN_POINT('',(-13.5573012957478,-1.,11.3142715795005));
#138722=CARTESIAN_POINT('',(-14.4917200414816,-1.4,10.9455382587174));
#138723=CARTESIAN_POINT('Origin',(-14.2088773290073,-1.4,10.6626955462424));
#138724=CARTESIAN_POINT('',(-13.8401440082221,-1.4,11.5971142919754));
#138725=CARTESIAN_POINT('Ctrl Pts',(-14.4917200414816,-1.4,10.9455382587174));
#138726=CARTESIAN_POINT('Ctrl Pts',(-14.1184687028433,-1.4,11.3187895973548));
#138727=CARTESIAN_POINT('Ctrl Pts',(-13.6284819468182,-1.4,11.1224579837265));
#138728=CARTESIAN_POINT('Ctrl Pts',(-13.1384951907931,-1.4,10.9261263700981));
#138729=CARTESIAN_POINT('Ctrl Pts',(-13.1262499063287,-1.4,10.398411317633));
#138730=CARTESIAN_POINT('Ctrl Pts',(-14.4917200414816,-1.,10.9455382587174));
#138731=CARTESIAN_POINT('Ctrl Pts',(-14.1184687028433,-1.,11.3187895973548));
#138732=CARTESIAN_POINT('Ctrl Pts',(-13.6284819468182,-1.,11.1224579837265));
#138733=CARTESIAN_POINT('Ctrl Pts',(-13.1384951907931,-1.,10.9261263700981));
#138734=CARTESIAN_POINT('Ctrl Pts',(-13.1262499063287,-1.,10.398411317633));
#138735=CARTESIAN_POINT('Ctrl Pts',(-14.2088773290073,-1.,10.6626955462424));
#138736=CARTESIAN_POINT('Ctrl Pts',(-14.0222516596882,-1.,10.8493212155611));
#138737=CARTESIAN_POINT('Ctrl Pts',(-13.7772582816756,-1.,10.751155408747));
#138738=CARTESIAN_POINT('Ctrl Pts',(-13.5322649036631,-1.,10.6529896019328));
#138739=CARTESIAN_POINT('Ctrl Pts',(-13.5261422614309,-1.,10.3891320757002));
#138740=CARTESIAN_POINT('',(-13.5261422614309,-1.,10.3891320757002));
#138741=CARTESIAN_POINT('',(-13.1262499063287,-1.4,10.398411317633));
#138742=CARTESIAN_POINT('Origin',(-13.5261422614309,-1.4,10.3891320757002));
#138743=CARTESIAN_POINT('Origin',(-13.926034616533,-1.4,10.3798528337675));
#138744=CARTESIAN_POINT('Origin',(-13.926034616533,-1.,10.3798528337675));
#138745=CARTESIAN_POINT('Origin',(-8.47750127826606,-1.4,10.5062825051013));
#138746=CARTESIAN_POINT('',(-9.51278842517889,-1.,5.56354232141399));
#138747=CARTESIAN_POINT('',(-9.43078548284916,-1.4,5.95504649437932));
#138748=CARTESIAN_POINT('Origin',(-9.51278842517889,-1.4,5.56354232141399));
#138749=CARTESIAN_POINT('Origin',(-8.47750127826606,-1.4,10.5062825051013));
#138750=CARTESIAN_POINT('Origin',(-8.47750127826606,-1.,10.5062825051013));
#138751=CARTESIAN_POINT('Ctrl Pts',(-9.43078548284916,-1.4,5.95504649437932));
#138752=CARTESIAN_POINT('Ctrl Pts',(-9.03827037400146,-1.4,5.87283180534908));
#138753=CARTESIAN_POINT('Ctrl Pts',(-8.86928360398281,-1.4,5.50914122625096));
#138754=CARTESIAN_POINT('Ctrl Pts',(-8.70029683396417,-1.4,5.14545064715283));
#138755=CARTESIAN_POINT('Ctrl Pts',(-8.89058649647474,-1.4,4.79243901829667));
#138756=CARTESIAN_POINT('Ctrl Pts',(-9.43078548284916,-1.,5.95504649437932));
#138757=CARTESIAN_POINT('Ctrl Pts',(-9.03827037400146,-1.,5.87283180534908));
#138758=CARTESIAN_POINT('Ctrl Pts',(-8.86928360398281,-1.,5.50914122625096));
#138759=CARTESIAN_POINT('Ctrl Pts',(-8.70029683396417,-1.,5.14545064715283));
#138760=CARTESIAN_POINT('Ctrl Pts',(-8.89058649647474,-1.,4.79243901829667));
#138761=CARTESIAN_POINT('Ctrl Pts',(-9.51278842517889,-1.,5.56354232141399));
#138762=CARTESIAN_POINT('Ctrl Pts',(-9.31653087075504,-1.,5.52243497689887));
#138763=CARTESIAN_POINT('Ctrl Pts',(-9.23203748574572,-1.,5.34058968734981));
#138764=CARTESIAN_POINT('Ctrl Pts',(-9.1475441007364,-1.,5.15874439780075));
#138765=CARTESIAN_POINT('Ctrl Pts',(-9.24268893199168,-1.,4.98223858337267));
#138766=CARTESIAN_POINT('',(-9.24268893199168,-1.,4.98223858337267));
#138767=CARTESIAN_POINT('',(-8.89058649647473,-1.4,4.79243901829667));
#138768=CARTESIAN_POINT('Origin',(-9.24268893199168,-1.4,4.98223858337267));
#138769=CARTESIAN_POINT('Origin',(-9.59479136750862,-1.4,5.17203814844866));
#138770=CARTESIAN_POINT('Origin',(-9.59479136750862,-1.,5.17203814844866));
#138771=CARTESIAN_POINT('Origin',(9.00768359641396E-11,-1.4,2.56054600265843E-10));
#138772=CARTESIAN_POINT('',(-10.4918084095504,-1.,-0.414676126038993));
#138773=CARTESIAN_POINT('',(-10.0921204701253,-1.4,-0.398878940274965));
#138774=CARTESIAN_POINT('Origin',(-10.4918084095504,-1.4,-0.414676126038993));
#138775=CARTESIAN_POINT('Origin',(9.00768359641396E-11,-1.4,2.56054600265843E-10));
#138776=CARTESIAN_POINT('Origin',(9.00768387396972E-11,-1.,2.56054689085632E-10));
#138777=CARTESIAN_POINT('Ctrl Pts',(-10.0921204701253,-1.4,-0.398878940274966));
#138778=CARTESIAN_POINT('Ctrl Pts',(-10.0765894685756,-1.4,-0.791832096572013));
#138779=CARTESIAN_POINT('Ctrl Pts',(-10.3782486193375,-1.4,-1.04413182272041));
#138780=CARTESIAN_POINT('Ctrl Pts',(-10.6799077700994,-1.4,-1.29643154886882));
#138781=CARTESIAN_POINT('Ctrl Pts',(-11.063924568312,-1.4,-1.21167015586761));
#138782=CARTESIAN_POINT('Ctrl Pts',(-10.0921204701253,-0.999999999999999,
-0.398878940274966));
#138783=CARTESIAN_POINT('Ctrl Pts',(-10.0765894685756,-0.999999999999999,
-0.791832096572014));
#138784=CARTESIAN_POINT('Ctrl Pts',(-10.3782486193375,-0.999999999999999,
-1.04413182272042));
#138785=CARTESIAN_POINT('Ctrl Pts',(-10.6799077700994,-0.999999999999999,
-1.29643154886882));
#138786=CARTESIAN_POINT('Ctrl Pts',(-11.063924568312,-0.999999999999999,
-1.21167015586761));
#138787=CARTESIAN_POINT('Ctrl Pts',(-10.4918084095504,-1.,-0.41467612603899));
#138788=CARTESIAN_POINT('Ctrl Pts',(-10.4840429087756,-1.,-0.611152704187514));
#138789=CARTESIAN_POINT('Ctrl Pts',(-10.6348724841566,-1.,-0.737302567261716));
#138790=CARTESIAN_POINT('Ctrl Pts',(-10.7857020595375,-1.,-0.863452430335917));
#138791=CARTESIAN_POINT('Ctrl Pts',(-10.9777104586438,-1.,-0.821071733835315));
#138792=CARTESIAN_POINT('',(-10.9777104586438,-1.,-0.821071733835314));
#138793=CARTESIAN_POINT('',(-11.063924568312,-1.4,-1.21167015586761));
#138794=CARTESIAN_POINT('Origin',(-10.9777104586438,-1.4,-0.821071733835314));
#138795=CARTESIAN_POINT('Origin',(-10.8914963489756,-1.4,-0.430473311803018));
#138796=CARTESIAN_POINT('Origin',(-10.8914963489756,-1.,-0.430473311803018));
#138797=CARTESIAN_POINT('Origin',(-8.47750127826606,-1.4,10.5062825051013));
#138798=CARTESIAN_POINT('',(-14.3008035257912,-1.,0.473877462741344));
#138799=CARTESIAN_POINT('',(-14.5016070515679,-1.4,0.127932461280656));
#138800=CARTESIAN_POINT('Origin',(-14.3008035257912,-1.4,0.473877462741344));
#138801=CARTESIAN_POINT('Origin',(-8.47750127826606,-1.4,10.5062825051013));
#138802=CARTESIAN_POINT('Origin',(-8.47750127826606,-1.,10.5062825051013));
#138803=CARTESIAN_POINT('Ctrl Pts',(-14.5016070515679,-1.4,0.127932461280656));
#138804=CARTESIAN_POINT('Ctrl Pts',(-14.9000000000149,-1.4,0.359179359934449));
#138805=CARTESIAN_POINT('Ctrl Pts',(-14.9000000000144,-1.4,0.819822464202032));
#138806=CARTESIAN_POINT('Ctrl Pts',(-14.5016070515679,-0.999999999999999,
0.127932461280656));
#138807=CARTESIAN_POINT('Ctrl Pts',(-14.9000000000149,-0.999999999999999,
0.359179359934449));
#138808=CARTESIAN_POINT('Ctrl Pts',(-14.9000000000144,-1.,0.819822464202032));
#138809=CARTESIAN_POINT('Ctrl Pts',(-14.3008035257912,-1.,0.473877462741344));
#138810=CARTESIAN_POINT('Ctrl Pts',(-14.5000000000146,-1.,0.589500912068241));
#138811=CARTESIAN_POINT('Ctrl Pts',(-14.5000000000144,-1.,0.819822464202032));
#138812=CARTESIAN_POINT('',(-14.5000000000144,-1.,0.819822464202785));
#138813=CARTESIAN_POINT('',(-14.9000000000144,-1.4,0.819822464203537));
#138814=CARTESIAN_POINT('Origin',(-14.5000000000144,-1.4,0.819822464202785));
#138815=CARTESIAN_POINT('Origin',(-14.1000000000144,-1.4,0.819822464202032));
#138816=CARTESIAN_POINT('Origin',(-14.1000000000144,-1.,0.819822464202032));
#138817=CARTESIAN_POINT('Origin',(-14.5000000000079,-1.4,4.28313090144278));
#138818=CARTESIAN_POINT('',(-14.4999999999968,-1.,10.2058874503049));
#138819=CARTESIAN_POINT('',(-14.8999999999968,-1.4,10.2058874503056));
#138820=CARTESIAN_POINT('Origin',(-14.4999999999968,-1.4,10.2058874503049));
#138821=CARTESIAN_POINT('',(-14.9000000000079,-1.4,4.28313090144353));
#138822=CARTESIAN_POINT('',(-14.5000000000079,-1.,4.28313090144278));
#138823=CARTESIAN_POINT('Ctrl Pts',(-14.8999999999968,-1.4,10.2058874503041));
#138824=CARTESIAN_POINT('Ctrl Pts',(-14.8999999999965,-1.4,10.537258300203));
#138825=CARTESIAN_POINT('Ctrl Pts',(-14.6656854249453,-1.4,10.771572875254));
#138826=CARTESIAN_POINT('Ctrl Pts',(-14.8999999999968,-1.,10.2058874503041));
#138827=CARTESIAN_POINT('Ctrl Pts',(-14.8999999999965,-1.,10.537258300203));
#138828=CARTESIAN_POINT('Ctrl Pts',(-14.6656854249453,-1.,10.771572875254));
#138829=CARTESIAN_POINT('Ctrl Pts',(-14.4999999999968,-1.,10.2058874503041));
#138830=CARTESIAN_POINT('Ctrl Pts',(-14.4999999999966,-1.,10.3715728752536));
#138831=CARTESIAN_POINT('Ctrl Pts',(-14.3828427124711,-1.,10.4887301627791));
#138832=CARTESIAN_POINT('Origin',(-14.0999999999968,-1.4,10.2058874503041));
#138833=CARTESIAN_POINT('Origin',(-14.0999999999968,-1.,10.2058874503041));
#138834=CARTESIAN_POINT('Origin',(-8.47750127826606,-2.6,10.5062825051013));
#138835=CARTESIAN_POINT('',(-14.5016070515679,-2.6,0.127932461280655));
#138836=CARTESIAN_POINT('',(-14.5016070515679,-2.6,0.127932461280655));
#138837=CARTESIAN_POINT('',(-15.8541129444743,-2.6,1.0413155043157));
#138838=CARTESIAN_POINT('Origin',(-8.47750127826606,-2.6,10.5062825051013));
#138839=CARTESIAN_POINT('',(-15.8541129444743,-10.1,1.0413155043157));
#138840=CARTESIAN_POINT('',(-15.8541129444743,-2.6,1.0413155043157));
#138841=CARTESIAN_POINT('',(-12.1362808769477,-10.1,-0.922336477447361));
#138842=CARTESIAN_POINT('Origin',(-8.47750127826606,-10.1,10.5062825051013));
#138843=CARTESIAN_POINT('',(-12.136280876716,-7.19501169002543,-0.922336477521518));
#138844=CARTESIAN_POINT('',(-12.1362808769477,-2.6,-0.922336477447359));
#138845=CARTESIAN_POINT('',(-8.68954964093271,-5.49648661887902,-1.49184382745125));
#138846=CARTESIAN_POINT('Ctrl Pts',(-8.68954964093266,-5.4964866188789,
-1.49184382745125));
#138847=CARTESIAN_POINT('Ctrl Pts',(-8.87481436092436,-5.43513385013829,
-1.4885695594993));
#138848=CARTESIAN_POINT('Ctrl Pts',(-9.26624052344372,-5.36455736140126,
-1.47266896725833));
#138849=CARTESIAN_POINT('Ctrl Pts',(-9.8483467388184,-5.48100398345319,
-1.41973709154106));
#138850=CARTESIAN_POINT('Ctrl Pts',(-10.8839646004455,-6.01582765661507,
-1.27510485735236));
#138851=CARTESIAN_POINT('Ctrl Pts',(-11.5886799961236,-6.67315581787308,
-1.09764645444795));
#138852=CARTESIAN_POINT('Ctrl Pts',(-12.1362808769477,-7.19501169024617,
-0.922336477447363));
#138853=CARTESIAN_POINT('',(-8.68954964093293,-2.6,-1.49184382745124));
#138854=CARTESIAN_POINT('',(-8.68954964093293,-2.6,-1.49184382745124));
#138855=CARTESIAN_POINT('',(-11.063924568312,-2.6,-1.21167015586761));
#138856=CARTESIAN_POINT('Origin',(-8.47750127826606,-2.6,10.5062825051013));
#138857=CARTESIAN_POINT('',(-11.063924568312,-2.6,-1.21167015586761));
#138858=CARTESIAN_POINT('Origin',(-14.1000000000144,-2.6,0.819822464202031));
#138859=CARTESIAN_POINT('',(-14.9000000000144,-2.6,0.819822464203537));
#138860=CARTESIAN_POINT('',(-14.9000000000144,-2.6,0.819822464203537));
#138861=CARTESIAN_POINT('Origin',(-14.1000000000144,-2.6,0.819822464202031));
#138862=CARTESIAN_POINT('Origin',(-14.9000000000153,-1.6,0.369640547868617));
#138863=CARTESIAN_POINT('',(-14.8999999999968,-2.6,10.2058874503056));
#138864=CARTESIAN_POINT('',(-14.8999999999968,-1.6,10.2058874503056));
#138865=CARTESIAN_POINT('',(-14.9000000000324,-2.6,-8.71274169982173));
#138866=CARTESIAN_POINT('Origin',(-14.0999999999968,-1.6,10.2058874503041));
#138867=CARTESIAN_POINT('',(-14.6656854249453,-2.6,10.771572875254));
#138868=CARTESIAN_POINT('',(-14.6656854249453,-1.6,10.771572875254));
#138869=CARTESIAN_POINT('Origin',(-14.0999999999968,-2.6,10.2058874503041));
#138870=CARTESIAN_POINT('Origin',(-14.8999999999961,-1.6,10.5372583002038));
#138871=CARTESIAN_POINT('',(-14.4917200414816,-2.6,10.9455382587174));
#138872=CARTESIAN_POINT('',(-14.4917200414816,-2.6,10.9455382587174));
#138873=CARTESIAN_POINT('',(-14.8999999999961,-2.6,10.5372583002038));
#138874=CARTESIAN_POINT('Origin',(-8.31993898771739,-1.,8.19662125500606));
#138875=CARTESIAN_POINT('Origin',(-11.9915184469055,-1.4,-6.13955455136528));
#138876=CARTESIAN_POINT('',(-11.5237848152765,-1.4,-6.09584299941717));
#138877=CARTESIAN_POINT('',(-11.8824156877396,-0.999999999999998,-5.91868799012766));
#138878=CARTESIAN_POINT('Origin',(-11.8824156877396,-1.4,-5.91868799012766));
#138879=CARTESIAN_POINT('',(-14.7997235069111,-0.999999999999996,-11.8244574777011));
#138880=CARTESIAN_POINT('',(-11.9915184469055,-0.999999999999998,-6.13955455136528));
#138881=CARTESIAN_POINT('',(-14.441092634448,-1.4,-12.0016124869907));
#138882=CARTESIAN_POINT('Origin',(-14.7997235069111,-1.4,-11.8244574777011));
#138883=CARTESIAN_POINT('',(-11.6328875744424,-1.4,-6.3167095606548));
#138884=CARTESIAN_POINT('Ctrl Pts',(-14.441092634448,-1.4,-12.0016124869907));
#138885=CARTESIAN_POINT('Ctrl Pts',(-14.6327150753576,-1.4,-12.3895310868797));
#138886=CARTESIAN_POINT('Ctrl Pts',(-15.0612959521201,-1.4,-12.3302147141527));
#138887=CARTESIAN_POINT('Ctrl Pts',(-14.441092634448,-0.999999999999997,
-12.0016124869907));
#138888=CARTESIAN_POINT('Ctrl Pts',(-14.6327150753576,-0.999999999999997,
-12.3895310868797));
#138889=CARTESIAN_POINT('Ctrl Pts',(-15.0612959521201,-0.999999999999997,
-12.3302147141527));
#138890=CARTESIAN_POINT('Ctrl Pts',(-14.7997235069111,-0.999999999999997,
-11.8244574777011));
#138891=CARTESIAN_POINT('Ctrl Pts',(-14.8635976538809,-0.999999999999997,
-11.9537636776641));
#138892=CARTESIAN_POINT('Ctrl Pts',(-15.0064579461351,-0.999999999999997,
-11.9339915534218));
#138893=CARTESIAN_POINT('',(-15.0064579461351,-0.999999999999996,-11.9339915534218));
#138894=CARTESIAN_POINT('',(-15.0612959521201,-1.4,-12.3302147141527));
#138895=CARTESIAN_POINT('Origin',(-15.0064579461351,-1.4,-11.9339915534218));
#138896=CARTESIAN_POINT('Origin',(-14.9790389431426,-1.4,-11.7358799730564));
#138897=CARTESIAN_POINT('Origin',(-14.9790389431426,-0.999999999999996,
-11.7358799730564));
#138898=CARTESIAN_POINT('Origin',(-15.5,-1.4,-15.5));
#138899=CARTESIAN_POINT('',(-16.5800000000255,-0.999999999999996,-12.065818874907));
#138900=CARTESIAN_POINT('',(-16.4600000000227,-1.4,-12.4473945554729));
#138901=CARTESIAN_POINT('Origin',(-16.5800000000255,-1.4,-12.065818874907));
#138902=CARTESIAN_POINT('Origin',(-15.5,-1.4,-15.5));
#138903=CARTESIAN_POINT('Origin',(-15.5,-0.999999999999996,-15.5));
#138904=CARTESIAN_POINT('Ctrl Pts',(-16.4600000000227,-1.4,-12.4473945554729));
#138905=CARTESIAN_POINT('Ctrl Pts',(-16.8465727653177,-1.4,-12.5689660659206));
#138906=CARTESIAN_POINT('Ctrl Pts',(-17.1732863826715,-1.4,-12.3292238142085));
#138907=CARTESIAN_POINT('Ctrl Pts',(-17.5000000000253,-1.4,-12.0894815624965));
#138908=CARTESIAN_POINT('Ctrl Pts',(-17.5000000000283,-1.4,-11.6842431943471));
#138909=CARTESIAN_POINT('Ctrl Pts',(-16.4600000000227,-0.999999999999995,
-12.4473945554729));
#138910=CARTESIAN_POINT('Ctrl Pts',(-16.8465727653177,-0.999999999999996,
-12.5689660659206));
#138911=CARTESIAN_POINT('Ctrl Pts',(-17.1732863826715,-0.999999999999996,
-12.3292238142085));
#138912=CARTESIAN_POINT('Ctrl Pts',(-17.5000000000253,-0.999999999999996,
-12.0894815624965));
#138913=CARTESIAN_POINT('Ctrl Pts',(-17.5000000000283,-0.999999999999996,
-11.6842431943471));
#138914=CARTESIAN_POINT('Ctrl Pts',(-16.5800000000255,-0.999999999999997,
-12.065818874907));
#138915=CARTESIAN_POINT('Ctrl Pts',(-16.773286382673,-0.999999999999997,
-12.1266046301309));
#138916=CARTESIAN_POINT('Ctrl Pts',(-16.9366431913499,-0.999999999999997,
-12.0067335042748));
#138917=CARTESIAN_POINT('Ctrl Pts',(-17.1000000000268,-0.999999999999997,
-11.8868623784188));
#138918=CARTESIAN_POINT('Ctrl Pts',(-17.1000000000283,-0.999999999999997,
-11.6842431943441));
#138919=CARTESIAN_POINT('',(-17.1000000000283,-0.999999999999996,-11.6842431943441));
#138920=CARTESIAN_POINT('',(-17.5000000000283,-1.4,-11.6842431943471));
#138921=CARTESIAN_POINT('Origin',(-17.1000000000283,-1.4,-11.6842431943441));
#138922=CARTESIAN_POINT('Origin',(-16.7000000000283,-1.4,-11.6842431943411));
#138923=CARTESIAN_POINT('Origin',(-16.7000000000283,-0.999999999999996,
-11.6842431943411));
#138924=CARTESIAN_POINT('Origin',(-17.1000000000372,-1.4,-10.4863375378306));
#138925=CARTESIAN_POINT('',(-17.1000000000286,-0.999999999999996,-11.6441125497194));
#138926=CARTESIAN_POINT('',(-17.5000000000286,-1.4,-11.6441125497224));
#138927=CARTESIAN_POINT('Origin',(-17.1000000000286,-1.4,-11.6441125497194));
#138928=CARTESIAN_POINT('',(-17.5000000000372,-1.4,-10.4863375378336));
#138929=CARTESIAN_POINT('',(-17.1000000000372,-0.999999999999997,-10.4863375378306));
#138930=CARTESIAN_POINT('Ctrl Pts',(-17.5000000000286,-1.4,-11.6441125497165));
#138931=CARTESIAN_POINT('Ctrl Pts',(-17.5000000000299,-1.4,-11.3127416998175));
#138932=CARTESIAN_POINT('Ctrl Pts',(-17.2656854249779,-1.4,-11.0784271247672));
#138933=CARTESIAN_POINT('Ctrl Pts',(-17.5000000000286,-0.999999999999995,
-11.6441125497165));
#138934=CARTESIAN_POINT('Ctrl Pts',(-17.5000000000299,-0.999999999999995,
-11.3127416998175));
#138935=CARTESIAN_POINT('Ctrl Pts',(-17.2656854249779,-0.999999999999995,
-11.0784271247672));
#138936=CARTESIAN_POINT('Ctrl Pts',(-17.1000000000286,-0.999999999999996,
-11.6441125497165));
#138937=CARTESIAN_POINT('Ctrl Pts',(-17.1000000000293,-0.999999999999996,
-11.478427124767));
#138938=CARTESIAN_POINT('Ctrl Pts',(-16.9828427125033,-0.999999999999996,
-11.3612698372419));
#138939=CARTESIAN_POINT('',(-16.9828427125033,-0.999999999999996,-11.3612698372419));
#138940=CARTESIAN_POINT('',(-17.2656854249779,-1.4,-11.0784271247672));
#138941=CARTESIAN_POINT('Origin',(-16.9828427125033,-1.4,-11.3612698372419));
#138942=CARTESIAN_POINT('Origin',(-16.7000000000286,-1.4,-11.6441125497165));
#138943=CARTESIAN_POINT('Origin',(-16.7000000000286,-0.999999999999996,
-11.6441125497165));
#138944=CARTESIAN_POINT('Origin',(-15.2217176089063,-1.4,-9.6001447336449));
#138945=CARTESIAN_POINT('',(-14.8514718626079,-0.999999999999997,-9.22989898734649));
#138946=CARTESIAN_POINT('',(-15.1343145750825,-1.4,-8.94705627487187));
#138947=CARTESIAN_POINT('Origin',(-14.8514718626079,-1.4,-9.22989898734649));
#138948=CARTESIAN_POINT('',(-15.5045603213809,-1.4,-9.31730202117028));
#138949=CARTESIAN_POINT('',(-15.2217176089063,-0.999999999999997,-9.6001447336449));
#138950=CARTESIAN_POINT('Origin',(-15.7000000000318,-1.4,-8.38137084992263));
#138951=CARTESIAN_POINT('',(-14.5000000000318,-0.999999999999997,-8.38137084992489));
#138952=CARTESIAN_POINT('',(-14.9000000000318,-1.4,-8.38137084992414));
#138953=CARTESIAN_POINT('Origin',(-14.5000000000318,-1.4,-8.38137084992489));
#138954=CARTESIAN_POINT('Origin',(-15.7000000000318,-1.4,-8.38137084992263));
#138955=CARTESIAN_POINT('Origin',(-15.7000000000318,-0.999999999999997,
-8.38137084992263));
#138956=CARTESIAN_POINT('Origin',(-14.5000000000293,-1.4,-7.09270838774364));
#138957=CARTESIAN_POINT('',(-14.5000000000203,-0.999999999999999,-2.31508669338342));
#138958=CARTESIAN_POINT('',(-14.9000000000203,-1.4,-2.31508669338267));
#138959=CARTESIAN_POINT('Origin',(-14.5000000000203,-1.4,-2.31508669338342));
#138960=CARTESIAN_POINT('',(-14.9000000000293,-1.4,-7.09270838774289));
#138961=CARTESIAN_POINT('',(-14.5000000000293,-0.999999999999998,-7.09270838774364));
#138962=CARTESIAN_POINT('Ctrl Pts',(-14.9000000000203,-1.4,-2.31508669338417));
#138963=CARTESIAN_POINT('Ctrl Pts',(-14.9000000000199,-1.4,-1.88217329548528));
#138964=CARTESIAN_POINT('Ctrl Pts',(-14.5375908403063,-1.4,-1.64537462353789));
#138965=CARTESIAN_POINT('Ctrl Pts',(-14.1751816805932,-1.4,-1.40857595159125));
#138966=CARTESIAN_POINT('Ctrl Pts',(-13.7787143587772,-1.4,-1.58243702489929));
#138967=CARTESIAN_POINT('Ctrl Pts',(-14.9000000000203,-0.999999999999991,
-2.31508669338417));
#138968=CARTESIAN_POINT('Ctrl Pts',(-14.9000000000199,-0.999999999999992,
-1.88217329548528));
#138969=CARTESIAN_POINT('Ctrl Pts',(-14.5375908403063,-0.999999999999992,
-1.64537462353789));
#138970=CARTESIAN_POINT('Ctrl Pts',(-14.1751816805932,-0.999999999999992,
-1.40857595159125));
#138971=CARTESIAN_POINT('Ctrl Pts',(-13.7787143587772,-0.999999999999992,
-1.58243702489929));
#138972=CARTESIAN_POINT('Ctrl Pts',(-14.5000000000203,-0.999999999999998,
-2.31508669338417));
#138973=CARTESIAN_POINT('Ctrl Pts',(-14.5000000000201,-0.999999999999998,
-2.09862999443473));
#138974=CARTESIAN_POINT('Ctrl Pts',(-14.3187954201633,-0.999999999999998,
-1.98023065846104));
#138975=CARTESIAN_POINT('Ctrl Pts',(-14.1375908403068,-0.999999999999998,
-1.86183132248772));
#138976=CARTESIAN_POINT('Ctrl Pts',(-13.9393571793988,-0.999999999999998,
-1.94876185914174));
#138977=CARTESIAN_POINT('',(-13.9393571793988,-0.999999999999999,-1.94876185914173));
#138978=CARTESIAN_POINT('',(-13.7787143587772,-1.4,-1.58243702489929));
#138979=CARTESIAN_POINT('Origin',(-13.9393571793988,-1.4,-1.94876185914173));
#138980=CARTESIAN_POINT('Origin',(-14.1000000000203,-1.4,-2.31508669338417));
#138981=CARTESIAN_POINT('Origin',(-14.1000000000203,-0.999999999999999,
-2.31508669338417));
#138982=CARTESIAN_POINT('Origin',(-8.47750127826606,-1.4,10.5062825051013));
#138983=CARTESIAN_POINT('',(-12.9945355807443,-0.999999999999999,-2.32167138904082));
#138984=CARTESIAN_POINT('',(-12.8616816306714,-1.4,-1.9443786274484));
#138985=CARTESIAN_POINT('Origin',(-12.9945355807443,-1.4,-2.32167138904082));
#138986=CARTESIAN_POINT('Origin',(-8.47750127826606,-1.4,10.5062825051013));
#138987=CARTESIAN_POINT('Origin',(-8.47750127826606,-1.,10.5062825051013));
#138988=CARTESIAN_POINT('Ctrl Pts',(-12.8616816306714,-1.4,-1.9443786274484));
#138989=CARTESIAN_POINT('Ctrl Pts',(-12.3961845071422,-1.4,-2.10829147684258));
#138990=CARTESIAN_POINT('Ctrl Pts',(-12.4672085468558,-1.4,-2.59666692666902));
#138991=CARTESIAN_POINT('Ctrl Pts',(-12.8616816306714,-0.999999999999995,
-1.9443786274484));
#138992=CARTESIAN_POINT('Ctrl Pts',(-12.3961845071422,-0.999999999999995,
-2.10829147684258));
#138993=CARTESIAN_POINT('Ctrl Pts',(-12.4672085468558,-0.999999999999994,
-2.59666692666902));
#138994=CARTESIAN_POINT('Ctrl Pts',(-12.9945355807443,-0.999999999999998,
-2.32167138904082));
#138995=CARTESIAN_POINT('Ctrl Pts',(-12.8393698729012,-0.999999999999998,
-2.37630900550554));
#138996=CARTESIAN_POINT('Ctrl Pts',(-12.8630445528057,-0.999999999999998,
-2.53910082211435));
#138997=CARTESIAN_POINT('',(-12.8630445528057,-0.999999999999998,-2.53910082211435));
#138998=CARTESIAN_POINT('',(-12.4672085468558,-1.4,-2.59666692666902));
#138999=CARTESIAN_POINT('Origin',(-12.8630445528057,-1.4,-2.53910082211435));
#139000=CARTESIAN_POINT('Origin',(-13.0609625557807,-1.4,-2.51031776983702));
#139001=CARTESIAN_POINT('Origin',(-13.0609625557807,-0.999999999999998,
-2.51031776983702));
#139002=CARTESIAN_POINT('Origin',(-9.35,-1.4,-3.05000000003699));
#139003=CARTESIAN_POINT('',(-11.9482823515746,-0.999999999999998,-5.46897267898486));
#139004=CARTESIAN_POINT('',(-11.6555181429464,-1.4,-5.19641237713157));
#139005=CARTESIAN_POINT('Origin',(-11.9482823515746,-1.4,-5.46897267898486));
#139006=CARTESIAN_POINT('',(-12.5,-1.4,-3.05000000003699));
#139007=CARTESIAN_POINT('Origin',(-9.35,-1.4,-3.05000000003699));
#139008=CARTESIAN_POINT('Origin',(-9.35,-1.4,-3.05000000003699));
#139009=CARTESIAN_POINT('Origin',(-9.35,-0.999999999999998,-3.05000000003699));
#139010=CARTESIAN_POINT('Ctrl Pts',(-11.6555181429464,-1.4,-5.19641237713157));
#139011=CARTESIAN_POINT('Ctrl Pts',(-11.2791734498063,-1.4,-5.60065413761314));
#139012=CARTESIAN_POINT('Ctrl Pts',(-11.5237848152765,-1.4,-6.09584299941717));
#139013=CARTESIAN_POINT('Ctrl Pts',(-11.6555181429464,-0.999999999999997,
-5.19641237713157));
#139014=CARTESIAN_POINT('Ctrl Pts',(-11.2791734498063,-0.999999999999996,
-5.60065413761314));
#139015=CARTESIAN_POINT('Ctrl Pts',(-11.5237848152765,-0.999999999999996,
-6.09584299941717));
#139016=CARTESIAN_POINT('Ctrl Pts',(-11.9482823515746,-0.999999999999998,
-5.46897267898485));
#139017=CARTESIAN_POINT('Ctrl Pts',(-11.7601100050045,-0.999999999999998,
-5.67109355922564));
#139018=CARTESIAN_POINT('Ctrl Pts',(-11.8824156877396,-0.999999999999998,
-5.91868799012765));
#139019=CARTESIAN_POINT('Origin',(-12.2410465602027,-1.4,-5.74153298083814));
#139020=CARTESIAN_POINT('Origin',(-12.2410465602027,-0.999999999999998,
-5.74153298083814));
#139021=CARTESIAN_POINT('Origin',(-14.9000000000324,-1.6,-8.71274169982173));
#139022=CARTESIAN_POINT('',(-14.9000000000203,-10.1,-2.31508669338267));
#139023=CARTESIAN_POINT('',(-14.9000000000203,-10.3,-2.31508669338267));
#139024=CARTESIAN_POINT('',(-14.9000000000318,-10.1,-8.38137084992414));
#139025=CARTESIAN_POINT('',(-14.9000000000291,-10.1,-6.97072868003485));
#139026=CARTESIAN_POINT('',(-14.9000000000318,-1.6,-8.38137084992414));
#139027=CARTESIAN_POINT('Origin',(-14.1000000000203,-10.3,-2.31508669338417));
#139028=CARTESIAN_POINT('',(-13.7787143587772,-10.1,-1.58243702489929));
#139029=CARTESIAN_POINT('',(-13.7787143587772,-10.3,-1.58243702489929));
#139030=CARTESIAN_POINT('Origin',(-14.1000000000203,-10.1,-2.31508669338417));
#139031=CARTESIAN_POINT('Origin',(-8.47750127826606,-10.3,10.5062825051013));
#139032=CARTESIAN_POINT('',(-12.8616816306714,-10.1,-1.9443786274484));
#139033=CARTESIAN_POINT('',(-12.8616816306714,-10.3,-1.9443786274484));
#139034=CARTESIAN_POINT('Origin',(-8.47750127826606,-10.1,10.5062825051013));
#139035=CARTESIAN_POINT('Origin',(-13.0609625557807,-10.3,-2.51031776983702));
#139036=CARTESIAN_POINT('',(-12.4672085468558,-10.1,-2.59666692666902));
#139037=CARTESIAN_POINT('',(-12.4672085468558,-10.3,-2.59666692666902));
#139038=CARTESIAN_POINT('Origin',(-13.0609625557807,-10.1,-2.51031776983702));
#139039=CARTESIAN_POINT('Origin',(-9.35,-10.3,-3.05000000003699));
#139040=CARTESIAN_POINT('',(-12.5,-10.4,-3.05000000003699));
#139041=CARTESIAN_POINT('Origin',(-9.35,-10.4,-3.05000000003699));
#139042=CARTESIAN_POINT('',(-12.5,-10.3,-3.05000000003699));
#139043=CARTESIAN_POINT('',(-11.6555181429464,-10.1,-5.19641237713158));
#139044=CARTESIAN_POINT('',(-11.6555181429464,-10.3,-5.19641237713158));
#139045=CARTESIAN_POINT('',(-9.76798833941153,-10.1,-6.17214441503704));
#139046=CARTESIAN_POINT('Origin',(-9.35,-10.1,-3.05000000003699));
#139047=CARTESIAN_POINT('',(-9.76798833941153,-1.4,-6.17214441503704));
#139048=CARTESIAN_POINT('',(-9.76798833941153,-10.3,-6.17214441503704));
#139049=CARTESIAN_POINT('',(-8.1843866565298,-1.4,-5.97640488205934));
#139050=CARTESIAN_POINT('Origin',(-9.35,-1.4,-3.05000000003699));
#139051=CARTESIAN_POINT('',(-8.1843866565298,-10.1,-5.97640488205934));
#139052=CARTESIAN_POINT('',(-8.1843866565298,-10.3,-5.97640488205934));
#139053=CARTESIAN_POINT('',(-6.64846378001877,-10.1,-4.66993890386316));
#139054=CARTESIAN_POINT('Origin',(-9.35,-10.1,-3.05000000003699));
#139055=CARTESIAN_POINT('',(-6.64846378001877,-7.05,-4.66993890386316));
#139056=CARTESIAN_POINT('',(-6.64846378001877,-10.3,-4.66993890386316));
#139057=CARTESIAN_POINT('',(-11.5368071934914,-7.05,-0.782760643794657));
#139058=CARTESIAN_POINT('Origin',(-9.35,-7.05,-3.05000000003699));
#139059=CARTESIAN_POINT('',(-11.5368071934914,-10.1,-0.782760643794658));
#139060=CARTESIAN_POINT('',(-11.5368071934914,-2.6,-0.782760643794656));
#139061=CARTESIAN_POINT('Origin',(-9.35,-10.1,-3.05000000003699));
#139062=CARTESIAN_POINT('Origin',(-12.2410465602027,-10.3,-5.74153298083814));
#139063=CARTESIAN_POINT('',(-11.5237848152765,-10.1,-6.09584299941718));
#139064=CARTESIAN_POINT('',(-11.5237848152765,-10.3,-6.09584299941718));
#139065=CARTESIAN_POINT('Origin',(-12.2410465602027,-10.1,-5.74153298083814));
#139066=CARTESIAN_POINT('Origin',(-11.2373003829631,-10.3,-5.51588670961375));
#139067=CARTESIAN_POINT('',(-14.441092634448,-10.1,-12.0016124869907));
#139068=CARTESIAN_POINT('',(-14.441092634448,-10.3,-12.0016124869907));
#139069=CARTESIAN_POINT('',(-12.0443465189275,-10.1,-7.14966303363441));
#139070=CARTESIAN_POINT('Origin',(-15.3583079095877,-0.999999999999998,
-5.47267507566318));
#139071=CARTESIAN_POINT('Origin',(-5.6920614055489E-17,-1.4,9.32936375408611E-17));
#139072=CARTESIAN_POINT('',(-7.49853797666954,-1.4,-6.15320473424437));
#139073=CARTESIAN_POINT('',(-7.8077560370881,-0.999999999999998,-6.40694513526671));
#139074=CARTESIAN_POINT('Origin',(-7.8077560370881,-1.4,-6.40694513526671));
#139075=CARTESIAN_POINT('',(-1.36872658490553,-0.999999999999997,-10.0068270614005));
#139076=CARTESIAN_POINT('Origin',(-5.6920614055489E-17,-0.999999999999999,
1.82111479510874E-16));
#139077=CARTESIAN_POINT('',(-1.3145195915239,-1.4,-9.61051707935543));
#139078=CARTESIAN_POINT('Origin',(-1.36872658490553,-1.4,-10.0068270614005));
#139079=CARTESIAN_POINT('Origin',(-5.6920614055489E-17,-1.4,9.32936375408611E-17));
#139080=CARTESIAN_POINT('Ctrl Pts',(-1.3145195915239,-1.4,-9.61051707935543));
#139081=CARTESIAN_POINT('Ctrl Pts',(-0.796043967664363,-1.4,-9.68143380107428));
#139082=CARTESIAN_POINT('Ctrl Pts',(-0.795830131689239,-1.4,-10.2047368760032));
#139083=CARTESIAN_POINT('Ctrl Pts',(-1.3145195915239,-0.999999999999992,
-9.61051707935543));
#139084=CARTESIAN_POINT('Ctrl Pts',(-0.796043967664363,-0.999999999999992,
-9.68143380107428));
#139085=CARTESIAN_POINT('Ctrl Pts',(-0.795830131689239,-0.999999999999992,
-10.2047368760032));
#139086=CARTESIAN_POINT('Ctrl Pts',(-1.36872658490553,-0.999999999999997,
-10.0068270614005));
#139087=CARTESIAN_POINT('Ctrl Pts',(-1.19590137695235,-0.999999999999997,
-10.0304659686401));
#139088=CARTESIAN_POINT('Ctrl Pts',(-1.19583009829398,-0.999999999999997,
-10.2049003269497));
#139089=CARTESIAN_POINT('',(-1.19583009829397,-0.999999999999997,-10.2049003269497));
#139090=CARTESIAN_POINT('',(-0.795830131689239,-1.4,-10.2047368760032));
#139091=CARTESIAN_POINT('Origin',(-1.19583009829397,-1.4,-10.2049003269497));
#139092=CARTESIAN_POINT('Origin',(-1.39583008159634,-1.4,-10.204982052423));
#139093=CARTESIAN_POINT('Origin',(-1.39583008159634,-0.999999999999997,
-10.204982052423));
#139094=CARTESIAN_POINT('Origin',(-1.19695920643336,-1.4,-7.44172747482704));
#139095=CARTESIAN_POINT('',(-1.19309433051448,-0.999999999999995,-16.8999182745535));
#139096=CARTESIAN_POINT('',(-0.79309436390975,-1.39999999999999,-16.899754823607));
#139097=CARTESIAN_POINT('Origin',(-1.19309433051448,-1.39999999999999,-16.8999182745535));
#139098=CARTESIAN_POINT('',(-0.796959239828628,-1.4,-7.44156402388053));
#139099=CARTESIAN_POINT('',(-1.19695920643336,-0.999999999999997,-7.44172747482704));
#139100=CARTESIAN_POINT('Ctrl Pts',(-0.793094363909749,-1.39999999999999,
-16.899754823607));
#139101=CARTESIAN_POINT('Ctrl Pts',(-0.792992779166526,-1.39999999999999,
-17.1483547538275));
#139102=CARTESIAN_POINT('Ctrl Pts',(-0.968743571003919,-1.39999999999999,
-17.3241773769272));
#139103=CARTESIAN_POINT('Ctrl Pts',(-1.14449436284124,-1.39999999999999,
-17.5000000000268));
#139104=CARTESIAN_POINT('Ctrl Pts',(-1.39309431381685,-1.39999999999999,
-17.5000000000267));
#139105=CARTESIAN_POINT('Ctrl Pts',(-0.793094363909749,-0.999999999999954,
-16.899754823607));
#139106=CARTESIAN_POINT('Ctrl Pts',(-0.792992779166526,-0.999999999999954,
-17.1483547538275));
#139107=CARTESIAN_POINT('Ctrl Pts',(-0.968743571003919,-0.999999999999954,
-17.3241773769272));
#139108=CARTESIAN_POINT('Ctrl Pts',(-1.14449436284124,-0.999999999999954,
-17.5000000000268));
#139109=CARTESIAN_POINT('Ctrl Pts',(-1.39309431381685,-0.999999999999954,
-17.5000000000267));
#139110=CARTESIAN_POINT('Ctrl Pts',(-1.19309433051452,-0.999999999999994,
-16.8999182745535));
#139111=CARTESIAN_POINT('Ctrl Pts',(-1.19306046893345,-0.999999999999994,
-16.9827849179603));
#139112=CARTESIAN_POINT('Ctrl Pts',(-1.25164406621257,-0.999999999999994,
-17.0413924589935));
#139113=CARTESIAN_POINT('Ctrl Pts',(-1.31022766349166,-0.999999999999994,
-17.1000000000267));
#139114=CARTESIAN_POINT('Ctrl Pts',(-1.39309431381685,-0.999999999999994,
-17.1000000000267));
#139115=CARTESIAN_POINT('',(-1.39309431381659,-0.999999999999995,-17.1000000000267));
#139116=CARTESIAN_POINT('',(-1.39309431381607,-1.39999999999999,-17.5000000000267));
#139117=CARTESIAN_POINT('Origin',(-1.39309431381659,-1.39999999999999,-17.1000000000267));
#139118=CARTESIAN_POINT('Origin',(-1.39309431381685,-1.39999999999999,-16.9000000000267));
#139119=CARTESIAN_POINT('Origin',(-1.39309431381685,-0.999999999999995,
-16.9000000000267));
#139120=CARTESIAN_POINT('Origin',(-8.07557849842838,-1.4,-17.1000000000355));
#139121=CARTESIAN_POINT('',(-11.9672956534847,-0.999999999999995,-17.1000000000405));
#139122=CARTESIAN_POINT('',(-11.9672956534841,-1.39999999999999,-17.5000000000405));
#139123=CARTESIAN_POINT('Origin',(-11.9672956534847,-1.4,-17.1000000000405));
#139124=CARTESIAN_POINT('',(-8.07557849842786,-1.4,-17.5000000000355));
#139125=CARTESIAN_POINT('',(-8.07557849842838,-0.999999999999995,-17.1000000000355));
#139126=CARTESIAN_POINT('Ctrl Pts',(-11.9672956534849,-1.4,-17.5000000000405));
#139127=CARTESIAN_POINT('Ctrl Pts',(-12.2850405509874,-1.4,-17.5000000000406));
#139128=CARTESIAN_POINT('Ctrl Pts',(-12.4635977686079,-1.4,-17.2371708922072));
#139129=CARTESIAN_POINT('Ctrl Pts',(-12.6421549862285,-1.4,-16.9743417843737));
#139130=CARTESIAN_POINT('Ctrl Pts',(-12.5250910766189,-1.4,-16.6789473684552));
#139131=CARTESIAN_POINT('Ctrl Pts',(-11.9672956534849,-0.999999999999995,
-17.5000000000405));
#139132=CARTESIAN_POINT('Ctrl Pts',(-12.2850405509874,-0.999999999999995,
-17.5000000000406));
#139133=CARTESIAN_POINT('Ctrl Pts',(-12.4635977686079,-0.999999999999995,
-17.2371708922072));
#139134=CARTESIAN_POINT('Ctrl Pts',(-12.6421549862285,-0.999999999999995,
-16.9743417843737));
#139135=CARTESIAN_POINT('Ctrl Pts',(-12.5250910766189,-0.999999999999995,
-16.6789473684552));
#139136=CARTESIAN_POINT('Ctrl Pts',(-11.9672956534849,-0.999999999999996,
-17.1000000000405));
#139137=CARTESIAN_POINT('Ctrl Pts',(-12.0732106193191,-0.999999999999996,
-17.1000000000406));
#139138=CARTESIAN_POINT('Ctrl Pts',(-12.1327296918593,-0.999999999999996,
-17.0123902974294));
#139139=CARTESIAN_POINT('Ctrl Pts',(-12.1922487643995,-0.999999999999996,
-16.9247805948183));
#139140=CARTESIAN_POINT('Ctrl Pts',(-12.1532274611963,-0.999999999999996,
-16.8263157895121));
#139141=CARTESIAN_POINT('',(-12.1532274611963,-0.999999999999995,-16.8263157895121));
#139142=CARTESIAN_POINT('',(-12.5250910766189,-1.4,-16.6789473684552));
#139143=CARTESIAN_POINT('Origin',(-12.1532274611963,-1.4,-16.8263157895121));
#139144=CARTESIAN_POINT('Origin',(-11.9672956534849,-1.4,-16.9000000000405));
#139145=CARTESIAN_POINT('Origin',(-11.9672956534849,-0.999999999999995,
-16.9000000000405));
#139146=CARTESIAN_POINT('Origin',(-15.5,-1.4,-15.5));
#139147=CARTESIAN_POINT('',(-12.9679245658186,-0.999999999999996,-12.9409779220149));
#139148=CARTESIAN_POINT('',(-13.2492662807277,-1.4,-13.2253137084577));
#139149=CARTESIAN_POINT('Origin',(-12.9679245658186,-1.4,-12.9409779220149));
#139150=CARTESIAN_POINT('Origin',(-15.5,-1.4,-15.5));
#139151=CARTESIAN_POINT('Origin',(-15.5,-0.999999999999996,-15.5));
#139152=CARTESIAN_POINT('Ctrl Pts',(-13.2492662807277,-1.4,-13.2253137084577));
#139153=CARTESIAN_POINT('Ctrl Pts',(-13.5568224579683,-1.4,-12.9209961147482));
#139154=CARTESIAN_POINT('Ctrl Pts',(-13.3652000170587,-1.4,-12.5330775148592));
#139155=CARTESIAN_POINT('Ctrl Pts',(-13.2492662807277,-0.999999999999995,
-13.2253137084577));
#139156=CARTESIAN_POINT('Ctrl Pts',(-13.5568224579683,-0.999999999999995,
-12.9209961147482));
#139157=CARTESIAN_POINT('Ctrl Pts',(-13.3652000170587,-0.999999999999995,
-12.5330775148592));
#139158=CARTESIAN_POINT('Ctrl Pts',(-12.9679245658186,-0.999999999999997,
-12.9409779220149));
#139159=CARTESIAN_POINT('Ctrl Pts',(-13.0704432915655,-0.999999999999997,
-12.8395387241117));
#139160=CARTESIAN_POINT('Ctrl Pts',(-13.0065691445957,-0.999999999999997,
-12.7102325241487));
#139161=CARTESIAN_POINT('',(-13.0065691445957,-0.999999999999996,-12.7102325241487));
#139162=CARTESIAN_POINT('',(-13.3652000170587,-1.4,-12.5330775148592));
#139163=CARTESIAN_POINT('Origin',(-13.0065691445957,-1.4,-12.7102325241487));
#139164=CARTESIAN_POINT('Origin',(-12.8272537083641,-1.4,-12.7988100287935));
#139165=CARTESIAN_POINT('Origin',(-12.8272537083641,-0.999999999999996,
-12.7988100287935));
#139166=CARTESIAN_POINT('Origin',(-11.9125686467803,-1.4,-10.4955485895535));
#139167=CARTESIAN_POINT('',(-10.0269206021976,-0.999999999999998,-6.678261084678));
#139168=CARTESIAN_POINT('',(-10.3855514746607,-1.4,-6.50110607538848));
#139169=CARTESIAN_POINT('Origin',(-10.0269206021976,-1.4,-6.678261084678));
#139170=CARTESIAN_POINT('',(-12.2711995192434,-1.4,-10.318393580264));
#139171=CARTESIAN_POINT('',(-11.9125686467803,-0.999999999999997,-10.4955485895535));
#139172=CARTESIAN_POINT('Ctrl Pts',(-10.3855514746607,-1.4,-6.50110607538848));
#139173=CARTESIAN_POINT('Ctrl Pts',(-10.1948244706177,-1.4,-6.11500018915609));
#139174=CARTESIAN_POINT('Ctrl Pts',(-9.76798833941153,-1.4,-6.17214441503704));
#139175=CARTESIAN_POINT('Ctrl Pts',(-10.3855514746607,-0.999999999999997,
-6.50110607538848));
#139176=CARTESIAN_POINT('Ctrl Pts',(-10.1948244706177,-0.999999999999997,
-6.11500018915609));
#139177=CARTESIAN_POINT('Ctrl Pts',(-9.76798833941153,-0.999999999999997,
-6.17214441503704));
#139178=CARTESIAN_POINT('Ctrl Pts',(-10.0269206021976,-0.999999999999998,
-6.678261084678));
#139179=CARTESIAN_POINT('Ctrl Pts',(-9.96334493418329,-0.999999999999998,
-6.54955912260054));
#139180=CARTESIAN_POINT('Ctrl Pts',(-9.82106622378125,-0.999999999999998,
-6.56860719789419));
#139181=CARTESIAN_POINT('',(-9.82106622378125,-0.999999999999998,-6.56860719789418));
#139182=CARTESIAN_POINT('Origin',(-9.82106622378125,-1.4,-6.56860719789418));
#139183=CARTESIAN_POINT('Origin',(-9.84760516596611,-1.4,-6.76683858932276));
#139184=CARTESIAN_POINT('Origin',(-9.84760516596611,-0.999999999999998,
-6.76683858932276));
#139185=CARTESIAN_POINT('Origin',(-9.35,-1.4,-3.05000000003699));
#139186=CARTESIAN_POINT('',(-8.03637226370819,-0.999999999999998,-6.34801185120503));
#139187=CARTESIAN_POINT('Origin',(-8.03637226370819,-1.4,-6.34801185120503));
#139188=CARTESIAN_POINT('Origin',(-9.35,-0.999999999999998,-3.05000000003699));
#139189=CARTESIAN_POINT('Ctrl Pts',(-8.18438665652981,-1.4,-5.97640488205934));
#139190=CARTESIAN_POINT('Ctrl Pts',(-7.77682733610448,-1.4,-5.81407034487284));
#139191=CARTESIAN_POINT('Ctrl Pts',(-7.49853797666954,-1.4,-6.15320473424437));
#139192=CARTESIAN_POINT('Ctrl Pts',(-8.18438665652981,-0.999999999999996,
-5.97640488205934));
#139193=CARTESIAN_POINT('Ctrl Pts',(-7.77682733610448,-0.999999999999996,
-5.81407034487284));
#139194=CARTESIAN_POINT('Ctrl Pts',(-7.49853797666954,-0.999999999999996,
-6.15320473424437));
#139195=CARTESIAN_POINT('Ctrl Pts',(-8.03637226370819,-0.999999999999998,
-6.34801185120503));
#139196=CARTESIAN_POINT('Ctrl Pts',(-7.90051915689975,-0.999999999999998,
-6.29390033880953));
#139197=CARTESIAN_POINT('Ctrl Pts',(-7.8077560370881,-0.999999999999998,
-6.40694513526671));
#139198=CARTESIAN_POINT('Origin',(-7.96236506729739,-1.4,-6.53381533577788));
#139199=CARTESIAN_POINT('Origin',(-7.96236506729739,-0.999999999999998,
-6.53381533577788));
#139200=CARTESIAN_POINT('Origin',(-12.8272537083641,-10.3,-12.7988100287935));
#139201=CARTESIAN_POINT('',(-13.3652000170587,-10.1,-12.5330775148592));
#139202=CARTESIAN_POINT('',(-13.3652000170587,-10.3,-12.5330775148592));
#139203=CARTESIAN_POINT('',(-13.4147698236169,-10.1,-12.6770528346803));
#139204=CARTESIAN_POINT('Origin',(-12.8272537083641,-10.1,-12.7988100287935));
#139205=CARTESIAN_POINT('',(-13.4147698236169,-10.3,-12.6770528346803));
#139206=CARTESIAN_POINT('',(-13.4147698236169,-10.3,-12.6770528346803));
#139207=CARTESIAN_POINT('',(-13.2492662807277,-10.3,-13.2253137084577));
#139208=CARTESIAN_POINT('Origin',(-12.8272537083641,-10.3,-12.7988100287935));
#139209=CARTESIAN_POINT('',(-13.2492662807277,-10.3,-13.2253137084577));
#139210=CARTESIAN_POINT('Origin',(-13.5898168899543,-10.3,-12.9877897209636));
#139211=CARTESIAN_POINT('',(-10.3855514746607,-10.1,-6.50110607538849));
#139212=CARTESIAN_POINT('',(-10.3855514746607,-10.3,-6.50110607538848));
#139213=CARTESIAN_POINT('',(-12.6826584637285,-10.1,-11.1513470532436));
#139214=CARTESIAN_POINT('Origin',(-9.84760516596611,-10.3,-6.76683858932276));
#139215=CARTESIAN_POINT('Origin',(-9.84760516596611,-10.1,-6.76683858932276));
#139216=CARTESIAN_POINT('Origin',(-7.96236506729739,-10.3,-6.53381533577788));
#139217=CARTESIAN_POINT('',(-7.49853797666954,-10.1,-6.15320473424437));
#139218=CARTESIAN_POINT('',(-7.49853797666954,-10.3,-6.15320473424437));
#139219=CARTESIAN_POINT('Origin',(-7.96236506729739,-10.1,-6.53381533577788));
#139220=CARTESIAN_POINT('Origin',(-5.6920614055489E-17,-10.3,-2.28766658394441E-15));
#139221=CARTESIAN_POINT('',(-1.3145195915239,-10.1,-9.61051707935543));
#139222=CARTESIAN_POINT('',(-1.3145195915239,-10.3,-9.61051707935543));
#139223=CARTESIAN_POINT('Origin',(-5.6920614055489E-17,-10.1,-2.23416185986609E-15));
#139224=CARTESIAN_POINT('Origin',(-15.3583079095877,-0.999999999999998,
-5.47267507566318));
#139225=CARTESIAN_POINT('Origin',(1.2059399467532,-1.4,-14.5360946469435));
#139226=CARTESIAN_POINT('',(0.80690597004293,-1.4,-16.9002451764429));
#139227=CARTESIAN_POINT('',(1.20690593664767,-0.999999999999996,-16.9000817254963));
#139228=CARTESIAN_POINT('Origin',(1.20690593664767,-1.4,-16.9000817254963));
#139229=CARTESIAN_POINT('',(1.20416970133443,-0.999999999999998,-10.2039196212706));
#139230=CARTESIAN_POINT('',(1.2059399467532,-0.999999999999997,-14.5360946469435));
#139231=CARTESIAN_POINT('',(0.804169734729696,-1.4,-10.2040830722172));
#139232=CARTESIAN_POINT('Origin',(1.20416970133443,-1.4,-10.2039196212706));
#139233=CARTESIAN_POINT('',(0.805939980148468,-1.4,-14.5362580978901));
#139234=CARTESIAN_POINT('Ctrl Pts',(0.804169734729695,-1.4,-10.2040830722172));
#139235=CARTESIAN_POINT('Ctrl Pts',(0.80395589875457,-1.4,-9.68077999728824));
#139236=CARTESIAN_POINT('Ctrl Pts',(1.32237339244619,-1.4,-9.60943957263028));
#139237=CARTESIAN_POINT('Ctrl Pts',(0.804169734729694,-0.999999999999995,
-10.2040830722172));
#139238=CARTESIAN_POINT('Ctrl Pts',(0.803955898754569,-0.999999999999995,
-9.68077999728824));
#139239=CARTESIAN_POINT('Ctrl Pts',(1.32237339244619,-0.999999999999995,
-9.60943957263028));
#139240=CARTESIAN_POINT('Ctrl Pts',(1.20416970133443,-0.999999999999997,
-10.2039196212706));
#139241=CARTESIAN_POINT('Ctrl Pts',(1.20409842267606,-0.999999999999997,
-10.029485262961));
#139242=CARTESIAN_POINT('Ctrl Pts',(1.37690425390659,-0.999999999999997,
-10.0057051214084));
#139243=CARTESIAN_POINT('',(1.37690425390659,-0.999999999999998,-10.0057051214084));
#139244=CARTESIAN_POINT('',(1.32237339244619,-1.4,-9.60943957263028));
#139245=CARTESIAN_POINT('Origin',(1.37690425390659,-1.4,-10.0057051214084));
#139246=CARTESIAN_POINT('Origin',(1.4041696846368,-1.4,-10.2038378957974));
#139247=CARTESIAN_POINT('Origin',(1.4041696846368,-0.999999999999998,-10.2038378957974));
#139248=CARTESIAN_POINT('Origin',(-5.6920614055489E-17,-1.4,9.32936375408611E-17));
#139249=CARTESIAN_POINT('',(5.63745932045745,-0.999999999999998,-8.38027760346821));
#139250=CARTESIAN_POINT('',(5.41419360512517,-1.4,-8.0483854216423));
#139251=CARTESIAN_POINT('Origin',(5.63745932045745,-1.4,-8.38027760346821));
#139252=CARTESIAN_POINT('Origin',(-5.6920614055489E-17,-1.4,9.32936375408611E-17));
#139253=CARTESIAN_POINT('Origin',(-5.41450564939261E-17,-1.,1.82113427247051E-16));
#139254=CARTESIAN_POINT('Ctrl Pts',(5.41419360512517,-1.4,-8.0483854216423));
#139255=CARTESIAN_POINT('Ctrl Pts',(5.79937046939362,-1.4,-7.78927480428087));
#139256=CARTESIAN_POINT('Ctrl Pts',(6.14689326954821,-1.4,-8.09705302340923));
#139257=CARTESIAN_POINT('Ctrl Pts',(5.41419360512517,-0.999999999999997,
-8.0483854216423));
#139258=CARTESIAN_POINT('Ctrl Pts',(5.79937046939362,-0.999999999999997,
-7.78927480428087));
#139259=CARTESIAN_POINT('Ctrl Pts',(6.14689326954821,-0.999999999999997,
-8.09705302340923));
#139260=CARTESIAN_POINT('Ctrl Pts',(5.63745932045745,-0.999999999999998,
-8.38027760346822));
#139261=CARTESIAN_POINT('Ctrl Pts',(5.76585160854694,-0.999999999999998,
-8.29390739768107));
#139262=CARTESIAN_POINT('Ctrl Pts',(5.8816925419318,-0.999999999999998,
-8.39650013739052));
#139263=CARTESIAN_POINT('',(5.8816925419318,-0.999999999999998,-8.39650013739052));
#139264=CARTESIAN_POINT('',(6.14689326954821,-1.4,-8.09705302340923));
#139265=CARTESIAN_POINT('Origin',(5.8816925419318,-1.4,-8.39650013739052));
#139266=CARTESIAN_POINT('Origin',(5.74909217812359,-1.4,-8.54622369438117));
#139267=CARTESIAN_POINT('Origin',(5.74909217812359,-0.999999999999998,-8.54622369438117));
#139268=CARTESIAN_POINT('Origin',(8.6,-1.4,-5.32716721908225));
#139269=CARTESIAN_POINT('',(7.1958904109589,-0.999999999999998,-9.17924149951387));
#139270=CARTESIAN_POINT('',(7.33287671232876,-1.4,-8.80342937459372));
#139271=CARTESIAN_POINT('Origin',(7.1958904109589,-1.4,-9.17924149951387));
#139272=CARTESIAN_POINT('Origin',(8.6,-1.4,-5.32716721908225));
#139273=CARTESIAN_POINT('Origin',(8.6,-0.999999999999999,-5.32716721908225));
#139274=CARTESIAN_POINT('Origin',(6.1,-1.4,-12.1857384988751));
#139275=CARTESIAN_POINT('',(9.3,-0.999999999999997,-12.1857384988752));
#139276=CARTESIAN_POINT('',(9.7,-1.4,-12.1857384988752));
#139277=CARTESIAN_POINT('Origin',(9.3,-1.4,-12.1857384988752));
#139278=CARTESIAN_POINT('Origin',(6.1,-1.4,-12.1857384988751));
#139279=CARTESIAN_POINT('Origin',(6.1,-0.999999999999997,-12.1857384988751));
#139280=CARTESIAN_POINT('Origin',(9.3,-1.4,-11.8807427340099));
#139281=CARTESIAN_POINT('',(9.3,-0.999999999999997,-15.1));
#139282=CARTESIAN_POINT('',(9.7,-1.4,-15.1));
#139283=CARTESIAN_POINT('Origin',(9.3,-1.4,-15.1));
#139284=CARTESIAN_POINT('',(9.7,-1.4,-11.8807427340099));
#139285=CARTESIAN_POINT('',(9.3,-0.999999999999997,-11.8807427340099));
#139286=CARTESIAN_POINT('Origin',(15.1,-1.4,-15.1));
#139287=CARTESIAN_POINT('',(9.56715263178558,-0.999999999999996,-16.8400000000123));
#139288=CARTESIAN_POINT('',(9.94872831235209,-1.4,-16.7200000000114));
#139289=CARTESIAN_POINT('Origin',(9.56715263178558,-1.4,-16.8400000000123));
#139290=CARTESIAN_POINT('Origin',(15.1,-1.4,-15.1));
#139291=CARTESIAN_POINT('Origin',(15.1,-0.999999999999997,-15.1));
#139292=CARTESIAN_POINT('Ctrl Pts',(9.94872831235209,-1.4,-16.7200000000114));
#139293=CARTESIAN_POINT('Ctrl Pts',(10.0399069451865,-1.4,-17.0099295739836));
#139294=CARTESIAN_POINT('Ctrl Pts',(9.86010025640058,-1.4,-17.2549647869982));
#139295=CARTESIAN_POINT('Ctrl Pts',(9.68029356761475,-1.4,-17.5000000000127));
#139296=CARTESIAN_POINT('Ctrl Pts',(9.37636479150232,-1.4,-17.5000000000127));
#139297=CARTESIAN_POINT('Ctrl Pts',(9.94872831235209,-0.999999999999947,
-16.7200000000114));
#139298=CARTESIAN_POINT('Ctrl Pts',(10.0399069451865,-0.999999999999947,
-17.0099295739836));
#139299=CARTESIAN_POINT('Ctrl Pts',(9.86010025640058,-0.999999999999947,
-17.2549647869982));
#139300=CARTESIAN_POINT('Ctrl Pts',(9.68029356761475,-0.999999999999947,
-17.5000000000127));
#139301=CARTESIAN_POINT('Ctrl Pts',(9.37636479150232,-0.999999999999947,
-17.5000000000127));
#139302=CARTESIAN_POINT('Ctrl Pts',(9.56715263178553,-0.999999999999996,
-16.8400000000123));
#139303=CARTESIAN_POINT('Ctrl Pts',(9.59754550939699,-0.999999999999996,
-16.9366431913363));
#139304=CARTESIAN_POINT('Ctrl Pts',(9.53760994646837,-0.999999999999996,
-17.0183215956745));
#139305=CARTESIAN_POINT('Ctrl Pts',(9.47767438353977,-0.999999999999996,
-17.1000000000126));
#139306=CARTESIAN_POINT('Ctrl Pts',(9.37636479150232,-0.999999999999996,
-17.1000000000126));
#139307=CARTESIAN_POINT('',(9.37636479150258,-0.999999999999996,-17.1000000000127));
#139308=CARTESIAN_POINT('',(9.3763647915031,-1.4,-17.5000000000127));
#139309=CARTESIAN_POINT('Origin',(9.37636479150258,-1.4,-17.1000000000127));
#139310=CARTESIAN_POINT('Origin',(9.37636479150232,-1.4,-16.9000000000127));
#139311=CARTESIAN_POINT('Origin',(9.37636479150232,-0.999999999999996,-16.9000000000127));
#139312=CARTESIAN_POINT('Origin',(1.35908660826565,-1.4,-17.1000000000231));
#139313=CARTESIAN_POINT('',(1.40690591995029,-0.999999999999996,-17.1000000000231));
#139314=CARTESIAN_POINT('',(1.40690591995081,-1.4,-17.5000000000231));
#139315=CARTESIAN_POINT('Origin',(1.40690591995029,-1.4,-17.1000000000231));
#139316=CARTESIAN_POINT('',(1.35908660826617,-1.4,-17.5000000000231));
#139317=CARTESIAN_POINT('',(1.35908660826565,-0.999999999999996,-17.1000000000231));
#139318=CARTESIAN_POINT('Ctrl Pts',(1.40690591995003,-1.4,-17.5000000000231));
#139319=CARTESIAN_POINT('Ctrl Pts',(0.807151046297258,-1.4,-17.5000000000232));
#139320=CARTESIAN_POINT('Ctrl Pts',(0.806905970042931,-1.4,-16.9002451764429));
#139321=CARTESIAN_POINT('Ctrl Pts',(1.40690591995003,-0.999999999999993,
-17.5000000000231));
#139322=CARTESIAN_POINT('Ctrl Pts',(0.807151046297256,-0.999999999999993,
-17.5000000000232));
#139323=CARTESIAN_POINT('Ctrl Pts',(0.806905970042928,-0.999999999999994,
-16.9002451764429));
#139324=CARTESIAN_POINT('Ctrl Pts',(1.40690591995003,-0.999999999999996,
-17.1000000000231));
#139325=CARTESIAN_POINT('Ctrl Pts',(1.20698762873244,-0.999999999999996,
-17.1000000000231));
#139326=CARTESIAN_POINT('Ctrl Pts',(1.20690593664767,-0.999999999999996,
-16.9000817254963));
#139327=CARTESIAN_POINT('Origin',(1.40690591995003,-1.4,-16.9000000000231));
#139328=CARTESIAN_POINT('Origin',(1.40690591995003,-0.999999999999996,-16.9000000000231));
#139329=CARTESIAN_POINT('Origin',(9.7,-10.3,-12.1857384988752));
#139330=CARTESIAN_POINT('',(9.7,-10.3,-15.1));
#139331=CARTESIAN_POINT('',(9.7,-10.3,-15.1));
#139332=CARTESIAN_POINT('',(9.7,-10.3,-13.400000000037));
#139333=CARTESIAN_POINT('',(9.7,-10.3,-6.31786924944886));
#139334=CARTESIAN_POINT('',(9.7,-7.5,-13.400000000037));
#139335=CARTESIAN_POINT('',(9.7,-10.3,-13.400000000037));
#139336=CARTESIAN_POINT('',(9.7,-7.5,-12.1857384988752));
#139337=CARTESIAN_POINT('',(9.7,-7.5,-6.9928692494393));
#139338=CARTESIAN_POINT('',(9.7,-10.3,-12.1857384988752));
#139339=CARTESIAN_POINT('Origin',(15.1,-10.3,-15.1));
#139340=CARTESIAN_POINT('',(9.94872831235209,-10.3,-16.7200000000114));
#139341=CARTESIAN_POINT('',(9.94872831235209,-10.3,-16.7200000000114));
#139342=CARTESIAN_POINT('Origin',(15.1,-10.3,-15.1));
#139343=CARTESIAN_POINT('Origin',(9.37636479150232,-10.3,-16.9000000000127));
#139344=CARTESIAN_POINT('',(9.3763647915031,-10.3,-17.5000000000127));
#139345=CARTESIAN_POINT('',(9.3763647915031,-10.3,-17.5000000000127));
#139346=CARTESIAN_POINT('Origin',(9.37636479150232,-10.3,-16.9000000000127));
#139347=CARTESIAN_POINT('Origin',(9.81984848702787,-10.3,-17.5000000000121));
#139348=CARTESIAN_POINT('',(1.40690591995081,-10.3,-17.5000000000231));
#139349=CARTESIAN_POINT('',(1.40690591995081,-10.3,-17.5000000000231));
#139350=CARTESIAN_POINT('',(4.90992424351377,-10.3,-17.5000000000185));
#139351=CARTESIAN_POINT('Origin',(1.40690591995003,-10.3,-16.9000000000231));
#139352=CARTESIAN_POINT('',(0.806905970042931,-10.3,-16.9002451764429));
#139353=CARTESIAN_POINT('',(0.80690597004293,-10.3,-16.9002451764429));
#139354=CARTESIAN_POINT('Origin',(1.40690591995003,-10.3,-16.9000000000231));
#139355=CARTESIAN_POINT('Origin',(0.807151046297361,-10.3,-17.5000000000239));
#139356=CARTESIAN_POINT('',(0.804169734729696,-7.5,-10.2040830722172));
#139357=CARTESIAN_POINT('',(0.804169734729696,-10.3,-10.2040830722172));
#139358=CARTESIAN_POINT('',(0.803800167715777,-7.5,-9.29967232166704));
#139359=CARTESIAN_POINT('',(0.8039501151761,-7.5,-9.66662632470086));
#139360=CARTESIAN_POINT('',(0.803800167715815,-10.3,-9.29967232166704));
#139361=CARTESIAN_POINT('',(0.803800167715815,2.06492719942056E-15,-9.29967232166704));
#139362=CARTESIAN_POINT('',(0.803667430903156,-10.3,-8.97483651150704));
#139363=CARTESIAN_POINT('Origin',(-7.10167527050325,-0.999999999999997,
-11.5757469691446));
#139364=CARTESIAN_POINT('Origin',(6.1,-1.4,-12.1857384988751));
#139365=CARTESIAN_POINT('',(10.9,-1.4,-12.1857384988751));
#139366=CARTESIAN_POINT('',(11.3,-0.999999999999998,-12.1857384988751));
#139367=CARTESIAN_POINT('Origin',(11.3,-1.4,-12.1857384988751));
#139368=CARTESIAN_POINT('',(10.2531207906145,-0.999999999999999,-9.05658722439743));
#139369=CARTESIAN_POINT('Origin',(6.1,-0.999999999999998,-12.1857384988751));
#139370=CARTESIAN_POINT('',(9.93364996056724,-1.4,-9.29729116858802));
#139371=CARTESIAN_POINT('Origin',(10.2531207906145,-1.4,-9.05658722439743));
#139372=CARTESIAN_POINT('Origin',(6.1,-1.4,-12.1857384988751));
#139373=CARTESIAN_POINT('Ctrl Pts',(9.93364996056724,-1.4,-9.29729116858803));
#139374=CARTESIAN_POINT('Ctrl Pts',(9.73388216166068,-1.4,-9.03215224555127));
#139375=CARTESIAN_POINT('Ctrl Pts',(9.85238729399619,-1.4,-8.72205168831346));
#139376=CARTESIAN_POINT('Ctrl Pts',(9.97089242633171,-1.4,-8.41195113107564));
#139377=CARTESIAN_POINT('Ctrl Pts',(10.2965705850743,-1.4,-8.34761172707562));
#139378=CARTESIAN_POINT('Ctrl Pts',(9.93364996056724,-0.999999999999997,
-9.29729116858803));
#139379=CARTESIAN_POINT('Ctrl Pts',(9.73388216166068,-0.999999999999997,
-9.03215224555127));
#139380=CARTESIAN_POINT('Ctrl Pts',(9.85238729399619,-0.999999999999997,
-8.72205168831346));
#139381=CARTESIAN_POINT('Ctrl Pts',(9.97089242633171,-0.999999999999997,
-8.41195113107564));
#139382=CARTESIAN_POINT('Ctrl Pts',(10.2965705850743,-0.999999999999997,
-8.34761172707562));
#139383=CARTESIAN_POINT('Ctrl Pts',(10.2531207906145,-0.999999999999999,
-9.05658722439743));
#139384=CARTESIAN_POINT('Ctrl Pts',(10.1865315243123,-0.999999999999999,
-8.96820758338518));
#139385=CARTESIAN_POINT('Ctrl Pts',(10.2260332350908,-0.999999999999999,
-8.86484073097258));
#139386=CARTESIAN_POINT('Ctrl Pts',(10.2655349458693,-0.999999999999999,
-8.76147387855997));
#139387=CARTESIAN_POINT('Ctrl Pts',(10.3740943321169,-0.999999999999999,
-8.74002741055996));
#139388=CARTESIAN_POINT('',(10.3740943321169,-0.999999999999999,-8.74002741055996));
#139389=CARTESIAN_POINT('',(10.2965705850743,-1.4,-8.34761172707562));
#139390=CARTESIAN_POINT('Origin',(10.3740943321169,-1.4,-8.74002741055996));
#139391=CARTESIAN_POINT('Origin',(10.4128562056381,-1.4,-8.93623525230213));
#139392=CARTESIAN_POINT('Origin',(10.4128562056381,-0.999999999999999,-8.93623525230213));
#139393=CARTESIAN_POINT('Origin',(9.25,-1.4,-3.05000000003699));
#139394=CARTESIAN_POINT('',(11.7830419496669,-0.999999999999999,-8.26763341771092));
#139395=CARTESIAN_POINT('',(11.608349401414,-1.4,-7.90779663028513));
#139396=CARTESIAN_POINT('Origin',(11.7830419496669,-1.4,-8.26763341771092));
#139397=CARTESIAN_POINT('Origin',(9.25,-1.4,-3.05000000003699));
#139398=CARTESIAN_POINT('Origin',(9.25,-1.,-3.05000000003699));
#139399=CARTESIAN_POINT('Origin',(15.1,-1.4,-15.1));
#139400=CARTESIAN_POINT('',(14.0444055417443,-0.999999999999999,-7.57875248631252));
#139401=CARTESIAN_POINT('',(13.9888110834979,-1.4,-7.18263475607025));
#139402=CARTESIAN_POINT('Origin',(14.0444055417443,-1.4,-7.57875248631252));
#139403=CARTESIAN_POINT('Origin',(15.1,-1.4,-15.1));
#139404=CARTESIAN_POINT('Origin',(15.1,-0.999999999999998,-15.1));
#139405=CARTESIAN_POINT('Ctrl Pts',(13.9888110834979,-1.4,-7.18263475607025));
#139406=CARTESIAN_POINT('Ctrl Pts',(14.3498084270918,-1.4,-7.13196938511294));
#139407=CARTESIAN_POINT('Ctrl Pts',(14.6249042135416,-1.4,-7.37115209806196));
#139408=CARTESIAN_POINT('Ctrl Pts',(14.8999999999911,-1.4,-7.61033481101023));
#139409=CARTESIAN_POINT('Ctrl Pts',(14.8999999999907,-1.4,-7.97487021655479));
#139410=CARTESIAN_POINT('Ctrl Pts',(13.9888110834979,-0.999999999999998,
-7.18263475607025));
#139411=CARTESIAN_POINT('Ctrl Pts',(14.3498084270918,-0.999999999999998,
-7.13196938511294));
#139412=CARTESIAN_POINT('Ctrl Pts',(14.6249042135416,-0.999999999999998,
-7.37115209806196));
#139413=CARTESIAN_POINT('Ctrl Pts',(14.8999999999911,-0.999999999999998,
-7.61033481101023));
#139414=CARTESIAN_POINT('Ctrl Pts',(14.8999999999907,-0.999999999999998,
-7.97487021655479));
#139415=CARTESIAN_POINT('Ctrl Pts',(14.0444055417443,-0.999999999999999,
-7.57875248631252));
#139416=CARTESIAN_POINT('Ctrl Pts',(14.2249042135413,-0.999999999999999,
-7.55341980083387));
#139417=CARTESIAN_POINT('Ctrl Pts',(14.3624521067662,-0.999999999999999,
-7.67301115730838));
#139418=CARTESIAN_POINT('Ctrl Pts',(14.4999999999909,-0.999999999999999,
-7.79260251378251));
#139419=CARTESIAN_POINT('Ctrl Pts',(14.4999999999907,-0.999999999999999,
-7.97487021655479));
#139420=CARTESIAN_POINT('',(14.4999999999907,-0.999999999999999,-7.97487021655555));
#139421=CARTESIAN_POINT('',(14.8999999999907,-1.4,-7.9748702165563));
#139422=CARTESIAN_POINT('Origin',(14.4999999999907,-1.4,-7.97487021655555));
#139423=CARTESIAN_POINT('Origin',(14.0999999999907,-1.4,-7.97487021655479));
#139424=CARTESIAN_POINT('Origin',(14.0999999999907,-0.999999999999999,-7.97487021655479));
#139425=CARTESIAN_POINT('Origin',(14.4999999999885,-1.4,-9.18002967894291));
#139426=CARTESIAN_POINT('',(14.49999999999,-0.999999999999999,-8.38137084991965));
#139427=CARTESIAN_POINT('',(14.89999999999,-1.4,-8.3813708499204));
#139428=CARTESIAN_POINT('Origin',(14.49999999999,-1.4,-8.38137084991965));
#139429=CARTESIAN_POINT('',(14.8999999999885,-1.4,-9.18002967894366));
#139430=CARTESIAN_POINT('',(14.4999999999885,-0.999999999999999,-9.18002967894291));
#139431=CARTESIAN_POINT('Origin',(15.69999999999,-1.4,-8.38137084992191));
#139432=CARTESIAN_POINT('',(14.8514718625661,-0.999999999999999,-9.22989898734576));
#139433=CARTESIAN_POINT('',(15.1343145750407,-1.4,-8.94705627487115));
#139434=CARTESIAN_POINT('Origin',(14.8514718625661,-1.4,-9.22989898734576));
#139435=CARTESIAN_POINT('Origin',(15.69999999999,-1.4,-8.38137084992191));
#139436=CARTESIAN_POINT('Origin',(15.69999999999,-0.999999999999999,-8.38137084992191));
#139437=CARTESIAN_POINT('Origin',(14.895654763942,-1.4,-9.27408188872161));
#139438=CARTESIAN_POINT('',(16.9828427124746,-0.999999999999998,-11.3612698372543));
#139439=CARTESIAN_POINT('',(17.2656854249492,-1.4,-11.0784271247796));
#139440=CARTESIAN_POINT('Origin',(16.9828427124746,-1.4,-11.3612698372543));
#139441=CARTESIAN_POINT('',(15.1784974764166,-1.4,-8.991239176247));
#139442=CARTESIAN_POINT('',(14.895654763942,-0.999999999999999,-9.27408188872161));
#139443=CARTESIAN_POINT('Ctrl Pts',(17.2656854249492,-1.4,-11.0784271247796));
#139444=CARTESIAN_POINT('Ctrl Pts',(17.5,-1.4,-11.3127416998304));
#139445=CARTESIAN_POINT('Ctrl Pts',(17.5,-1.4,-11.6441125497289));
#139446=CARTESIAN_POINT('Ctrl Pts',(17.2656854249492,-0.999999999999998,
-11.0784271247796));
#139447=CARTESIAN_POINT('Ctrl Pts',(17.5,-0.999999999999998,-11.3127416998304));
#139448=CARTESIAN_POINT('Ctrl Pts',(17.5,-0.999999999999998,-11.6441125497289));
#139449=CARTESIAN_POINT('Ctrl Pts',(16.9828427124746,-0.999999999999998,
-11.3612698372543));
#139450=CARTESIAN_POINT('Ctrl Pts',(17.1,-0.999999999999998,-11.4784271247796));
#139451=CARTESIAN_POINT('Ctrl Pts',(17.1,-0.999999999999998,-11.6441125497289));
#139452=CARTESIAN_POINT('',(17.1,-0.999999999999998,-11.6441125497289));
#139453=CARTESIAN_POINT('',(17.5,-1.4,-11.6441125497289));
#139454=CARTESIAN_POINT('Origin',(17.1,-1.4,-11.6441125497289));
#139455=CARTESIAN_POINT('Origin',(16.7,-1.4,-11.6441125497289));
#139456=CARTESIAN_POINT('Origin',(16.7,-0.999999999999998,-11.6441125497289));
#139457=CARTESIAN_POINT('Origin',(17.1,-1.4,-9.52070091529622));
#139458=CARTESIAN_POINT('',(17.1,-0.999999999999998,-11.8673540249511));
#139459=CARTESIAN_POINT('',(17.5,-1.4,-11.8673540249511));
#139460=CARTESIAN_POINT('Origin',(17.1,-1.4,-11.8673540249511));
#139461=CARTESIAN_POINT('',(17.5,-1.4,-9.52070091529622));
#139462=CARTESIAN_POINT('',(17.1,-0.999999999999999,-9.52070091529622));
#139463=CARTESIAN_POINT('Ctrl Pts',(17.5,-1.4,-11.8673540249511));
#139464=CARTESIAN_POINT('Ctrl Pts',(17.5,-1.4,-12.2106641181924));
#139465=CARTESIAN_POINT('Ctrl Pts',(17.2040270258257,-1.4,-12.3846233624993));
#139466=CARTESIAN_POINT('Ctrl Pts',(16.9080540516514,-1.4,-12.5585826068061));
#139467=CARTESIAN_POINT('Ctrl Pts',(16.6081081081081,-1.4,-12.3915668857698));
#139468=CARTESIAN_POINT('Ctrl Pts',(17.5,-0.999999999999996,-11.8673540249511));
#139469=CARTESIAN_POINT('Ctrl Pts',(17.5,-0.999999999999996,-12.2106641181924));
#139470=CARTESIAN_POINT('Ctrl Pts',(17.2040270258257,-0.999999999999996,
-12.3846233624993));
#139471=CARTESIAN_POINT('Ctrl Pts',(16.9080540516514,-0.999999999999996,
-12.5585826068061));
#139472=CARTESIAN_POINT('Ctrl Pts',(16.6081081081081,-0.999999999999996,
-12.3915668857698));
#139473=CARTESIAN_POINT('Ctrl Pts',(17.1,-0.999999999999998,-11.8673540249511));
#139474=CARTESIAN_POINT('Ctrl Pts',(17.1,-0.999999999999998,-11.9817907226982));
#139475=CARTESIAN_POINT('Ctrl Pts',(17.0013423419419,-0.999999999999998,
-12.0397771374671));
#139476=CARTESIAN_POINT('Ctrl Pts',(16.9026846838838,-0.999999999999998,
-12.0977635522361));
#139477=CARTESIAN_POINT('Ctrl Pts',(16.8027027027027,-0.999999999999998,
-12.042091645224));
#139478=CARTESIAN_POINT('',(16.8027027027027,-0.999999999999998,-12.042091645224));
#139479=CARTESIAN_POINT('',(16.6081081081081,-1.4,-12.3915668857698));
#139480=CARTESIAN_POINT('Origin',(16.8027027027027,-1.4,-12.042091645224));
#139481=CARTESIAN_POINT('Origin',(16.9,-1.4,-11.8673540249511));
#139482=CARTESIAN_POINT('Origin',(16.9,-0.999999999999998,-11.8673540249511));
#139483=CARTESIAN_POINT('Origin',(15.1,-1.4,-15.1));
#139484=CARTESIAN_POINT('',(12.0487179487179,-0.999999999999998,-13.3854511253615));
#139485=CARTESIAN_POINT('',(12.3974358974359,-1.4,-13.5813995681774));
#139486=CARTESIAN_POINT('Origin',(12.0487179487179,-1.4,-13.3854511253615));
#139487=CARTESIAN_POINT('Origin',(15.1,-1.4,-15.1));
#139488=CARTESIAN_POINT('Origin',(15.1,-0.999999999999998,-15.1));
#139489=CARTESIAN_POINT('Ctrl Pts',(12.3974358974359,-1.4,-13.5813995681774));
#139490=CARTESIAN_POINT('Ctrl Pts',(12.0949042531665,-1.4,-14.1197973880112));
#139491=CARTESIAN_POINT('Ctrl Pts',(11.4974521265833,-1.4,-13.9634370201832));
#139492=CARTESIAN_POINT('Ctrl Pts',(10.9,-1.4,-13.8070766523552));
#139493=CARTESIAN_POINT('Ctrl Pts',(10.9,-1.4,-13.1895026825457));
#139494=CARTESIAN_POINT('Ctrl Pts',(12.3974358974359,-0.999999999999997,
-13.5813995681774));
#139495=CARTESIAN_POINT('Ctrl Pts',(12.0949042531665,-0.999999999999996,
-14.1197973880112));
#139496=CARTESIAN_POINT('Ctrl Pts',(11.4974521265833,-0.999999999999996,
-13.9634370201832));
#139497=CARTESIAN_POINT('Ctrl Pts',(10.9,-0.999999999999996,-13.8070766523552));
#139498=CARTESIAN_POINT('Ctrl Pts',(10.9,-0.999999999999997,-13.1895026825457));
#139499=CARTESIAN_POINT('Ctrl Pts',(12.0487179487179,-0.999999999999999,
-13.3854511253615));
#139500=CARTESIAN_POINT('Ctrl Pts',(11.8974521265833,-0.999999999999999,
-13.6546500352785));
#139501=CARTESIAN_POINT('Ctrl Pts',(11.5987260632916,-0.999999999999999,
-13.5764698513645));
#139502=CARTESIAN_POINT('Ctrl Pts',(11.3,-0.999999999999999,-13.4982896674504));
#139503=CARTESIAN_POINT('Ctrl Pts',(11.3,-0.999999999999999,-13.1895026825457));
#139504=CARTESIAN_POINT('',(11.3,-0.999999999999998,-13.1895026825457));
#139505=CARTESIAN_POINT('',(10.9,-1.4,-13.1895026825457));
#139506=CARTESIAN_POINT('Origin',(11.3,-1.4,-13.1895026825457));
#139507=CARTESIAN_POINT('Origin',(11.7,-1.4,-13.1895026825457));
#139508=CARTESIAN_POINT('Origin',(11.7,-0.999999999999998,-13.1895026825457));
#139509=CARTESIAN_POINT('Origin',(11.3,-1.4,-13.1762595651582));
#139510=CARTESIAN_POINT('',(10.9,-1.4,-13.1762595651582));
#139511=CARTESIAN_POINT('',(11.3,-0.999999999999998,-13.1762595651582));
#139512=CARTESIAN_POINT('Origin',(16.7,-4.55,-11.6441125497289));
#139513=CARTESIAN_POINT('',(17.5,-7.5,-11.6441125497289));
#139514=CARTESIAN_POINT('',(17.5,-4.55,-11.6441125497289));
#139515=CARTESIAN_POINT('',(17.2656854249492,-7.5,-11.0784271247796));
#139516=CARTESIAN_POINT('Origin',(16.7,-7.5,-11.6441125497289));
#139517=CARTESIAN_POINT('',(17.2656854249492,-4.55,-11.0784271247796));
#139518=CARTESIAN_POINT('Origin',(17.5,-7.5,-7.788882700276));
#139519=CARTESIAN_POINT('',(17.5,-7.5,-11.8673540249511));
#139520=CARTESIAN_POINT('',(17.5,-7.5,-11.8673540249511));
#139521=CARTESIAN_POINT('',(17.5,-7.5,-4.79444135013972));
#139522=CARTESIAN_POINT('Origin',(16.9,-7.5,-11.8673540249511));
#139523=CARTESIAN_POINT('',(16.6081081081081,-7.5,-12.3915668857698));
#139524=CARTESIAN_POINT('',(16.6081081081081,-7.5,-12.3915668857698));
#139525=CARTESIAN_POINT('Origin',(16.9,-7.5,-11.8673540249511));
#139526=CARTESIAN_POINT('Origin',(15.1,-7.5,-15.1));
#139527=CARTESIAN_POINT('',(12.3974358974359,-7.5,-13.5813995681774));
#139528=CARTESIAN_POINT('',(12.3974358974359,-7.5,-13.5813995681774));
#139529=CARTESIAN_POINT('Origin',(15.1,-7.5,-15.1));
#139530=CARTESIAN_POINT('Origin',(11.7,-7.5,-13.1895026825457));
#139531=CARTESIAN_POINT('',(10.9,-7.5,-13.1895026825457));
#139532=CARTESIAN_POINT('',(10.9,-7.5,-13.1895026825457));
#139533=CARTESIAN_POINT('Origin',(11.7,-7.5,-13.1895026825457));
#139534=CARTESIAN_POINT('Origin',(10.9,-10.3,-15.1));
#139535=CARTESIAN_POINT('',(10.9,-7.5,-12.1857384988751));
#139536=CARTESIAN_POINT('',(10.9,-8.9,-12.1857384988751));
#139537=CARTESIAN_POINT('',(10.9,-7.5,-12.5463002638159));
#139538=CARTESIAN_POINT('Origin',(6.1,-8.9,-12.1857384988751));
#139539=CARTESIAN_POINT('',(9.93364996056724,-7.5,-9.29729116858802));
#139540=CARTESIAN_POINT('',(9.93364996056724,-8.9,-9.29729116858802));
#139541=CARTESIAN_POINT('Origin',(6.1,-7.5,-12.1857384988751));
#139542=CARTESIAN_POINT('Origin',(13.4742124752016,-0.999999999999998,-11.2525191303165));
#139543=CARTESIAN_POINT('Origin',(15.1,-1.4,-15.1));
#139544=CARTESIAN_POINT('',(14.1784701326418,-1.4,-5.75034285186144));
#139545=CARTESIAN_POINT('',(14.1392350663191,-1.,-5.35227174066313));
#139546=CARTESIAN_POINT('Origin',(14.1392350663191,-1.4,-5.35227174066313));
#139547=CARTESIAN_POINT('',(10.822232934276,-1.,-6.28853108686908));
#139548=CARTESIAN_POINT('Origin',(15.1,-0.999999999999998,-15.1));
#139549=CARTESIAN_POINT('',(10.9969254825289,-1.4,-6.64836787429487));
#139550=CARTESIAN_POINT('Origin',(10.822232934276,-1.4,-6.28853108686908));
#139551=CARTESIAN_POINT('Origin',(15.1,-1.4,-15.1));
#139552=CARTESIAN_POINT('Origin',(9.24999999999998,-1.4,-3.05000000003696));
#139553=CARTESIAN_POINT('',(8.1053957606026,-1.,-6.46319222069398));
#139554=CARTESIAN_POINT('',(7.97821751178067,-1.4,-6.84243580076698));
#139555=CARTESIAN_POINT('Origin',(8.1053957606026,-1.4,-6.46319222069398));
#139556=CARTESIAN_POINT('Origin',(9.24999999999998,-1.4,-3.05000000003696));
#139557=CARTESIAN_POINT('Origin',(9.24999999999998,-1.,-3.05000000003696));
#139558=CARTESIAN_POINT('Ctrl Pts',(7.97821751178067,-1.4,-6.84243580076698));
#139559=CARTESIAN_POINT('Ctrl Pts',(7.68528093764713,-1.4,-6.74420035929417));
#139560=CARTESIAN_POINT('Ctrl Pts',(7.59510710075531,-1.4,-6.44868264820621));
#139561=CARTESIAN_POINT('Ctrl Pts',(7.5049332638635,-1.4,-6.15316493711826));
#139562=CARTESIAN_POINT('Ctrl Pts',(7.69312168782831,-1.4,-5.90811972595898));
#139563=CARTESIAN_POINT('Ctrl Pts',(7.97821751178067,-0.999999999999999,
-6.84243580076698));
#139564=CARTESIAN_POINT('Ctrl Pts',(7.68528093764713,-0.999999999999999,
-6.74420035929417));
#139565=CARTESIAN_POINT('Ctrl Pts',(7.59510710075531,-0.999999999999999,
-6.44868264820621));
#139566=CARTESIAN_POINT('Ctrl Pts',(7.5049332638635,-0.999999999999999,
-6.15316493711826));
#139567=CARTESIAN_POINT('Ctrl Pts',(7.69312168782831,-1.,-5.90811972595898));
#139568=CARTESIAN_POINT('Ctrl Pts',(8.1053957606026,-1.,-6.46319222069398));
#139569=CARTESIAN_POINT('Ctrl Pts',(8.00775023589142,-1.,-6.43044707353637));
#139570=CARTESIAN_POINT('Ctrl Pts',(7.97769229026082,-1.,-6.33194116984039));
#139571=CARTESIAN_POINT('Ctrl Pts',(7.94763434463021,-1.,-6.2334352661444));
#139572=CARTESIAN_POINT('Ctrl Pts',(8.01036381928515,-1.,-6.15175352909131));
#139573=CARTESIAN_POINT('',(8.01036381928515,-1.,-6.15175352909131));
#139574=CARTESIAN_POINT('',(7.69312168782831,-1.4,-5.90811972595898));
#139575=CARTESIAN_POINT('Origin',(8.01036381928515,-1.4,-6.15175352909131));
#139576=CARTESIAN_POINT('Origin',(8.16898488501357,-1.4,-6.27357043065747));
#139577=CARTESIAN_POINT('Origin',(8.16898488501357,-1.,-6.27357043065747));
#139578=CARTESIAN_POINT('Origin',(-2.12720466293355E-17,-1.4,-4.34446022993834E-16));
#139579=CARTESIAN_POINT('',(10.0541415178882,-1.,0.961373152462686));
#139580=CARTESIAN_POINT('',(9.65595769539761,-1.4,0.923298968206739));
#139581=CARTESIAN_POINT('Origin',(10.0541415178882,-1.4,0.961373152462686));
#139582=CARTESIAN_POINT('Origin',(-2.12720466293355E-17,-1.4,-4.34446022993834E-16));
#139583=CARTESIAN_POINT('Origin',(-1.84964890677726E-17,-1.,-3.45626233287644E-16));
#139584=CARTESIAN_POINT('Ctrl Pts',(9.65595769539761,-1.4,0.923298968206736));
#139585=CARTESIAN_POINT('Ctrl Pts',(9.60913873782649,-1.4,1.41293654954985));
#139586=CARTESIAN_POINT('Ctrl Pts',(10.0800826957381,-1.4,1.55488289278605));
#139587=CARTESIAN_POINT('Ctrl Pts',(9.65595769539761,-1.,0.923298968206736));
#139588=CARTESIAN_POINT('Ctrl Pts',(9.60913873782649,-1.,1.41293654954985));
#139589=CARTESIAN_POINT('Ctrl Pts',(10.0800826957381,-1.,1.55488289278605));
#139590=CARTESIAN_POINT('Ctrl Pts',(10.0541415178882,-1.,0.961373152462686));
#139591=CARTESIAN_POINT('Ctrl Pts',(10.0385351986979,-1.,1.12458567957706));
#139592=CARTESIAN_POINT('Ctrl Pts',(10.1955165180017,-1.,1.17190112732246));
#139593=CARTESIAN_POINT('',(10.1955165180017,-1.,1.17190112732246));
#139594=CARTESIAN_POINT('',(10.0800826957381,-1.4,1.55488289278605));
#139595=CARTESIAN_POINT('Origin',(10.1955165180017,-1.4,1.17190112732246));
#139596=CARTESIAN_POINT('Origin',(10.2532334291335,-1.4,0.980410244590661));
#139597=CARTESIAN_POINT('Origin',(10.2532334291335,-1.,0.980410244590661));
#139598=CARTESIAN_POINT('Origin',(15.1,-1.4,-15.1));
#139599=CARTESIAN_POINT('',(14.07589629876,-1.,1.86407781553888));
#139600=CARTESIAN_POINT('',(14.0517925975114,-1.4,2.2633509195493));
#139601=CARTESIAN_POINT('Origin',(14.07589629876,-1.4,1.86407781553888));
#139602=CARTESIAN_POINT('Origin',(15.1,-1.4,-15.1));
#139603=CARTESIAN_POINT('Origin',(15.1,-0.999999999999998,-15.1));
#139604=CARTESIAN_POINT('Ctrl Pts',(14.0517925975114,-1.4,2.2633509195493));
#139605=CARTESIAN_POINT('Ctrl Pts',(14.3967534618246,-1.4,2.2841758474804));
#139606=CARTESIAN_POINT('Ctrl Pts',(14.6483767309169,-1.4,2.04728472062595));
#139607=CARTESIAN_POINT('Ctrl Pts',(14.9000000000088,-1.4,1.81039359377226));
#139608=CARTESIAN_POINT('Ctrl Pts',(14.9000000000085,-1.4,1.46480471152845));
#139609=CARTESIAN_POINT('Ctrl Pts',(14.0517925975114,-1.,2.2633509195493));
#139610=CARTESIAN_POINT('Ctrl Pts',(14.3967534618246,-1.,2.2841758474804));
#139611=CARTESIAN_POINT('Ctrl Pts',(14.6483767309169,-1.,2.04728472062595));
#139612=CARTESIAN_POINT('Ctrl Pts',(14.9000000000088,-1.,1.81039359377226));
#139613=CARTESIAN_POINT('Ctrl Pts',(14.9000000000085,-1.,1.46480471152845));
#139614=CARTESIAN_POINT('Ctrl Pts',(14.07589629876,-1.,1.86407781553887));
#139615=CARTESIAN_POINT('Ctrl Pts',(14.2483767309166,-1.,1.87449027950442));
#139616=CARTESIAN_POINT('Ctrl Pts',(14.3741883654627,-1.,1.7560447160772));
#139617=CARTESIAN_POINT('Ctrl Pts',(14.5000000000087,-1.,1.63759915265035));
#139618=CARTESIAN_POINT('Ctrl Pts',(14.5000000000085,-1.,1.46480471152845));
#139619=CARTESIAN_POINT('',(14.5000000000085,-1.,1.46480471152769));
#139620=CARTESIAN_POINT('',(14.9000000000085,-1.4,1.46480471152694));
#139621=CARTESIAN_POINT('Origin',(14.5000000000085,-1.4,1.46480471152769));
#139622=CARTESIAN_POINT('Origin',(14.1000000000085,-1.4,1.46480471152845));
#139623=CARTESIAN_POINT('Origin',(14.1000000000085,-1.,1.46480471152845));
#139624=CARTESIAN_POINT('Origin',(14.5000000000057,-1.4,-0.0418535935887179));
#139625=CARTESIAN_POINT('',(14.4999999999964,-1.,-4.95420062946558));
#139626=CARTESIAN_POINT('',(14.8999999999964,-1.4,-4.95420062946633));
#139627=CARTESIAN_POINT('Origin',(14.4999999999964,-1.4,-4.95420062946558));
#139628=CARTESIAN_POINT('',(14.9000000000057,-1.4,-0.0418535935894708));
#139629=CARTESIAN_POINT('',(14.5000000000057,-1.,-0.0418535935887179));
#139630=CARTESIAN_POINT('Ctrl Pts',(14.8999999999964,-1.4,-4.95420062946483));
#139631=CARTESIAN_POINT('Ctrl Pts',(14.8999999999957,-1.4,-5.67922673365207));
#139632=CARTESIAN_POINT('Ctrl Pts',(14.1784701326418,-1.4,-5.75034285186144));
#139633=CARTESIAN_POINT('Ctrl Pts',(14.8999999999964,-0.999999999999999,
-4.95420062946483));
#139634=CARTESIAN_POINT('Ctrl Pts',(14.8999999999957,-0.999999999999998,
-5.67922673365208));
#139635=CARTESIAN_POINT('Ctrl Pts',(14.1784701326418,-0.999999999999998,
-5.75034285186144));
#139636=CARTESIAN_POINT('Ctrl Pts',(14.4999999999964,-1.,-4.95420062946483));
#139637=CARTESIAN_POINT('Ctrl Pts',(14.4999999999961,-1.,-5.31671368155845));
#139638=CARTESIAN_POINT('Ctrl Pts',(14.1392350663191,-1.,-5.35227174066313));
#139639=CARTESIAN_POINT('Origin',(14.0999999999964,-1.4,-4.95420062946483));
#139640=CARTESIAN_POINT('Origin',(14.0999999999964,-1.,-4.95420062946483));
#139641=CARTESIAN_POINT('Origin',(15.1,-7.5,-15.1));
#139642=CARTESIAN_POINT('',(14.0517925975114,-6.6,2.2633509195493));
#139643=CARTESIAN_POINT('',(14.0517925975114,-7.5,2.2633509195493));
#139644=CARTESIAN_POINT('',(10.0800826957381,-6.6,1.55488289278605));
#139645=CARTESIAN_POINT('Origin',(15.1,-6.6,-15.1));
#139646=CARTESIAN_POINT('',(10.0800826957381,-7.5,1.55488289278604));
#139647=CARTESIAN_POINT('Origin',(14.1000000000085,-7.5,1.46480471152845));
#139648=CARTESIAN_POINT('',(14.9000000000085,-6.6,1.46480471152694));
#139649=CARTESIAN_POINT('',(14.9000000000085,-7.5,1.46480471152694));
#139650=CARTESIAN_POINT('Origin',(14.1000000000085,-6.6,1.46480471152845));
#139651=CARTESIAN_POINT('Origin',(14.9000000000101,-1.6,2.29381194316098));
#139652=CARTESIAN_POINT('',(14.8999999999964,-6.6,-4.95420062946633));
#139653=CARTESIAN_POINT('',(14.8999999999964,-7.5,-4.95420062946633));
#139654=CARTESIAN_POINT('',(14.9000000000107,-6.6,2.61274169977414));
#139655=CARTESIAN_POINT('Origin',(14.0999999999964,-7.5,-4.95420062946483));
#139656=CARTESIAN_POINT('',(14.1784701326418,-6.6,-5.75034285186144));
#139657=CARTESIAN_POINT('',(14.1784701326418,-7.5,-5.75034285186144));
#139658=CARTESIAN_POINT('Origin',(14.0999999999964,-6.6,-4.95420062946483));
#139659=CARTESIAN_POINT('Origin',(15.1,-7.5,-15.1));
#139660=CARTESIAN_POINT('',(10.9969254825289,-6.6,-6.64836787429487));
#139661=CARTESIAN_POINT('',(10.9969254825289,-7.5,-6.64836787429487));
#139662=CARTESIAN_POINT('Origin',(15.1,-6.6,-15.1));
#139663=CARTESIAN_POINT('Origin',(12.2475425854112,-1.,-2.37751913033493));
#139664=CARTESIAN_POINT('Origin',(7.1,-1.4,10.2));
#139665=CARTESIAN_POINT('',(8.08895342530817,-1.4,6.7385016073135));
#139666=CARTESIAN_POINT('',(8.1988371392313,-1.,6.35389067479278));
#139667=CARTESIAN_POINT('Origin',(8.1988371392313,-1.4,6.35389067479278));
#139668=CARTESIAN_POINT('',(10.1654292935143,-1.,7.63034180357297));
#139669=CARTESIAN_POINT('Origin',(7.1,-1.,10.2));
#139670=CARTESIAN_POINT('',(9.85888636416284,-1.4,7.88730762321568));
#139671=CARTESIAN_POINT('Origin',(10.1654292935143,-1.4,7.63034180357297));
#139672=CARTESIAN_POINT('Origin',(7.1,-1.4,10.2));
#139673=CARTESIAN_POINT('Ctrl Pts',(9.85888636416284,-1.40000000000001,
7.88730762321567));
#139674=CARTESIAN_POINT('Ctrl Pts',(10.0378132267164,-1.40000000000001,
8.10075532868519));
#139675=CARTESIAN_POINT('Ctrl Pts',(10.3106112119491,-1.40000000000001,
8.15693365516831));
#139676=CARTESIAN_POINT('Ctrl Pts',(9.85888636416284,-1.,7.88730762321567));
#139677=CARTESIAN_POINT('Ctrl Pts',(10.0378132267164,-1.,8.10075532868519));
#139678=CARTESIAN_POINT('Ctrl Pts',(10.3106112119491,-1.,8.15693365516831));
#139679=CARTESIAN_POINT('Ctrl Pts',(10.1654292935143,-1.00000000000001,
7.63034180357297));
#139680=CARTESIAN_POINT('Ctrl Pts',(10.254892724791,-1.00000000000001,7.73706565630773));
#139681=CARTESIAN_POINT('Ctrl Pts',(10.3912917174074,-1.00000000000001,
7.76515481954929));
#139682=CARTESIAN_POINT('',(10.3912917174074,-1.,7.76515481954929));
#139683=CARTESIAN_POINT('',(10.3106112119491,-1.40000000000001,8.15693365516831));
#139684=CARTESIAN_POINT('Origin',(10.3912917174074,-1.40000000000001,7.76515481954929));
#139685=CARTESIAN_POINT('Origin',(10.4719722228657,-1.40000000000001,7.37337598393028));
#139686=CARTESIAN_POINT('Origin',(10.4719722228657,-1.,7.37337598393028));
#139687=CARTESIAN_POINT('Origin',(15.1,-1.4,-15.1));
#139688=CARTESIAN_POINT('',(13.5486494229367,-1.,8.19335849549308));
#139689=CARTESIAN_POINT('',(13.5220680886962,-1.4,8.5924743090986));
#139690=CARTESIAN_POINT('Origin',(13.5486494229367,-1.4,8.19335849549308));
#139691=CARTESIAN_POINT('Origin',(15.1,-1.4,-15.1));
#139692=CARTESIAN_POINT('Origin',(15.1,-0.999999999999998,-15.1));
#139693=CARTESIAN_POINT('Origin',(13.4954867544557,-1.40000000000001,8.99159012270412));
#139694=CARTESIAN_POINT('',(14.2949988360186,-1.,8.96365391975718));
#139695=CARTESIAN_POINT('',(13.8952427952371,-1.40000000000001,8.97762202123065));
#139696=CARTESIAN_POINT('Origin',(14.2949988360186,-1.40000000000001,8.96365391975718));
#139697=CARTESIAN_POINT('Origin',(13.4954867544557,-1.40000000000001,8.99159012270412));
#139698=CARTESIAN_POINT('Origin',(13.4954867544557,-1.,8.99159012270412));
#139699=CARTESIAN_POINT('Origin',(6.09999999999969,-1.4,9.24999999996331));
#139700=CARTESIAN_POINT('',(14.2987503886286,-1.,9.10684950238171));
#139701=CARTESIAN_POINT('',(13.8988113452808,-1.4,9.11383245348325));
#139702=CARTESIAN_POINT('Origin',(14.2987503886286,-1.4,9.10684950238171));
#139703=CARTESIAN_POINT('Origin',(6.09999999999969,-1.4,9.24999999996331));
#139704=CARTESIAN_POINT('Origin',(6.09999999999969,-1.,9.24999999996331));
#139705=CARTESIAN_POINT('Ctrl Pts',(13.8988113452808,-1.4,9.11383245348325));
#139706=CARTESIAN_POINT('Ctrl Pts',(13.9121679064567,-1.4,9.87881136017178));
#139707=CARTESIAN_POINT('Ctrl Pts',(14.6769816890462,-1.4,9.89957198073334));
#139708=CARTESIAN_POINT('Ctrl Pts',(13.8988113452808,-1.,9.11383245348325));
#139709=CARTESIAN_POINT('Ctrl Pts',(13.9121679064567,-1.,9.87881136017178));
#139710=CARTESIAN_POINT('Ctrl Pts',(14.6769816890462,-1.,9.89957198073334));
#139711=CARTESIAN_POINT('Ctrl Pts',(14.2987503886286,-1.,9.10684950238171));
#139712=CARTESIAN_POINT('Ctrl Pts',(14.3054286692165,-1.,9.48933895572597));
#139713=CARTESIAN_POINT('Ctrl Pts',(14.6878355605112,-1.,9.49971926600675));
#139714=CARTESIAN_POINT('',(14.6878355605112,-1.,9.49971926600675));
#139715=CARTESIAN_POINT('',(14.6769816890462,-1.4,9.89957198073334));
#139716=CARTESIAN_POINT('Origin',(14.6878355605112,-1.4,9.49971926600675));
#139717=CARTESIAN_POINT('Origin',(14.6986894319763,-1.4,9.09986655128017));
#139718=CARTESIAN_POINT('Origin',(14.6986894319763,-1.,9.09986655128017));
#139719=CARTESIAN_POINT('Origin',(12.9190134222136,-1.4,9.45170516624805));
#139720=CARTESIAN_POINT('',(16.8945730642675,-1.,9.55962043546442));
#139721=CARTESIAN_POINT('',(16.8837191928024,-1.4,9.959473150191));
#139722=CARTESIAN_POINT('Origin',(16.8945730642675,-1.4,9.55962043546442));
#139723=CARTESIAN_POINT('',(12.9081595507485,-1.4,9.85155788097463));
#139724=CARTESIAN_POINT('',(12.9190134222136,-1.,9.45170516624805));
#139725=CARTESIAN_POINT('Ctrl Pts',(16.8837191928024,-1.4,9.959473150191));
#139726=CARTESIAN_POINT('Ctrl Pts',(17.1369366949554,-1.4,9.96634665665939));
#139727=CARTESIAN_POINT('Ctrl Pts',(17.3184683474777,-1.4,9.78967575464012));
#139728=CARTESIAN_POINT('Ctrl Pts',(17.5,-1.4,9.61300485262085));
#139729=CARTESIAN_POINT('Ctrl Pts',(17.5,-1.4,9.35969407810112));
#139730=CARTESIAN_POINT('Ctrl Pts',(16.8837191928024,-1.,9.959473150191));
#139731=CARTESIAN_POINT('Ctrl Pts',(17.1369366949554,-1.,9.96634665665939));
#139732=CARTESIAN_POINT('Ctrl Pts',(17.3184683474777,-1.,9.78967575464012));
#139733=CARTESIAN_POINT('Ctrl Pts',(17.5,-1.,9.61300485262085));
#139734=CARTESIAN_POINT('Ctrl Pts',(17.5,-1.,9.35969407810112));
#139735=CARTESIAN_POINT('Ctrl Pts',(16.8945730642675,-1.,9.55962043546442));
#139736=CARTESIAN_POINT('Ctrl Pts',(16.9789788983185,-1.,9.56191160428721));
#139737=CARTESIAN_POINT('Ctrl Pts',(17.0394894491592,-1.,9.50302130361412));
#139738=CARTESIAN_POINT('Ctrl Pts',(17.1,-1.,9.44413100294103));
#139739=CARTESIAN_POINT('Ctrl Pts',(17.1,-1.,9.35969407810112));
#139740=CARTESIAN_POINT('',(17.1,-1.,9.35969407810112));
#139741=CARTESIAN_POINT('',(17.5,-1.4,9.35969407810112));
#139742=CARTESIAN_POINT('Origin',(17.1,-1.4,9.35969407810112));
#139743=CARTESIAN_POINT('Origin',(16.9,-1.4,9.35969407810112));
#139744=CARTESIAN_POINT('Origin',(16.9,-1.,9.35969407810112));
#139745=CARTESIAN_POINT('Origin',(17.1,-1.4,3.79934138063425));
#139746=CARTESIAN_POINT('',(17.1,-1.,5.54411254966196));
#139747=CARTESIAN_POINT('',(17.5,-1.4,5.54411254966196));
#139748=CARTESIAN_POINT('Origin',(17.1,-1.4,5.54411254966196));
#139749=CARTESIAN_POINT('',(17.5,-1.4,3.79934138063425));
#139750=CARTESIAN_POINT('',(17.1,-1.,3.79934138063425));
#139751=CARTESIAN_POINT('Ctrl Pts',(17.5,-1.4,5.54411254966196));
#139752=CARTESIAN_POINT('Ctrl Pts',(17.5,-1.4,5.21274169976348));
#139753=CARTESIAN_POINT('Ctrl Pts',(17.2656854249492,-1.4,4.97842712471272));
#139754=CARTESIAN_POINT('Ctrl Pts',(17.5,-1.,5.54411254966196));
#139755=CARTESIAN_POINT('Ctrl Pts',(17.5,-1.,5.21274169976348));
#139756=CARTESIAN_POINT('Ctrl Pts',(17.2656854249492,-1.,4.97842712471272));
#139757=CARTESIAN_POINT('Ctrl Pts',(17.1,-1.,5.54411254966196));
#139758=CARTESIAN_POINT('Ctrl Pts',(17.1,-1.,5.37842712471272));
#139759=CARTESIAN_POINT('Ctrl Pts',(16.9828427124746,-1.,5.26126983718734));
#139760=CARTESIAN_POINT('',(16.9828427124746,-1.,5.26126983718734));
#139761=CARTESIAN_POINT('',(17.2656854249492,-1.4,4.97842712471272));
#139762=CARTESIAN_POINT('Origin',(16.9828427124746,-1.4,5.26126983718734));
#139763=CARTESIAN_POINT('Origin',(16.7,-1.4,5.54411254966196));
#139764=CARTESIAN_POINT('Origin',(16.7,-1.,5.54411254966196));
#139765=CARTESIAN_POINT('Origin',(14.2407923014043,-1.4,2.51921942611707));
#139766=CARTESIAN_POINT('',(16.1199627900832,-1.,4.39838991479596));
#139767=CARTESIAN_POINT('',(16.4028055025579,-1.4,4.11554720232134));
#139768=CARTESIAN_POINT('Origin',(16.1199627900832,-1.4,4.39838991479596));
#139769=CARTESIAN_POINT('',(14.523635013879,-1.4,2.23637671364245));
#139770=CARTESIAN_POINT('',(14.2407923014043,-1.,2.51921942611707));
#139771=CARTESIAN_POINT('Ctrl Pts',(16.4028055025579,-1.4,4.11554720232134));
#139772=CARTESIAN_POINT('Ctrl Pts',(16.1560511668722,-1.4,3.86879286663565));
#139773=CARTESIAN_POINT('Ctrl Pts',(15.8073298678648,-1.4,3.88178748005695));
#139774=CARTESIAN_POINT('Ctrl Pts',(16.4028055025579,-1.,4.11554720232134));
#139775=CARTESIAN_POINT('Ctrl Pts',(16.1560511668722,-1.,3.86879286663565));
#139776=CARTESIAN_POINT('Ctrl Pts',(15.8073298678648,-1.,3.88178748005695));
#139777=CARTESIAN_POINT('Ctrl Pts',(16.1199627900832,-1.,4.39838991479596));
#139778=CARTESIAN_POINT('Ctrl Pts',(15.9965856222404,-1.,4.27501274695311));
#139779=CARTESIAN_POINT('Ctrl Pts',(15.8222249727367,-1.,4.28151005366376));
#139780=CARTESIAN_POINT('',(15.8222249727367,-1.,4.28151005366376));
#139781=CARTESIAN_POINT('',(15.8073298678648,-1.4,3.88178748005695));
#139782=CARTESIAN_POINT('Origin',(15.8222249727367,-1.4,4.28151005366376));
#139783=CARTESIAN_POINT('Origin',(15.8371200776086,-1.4,4.68123262727058));
#139784=CARTESIAN_POINT('Origin',(15.8371200776086,-1.,4.68123262727058));
#139785=CARTESIAN_POINT('Origin',(15.1,-1.4,-15.1));
#139786=CARTESIAN_POINT('',(9.66476438899747,-1.,3.51780746286748));
#139787=CARTESIAN_POINT('',(9.77686021437815,-1.4,3.13383542491129));
#139788=CARTESIAN_POINT('Origin',(9.66476438899747,-1.4,3.51780746286748));
#139789=CARTESIAN_POINT('Origin',(15.1,-1.4,-15.1));
#139790=CARTESIAN_POINT('Origin',(15.1,-0.999999999999998,-15.1));
#139791=CARTESIAN_POINT('Ctrl Pts',(9.77686021437815,-1.4,3.13383542491129));
#139792=CARTESIAN_POINT('Ctrl Pts',(9.24757706328966,-1.4,2.97931784077377));
#139793=CARTESIAN_POINT('Ctrl Pts',(9.04898541943487,-1.4,3.49368900717495));
#139794=CARTESIAN_POINT('Ctrl Pts',(9.77686021437815,-0.999999999999996,
3.13383542491129));
#139795=CARTESIAN_POINT('Ctrl Pts',(9.24757706328966,-0.999999999999996,
2.97931784077376));
#139796=CARTESIAN_POINT('Ctrl Pts',(9.04898541943487,-0.999999999999996,
3.49368900717495));
#139797=CARTESIAN_POINT('Ctrl Pts',(9.66476438899747,-1.,3.51780746286748));
#139798=CARTESIAN_POINT('Ctrl Pts',(9.48833667196797,-1.,3.4663016014883));
#139799=CARTESIAN_POINT('Ctrl Pts',(9.42213945734972,-1.,3.63775865695536));
#139800=CARTESIAN_POINT('',(9.42213945734971,-1.,3.63775865695536));
#139801=CARTESIAN_POINT('',(9.04898541943487,-1.4,3.49368900717495));
#139802=CARTESIAN_POINT('Origin',(9.42213945734971,-1.4,3.63775865695536));
#139803=CARTESIAN_POINT('Origin',(9.60871647630713,-1.4,3.70979348184556));
#139804=CARTESIAN_POINT('Origin',(9.60871647630713,-1.,3.70979348184556));
#139805=CARTESIAN_POINT('Origin',(-2.12720466293355E-17,-1.4,-4.34446022993834E-16));
#139806=CARTESIAN_POINT('',(8.09351144286873,-1.,6.04194277729877));
#139807=CARTESIAN_POINT('',(7.77297633622046,-1.4,5.8026579148315));
#139808=CARTESIAN_POINT('Origin',(8.09351144286873,-1.4,6.04194277729877));
#139809=CARTESIAN_POINT('Origin',(-2.12720466293355E-17,-1.4,-4.34446022993834E-16));
#139810=CARTESIAN_POINT('Origin',(-1.84964890677726E-17,-1.,-3.45626233287644E-16));
#139811=CARTESIAN_POINT('Ctrl Pts',(7.77297633622047,-1.4,5.80265791483149));
#139812=CARTESIAN_POINT('Ctrl Pts',(7.58454074891624,-1.4,6.05507764773938));
#139813=CARTESIAN_POINT('Ctrl Pts',(7.68530753049779,-1.4,6.35352320031752));
#139814=CARTESIAN_POINT('Ctrl Pts',(7.78607431207935,-1.4,6.65196875289566));
#139815=CARTESIAN_POINT('Ctrl Pts',(8.08895342530817,-1.4,6.7385016073135));
#139816=CARTESIAN_POINT('Ctrl Pts',(7.77297633622047,-1.,5.80265791483149));
#139817=CARTESIAN_POINT('Ctrl Pts',(7.58454074891624,-1.,6.05507764773938));
#139818=CARTESIAN_POINT('Ctrl Pts',(7.68530753049779,-1.,6.35352320031752));
#139819=CARTESIAN_POINT('Ctrl Pts',(7.78607431207935,-1.,6.65196875289566));
#139820=CARTESIAN_POINT('Ctrl Pts',(8.08895342530817,-1.,6.7385016073135));
#139821=CARTESIAN_POINT('Ctrl Pts',(8.09351144286873,-1.,6.04194277729878));
#139822=CARTESIAN_POINT('Ctrl Pts',(8.03069958043399,-1.,6.12608268826807));
#139823=CARTESIAN_POINT('Ctrl Pts',(8.06428850762784,-1.,6.22556453912745));
#139824=CARTESIAN_POINT('Ctrl Pts',(8.09787743482169,-1.,6.32504638998683));
#139825=CARTESIAN_POINT('Ctrl Pts',(8.1988371392313,-1.,6.35389067479278));
#139826=CARTESIAN_POINT('Origin',(8.25377899619286,-1.4,6.16158520853242));
#139827=CARTESIAN_POINT('Origin',(8.25377899619286,-1.,6.16158520853242));
#139828=CARTESIAN_POINT('Origin',(16.7,-4.55,5.54411254966196));
#139829=CARTESIAN_POINT('',(17.2656854249492,-7.5,4.97842712471272));
#139830=CARTESIAN_POINT('',(17.2656854249492,-4.55,4.97842712471272));
#139831=CARTESIAN_POINT('',(17.5,-7.5,5.54411254966196));
#139832=CARTESIAN_POINT('Origin',(16.7,-7.5,5.54411254966196));
#139833=CARTESIAN_POINT('',(17.5,-4.55,5.54411254966196));
#139834=CARTESIAN_POINT('Origin',(17.9686291501015,-1.6,5.68137084986501));
#139835=CARTESIAN_POINT('',(16.4028055025579,-7.5,4.11554720232134));
#139836=CARTESIAN_POINT('',(16.4028055025579,-7.5,4.11554720232134));
#139837=CARTESIAN_POINT('',(17.9686291501015,-7.5,5.68137084986501));
#139838=CARTESIAN_POINT('Origin',(15.8371200776086,-7.5,4.68123262727057));
#139839=CARTESIAN_POINT('',(15.8073298678648,-7.5,3.88178748005694));
#139840=CARTESIAN_POINT('',(15.8073298678648,-7.5,3.88178748005694));
#139841=CARTESIAN_POINT('Origin',(15.8371200776086,-7.5,4.68123262727057));
#139842=CARTESIAN_POINT('Origin',(15.1,-7.5,-15.1));
#139843=CARTESIAN_POINT('',(9.77686021437815,-7.5,3.13383542491129));
#139844=CARTESIAN_POINT('',(9.77686021437815,-7.5,3.13383542491129));
#139845=CARTESIAN_POINT('Origin',(15.1,-7.5,-15.1));
#139846=CARTESIAN_POINT('Origin',(9.60871647630713,-7.5,3.70979348184556));
#139847=CARTESIAN_POINT('',(9.04898541943487,-7.5,3.49368900717495));
#139848=CARTESIAN_POINT('',(9.04898541943487,-7.5,3.49368900717495));
#139849=CARTESIAN_POINT('Origin',(9.60871647630713,-7.5,3.70979348184556));
#139850=CARTESIAN_POINT('Origin',(-2.12720466293355E-17,-7.5,-1.66578428666901E-15));
#139851=CARTESIAN_POINT('',(7.77297633622046,-7.5,5.8026579148315));
#139852=CARTESIAN_POINT('',(7.77297633622046,-7.5,5.8026579148315));
#139853=CARTESIAN_POINT('Origin',(-2.12720466293355E-17,-7.5,-1.66578428666901E-15));
#139854=CARTESIAN_POINT('Origin',(8.25377899619286,-10.3,6.16158520853241));
#139855=CARTESIAN_POINT('',(8.08895342530817,-7.5,6.7385016073135));
#139856=CARTESIAN_POINT('',(8.08895342530817,-10.3,6.7385016073135));
#139857=CARTESIAN_POINT('Origin',(8.25377899619286,-7.5,6.16158520853241));
#139858=CARTESIAN_POINT('Origin',(7.1,-10.3,10.2));
#139859=CARTESIAN_POINT('',(9.85888636416284,-10.3,7.88730762321568));
#139860=CARTESIAN_POINT('',(9.85888636416284,-10.3,7.88730762321568));
#139861=CARTESIAN_POINT('',(6.86069632012767,-10.3,6.60796245164397));
#139862=CARTESIAN_POINT('Origin',(7.1,-10.3,10.2));
#139863=CARTESIAN_POINT('',(6.86069632012767,-7.5,6.60796245164398));
#139864=CARTESIAN_POINT('',(6.86069632012767,-1.92632982761137E-14,6.60796245164398));
#139865=CARTESIAN_POINT('Origin',(7.1,-7.5,10.2));
#139866=CARTESIAN_POINT('Origin',(12.2475425854112,-1.,-2.37751913033493));
#139867=CARTESIAN_POINT('Origin',(-8.47750127826606,-1.4,10.5062825051013));
#139868=CARTESIAN_POINT('',(-3.82759827224048,-1.4,10.4762486150055));
#139869=CARTESIAN_POINT('',(-3.42760661580818,-1.,10.4736650545671));
#139870=CARTESIAN_POINT('Origin',(-3.42760661580818,-1.4,10.4736650545671));
#139871=CARTESIAN_POINT('',(-6.8700032327,-1.,15.2936043068503));
#139872=CARTESIAN_POINT('Origin',(-8.47750127826606,-1.,10.5062825051013));
#139873=CARTESIAN_POINT('',(-6.99732981056662,-1.4,14.9144105007712));
#139874=CARTESIAN_POINT('Origin',(-6.8700032327,-1.4,15.2936043068503));
#139875=CARTESIAN_POINT('Origin',(-8.47750127826606,-1.4,10.5062825051013));
#139876=CARTESIAN_POINT('Ctrl Pts',(-6.99732981056662,-1.4,14.9144105007712));
#139877=CARTESIAN_POINT('Ctrl Pts',(-7.59675516644186,-1.4,15.1156869404874));
#139878=CARTESIAN_POINT('Ctrl Pts',(-7.53937602191996,-1.4,15.7453936946397));
#139879=CARTESIAN_POINT('Ctrl Pts',(-7.48199687739805,-1.4,16.3751004487919));
#139880=CARTESIAN_POINT('Ctrl Pts',(-6.85606479211595,-1.4,16.4647218026392));
#139881=CARTESIAN_POINT('Ctrl Pts',(-6.99732981056662,-1.,14.9144105007711));
#139882=CARTESIAN_POINT('Ctrl Pts',(-7.59675516644186,-1.,15.1156869404874));
#139883=CARTESIAN_POINT('Ctrl Pts',(-7.53937602191996,-1.,15.7453936946397));
#139884=CARTESIAN_POINT('Ctrl Pts',(-7.48199687739805,-1.,16.3751004487919));
#139885=CARTESIAN_POINT('Ctrl Pts',(-6.85606479211595,-1.,16.4647218026392));
#139886=CARTESIAN_POINT('Ctrl Pts',(-6.8700032327,-1.,15.2936043068503));
#139887=CARTESIAN_POINT('Ctrl Pts',(-7.16971591063762,-1.,15.3942425267084));
#139888=CARTESIAN_POINT('Ctrl Pts',(-7.14102633837667,-1.,15.7090959037845));
#139889=CARTESIAN_POINT('Ctrl Pts',(-7.11233676611572,-1.,16.0239492808607));
#139890=CARTESIAN_POINT('Ctrl Pts',(-6.79937072347466,-1.,16.0687599577843));
#139891=CARTESIAN_POINT('',(-6.79937072347466,-1.,16.0687599577843));
#139892=CARTESIAN_POINT('',(-6.85606479211595,-1.4,16.4647218026392));
#139893=CARTESIAN_POINT('Origin',(-6.79937072347466,-1.4,16.0687599577843));
#139894=CARTESIAN_POINT('Origin',(-6.74267665483338,-1.4,15.6727981129294));
#139895=CARTESIAN_POINT('Origin',(-6.74267665483338,-1.,15.6727981129294));
#139896=CARTESIAN_POINT('Origin',(-4.95681349263295,-1.4,3.2));
#139897=CARTESIAN_POINT('',(-4.95681349263295,-1.,16.2));
#139898=CARTESIAN_POINT('',(-4.95681349263295,-1.4,16.6));
#139899=CARTESIAN_POINT('Origin',(-4.95681349263295,-1.4,16.2));
#139900=CARTESIAN_POINT('Origin',(-4.95681349263295,-1.4,3.2));
#139901=CARTESIAN_POINT('Origin',(-4.95681349263295,-1.,3.2));
#139902=CARTESIAN_POINT('Origin',(-6.63837624017517,-1.4,16.2));
#139903=CARTESIAN_POINT('',(1.39248124878044,-1.,16.2));
#139904=CARTESIAN_POINT('',(1.39248124878044,-1.4,16.6));
#139905=CARTESIAN_POINT('Origin',(1.39248124878044,-1.4,16.2));
#139906=CARTESIAN_POINT('',(-6.63837624017517,-1.4,16.6));
#139907=CARTESIAN_POINT('',(-6.63837624017517,-1.,16.2));
#139908=CARTESIAN_POINT('Ctrl Pts',(1.39248124878044,-1.4,16.6));
#139909=CARTESIAN_POINT('Ctrl Pts',(1.87120813518912,-1.4,16.6));
#139910=CARTESIAN_POINT('Ctrl Pts',(2.09748000071234,-1.4,16.178122678207));
#139911=CARTESIAN_POINT('Ctrl Pts',(1.39248124878044,-1.,16.6));
#139912=CARTESIAN_POINT('Ctrl Pts',(1.87120813518912,-1.,16.6));
#139913=CARTESIAN_POINT('Ctrl Pts',(2.09748000071234,-1.,16.178122678207));
#139914=CARTESIAN_POINT('Ctrl Pts',(1.39248124878044,-1.,16.2));
#139915=CARTESIAN_POINT('Ctrl Pts',(1.63184469198478,-1.,16.2));
#139916=CARTESIAN_POINT('Ctrl Pts',(1.74498062474639,-1.,15.9890613391035));
#139917=CARTESIAN_POINT('',(1.74498062474639,-1.,15.9890613391035));
#139918=CARTESIAN_POINT('',(2.09748000071234,-1.4,16.178122678207));
#139919=CARTESIAN_POINT('Origin',(1.74498062474639,-1.4,15.9890613391035));
#139920=CARTESIAN_POINT('Origin',(1.39248124878044,-1.4,15.8));
#139921=CARTESIAN_POINT('Origin',(1.39248124878044,-1.,15.8));
#139922=CARTESIAN_POINT('Origin',(-8.47750127826606,-1.4,10.5062825051013));
#139923=CARTESIAN_POINT('',(3.12239099121706,-1.,10.5562758685179));
#139924=CARTESIAN_POINT('',(3.52238727637165,-1.4,10.5579997776013));
#139925=CARTESIAN_POINT('Origin',(3.12239099121706,-1.4,10.5562758685179));
#139926=CARTESIAN_POINT('Origin',(-8.47750127826606,-1.4,10.5062825051013));
#139927=CARTESIAN_POINT('Origin',(-8.47750127826606,-1.,10.5062825051013));
#139928=CARTESIAN_POINT('Ctrl Pts',(3.52238727637165,-1.4,10.5579997776013));
#139929=CARTESIAN_POINT('Ctrl Pts',(3.52408213740859,-1.4,10.1647434712322));
#139930=CARTESIAN_POINT('Ctrl Pts',(3.21373231632171,-1.4,9.92321421088415));
#139931=CARTESIAN_POINT('Ctrl Pts',(2.90338249523483,-1.4,9.68168495053607));
#139932=CARTESIAN_POINT('Ctrl Pts',(2.52258592029807,-1.4,9.77990594406283));
#139933=CARTESIAN_POINT('Ctrl Pts',(3.52238727637165,-1.,10.5579997776013));
#139934=CARTESIAN_POINT('Ctrl Pts',(3.52408213740859,-1.,10.1647434712322));
#139935=CARTESIAN_POINT('Ctrl Pts',(3.21373231632171,-1.,9.92321421088415));
#139936=CARTESIAN_POINT('Ctrl Pts',(2.90338249523483,-1.,9.68168495053607));
#139937=CARTESIAN_POINT('Ctrl Pts',(2.52258592029807,-1.,9.77990594406283));
#139938=CARTESIAN_POINT('Ctrl Pts',(3.12239099121706,-1.,10.5562758685179));
#139939=CARTESIAN_POINT('Ctrl Pts',(3.12323842173553,-1.,10.3596477153334));
#139940=CARTESIAN_POINT('Ctrl Pts',(2.96806351119209,-1.,10.2388830851594));
#139941=CARTESIAN_POINT('Ctrl Pts',(2.81288860064865,-1.,10.1181184549853));
#139942=CARTESIAN_POINT('Ctrl Pts',(2.62249031318027,-1.,10.1672289517487));
#139943=CARTESIAN_POINT('',(2.62249031318027,-1.,10.1672289517487));
#139944=CARTESIAN_POINT('',(2.52258592029807,-1.4,9.77990594406283));
#139945=CARTESIAN_POINT('Origin',(2.62249031318027,-1.4,10.1672289517487));
#139946=CARTESIAN_POINT('Origin',(2.72239470606247,-1.4,10.5545519594346));
#139947=CARTESIAN_POINT('Origin',(2.72239470606247,-1.,10.5545519594346));
#139948=CARTESIAN_POINT('Origin',(9.00768359641396E-11,-1.4,2.56054600265843E-10));
#139949=CARTESIAN_POINT('',(-2.91650982324592,-1.,10.0868216227845));
#139950=CARTESIAN_POINT('',(-2.80540468711597,-1.4,9.70256175144017));
#139951=CARTESIAN_POINT('Origin',(-2.91650982324592,-1.4,10.0868216227845));
#139952=CARTESIAN_POINT('Origin',(9.00768359641396E-11,-1.4,2.56054600265843E-10));
#139953=CARTESIAN_POINT('Origin',(9.00768387396972E-11,-1.,2.56054689085632E-10));
#139954=CARTESIAN_POINT('Ctrl Pts',(-2.80540468711597,-1.4,9.70256175144017));
#139955=CARTESIAN_POINT('Ctrl Pts',(-3.19065678822161,-1.4,9.59116972138524));
#139956=CARTESIAN_POINT('Ctrl Pts',(-3.51042264606467,-1.4,9.83319691391525));
#139957=CARTESIAN_POINT('Ctrl Pts',(-3.83018850390773,-1.4,10.0752241064453));
#139958=CARTESIAN_POINT('Ctrl Pts',(-3.82759827224048,-1.4,10.4762486150055));
#139959=CARTESIAN_POINT('Ctrl Pts',(-2.80540468711597,-1.,9.70256175144017));
#139960=CARTESIAN_POINT('Ctrl Pts',(-3.19065678822161,-1.,9.59116972138524));
#139961=CARTESIAN_POINT('Ctrl Pts',(-3.51042264606467,-1.,9.83319691391525));
#139962=CARTESIAN_POINT('Ctrl Pts',(-3.83018850390773,-1.,10.0752241064453));
#139963=CARTESIAN_POINT('Ctrl Pts',(-3.82759827224049,-1.,10.4762486150055));
#139964=CARTESIAN_POINT('Ctrl Pts',(-2.91650982324592,-1.,10.0868216227845));
#139965=CARTESIAN_POINT('Ctrl Pts',(-3.10913587379874,-1.,10.031125607757));
#139966=CARTESIAN_POINT('Ctrl Pts',(-3.26901880272027,-1.,10.152139204022));
#139967=CARTESIAN_POINT('Ctrl Pts',(-3.4289017316418,-1.,10.273152800287));
#139968=CARTESIAN_POINT('Ctrl Pts',(-3.42760661580818,-1.,10.4736650545671));
#139969=CARTESIAN_POINT('Origin',(-3.02761495937587,-1.4,10.4710814941288));
#139970=CARTESIAN_POINT('Origin',(-3.02761495937587,-1.,10.4710814941288));
#139971=CARTESIAN_POINT('Origin',(-8.47750127826606,-2.6,10.5062825051013));
#139972=CARTESIAN_POINT('',(3.52238727637165,-2.6,10.5579997776013));
#139973=CARTESIAN_POINT('',(3.52238727637165,-2.6,10.5579997776013));
#139974=CARTESIAN_POINT('',(3.51261604728234,-2.6,10.0193671946169));
#139975=CARTESIAN_POINT('Origin',(-8.47750127826606,-2.6,10.5062825051013));
#139976=CARTESIAN_POINT('',(3.51261604728234,-10.3,10.0193671946169));
#139977=CARTESIAN_POINT('',(3.51261604728234,-2.6,10.0193671946169));
#139978=CARTESIAN_POINT('',(1.22705833076043,-10.3,17.5647187904871));
#139979=CARTESIAN_POINT('Origin',(-8.47750127826606,-10.3,10.5062825051013));
#139980=CARTESIAN_POINT('',(1.22705833076043,-2.6,17.5647187904871));
#139981=CARTESIAN_POINT('',(1.22705833076043,-2.6,17.5647187904871));
#139982=CARTESIAN_POINT('',(2.09748000071234,-2.6,16.178122678207));
#139983=CARTESIAN_POINT('Origin',(-8.47750127826606,-2.6,10.5062825051013));
#139984=CARTESIAN_POINT('',(2.09748000071234,-2.6,16.178122678207));
#139985=CARTESIAN_POINT('Origin',(2.72239470606247,-2.6,10.5545519594346));
#139986=CARTESIAN_POINT('',(2.52258592029807,-2.6,9.77990594406283));
#139987=CARTESIAN_POINT('',(2.52258592029807,-2.6,9.77990594406283));
#139988=CARTESIAN_POINT('Origin',(2.72239470606247,-2.6,10.5545519594346));
#139989=CARTESIAN_POINT('Origin',(9.00768359641396E-11,-2.6,2.56054600265843E-10));
#139990=CARTESIAN_POINT('',(-2.80540468711597,-2.6,9.70256175144017));
#139991=CARTESIAN_POINT('',(-2.80540468711597,-2.6,9.70256175144017));
#139992=CARTESIAN_POINT('Origin',(9.00768359641396E-11,-2.6,2.56054600265843E-10));
#139993=CARTESIAN_POINT('Origin',(-3.02761495937587,-2.6,10.4710814941288));
#139994=CARTESIAN_POINT('',(-3.82759827224048,-2.6,10.4762486150055));
#139995=CARTESIAN_POINT('',(-3.82759827224048,-2.6,10.4762486150055));
#139996=CARTESIAN_POINT('Origin',(-3.02761495937587,-2.6,10.4710814941288));
#139997=CARTESIAN_POINT('Origin',(-8.47750127826606,-2.6,10.5062825051013));
#139998=CARTESIAN_POINT('',(-6.99732981056662,-2.6,14.9144105007712));
#139999=CARTESIAN_POINT('',(-6.99732981056662,-2.6,14.9144105007712));
#140000=CARTESIAN_POINT('Origin',(-8.47750127826606,-2.6,10.5062825051013));
#140001=CARTESIAN_POINT('Origin',(-8.31993898771739,-1.,8.19662125500606));
#140002=CARTESIAN_POINT('Origin',(5.39067671315598,-1.4,15.8));
#140003=CARTESIAN_POINT('',(4.34802179419235,-1.4,16.2));
#140004=CARTESIAN_POINT('',(4.34802179419235,-1.,15.8));
#140005=CARTESIAN_POINT('Origin',(4.34802179419235,-1.4,15.8));
#140006=CARTESIAN_POINT('',(9.34289321881345,-1.,15.8));
#140007=CARTESIAN_POINT('',(5.39067671315598,-1.,15.8));
#140008=CARTESIAN_POINT('',(9.34289321881345,-1.4,16.2));
#140009=CARTESIAN_POINT('Origin',(9.34289321881345,-1.4,15.8));
#140010=CARTESIAN_POINT('',(5.39067671315598,-1.4,16.2));
#140011=CARTESIAN_POINT('Ctrl Pts',(9.34289321881345,-1.4,16.2));
#140012=CARTESIAN_POINT('Ctrl Pts',(9.94289321881345,-1.4,16.2));
#140013=CARTESIAN_POINT('Ctrl Pts',(9.94289321881345,-1.4,15.6));
#140014=CARTESIAN_POINT('Ctrl Pts',(9.34289321881345,-1.,16.2));
#140015=CARTESIAN_POINT('Ctrl Pts',(9.94289321881345,-1.,16.2));
#140016=CARTESIAN_POINT('Ctrl Pts',(9.94289321881345,-1.,15.6));
#140017=CARTESIAN_POINT('Ctrl Pts',(9.34289321881345,-1.,15.8));
#140018=CARTESIAN_POINT('Ctrl Pts',(9.54289321881345,-1.,15.8));
#140019=CARTESIAN_POINT('Ctrl Pts',(9.54289321881345,-1.,15.6));
#140020=CARTESIAN_POINT('',(9.54289321881345,-1.,15.6));
#140021=CARTESIAN_POINT('',(9.94289321881345,-1.4,15.6));
#140022=CARTESIAN_POINT('Origin',(9.54289321881345,-1.4,15.6));
#140023=CARTESIAN_POINT('Origin',(9.34289321881345,-1.4,15.6));
#140024=CARTESIAN_POINT('Origin',(9.34289321881345,-1.,15.6));
#140025=CARTESIAN_POINT('Origin',(9.54289321881345,-1.4,15.2521525008107));
#140026=CARTESIAN_POINT('',(9.54289321881345,-1.,13.7509759234611));
#140027=CARTESIAN_POINT('',(9.94289321881345,-1.4,13.7509759234611));
#140028=CARTESIAN_POINT('Origin',(9.54289321881345,-1.4,13.7509759234611));
#140029=CARTESIAN_POINT('',(9.94289321881345,-1.4,15.2521525008107));
#140030=CARTESIAN_POINT('',(9.54289321881345,-1.,15.2521525008107));
#140031=CARTESIAN_POINT('Ctrl Pts',(9.94289321881345,-1.4,13.7509759234611));
#140032=CARTESIAN_POINT('Ctrl Pts',(9.94289321881345,-1.4,13.39656921145));
#140033=CARTESIAN_POINT('Ctrl Pts',(9.63250676288208,-1.4,13.2255009049379));
#140034=CARTESIAN_POINT('Ctrl Pts',(9.32212030695072,-1.4,13.0544325984258));
#140035=CARTESIAN_POINT('Ctrl Pts',(9.0224799018401,-1.4,13.243693648681));
#140036=CARTESIAN_POINT('Ctrl Pts',(9.94289321881345,-1.,13.7509759234611));
#140037=CARTESIAN_POINT('Ctrl Pts',(9.94289321881345,-1.,13.39656921145));
#140038=CARTESIAN_POINT('Ctrl Pts',(9.63250676288208,-1.,13.2255009049379));
#140039=CARTESIAN_POINT('Ctrl Pts',(9.32212030695072,-1.,13.0544325984258));
#140040=CARTESIAN_POINT('Ctrl Pts',(9.0224799018401,-1.,13.243693648681));
#140041=CARTESIAN_POINT('Ctrl Pts',(9.54289321881345,-1.,13.7509759234611));
#140042=CARTESIAN_POINT('Ctrl Pts',(9.54289321881345,-1.,13.6328403527907));
#140043=CARTESIAN_POINT('Ctrl Pts',(9.43943106683633,-1.,13.5758175839534));
#140044=CARTESIAN_POINT('Ctrl Pts',(9.3359689148592,-1.,13.518794815116));
#140045=CARTESIAN_POINT('Ctrl Pts',(9.23608877982233,-1.,13.5818818318677));
#140046=CARTESIAN_POINT('',(9.23608877982233,-1.,13.5818818318677));
#140047=CARTESIAN_POINT('',(9.0224799018401,-1.4,13.243693648681));
#140048=CARTESIAN_POINT('Origin',(9.23608877982233,-1.4,13.5818818318677));
#140049=CARTESIAN_POINT('Origin',(9.34289321881345,-1.4,13.7509759234611));
#140050=CARTESIAN_POINT('Origin',(9.34289321881345,-1.,13.7509759234611));
#140051=CARTESIAN_POINT('Origin',(7.1,-1.4,10.2));
#140052=CARTESIAN_POINT('',(5.02890240319562,-1.,13.6220687813823));
#140053=CARTESIAN_POINT('',(5.23601216287606,-1.4,13.279861903244));
#140054=CARTESIAN_POINT('Origin',(5.02890240319562,-1.4,13.6220687813823));
#140055=CARTESIAN_POINT('Origin',(7.1,-1.4,10.2));
#140056=CARTESIAN_POINT('Origin',(7.1,-1.,10.2));
#140057=CARTESIAN_POINT('Ctrl Pts',(5.23601216287606,-1.4,13.279861903244));
#140058=CARTESIAN_POINT('Ctrl Pts',(4.97614696981528,-1.4,13.1225868128749));
#140059=CARTESIAN_POINT('Ctrl Pts',(4.69555487551437,-1.4,13.2389201667807));
#140060=CARTESIAN_POINT('Ctrl Pts',(4.41496278121346,-1.4,13.3552535206864));
#140061=CARTESIAN_POINT('Ctrl Pts',(4.34261496676317,-1.4,13.6502639719579));
#140062=CARTESIAN_POINT('Ctrl Pts',(5.23601216287606,-1.,13.279861903244));
#140063=CARTESIAN_POINT('Ctrl Pts',(4.97614696981528,-1.,13.1225868128749));
#140064=CARTESIAN_POINT('Ctrl Pts',(4.69555487551437,-1.,13.2389201667807));
#140065=CARTESIAN_POINT('Ctrl Pts',(4.41496278121346,-1.,13.3552535206864));
#140066=CARTESIAN_POINT('Ctrl Pts',(4.34261496676317,-1.,13.6502639719579));
#140067=CARTESIAN_POINT('Ctrl Pts',(5.02890240319562,-1.,13.6220687813823));
#140068=CARTESIAN_POINT('Ctrl Pts',(4.94228067217536,-1.,13.5696437512592));
#140069=CARTESIAN_POINT('Ctrl Pts',(4.84874997407506,-1.,13.6084215358945));
#140070=CARTESIAN_POINT('Ctrl Pts',(4.75521927597476,-1.,13.6471993205297));
#140071=CARTESIAN_POINT('Ctrl Pts',(4.73110333782466,-1.,13.7455361376202));
#140072=CARTESIAN_POINT('',(4.73110333782466,-1.,13.7455361376202));
#140073=CARTESIAN_POINT('',(4.34261496676317,-1.4,13.6502639719579));
#140074=CARTESIAN_POINT('Origin',(4.73110333782466,-1.4,13.7455361376202));
#140075=CARTESIAN_POINT('Origin',(4.9253475233554,-1.4,13.7931722204514));
#140076=CARTESIAN_POINT('Origin',(4.9253475233554,-1.,13.7931722204514));
#140077=CARTESIAN_POINT('Origin',(-8.47750127826606,-1.4,10.5062825051013));
#140078=CARTESIAN_POINT('',(4.16214464821469,-1.,15.5261780073203));
#140079=CARTESIAN_POINT('',(3.79039035625937,-1.4,15.3785340219609));
#140080=CARTESIAN_POINT('Origin',(4.16214464821469,-1.4,15.5261780073203));
#140081=CARTESIAN_POINT('Origin',(-8.47750127826606,-1.4,10.5062825051013));
#140082=CARTESIAN_POINT('Origin',(-8.47750127826606,-1.,10.5062825051013));
#140083=CARTESIAN_POINT('Ctrl Pts',(3.79039035625937,-1.4,15.3785340219609));
#140084=CARTESIAN_POINT('Ctrl Pts',(3.67305500089253,-1.4,15.673973906285));
#140085=CARTESIAN_POINT('Ctrl Pts',(3.8515947669147,-1.4,15.9369869531425));
#140086=CARTESIAN_POINT('Ctrl Pts',(4.03013453293687,-1.4,16.2));
#140087=CARTESIAN_POINT('Ctrl Pts',(4.34802179419235,-1.4,16.2));
#140088=CARTESIAN_POINT('Ctrl Pts',(3.79039035625937,-0.999999999999999,
15.3785340219609));
#140089=CARTESIAN_POINT('Ctrl Pts',(3.67305500089253,-0.999999999999999,
15.673973906285));
#140090=CARTESIAN_POINT('Ctrl Pts',(3.8515947669147,-0.999999999999999,
15.9369869531425));
#140091=CARTESIAN_POINT('Ctrl Pts',(4.03013453293687,-0.999999999999999,
16.2));
#140092=CARTESIAN_POINT('Ctrl Pts',(4.34802179419235,-0.999999999999999,
16.2));
#140093=CARTESIAN_POINT('Ctrl Pts',(4.16214464821469,-1.,15.5261780073203));
#140094=CARTESIAN_POINT('Ctrl Pts',(4.12303286309241,-1.,15.6246579687617));
#140095=CARTESIAN_POINT('Ctrl Pts',(4.18254611843313,-1.,15.7123289843808));
#140096=CARTESIAN_POINT('Ctrl Pts',(4.24205937377385,-1.,15.8));
#140097=CARTESIAN_POINT('Ctrl Pts',(4.34802179419235,-1.,15.8));
#140098=CARTESIAN_POINT('Origin',(4.34802179419235,-1.4,15.6));
#140099=CARTESIAN_POINT('Origin',(4.34802179419235,-1.,15.6));
#140100=CARTESIAN_POINT('Origin',(4.9253475233554,-10.3,13.7931722204514));
#140101=CARTESIAN_POINT('',(4.34261496676317,-10.3,13.6502639719579));
#140102=CARTESIAN_POINT('',(4.34261496676317,-10.3,13.6502639719579));
#140103=CARTESIAN_POINT('',(5.23601216287606,-10.3,13.279861903244));
#140104=CARTESIAN_POINT('Origin',(4.9253475233554,-10.3,13.7931722204514));
#140105=CARTESIAN_POINT('',(5.23601216287606,-10.3,13.279861903244));
#140106=CARTESIAN_POINT('Origin',(-8.47750127826606,-10.3,10.5062825051013));
#140107=CARTESIAN_POINT('',(3.79039035625937,-10.3,15.3785340219609));
#140108=CARTESIAN_POINT('',(3.79039035625937,-10.3,15.3785340219609));
#140109=CARTESIAN_POINT('Origin',(-8.47750127826606,-10.3,10.5062825051013));
#140110=CARTESIAN_POINT('Origin',(4.34802179419235,-10.3,15.6));
#140111=CARTESIAN_POINT('',(4.34802179419235,-10.3,16.2));
#140112=CARTESIAN_POINT('',(4.34802179419235,-10.3,16.2));
#140113=CARTESIAN_POINT('Origin',(4.34802179419235,-10.3,15.6));
#140114=CARTESIAN_POINT('Origin',(3.87327121127015,-10.3,16.2));
#140115=CARTESIAN_POINT('',(9.34289321881345,-10.3,16.2));
#140116=CARTESIAN_POINT('',(9.34289321881345,-10.3,16.2));
#140117=CARTESIAN_POINT('',(1.93663560562379,-10.3,16.2));
#140118=CARTESIAN_POINT('Origin',(6.9080822150418,-1.,14.3043050016214));
#140119=CARTESIAN_POINT('Ctrl Pts',(-6.55757245707085,-7.39135402382937,
-5.14568636426237));
#140120=CARTESIAN_POINT('Ctrl Pts',(-6.75982089367161,-7.08279689100774,
-4.90112778377594));
#140121=CARTESIAN_POINT('Ctrl Pts',(-7.14201290222532,-6.4731824979059,
-4.38535750463086));
#140122=CARTESIAN_POINT('Ctrl Pts',(-7.56887561359513,-5.75729102255351,
-3.6687283197766));
#140123=CARTESIAN_POINT('Ctrl Pts',(-7.8920474790012,-5.32284996799027,
-3.00366070100896));
#140124=CARTESIAN_POINT('Ctrl Pts',(-8.06413796370095,-5.26314068500446,
-2.52167799537569));
#140125=CARTESIAN_POINT('Ctrl Pts',(-8.15634056422202,-5.39508785844239,
-2.13936273187432));
#140126=CARTESIAN_POINT('Ctrl Pts',(-8.19249518591845,-5.49079764276997,
-1.95623948829439));
#140127=CARTESIAN_POINT('Ctrl Pts',(-8.20848794733666,-5.54462134203543,
-1.86605338286933));
#140128=CARTESIAN_POINT('Ctrl Pts',(-6.59430671722206,-7.38479153604685,
-5.18370054092997));
#140129=CARTESIAN_POINT('Ctrl Pts',(-6.79566621980483,-7.07478422459138,
-4.93751456041579));
#140130=CARTESIAN_POINT('Ctrl Pts',(-7.17539501607384,-6.46212556707381,
-4.41814889099274));
#140131=CARTESIAN_POINT('Ctrl Pts',(-7.59517884839189,-5.74110238786913,
-3.69584015502338));
#140132=CARTESIAN_POINT('Ctrl Pts',(-7.91048502875434,-5.30205110155698,
-3.01914042655875));
#140133=CARTESIAN_POINT('Ctrl Pts',(-8.0839783182176,-5.24156135558239,
-2.52556156479809));
#140134=CARTESIAN_POINT('Ctrl Pts',(-8.18241342906123,-5.37510035618311,
-2.13771736365271));
#140135=CARTESIAN_POINT('Ctrl Pts',(-8.22157653308709,-5.47181651588286,
-1.95300235825357));
#140136=CARTESIAN_POINT('Ctrl Pts',(-8.2390509222775,-5.52617607587092,
-1.86220817076219));
#140137=CARTESIAN_POINT('Ctrl Pts',(-6.63595837298398,-7.34560921902525,
-5.26646136899686));
#140138=CARTESIAN_POINT('Ctrl Pts',(-6.83696744747848,-7.03490859729009,
-5.01596598714684));
#140139=CARTESIAN_POINT('Ctrl Pts',(-7.2145648216538,-6.4206676920658,-4.48700804201576));
#140140=CARTESIAN_POINT('Ctrl Pts',(-7.62626818611773,-5.69746584040132,
-3.74806941119204));
#140141=CARTESIAN_POINT('Ctrl Pts',(-7.93365762652132,-5.25679153997054,
-3.04563128053137));
#140142=CARTESIAN_POINT('Ctrl Pts',(-8.11137309037109,-5.19604966097288,
-2.52942016455644));
#140143=CARTESIAN_POINT('Ctrl Pts',(-8.21991249163311,-5.33007531761683,
-2.12876153722579));
#140144=CARTESIAN_POINT('Ctrl Pts',(-8.26402480718159,-5.42712564949736,
-1.93944532704854));
#140145=CARTESIAN_POINT('Ctrl Pts',(-8.28394949950606,-5.48167291123861,
-1.84665693304245));
#140146=CARTESIAN_POINT('Ctrl Pts',(-6.61728073072348,-7.27860819075006,
-5.33501354889539));
#140147=CARTESIAN_POINT('Ctrl Pts',(-6.82106903448059,-6.96941256165192,
-5.08222060797199));
#140148=CARTESIAN_POINT('Ctrl Pts',(-7.20417049462418,-6.35841500575385,
-4.54716168525424));
#140149=CARTESIAN_POINT('Ctrl Pts',(-7.62219974155008,-5.64034159634881,
-3.79386037188604));
#140150=CARTESIAN_POINT('Ctrl Pts',(-7.93630514231034,-5.20403706084519,
-3.06676953823316));
#140151=CARTESIAN_POINT('Ctrl Pts',(-8.12120138882497,-5.1440183658169,
-2.52725608769133));
#140152=CARTESIAN_POINT('Ctrl Pts',(-8.23556860403889,-5.27658630428028,
-2.11084110731329));
#140153=CARTESIAN_POINT('Ctrl Pts',(-8.2820116585493,-5.37269616280061,
-1.91519718281657));
#140154=CARTESIAN_POINT('Ctrl Pts',(-8.30297761570752,-5.42673591685656,
-1.81954222176521));
#140155=CARTESIAN_POINT('Ctrl Pts',(-6.59975017030691,-7.24993266759206,
-5.35661252001056));
#140156=CARTESIAN_POINT('Ctrl Pts',(-6.8050244734344,-6.94137553477043,
-5.10369911401669));
#140157=CARTESIAN_POINT('Ctrl Pts',(-7.19130954300827,-6.33176114166859,
-4.56771477257368));
#140158=CARTESIAN_POINT('Ctrl Pts',(-7.61421928816731,-5.6158696663162,
-3.8104955293341));
#140159=CARTESIAN_POINT('Ctrl Pts',(-7.93365040706529,-5.18142861175297,
-3.0744143426353));
#140160=CARTESIAN_POINT('Ctrl Pts',(-8.12203784210238,-5.12171932876715,
-2.52526953516964));
#140161=CARTESIAN_POINT('Ctrl Pts',(-8.23787448960478,-5.25366650220508,
-2.10202721872779));
#140162=CARTESIAN_POINT('Ctrl Pts',(-8.28468233453968,-5.34937628653266,
-1.90364658626372));
#140163=CARTESIAN_POINT('Ctrl Pts',(-8.30575868734589,-5.40319998579812,
-1.80675748997431));
#140164=CARTESIAN_POINT('',(-6.73177848765117,-7.12225772049266,-4.9282600804168));
#140165=CARTESIAN_POINT('',(-6.59975017049921,-7.24993266730301,-5.35661251977363));
#140166=CARTESIAN_POINT('Ctrl Pts',(-6.73176791483545,-7.12238125060388,
-4.92820584999411));
#140167=CARTESIAN_POINT('Ctrl Pts',(-6.73291165817144,-7.12938693500352,
-4.94184209885323));
#140168=CARTESIAN_POINT('Ctrl Pts',(-6.73358004363714,-7.13594979039427,
-4.95571899778471));
#140169=CARTESIAN_POINT('Ctrl Pts',(-6.73375401539604,-7.14213917334584,
-4.96978923814906));
#140170=CARTESIAN_POINT('Ctrl Pts',(-6.73399096594941,-7.1505691491342,
-4.98895298783715));
#140171=CARTESIAN_POINT('Ctrl Pts',(-6.7333094802454,-7.15824588042621,
-5.00833307284922));
#140172=CARTESIAN_POINT('Ctrl Pts',(-6.73168615754098,-7.16532994738964,
-5.02780762926736));
#140173=CARTESIAN_POINT('Ctrl Pts',(-6.72999471031469,-7.17271130501096,
-5.04809945685464));
#140174=CARTESIAN_POINT('Ctrl Pts',(-6.72728147209107,-7.17944881713203,
-5.06849489905558));
#140175=CARTESIAN_POINT('Ctrl Pts',(-6.72349592319277,-7.18568153871056,
-5.08888655201071));
#140176=CARTESIAN_POINT('Ctrl Pts',(-6.7196452262645,-7.19202152334213,
-5.10962913849061));
#140177=CARTESIAN_POINT('Ctrl Pts',(-6.71468577087202,-7.19783862981343,
-5.1303691323216));
#140178=CARTESIAN_POINT('Ctrl Pts',(-6.70852834943669,-7.20324367517375,
-5.15100588876705));
#140179=CARTESIAN_POINT('Ctrl Pts',(-6.70717535709377,-7.20443134521752,
-5.1555404774332));
#140180=CARTESIAN_POINT('Ctrl Pts',(-6.70576436140481,-7.20559900428378,
-5.16007008359584));
#140181=CARTESIAN_POINT('Ctrl Pts',(-6.70429412847365,-7.20674764453472,
-5.16459361682719));
#140182=CARTESIAN_POINT('Ctrl Pts',(-6.70322323205129,-7.20758429749579,
-5.16788849306837));
#140183=CARTESIAN_POINT('Ctrl Pts',(-6.70212287726058,-7.2084093020696,
-5.17117411068902));
#140184=CARTESIAN_POINT('Ctrl Pts',(-6.70099292278369,-7.2092231196394,
-5.17444999841023));
#140185=CARTESIAN_POINT('Ctrl Pts',(-6.69378551829264,-7.21441404770547,
-5.19534521884339));
#140186=CARTESIAN_POINT('Ctrl Pts',(-6.68537758112975,-7.21915261740078,
-5.21584416659399));
#140187=CARTESIAN_POINT('Ctrl Pts',(-6.67585574084893,-7.22361502853928,
-5.23585192639533));
#140188=CARTESIAN_POINT('Ctrl Pts',(-6.66582683814292,-7.22831507452013,
-5.25692515074012));
#140189=CARTESIAN_POINT('Ctrl Pts',(-6.65456230470562,-7.2327077631601,
-5.27745486626376));
#140190=CARTESIAN_POINT('Ctrl Pts',(-6.64211215477387,-7.23696957402667,
-5.29732416150095));
#140191=CARTESIAN_POINT('Ctrl Pts',(-6.62966200484213,-7.24123138489323,
-5.31719345673814));
#140192=CARTESIAN_POINT('Ctrl Pts',(-6.61602588604064,-7.24536099521506,
-5.33640382478608));
#140193=CARTESIAN_POINT('Ctrl Pts',(-6.60120676753226,-7.2495243906536,
-5.3548105998295));
#140194=CARTESIAN_POINT('Ctrl Pts',(-6.6007224198111,-7.2496604669723,-5.35541220643256));
#140195=CARTESIAN_POINT('Ctrl Pts',(-6.60023688716911,-7.24979655733683,
-5.35601284816904));
#140196=CARTESIAN_POINT('Ctrl Pts',(-6.59975017030691,-7.24993266759206,
-5.35661252001056));
#140197=CARTESIAN_POINT('',(-8.30575868734442,-5.40319998579812,-1.80675748998109));
#140198=CARTESIAN_POINT('Ctrl Pts',(-6.59975017030691,-7.24993266759206,
-5.35661252001056));
#140199=CARTESIAN_POINT('Ctrl Pts',(-6.8050244734344,-6.94137553477043,
-5.10369911401669));
#140200=CARTESIAN_POINT('Ctrl Pts',(-7.19130954300827,-6.33176114166859,
-4.56771477257368));
#140201=CARTESIAN_POINT('Ctrl Pts',(-7.61421928816731,-5.6158696663162,
-3.8104955293341));
#140202=CARTESIAN_POINT('Ctrl Pts',(-7.93365040706529,-5.18142861175297,
-3.0744143426353));
#140203=CARTESIAN_POINT('Ctrl Pts',(-8.12203784210238,-5.12171932876715,
-2.52526953516964));
#140204=CARTESIAN_POINT('Ctrl Pts',(-8.23787448960478,-5.25366650220508,
-2.10202721872779));
#140205=CARTESIAN_POINT('Ctrl Pts',(-8.28468233453968,-5.34937628653266,
-1.90364658626372));
#140206=CARTESIAN_POINT('Ctrl Pts',(-8.30575868734589,-5.40319998579812,
-1.80675748997431));
#140207=CARTESIAN_POINT('',(-8.20848794733666,-5.54462134203543,-1.86605338286933));
#140208=CARTESIAN_POINT('Origin',(-8.11032907117305,-5.40319998579812,-1.76424554903373));
#140209=CARTESIAN_POINT('Ctrl Pts',(-8.20848794733666,-5.54462134203543,
-1.86605338286933));
#140210=CARTESIAN_POINT('Ctrl Pts',(-8.19249518591845,-5.49079764276997,
-1.95623948829439));
#140211=CARTESIAN_POINT('Ctrl Pts',(-8.15634056422202,-5.39508785844239,
-2.13936273187432));
#140212=CARTESIAN_POINT('Ctrl Pts',(-8.06413796370095,-5.26314068500446,
-2.52167799537569));
#140213=CARTESIAN_POINT('Ctrl Pts',(-7.8920474790012,-5.32284996799027,
-3.00366070100896));
#140214=CARTESIAN_POINT('Ctrl Pts',(-7.56887561359513,-5.75729102255351,
-3.6687283197766));
#140215=CARTESIAN_POINT('Ctrl Pts',(-7.19183563386273,-6.38962479209568,
-4.30171369454974));
#140216=CARTESIAN_POINT('Ctrl Pts',(-6.87047660210866,-6.90569934085639,
-4.74940342070924));
#140217=CARTESIAN_POINT('Ctrl Pts',(-6.73179386229792,-7.12234071719252,
-4.92817240258013));
#140218=CARTESIAN_POINT('Ctrl Pts',(-8.20848794733648,-5.54462134203483,
-1.86605338287034));
#140219=CARTESIAN_POINT('Ctrl Pts',(-8.22570432892313,-5.60256313961292,
-1.76896705962691));
#140220=CARTESIAN_POINT('Ctrl Pts',(-8.30203822855091,-5.67885398422639,
-1.60363731207959));
#140221=CARTESIAN_POINT('Ctrl Pts',(-8.51961092920762,-5.69711542803795,
-1.45079338011714));
#140222=CARTESIAN_POINT('Ctrl Pts',(-8.66564229791336,-5.66327831149784,
-1.42362085501337));
#140223=CARTESIAN_POINT('Ctrl Pts',(-8.73598097951737,-5.63790797511633,
-1.42417566375139));
#140224=CARTESIAN_POINT('Ctrl Pts',(-8.26197315348204,-5.51234212624656,
-1.85932426168421));
#140225=CARTESIAN_POINT('Ctrl Pts',(-8.27437032427531,-5.56818098336045,
-1.77251643685663));
#140226=CARTESIAN_POINT('Ctrl Pts',(-8.3392891469759,-5.642057191414,-1.62376201038179));
#140227=CARTESIAN_POINT('Ctrl Pts',(-8.5321969224146,-5.65975617308337,
-1.4872628671831));
#140228=CARTESIAN_POINT('Ctrl Pts',(-8.66236637734033,-5.62701114347325,
-1.46459597020112));
#140229=CARTESIAN_POINT('Ctrl Pts',(-8.7247932961205,-5.6024788095447,-1.46627251165308));
#140230=CARTESIAN_POINT('Ctrl Pts',(-8.29926952018809,-5.45811715826701,
-1.8365885308239));
#140231=CARTESIAN_POINT('Ctrl Pts',(-8.31007945872644,-5.51489858344653,
-1.76137839707867));
#140232=CARTESIAN_POINT('Ctrl Pts',(-8.36725749645066,-5.58989957876681,
-1.63099116012873));
#140233=CARTESIAN_POINT('Ctrl Pts',(-8.53788390290437,-5.60786132493498,
-1.51041285785609));
#140234=CARTESIAN_POINT('Ctrl Pts',(-8.65267646235137,-5.57461521980001,
-1.49020536934065));
#140235=CARTESIAN_POINT('Ctrl Pts',(-8.70746447552891,-5.54969839474843,
-1.49152721040301));
#140236=CARTESIAN_POINT('Ctrl Pts',(-8.30575868734471,-5.40319998579752,
-1.80675748997975));
#140237=CARTESIAN_POINT('Ctrl Pts',(-8.32052873133615,-5.46114178337561,
-1.73885882518281));
#140238=CARTESIAN_POINT('Ctrl Pts',(-8.37815380678821,-5.53743262798908,
-1.62294165666584));
#140239=CARTESIAN_POINT('Ctrl Pts',(-8.53500933031641,-5.55569407180065,
-1.5139172416936));
#140240=CARTESIAN_POINT('Ctrl Pts',(-8.63932760832842,-5.52185695526053,
-1.49273142435505));
#140241=CARTESIAN_POINT('Ctrl Pts',(-8.6895496409325,-5.49648661887902,
-1.49184382745125));
#140242=CARTESIAN_POINT('',(-8.73598097951737,-5.63790797511633,-1.42417566375139));
#140243=CARTESIAN_POINT('Origin',(-8.68601550155451,-5.49648661887902,-1.29187505524205));
#140244=CARTESIAN_POINT('Ctrl Pts',(-8.73598097951737,-5.63790797511633,
-1.42417566375139));
#140245=CARTESIAN_POINT('Ctrl Pts',(-8.66564229791336,-5.66327831149784,
-1.42362085501337));
#140246=CARTESIAN_POINT('Ctrl Pts',(-8.51961092920762,-5.69711542803795,
-1.45079338011714));
#140247=CARTESIAN_POINT('Ctrl Pts',(-8.30203822855091,-5.67885398422639,
-1.60363731207959));
#140248=CARTESIAN_POINT('Ctrl Pts',(-8.22570432892313,-5.60256313961292,
-1.76896705962691));
#140249=CARTESIAN_POINT('Ctrl Pts',(-8.20848794733648,-5.54462134203483,
-1.86605338287034));
#140250=CARTESIAN_POINT('Ctrl Pts',(-8.30575868734471,-5.40319998579752,
-1.80675748997975));
#140251=CARTESIAN_POINT('Ctrl Pts',(-8.32052873133615,-5.46114178337561,
-1.73885882518281));
#140252=CARTESIAN_POINT('Ctrl Pts',(-8.37815380678821,-5.53743262798908,
-1.62294165666584));
#140253=CARTESIAN_POINT('Ctrl Pts',(-8.53500933031641,-5.55569407180065,
-1.5139172416936));
#140254=CARTESIAN_POINT('Ctrl Pts',(-8.63932760832842,-5.52185695526053,
-1.49273142435505));
#140255=CARTESIAN_POINT('Ctrl Pts',(-8.6895496409325,-5.49648661887902,
-1.49184382745125));
#140256=CARTESIAN_POINT('Ctrl Pts',(-8.73598097951772,-5.63790797511621,
-1.42417566375139));
#140257=CARTESIAN_POINT('Ctrl Pts',(-8.90608013788385,-5.5765552063756,
-1.42551735081822));
#140258=CARTESIAN_POINT('Ctrl Pts',(-9.2607737387321,-5.50597871763856,
-1.41691940563236));
#140259=CARTESIAN_POINT('Ctrl Pts',(-9.78761036667993,-5.6224253396905,
-1.35940353299553));
#140260=CARTESIAN_POINT('Ctrl Pts',(-10.7490450394837,-6.15724901285239,
-1.19114732392076));
#140261=CARTESIAN_POINT('Ctrl Pts',(-11.4346764894942,-6.81457717411039,
-1.0024272195599));
#140262=CARTESIAN_POINT('Ctrl Pts',(-11.9675786126161,-7.33643304648348,
-0.82348831362286));
#140263=CARTESIAN_POINT('Ctrl Pts',(-8.72958801757661,-5.61766273764671,
-1.4482310054095));
#140264=CARTESIAN_POINT('Ctrl Pts',(-8.90186687848093,-5.55573534105649,
-1.4479368219087));
#140265=CARTESIAN_POINT('Ctrl Pts',(-9.26239084548173,-5.48442219169093,
-1.43692373533481));
#140266=CARTESIAN_POINT('Ctrl Pts',(-9.79819135996713,-5.60204483004328,
-1.38216037519801));
#140267=CARTESIAN_POINT('Ctrl Pts',(-10.7695899593085,-6.14160038605648,
-1.2249245242093));
#140268=CARTESIAN_POINT('Ctrl Pts',(-11.4562523641124,-6.80244679525222,
-1.04191725589513));
#140269=CARTESIAN_POINT('Ctrl Pts',(-11.9907277518307,-7.32656702812379,
-0.865930760169916));
#140270=CARTESIAN_POINT('Ctrl Pts',(-8.71496589733162,-5.57251604392361,
-1.48117231511046));
#140271=CARTESIAN_POINT('Ctrl Pts',(-8.89218445918492,-5.51039924206827,
-1.47848223790221));
#140272=CARTESIAN_POINT('Ctrl Pts',(-9.26474568365955,-5.43887548480292,
-1.46396685256936));
#140273=CARTESIAN_POINT('Ctrl Pts',(-9.81889517320176,-5.55689222737881,
-1.41257201003397));
#140274=CARTESIAN_POINT('Ctrl Pts',(-10.8151018059367,-6.09806657044163,
-1.27028840934711));
#140275=CARTESIAN_POINT('Ctrl Pts',(-11.5087297589057,-6.76059811347898,
-1.09631471034077));
#140276=CARTESIAN_POINT('Ctrl Pts',(-12.0490661719394,-7.28572395405559,
-0.924516784598555));
#140277=CARTESIAN_POINT('Ctrl Pts',(-8.69722742718828,-5.51929166568008,
-1.49170813443058));
#140278=CARTESIAN_POINT('Ctrl Pts',(-8.88012225811069,-5.45771058941653,
-1.4883556607762));
#140279=CARTESIAN_POINT('Ctrl Pts',(-9.26595248827283,-5.38685152183972,
-1.47253893791997));
#140280=CARTESIAN_POINT('Ctrl Pts',(-9.83983744636612,-5.50376842165011,
-1.42058142214234));
#140281=CARTESIAN_POINT('Ctrl Pts',(-10.8642279877717,-6.04048923813472,
-1.27865017845492));
#140282=CARTESIAN_POINT('Ctrl Pts',(-11.5663403083829,-6.69937482262425,
-1.10351864069462));
#140283=CARTESIAN_POINT('Ctrl Pts',(-12.1123767090216,-7.22220505445906,
-0.929989202773578));
#140284=CARTESIAN_POINT('Ctrl Pts',(-8.68954964093266,-5.4964866188789,
-1.49184382745125));
#140285=CARTESIAN_POINT('Ctrl Pts',(-8.87481436092436,-5.43513385013829,
-1.4885695594993));
#140286=CARTESIAN_POINT('Ctrl Pts',(-9.26624052344372,-5.36455736140126,
-1.47266896725833));
#140287=CARTESIAN_POINT('Ctrl Pts',(-9.8483467388184,-5.48100398345319,
-1.41973709154106));
#140288=CARTESIAN_POINT('Ctrl Pts',(-10.8839646004455,-6.01582765661507,
-1.27510485735236));
#140289=CARTESIAN_POINT('Ctrl Pts',(-11.5886799961236,-6.67315581787308,
-1.09764645444795));
#140290=CARTESIAN_POINT('Ctrl Pts',(-12.1362808769477,-7.19501169024617,
-0.922336477447363));
#140291=CARTESIAN_POINT('',(-11.720329716163,-7.09759078643408,-0.903811780387333));
#140292=CARTESIAN_POINT('Ctrl Pts',(-12.1362808769477,-7.19501169024617,
-0.922336477447363));
#140293=CARTESIAN_POINT('Ctrl Pts',(-12.1356058178704,-7.1949090851414,
-0.92255259213136));
#140294=CARTESIAN_POINT('Ctrl Pts',(-12.1349303707403,-7.19480649116483,
-0.92276748566852));
#140295=CARTESIAN_POINT('Ctrl Pts',(-12.1342545392746,-7.19470390378757,
-0.922981158839793));
#140296=CARTESIAN_POINT('Ctrl Pts',(-12.1124520082791,-7.19139440343733,
-0.929874321079293));
#140297=CARTESIAN_POINT('Ctrl Pts',(-12.0903590888155,-7.18810662017071,
-0.935467523380962));
#140298=CARTESIAN_POINT('Ctrl Pts',(-12.0680949384848,-7.18469061225302,
-0.939801108152501));
#140299=CARTESIAN_POINT('Ctrl Pts',(-12.0461316693408,-7.18132076879709,
-0.944076128186122));
#140300=CARTESIAN_POINT('Ctrl Pts',(-12.0240005435959,-7.17782726878866,
-0.947125084551186));
#140301=CARTESIAN_POINT('Ctrl Pts',(-12.0018081000388,-7.17405656013424,
-0.948939718809822));
#140302=CARTESIAN_POINT('Ctrl Pts',(-11.9835242742012,-7.17094996305561,
-0.950434752768501));
#140303=CARTESIAN_POINT('Ctrl Pts',(-11.9651983957458,-7.16765532782976,
-0.951091096725075));
#140304=CARTESIAN_POINT('Ctrl Pts',(-11.9468945090915,-7.16407368887123,
-0.950881242320794));
#140305=CARTESIAN_POINT('Ctrl Pts',(-11.9365164786444,-7.16204295305734,
-0.950762258006794));
#140306=CARTESIAN_POINT('Ctrl Pts',(-11.9261456459944,-7.15991966508634,
-0.950364375632169));
#140307=CARTESIAN_POINT('Ctrl Pts',(-11.9157926875919,-7.15769064124147,
-0.949694791663599));
#140308=CARTESIAN_POINT('Ctrl Pts',(-11.8946462833602,-7.15313775525154,
-0.948327134930536));
#140309=CARTESIAN_POINT('Ctrl Pts',(-11.8738130426135,-7.14819787356317,
-0.945844033494343));
#140310=CARTESIAN_POINT('Ctrl Pts',(-11.8533514464485,-7.14276269857209,
-0.942352303314894));
#140311=CARTESIAN_POINT('Ctrl Pts',(-11.8333562318705,-7.13745140763763,
-0.938940160214053));
#140312=CARTESIAN_POINT('Ctrl Pts',(-11.8137150547943,-7.1316677042646,
-0.93456377027132));
#140313=CARTESIAN_POINT('Ctrl Pts',(-11.7945026420297,-7.12527752047938,
-0.929293324324193));
#140314=CARTESIAN_POINT('Ctrl Pts',(-11.7764881809649,-7.11928578386585,
-0.924351506527949));
#140315=CARTESIAN_POINT('Ctrl Pts',(-11.7588502247179,-7.11276106497496,
-0.918622782484977));
#140316=CARTESIAN_POINT('Ctrl Pts',(-11.7416771845018,-7.1055583986353,
-0.912152583906187));
#140317=CARTESIAN_POINT('Ctrl Pts',(-11.7346823377481,-7.10262464045215,
-0.909517171250373));
#140318=CARTESIAN_POINT('Ctrl Pts',(-11.7277649828676,-7.09957797351498,
-0.906758662971134));
#140319=CARTESIAN_POINT('Ctrl Pts',(-11.7209327506114,-7.09640666702022,
-0.903879959984334));
#140320=CARTESIAN_POINT('Ctrl Pts',(-11.7212088289358,-7.09667288316797,
-0.903792747022583));
#140321=CARTESIAN_POINT('Ctrl Pts',(-11.2647820308748,-6.65654480564138,
-1.04798290473443));
#140322=CARTESIAN_POINT('Ctrl Pts',(-10.6507952163715,-6.10259492893934,
-1.20834156836267));
#140323=CARTESIAN_POINT('Ctrl Pts',(-9.78761036667993,-5.6224253396905,
-1.35940353299553));
#140324=CARTESIAN_POINT('Ctrl Pts',(-9.2607737387321,-5.50597871763856,
-1.41691940563236));
#140325=CARTESIAN_POINT('Ctrl Pts',(-8.90608013788385,-5.5765552063756,
-1.42551735081822));
#140326=CARTESIAN_POINT('Ctrl Pts',(-8.73598097951772,-5.63790797511621,
-1.42417566375139));
#140327=CARTESIAN_POINT('Origin',(-8.69661791968849,4.20059847321333E-16,
-1.89178137186966));
#140328=CARTESIAN_POINT('',(-8.30575868734294,-2.6,-1.80675748998788));
#140329=CARTESIAN_POINT('',(-8.30575868734294,4.011807530597E-16,-1.80675748998788));
#140330=CARTESIAN_POINT('Origin',(-8.69661791968849,-2.6,-1.89178137186966));
#140331=CARTESIAN_POINT('Origin',(0.,0.,0.));
#140332=CARTESIAN_POINT('',(-6.59975017030735,-10.1,-5.35661252001003));
#140333=CARTESIAN_POINT('',(-6.59975017030735,-10.3,-5.35661252001003));
#140334=CARTESIAN_POINT('',(0.00347333261335205,-10.1,-8.49999929035314));
#140335=CARTESIAN_POINT('Origin',(0.,-10.1,-2.24265050974282E-15));
#140336=CARTESIAN_POINT('',(0.00347333261332719,-7.5,-8.49999929035059));
#140337=CARTESIAN_POINT('',(0.00347333261332719,1.88737898428894E-15,-8.49999929035059));
#140338=CARTESIAN_POINT('',(5.63796910874814,-7.5,-6.36107729310073));
#140339=CARTESIAN_POINT('Origin',(0.,-7.5,-1.66533453693773E-15));
#140340=CARTESIAN_POINT('',(6.27943617390152,-6.6,-5.72875914469243));
#140341=CARTESIAN_POINT('Ctrl Pts',(5.63796910874819,-7.49999999999993,
-6.36107729310069));
#140342=CARTESIAN_POINT('Ctrl Pts',(5.67409984605671,-7.45172701336858,
-6.32905378962232));
#140343=CARTESIAN_POINT('Ctrl Pts',(5.70986959776522,-7.40356504020207,
-6.29680055298516));
#140344=CARTESIAN_POINT('Ctrl Pts',(5.92847216942438,-7.10694555119756,
-6.09631105969112));
#140345=CARTESIAN_POINT('Ctrl Pts',(6.10772709056793,-6.85356360695371,
-5.9169737653527));
#140346=CARTESIAN_POINT('Ctrl Pts',(6.27943617390152,-6.6,-5.72875914469242));
#140347=CARTESIAN_POINT('',(8.44432226295358,-6.6,0.971298882623956));
#140348=CARTESIAN_POINT('Origin',(-7.2099444470286E-17,-6.6,-1.49003062450498E-15));
#140349=CARTESIAN_POINT('',(8.28947420569055,-7.5,1.88005781644903));
#140350=CARTESIAN_POINT('Ctrl Pts',(8.28947420569055,-7.5,1.88005781644903));
#140351=CARTESIAN_POINT('Ctrl Pts',(8.29772790894898,-7.46315114007885,
1.84366592484676));
#140352=CARTESIAN_POINT('Ctrl Pts',(8.30574546103206,-7.42632827323882,
1.8072042671372));
#140353=CARTESIAN_POINT('Ctrl Pts',(8.31352574751022,-7.3895345357671,1.77067491242312));
#140354=CARTESIAN_POINT('Ctrl Pts',(8.36906359788408,-7.12689059686646,
1.5099182112324));
#140355=CARTESIAN_POINT('Ctrl Pts',(8.41310047956988,-6.86272854589131,
1.24273623855277));
#140356=CARTESIAN_POINT('Ctrl Pts',(8.44432226295358,-6.6,0.971298882623954));
#140357=CARTESIAN_POINT('',(5.03883335853763,-7.5,6.8454480046881));
#140358=CARTESIAN_POINT('Origin',(0.,-7.5,-1.66533453693773E-15));
#140359=CARTESIAN_POINT('',(5.03883335853763,-10.3,6.8454480046881));
#140360=CARTESIAN_POINT('',(5.03883335853763,-4.81067232832666E-17,6.84544800468811));
#140361=CARTESIAN_POINT('',(5.03722331003166,-10.3,6.84663284577709));
#140362=CARTESIAN_POINT('Origin',(-7.2099444470286E-17,-10.3,-2.28766658394441E-15));
#140363=CARTESIAN_POINT('',(5.03722331003166,-2.6,6.84663284577709));
#140364=CARTESIAN_POINT('',(5.03722331003166,-2.6,6.84663284577709));
#140365=CARTESIAN_POINT('',(-8.5,-2.6,-1.61826575208033E-15));
#140366=CARTESIAN_POINT('Origin',(0.,-2.6,-5.77315972805081E-16));
#140367=CARTESIAN_POINT('',(-8.5,2.31137282485971E-31,-1.04094977927525E-15));
#140368=CARTESIAN_POINT('',(-8.5,2.31137282485971E-31,-1.04094977927525E-15));
#140369=CARTESIAN_POINT('Origin',(0.,0.,0.));
#140370=CARTESIAN_POINT('Origin',(0.,-2.6,-5.77315972805081E-16));
#140371=CARTESIAN_POINT('Origin',(-9.35,-6.25,-3.05000000003699));
#140372=CARTESIAN_POINT('Ctrl Pts',(-11.5368071934914,-7.05,-0.782760643794657));
#140373=CARTESIAN_POINT('Ctrl Pts',(-11.5844488890167,-7.05,-0.828712211368656));
#140374=CARTESIAN_POINT('Ctrl Pts',(-11.6417386809522,-7.06395036419954,
-0.867768806826326));
#140375=CARTESIAN_POINT('Ctrl Pts',(-11.7073160840573,-7.09173525292199,
-0.898191855681428));
#140376=CARTESIAN_POINT('Ctrl Pts',(-11.71381758951,-7.09460545954183,-0.901067364263082));
#140377=CARTESIAN_POINT('Ctrl Pts',(-11.720329716163,-7.09759078643408,
-0.903811780387334));
#140378=CARTESIAN_POINT('Ctrl Pts',(-6.73177848765117,-7.12225772049266,
-4.9282600804168));
#140379=CARTESIAN_POINT('Ctrl Pts',(-6.72976354048857,-7.10991695334985,
-4.90428006259042));
#140380=CARTESIAN_POINT('Ctrl Pts',(-6.72623571781636,-7.09867178972273,
-4.87972758418512));
#140381=CARTESIAN_POINT('Ctrl Pts',(-6.7076526749211,-7.06395036419954,
-4.79132127310591));
#140382=CARTESIAN_POINT('Ctrl Pts',(-6.68250369548387,-7.05,-4.72670651672613));
#140383=CARTESIAN_POINT('Ctrl Pts',(-6.64846378001877,-7.05,-4.66993890386316));
#140384=CARTESIAN_POINT('Origin',(-16.1000000000146,-2.6,0.725816604289514));
#140385=CARTESIAN_POINT('',(-16.5000000000146,-10.1,0.725816604290266));
#140386=CARTESIAN_POINT('Origin',(-16.1000000000146,-10.1,0.725816604289513));
#140387=CARTESIAN_POINT('',(-16.5000000000146,-2.6,0.725816604290267));
#140388=CARTESIAN_POINT('Origin',(-16.1000000000146,-2.6,0.725816604289514));
#140389=CARTESIAN_POINT('',(-16.5000000000146,-2.6,0.725816604290267));
#140390=CARTESIAN_POINT('Origin',(-15.7415106627401,-10.1,-2.75165772610856));
#140391=CARTESIAN_POINT('',(-16.5000000000305,-10.1,-7.71862915012594));
#140392=CARTESIAN_POINT('',(-16.5000000000167,-10.1,-0.400828863065334));
#140393=CARTESIAN_POINT('',(-16.7343145750813,-10.1,-8.28431457507367));
#140394=CARTESIAN_POINT('Origin',(-17.3000000000305,-10.1,-7.71862915012444));
#140395=CARTESIAN_POINT('',(-17.8000000000336,-10.1,-9.35000000002598));
#140396=CARTESIAN_POINT('',(-15.7571789150852,-10.1,-7.30717891507761));
#140397=CARTESIAN_POINT('',(-16.6686291501351,-10.1,-10.4813708499245));
#140398=CARTESIAN_POINT('',(-17.8000000000336,-10.1,-9.35000000002598));
#140399=CARTESIAN_POINT('',(-15.1343145750825,-10.1,-8.94705627487187));
#140400=CARTESIAN_POINT('',(-15.691493490136,-10.1,-9.50423518992531));
#140401=CARTESIAN_POINT('Origin',(-15.7000000000318,-10.1,-8.38137084992263));
#140402=CARTESIAN_POINT('Origin',(-11.9533418970136,-10.1,-0.350905528319928));
#140403=CARTESIAN_POINT('Origin',(-16.5000000000123,-24.4,1.94999999997646));
#140404=CARTESIAN_POINT('',(-16.4999999999955,-2.6,10.8686291501049));
#140405=CARTESIAN_POINT('',(-16.4999999999949,-2.6,11.2000000000031));
#140406=CARTESIAN_POINT('',(-16.4999999999955,-3.44027676348872E-15,10.8686291501049));
#140407=CARTESIAN_POINT('',(-16.4999999999955,-24.4,10.8686291501049));
#140408=CARTESIAN_POINT('',(-16.5000000000305,6.86923662425558E-16,-7.71862915012594));
#140409=CARTESIAN_POINT('',(-16.5000000000059,-2.22044604925031E-15,5.37500000000578));
#140410=CARTESIAN_POINT('',(-16.5000000000305,-24.4,-7.71862915012594));
#140411=CARTESIAN_POINT('Origin',(11.2581254575403,-10.3,-18.3));
#140412=CARTESIAN_POINT('',(11.8728253843338,-10.3,-17.788));
#140413=CARTESIAN_POINT('',(11.2581254575403,-10.3,-19.1000000000102));
#140414=CARTESIAN_POINT('Origin',(11.2581254575403,-10.3,-18.3));
#140415=CARTESIAN_POINT('',(11.2581254575403,-7.5,-19.1));
#140416=CARTESIAN_POINT('',(11.2581254575403,-10.3,-19.1));
#140417=CARTESIAN_POINT('',(11.8728253843338,-7.5,-17.788));
#140418=CARTESIAN_POINT('Origin',(11.2581254575403,-7.5,-18.3));
#140419=CARTESIAN_POINT('',(11.8728253843338,-10.3,-17.788));
#140420=CARTESIAN_POINT('Origin',(-2.25730545366787E-11,-10.3,-0.450000000022575));
#140421=CARTESIAN_POINT('',(10.9,-10.3,-15.1));
#140422=CARTESIAN_POINT('Origin',(15.1,-10.3,-15.1));
#140423=CARTESIAN_POINT('',(10.9,-10.3,-13.800000000037));
#140424=CARTESIAN_POINT('',(10.9,-10.3,-11.6000000000162));
#140425=CARTESIAN_POINT('',(10.5,-10.3,-13.400000000037));
#140426=CARTESIAN_POINT('Origin',(10.5,-10.3,-13.800000000037));
#140427=CARTESIAN_POINT('',(5.24999999998871,-10.3,-13.400000000037));
#140428=CARTESIAN_POINT('',(-0.796199698700571,-10.3,-9.30032612545083));
#140429=CARTESIAN_POINT('Origin',(0.00380023450634744,-10.3,-9.29999922356006));
#140430=CARTESIAN_POINT('',(-0.79309436390975,-10.3,-16.899754823607));
#140431=CARTESIAN_POINT('',(-0.797984158749954,-10.3,-4.93336481758792));
#140432=CARTESIAN_POINT('',(-1.39309431381607,-10.3,-17.5000000000267));
#140433=CARTESIAN_POINT('Origin',(-1.39309431381685,-10.3,-16.9000000000267));
#140434=CARTESIAN_POINT('',(-11.9672956534841,-10.3,-17.5000000000405));
#140435=CARTESIAN_POINT('',(-0.39642454364202,-10.3,-17.5000000000254));
#140436=CARTESIAN_POINT('',(-12.5250910766189,-10.3,-16.6789473684552));
#140437=CARTESIAN_POINT('Origin',(-11.9672956534849,-10.3,-16.9000000000405));
#140438=CARTESIAN_POINT('Origin',(-15.5,-10.3,-15.5));
#140439=CARTESIAN_POINT('',(-13.9781746176887,-10.3,-12.419231543135));
#140440=CARTESIAN_POINT('Origin',(-9.35,-10.3,-3.05000000003699));
#140441=CARTESIAN_POINT('',(-14.5846229736965,-10.3,-12.1880260147795));
#140442=CARTESIAN_POINT('Origin',(-15.5,-10.3,-15.5));
#140443=CARTESIAN_POINT('',(-15.0612959521201,-10.3,-12.3302147141527));
#140444=CARTESIAN_POINT('Origin',(-14.9790389431426,-10.3,-11.7358799730564));
#140445=CARTESIAN_POINT('',(-16.4600000000227,-10.3,-12.4473945554729));
#140446=CARTESIAN_POINT('Origin',(-15.5,-10.3,-15.5));
#140447=CARTESIAN_POINT('',(-17.5000000000283,-10.3,-11.6842431943471));
#140448=CARTESIAN_POINT('Origin',(-16.7000000000283,-10.3,-11.6842431943411));
#140449=CARTESIAN_POINT('',(-17.5000000000286,-10.3,-11.6441125497224));
#140450=CARTESIAN_POINT('',(-17.5,-10.3,-15.4999999999881));
#140451=CARTESIAN_POINT('',(-17.2656854249779,-10.3,-11.0784271247672));
#140452=CARTESIAN_POINT('Origin',(-16.7000000000286,-10.3,-11.6441125497165));
#140453=CARTESIAN_POINT('',(-16.6686291501351,-10.3,-10.4813708499245));
#140454=CARTESIAN_POINT('',(-17.5000000000311,-10.3,-11.3127416998205));
#140455=CARTESIAN_POINT('',(-17.8000000000336,-10.3,-9.35000000002598));
#140456=CARTESIAN_POINT('',(-15.0093145750824,-10.3,-12.1406854249771));
#140457=CARTESIAN_POINT('',(-18.8656854249492,-10.3,-10.4156854249416));
#140458=CARTESIAN_POINT('',(-16.5000000000311,-10.3,-8.05000000002353));
#140459=CARTESIAN_POINT('',(-19.1,-10.3,-10.9813708498909));
#140460=CARTESIAN_POINT('Origin',(-18.3,-10.3,-10.9813708498909));
#140461=CARTESIAN_POINT('',(-19.1,-10.3,-15.5));
#140462=CARTESIAN_POINT('',(-19.1,-10.3,4.01764068713489));
#140463=CARTESIAN_POINT('',(-15.5,-10.3,-19.1000000000451));
#140464=CARTESIAN_POINT('Origin',(-15.5,-10.3,-15.5));
#140465=CARTESIAN_POINT('',(-15.5,-10.3,-19.1000000000451));
#140466=CARTESIAN_POINT('',(-17.1,-10.3,-15.5));
#140467=CARTESIAN_POINT('Origin',(-15.5,-10.3,-15.5));
#140468=CARTESIAN_POINT('Origin',(15.1,-10.3,-15.1));
#140469=CARTESIAN_POINT('',(10.9,-7.5,-15.1));
#140470=CARTESIAN_POINT('Origin',(15.1,-7.5,-15.1));
#140471=CARTESIAN_POINT('',(10.9,-10.3,-15.1));
#140472=CARTESIAN_POINT('Origin',(13.1,-7.5,-1.80000000000345));
#140473=CARTESIAN_POINT('',(15.1,-7.5,-19.1));
#140474=CARTESIAN_POINT('',(-1.2,-7.5,-19.1));
#140475=CARTESIAN_POINT('',(19.1,-7.5,-15.1));
#140476=CARTESIAN_POINT('Origin',(15.1,-7.5,-15.1));
#140477=CARTESIAN_POINT('',(19.1,-7.5,-10.9813708499319));
#140478=CARTESIAN_POINT('',(19.1,-7.5,-10.4500000000017));
#140479=CARTESIAN_POINT('',(18.8656854249492,-7.5,-10.4156854249827));
#140480=CARTESIAN_POINT('Origin',(18.3,-7.5,-10.9813708499319));
#140481=CARTESIAN_POINT('',(16.734314575042,-7.5,-8.28431457507544));
#140482=CARTESIAN_POINT('',(16.4999999999906,-7.5,-8.05000000002406));
#140483=CARTESIAN_POINT('',(16.4999999999912,-7.5,-7.7186291501247));
#140484=CARTESIAN_POINT('Origin',(17.2999999999912,-7.5,-7.71862915012621));
#140485=CARTESIAN_POINT('',(16.4999999999931,-7.5,-6.72119489704348));
#140486=CARTESIAN_POINT('',(16.5000000000094,-7.5,1.94999999997594));
#140487=CARTESIAN_POINT('',(11.3899837160979,-7.5,-7.45800064600289));
#140488=CARTESIAN_POINT('Origin',(15.1,-7.5,-15.1));
#140489=CARTESIAN_POINT('Origin',(9.25,-7.5,-3.05000000003699));
#140490=CARTESIAN_POINT('Origin',(0.00380023450634622,-7.5,-9.29999922356006));
#140491=CARTESIAN_POINT('',(1.32237339244619,-7.5,-9.60943957263028));
#140492=CARTESIAN_POINT('Origin',(1.4041696846368,-7.5,-10.2038378957974));
#140493=CARTESIAN_POINT('',(5.41419360512517,-7.5,-8.0483854216423));
#140494=CARTESIAN_POINT('Origin',(-5.6920614055489E-17,-7.5,-1.53860044684792E-15));
#140495=CARTESIAN_POINT('',(6.14689326954821,-7.5,-8.09705302340923));
#140496=CARTESIAN_POINT('Origin',(5.74909217812359,-7.5,-8.54622369438117));
#140497=CARTESIAN_POINT('',(7.33287671232876,-7.5,-8.80342937459372));
#140498=CARTESIAN_POINT('Origin',(8.6,-7.5,-5.32716721908225));
#140499=CARTESIAN_POINT('Origin',(6.1,-7.5,-12.1857384988752));
#140500=CARTESIAN_POINT('',(10.5,-7.5,-13.400000000037));
#140501=CARTESIAN_POINT('',(9.25,-7.5,-13.400000000037));
#140502=CARTESIAN_POINT('',(10.9,-7.5,-13.800000000037));
#140503=CARTESIAN_POINT('Origin',(10.5,-7.5,-13.800000000037));
#140504=CARTESIAN_POINT('',(10.9,-7.5,-8.45000000000173));
#140505=CARTESIAN_POINT('',(15.1343145750407,-7.5,-8.94705627487115));
#140506=CARTESIAN_POINT('',(14.89999999999,-7.5,-8.3813708499204));
#140507=CARTESIAN_POINT('Origin',(15.69999999999,-7.5,-8.38137084992191));
#140508=CARTESIAN_POINT('',(14.8999999999893,-7.5,-8.71274169981976));
#140509=CARTESIAN_POINT('',(10.2965705850743,-7.5,-8.34761172707562));
#140510=CARTESIAN_POINT('Origin',(10.4128562056381,-7.5,-8.93623525230213));
#140511=CARTESIAN_POINT('',(11.608349401414,-7.5,-7.90779663028513));
#140512=CARTESIAN_POINT('Origin',(9.25,-7.5,-3.05000000003699));
#140513=CARTESIAN_POINT('',(13.9888110834979,-7.5,-7.18263475607025));
#140514=CARTESIAN_POINT('Origin',(15.1,-7.5,-15.1));
#140515=CARTESIAN_POINT('',(14.8999999999907,-7.5,-7.9748702165563));
#140516=CARTESIAN_POINT('Origin',(14.0999999999907,-7.5,-7.97487021655479));
#140517=CARTESIAN_POINT('',(14.9000000000107,-7.5,2.61274169977414));
#140518=CARTESIAN_POINT('',(13.55,-7.5,-15.1));
#140519=CARTESIAN_POINT('Origin',(15.1,-7.5,-15.1));
#140520=CARTESIAN_POINT('Origin',(-15.5,4.2410519540681E-15,-19.1));
#140521=CARTESIAN_POINT('',(-15.5,4.24105195407812E-15,-19.1000000000451));
#140522=CARTESIAN_POINT('',(-15.5,4.24105195407812E-15,-19.1000000000451));
#140523=CARTESIAN_POINT('',(15.1,4.2410519540681E-15,-19.1));
#140524=CARTESIAN_POINT('',(-69.9000013262034,4.2410519540681E-15,-19.1));
#140525=CARTESIAN_POINT('',(15.1,4.2410519540681E-15,-19.1));
#140526=CARTESIAN_POINT('Origin',(18.3,-12.2,-10.9813708499319));
#140527=CARTESIAN_POINT('',(19.1,2.43835415190839E-15,-10.9813708499319));
#140528=CARTESIAN_POINT('',(19.1,-12.2,-10.9813708499319));
#140529=CARTESIAN_POINT('',(18.8656854249492,1.57444844383239E-15,-10.4156854249827));
#140530=CARTESIAN_POINT('Origin',(18.3,2.22044604925031E-15,-10.9813708499319));
#140531=CARTESIAN_POINT('',(18.8656854249492,-12.2,-10.4156854249827));
#140532=CARTESIAN_POINT('Origin',(19.1,-24.4,-10.6500000000335));
#140533=CARTESIAN_POINT('',(16.734314575042,1.101189045516E-15,-8.28431457507544));
#140534=CARTESIAN_POINT('',(11.7749999999916,0.,-3.3250000000251));
#140535=CARTESIAN_POINT('',(16.734314575042,-24.4,-8.28431457507545));
#140536=CARTESIAN_POINT('Origin',(-2.25752749827279E-11,9.99200722212761E-17,
-0.450000000022572));
#140537=CARTESIAN_POINT('',(19.1,3.35287353436797E-15,-15.1));
#140538=CARTESIAN_POINT('',(19.1,4.2410519540681E-15,-19.1));
#140539=CARTESIAN_POINT('Origin',(15.1,3.35287353436797E-15,-15.1));
#140540=CARTESIAN_POINT('',(-19.1,4.33378681544358E-15,-15.5));
#140541=CARTESIAN_POINT('Origin',(-15.5,3.44169137633798E-15,-15.5));
#140542=CARTESIAN_POINT('',(-19.1,3.33044959100488E-15,-10.9813708498909));
#140543=CARTESIAN_POINT('',(-19.1,0.,4.0176406871349));
#140544=CARTESIAN_POINT('',(-18.8656854249492,1.86310643022669E-15,-10.4156854249416));
#140545=CARTESIAN_POINT('Origin',(-18.3,4.44089209850063E-15,-10.9813708498909));
#140546=CARTESIAN_POINT('',(-16.7343145750813,1.38984703191903E-15,-8.28431457507367));
#140547=CARTESIAN_POINT('',(-10.4750000000288,0.,-2.02500000002115));
#140548=CARTESIAN_POINT('Origin',(-17.3000000000305,0.,-7.71862915012443));
#140549=CARTESIAN_POINT('',(-16.2656854249441,-5.7894794125451E-15,11.4343145750533));
#140550=CARTESIAN_POINT('Origin',(-15.6999999999955,0.,10.8686291501034));
#140551=CARTESIAN_POINT('',(-9.73431457503237,-7.23973507252925E-15,17.9656854249499));
#140552=CARTESIAN_POINT('',(-12.3391827499422,-6.66133814775094E-15,15.3608172500461));
#140553=CARTESIAN_POINT('',(-9.16862915008379,-4.04121180963557E-15,18.2));
#140554=CARTESIAN_POINT('Origin',(-9.16862915008379,-4.44089209850063E-15,
17.4));
#140555=CARTESIAN_POINT('',(11.5427649064299,-4.04121180963557E-15,18.2));
#140556=CARTESIAN_POINT('',(-11.2907461519216,-4.04121180963557E-15,18.2));
#140557=CARTESIAN_POINT('',(12.6059538781827,-4.13252265231712E-15,18.6112274770755));
#140558=CARTESIAN_POINT('Origin',(11.5427649064299,-4.39204228541712E-15,
19.78));
#140559=CARTESIAN_POINT('',(17.0909902576697,-4.10898067127859E-15,18.5052038200428));
#140560=CARTESIAN_POINT('Origin',(14.7928932188134,-3.59870062220636E-15,
16.2071067811865));
#140561=CARTESIAN_POINT('',(18.5052038200428,-3.79496217954183E-15,17.0909902576697));
#140562=CARTESIAN_POINT('',(18.5052038200428,-3.79496217954183E-15,17.0909902576697));
#140563=CARTESIAN_POINT('',(19.3750857890412,-3.1235797785265E-15,14.067352726634));
#140564=CARTESIAN_POINT('Origin',(16.2071067811865,-3.28468213046961E-15,
14.7928932188135));
#140565=CARTESIAN_POINT('',(19.1,-2.58326727508653E-15,11.6340015374781));
#140566=CARTESIAN_POINT('Origin',(30.,-2.58326727508653E-15,11.6340015374781));
#140567=CARTESIAN_POINT('',(19.1,-1.08388206185084E-15,4.88137084986501));
#140568=CARTESIAN_POINT('',(19.1,4.2410519540681E-15,-19.1));
#140569=CARTESIAN_POINT('',(18.8656854249492,-1.57444844383014E-15,4.31568542491578));
#140570=CARTESIAN_POINT('Origin',(18.3,-2.22044604925031E-15,4.88137084986501));
#140571=CARTESIAN_POINT('',(16.7343145750595,-1.10118904551765E-15,2.18431457502608));
#140572=CARTESIAN_POINT('',(11.7750000000018,0.,-2.77500000003168));
#140573=CARTESIAN_POINT('',(16.5000000000088,-1.30309744108929E-15,1.61862915007835));
#140574=CARTESIAN_POINT('Origin',(17.3000000000088,0.,1.61862915007684));
#140575=CARTESIAN_POINT('',(16.4999999999912,7.70190389262261E-16,-7.7186291501247));
#140576=CARTESIAN_POINT('',(16.4999999999977,0.,-4.25000000003884));
#140577=CARTESIAN_POINT('Origin',(17.2999999999912,0.,-7.7186291501262));
#140578=CARTESIAN_POINT('',(17.338477631085,-3.53589692385901E-15,15.9242640687119));
#140579=CARTESIAN_POINT('',(15.9242640687119,-3.84991541559577E-15,17.338477631085));
#140580=CARTESIAN_POINT('',(16.3903174593052,-3.74643077460751E-15,16.8724242404918));
#140581=CARTESIAN_POINT('',(13.661522368915,-3.34748582881696E-15,15.0757359312881));
#140582=CARTESIAN_POINT('Origin',(14.7928932188134,-3.59870062220636E-15,
16.2071067811865));
#140583=CARTESIAN_POINT('',(15.0757359312881,-3.0334673370802E-15,13.661522368915));
#140584=CARTESIAN_POINT('',(14.8346825406948,-3.08699194196033E-15,13.9025757595082));
#140585=CARTESIAN_POINT('Origin',(16.2071067811865,-3.28468213046961E-15,
14.7928932188135));
#140586=CARTESIAN_POINT('',(-17.1,3.44169137633798E-15,-15.5));
#140587=CARTESIAN_POINT('Origin',(-15.5,3.44169137633798E-15,-15.5));
#140588=CARTESIAN_POINT('',(13.55,3.35287353436797E-15,-15.1));
#140589=CARTESIAN_POINT('Origin',(15.1,3.35287353436797E-15,-15.1));
#140590=CARTESIAN_POINT('',(-11.5275012782661,-2.33286334807598E-15,10.5062825051013));
#140591=CARTESIAN_POINT('Origin',(-8.47750127826606,-2.33286334807598E-15,
10.5062825051013));
#140592=CARTESIAN_POINT('Origin',(17.2999999999912,-24.4,-7.71862915012621));
#140593=CARTESIAN_POINT('',(16.4999999999912,-24.4,-7.7186291501247));
#140594=CARTESIAN_POINT('Origin',(16.4999999999906,-24.4,-8.05000000002406));
#140595=CARTESIAN_POINT('',(16.5000000000088,-6.6,1.61862915007835));
#140596=CARTESIAN_POINT('',(16.5000000000088,-24.4,1.61862915007834));
#140597=CARTESIAN_POINT('',(16.4999999999948,-6.6,-5.80993508719201));
#140598=CARTESIAN_POINT('',(16.5000000000094,-6.6,1.94999999997594));
#140599=CARTESIAN_POINT('Ctrl Pts',(16.4999999999931,-7.50000000000005,
-6.72119489704353));
#140600=CARTESIAN_POINT('Ctrl Pts',(16.4999999999939,-7.0732084403293,-6.28848666173585));
#140601=CARTESIAN_POINT('Ctrl Pts',(16.4999999999948,-6.6,-5.809935087192));
#140602=CARTESIAN_POINT('Origin',(17.3000000000088,-24.4,1.61862915007684));
#140603=CARTESIAN_POINT('',(16.7343145750595,-6.6,2.18431457502608));
#140604=CARTESIAN_POINT('Origin',(17.3000000000088,-6.6,1.61862915007684));
#140605=CARTESIAN_POINT('',(16.7343145750595,-24.4,2.18431457502608));
#140606=CARTESIAN_POINT('Origin',(18.3,-12.2,4.88137084986501));
#140607=CARTESIAN_POINT('',(19.1,-7.5,4.88137084986501));
#140608=CARTESIAN_POINT('',(19.1,-12.2,4.88137084986501));
#140609=CARTESIAN_POINT('',(18.8656854249492,-7.5,4.31568542491577));
#140610=CARTESIAN_POINT('Origin',(18.3,-7.5,4.88137084986501));
#140611=CARTESIAN_POINT('',(18.8656854249492,-12.2,4.31568542491577));
#140612=CARTESIAN_POINT('Origin',(16.5000000000094,-24.4,1.94999999997594));
#140613=CARTESIAN_POINT('',(17.5765623826223,-7.5,3.02656238258888));
#140614=CARTESIAN_POINT('',(14.7125000000122,-7.5,0.162499999978742));
#140615=CARTESIAN_POINT('',(16.7650854557587,-6.6,2.2150854557252));
#140616=CARTESIAN_POINT('Ctrl Pts',(16.7650854557587,-6.6,2.2150854557252));
#140617=CARTESIAN_POINT('Ctrl Pts',(17.1605923305092,-7.03154955968907,
2.61059233047575));
#140618=CARTESIAN_POINT('Ctrl Pts',(17.5765623826223,-7.5,3.02656238258888));
#140619=CARTESIAN_POINT('',(19.1,-6.6,4.54999999996654));
#140620=CARTESIAN_POINT('Origin',(13.1,-7.5,-1.80000000000345));
#140621=CARTESIAN_POINT('',(19.1,-7.5,10.5927097051057));
#140622=CARTESIAN_POINT('',(19.1,-7.5,1.1207142142697));
#140623=CARTESIAN_POINT('',(18.0728653213373,-7.5,11.5923414919222));
#140624=CARTESIAN_POINT('Origin',(18.1,-7.5,10.5927097051057));
#140625=CARTESIAN_POINT('',(14.7581088559379,-7.5,11.502363509309));
#140626=CARTESIAN_POINT('',(14.5178464431778,-7.5,11.4958416645148));
#140627=CARTESIAN_POINT('',(13.2896259362394,-7.5,12.0874135205689));
#140628=CARTESIAN_POINT('Origin',(14.7038394986125,-7.5,13.501627082942));
#140629=CARTESIAN_POINT('',(13.8999999999996,-7.5,11.4770394568086));
#140630=CARTESIAN_POINT('',(15.5737177837348,-7.5,9.80332167307343));
#140631=CARTESIAN_POINT('',(13.8999999999997,-7.5,9.24999999996345));
#140632=CARTESIAN_POINT('',(13.8999999999997,-7.5,6.29999983906575));
#140633=CARTESIAN_POINT('',(13.8988113452808,-7.5,9.11383245348325));
#140634=CARTESIAN_POINT('Origin',(6.09999999999969,-7.5,9.2499999999633));
#140635=CARTESIAN_POINT('',(14.6769816890462,-7.5,9.89957198073334));
#140636=CARTESIAN_POINT('Origin',(14.6986894319763,-7.5,9.09986655128017));
#140637=CARTESIAN_POINT('',(16.8837191928024,-7.5,9.959473150191));
#140638=CARTESIAN_POINT('',(13.3419069426877,-7.5,9.86333181239245));
#140639=CARTESIAN_POINT('',(17.5,-7.5,9.35969407810112));
#140640=CARTESIAN_POINT('Origin',(16.9,-7.5,9.35969407810112));
#140641=CARTESIAN_POINT('',(17.5,-7.5,4.08810094579999));
#140642=CARTESIAN_POINT('',(5.47101535039538,-7.5,6.69083194173083));
#140643=CARTESIAN_POINT('Origin',(0.213371879229554,-7.49999999999998,-93.1708583360234));
#140644=CARTESIAN_POINT('Origin',(5.5130764981647,-7.5,7.48972546395287));
#140645=CARTESIAN_POINT('Origin',(15.1,-7.5,-15.1));
#140646=CARTESIAN_POINT('Origin',(-9.16862915008379,-12.2,17.4));
#140647=CARTESIAN_POINT('',(-9.73431457503237,-2.60000000000001,17.9656854249499));
#140648=CARTESIAN_POINT('',(-9.73431457503237,-12.2,17.9656854249499));
#140649=CARTESIAN_POINT('',(-9.16862915008379,-2.6,18.2));
#140650=CARTESIAN_POINT('Origin',(-9.16862915008379,-2.6,17.4));
#140651=CARTESIAN_POINT('',(-9.16862915008379,-12.2,18.2));
#140652=CARTESIAN_POINT('Origin',(-10.6033654998821,-24.4,17.0966345001022));
#140653=CARTESIAN_POINT('',(-16.2656854249441,-2.60000000000001,11.4343145750533));
#140654=CARTESIAN_POINT('',(-16.2656854249441,-24.4,11.4343145750533));
#140655=CARTESIAN_POINT('',(-12.3391827499422,-2.60000000000001,15.3608172500461));
#140656=CARTESIAN_POINT('Origin',(-15.6999999999955,-24.4,10.8686291501034));
#140657=CARTESIAN_POINT('Origin',(-15.6999999999955,-2.6,10.8686291501034));
#140658=CARTESIAN_POINT('Origin',(-2.25752749827279E-11,-2.6,-0.450000000022573));
#140659=CARTESIAN_POINT('',(-13.1262499063287,-2.6,10.398411317633));
#140660=CARTESIAN_POINT('Origin',(-13.926034616533,-2.6,10.3798528337675));
#140661=CARTESIAN_POINT('',(-9.43078548284916,-2.6,5.95504649437932));
#140662=CARTESIAN_POINT('Origin',(-8.47750127826606,-2.6,10.5062825051013));
#140663=CARTESIAN_POINT('',(-8.89058649647473,-2.6,4.79243901829667));
#140664=CARTESIAN_POINT('Origin',(-9.59479136750862,-2.6,5.17203814844866));
#140665=CARTESIAN_POINT('',(-10.0921204701253,-2.6,-0.398878940274963));
#140666=CARTESIAN_POINT('Origin',(9.00768359641396E-11,-2.6,2.56054600265843E-10));
#140667=CARTESIAN_POINT('Origin',(-10.8914963489756,-2.6,-0.430473311803018));
#140668=CARTESIAN_POINT('Origin',(7.25952771151622,-2.6,9.86720616009051));
#140669=CARTESIAN_POINT('',(-6.85606479211595,-2.6,16.4647218026392));
#140670=CARTESIAN_POINT('Origin',(-6.74267665483338,-2.6,15.6727981129294));
#140671=CARTESIAN_POINT('',(-4.95681349263295,-2.6,16.6));
#140672=CARTESIAN_POINT('Origin',(-4.95681349263295,-2.6,3.2));
#140673=CARTESIAN_POINT('',(1.39248124878044,-2.6,16.6));
#140674=CARTESIAN_POINT('',(-2.47840674632776,-2.6,16.6));
#140675=CARTESIAN_POINT('Origin',(1.39248124878044,-2.6,15.8));
#140676=CARTESIAN_POINT('',(1.55054365106131,-2.6,18.2));
#140677=CARTESIAN_POINT('Origin',(1.55054365106131,-2.6,17.8));
#140678=CARTESIAN_POINT('',(19.1,-2.6,18.2));
#140679=CARTESIAN_POINT('',(-11.5275012782661,-2.6,10.5062825051013));
#140680=CARTESIAN_POINT('Origin',(-8.47750127826606,-2.6,10.5062825051013));
#140681=CARTESIAN_POINT('Origin',(-17.3000000000305,-24.4,-7.71862915012444));
#140682=CARTESIAN_POINT('',(-16.7343145750813,-24.4,-8.28431457507368));
#140683=CARTESIAN_POINT('Origin',(-18.3,-24.4,-10.9813708498909));
#140684=CARTESIAN_POINT('',(-19.1,-24.4,-10.9813708498909));
#140685=CARTESIAN_POINT('',(-18.8656854249492,-24.4,-10.4156854249417));
#140686=CARTESIAN_POINT('Origin',(-16.5000000000311,-24.4,-8.05000000002354));
#140687=CARTESIAN_POINT('',(-17.8000000000336,-17.35,-9.35000000002598));
#140688=CARTESIAN_POINT('Origin',(-16.6686291501351,-10.3,-10.4813708499245));
#140689=CARTESIAN_POINT('',(-16.6686291501351,-5.95,-10.4813708499245));
#140690=CARTESIAN_POINT('Origin',(9.25,-7.5,-3.05000000003699));
#140691=CARTESIAN_POINT('',(11.608349401414,-7.5,-7.90779663028513));
#140692=CARTESIAN_POINT('',(10.2965705850743,-8.9,-8.34761172707562));
#140693=CARTESIAN_POINT('Origin',(15.1,-7.5,-15.1));
#140694=CARTESIAN_POINT('',(13.9888110834979,-7.5,-7.18263475607025));
#140695=CARTESIAN_POINT('Origin',(14.0999999999907,-7.5,-7.97487021655479));
#140696=CARTESIAN_POINT('',(14.8999999999907,-7.5,-7.9748702165563));
#140697=CARTESIAN_POINT('Origin',(14.8999999999924,-1.6,-7.10754022756819));
#140698=CARTESIAN_POINT('',(14.89999999999,-1.6,-8.3813708499204));
#140699=CARTESIAN_POINT('Origin',(15.69999999999,-1.6,-8.38137084992191));
#140700=CARTESIAN_POINT('',(15.1343145750407,-1.6,-8.94705627487115));
#140701=CARTESIAN_POINT('Origin',(14.8999999999893,-1.6,-8.71274169981976));
#140702=CARTESIAN_POINT('Origin',(8.16898488501357,-7.5,-6.27357043065748));
#140703=CARTESIAN_POINT('',(7.69312168782831,-6.6,-5.90811972595898));
#140704=CARTESIAN_POINT('',(7.69312168782831,-7.5,-5.90811972595898));
#140705=CARTESIAN_POINT('',(7.97821751178067,-6.6,-6.84243580076698));
#140706=CARTESIAN_POINT('Origin',(8.16898488501357,-6.6,-6.27357043065748));
#140707=CARTESIAN_POINT('',(7.97821751178067,-7.5,-6.84243580076698));
#140708=CARTESIAN_POINT('Origin',(-2.12720466293355E-17,-7.5,-1.66578428666901E-15));
#140709=CARTESIAN_POINT('',(9.65595769539761,-6.6,0.923298968206738));
#140710=CARTESIAN_POINT('',(9.65595769539761,-7.5,0.923298968206738));
#140711=CARTESIAN_POINT('Origin',(-2.12720466293355E-17,-6.6,-1.48411142809398E-15));
#140712=CARTESIAN_POINT('Origin',(10.2532334291335,-7.5,0.98041024459066));
#140713=CARTESIAN_POINT('Origin',(10.2532334291335,-6.6,0.98041024459066));
#140714=CARTESIAN_POINT('Origin',(15.1,-10.3,-15.1));
#140715=CARTESIAN_POINT('',(13.5220680886962,-10.3,8.5924743090986));
#140716=CARTESIAN_POINT('',(13.5220680886962,-10.3,8.5924743090986));
#140717=CARTESIAN_POINT('',(10.3106112119491,-10.3,8.1569336551683));
#140718=CARTESIAN_POINT('Origin',(15.1,-10.3,-15.1));
#140719=CARTESIAN_POINT('',(10.3106112119491,-10.3,8.1569336551683));
#140720=CARTESIAN_POINT('Origin',(13.4954867544557,-10.3,8.99159012270412));
#140721=CARTESIAN_POINT('',(13.8952427952371,-10.3,8.97762202123065));
#140722=CARTESIAN_POINT('',(13.8952427952371,-10.3,8.97762202123065));
#140723=CARTESIAN_POINT('Origin',(13.4954867544557,-10.3,8.99159012270412));
#140724=CARTESIAN_POINT('Origin',(6.09999999999969,-7.5,9.2499999999633));
#140725=CARTESIAN_POINT('',(13.8988113452808,-7.5,9.11383245348325));
#140726=CARTESIAN_POINT('',(13.8999999999997,-10.3,9.24999999996345));
#140727=CARTESIAN_POINT('',(13.8999999999997,-7.5,9.24999999996345));
#140728=CARTESIAN_POINT('Origin',(6.09999999999969,-10.3,9.2499999999633));
#140729=CARTESIAN_POINT('Origin',(14.6986894319763,-7.5,9.09986655128017));
#140730=CARTESIAN_POINT('',(14.6769816890462,-7.5,9.89957198073334));
#140731=CARTESIAN_POINT('Origin',(13.8999999999997,-7.5,9.87848106632152));
#140732=CARTESIAN_POINT('',(16.8837191928024,-7.5,9.959473150191));
#140733=CARTESIAN_POINT('Origin',(16.9,-7.5,9.35969407810112));
#140734=CARTESIAN_POINT('',(17.5,-7.5,9.35969407810112));
#140735=CARTESIAN_POINT('Origin',(17.5,-7.5,9.97620189160342));
#140736=CARTESIAN_POINT('Origin',(15.8325427278768,-6.6,-1.75748667391245));
#140737=CARTESIAN_POINT('Origin',(15.1,-6.6,-15.1));
#140738=CARTESIAN_POINT('Origin',(15.1,-6.6,-15.1));
#140739=CARTESIAN_POINT('Origin',(-15.5,-10.3,-15.5));
#140740=CARTESIAN_POINT('',(-16.4600000000227,-10.3,-12.4473945554729));
#140741=CARTESIAN_POINT('',(-15.0612959521201,-10.3,-12.3302147141527));
#140742=CARTESIAN_POINT('Origin',(-16.7000000000283,-10.3,-11.6842431943411));
#140743=CARTESIAN_POINT('',(-17.5000000000283,-10.3,-11.6842431943471));
#140744=CARTESIAN_POINT('Origin',(-17.5,-1.6,-15.4999999999881));
#140745=CARTESIAN_POINT('',(-17.5000000000286,-1.6,-11.6441125497224));
#140746=CARTESIAN_POINT('Origin',(-16.7000000000286,-1.6,-11.6441125497165));
#140747=CARTESIAN_POINT('',(-17.2656854249779,-1.6,-11.0784271247672));
#140748=CARTESIAN_POINT('Origin',(-17.5000000000311,-1.6,-11.3127416998205));
#140749=CARTESIAN_POINT('',(-15.1343145750825,-1.6,-8.94705627487187));
#140750=CARTESIAN_POINT('Origin',(-15.7000000000318,-1.6,-8.38137084992263));
#140751=CARTESIAN_POINT('Origin',(-9.59479136750862,-2.6,5.17203814844866));
#140752=CARTESIAN_POINT('',(-8.89058649647473,-2.6,4.79243901829667));
#140753=CARTESIAN_POINT('',(-9.43078548284916,-2.6,5.95504649437932));
#140754=CARTESIAN_POINT('Origin',(9.00768359641396E-11,-2.6,2.56054600265843E-10));
#140755=CARTESIAN_POINT('',(-10.0921204701253,-2.6,-0.398878940274965));
#140756=CARTESIAN_POINT('Origin',(-10.8914963489756,-2.6,-0.430473311803018));
#140757=CARTESIAN_POINT('Origin',(-13.926034616533,-2.6,10.3798528337675));
#140758=CARTESIAN_POINT('',(-13.1262499063287,-2.6,10.398411317633));
#140759=CARTESIAN_POINT('Origin',(-8.47750127826606,-2.6,10.5062825051013));
#140760=CARTESIAN_POINT('Origin',(-19.1,-24.4,8.48528137429235));
#140761=CARTESIAN_POINT('',(-19.1,4.88334721263554E-15,-15.5));
#140762=CARTESIAN_POINT('Origin',(15.1,-7.05,-15.1));
#140763=CARTESIAN_POINT('Origin',(15.1,-6.6,-15.1));
#140764=CARTESIAN_POINT('Origin',(19.1,4.2410519540681E-15,-19.1));
#140765=CARTESIAN_POINT('',(19.1,3.35287353436797E-15,-15.1));
#140766=CARTESIAN_POINT('Origin',(19.1,4.2410519540681E-15,-19.1));
#140767=CARTESIAN_POINT('',(19.1,-5.,11.6340015374781));
#140768=CARTESIAN_POINT('',(19.1,-5.5,11.6340015374781));
#140769=CARTESIAN_POINT('',(19.1,-5.,10.5927097051057));
#140770=CARTESIAN_POINT('',(19.1,-5.,-1.9375));
#140771=CARTESIAN_POINT('',(19.1,-2.75,10.5927097051057));
#140772=CARTESIAN_POINT('Origin',(-15.5,3.44169137633798E-15,-15.5));
#140773=CARTESIAN_POINT('Origin',(-4.21607216363254,-10.1,-7.2584996763473));
#140774=CARTESIAN_POINT('',(-0.796199698700571,-10.1,-9.30032612545083));
#140775=CARTESIAN_POINT('Origin',(0.00380023450634744,-10.1,-9.29999922356006));
#140776=CARTESIAN_POINT('Origin',(-6.1338854524033,-10.1,-4.97849869506814));
#140777=CARTESIAN_POINT('',(-0.795830131689239,-10.1,-10.2047368760032));
#140778=CARTESIAN_POINT('Origin',(-1.39583008159634,-10.1,-10.204982052423));
#140779=CARTESIAN_POINT('',(-0.795830131689239,-10.1,-10.2047368760032));
#140780=CARTESIAN_POINT('Origin',(-1.39583008159634,-10.3,-10.204982052423));
#140781=CARTESIAN_POINT('',(-0.795830131689239,-10.3,-10.2047368760032));
#140782=CARTESIAN_POINT('Origin',(-6.1338854524033,-10.3,-4.97849869506814));
#140783=CARTESIAN_POINT('Origin',(-11.9533418970136,-2.6,-0.350905528319926));
#140784=CARTESIAN_POINT('Origin',(-2.25730545366787E-11,-10.4,-0.450000000022575));
#140785=CARTESIAN_POINT('',(-7.8,-10.4,-3.05000000003699));
#140786=CARTESIAN_POINT('Origin',(-9.35,-10.4,-3.05000000003699));
#140787=CARTESIAN_POINT('Origin',(-15.5,-10.3,-15.5));
#140788=CARTESIAN_POINT('',(-13.9781746176887,-10.1,-12.419231543135));
#140789=CARTESIAN_POINT('',(-13.9781746176887,-10.3,-12.419231543135));
#140790=CARTESIAN_POINT('',(-14.5846229736965,-10.1,-12.1880260147795));
#140791=CARTESIAN_POINT('Origin',(-15.5,-10.1,-15.5));
#140792=CARTESIAN_POINT('',(-14.5846229736965,-10.3,-12.1880260147795));
#140793=CARTESIAN_POINT('Origin',(-9.35,-10.3,-3.05000000003699));
#140794=CARTESIAN_POINT('Origin',(-9.35,-10.1,-3.05000000003699));
#140795=CARTESIAN_POINT('Origin',(-12.176305656554,-10.1,-9.1169160676784));
#140796=CARTESIAN_POINT('Origin',(-14.9790389431426,-10.1,-11.7358799730564));
#140797=CARTESIAN_POINT('Origin',(-14.9790389431426,-10.3,-11.7358799730564));
#140798=CARTESIAN_POINT('Origin',(0.213371879229554,-4.4814254252597E-16,
-93.1708583360234));
#140799=CARTESIAN_POINT('',(5.47101535039538,-10.3,6.69083194173083));
#140800=CARTESIAN_POINT('Origin',(0.213371879229554,-10.3,-93.1708583360234));
#140801=CARTESIAN_POINT('',(5.47101535039538,-2.26218921073957E-14,6.69083194173083));
#140802=CARTESIAN_POINT('Origin',(5.5130764981647,-1.91165057187814E-16,
7.48972546395287));
#140803=CARTESIAN_POINT('Origin',(5.5130764981647,-10.3,7.48972546395286));
#140804=CARTESIAN_POINT('Origin',(9.94289321881345,-10.3,16.2));
#140805=CARTESIAN_POINT('',(9.94289321881345,-10.3,13.7509759234611));
#140806=CARTESIAN_POINT('',(9.94289321881345,-10.3,13.7509759234611));
#140807=CARTESIAN_POINT('',(9.94289321881345,-10.3,15.6));
#140808=CARTESIAN_POINT('',(9.94289321881345,-10.3,7.87499999998871));
#140809=CARTESIAN_POINT('',(9.94289321881345,-10.3,15.6));
#140810=CARTESIAN_POINT('Origin',(9.34289321881345,-10.3,13.7509759234611));
#140811=CARTESIAN_POINT('',(9.0224799018401,-10.3,13.243693648681));
#140812=CARTESIAN_POINT('',(9.0224799018401,-10.3,13.243693648681));
#140813=CARTESIAN_POINT('Origin',(9.34289321881345,-10.3,13.7509759234611));
#140814=CARTESIAN_POINT('Origin',(7.1,-10.3,10.2));
#140815=CARTESIAN_POINT('Origin',(7.1,-10.3,10.2));
#140816=CARTESIAN_POINT('Origin',(5.74909217812359,-10.3,-8.54622369438117));
#140817=CARTESIAN_POINT('',(6.14689326954821,-10.3,-8.09705302340923));
#140818=CARTESIAN_POINT('',(5.41419360512517,-10.3,-8.0483854216423));
#140819=CARTESIAN_POINT('Origin',(8.6,-10.3,-5.32716721908225));
#140820=CARTESIAN_POINT('',(7.33287671232876,-10.3,-8.80342937459372));
#140821=CARTESIAN_POINT('Origin',(6.1,-10.3,-12.1857384988752));
#140822=CARTESIAN_POINT('Origin',(-0.796152266589922,-10.3,-9.41640280839959));
#140823=CARTESIAN_POINT('',(-0.79309436390975,-10.3,-16.899754823607));
#140824=CARTESIAN_POINT('',(-0.796199698700571,-10.3,-9.30032612545083));
#140825=CARTESIAN_POINT('Origin',(-1.39309431381685,-10.3,-16.9000000000267));
#140826=CARTESIAN_POINT('',(-1.39309431381607,-10.3,-17.5000000000267));
#140827=CARTESIAN_POINT('Origin',(-0.792849087283714,-10.3,-17.500000000026));
#140828=CARTESIAN_POINT('',(-11.9672956534841,-10.3,-17.5000000000405));
#140829=CARTESIAN_POINT('Origin',(-11.9672956534849,-10.3,-16.9000000000405));
#140830=CARTESIAN_POINT('',(-12.5250910766189,-10.3,-16.6789473684552));
#140831=CARTESIAN_POINT('Origin',(-15.5,-10.3,-15.5));
#140832=CARTESIAN_POINT('Origin',(-6.74267665483338,-2.6,15.6727981129294));
#140833=CARTESIAN_POINT('',(-6.85606479211595,-2.6,16.4647218026392));
#140834=CARTESIAN_POINT('Origin',(-4.95681349263295,-2.6,3.2));
#140835=CARTESIAN_POINT('',(-4.95681349263295,-2.6,16.6));
#140836=CARTESIAN_POINT('Origin',(-4.95681349263295,-2.6,16.6));
#140837=CARTESIAN_POINT('',(1.39248124878044,-2.6,16.6));
#140838=CARTESIAN_POINT('Origin',(1.39248124878044,-2.6,15.8));
#140839=CARTESIAN_POINT('Origin',(9.34289321881345,-10.3,15.6));
#140840=CARTESIAN_POINT('Origin',(9.34289321881345,-10.3,15.6));
#140841=CARTESIAN_POINT('Origin',(10.4128562056381,-8.9,-8.93623525230213));
#140842=CARTESIAN_POINT('Origin',(-5.6920614055489E-17,-10.3,-2.28766658394441E-15));
#140843=CARTESIAN_POINT('',(1.32237339244619,-10.3,-9.60943957263029));
#140844=CARTESIAN_POINT('Origin',(1.4041696846368,-10.3,-10.2038378957974));
#140845=CARTESIAN_POINT('Origin',(0.00380023450634744,-10.3,-9.29999922356006));
#140846=CARTESIAN_POINT('Origin',(-2.25730545366787E-11,-10.3,-0.450000000022575));
#140847=CARTESIAN_POINT('Origin',(10.4719722228657,-10.3,7.37337598393027));
#140848=CARTESIAN_POINT('',(13.8999999999996,-10.3,11.4770394568086));
#140849=CARTESIAN_POINT('',(13.8999999999997,-10.3,6.97499983905631));
#140850=CARTESIAN_POINT('',(12.1286796564404,-10.3,13.2483598003679));
#140851=CARTESIAN_POINT('',(11.961217783734,-10.3,13.4158216730743));
#140852=CARTESIAN_POINT('',(11.5428932188134,-10.3,14.662573362741));
#140853=CARTESIAN_POINT('Origin',(13.5428932188134,-10.3,14.662573362741));
#140854=CARTESIAN_POINT('',(11.5428932188134,-10.3,17.2));
#140855=CARTESIAN_POINT('',(11.5428932188134,-10.3,8.87499999998871));
#140856=CARTESIAN_POINT('',(10.5428932188134,-10.3,18.2));
#140857=CARTESIAN_POINT('Origin',(10.5428932188134,-10.3,17.2));
#140858=CARTESIAN_POINT('',(1.55054365106132,-10.3,18.2));
#140859=CARTESIAN_POINT('',(19.1,-10.3,18.2));
#140860=CARTESIAN_POINT('Origin',(1.55054365106131,-10.3,17.8));
#140861=CARTESIAN_POINT('Origin',(7.25952771151622,-10.3,9.86720616009051));
#140862=CARTESIAN_POINT('',(9.4,-10.3,10.2));
#140863=CARTESIAN_POINT('Origin',(7.1,-10.3,10.2));
#140864=CARTESIAN_POINT('Origin',(9.25,-7.05,-3.05000000003699));
#140865=CARTESIAN_POINT('Origin',(9.24999999999998,-6.6,-3.05000000003696));
#140866=CARTESIAN_POINT('Origin',(9.25,-6.6,-3.05000000003699));
#140867=CARTESIAN_POINT('',(10.9969254825289,-6.6,-6.64836787429487));
#140868=CARTESIAN_POINT('Origin',(9.24999999999998,-7.5,-3.05000000003696));
#140869=CARTESIAN_POINT('Origin',(7.25952771151622,-2.6,9.86720616009051));
#140870=CARTESIAN_POINT('Origin',(10.5,-10.3,-13.400000000037));
#140871=CARTESIAN_POINT('',(10.5,-10.3,-13.400000000037));
#140872=CARTESIAN_POINT('Origin',(10.5,-10.3,-13.800000000037));
#140873=CARTESIAN_POINT('',(10.9,-10.3,-13.800000000037));
#140874=CARTESIAN_POINT('Origin',(10.9,-10.3,-15.1));
#140875=CARTESIAN_POINT('Origin',(10.4719722228657,-10.3,7.37337598393027));
#140876=CARTESIAN_POINT('Origin',(18.4241839371104,-6.6,-4.3509818715809));
#140877=CARTESIAN_POINT('Origin',(7.1,-1.00000000000001,10.2));
#140878=CARTESIAN_POINT('',(8.7,-1.00000000000001,10.2));
#140879=CARTESIAN_POINT('Origin',(7.1,-1.00000000000001,10.2));
#140880=CARTESIAN_POINT('Origin',(7.1,-24.4,10.2));
#140881=CARTESIAN_POINT('',(8.7,-4.9,10.2));
#140882=CARTESIAN_POINT('Origin',(7.1,-4.9,10.2));
#140883=CARTESIAN_POINT('',(8.7,-24.4,10.2));
#140884=CARTESIAN_POINT('Origin',(7.1,-4.9,10.2));
#140885=CARTESIAN_POINT('',(9.1,-4.9,10.2));
#140886=CARTESIAN_POINT('Origin',(7.1,-4.9,10.2));
#140887=CARTESIAN_POINT('Origin',(15.1,3.35287353436797E-15,-15.1));
#140888=CARTESIAN_POINT('',(13.55,3.35287353436797E-15,-15.1));
#140889=CARTESIAN_POINT('Origin',(14.7928932188134,-5.5,16.2071067811865));
#140890=CARTESIAN_POINT('',(12.6059538781827,-5.,18.6112274770755));
#140891=CARTESIAN_POINT('',(12.6059538781827,-5.50000000000001,18.6112274770755));
#140892=CARTESIAN_POINT('',(17.0909902576697,-5.,18.5052038200428));
#140893=CARTESIAN_POINT('Origin',(14.7928932188134,-5.,16.2071067811865));
#140894=CARTESIAN_POINT('',(17.0909902576697,-5.50000000000001,18.5052038200428));
#140895=CARTESIAN_POINT('Origin',(17.0909902576697,-5.50000000000001,18.5052038200428));
#140896=CARTESIAN_POINT('',(18.5052038200428,-5.,17.0909902576697));
#140897=CARTESIAN_POINT('',(18.5052038200428,-5.5,17.0909902576697));
#140898=CARTESIAN_POINT('',(17.557043648263,-5.,18.0391504294495));
#140899=CARTESIAN_POINT('Origin',(16.2071067811865,-5.5,14.7928932188135));
#140900=CARTESIAN_POINT('',(19.3750857890412,-5.,14.0673527266339));
#140901=CARTESIAN_POINT('',(19.3750857890412,-5.5,14.0673527266339));
#140902=CARTESIAN_POINT('Origin',(16.2071067811865,-5.,14.7928932188135));
#140903=CARTESIAN_POINT('Origin',(14.7928932188134,-5.5,16.2071067811865));
#140904=CARTESIAN_POINT('',(13.661522368915,-5.,15.0757359312881));
#140905=CARTESIAN_POINT('',(15.9242640687119,-5.,17.338477631085));
#140906=CARTESIAN_POINT('Origin',(14.7928932188134,-5.,16.2071067811865));
#140907=CARTESIAN_POINT('',(13.661522368915,-5.5,15.0757359312881));
#140908=CARTESIAN_POINT('',(15.9242640687119,-5.5,17.338477631085));
#140909=CARTESIAN_POINT('Origin',(15.0757359312881,-5.5,13.661522368915));
#140910=CARTESIAN_POINT('',(15.0757359312881,-5.,13.661522368915));
#140911=CARTESIAN_POINT('',(14.8346825406948,-5.,13.9025757595082));
#140912=CARTESIAN_POINT('',(15.0757359312881,-5.5,13.661522368915));
#140913=CARTESIAN_POINT('Origin',(16.2071067811865,-5.5,14.7928932188135));
#140914=CARTESIAN_POINT('',(17.338477631085,-5.,15.9242640687119));
#140915=CARTESIAN_POINT('Origin',(16.2071067811865,-5.,14.7928932188135));
#140916=CARTESIAN_POINT('',(17.338477631085,-5.5,15.9242640687119));
#140917=CARTESIAN_POINT('Origin',(15.9242640687119,-5.5,17.338477631085));
#140918=CARTESIAN_POINT('',(16.3903174593052,-5.,16.8724242404917));
#140919=CARTESIAN_POINT('Origin',(-9.25,-7.2,-3.05000000003699));
#140920=CARTESIAN_POINT('',(-7.8,-7.2,-3.05000000003699));
#140921=CARTESIAN_POINT('Origin',(-9.35,-7.2,-3.05000000003699));
#140922=CARTESIAN_POINT('Origin',(-8.47750127826606,-2.33286334807598E-15,
10.5062825051013));
#140923=CARTESIAN_POINT('',(-11.5275012782661,-2.33286334807598E-15,10.5062825051013));
#140924=CARTESIAN_POINT('Origin',(7.1,-10.3,10.2));
#140925=CARTESIAN_POINT('',(9.1,-10.,10.2));
#140926=CARTESIAN_POINT('Origin',(7.1,-10.,10.2));
#140927=CARTESIAN_POINT('',(9.1,-10.3,10.2));
#140928=CARTESIAN_POINT('Origin',(11.5427649064299,-5.50000000000001,19.78));
#140929=CARTESIAN_POINT('',(11.5427649064299,-5.,18.2));
#140930=CARTESIAN_POINT('Origin',(11.5427649064299,-5.,19.78));
#140931=CARTESIAN_POINT('',(11.5427649064299,-5.50000000000001,18.2));
#140932=CARTESIAN_POINT('Origin',(14.7038394986125,-5.5,13.501627082942));
#140933=CARTESIAN_POINT('',(13.2896259362394,-5.,12.0874135205689));
#140934=CARTESIAN_POINT('',(14.7581088559379,-5.,11.502363509309));
#140935=CARTESIAN_POINT('Origin',(14.7038394986125,-5.,13.501627082942));
#140936=CARTESIAN_POINT('',(13.2896259362394,-5.5,12.0874135205689));
#140937=CARTESIAN_POINT('',(14.7581088559379,-5.5,11.502363509309));
#140938=CARTESIAN_POINT('Origin',(16.2952944868403,-5.5,11.5440899116599));
#140939=CARTESIAN_POINT('',(18.0728653213373,-5.,11.5923414919222));
#140940=CARTESIAN_POINT('',(18.0728653213373,-2.75,11.5923414919222));
#140941=CARTESIAN_POINT('',(16.0352973695706,-5.,11.5370323747515));
#140942=CARTESIAN_POINT('Origin',(30.,-5.5,11.6340015374781));
#140943=CARTESIAN_POINT('Origin',(30.,-5.,11.6340015374781));
#140944=CARTESIAN_POINT('Origin',(15.1,3.35287353436797E-15,-15.1));
#140945=CARTESIAN_POINT('Origin',(18.1,-2.75,10.5927097051057));
#140946=CARTESIAN_POINT('Origin',(18.1,-5.,10.5927097051057));
#140947=CARTESIAN_POINT('Origin',(15.675,-5.,15.225));
#140948=CARTESIAN_POINT('',(11.5428932188134,-5.,14.662573362741));
#140949=CARTESIAN_POINT('',(12.1286796564404,-5.,13.2483598003679));
#140950=CARTESIAN_POINT('Origin',(13.5428932188134,-5.,14.662573362741));
#140951=CARTESIAN_POINT('',(12.2043420607724,-5.,13.1726973960359));
#140952=CARTESIAN_POINT('',(10.5428932188134,-5.,18.2));
#140953=CARTESIAN_POINT('',(17.3875,-5.,18.2));
#140954=CARTESIAN_POINT('',(11.5428932188134,-5.,17.2));
#140955=CARTESIAN_POINT('Origin',(10.5428932188134,-5.,17.2));
#140956=CARTESIAN_POINT('',(11.5428932188134,-5.,16.7125));
#140957=CARTESIAN_POINT('Origin',(15.1,-7.05,-15.1));
#140958=CARTESIAN_POINT('Origin',(-15.5,3.44169137633798E-15,-15.5));
#140959=CARTESIAN_POINT('',(-17.1,3.44169137633798E-15,-15.5));
#140960=CARTESIAN_POINT('Origin',(-9.35,-10.3,-3.05000000003699));
#140961=CARTESIAN_POINT('',(-7.8,-10.3,-3.05000000003699));
#140962=CARTESIAN_POINT('Origin',(7.1,-10.15,10.2));
#140963=CARTESIAN_POINT('',(9.25,-10.15,10.2));
#140964=CARTESIAN_POINT('Origin',(1.55054365106131,-2.6,17.8));
#140965=CARTESIAN_POINT('',(1.55054365106131,-2.6,18.2));
#140966=CARTESIAN_POINT('Origin',(19.1,-4.04121180963557E-15,18.2));
#140967=CARTESIAN_POINT('',(10.5428932188134,-2.75,18.2));
#140968=CARTESIAN_POINT('Origin',(10.5428932188134,-2.75,17.2));
#140969=CARTESIAN_POINT('',(11.5428932188134,-2.75,17.2));
#140970=CARTESIAN_POINT('Origin',(11.5428932188134,-5.50000000000001,18.2));
#140971=CARTESIAN_POINT('',(11.5428932188134,-5.50000000000001,14.662573362741));
#140972=CARTESIAN_POINT('Origin',(13.5428932188134,-5.50000000000001,14.662573362741));
#140973=CARTESIAN_POINT('',(12.1286796564404,-5.50000000000001,13.2483598003679));
#140974=CARTESIAN_POINT('Origin',(11.4951643931407,-5.5,13.8818750636676));
#140975=CARTESIAN_POINT('',(13.8999999999996,-6.5,11.4770394568086));
#140976=CARTESIAN_POINT('Origin',(13.8999999999996,-7.5,14.3999996781349));
#140977=CARTESIAN_POINT('Origin',(3.56597033699713E-16,-18.2,11.6));
#140978=CARTESIAN_POINT('',(-3.17746460160488,-19.0909089210171,6.83040013131191));
#140979=CARTESIAN_POINT('',(-2.3,-20.5664319132398,8.65129518522849));
#140980=CARTESIAN_POINT('Ctrl Pts',(-3.17746460160488,-19.0909089210171,
6.83040013131191));
#140981=CARTESIAN_POINT('Ctrl Pts',(-3.13315640143359,-19.248936003566,
6.89428549599595));
#140982=CARTESIAN_POINT('Ctrl Pts',(-3.07905321107781,-19.3953385241206,
6.97496500901045));
#140983=CARTESIAN_POINT('Ctrl Pts',(-2.91283443393186,-19.7751825843832,
7.23829491707707));
#140984=CARTESIAN_POINT('Ctrl Pts',(-2.78681144529922,-19.9793063971522,
7.45724834891686));
#140985=CARTESIAN_POINT('Ctrl Pts',(-2.54447355256091,-20.3113748120439,
7.96074874984413));
#140986=CARTESIAN_POINT('Ctrl Pts',(-2.42818675997411,-20.4389117240242,
8.24557800636064));
#140987=CARTESIAN_POINT('Ctrl Pts',(-2.32051730171903,-20.5463637099844,
8.58397368821829));
#140988=CARTESIAN_POINT('Ctrl Pts',(-2.31014109346683,-20.5565755067051,
8.6175231927284));
#140989=CARTESIAN_POINT('Ctrl Pts',(-2.3,-20.5664319132398,8.65129518522849));
#140990=CARTESIAN_POINT('',(-2.3,-20.5664319132398,6.22469676050457));
#140991=CARTESIAN_POINT('Ctrl Pts',(-2.3,-20.5664319132398,6.22469676050457));
#140992=CARTESIAN_POINT('Ctrl Pts',(-2.48457597975064,-20.3870374624419,
6.36499899257086));
#140993=CARTESIAN_POINT('Ctrl Pts',(-2.65218676613499,-20.1805459930308,
6.48360541114717));
#140994=CARTESIAN_POINT('Ctrl Pts',(-2.94119052469523,-19.7229874823135,
6.68052442957258));
#140995=CARTESIAN_POINT('Ctrl Pts',(-3.07628642332023,-19.4360520008276,
6.76703831626945));
#140996=CARTESIAN_POINT('Ctrl Pts',(-3.16994744110375,-19.1173998416605,
6.82570105370662));
#140997=CARTESIAN_POINT('Ctrl Pts',(-3.17374660773455,-19.1041693044674,
6.82807740667823));
#140998=CARTESIAN_POINT('Ctrl Pts',(-3.17746460160488,-19.0909089210171,
6.83040013131191));
#140999=CARTESIAN_POINT('',(-2.3,-20.5664319132398,11.6));
#141000=CARTESIAN_POINT('Origin',(-2.3,-22.8,6.19999999999999));
#141001=CARTESIAN_POINT('',(-2.3,-22.8,8.65129518522849));
#141002=CARTESIAN_POINT('',(-2.3,-10.3,8.65129518522849));
#141003=CARTESIAN_POINT('',(-2.3,-22.8,6.22469676050457));
#141004=CARTESIAN_POINT('',(-2.3,-10.3,6.22469676050457));
#141005=CARTESIAN_POINT('',(-2.3,-22.8,8.2207882501999));
#141006=CARTESIAN_POINT('Origin',(3.04851216033843,-22.8,10.2415765003998));
#141007=CARTESIAN_POINT('',(-3.17746460160488,-22.8,6.8304001313119));
#141008=CARTESIAN_POINT('Origin',(-9.35000000000002,-22.8,-3.05000000003702));
#141009=CARTESIAN_POINT('Origin',(-8.4775012782713,-22.8,10.5062825050979));
#141010=CARTESIAN_POINT('Origin',(-8.4775012782713,-10.3,10.5062825050979));
#141011=CARTESIAN_POINT('',(-3.17746460160488,-10.3,6.83040013131191));
#141012=CARTESIAN_POINT('Origin',(-9.35,-10.3,-3.05000000003699));
#141013=CARTESIAN_POINT('Origin',(-10.7086647932826,-22.8,15.8599643568047));
#141014=CARTESIAN_POINT('',(-10.4009181015562,-6.3,15.1215254807077));
#141015=CARTESIAN_POINT('',(-10.1429793683341,-6.3,15.2942789318548));
#141016=CARTESIAN_POINT('Origin',(-10.7086647932826,-6.3,15.8599643568047));
#141017=CARTESIAN_POINT('',(-10.1429793683341,-15.7,15.2942789318548));
#141018=CARTESIAN_POINT('',(-10.1429793683341,-22.8,15.2942789318548));
#141019=CARTESIAN_POINT('',(-10.4009181015562,-15.7,15.1215254807077));
#141020=CARTESIAN_POINT('Origin',(-10.7086647932826,-15.7,15.8599643568047));
#141021=CARTESIAN_POINT('',(-10.4009181015562,-22.8,15.1215254807077));
#141022=CARTESIAN_POINT('Origin',(-9.46958677130784,-6.3,12.0780860478535));
#141023=CARTESIAN_POINT('',(-13.0927442538679,-6.3,12.4296993284023));
#141024=CARTESIAN_POINT('Origin',(-8.47750127826595,-6.3,10.5062825051013));
#141025=CARTESIAN_POINT('',(-13.2654977050156,-6.3,12.1717605951805));
#141026=CARTESIAN_POINT('Origin',(-13.8311831299642,-6.3,12.7374460201304));
#141027=CARTESIAN_POINT('',(-14.6656854249453,-6.3,10.771572875254));
#141028=CARTESIAN_POINT('',(-11.8753061227997,-6.3,13.5619521773932));
#141029=CARTESIAN_POINT('',(-14.8999999999968,-6.3,10.2058874503057));
#141030=CARTESIAN_POINT('Origin',(-14.0999999999968,-6.3,10.2058874503041));
#141031=CARTESIAN_POINT('',(-14.9000000000043,-6.3,6.20189169841771));
#141032=CARTESIAN_POINT('',(-14.8999999999947,-6.3,11.3076721740337));
#141033=CARTESIAN_POINT('',(-15.0836363636405,-6.3,5.86545927302009));
#141034=CARTESIAN_POINT('Origin',(-15.3000000000043,-6.3,6.20189169841847));
#141035=CARTESIAN_POINT('',(-15.8545454545506,-6.3,5.31964087814201));
#141036=CARTESIAN_POINT('Origin',(-9.35,-6.3,-3.05000000003698));
#141037=CARTESIAN_POINT('',(-16.5000000000054,-6.3,5.63547638297971));
#141038=CARTESIAN_POINT('Origin',(-16.1000000000054,-6.3,5.63547638297895));
#141039=CARTESIAN_POINT('',(-16.4999999999955,-6.3,10.8686291501049));
#141040=CARTESIAN_POINT('',(-16.5000000000028,-6.3,7.01404302392158));
#141041=CARTESIAN_POINT('',(-16.2656854249441,-6.3,11.4343145750533));
#141042=CARTESIAN_POINT('Origin',(-15.6999999999955,-6.3,10.8686291501034));
#141043=CARTESIAN_POINT('',(-9.73431457503237,-6.30000000000001,17.9656854249499));
#141044=CARTESIAN_POINT('',(-11.5745579308,-6.3,16.1254420691865));
#141045=CARTESIAN_POINT('',(-9.16862915008378,-6.30000000000001,18.2));
#141046=CARTESIAN_POINT('Origin',(-9.16862915008378,-6.30000000000001,17.4));
#141047=CARTESIAN_POINT('',(0.550543651061315,-6.30000000000001,18.2));
#141048=CARTESIAN_POINT('',(-4.73479338565392,-6.30000000000001,18.2));
#141049=CARTESIAN_POINT('',(0.748897957688963,-6.30000000000001,17.4526448948953));
#141050=CARTESIAN_POINT('Origin',(0.550543651061315,-6.30000000000001,17.8));
#141051=CARTESIAN_POINT('',(-0.459727007153423,-6.30000000000001,16.7624694423079));
#141052=CARTESIAN_POINT('',(-4.26116725349562,-6.3,14.5916879188221));
#141053=CARTESIAN_POINT('',(-0.755737525613271,-6.30000000000001,16.6));
#141054=CARTESIAN_POINT('Origin',(-5.41858467284464,-6.30000000000001,25.4463470699242));
#141055=CARTESIAN_POINT('',(-8.50588745028793,-6.30000000000001,16.6));
#141056=CARTESIAN_POINT('',(-7.2132001319704,-6.3,16.6));
#141057=CARTESIAN_POINT('',(-9.07157287523651,-6.30000000000001,16.3656854249499));
#141058=CARTESIAN_POINT('Origin',(-8.50588745028793,-6.3,15.8));
#141059=CARTESIAN_POINT('',(-9.32581890600149,-6.3,16.1114393941855));
#141060=CARTESIAN_POINT('Origin',(-8.47750127826595,-22.8,10.5062825051013));
#141061=CARTESIAN_POINT('',(-13.0927442538679,-15.7,12.4296993284023));
#141062=CARTESIAN_POINT('Origin',(-8.47750127826595,-15.7,10.5062825051013));
#141063=CARTESIAN_POINT('',(-13.0927442538679,-22.8,12.4296993284023));
#141064=CARTESIAN_POINT('Origin',(-13.8311831299642,-22.8,12.7374460201304));
#141065=CARTESIAN_POINT('',(-13.2654977050156,-15.7,12.1717605951805));
#141066=CARTESIAN_POINT('Origin',(-13.8311831299642,-15.7,12.7374460201304));
#141067=CARTESIAN_POINT('',(-13.2654977050156,-22.8,12.1717605951805));
#141068=CARTESIAN_POINT('Origin',(-12.3362327337785,-22.8,13.1010255664155));
#141069=CARTESIAN_POINT('',(-14.4917200414815,-15.7,10.9455382587175));
#141070=CARTESIAN_POINT('',(-14.4917200414815,-15.7,10.9455382587175));
#141071=CARTESIAN_POINT('',(-14.4917200414815,-24.,10.9455382587175));
#141072=CARTESIAN_POINT('',(-14.4917200414815,-15.9,10.9455382587175));
#141073=CARTESIAN_POINT('',(-14.6656854249453,-24.,10.771572875254));
#141074=CARTESIAN_POINT('',(-14.5858675678007,-24.,10.8513907323985));
#141075=CARTESIAN_POINT('',(-14.6656854249453,-22.8,10.771572875254));
#141076=CARTESIAN_POINT('Origin',(-8.47750127826595,-24.,10.5062825051013));
#141077=CARTESIAN_POINT('',(-12.344773048718,-24.,7.92428539947466));
#141078=CARTESIAN_POINT('',(-12.6774415881118,-24.4,7.7021781215713));
#141079=CARTESIAN_POINT('Origin',(-12.6774415881118,-24.,7.7021781215713));
#141080=CARTESIAN_POINT('',(-13.5261422614307,-24.4,10.3891320757003));
#141081=CARTESIAN_POINT('Origin',(-8.47750127826595,-24.4,10.5062825051013));
#141082=CARTESIAN_POINT('',(-13.1262499063286,-24.,10.3984113176331));
#141083=CARTESIAN_POINT('Origin',(-13.5261422614307,-24.,10.3891320757003));
#141084=CARTESIAN_POINT('Origin',(-8.47750127826595,-24.,10.5062825051013));
#141085=CARTESIAN_POINT('Ctrl Pts',(-13.1262499063286,-24.,10.3984113176331));
#141086=CARTESIAN_POINT('Ctrl Pts',(-13.138495190793,-24.,10.9261263700982));
#141087=CARTESIAN_POINT('Ctrl Pts',(-13.6284819468181,-24.,11.1224579837266));
#141088=CARTESIAN_POINT('Ctrl Pts',(-14.1184687028432,-24.,11.3187895973549));
#141089=CARTESIAN_POINT('Ctrl Pts',(-14.4917200414815,-24.,10.9455382587175));
#141090=CARTESIAN_POINT('Ctrl Pts',(-13.1262499063286,-24.4,10.3984113176331));
#141091=CARTESIAN_POINT('Ctrl Pts',(-13.138495190793,-24.4,10.9261263700982));
#141092=CARTESIAN_POINT('Ctrl Pts',(-13.6284819468181,-24.4,11.1224579837266));
#141093=CARTESIAN_POINT('Ctrl Pts',(-14.1184687028432,-24.4,11.3187895973549));
#141094=CARTESIAN_POINT('Ctrl Pts',(-14.4917200414815,-24.4,10.9455382587175));
#141095=CARTESIAN_POINT('Ctrl Pts',(-13.5261422614307,-24.4,10.3891320757003));
#141096=CARTESIAN_POINT('Ctrl Pts',(-13.532264903663,-24.4,10.6529896019329));
#141097=CARTESIAN_POINT('Ctrl Pts',(-13.7772582816755,-24.4,10.7511554087471));
#141098=CARTESIAN_POINT('Ctrl Pts',(-14.022251659688,-24.4,10.8493212155613));
#141099=CARTESIAN_POINT('Ctrl Pts',(-14.2088773290072,-24.4,10.6626955462425));
#141100=CARTESIAN_POINT('',(-14.2088773290072,-24.4,10.6626955462425));
#141101=CARTESIAN_POINT('Origin',(-14.2088773290072,-24.,10.6626955462425));
#141102=CARTESIAN_POINT('Origin',(-13.9260346165329,-24.,10.3798528337676));
#141103=CARTESIAN_POINT('Origin',(-13.9260346165329,-24.4,10.3798528337676));
#141104=CARTESIAN_POINT('Origin',(-14.3030248553264,-24.,10.5685480199236));
#141105=CARTESIAN_POINT('',(-14.3828427124711,-24.4,10.4887301627791));
#141106=CARTESIAN_POINT('Origin',(-14.3828427124711,-24.,10.4887301627791));
#141107=CARTESIAN_POINT('',(-14.3030248553264,-24.4,10.5685480199236));
#141108=CARTESIAN_POINT('Ctrl Pts',(-14.6656854249453,-24.,10.771572875254));
#141109=CARTESIAN_POINT('Ctrl Pts',(-14.8999999999965,-24.,10.537258300203));
#141110=CARTESIAN_POINT('Ctrl Pts',(-14.8999999999968,-24.,10.2058874503041));
#141111=CARTESIAN_POINT('Ctrl Pts',(-14.6656854249453,-24.4,10.771572875254));
#141112=CARTESIAN_POINT('Ctrl Pts',(-14.8999999999965,-24.4,10.537258300203));
#141113=CARTESIAN_POINT('Ctrl Pts',(-14.8999999999968,-24.4,10.2058874503041));
#141114=CARTESIAN_POINT('Ctrl Pts',(-14.3828427124711,-24.4,10.4887301627791));
#141115=CARTESIAN_POINT('Ctrl Pts',(-14.4999999999966,-24.4,10.3715728752536));
#141116=CARTESIAN_POINT('Ctrl Pts',(-14.4999999999968,-24.4,10.2058874503041));
#141117=CARTESIAN_POINT('',(-14.4999999999968,-24.4,10.2058874503049));
#141118=CARTESIAN_POINT('',(-14.8999999999968,-24.,10.2058874503056));
#141119=CARTESIAN_POINT('Origin',(-14.4999999999968,-24.,10.2058874503049));
#141120=CARTESIAN_POINT('Origin',(-14.0999999999968,-24.,10.2058874503041));
#141121=CARTESIAN_POINT('Origin',(-14.0999999999968,-24.4,10.2058874503041));
#141122=CARTESIAN_POINT('Origin',(-14.4999999999983,-24.,9.40207938827399));
#141123=CARTESIAN_POINT('',(-14.5000000000022,-24.4,7.31327650886668));
#141124=CARTESIAN_POINT('',(-14.9000000000022,-24.,7.31327650886744));
#141125=CARTESIAN_POINT('Origin',(-14.5000000000022,-24.,7.31327650886668));
#141126=CARTESIAN_POINT('',(-14.8999999999983,-24.,9.40207938827475));
#141127=CARTESIAN_POINT('',(-14.4999999999983,-24.4,9.40207938827399));
#141128=CARTESIAN_POINT('Ctrl Pts',(-14.9000000000022,-24.,7.31327650886593));
#141129=CARTESIAN_POINT('Ctrl Pts',(-14.9000000000026,-24.,6.87608602594433));
#141130=CARTESIAN_POINT('Ctrl Pts',(-14.5320493798966,-24.,6.63997617964215));
#141131=CARTESIAN_POINT('Ctrl Pts',(-14.1640987597902,-24.,6.40386633333922));
#141132=CARTESIAN_POINT('Ctrl Pts',(-13.7666666666687,-24.,6.58602903455695));
#141133=CARTESIAN_POINT('Ctrl Pts',(-14.9000000000022,-24.4,7.31327650886593));
#141134=CARTESIAN_POINT('Ctrl Pts',(-14.9000000000026,-24.4,6.87608602594433));
#141135=CARTESIAN_POINT('Ctrl Pts',(-14.5320493798966,-24.4,6.63997617964215));
#141136=CARTESIAN_POINT('Ctrl Pts',(-14.1640987597902,-24.4,6.40386633333922));
#141137=CARTESIAN_POINT('Ctrl Pts',(-13.7666666666687,-24.4,6.58602903455695));
#141138=CARTESIAN_POINT('Ctrl Pts',(-14.5000000000022,-24.4,7.31327650886593));
#141139=CARTESIAN_POINT('Ctrl Pts',(-14.5000000000024,-24.4,7.09468126740513));
#141140=CARTESIAN_POINT('Ctrl Pts',(-14.3160246899494,-24.4,6.97662634425404));
#141141=CARTESIAN_POINT('Ctrl Pts',(-14.1320493798962,-24.4,6.85857142110258));
#141142=CARTESIAN_POINT('Ctrl Pts',(-13.9333333333355,-24.4,6.94965277171144));
#141143=CARTESIAN_POINT('',(-13.9333333333355,-24.4,6.94965277171144));
#141144=CARTESIAN_POINT('',(-13.7666666666687,-24.,6.58602903455695));
#141145=CARTESIAN_POINT('Origin',(-13.9333333333355,-24.,6.94965277171144));
#141146=CARTESIAN_POINT('Origin',(-14.1000000000022,-24.,7.31327650886593));
#141147=CARTESIAN_POINT('Origin',(-14.1000000000022,-24.4,7.31327650886593));
#141148=CARTESIAN_POINT('Origin',(-9.35,-24.,-3.05000000003699));
#141149=CARTESIAN_POINT('',(-12.7813870032049,-24.4,7.40110440257217));
#141150=CARTESIAN_POINT('',(-12.6566092939974,-24.,7.02106424247729));
#141151=CARTESIAN_POINT('Origin',(-12.7813870032049,-24.,7.40110440257217));
#141152=CARTESIAN_POINT('Origin',(-9.35,-24.,-3.05000000003699));
#141153=CARTESIAN_POINT('Origin',(-9.35,-24.4,-3.05000000003699));
#141154=CARTESIAN_POINT('Ctrl Pts',(-12.6566092939974,-24.,7.02106424247729));
#141155=CARTESIAN_POINT('Ctrl Pts',(-12.3737754104109,-24.,7.11392643912346));
#141156=CARTESIAN_POINT('Ctrl Pts',(-12.2766257747715,-24.,7.39531645594302));
#141157=CARTESIAN_POINT('Ctrl Pts',(-12.1794761391321,-24.,7.67670647276257));
#141158=CARTESIAN_POINT('Ctrl Pts',(-12.344773048718,-24.,7.92428539947466));
#141159=CARTESIAN_POINT('Ctrl Pts',(-12.6566092939974,-24.4,7.02106424247729));
#141160=CARTESIAN_POINT('Ctrl Pts',(-12.3737754104109,-24.4,7.11392643912346));
#141161=CARTESIAN_POINT('Ctrl Pts',(-12.2766257747715,-24.4,7.39531645594302));
#141162=CARTESIAN_POINT('Ctrl Pts',(-12.1794761391321,-24.4,7.67670647276257));
#141163=CARTESIAN_POINT('Ctrl Pts',(-12.344773048718,-24.4,7.92428539947466));
#141164=CARTESIAN_POINT('Ctrl Pts',(-12.7813870032049,-24.4,7.40110440257217));
#141165=CARTESIAN_POINT('Ctrl Pts',(-12.6871090420094,-24.4,7.4320584681209));
#141166=CARTESIAN_POINT('Ctrl Pts',(-12.6547258301296,-24.4,7.52585514039408));
#141167=CARTESIAN_POINT('Ctrl Pts',(-12.6223426182498,-24.4,7.61965181266726));
#141168=CARTESIAN_POINT('Ctrl Pts',(-12.6774415881118,-24.4,7.7021781215713));
#141169=CARTESIAN_POINT('Origin',(-12.8437758578086,-24.,7.59112448261961));
#141170=CARTESIAN_POINT('Origin',(-12.8437758578086,-24.4,7.59112448261961));
#141171=CARTESIAN_POINT('Origin',(-14.1000000000022,-15.9,7.31327650886593));
#141172=CARTESIAN_POINT('',(-13.7666666666687,-15.9,6.58602903455695));
#141173=CARTESIAN_POINT('',(-13.7666666666687,-15.9,6.58602903455696));
#141174=CARTESIAN_POINT('',(-14.9000000000022,-15.9,7.31327650886744));
#141175=CARTESIAN_POINT('Origin',(-14.1000000000022,-15.9,7.31327650886593));
#141176=CARTESIAN_POINT('',(-14.9000000000022,-15.9,7.31327650886744));
#141177=CARTESIAN_POINT('Origin',(-9.35,-15.9,-3.05000000003699));
#141178=CARTESIAN_POINT('',(-12.6566092939974,-15.9,7.02106424247729));
#141179=CARTESIAN_POINT('',(-12.6566092939974,-15.9,7.02106424247729));
#141180=CARTESIAN_POINT('Origin',(-9.35,-15.9,-3.05000000003699));
#141181=CARTESIAN_POINT('Origin',(-12.8437758578086,-15.9,7.59112448261961));
#141182=CARTESIAN_POINT('',(-12.344773048718,-15.9,7.92428539947466));
#141183=CARTESIAN_POINT('',(-12.344773048718,-15.9,7.92428539947466));
#141184=CARTESIAN_POINT('Origin',(-12.8437758578086,-15.9,7.59112448261961));
#141185=CARTESIAN_POINT('Origin',(-8.47750127826595,-15.9,10.5062825051013));
#141186=CARTESIAN_POINT('',(-13.1262499063286,-15.7,10.3984113176331));
#141187=CARTESIAN_POINT('',(-13.1262499063286,-15.9,10.3984113176331));
#141188=CARTESIAN_POINT('',(-11.8432759364864,-15.7,7.29784660110059));
#141189=CARTESIAN_POINT('Origin',(-8.47750127826606,-15.7,10.5062825051013));
#141190=CARTESIAN_POINT('',(-11.8432759364864,-15.9,7.29784660110059));
#141191=CARTESIAN_POINT('',(-11.8432759364864,-15.7,7.29784660110059));
#141192=CARTESIAN_POINT('Origin',(-8.47750127826606,-15.9,10.5062825051013));
#141193=CARTESIAN_POINT('Origin',(-16.5006469797908,-24.4,8.26690047634872));
#141194=CARTESIAN_POINT('Origin',(9.25,-24.,-3.05000000003699));
#141195=CARTESIAN_POINT('',(6.50051930977378,-24.4,-5.37386659131824));
#141196=CARTESIAN_POINT('',(10.822232934276,-24.4,-6.28853108686909));
#141197=CARTESIAN_POINT('Origin',(9.25,-24.4,-3.05000000003699));
#141198=CARTESIAN_POINT('',(10.9969254825289,-24.,-6.64836787429488));
#141199=CARTESIAN_POINT('Origin',(10.822232934276,-24.,-6.28853108686909));
#141200=CARTESIAN_POINT('',(6.10786135295693,-24.,-5.52527063630252));
#141201=CARTESIAN_POINT('Origin',(9.25,-24.,-3.05000000003699));
#141202=CARTESIAN_POINT('Ctrl Pts',(6.10786135295693,-24.,-5.52527063630252));
#141203=CARTESIAN_POINT('Ctrl Pts',(6.10786135295693,-24.0499820482805,
-5.52527063630252));
#141204=CARTESIAN_POINT('Ctrl Pts',(6.11697130800671,-24.0993789543098,
-5.52169964929554));
#141205=CARTESIAN_POINT('Ctrl Pts',(6.15258459790043,-24.1929052251116,
-5.50777794808829));
#141206=CARTESIAN_POINT('Ctrl Pts',(6.17903125593076,-24.2358257575373,
-5.49745098428682));
#141207=CARTESIAN_POINT('Ctrl Pts',(6.24702590778167,-24.310651122957,-5.47102267386603));
#141208=CARTESIAN_POINT('Ctrl Pts',(6.28847953134104,-24.3411725421678,
-5.45496465532731));
#141209=CARTESIAN_POINT('Ctrl Pts',(6.35969905795551,-24.374843044091,-5.42755871292796));
#141210=CARTESIAN_POINT('Ctrl Pts',(6.3863963541329,-24.3840391504725,-5.41731874741856));
#141211=CARTESIAN_POINT('Ctrl Pts',(6.44133303396774,-24.3965469939097,
-5.39633290753587));
#141212=CARTESIAN_POINT('Ctrl Pts',(6.46946853864456,-24.3997869203202,
-5.38562749022657));
#141213=CARTESIAN_POINT('Ctrl Pts',(6.49863348682723,-24.3999966111496,
-5.3745807206615));
#141214=CARTESIAN_POINT('Ctrl Pts',(6.49957638848971,-24.4,-5.37422363275274));
#141215=CARTESIAN_POINT('Ctrl Pts',(6.50051930977378,-24.4,-5.37386659131824));
#141216=CARTESIAN_POINT('Origin',(8.6,-24.,-0.741996797474058));
#141217=CARTESIAN_POINT('',(6.50005584528697,-24.4,-0.726681867288135));
#141218=CARTESIAN_POINT('',(6.5,-24.4,-0.741996797474059));
#141219=CARTESIAN_POINT('Origin',(8.6,-24.4,-0.741996797474058));
#141220=CARTESIAN_POINT('',(6.09999999999987,-24.,-0.741996797474059));
#141221=CARTESIAN_POINT('Origin',(6.5,-24.,-0.741996797474058));
#141222=CARTESIAN_POINT('',(6.10539366127889,-24.,-0.57786509787753));
#141223=CARTESIAN_POINT('Origin',(8.6,-24.,-0.741996797474058));
#141224=CARTESIAN_POINT('Ctrl Pts',(6.10539366127889,-24.,-0.57786509787753));
#141225=CARTESIAN_POINT('Ctrl Pts',(6.10539366127889,-24.0498896942439,
-0.57786509787753));
#141226=CARTESIAN_POINT('Ctrl Pts',(6.11451322581987,-24.0991909205108,
-0.581363208838736));
#141227=CARTESIAN_POINT('Ctrl Pts',(6.15017006506992,-24.1925840562392,
-0.59500177188774));
#141228=CARTESIAN_POINT('Ctrl Pts',(6.17666097503203,-24.2354570848239,
-0.605122847790428));
#141229=CARTESIAN_POINT('Ctrl Pts',(6.24481762949856,-24.3102959529889,
-0.631038317531357));
#141230=CARTESIAN_POINT('Ctrl Pts',(6.286411708346,-24.3408530312395,-0.6467985164514));
#141231=CARTESIAN_POINT('Ctrl Pts',(6.35799432343061,-24.374663196465,-0.673735247695183));
#141232=CARTESIAN_POINT('Ctrl Pts',(6.38491858000175,-24.3839243701463,
-0.683832560852813));
#141233=CARTESIAN_POINT('Ctrl Pts',(6.44032696159033,-24.3965207054082,
-0.704524093670561));
#141234=CARTESIAN_POINT('Ctrl Pts',(6.46870751806677,-24.3997833674192,
-0.715078832732869));
#141235=CARTESIAN_POINT('Ctrl Pts',(6.49813509433547,-24.3999965227155,
-0.725971094000813));
#141236=CARTESIAN_POINT('Ctrl Pts',(6.49909545970173,-24.4,-0.726326505204189));
#141237=CARTESIAN_POINT('Ctrl Pts',(6.50005584528697,-24.4,-0.726681867288135));
#141238=CARTESIAN_POINT('Origin',(6.5,-24.,-0.875559616590781));
#141239=CARTESIAN_POINT('',(6.5,-24.4,-5.32716721908225));
#141240=CARTESIAN_POINT('',(6.09999999999996,-24.,-5.32716721908225));
#141241=CARTESIAN_POINT('Origin',(6.5,-24.,-5.32716721908225));
#141242=CARTESIAN_POINT('',(6.1,-24.,-0.875559616590781));
#141243=CARTESIAN_POINT('',(6.5,-24.4,-0.875559616590781));
#141244=CARTESIAN_POINT('Origin',(8.6,-24.,-5.32716721908225));
#141245=CARTESIAN_POINT('Origin',(8.6,-24.,-5.32716721908225));
#141246=CARTESIAN_POINT('Origin',(8.6,-24.4,-5.32716721908225));
#141247=CARTESIAN_POINT('Origin',(15.1,-24.,-15.1));
#141248=CARTESIAN_POINT('',(14.5000000000093,-24.4,1.88436706275989));
#141249=CARTESIAN_POINT('',(7.67776706572399,-24.4,0.188531086795103));
#141250=CARTESIAN_POINT('Origin',(15.1,-24.4,-15.1));
#141251=CARTESIAN_POINT('',(7.5030745174711,-24.,0.548367874220887));
#141252=CARTESIAN_POINT('Origin',(7.67776706572399,-24.,0.188531086795103));
#141253=CARTESIAN_POINT('',(14.9000000000101,-24.,2.29381194316097));
#141254=CARTESIAN_POINT('Origin',(15.1,-24.,-15.1));
#141255=CARTESIAN_POINT('Ctrl Pts',(14.9000000000101,-24.,2.29381194316097));
#141256=CARTESIAN_POINT('Ctrl Pts',(14.9000000000101,-24.0372063911278,
2.29381194316097));
#141257=CARTESIAN_POINT('Ctrl Pts',(14.8948129067846,-24.0735699191394,
2.28856685120141));
#141258=CARTESIAN_POINT('Ctrl Pts',(14.8740024198881,-24.1476753497927,
2.26749744126914));
#141259=CARTESIAN_POINT('Ctrl Pts',(14.8573938075257,-24.1834986088516,
2.25067154531768));
#141260=CARTESIAN_POINT('Ctrl Pts',(14.8103292966639,-24.2573026498551,
2.20288809341834));
#141261=CARTESIAN_POINT('Ctrl Pts',(14.7773043663909,-24.2916813383689,
2.16928922247749));
#141262=CARTESIAN_POINT('Ctrl Pts',(14.7064030541314,-24.3455212572614,
2.09689931539744));
#141263=CARTESIAN_POINT('Ctrl Pts',(14.6680189554609,-24.3653387142152,
2.05759047151054));
#141264=CARTESIAN_POINT('Ctrl Pts',(14.5877079846584,-24.3926910207608,
1.97503908071189));
#141265=CARTESIAN_POINT('Ctrl Pts',(14.5450918954055,-24.3996912357087,
1.93107222774991));
#141266=CARTESIAN_POINT('Ctrl Pts',(14.5018850095481,-24.3999966689777,
1.88631975494096));
#141267=CARTESIAN_POINT('Ctrl Pts',(14.5009424821723,-24.4,1.88534342752733));
#141268=CARTESIAN_POINT('Ctrl Pts',(14.5000000000093,-24.4,1.88436706275988));
#141269=CARTESIAN_POINT('Origin',(9.25,-24.,-3.05000000003699));
#141270=CARTESIAN_POINT('Origin',(9.25,-24.,-3.05000000003699));
#141271=CARTESIAN_POINT('Origin',(9.25,-24.4,-3.05000000003699));
#141272=CARTESIAN_POINT('Origin',(15.1,-24.,-15.1));
#141273=CARTESIAN_POINT('',(14.899999999995,-24.,-5.70716730244972));
#141274=CARTESIAN_POINT('Origin',(15.1,-24.,-15.1));
#141275=CARTESIAN_POINT('',(14.4999999999957,-24.4,-5.32343232644195));
#141276=CARTESIAN_POINT('Origin',(15.1,-24.4,-15.1));
#141277=CARTESIAN_POINT('Ctrl Pts',(14.4999999999947,-24.4,-5.32343232644195));
#141278=CARTESIAN_POINT('Ctrl Pts',(14.5009421725839,-24.4,-5.32431844938398));
#141279=CARTESIAN_POINT('Ctrl Pts',(14.5018842876012,-24.3999966711656,
-5.32520463865279));
#141280=CARTESIAN_POINT('Ctrl Pts',(14.5439766889831,-24.3996992464686,
-5.36480374024527));
#141281=CARTESIAN_POINT('Ctrl Pts',(14.585204113278,-24.3930574770938,-5.40382483561486));
#141282=CARTESIAN_POINT('Ctrl Pts',(14.6632392768287,-24.3673887589727,
-5.47811640684428));
#141283=CARTESIAN_POINT('Ctrl Pts',(14.7005942801588,-24.3486989590473,
-5.51389178275807));
#141284=CARTESIAN_POINT('Ctrl Pts',(14.7720840023387,-24.2967337204839,
-5.58270349652219));
#141285=CARTESIAN_POINT('Ctrl Pts',(14.8063215119823,-24.2621974509716,
-5.61586680033281));
#141286=CARTESIAN_POINT('Ctrl Pts',(14.8552444363892,-24.1877890402947,
-5.66343415251741));
#141287=CARTESIAN_POINT('Ctrl Pts',(14.8725660409886,-24.1514550547615,
-5.68034270422849));
#141288=CARTESIAN_POINT('Ctrl Pts',(14.8943560092086,-24.0762686187014,
-5.70163858223181));
#141289=CARTESIAN_POINT('Ctrl Pts',(14.8998530362039,-24.0393411392285,
-5.70702343466547));
#141290=CARTESIAN_POINT('Ctrl Pts',(14.899999033164,-24.0010156783502,-5.70716635598636));
#141291=CARTESIAN_POINT('Ctrl Pts',(14.899999999995,-24.0005077614335,-5.70716730244972));
#141292=CARTESIAN_POINT('Ctrl Pts',(14.899999999995,-24.,-5.70716730244972));
#141293=CARTESIAN_POINT('Origin',(14.4999999999963,-24.,-5.02907458701124));
#141294=CARTESIAN_POINT('',(14.8999999999963,-24.,-5.02907458701199));
#141295=CARTESIAN_POINT('',(14.4999999999963,-24.4,-5.02907458701124));
#141296=CARTESIAN_POINT('Origin',(9.25,-23.,-3.05000000003699));
#141297=CARTESIAN_POINT('',(10.9969254825289,-23.,-6.64836787429488));
#141298=CARTESIAN_POINT('',(10.9969254825289,-23.,-6.64836787429488));
#141299=CARTESIAN_POINT('',(6.10786135295693,-23.,-5.52527063630252));
#141300=CARTESIAN_POINT('Origin',(9.25,-23.,-3.05000000003699));
#141301=CARTESIAN_POINT('',(6.10786135295693,-23.,-5.52527063630252));
#141302=CARTESIAN_POINT('Origin',(15.1,-23.,-15.1));
#141303=CARTESIAN_POINT('',(14.899999999995,-23.,-5.70716730244972));
#141304=CARTESIAN_POINT('',(14.899999999995,-23.,-5.70716730244972));
#141305=CARTESIAN_POINT('Origin',(15.1,-23.,-15.1));
#141306=CARTESIAN_POINT('Origin',(14.899999999995,-24.,-5.70716730244972));
#141307=CARTESIAN_POINT('',(14.9000000000101,-23.,2.29381194316097));
#141308=CARTESIAN_POINT('',(14.9000000000101,-23.,2.29381194316097));
#141309=CARTESIAN_POINT('',(14.9000000000101,-23.,2.29381194316097));
#141310=CARTESIAN_POINT('Origin',(15.1,-23.,-15.1));
#141311=CARTESIAN_POINT('',(7.5030745174711,-23.,0.548367874220887));
#141312=CARTESIAN_POINT('',(7.5030745174711,-23.,0.548367874220887));
#141313=CARTESIAN_POINT('Origin',(15.1,-23.,-15.1));
#141314=CARTESIAN_POINT('Origin',(18.4241839371104,-24.4,-4.3509818715809));
#141315=CARTESIAN_POINT('Origin',(9.25,-24.,-3.05000000003698));
#141316=CARTESIAN_POINT('',(2.7,-24.4,6.94499874933762));
#141317=CARTESIAN_POINT('',(2.34026510098007,-24.1749022653573,6.25536451384759));
#141318=CARTESIAN_POINT('Ctrl Pts',(2.69999999999885,-24.4,6.94499874933762));
#141319=CARTESIAN_POINT('Ctrl Pts',(2.69938450726401,-24.4,6.94385951802002));
#141320=CARTESIAN_POINT('Ctrl Pts',(2.69876909427848,-24.3999985793826,
6.94272023953584));
#141321=CARTESIAN_POINT('Ctrl Pts',(2.64677346130994,-24.3997585865573,
6.84644726556242));
#141322=CARTESIAN_POINT('Ctrl Pts',(2.59493609531246,-24.3896208822043,
6.74905244702875));
#141323=CARTESIAN_POINT('Ctrl Pts',(2.49299662506508,-24.3470125596353,
6.55473757267498));
#141324=CARTESIAN_POINT('Ctrl Pts',(2.44575302778059,-24.3139777797754,
6.46307557893406));
#141325=CARTESIAN_POINT('Ctrl Pts',(2.38360876150232,-24.2471543612356,
6.34125351739879));
#141326=CARTESIAN_POINT('Ctrl Pts',(2.36029692449435,-24.2155260551564,
6.2951814529358));
#141327=CARTESIAN_POINT('Ctrl Pts',(2.34093461680916,-24.1762742976837,
6.2566955074144));
#141328=CARTESIAN_POINT('Ctrl Pts',(2.34059937404234,-24.1755897903934,
6.25602908229548));
#141329=CARTESIAN_POINT('Ctrl Pts',(2.34026510098007,-24.1749022653573,
6.2553645138476));
#141330=CARTESIAN_POINT('',(3.60315794694916,-24.4,7.48165109691342));
#141331=CARTESIAN_POINT('Origin',(9.25,-24.4,-3.05000000003698));
#141332=CARTESIAN_POINT('',(3.79217358052409,-24.,7.12912721082302));
#141333=CARTESIAN_POINT('Origin',(3.60315794694916,-24.,7.48165109691342));
#141334=CARTESIAN_POINT('',(2.2595024242038,-24.,6.14431583328021));
#141335=CARTESIAN_POINT('Origin',(9.25,-24.,-3.05000000003698));
#141336=CARTESIAN_POINT('Ctrl Pts',(2.34026510098008,-24.1749022653573,
6.2553645138476));
#141337=CARTESIAN_POINT('Ctrl Pts',(2.3186515458434,-24.1523299103811,6.22564587553467));
#141338=CARTESIAN_POINT('Ctrl Pts',(2.29829947779473,-24.1261400525693,
6.19766178196775));
#141339=CARTESIAN_POINT('Ctrl Pts',(2.27605378247541,-24.081552511153,6.16707395090368));
#141340=CARTESIAN_POINT('Ctrl Pts',(2.26879935823777,-24.0627177020031,
6.15709911757692));
#141341=CARTESIAN_POINT('Ctrl Pts',(2.26159865293807,-24.0317064411739,
6.14719814778983));
#141342=CARTESIAN_POINT('Ctrl Pts',(2.25950242420381,-24.0145787786788,
6.14431583328023));
#141343=CARTESIAN_POINT('Ctrl Pts',(2.2595024242038,-24.,6.14431583328023));
#141344=CARTESIAN_POINT('Ctrl Pts',(3.79217358052409,-24.,7.12912721082302));
#141345=CARTESIAN_POINT('Ctrl Pts',(4.03063238157239,-24.,7.25698362889877));
#141346=CARTESIAN_POINT('Ctrl Pts',(4.09266745560454,-24.,7.52034936894553));
#141347=CARTESIAN_POINT('Ctrl Pts',(4.15470252963669,-24.,7.7837151089923));
#141348=CARTESIAN_POINT('Ctrl Pts',(3.99837965786692,-24.,8.00456126178243));
#141349=CARTESIAN_POINT('Ctrl Pts',(3.79217358052409,-24.4,7.12912721082302));
#141350=CARTESIAN_POINT('Ctrl Pts',(4.03063238157239,-24.4,7.25698362889877));
#141351=CARTESIAN_POINT('Ctrl Pts',(4.09266745560454,-24.4,7.52034936894553));
#141352=CARTESIAN_POINT('Ctrl Pts',(4.15470252963669,-24.4,7.7837151089923));
#141353=CARTESIAN_POINT('Ctrl Pts',(3.99837965786692,-24.4,8.00456126178243));
#141354=CARTESIAN_POINT('Ctrl Pts',(3.60315794694916,-24.4,7.48165109691342));
#141355=CARTESIAN_POINT('Ctrl Pts',(3.68264421396526,-24.4,7.52426990293866));
#141356=CARTESIAN_POINT('Ctrl Pts',(3.70332257197598,-24.4,7.61205848295425));
#141357=CARTESIAN_POINT('Ctrl Pts',(3.7240009299867,-24.4,7.69984706296984));
#141358=CARTESIAN_POINT('Ctrl Pts',(3.67189330606344,-24.4,7.77346244723322));
#141359=CARTESIAN_POINT('',(3.67189330606344,-24.4,7.77346244723322));
#141360=CARTESIAN_POINT('',(3.99837965786692,-24.,8.00456126178243));
#141361=CARTESIAN_POINT('Origin',(3.67189330606344,-24.,7.77346244723322));
#141362=CARTESIAN_POINT('Origin',(3.5086501301617,-24.,7.65791303995861));
#141363=CARTESIAN_POINT('Origin',(3.5086501301617,-24.4,7.65791303995861));
#141364=CARTESIAN_POINT('Origin',(7.1,-24.,10.2));
#141365=CARTESIAN_POINT('',(2.99999999999999,-24.4,11.1110433579144));
#141366=CARTESIAN_POINT('',(2.99999999999999,-24.3874411221899,10.2674423504838));
#141367=CARTESIAN_POINT('Ctrl Pts',(2.99999999999999,-24.4,11.1110433579144));
#141368=CARTESIAN_POINT('Ctrl Pts',(2.99999999999999,-24.4,11.0262276390181));
#141369=CARTESIAN_POINT('Ctrl Pts',(2.99999999999999,-24.3984722201137,
10.9244602435706));
#141370=CARTESIAN_POINT('Ctrl Pts',(2.99999999999999,-24.3933294319036,
10.6618000221546));
#141371=CARTESIAN_POINT('Ctrl Pts',(2.99999999999999,-24.3882215189204,
10.4523039043015));
#141372=CARTESIAN_POINT('Ctrl Pts',(2.99999999999999,-24.3874411221899,
10.2674423504838));
#141373=CARTESIAN_POINT('',(5.0999999999996,-24.4,13.8932370625237));
#141374=CARTESIAN_POINT('Origin',(7.1,-24.4,10.2));
#141375=CARTESIAN_POINT('',(5.4999999999996,-24.,13.6467375879226));
#141376=CARTESIAN_POINT('Ctrl Pts',(5.4999999999996,-24.,13.6467375879226));
#141377=CARTESIAN_POINT('Ctrl Pts',(5.4999999999996,-24.043623376554,13.6467375879226));
#141378=CARTESIAN_POINT('Ctrl Pts',(5.49287202409357,-24.0865043128084,
13.6512950950102));
#141379=CARTESIAN_POINT('Ctrl Pts',(5.46477408706084,-24.170362369205,13.6691611438001));
#141380=CARTESIAN_POINT('Ctrl Pts',(5.4433360290039,-24.2097990038533,13.6827576452369));
#141381=CARTESIAN_POINT('Ctrl Pts',(5.38582695891643,-24.2843713974945,
13.7189116659061));
#141382=CARTESIAN_POINT('Ctrl Pts',(5.34841009281781,-24.3171808215248,
13.7422645921124));
#141383=CARTESIAN_POINT('Ctrl Pts',(5.27605644800346,-24.3610238413703,
13.7868820291226));
#141384=CARTESIAN_POINT('Ctrl Pts',(5.2427453790336,-24.3753624648512,13.8072640754931));
#141385=CARTESIAN_POINT('Ctrl Pts',(5.17389448060471,-24.3947460974665,
13.8490138439509));
#141386=CARTESIAN_POINT('Ctrl Pts',(5.13833439111214,-24.3997525395457,
13.8703923861214));
#141387=CARTESIAN_POINT('Ctrl Pts',(5.10178368010527,-24.3999970171617,
13.8921744392635));
#141388=CARTESIAN_POINT('Ctrl Pts',(5.10089186521198,-24.4,13.8927057932241));
#141389=CARTESIAN_POINT('Ctrl Pts',(5.0999999999996,-24.4,13.8932370625237));
#141390=CARTESIAN_POINT('Origin',(7.1,-24.,10.2));
#141391=CARTESIAN_POINT('',(2.92511356012264,-24.4,9.74138991056875));
#141392=CARTESIAN_POINT('Origin',(7.1,-24.4,10.2));
#141393=CARTESIAN_POINT('Ctrl Pts',(2.99999999999999,-24.3874411221899,
10.2674423504838));
#141394=CARTESIAN_POINT('Ctrl Pts',(2.96910221504019,-24.3946244822332,
10.0906889153863));
#141395=CARTESIAN_POINT('Ctrl Pts',(2.94468295018221,-24.3998756487825,
9.91725158038943));
#141396=CARTESIAN_POINT('Ctrl Pts',(2.92555818538903,-24.3999992746164,
9.74540441364033));
#141397=CARTESIAN_POINT('Ctrl Pts',(2.9253355193279,-24.4,9.74339719961947));
#141398=CARTESIAN_POINT('Ctrl Pts',(2.92511356012264,-24.4,9.74138991056876));
#141399=CARTESIAN_POINT('Origin',(9.25,-10.3,-3.05000000003698));
#141400=CARTESIAN_POINT('',(3.79217358052409,-19.450790764769,7.12912721082303));
#141401=CARTESIAN_POINT('',(3.79217358052409,-10.3,7.12912721082302));
#141402=CARTESIAN_POINT('',(4.20575266919785,-19.0059957824439,7.34028723688267));
#141403=CARTESIAN_POINT('Ctrl Pts',(3.79217358052409,-19.450790764769,7.12912721082303));
#141404=CARTESIAN_POINT('Ctrl Pts',(3.92894707189985,-19.3006588374492,
7.20246217945552));
#141405=CARTESIAN_POINT('Ctrl Pts',(4.06689863056173,-19.152147384955,7.27287676999272));
#141406=CARTESIAN_POINT('Ctrl Pts',(4.20575266919785,-19.0059957824439,
7.34028723688266));
#141407=CARTESIAN_POINT('',(4.20575266919785,-10.8312625177592,7.34028723688267));
#141408=CARTESIAN_POINT('',(4.20575266919785,-10.3,7.34028723688267));
#141409=CARTESIAN_POINT('',(3.96202237101811,-10.5713843344211,7.218388023182));
#141410=CARTESIAN_POINT('Ctrl Pts',(3.96202237101812,-10.5713843344211,
7.218388023182));
#141411=CARTESIAN_POINT('Ctrl Pts',(4.04291734656614,-10.658723483699,7.26004702749969));
#141412=CARTESIAN_POINT('Ctrl Pts',(4.12417858841689,-10.7454012583632,
7.30068488231253));
#141413=CARTESIAN_POINT('Ctrl Pts',(4.20575266919785,-10.8312625177592,
7.34028723688266));
#141414=CARTESIAN_POINT('',(3.96202237101811,-10.3,7.218388023182));
#141415=CARTESIAN_POINT('',(3.96202237101811,-10.3,7.218388023182));
#141416=CARTESIAN_POINT('',(0.753380028274003,-10.3,4.77367874183802));
#141417=CARTESIAN_POINT('Origin',(9.25,-10.3,-3.05000000003698));
#141418=CARTESIAN_POINT('',(0.753380028239878,-16.1330170457644,4.77367874180096));
#141419=CARTESIAN_POINT('',(0.753380028274003,-10.3,4.77367874183802));
#141420=CARTESIAN_POINT('',(1.06586901379278,-16.2754420649312,5.09999999999999));
#141421=CARTESIAN_POINT('Ctrl Pts',(0.753380028237917,-16.1330170457761,
4.77367874179883));
#141422=CARTESIAN_POINT('Ctrl Pts',(0.827841722403025,-16.1601570631323,
4.85454513964712));
#141423=CARTESIAN_POINT('Ctrl Pts',(0.902862648270401,-16.1920729653029,
4.9336847969506));
#141424=CARTESIAN_POINT('Ctrl Pts',(1.00701139399119,-16.2437237651945,
5.04057678208364));
#141425=CARTESIAN_POINT('Ctrl Pts',(1.03650440201479,-16.2591791978977,
5.07051241360133));
#141426=CARTESIAN_POINT('Ctrl Pts',(1.06586901379278,-16.2754420649312,
5.09999999999999));
#141427=CARTESIAN_POINT('',(2.33335341373322,-15.866448662099,6.19999999999999));
#141428=CARTESIAN_POINT('Ctrl Pts',(1.06586901379278,-16.2754420649312,
5.09999999999999));
#141429=CARTESIAN_POINT('Ctrl Pts',(1.08669238122262,-16.2630712876422,
5.12091057259128));
#141430=CARTESIAN_POINT('Ctrl Pts',(1.10765038033297,-16.25092019906,5.14179603489229));
#141431=CARTESIAN_POINT('Ctrl Pts',(1.497746484828,-16.0303633776365,5.52755122732));
#141432=CARTESIAN_POINT('Ctrl Pts',(1.90762157781984,-15.8909333123056,
5.88166090275419));
#141433=CARTESIAN_POINT('Ctrl Pts',(2.33335341373322,-15.866448662099,6.19999999999999));
#141434=CARTESIAN_POINT('',(2.33335341373322,-20.533551337901,6.19999999999999));
#141435=CARTESIAN_POINT('Ctrl Pts',(2.33335341373322,-15.866448662099,6.19999999999999));
#141436=CARTESIAN_POINT('Ctrl Pts',(2.50458376491819,-16.0376644900874,
6.328036737728));
#141437=CARTESIAN_POINT('Ctrl Pts',(2.6600024453182,-16.2320241427132,6.43676776431048));
#141438=CARTESIAN_POINT('Ctrl Pts',(2.94074307716937,-16.6760756161761,
6.62621602757801));
#141439=CARTESIAN_POINT('Ctrl Pts',(3.07603900473761,-16.9632728375209,
6.71196137328473));
#141440=CARTESIAN_POINT('Ctrl Pts',(3.25582314080075,-17.5745988720813,
6.82337466030348));
#141441=CARTESIAN_POINT('Ctrl Pts',(3.3,-17.8987366888933,6.84949493657468));
#141442=CARTESIAN_POINT('Ctrl Pts',(3.3,-18.5012633111067,6.84949493657468));
#141443=CARTESIAN_POINT('Ctrl Pts',(3.25582314080075,-18.8254011279188,
6.82337466030348));
#141444=CARTESIAN_POINT('Ctrl Pts',(3.07603900473761,-19.4367271624791,
6.71196137328473));
#141445=CARTESIAN_POINT('Ctrl Pts',(2.94074307716937,-19.7239243838239,
6.62621602757801));
#141446=CARTESIAN_POINT('Ctrl Pts',(2.6600024453182,-20.1679758572868,6.43676776431048));
#141447=CARTESIAN_POINT('Ctrl Pts',(2.50458376491819,-20.3623355099126,
6.328036737728));
#141448=CARTESIAN_POINT('Ctrl Pts',(2.33335341373322,-20.533551337901,6.19999999999999));
#141449=CARTESIAN_POINT('',(2.2595024242038,-20.5281396051547,6.14431583328021));
#141450=CARTESIAN_POINT('Ctrl Pts',(2.33335341373322,-20.533551337901,6.19999999999999));
#141451=CARTESIAN_POINT('Ctrl Pts',(2.30868348710064,-20.5321325233486,
6.18155317147826));
#141452=CARTESIAN_POINT('Ctrl Pts',(2.28406566649289,-20.530325389613,6.16299142467695));
#141453=CARTESIAN_POINT('Ctrl Pts',(2.2595024242038,-20.5281396051547,6.14431583328021));
#141454=CARTESIAN_POINT('',(2.2595024242038,-10.3,6.14431583328021));
#141455=CARTESIAN_POINT('Origin',(3.5086501301617,-10.3,7.65791303995861));
#141456=CARTESIAN_POINT('',(3.99837965786692,-18.7372583002031,8.00456126178243));
#141457=CARTESIAN_POINT('',(3.99837965786692,-10.3,8.00456126178243));
#141458=CARTESIAN_POINT('Ctrl Pts',(3.99837965786692,-18.7372583002031,
8.00456126178243));
#141459=CARTESIAN_POINT('Ctrl Pts',(4.03732967732535,-18.7372583002031,
7.94953436871739));
#141460=CARTESIAN_POINT('Ctrl Pts',(4.06767008908906,-18.7513211403521,
7.88573623665628));
#141461=CARTESIAN_POINT('Ctrl Pts',(4.10395213346578,-18.8019424520368,
7.75802399444114));
#141462=CARTESIAN_POINT('Ctrl Pts',(4.11016145474904,-18.8381784329961,
7.69405845595038));
#141463=CARTESIAN_POINT('Ctrl Pts',(4.10559496170999,-18.9320481917235,
7.5550706062975));
#141464=CARTESIAN_POINT('Ctrl Pts',(4.0852693413741,-19.0015084112899,7.47411890040826));
#141465=CARTESIAN_POINT('Ctrl Pts',(4.01784669559515,-19.1480722446802,
7.33082157667108));
#141466=CARTESIAN_POINT('Ctrl Pts',(3.97063386025383,-19.2251902002209,
7.26854514914513));
#141467=CARTESIAN_POINT('Ctrl Pts',(3.88247112583277,-19.3459928754066,
7.18595811268406));
#141468=CARTESIAN_POINT('Ctrl Pts',(3.83978846512759,-19.3985254147898,
7.15465727541167));
#141469=CARTESIAN_POINT('Ctrl Pts',(3.79217358052409,-19.450790764769,7.12912721082302));
#141470=CARTESIAN_POINT('Origin',(7.1,-24.4,10.2));
#141471=CARTESIAN_POINT('',(5.4999999999996,-18.7372583002031,13.6467375879226));
#141472=CARTESIAN_POINT('',(5.4999999999996,-24.4,13.6467375879226));
#141473=CARTESIAN_POINT('',(5.32295533693765,-18.7372583001967,13.5588855689756));
#141474=CARTESIAN_POINT('Origin',(7.1,-18.7372583002031,10.2));
#141475=CARTESIAN_POINT('',(3.43393944403533,-22.3025065380446,11.2));
#141476=CARTESIAN_POINT('Ctrl Pts',(5.32295533692251,-18.7372583001948,
13.5588855689689));
#141477=CARTESIAN_POINT('Ctrl Pts',(5.31543781191846,-18.8117391408375,
13.5549083636091));
#141478=CARTESIAN_POINT('Ctrl Pts',(5.30636187833369,-18.88600809146,13.5500757822301));
#141479=CARTESIAN_POINT('Ctrl Pts',(5.24790374924743,-19.2933639529239,
13.5185380397245));
#141480=CARTESIAN_POINT('Ctrl Pts',(5.16846423487534,-19.6208923989795,
13.4749524190562));
#141481=CARTESIAN_POINT('Ctrl Pts',(4.92922830421624,-20.319228523667,13.3228547377802));
#141482=CARTESIAN_POINT('Ctrl Pts',(4.75571610594006,-20.6793655488159,
13.2024143398389));
#141483=CARTESIAN_POINT('Ctrl Pts',(4.55878273226527,-21.,13.0252813661947));
#141484=CARTESIAN_POINT('Ctrl Pts',(4.41276324398597,-21.2377396863364,
12.8939432101154));
#141485=CARTESIAN_POINT('Ctrl Pts',(4.24917117087481,-21.4582044314781,
12.7230082485295));
#141486=CARTESIAN_POINT('Ctrl Pts',(3.8930603371699,-21.8849218960272,12.2680071579846));
#141487=CARTESIAN_POINT('Ctrl Pts',(3.67726565735291,-22.0909313543125,
11.9071305384491));
#141488=CARTESIAN_POINT('Ctrl Pts',(3.49330913993195,-22.2523441140072,
11.4010209787851));
#141489=CARTESIAN_POINT('Ctrl Pts',(3.46159216327806,-22.2793602584562,
11.301376543281));
#141490=CARTESIAN_POINT('Ctrl Pts',(3.43393944403533,-22.3025065380446,
11.2));
#141491=CARTESIAN_POINT('',(3.40807692379814,-18.7372583002031,9.30016445979934));
#141492=CARTESIAN_POINT('Ctrl Pts',(3.43393944403533,-22.3025065380446,
11.2));
#141493=CARTESIAN_POINT('Ctrl Pts',(3.38538330748545,-22.1110106189331,
11.0219902630444));
#141494=CARTESIAN_POINT('Ctrl Pts',(3.35318020866045,-21.9134486134528,
10.8519898266241));
#141495=CARTESIAN_POINT('Ctrl Pts',(3.31274055197059,-21.5315989463264,
10.546834566985));
#141496=CARTESIAN_POINT('Ctrl Pts',(3.30151522006465,-21.2950143493326,
10.3728117862555));
#141497=CARTESIAN_POINT('Ctrl Pts',(3.29999012118781,-21.0613145694522,
10.2176726278714));
#141498=CARTESIAN_POINT('Ctrl Pts',(3.29994830585796,-21.0309600750686,
10.1978078267685));
#141499=CARTESIAN_POINT('Ctrl Pts',(3.30006446200803,-21.,10.1778661547474));
#141500=CARTESIAN_POINT('Ctrl Pts',(3.30178228928965,-20.5421330548263,
9.88294980103293));
#141501=CARTESIAN_POINT('Ctrl Pts',(3.33837991246433,-20.0541154947359,
9.63659924188226));
#141502=CARTESIAN_POINT('Ctrl Pts',(3.38373137758155,-19.3064142028621,
9.40336523861826));
#141503=CARTESIAN_POINT('Ctrl Pts',(3.39632541877288,-19.0737391684594,
9.34905336737836));
#141504=CARTESIAN_POINT('Ctrl Pts',(3.4059639616169,-18.8035071049694,9.30886402172908));
#141505=CARTESIAN_POINT('Ctrl Pts',(3.40706313605649,-18.7704004107024,
9.30432391582275));
#141506=CARTESIAN_POINT('Ctrl Pts',(3.40807692379814,-18.7372583002031,
9.30016445979934));
#141507=CARTESIAN_POINT('Origin',(7.1,-18.7372583002031,10.2));
#141508=CARTESIAN_POINT('Origin',(5.09999999999967,-24.,10.2414572515418));
#141509=CARTESIAN_POINT('',(5.09999999999956,-24.4,16.));
#141510=CARTESIAN_POINT('',(5.09999999999967,-24.4,10.2414572515418));
#141511=CARTESIAN_POINT('',(5.49999999999956,-24.,16.));
#141512=CARTESIAN_POINT('Origin',(5.09999999999956,-24.,16.));
#141513=CARTESIAN_POINT('',(5.49999999999967,-24.,10.2414572515418));
#141514=CARTESIAN_POINT('Origin',(3.04851216033843,-24.4,10.2415765003998));
#141515=CARTESIAN_POINT('',(2.99999999999999,-24.4,16.2));
#141516=CARTESIAN_POINT('',(2.99999999999999,-24.4,14.2207882501964));
#141517=CARTESIAN_POINT('',(4.89999999999956,-24.4,16.2));
#141518=CARTESIAN_POINT('',(-0.954150666147262,-24.4,16.2));
#141519=CARTESIAN_POINT('Origin',(4.89999999999956,-24.4,16.));
#141520=CARTESIAN_POINT('Origin',(2.99999999999999,-22.8,18.199999999993));
#141521=CARTESIAN_POINT('',(2.99999999999999,-24.,11.1958530281318));
#141522=CARTESIAN_POINT('Origin',(2.99999999999999,-24.,9.96025655312461));
#141523=CARTESIAN_POINT('',(2.99999999999999,-22.6247197197547,11.1958530281318));
#141524=CARTESIAN_POINT('',(2.99999999999999,-22.8,11.1958530281318));
#141525=CARTESIAN_POINT('',(2.99999999999999,-22.6297291113566,11.2));
#141526=CARTESIAN_POINT('Ctrl Pts',(2.99999999999999,-22.6297291113566,
11.2));
#141527=CARTESIAN_POINT('Ctrl Pts',(2.99999999999999,-22.6272234444407,
11.1979253409942));
#141528=CARTESIAN_POINT('Ctrl Pts',(2.99999999999999,-22.6247197197547,
11.1958530281318));
#141529=CARTESIAN_POINT('',(3.00000000000928,-22.629729097456,14.395853022084));
#141530=CARTESIAN_POINT('',(2.99999999999999,-22.6297291113566,11.6));
#141531=CARTESIAN_POINT('',(2.99999999999999,-21.2805843601499,16.3958530281318));
#141532=CARTESIAN_POINT('Ctrl Pts',(2.99999999999999,-21.2805843601499,
16.3958530281318));
#141533=CARTESIAN_POINT('Ctrl Pts',(2.99999999999999,-21.8817576684837,
15.5754919688216));
#141534=CARTESIAN_POINT('Ctrl Pts',(2.99999999999999,-22.6297291101028,
14.3958530301092));
#141535=CARTESIAN_POINT('',(2.99999999999999,-21.7512078069108,16.6));
#141536=CARTESIAN_POINT('Ctrl Pts',(2.99999999999999,-21.2805843601499,
16.3958530281318));
#141537=CARTESIAN_POINT('Ctrl Pts',(2.99999999999999,-21.3068354153031,
16.4293435697378));
#141538=CARTESIAN_POINT('Ctrl Pts',(2.99999999999999,-21.3399515768309,
16.4595872648773));
#141539=CARTESIAN_POINT('Ctrl Pts',(2.99999999999999,-21.4209067702055,
16.5184033153281));
#141540=CARTESIAN_POINT('Ctrl Pts',(2.99999999999999,-21.4862885611465,
16.549963078009));
#141541=CARTESIAN_POINT('Ctrl Pts',(2.99999999999999,-21.6069095263048,
16.5880803850168));
#141542=CARTESIAN_POINT('Ctrl Pts',(2.99999999999999,-21.6852076397025,
16.6));
#141543=CARTESIAN_POINT('Ctrl Pts',(2.99999999999999,-21.7512078069108,
16.6));
#141544=CARTESIAN_POINT('',(2.99999999999999,-24.,16.6));
#141545=CARTESIAN_POINT('',(2.99999999999999,-16.55,16.6));
#141546=CARTESIAN_POINT('Origin',(3.,-24.,16.2));
#141547=CARTESIAN_POINT('Ctrl Pts',(5.49999999999956,-24.,16.));
#141548=CARTESIAN_POINT('Ctrl Pts',(5.49999999999955,-24.,16.6));
#141549=CARTESIAN_POINT('Ctrl Pts',(4.89999999999956,-24.,16.6));
#141550=CARTESIAN_POINT('Ctrl Pts',(5.49999999999956,-24.4,16.));
#141551=CARTESIAN_POINT('Ctrl Pts',(5.49999999999955,-24.4,16.6));
#141552=CARTESIAN_POINT('Ctrl Pts',(4.89999999999956,-24.4,16.6));
#141553=CARTESIAN_POINT('Ctrl Pts',(5.09999999999956,-24.4,16.));
#141554=CARTESIAN_POINT('Ctrl Pts',(5.09999999999956,-24.4,16.2));
#141555=CARTESIAN_POINT('Ctrl Pts',(4.89999999999956,-24.4,16.2));
#141556=CARTESIAN_POINT('',(4.89999999999956,-24.,16.6));
#141557=CARTESIAN_POINT('Origin',(4.89999999999956,-24.,16.2));
#141558=CARTESIAN_POINT('Origin',(4.89999999999956,-24.,16.));
#141559=CARTESIAN_POINT('Origin',(-0.954150666147262,-24.,16.2));
#141560=CARTESIAN_POINT('',(-0.954150666147262,-24.,16.6));
#141561=CARTESIAN_POINT('Origin',(5.49999999999967,-16.5524667901538,10.2413380026838));
#141562=CARTESIAN_POINT('',(5.49999999999956,-12.5846724700528,16.));
#141563=CARTESIAN_POINT('',(5.49999999999956,-13.4262333950769,16.));
#141564=CARTESIAN_POINT('',(5.49999999999956,-12.5535531013342,15.9538461538416));
#141565=CARTESIAN_POINT('Origin',(5.49999999999956,-12.238262308539,16.1999999999999));
#141566=CARTESIAN_POINT('',(5.49999999999963,-12.5141521334422,12.4978250586149));
#141567=CARTESIAN_POINT('Origin',(5.49999999999959,-14.8,14.199999999963));
#141568=CARTESIAN_POINT('',(5.4999999999996,-17.7372583002031,12.4978250586149));
#141569=CARTESIAN_POINT('',(5.4999999999996,-24.4,12.4978250586149));
#141570=CARTESIAN_POINT('Ctrl Pts',(5.4999999999996,-18.737258300203,13.6467375879226));
#141571=CARTESIAN_POINT('Ctrl Pts',(5.49999999999962,-18.1372583002031,
12.985242495291));
#141572=CARTESIAN_POINT('Ctrl Pts',(5.49999999999962,-17.7372583002032,
12.4978250586151));
#141573=CARTESIAN_POINT('',(5.49999999999962,-14.8,12.549999999963));
#141574=CARTESIAN_POINT('Origin',(5.49999999999959,-14.8,14.199999999963));
#141575=CARTESIAN_POINT('Origin',(4.89999999999956,-13.4262333950769,16.));
#141576=CARTESIAN_POINT('',(4.89999999999956,-12.238262308539,16.6));
#141577=CARTESIAN_POINT('',(4.89999999999956,-13.4262333950769,16.6));
#141578=CARTESIAN_POINT('Ctrl Pts',(5.49999999999956,-12.5846724700528,
16.));
#141579=CARTESIAN_POINT('Ctrl Pts',(5.49999999999956,-12.5940887807114,
16.0163095284805));
#141580=CARTESIAN_POINT('Ctrl Pts',(5.49932802856564,-12.6023867107517,
16.0333635630483));
#141581=CARTESIAN_POINT('Ctrl Pts',(5.49367232615558,-12.629123862268,16.0998863384286));
#141582=CARTESIAN_POINT('Ctrl Pts',(5.48249827863786,-12.638262308539,16.1524460685814));
#141583=CARTESIAN_POINT('Ctrl Pts',(5.44738870998965,-12.638262308539,16.2517509248842));
#141584=CARTESIAN_POINT('Ctrl Pts',(5.42063930011652,-12.6277423449409,
16.3033655674568));
#141585=CARTESIAN_POINT('Ctrl Pts',(5.35597524083088,-12.5914895471395,
16.3939321009808));
#141586=CARTESIAN_POINT('Ctrl Pts',(5.31811815076933,-12.56591478853,16.4329882568349));
#141587=CARTESIAN_POINT('Ctrl Pts',(5.22634454907965,-12.4998649350384,
16.5084457181327));
#141588=CARTESIAN_POINT('Ctrl Pts',(5.16276007011936,-12.4504558640288,
16.5438950744375));
#141589=CARTESIAN_POINT('Ctrl Pts',(5.03098863695038,-12.3452667223669,
16.5896665496838));
#141590=CARTESIAN_POINT('Ctrl Pts',(4.96277844627394,-12.289520695278,16.5999999999999));
#141591=CARTESIAN_POINT('Ctrl Pts',(4.89999999999955,-12.238262308539,16.5999999999999));
#141592=CARTESIAN_POINT('Origin',(-4.95681349263295,-10.3,16.6));
#141593=CARTESIAN_POINT('',(-3.65042002992564,-15.3215437309242,16.6));
#141594=CARTESIAN_POINT('Origin',(1.12776416393948E-15,-18.2,16.6));
#141595=CARTESIAN_POINT('',(-3.65042002992564,-10.3,16.6));
#141596=CARTESIAN_POINT('',(-3.65042002992564,-10.3,16.6));
#141597=CARTESIAN_POINT('',(-7.62176460923847,-10.3,16.6));
#141598=CARTESIAN_POINT('',(-1.35407769578341,-10.3,16.6));
#141599=CARTESIAN_POINT('',(-7.62176460923847,-15.7,16.6));
#141600=CARTESIAN_POINT('',(-7.62176460923847,-10.3,16.6));
#141601=CARTESIAN_POINT('',(-8.50588745028793,-15.7,16.6));
#141602=CARTESIAN_POINT('',(-8.50588745028793,-15.7,16.6));
#141603=CARTESIAN_POINT('',(-8.50588745028793,-16.55,16.6));
#141604=CARTESIAN_POINT('',(-0.755737525613271,-10.3,16.6));
#141605=CARTESIAN_POINT('',(-0.755737525613271,-21.1,16.6));
#141606=CARTESIAN_POINT('',(10.8999999999996,-10.3,16.6));
#141607=CARTESIAN_POINT('',(7.27432905053284,-10.3,16.6));
#141608=CARTESIAN_POINT('',(10.8999999999996,-11.8066740906056,16.6));
#141609=CARTESIAN_POINT('',(10.8999999999996,-10.3,16.6));
#141610=CARTESIAN_POINT('',(8.28666521865374,-11.8066740906056,16.6));
#141611=CARTESIAN_POINT('',(13.8999999999996,-11.8066740906056,16.6));
#141612=CARTESIAN_POINT('',(7.96034186369749,-12.238262308539,16.6));
#141613=CARTESIAN_POINT('Ctrl Pts',(8.28666521865374,-11.8066740906056,
16.6));
#141614=CARTESIAN_POINT('Ctrl Pts',(8.1108270602786,-12.0320528721918,16.6));
#141615=CARTESIAN_POINT('Ctrl Pts',(7.96034186369749,-12.238262308539,16.6));
#141616=CARTESIAN_POINT('',(8.49999999999956,-12.238262308539,16.6));
#141617=CARTESIAN_POINT('Origin',(3.234855708905,-24.,10.646656929178));
#141618=CARTESIAN_POINT('',(2.7,-24.4,9.08346239821099));
#141619=CARTESIAN_POINT('',(3.234855708905,-24.4,10.646656929178));
#141620=CARTESIAN_POINT('',(2.3,-24.,9.14999999999999));
#141621=CARTESIAN_POINT('Origin',(2.7,-24.,9.08346239821099));
#141622=CARTESIAN_POINT('',(2.85639594574927,-24.,10.776149043502));
#141623=CARTESIAN_POINT('Origin',(2.7,-24.,9.6957882501999));
#141624=CARTESIAN_POINT('',(2.3,-24.,6.19999999999999));
#141625=CARTESIAN_POINT('Origin',(2.7,-24.,6.74999999999999));
#141626=CARTESIAN_POINT('',(2.3,-24.,9.6957882501999));
#141627=CARTESIAN_POINT('',(2.7,-24.4,9.6957882501999));
#141628=CARTESIAN_POINT('Origin',(2.99999999999999,-22.8,11.1958530281318));
#141629=CARTESIAN_POINT('',(2.3,-20.5664319132398,9.14999999999999));
#141630=CARTESIAN_POINT('',(2.3,-22.8,9.14999999999999));
#141631=CARTESIAN_POINT('Ctrl Pts',(2.99999999999999,-22.6247197197547,
11.1958530281318));
#141632=CARTESIAN_POINT('Ctrl Pts',(2.54392068220353,-21.3234927580979,
9.86289409472867));
#141633=CARTESIAN_POINT('Ctrl Pts',(2.3,-20.5664319132398,9.14999999999999));
#141634=CARTESIAN_POINT('Origin',(2.3,-22.8,9.14999999999999));
#141635=CARTESIAN_POINT('',(2.3,-20.5664319132398,6.19999999999997));
#141636=CARTESIAN_POINT('',(2.3,-22.8,6.19999999999999));
#141637=CARTESIAN_POINT('',(2.3,-20.5664319132399,11.6));
#141638=CARTESIAN_POINT('Origin',(7.1,-24.,10.2));
#141639=CARTESIAN_POINT('',(11.0937451095552,-24.4,11.499999999963));
#141640=CARTESIAN_POINT('',(11.2999891909638,-24.4,10.1904713176424));
#141641=CARTESIAN_POINT('Origin',(7.1,-24.4,10.2));
#141642=CARTESIAN_POINT('',(10.8999902203958,-24.,10.1913788112003));
#141643=CARTESIAN_POINT('Origin',(11.2999891909638,-24.,10.1904713176424));
#141644=CARTESIAN_POINT('',(10.4985290936118,-24.,11.899999999963));
#141645=CARTESIAN_POINT('Origin',(7.1,-24.,10.2));
#141646=CARTESIAN_POINT('Ctrl Pts',(11.0937451095552,-24.4,11.499999999963));
#141647=CARTESIAN_POINT('Ctrl Pts',(11.0924567483356,-24.4,11.5009355247485));
#141648=CARTESIAN_POINT('Ctrl Pts',(11.0911681658151,-24.3999967179757,
11.5018707575305));
#141649=CARTESIAN_POINT('Ctrl Pts',(11.0231542191183,-24.3996506319442,
11.5512102927633));
#141650=CARTESIAN_POINT('Ctrl Pts',(10.9549864097868,-24.3905292179535,
11.5994056955316));
#141651=CARTESIAN_POINT('Ctrl Pts',(10.8262909213129,-24.3560435733156,
11.6880601135325));
#141652=CARTESIAN_POINT('Ctrl Pts',(10.7632529694956,-24.3309943848462,
11.730357597492));
#141653=CARTESIAN_POINT('Ctrl Pts',(10.6545605129792,-24.2665454594411,
11.8016069437028));
#141654=CARTESIAN_POINT('Ctrl Pts',(10.6108433428765,-24.2311087701909,
11.8295581358754));
#141655=CARTESIAN_POINT('Ctrl Pts',(10.5541231913578,-24.1654279391003,
11.8654132910912));
#141656=CARTESIAN_POINT('Ctrl Pts',(10.5340339349874,-24.1354346237366,
11.8779647727759));
#141657=CARTESIAN_POINT('Ctrl Pts',(10.5089740421432,-24.0763110214604,
11.8935467247689));
#141658=CARTESIAN_POINT('Ctrl Pts',(10.5017642773951,-24.049084401109,11.8980004953156));
#141659=CARTESIAN_POINT('Ctrl Pts',(10.4988131157112,-24.0137087622167,
11.8998245213102));
#141660=CARTESIAN_POINT('Ctrl Pts',(10.4985290936118,-24.006841140788,11.899999999963));
#141661=CARTESIAN_POINT('Ctrl Pts',(10.4985290936118,-24.,11.899999999963));
#141662=CARTESIAN_POINT('Ctrl Pts',(10.8999902203958,-24.,10.1913788112003));
#141663=CARTESIAN_POINT('Ctrl Pts',(10.8993682056462,-24.,9.91721128970292));
#141664=CARTESIAN_POINT('Ctrl Pts',(11.1062409847674,-24.,9.73728944554553));
#141665=CARTESIAN_POINT('Ctrl Pts',(11.3131137638887,-24.,9.55736760138814));
#141666=CARTESIAN_POINT('Ctrl Pts',(11.5845457335763,-24.,9.59600569888118));
#141667=CARTESIAN_POINT('Ctrl Pts',(10.8999902203958,-24.4,10.1913788112003));
#141668=CARTESIAN_POINT('Ctrl Pts',(10.8993682056462,-24.4,9.91721128970292));
#141669=CARTESIAN_POINT('Ctrl Pts',(11.1062409847674,-24.4,9.73728944554553));
#141670=CARTESIAN_POINT('Ctrl Pts',(11.3131137638887,-24.4,9.55736760138814));
#141671=CARTESIAN_POINT('Ctrl Pts',(11.5845457335763,-24.4,9.59600569888118));
#141672=CARTESIAN_POINT('Ctrl Pts',(11.2999891909638,-24.4,10.1904713176424));
#141673=CARTESIAN_POINT('Ctrl Pts',(11.2997818527139,-24.4,10.09908214381));
#141674=CARTESIAN_POINT('Ctrl Pts',(11.3687394457543,-24.4,10.0391081957575));
#141675=CARTESIAN_POINT('Ctrl Pts',(11.4376970387948,-24.4,9.97913424770505));
#141676=CARTESIAN_POINT('Ctrl Pts',(11.5281743620239,-24.4,9.99201361353606));
#141677=CARTESIAN_POINT('',(11.5281743620239,-24.4,9.99201361353606));
#141678=CARTESIAN_POINT('',(11.5845457335763,-24.,9.59600569888119));
#141679=CARTESIAN_POINT('Origin',(11.5281743620239,-24.,9.99201361353606));
#141680=CARTESIAN_POINT('Origin',(11.4999886762478,-24.,10.1900175708635));
#141681=CARTESIAN_POINT('Origin',(11.4999886762478,-24.4,10.1900175708635));
#141682=CARTESIAN_POINT('Origin',(15.1,-24.,-15.1000000000002));
#141683=CARTESIAN_POINT('',(11.7266197306119,-24.4,10.0194623972745));
#141684=CARTESIAN_POINT('',(11.7798591918362,-24.,9.62302127961819));
#141685=CARTESIAN_POINT('Origin',(11.7266197306119,-24.,10.0194623972745));
#141686=CARTESIAN_POINT('Origin',(15.1,-24.,-15.1000000000002));
#141687=CARTESIAN_POINT('Origin',(15.1,-24.4,-15.1000000000002));
#141688=CARTESIAN_POINT('Ctrl Pts',(11.7798591918362,-24.,9.62302127961819));
#141689=CARTESIAN_POINT('Ctrl Pts',(12.2999999999997,-24.,9.69287280397854));
#141690=CARTESIAN_POINT('Ctrl Pts',(12.2999999999997,-24.,10.2176829561026));
#141691=CARTESIAN_POINT('Ctrl Pts',(11.7798591918362,-24.4,9.62302127961819));
#141692=CARTESIAN_POINT('Ctrl Pts',(12.2999999999997,-24.4,9.69287280397853));
#141693=CARTESIAN_POINT('Ctrl Pts',(12.2999999999997,-24.4,10.2176829561026));
#141694=CARTESIAN_POINT('Ctrl Pts',(11.7266197306119,-24.4,10.0194623972745));
#141695=CARTESIAN_POINT('Ctrl Pts',(11.8999999999997,-24.4,10.0427462387279));
#141696=CARTESIAN_POINT('Ctrl Pts',(11.8999999999997,-24.4,10.2176829561026));
#141697=CARTESIAN_POINT('',(11.8999999999997,-24.4,10.2176829561026));
#141698=CARTESIAN_POINT('',(12.2999999999997,-24.,10.2176829561026));
#141699=CARTESIAN_POINT('Origin',(11.8999999999997,-24.,10.2176829561026));
#141700=CARTESIAN_POINT('Origin',(11.6999999999997,-24.,10.2176829561026));
#141701=CARTESIAN_POINT('Origin',(11.6999999999997,-24.4,10.2176829561026));
#141702=CARTESIAN_POINT('Origin',(11.8999999999997,-24.,9.96444707415598));
#141703=CARTESIAN_POINT('',(12.2999999999997,-24.,11.899999999963));
#141704=CARTESIAN_POINT('',(12.2999999999997,-24.,9.96444707415599));
#141705=CARTESIAN_POINT('',(11.8999999999997,-24.4,11.499999999963));
#141706=CARTESIAN_POINT('',(11.8999999999997,-24.4,9.96444707415598));
#141707=CARTESIAN_POINT('Origin',(11.8999999999997,-24.,11.499999999963));
#141708=CARTESIAN_POINT('Origin',(8.47425608016909,-24.,11.499999999963));
#141709=CARTESIAN_POINT('',(8.47425608016909,-24.,11.899999999963));
#141710=CARTESIAN_POINT('',(8.47425608016909,-24.4,11.499999999963));
#141711=CARTESIAN_POINT('Origin',(12.2999999999997,-10.3,9.68731764791195));
#141712=CARTESIAN_POINT('',(12.2999999999997,-17.5694764848252,11.899999999963));
#141713=CARTESIAN_POINT('',(12.2999999999997,-16.55,11.899999999963));
#141714=CARTESIAN_POINT('',(12.2999999999997,-11.8066740905561,12.2));
#141715=CARTESIAN_POINT('Origin',(12.2999999999996,-14.8,14.199999999963));
#141716=CARTESIAN_POINT('',(12.2999999999997,-10.3,12.2));
#141717=CARTESIAN_POINT('',(12.2999999999997,-10.3,12.2));
#141718=CARTESIAN_POINT('',(12.2999999999997,-10.3,10.2176829561026));
#141719=CARTESIAN_POINT('',(12.2999999999997,-10.3,9.67578794473567));
#141720=CARTESIAN_POINT('',(12.2999999999997,-10.3,10.2176829561026));
#141721=CARTESIAN_POINT('Origin',(13.8999999999998,-22.8,11.899999999963));
#141722=CARTESIAN_POINT('',(10.4985290936118,-18.7372583002031,11.899999999963));
#141723=CARTESIAN_POINT('',(10.4985290936118,-24.4,11.899999999963));
#141724=CARTESIAN_POINT('',(9.32485954615698,-17.7372583002031,11.899999999963));
#141725=CARTESIAN_POINT('Ctrl Pts',(10.4985290936118,-18.7372583002031,
11.899999999963));
#141726=CARTESIAN_POINT('Ctrl Pts',(9.83672072559501,-18.1453701441239,
11.899999999963));
#141727=CARTESIAN_POINT('Ctrl Pts',(9.33545999193445,-17.7456813369822,
11.899999999963));
#141728=CARTESIAN_POINT('Ctrl Pts',(9.32485954615698,-17.7372583002031,
11.899999999963));
#141729=CARTESIAN_POINT('',(9.32485954615879,-17.0248595461262,11.8999999999606));
#141730=CARTESIAN_POINT('',(9.32485954615698,-24.4,11.899999999963));
#141731=CARTESIAN_POINT('',(11.8999999999998,-17.0248595461287,11.899999999963));
#141732=CARTESIAN_POINT('',(13.8999999999996,-17.0248595461287,11.899999999963));
#141733=CARTESIAN_POINT('Ctrl Pts',(11.8999999999998,-17.0248595461287,
11.899999999963));
#141734=CARTESIAN_POINT('Ctrl Pts',(11.9442850147497,-17.0248595461287,
11.899999999963));
#141735=CARTESIAN_POINT('Ctrl Pts',(11.9956860440864,-17.0383505886509,
11.899999999963));
#141736=CARTESIAN_POINT('Ctrl Pts',(12.0829656062854,-17.0830517207412,
11.899999999963));
#141737=CARTESIAN_POINT('Ctrl Pts',(12.13151199187,-17.1255662498947,11.899999999963));
#141738=CARTESIAN_POINT('Ctrl Pts',(12.2060204418464,-17.2176526173486,
11.899999999963));
#141739=CARTESIAN_POINT('Ctrl Pts',(12.2421146765233,-17.28636338603,11.899999999963));
#141740=CARTESIAN_POINT('Ctrl Pts',(12.2861083322068,-17.4146162004345,
11.899999999963));
#141741=CARTESIAN_POINT('Ctrl Pts',(12.2999999999998,-17.4985665379817,
11.899999999963));
#141742=CARTESIAN_POINT('Ctrl Pts',(12.2999999999998,-17.5694764848252,
11.899999999963));
#141743=CARTESIAN_POINT('Origin',(7.1,-24.4,10.2));
#141744=CARTESIAN_POINT('',(10.8999902203958,-18.7372583002031,10.1913788112003));
#141745=CARTESIAN_POINT('',(10.8999902203958,-10.3,10.1913788112003));
#141746=CARTESIAN_POINT('Origin',(7.1,-18.7372583002031,10.2));
#141747=CARTESIAN_POINT('Origin',(3.04851216033843,-24.4,10.2415765003998));
#141748=CARTESIAN_POINT('Origin',(5.65685424949238,-24.,-12.8999999999999));
#141749=CARTESIAN_POINT('',(9.28759150877464,-23.9860345618388,-12.1992436937665));
#141750=CARTESIAN_POINT('',(9.28736209575136,-24.,-12.1993418985011));
#141751=CARTESIAN_POINT('Ctrl Pts',(9.28759150880459,-23.98603456184,-12.1992436937537));
#141752=CARTESIAN_POINT('Ctrl Pts',(9.28743869432123,-23.9906846184834,
-12.1993091465896));
#141753=CARTESIAN_POINT('Ctrl Pts',(9.28736209575136,-23.9953405449403,
-12.1993418985011));
#141754=CARTESIAN_POINT('Ctrl Pts',(9.28736209575136,-24.,-12.1993418985011));
#141755=CARTESIAN_POINT('',(3.29032212515741,-23.9860345609289,-10.0587259632996));
#141756=CARTESIAN_POINT('Origin',(5.65685424949238,-23.9860345609261,-12.8999999999999));
#141757=CARTESIAN_POINT('',(3.29051067971883,-24.,-10.0588862911288));
#141758=CARTESIAN_POINT('Ctrl Pts',(3.29051067971883,-24.,-10.0588862911288));
#141759=CARTESIAN_POINT('Ctrl Pts',(3.29051067971883,-23.9953398535192,
-10.0588862911288));
#141760=CARTESIAN_POINT('Ctrl Pts',(3.29044771115612,-23.9906840233497,
-10.0588327519088));
#141761=CARTESIAN_POINT('Ctrl Pts',(3.29032212515734,-23.9860345609289,
-10.0587259632996));
#141762=CARTESIAN_POINT('',(3.3089883286316,-24.4,-9.54187032534883));
#141763=CARTESIAN_POINT('Ctrl Pts',(3.30898832863159,-24.4,-9.54187032534883));
#141764=CARTESIAN_POINT('Ctrl Pts',(3.3089127945394,-24.4,-9.54302222643878));
#141765=CARTESIAN_POINT('Ctrl Pts',(3.30883748342679,-24.399996957327,-9.54417414390669));
#141766=CARTESIAN_POINT('Ctrl Pts',(3.30550334651522,-24.399726789429,-9.59532351692953));
#141767=CARTESIAN_POINT('Ctrl Pts',(3.30266654088576,-24.3937324334157,
-9.6454638152666));
#141768=CARTESIAN_POINT('Ctrl Pts',(3.29802761162445,-24.3705240815341,
-9.74158961799118));
#141769=CARTESIAN_POINT('Ctrl Pts',(3.29619025535583,-24.3535039951622,
-9.78793108463616));
#141770=CARTESIAN_POINT('Ctrl Pts',(3.29317220178152,-24.3044744324752,
-9.88126024765772));
#141771=CARTESIAN_POINT('Ctrl Pts',(3.29213934109232,-24.2703518742144,
-9.92746145303948));
#141772=CARTESIAN_POINT('Ctrl Pts',(3.29102336292671,-24.1952991262786,
-9.99546731421881));
#141773=CARTESIAN_POINT('Ctrl Pts',(3.29078368451477,-24.1574693504857,
-10.0200507383762));
#141774=CARTESIAN_POINT('Ctrl Pts',(3.29054076369835,-24.0787815416442,
-10.0511334347581));
#141775=CARTESIAN_POINT('Ctrl Pts',(3.29051067971883,-24.0397880746094,
-10.0588862911288));
#141776=CARTESIAN_POINT('Ctrl Pts',(3.29051067971883,-24.,-10.0588862911288));
#141777=CARTESIAN_POINT('',(6.61977032797715,-24.4,-8.91724945296497));
#141778=CARTESIAN_POINT('Origin',(5.65685424949238,-24.4,-12.8999999999999));
#141779=CARTESIAN_POINT('',(7.20805405049754,-24.3984199843545,-9.1458714239949));
#141780=CARTESIAN_POINT('Ctrl Pts',(7.20805405049754,-24.3984199843545,
-9.1458714239949));
#141781=CARTESIAN_POINT('Ctrl Pts',(6.90636576576306,-24.397809874008,-9.02861943572731));
#141782=CARTESIAN_POINT('Ctrl Pts',(6.7786421819491,-24.39962955605,-8.97898757769515));
#141783=CARTESIAN_POINT('Ctrl Pts',(6.67099081608409,-24.399947062377,-8.93715374025662));
#141784=CARTESIAN_POINT('Ctrl Pts',(6.64964997085853,-24.3999890424235,
-8.92886064780516));
#141785=CARTESIAN_POINT('Ctrl Pts',(6.62551569595268,-24.3999993697358,
-8.91948209361555));
#141786=CARTESIAN_POINT('Ctrl Pts',(6.62264293759876,-24.4,-8.91836574382844));
#141787=CARTESIAN_POINT('Ctrl Pts',(6.61977032797715,-24.4,-8.91724945296497));
#141788=CARTESIAN_POINT('',(9.38783269785609,-24.3739393224439,-11.5863664642257));
#141789=CARTESIAN_POINT('Ctrl Pts',(9.38783269785609,-24.3739393224439,
-11.5863664642257));
#141790=CARTESIAN_POINT('Ctrl Pts',(9.26990225756709,-24.3877368249567,
-11.1420300359286));
#141791=CARTESIAN_POINT('Ctrl Pts',(9.068557708432,-24.3930188075499,-10.7236304265978));
#141792=CARTESIAN_POINT('Ctrl Pts',(8.58163711558267,-24.3980317489178,
-10.0688695190312));
#141793=CARTESIAN_POINT('Ctrl Pts',(8.32848943789226,-24.3986403983757,
-9.81649678623844));
#141794=CARTESIAN_POINT('Ctrl Pts',(7.78572548264438,-24.3991085362301,
-9.41576798370814));
#141795=CARTESIAN_POINT('Ctrl Pts',(7.50514199796396,-24.3990207913455,
-9.26133547842921));
#141796=CARTESIAN_POINT('Ctrl Pts',(7.20805405049754,-24.3984199843545,
-9.1458714239949));
#141797=CARTESIAN_POINT('Ctrl Pts',(9.28736209575136,-24.,-12.1993418985011));
#141798=CARTESIAN_POINT('Ctrl Pts',(9.28736209575136,-24.0226784817566,
-12.1993418985011));
#141799=CARTESIAN_POINT('Ctrl Pts',(9.2888110615892,-24.0451292520319,-12.1966331561604));
#141800=CARTESIAN_POINT('Ctrl Pts',(9.29445398178838,-24.0898867003991,
-12.1858228852564));
#141801=CARTESIAN_POINT('Ctrl Pts',(9.29870760508546,-24.1117158371081,
-12.1775929804491));
#141802=CARTESIAN_POINT('Ctrl Pts',(9.31367063881442,-24.1705623930577,
-12.1473840540648));
#141803=CARTESIAN_POINT('Ctrl Pts',(9.32706218188048,-24.2053291077597,
-12.1192924667623));
#141804=CARTESIAN_POINT('Ctrl Pts',(9.36003187846609,-24.2738464175524,
-12.0372926322239));
#141805=CARTESIAN_POINT('Ctrl Pts',(9.37926713369123,-24.3028996833776,
-11.9809172492032));
#141806=CARTESIAN_POINT('Ctrl Pts',(9.40700119469152,-24.3468831586282,
-11.847323417685));
#141807=CARTESIAN_POINT('Ctrl Pts',(9.41407362988669,-24.360132393681,-11.7709710919796));
#141808=CARTESIAN_POINT('Ctrl Pts',(9.40317973190691,-24.3708302579929,
-11.6559864908138));
#141809=CARTESIAN_POINT('Ctrl Pts',(9.39697144103178,-24.3728701173123,
-11.6207992747186));
#141810=CARTESIAN_POINT('Ctrl Pts',(9.38783269785609,-24.3739393224439,
-11.5863664642257));
#141811=CARTESIAN_POINT('Ctrl Pts',(9.28736209575136,-24.,-12.1993418985011));
#141812=CARTESIAN_POINT('Ctrl Pts',(9.72748477929187,-24.,-12.0110470586274));
#141813=CARTESIAN_POINT('Ctrl Pts',(9.64163093544796,-24.,-11.540099035182));
#141814=CARTESIAN_POINT('Ctrl Pts',(9.28736209575136,-24.2759603294941,
-12.1993418985011));
#141815=CARTESIAN_POINT('Ctrl Pts',(9.72748477929187,-24.2759603294941,
-12.0110470586274));
#141816=CARTESIAN_POINT('Ctrl Pts',(9.64163093544796,-24.2759603294941,
-11.540099035182));
#141817=CARTESIAN_POINT('Ctrl Pts',(9.18588826821947,-24.3739393224439,
-11.9621557211613));
#141818=CARTESIAN_POINT('Ctrl Pts',(9.4367721008869,-24.3739393224439,-11.8548217143816));
#141819=CARTESIAN_POINT('Ctrl Pts',(9.38783269785609,-24.3739393224439,
-11.5863664642257));
#141820=CARTESIAN_POINT('',(9.64163093544796,-24.,-11.540099035182));
#141821=CARTESIAN_POINT('Origin',(9.24811638706485,-24.,-11.6118367533701));
#141822=CARTESIAN_POINT('Origin',(9.0513591128733,-24.,-11.6477056124642));
#141823=CARTESIAN_POINT('Origin',(6.1,-24.,-12.1857384988752));
#141824=CARTESIAN_POINT('',(7.33287671232877,-24.,-8.80342937459372));
#141825=CARTESIAN_POINT('Origin',(7.1958904109589,-24.,-9.17924149951388));
#141826=CARTESIAN_POINT('Origin',(6.1,-24.,-12.1857384988752));
#141827=CARTESIAN_POINT('Origin',(8.6,-24.,-5.32716721908225));
#141828=CARTESIAN_POINT('',(4.5,-24.4,-5.32716721908225));
#141829=CARTESIAN_POINT('Origin',(8.6,-24.4,-5.32716721908225));
#141830=CARTESIAN_POINT('',(4.9,-24.,-5.32716721908225));
#141831=CARTESIAN_POINT('Origin',(4.5,-24.,-5.32716721908225));
#141832=CARTESIAN_POINT('Origin',(8.6,-24.,-5.32716721908225));
#141833=CARTESIAN_POINT('Origin',(-3.45175358661618,-24.4,-3.05000000003699));
#141834=CARTESIAN_POINT('',(1.01279069686664,-24.4,-6.14651140747171));
#141835=CARTESIAN_POINT('Origin',(9.25,-24.4,-3.05000000003699));
#141836=CARTESIAN_POINT('',(0.999999999210583,-24.4,-6.07613614821183));
#141837=CARTESIAN_POINT('Origin',(1.19999999921058,-24.4,-6.07613614821183));
#141838=CARTESIAN_POINT('',(0.999999999210583,-24.4,-4.25000000003699));
#141839=CARTESIAN_POINT('',(0.999999999210583,-24.4,-4.75788611936281));
#141840=CARTESIAN_POINT('',(1.19999999921058,-24.4,-4.05000000003699));
#141841=CARTESIAN_POINT('Origin',(1.19999999921058,-24.4,-4.25000000003699));
#141842=CARTESIAN_POINT('',(4.3,-24.4,-4.05000000003699));
#141843=CARTESIAN_POINT('',(-1.71792900372085,-24.4,-4.05000000003699));
#141844=CARTESIAN_POINT('',(4.5,-24.4,-4.25000000003699));
#141845=CARTESIAN_POINT('Origin',(4.3,-24.4,-4.25000000003699));
#141846=CARTESIAN_POINT('',(4.5,-24.4,-4.18858360955962));
#141847=CARTESIAN_POINT('Origin',(4.5,-24.,-4.18858360955962));
#141848=CARTESIAN_POINT('',(4.9,-24.,-4.25000000003699));
#141849=CARTESIAN_POINT('Origin',(4.5,-24.,-4.25000000003699));
#141850=CARTESIAN_POINT('',(4.9,-24.,-4.18858360955962));
#141851=CARTESIAN_POINT('Ctrl Pts',(4.9,-24.,-4.25000000003699));
#141852=CARTESIAN_POINT('Ctrl Pts',(4.9,-24.,-3.65000000003699));
#141853=CARTESIAN_POINT('Ctrl Pts',(4.3,-24.,-3.65000000003699));
#141854=CARTESIAN_POINT('Ctrl Pts',(4.9,-24.4,-4.25000000003699));
#141855=CARTESIAN_POINT('Ctrl Pts',(4.9,-24.4,-3.65000000003699));
#141856=CARTESIAN_POINT('Ctrl Pts',(4.3,-24.4,-3.65000000003699));
#141857=CARTESIAN_POINT('Ctrl Pts',(4.5,-24.4,-4.25000000003699));
#141858=CARTESIAN_POINT('Ctrl Pts',(4.5,-24.4,-4.05000000003699));
#141859=CARTESIAN_POINT('Ctrl Pts',(4.3,-24.4,-4.05000000003699));
#141860=CARTESIAN_POINT('',(4.3,-24.,-3.65000000003699));
#141861=CARTESIAN_POINT('Origin',(4.3,-24.,-4.05000000003699));
#141862=CARTESIAN_POINT('Origin',(4.3,-24.,-4.25000000003699));
#141863=CARTESIAN_POINT('Origin',(-1.71792900372085,-24.,-4.05000000003699));
#141864=CARTESIAN_POINT('',(1.19999999921058,-24.,-3.65000000003699));
#141865=CARTESIAN_POINT('Origin',(1.19999999921058,-24.,-4.05000000003699));
#141866=CARTESIAN_POINT('',(-1.71792900372085,-24.,-3.65000000003699));
#141867=CARTESIAN_POINT('Ctrl Pts',(1.19999999921058,-24.,-3.65000000003699));
#141868=CARTESIAN_POINT('Ctrl Pts',(0.599999999210583,-24.,-3.65000000003699));
#141869=CARTESIAN_POINT('Ctrl Pts',(0.599999999210583,-24.,-4.25000000003699));
#141870=CARTESIAN_POINT('Ctrl Pts',(1.19999999921058,-24.4,-3.65000000003699));
#141871=CARTESIAN_POINT('Ctrl Pts',(0.599999999210583,-24.4,-3.65000000003699));
#141872=CARTESIAN_POINT('Ctrl Pts',(0.599999999210583,-24.4,-4.25000000003699));
#141873=CARTESIAN_POINT('Ctrl Pts',(1.19999999921058,-24.4,-4.05000000003699));
#141874=CARTESIAN_POINT('Ctrl Pts',(0.999999999210583,-24.4,-4.05000000003699));
#141875=CARTESIAN_POINT('Ctrl Pts',(0.999999999210583,-24.4,-4.25000000003699));
#141876=CARTESIAN_POINT('',(0.599999999210583,-24.,-4.25000000003699));
#141877=CARTESIAN_POINT('Origin',(0.999999999210583,-24.,-4.25000000003699));
#141878=CARTESIAN_POINT('Origin',(1.19999999921058,-24.,-4.25000000003699));
#141879=CARTESIAN_POINT('Origin',(0.999999999210583,-24.,-4.75788611936281));
#141880=CARTESIAN_POINT('',(0.599999999210583,-24.,-6.07613614821183));
#141881=CARTESIAN_POINT('Origin',(0.999999999210583,-24.,-6.07613614821183));
#141882=CARTESIAN_POINT('',(0.599999999210583,-24.,-4.75788611936281));
#141883=CARTESIAN_POINT('Ctrl Pts',(0.599999999210582,-24.,-6.07613614821183));
#141884=CARTESIAN_POINT('Ctrl Pts',(0.599999999210582,-24.,-6.18518609949224));
#141885=CARTESIAN_POINT('Ctrl Pts',(0.638372092178763,-24.,-6.28726192599147));
#141886=CARTESIAN_POINT('Ctrl Pts',(0.599999999210582,-24.4,-6.07613614821183));
#141887=CARTESIAN_POINT('Ctrl Pts',(0.599999999210582,-24.4,-6.18518609949224));
#141888=CARTESIAN_POINT('Ctrl Pts',(0.638372092178763,-24.4,-6.28726192599147));
#141889=CARTESIAN_POINT('Ctrl Pts',(0.999999999210582,-24.4,-6.07613614821183));
#141890=CARTESIAN_POINT('Ctrl Pts',(0.999999999210582,-24.4,-6.11248613197196));
#141891=CARTESIAN_POINT('Ctrl Pts',(1.01279069686664,-24.4,-6.14651140747171));
#141892=CARTESIAN_POINT('',(0.638372092178764,-24.,-6.28726192599147));
#141893=CARTESIAN_POINT('Origin',(1.01279069686664,-24.,-6.14651140747171));
#141894=CARTESIAN_POINT('Origin',(1.19999999921058,-24.,-6.07613614821183));
#141895=CARTESIAN_POINT('Origin',(9.25,-24.,-3.05000000003699));
#141896=CARTESIAN_POINT('Origin',(9.25,-24.,-3.05000000003699));
#141897=CARTESIAN_POINT('Origin',(9.0513591128733,-19.9,-11.6477056124642));
#141898=CARTESIAN_POINT('',(9.64163093544796,-20.,-11.540099035182));
#141899=CARTESIAN_POINT('',(9.64163093544796,-19.9,-11.540099035182));
#141900=CARTESIAN_POINT('',(9.03750044632957,-20.,-12.2475455389126));
#141901=CARTESIAN_POINT('Origin',(9.0513591128733,-20.,-11.6477056124642));
#141902=CARTESIAN_POINT('',(9.03750044632957,-22.5020352696956,-12.2475455389126));
#141903=CARTESIAN_POINT('',(9.03750044632957,-19.9,-12.2475455389126));
#141904=CARTESIAN_POINT('Ctrl Pts',(9.03750044632957,-22.5020352696956,
-12.2475455389126));
#141905=CARTESIAN_POINT('Ctrl Pts',(9.09123412340781,-22.6355177185059,
-12.248786998642));
#141906=CARTESIAN_POINT('Ctrl Pts',(9.13679223934425,-22.7752399470139,
-12.2427744067466));
#141907=CARTESIAN_POINT('Ctrl Pts',(9.24836945479761,-23.2096289940093,
-12.2195751234883));
#141908=CARTESIAN_POINT('Ctrl Pts',(9.28517493986822,-23.5143240465938,
-12.2002907823841));
#141909=CARTESIAN_POINT('Ctrl Pts',(9.28930197413971,-23.8000000000006,
-12.1985079316063));
#141910=CARTESIAN_POINT('Ctrl Pts',(9.2901945404804,-23.8617840133094,-12.1981223490087));
#141911=CARTESIAN_POINT('Ctrl Pts',(9.28963512742458,-23.9238484297288,
-12.1983683799008));
#141912=CARTESIAN_POINT('Ctrl Pts',(9.28759150880459,-23.98603456184,-12.1992436937537));
#141913=CARTESIAN_POINT('Origin',(6.1,-19.9,-12.1857384988752));
#141914=CARTESIAN_POINT('',(7.33287671232877,-20.,-8.80342937459372));
#141915=CARTESIAN_POINT('',(7.33287671232877,-19.9,-8.80342937459372));
#141916=CARTESIAN_POINT('Origin',(6.1,-20.,-12.1857384988752));
#141917=CARTESIAN_POINT('Origin',(8.6,-19.9,-5.32716721908225));
#141918=CARTESIAN_POINT('',(4.9,-20.,-5.32716721908225));
#141919=CARTESIAN_POINT('',(4.9,-19.9,-5.32716721908225));
#141920=CARTESIAN_POINT('Origin',(8.6,-20.,-5.32716721908225));
#141921=CARTESIAN_POINT('Origin',(4.9,-19.9,-5.32716721908225));
#141922=CARTESIAN_POINT('',(4.9,-20.,-4.25000000003699));
#141923=CARTESIAN_POINT('',(4.9,-19.9,-4.25000000003699));
#141924=CARTESIAN_POINT('',(4.9,-20.,-2.88858360955241));
#141925=CARTESIAN_POINT('Origin',(4.3,-19.9,-4.25000000003699));
#141926=CARTESIAN_POINT('',(4.3,-20.,-3.65000000003699));
#141927=CARTESIAN_POINT('',(4.3,-19.9,-3.65000000003699));
#141928=CARTESIAN_POINT('Origin',(4.3,-20.,-4.25000000003699));
#141929=CARTESIAN_POINT('Origin',(0.0158955791744741,-19.9,-3.65000000003699));
#141930=CARTESIAN_POINT('',(1.19999999921058,-20.,-3.65000000003699));
#141931=CARTESIAN_POINT('',(1.19999999921058,-19.9,-3.65000000003699));
#141932=CARTESIAN_POINT('',(-1.31220842229031,-20.,-3.65000000003699));
#141933=CARTESIAN_POINT('Origin',(1.19999999921058,-19.9,-4.25000000003699));
#141934=CARTESIAN_POINT('',(0.599999999210583,-20.,-4.25000000003699));
#141935=CARTESIAN_POINT('',(0.599999999210583,-19.9,-4.25000000003699));
#141936=CARTESIAN_POINT('Origin',(1.19999999921058,-20.,-4.25000000003699));
#141937=CARTESIAN_POINT('Origin',(0.599999999210582,-19.9,-6.46577223868862));
#141938=CARTESIAN_POINT('',(0.599999999210583,-20.,-6.07613614821183));
#141939=CARTESIAN_POINT('',(0.599999999210583,-21.1,-6.07613614821183));
#141940=CARTESIAN_POINT('',(0.599999999210583,-20.,-3.4578861193556));
#141941=CARTESIAN_POINT('Origin',(1.19999999921058,-21.1,-6.07613614821183));
#141942=CARTESIAN_POINT('',(0.638372092178764,-20.,-6.28726192599147));
#141943=CARTESIAN_POINT('',(0.638372092178764,-21.1,-6.28726192599147));
#141944=CARTESIAN_POINT('Origin',(1.19999999921058,-20.,-6.07613614821183));
#141945=CARTESIAN_POINT('Origin',(9.25,-21.1,-3.05000000003699));
#141946=CARTESIAN_POINT('Ctrl Pts',(9.03750044632957,-22.5020352696956,
-12.2475455389126));
#141947=CARTESIAN_POINT('Ctrl Pts',(8.98537162787598,-22.3725395284934,
-12.2463411577428));
#141948=CARTESIAN_POINT('Ctrl Pts',(8.92564846760114,-22.2460178877848,
-12.2445240024109));
#141949=CARTESIAN_POINT('Ctrl Pts',(8.71336297104777,-21.8572772044711,
-12.2354893007256));
#141950=CARTESIAN_POINT('Ctrl Pts',(8.53368079632539,-21.610148441077,-12.2244104567008));
#141951=CARTESIAN_POINT('Ctrl Pts',(8.12142382370261,-21.1750909413994,
-12.1828657208104));
#141952=CARTESIAN_POINT('Ctrl Pts',(7.88887334972075,-20.9871548429568,
-12.1522357203516));
#141953=CARTESIAN_POINT('Ctrl Pts',(7.41647976391155,-20.6988748539929,
-12.0683269172958));
#141954=CARTESIAN_POINT('Ctrl Pts',(7.15662707779066,-20.5802100071682,
-12.0129405712226));
#141955=CARTESIAN_POINT('Ctrl Pts',(6.62192580066298,-20.4243112646203,
-11.8709829857734));
#141956=CARTESIAN_POINT('Ctrl Pts',(6.34714997371524,-20.3871246330873,
-11.784085965654));
#141957=CARTESIAN_POINT('Ctrl Pts',(5.84722372089706,-20.3871246330873,
-11.6017196823151));
#141958=CARTESIAN_POINT('Ctrl Pts',(5.58103575919986,-20.4243112646203,
-11.4912804853426));
#141959=CARTESIAN_POINT('Ctrl Pts',(5.08052131739254,-20.5802100071682,
-11.2556054858818));
#141960=CARTESIAN_POINT('Ctrl Pts',(4.84604074311545,-20.6988748539929,
-11.130665796022));
#141961=CARTESIAN_POINT('Ctrl Pts',(4.43057607697443,-20.9871548429568,
-10.8906960097316));
#141962=CARTESIAN_POINT('Ctrl Pts',(4.23292528343976,-21.1750909413994,
-10.7643944511806));
#141963=CARTESIAN_POINT('Ctrl Pts',(3.89075001978357,-21.610148441077,-10.5307325897267));
#141964=CARTESIAN_POINT('Ctrl Pts',(3.74613849230621,-21.8572772044711,
-10.423513511114));
#141965=CARTESIAN_POINT('Ctrl Pts',(3.40776601711932,-22.6391281658009,
-10.1625026467189));
#141966=CARTESIAN_POINT('Ctrl Pts',(3.29568612325364,-23.2300913446515,
-10.0632891899245));
#141967=CARTESIAN_POINT('Ctrl Pts',(3.2889159286883,-23.8,-10.0575299995985));
#141968=CARTESIAN_POINT('Ctrl Pts',(3.28817872204094,-23.8620573670452,
-10.0569028812268));
#141969=CARTESIAN_POINT('Ctrl Pts',(3.2886489655866,-23.9240906131805,-10.057303237953));
#141970=CARTESIAN_POINT('Ctrl Pts',(3.29032212515734,-23.9860345609289,
-10.0587259632996));
#141971=CARTESIAN_POINT('',(9.25,-20.,-12.250000000037));
#141972=CARTESIAN_POINT('Origin',(9.25,-20.,-3.05000000003699));
#141973=CARTESIAN_POINT('',(9.25,-15.9,-12.250000000037));
#141974=CARTESIAN_POINT('',(9.25,-21.1,-12.250000000037));
#141975=CARTESIAN_POINT('',(0.194290142826891,-15.9,-4.67299691398904));
#141976=CARTESIAN_POINT('Origin',(9.25,-15.9,-3.05000000003699));
#141977=CARTESIAN_POINT('',(0.194290142826895,-16.4303892440217,-4.67299691398904));
#141978=CARTESIAN_POINT('',(0.194290142826893,-21.1,-4.67299691398904));
#141979=CARTESIAN_POINT('',(0.47847834656078,-17.2370030965064,-5.82496087962556));
#141980=CARTESIAN_POINT('Origin',(9.25,-15.2939545703814,-3.05000000003699));
#141981=CARTESIAN_POINT('',(0.644705633055379,-17.4355690700213,-6.30406036490954));
#141982=CARTESIAN_POINT('Ctrl Pts',(0.644705633059486,-17.4355690700257,
-6.3040603649199));
#141983=CARTESIAN_POINT('Ctrl Pts',(0.603246655335933,-17.4006034041543,
-6.19442296811137));
#141984=CARTESIAN_POINT('Ctrl Pts',(0.565483129929027,-17.368112123324,
-6.08802112521124));
#141985=CARTESIAN_POINT('Ctrl Pts',(0.513579180401821,-17.3023542725618,
-5.93419691137546));
#141986=CARTESIAN_POINT('Ctrl Pts',(0.494843565862922,-17.2732246177677,
-5.87669057301615));
#141987=CARTESIAN_POINT('Ctrl Pts',(0.478478346560781,-17.2370030965064,
-5.82496087962556));
#141988=CARTESIAN_POINT('',(0.227169467729596,-19.1738552422879,-4.84681083758479));
#141989=CARTESIAN_POINT('Ctrl Pts',(0.227169467729604,-19.1738552422878,
-4.84681083758478));
#141990=CARTESIAN_POINT('Ctrl Pts',(0.288341103269117,-19.1595858444531,
-5.15398913889562));
#141991=CARTESIAN_POINT('Ctrl Pts',(0.364344206904044,-19.1359275310739,
-5.45154142969646));
#141992=CARTESIAN_POINT('Ctrl Pts',(0.531373163443829,-19.0522811885239,
-6.00095643599083));
#141993=CARTESIAN_POINT('Ctrl Pts',(0.64706147259344,-18.9778030839297,
-6.32116532630702));
#141994=CARTESIAN_POINT('Ctrl Pts',(0.792548014213962,-18.813342562401,
-6.67277297469914));
#141995=CARTESIAN_POINT('Ctrl Pts',(0.845006682143811,-18.7418056498301,
-6.79239746305243));
#141996=CARTESIAN_POINT('Ctrl Pts',(0.914713320592898,-18.6089688816776,
-6.94460170106634));
#141997=CARTESIAN_POINT('Ctrl Pts',(0.944350360166487,-18.5391485007925,
-7.00709614019699));
#141998=CARTESIAN_POINT('Ctrl Pts',(0.976481807510859,-18.4195181965843,
-7.07361815041777));
#141999=CARTESIAN_POINT('Ctrl Pts',(0.985172457114319,-18.3771538424934,
-7.09138547440372));
#142000=CARTESIAN_POINT('Ctrl Pts',(0.996932135198067,-18.2897944712841,
-7.11534824541121));
#142001=CARTESIAN_POINT('Ctrl Pts',(1.,-18.2448003741776,-7.12154761734421));
#142002=CARTESIAN_POINT('Ctrl Pts',(1.,-18.1551996258224,-7.12154761734421));
#142003=CARTESIAN_POINT('Ctrl Pts',(0.996932135198067,-18.1102055287159,
-7.11534824541121));
#142004=CARTESIAN_POINT('Ctrl Pts',(0.98517245711432,-18.0228461575066,
-7.09138547440372));
#142005=CARTESIAN_POINT('Ctrl Pts',(0.97648180751086,-17.9804818034157,
-7.07361815041777));
#142006=CARTESIAN_POINT('Ctrl Pts',(0.944350360166488,-17.8608514992075,
-7.00709614019699));
#142007=CARTESIAN_POINT('Ctrl Pts',(0.914713320592898,-17.7910311183224,
-6.94460170106634));
#142008=CARTESIAN_POINT('Ctrl Pts',(0.845006682143811,-17.6581943501699,
-6.79239746305243));
#142009=CARTESIAN_POINT('Ctrl Pts',(0.792548014213962,-17.586657437599,
-6.67277297469914));
#142010=CARTESIAN_POINT('Ctrl Pts',(0.715345229333762,-17.4993860644298,
-6.48619152641746));
#142011=CARTESIAN_POINT('Ctrl Pts',(0.679882242726209,-17.4652363133496,
-6.39708417120235));
#142012=CARTESIAN_POINT('Ctrl Pts',(0.644705633055442,-17.4355690700223,
-6.30406036490921));
#142013=CARTESIAN_POINT('',(0.194290142826893,-19.2201728349062,-4.67299691398903));
#142014=CARTESIAN_POINT('Ctrl Pts',(0.194292330138919,-19.2200994892544,
-4.67313792326464));
#142015=CARTESIAN_POINT('Ctrl Pts',(0.196951382332334,-19.2121899859122,
-4.68795556951401));
#142016=CARTESIAN_POINT('Ctrl Pts',(0.19974428037187,-19.2053433257718,
-4.70328228986047));
#142017=CARTESIAN_POINT('Ctrl Pts',(0.202641290095105,-19.1995065588509,
-4.71897015143785));
#142018=CARTESIAN_POINT('Ctrl Pts',(0.204743381693374,-19.195271357772,
-4.73035337937532));
#142019=CARTESIAN_POINT('Ctrl Pts',(0.20690081470169,-19.1915680174414,
-4.74192775747502));
#142020=CARTESIAN_POINT('Ctrl Pts',(0.209112002429709,-19.1883798624547,
-4.75365040315691));
#142021=CARTESIAN_POINT('Ctrl Pts',(0.212120691938237,-19.1840418461306,
-4.76960101676983));
#142022=CARTESIAN_POINT('Ctrl Pts',(0.215230415767539,-19.1806621755999,
-4.78580553951459));
#142023=CARTESIAN_POINT('Ctrl Pts',(0.21839854029795,-19.1782166203877,
-4.80213822120128));
#142024=CARTESIAN_POINT('Ctrl Pts',(0.221271933531467,-19.1759985756955,
-4.81695147004717));
#142025=CARTESIAN_POINT('Ctrl Pts',(0.224194281023603,-19.1745492587607,
-4.83187069759389));
#142026=CARTESIAN_POINT('Ctrl Pts',(0.227169467729732,-19.1738552422878,
-4.84681083758542));
#142027=CARTESIAN_POINT('',(0.194290142826891,-20.,-4.67299691398904));
#142028=CARTESIAN_POINT('',(0.194290142826893,-21.1,-4.67299691398904));
#142029=CARTESIAN_POINT('Origin',(9.25,-20.,-3.05000000003699));
#142030=CARTESIAN_POINT('Origin',(5.65685424949238,-23.8568542494924,-12.8999999999999));
#142031=CARTESIAN_POINT('Origin',(15.1,-24.,-15.1));
#142032=CARTESIAN_POINT('',(11.6304347826087,-24.,-12.7331207884076));
#142033=CARTESIAN_POINT('',(11.3,-24.4,-12.5077037206369));
#142034=CARTESIAN_POINT('Origin',(11.3,-24.,-12.5077037206369));
#142035=CARTESIAN_POINT('',(15.1517070744679,-24.4,-10.5002906202185));
#142036=CARTESIAN_POINT('Origin',(15.1,-24.4,-15.1));
#142037=CARTESIAN_POINT('',(15.1472108071229,-24.,-10.9002653488952));
#142038=CARTESIAN_POINT('Origin',(15.1517070744679,-24.,-10.5002906202185));
#142039=CARTESIAN_POINT('Origin',(15.1,-24.,-15.1));
#142040=CARTESIAN_POINT('Ctrl Pts',(15.1472108071229,-24.,-10.9002653488952));
#142041=CARTESIAN_POINT('Ctrl Pts',(15.6849777763716,-24.,-10.906310590981));
#142042=CARTESIAN_POINT('Ctrl Pts',(15.8935746197026,-24.,-10.4106118769225));
#142043=CARTESIAN_POINT('Ctrl Pts',(16.1021714630336,-24.,-9.91491316286401));
#142044=CARTESIAN_POINT('Ctrl Pts',(15.7218887667622,-24.,-9.53463046659261));
#142045=CARTESIAN_POINT('Ctrl Pts',(15.1472108071229,-24.4,-10.9002653488952));
#142046=CARTESIAN_POINT('Ctrl Pts',(15.6849777763716,-24.4,-10.906310590981));
#142047=CARTESIAN_POINT('Ctrl Pts',(15.8935746197026,-24.4,-10.4106118769225));
#142048=CARTESIAN_POINT('Ctrl Pts',(16.1021714630336,-24.4,-9.91491316286401));
#142049=CARTESIAN_POINT('Ctrl Pts',(15.7218887667622,-24.4,-9.53463046659261));
#142050=CARTESIAN_POINT('Ctrl Pts',(15.1517070744679,-24.4,-10.5002906202185));
#142051=CARTESIAN_POINT('Ctrl Pts',(15.4205905590923,-24.4,-10.5033132412614));
#142052=CARTESIAN_POINT('Ctrl Pts',(15.5248889807578,-24.4,-10.2554638842322));
#142053=CARTESIAN_POINT('Ctrl Pts',(15.6291874024233,-24.4,-10.0076145272029));
#142054=CARTESIAN_POINT('Ctrl Pts',(15.4390460542876,-24.4,-9.81747317906723));
#142055=CARTESIAN_POINT('',(15.4390460542876,-24.4,-9.81747317906723));
#142056=CARTESIAN_POINT('',(15.7218887667622,-24.,-9.53463046659261));
#142057=CARTESIAN_POINT('Origin',(15.4390460542876,-24.,-9.81747317906723));
#142058=CARTESIAN_POINT('Origin',(15.1562033418129,-24.,-10.1003158915419));
#142059=CARTESIAN_POINT('Origin',(15.1562033418129,-24.4,-10.1003158915419));
#142060=CARTESIAN_POINT('Origin',(10.1478480409737,-24.,-4.5262751657534));
#142061=CARTESIAN_POINT('',(14.8514718625661,-24.4,-9.22989898734577));
#142062=CARTESIAN_POINT('',(15.1343145750407,-24.,-8.94705627487115));
#142063=CARTESIAN_POINT('Origin',(14.8514718625661,-24.,-9.22989898734577));
#142064=CARTESIAN_POINT('',(10.4306907534484,-24.,-4.24343245327878));
#142065=CARTESIAN_POINT('',(10.1478480409737,-24.4,-4.5262751657534));
#142066=CARTESIAN_POINT('Origin',(15.69999999999,-24.,-8.38137084992192));
#142067=CARTESIAN_POINT('',(14.49999999999,-24.4,-8.38137084991966));
#142068=CARTESIAN_POINT('',(14.89999999999,-24.,-8.38137084992041));
#142069=CARTESIAN_POINT('Origin',(14.49999999999,-24.,-8.38137084991966));
#142070=CARTESIAN_POINT('Origin',(15.69999999999,-24.,-8.38137084992192));
#142071=CARTESIAN_POINT('Origin',(15.69999999999,-24.4,-8.38137084992192));
#142072=CARTESIAN_POINT('Origin',(14.4999999999975,-24.,-4.37858365125987));
#142073=CARTESIAN_POINT('',(14.4999999999902,-24.4,-8.27794038524243));
#142074=CARTESIAN_POINT('',(14.8999999999902,-24.,-8.27794038524318));
#142075=CARTESIAN_POINT('Origin',(14.4999999999902,-24.,-8.27794038524243));
#142076=CARTESIAN_POINT('',(14.8999999999975,-24.,-4.37858365126063));
#142077=CARTESIAN_POINT('',(14.4999999999975,-24.4,-4.37858365125987));
#142078=CARTESIAN_POINT('Ctrl Pts',(14.8999999999902,-24.,-8.27794038524318));
#142079=CARTESIAN_POINT('Ctrl Pts',(14.8999999999908,-24.,-7.91192841075916));
#142080=CARTESIAN_POINT('Ctrl Pts',(14.6230576451076,-24.,-7.67262170893618));
#142081=CARTESIAN_POINT('Ctrl Pts',(14.3461152902243,-24.,-7.4333150071132));
#142082=CARTESIAN_POINT('Ctrl Pts',(13.9839732502781,-24.,-7.48639898180705));
#142083=CARTESIAN_POINT('Ctrl Pts',(14.8999999999902,-24.4,-8.27794038524318));
#142084=CARTESIAN_POINT('Ctrl Pts',(14.8999999999908,-24.4,-7.91192841075916));
#142085=CARTESIAN_POINT('Ctrl Pts',(14.6230576451076,-24.4,-7.67262170893618));
#142086=CARTESIAN_POINT('Ctrl Pts',(14.3461152902243,-24.4,-7.4333150071132));
#142087=CARTESIAN_POINT('Ctrl Pts',(13.9839732502781,-24.4,-7.48639898180705));
#142088=CARTESIAN_POINT('Ctrl Pts',(14.4999999999902,-24.4,-8.27794038524243));
#142089=CARTESIAN_POINT('Ctrl Pts',(14.4999999999905,-24.4,-8.09493439800042));
#142090=CARTESIAN_POINT('Ctrl Pts',(14.3615288225489,-24.4,-7.97528104708893));
#142091=CARTESIAN_POINT('Ctrl Pts',(14.2230576451072,-24.4,-7.85562769617744));
#142092=CARTESIAN_POINT('Ctrl Pts',(14.0419866251341,-24.4,-7.88216968352437));
#142093=CARTESIAN_POINT('',(14.0419866251341,-24.4,-7.88216968352437));
#142094=CARTESIAN_POINT('',(13.9839732502781,-24.,-7.48639898180705));
#142095=CARTESIAN_POINT('Origin',(14.0419866251341,-24.,-7.88216968352437));
#142096=CARTESIAN_POINT('Origin',(14.0999999999902,-24.,-8.27794038524168));
#142097=CARTESIAN_POINT('Origin',(14.0999999999902,-24.4,-8.27794038524168));
#142098=CARTESIAN_POINT('Origin',(9.25,-24.,-3.05000000003699));
#142099=CARTESIAN_POINT('',(11.7393688126037,-24.,-8.17767422085447));
#142100=CARTESIAN_POINT('',(11.9140613608566,-24.4,-8.53751100828026));
#142101=CARTESIAN_POINT('Origin',(11.9140613608566,-24.,-8.53751100828026));
#142102=CARTESIAN_POINT('',(10.5587573250099,-24.4,-9.00794883031683));
#142103=CARTESIAN_POINT('Origin',(9.25,-24.4,-3.05000000003699));
#142104=CARTESIAN_POINT('',(10.4729371725502,-24.,-8.61726366111815));
#142105=CARTESIAN_POINT('Origin',(10.5587573250099,-24.,-9.00794883031683));
#142106=CARTESIAN_POINT('Origin',(9.25,-24.,-3.05000000003699));
#142107=CARTESIAN_POINT('Ctrl Pts',(10.4729371725502,-24.,-8.61726366111815));
#142108=CARTESIAN_POINT('Ctrl Pts',(10.1641684413763,-24.,-8.68508957741407));
#142109=CARTESIAN_POINT('Ctrl Pts',(10.0455250613722,-24.,-8.97811215786373));
#142110=CARTESIAN_POINT('Ctrl Pts',(9.92688168136818,-24.,-9.27113473831338));
#142111=CARTESIAN_POINT('Ctrl Pts',(10.1014821344353,-24.,-9.53467442424495));
#142112=CARTESIAN_POINT('Ctrl Pts',(10.4729371725502,-24.4,-8.61726366111815));
#142113=CARTESIAN_POINT('Ctrl Pts',(10.1641684413763,-24.4,-8.68508957741407));
#142114=CARTESIAN_POINT('Ctrl Pts',(10.0455250613722,-24.4,-8.97811215786373));
#142115=CARTESIAN_POINT('Ctrl Pts',(9.92688168136818,-24.4,-9.27113473831338));
#142116=CARTESIAN_POINT('Ctrl Pts',(10.1014821344353,-24.4,-9.53467442424495));
#142117=CARTESIAN_POINT('Ctrl Pts',(10.5587573250099,-24.4,-9.00794883031683));
#142118=CARTESIAN_POINT('Ctrl Pts',(10.4558344146186,-24.4,-9.03055746908214));
#142119=CARTESIAN_POINT('Ctrl Pts',(10.4162866212839,-24.4,-9.12823166256536));
#142120=CARTESIAN_POINT('Ctrl Pts',(10.3767388279492,-24.4,-9.22590585604857));
#142121=CARTESIAN_POINT('Ctrl Pts',(10.4349389789716,-24.4,-9.31375241802576));
#142122=CARTESIAN_POINT('',(10.4349389789716,-24.4,-9.31375241802576));
#142123=CARTESIAN_POINT('',(10.1014821344353,-24.,-9.53467442424495));
#142124=CARTESIAN_POINT('Origin',(10.4349389789716,-24.,-9.31375241802576));
#142125=CARTESIAN_POINT('Origin',(10.6016674012397,-24.,-9.20329141491617));
#142126=CARTESIAN_POINT('Origin',(10.6016674012397,-24.4,-9.20329141491617));
#142127=CARTESIAN_POINT('Origin',(6.1,-24.,-12.1857384988752));
#142128=CARTESIAN_POINT('',(11.3,-24.4,-12.1857384988752));
#142129=CARTESIAN_POINT('',(10.9,-24.,-12.1857384988752));
#142130=CARTESIAN_POINT('Origin',(11.3,-24.,-12.1857384988752));
#142131=CARTESIAN_POINT('Origin',(6.1,-24.,-12.1857384988752));
#142132=CARTESIAN_POINT('Origin',(6.1,-24.4,-12.1857384988752));
#142133=CARTESIAN_POINT('Origin',(11.3,-24.,-7.32500000002662));
#142134=CARTESIAN_POINT('',(10.9,-24.,-12.5077037206369));
#142135=CARTESIAN_POINT('Origin',(11.3,-24.,-12.5077037206369));
#142136=CARTESIAN_POINT('',(10.9,-24.,-7.32500000002662));
#142137=CARTESIAN_POINT('',(11.3,-24.4,-7.32500000002662));
#142138=CARTESIAN_POINT('Origin',(15.1,-24.,-15.1));
#142139=CARTESIAN_POINT('Origin',(15.1,-24.,-15.1));
#142140=CARTESIAN_POINT('Origin',(15.1,-24.4,-15.1));
#142141=CARTESIAN_POINT('Origin',(11.3,-24.,-12.5077037206369));
#142142=CARTESIAN_POINT('Origin',(11.3,-24.,-12.5077037206369));
#142143=CARTESIAN_POINT('Origin',(17.9686291501015,-23.,-11.7813708499319));
#142144=CARTESIAN_POINT('',(15.1343145750407,-22.1,-8.94705627487116));
#142145=CARTESIAN_POINT('',(15.1343145750407,-23.,-8.94705627487115));
#142146=CARTESIAN_POINT('',(15.7218887667622,-22.1,-9.53463046659261));
#142147=CARTESIAN_POINT('',(17.9686291501015,-22.1,-11.7813708499319));
#142148=CARTESIAN_POINT('',(15.7218887667622,-22.1,-9.53463046659261));
#142149=CARTESIAN_POINT('Origin',(15.69999999999,-23.,-8.38137084992192));
#142150=CARTESIAN_POINT('',(14.89999999999,-22.1,-8.38137084992041));
#142151=CARTESIAN_POINT('',(14.89999999999,-23.,-8.38137084992041));
#142152=CARTESIAN_POINT('Origin',(15.69999999999,-22.1,-8.38137084992192));
#142153=CARTESIAN_POINT('Origin',(14.899999999995,-24.,-5.70716730244972));
#142154=CARTESIAN_POINT('',(14.8999999999902,-22.1,-8.27794038524318));
#142155=CARTESIAN_POINT('',(14.8999999999902,-22.1,-8.27794038524318));
#142156=CARTESIAN_POINT('',(14.8999999999893,-22.1,-8.71274169981977));
#142157=CARTESIAN_POINT('Origin',(14.0999999999902,-22.1,-8.27794038524168));
#142158=CARTESIAN_POINT('',(13.9839732502781,-22.1,-7.48639898180705));
#142159=CARTESIAN_POINT('',(13.9839732502781,-22.1,-7.48639898180705));
#142160=CARTESIAN_POINT('Origin',(14.0999999999902,-22.1,-8.27794038524168));
#142161=CARTESIAN_POINT('Origin',(15.1,-22.1,-15.1));
#142162=CARTESIAN_POINT('',(11.7393688126037,-22.1,-8.17767422085447));
#142163=CARTESIAN_POINT('',(11.7393688126037,-22.1,-8.17767422085447));
#142164=CARTESIAN_POINT('Origin',(15.1,-22.1,-15.1));
#142165=CARTESIAN_POINT('Origin',(9.25,-22.1,-3.05000000003699));
#142166=CARTESIAN_POINT('',(10.4729371725502,-22.1,-8.61726366111815));
#142167=CARTESIAN_POINT('',(10.4729371725502,-22.1,-8.61726366111815));
#142168=CARTESIAN_POINT('Origin',(9.25,-22.1,-3.05000000003699));
#142169=CARTESIAN_POINT('Origin',(-3.45175358661618,-24.4,-3.05000000003699));
#142170=CARTESIAN_POINT('Origin',(17.1,-24.,0.396768100868128));
#142171=CARTESIAN_POINT('',(17.5,-24.,5.54411254966196));
#142172=CARTESIAN_POINT('',(17.1,-24.4,5.54411254966196));
#142173=CARTESIAN_POINT('Origin',(17.1,-24.,5.54411254966196));
#142174=CARTESIAN_POINT('',(17.1,-24.4,11.));
#142175=CARTESIAN_POINT('',(17.1,-24.4,0.396768100868128));
#142176=CARTESIAN_POINT('',(17.5,-24.,11.));
#142177=CARTESIAN_POINT('Origin',(17.1,-24.,11.));
#142178=CARTESIAN_POINT('',(17.5,-24.,0.396768100868128));
#142179=CARTESIAN_POINT('Ctrl Pts',(17.5,-24.,11.));
#142180=CARTESIAN_POINT('Ctrl Pts',(17.5,-24.,11.6));
#142181=CARTESIAN_POINT('Ctrl Pts',(16.9,-24.,11.6));
#142182=CARTESIAN_POINT('Ctrl Pts',(17.5,-24.4,11.));
#142183=CARTESIAN_POINT('Ctrl Pts',(17.5,-24.4,11.6));
#142184=CARTESIAN_POINT('Ctrl Pts',(16.9,-24.4,11.6));
#142185=CARTESIAN_POINT('Ctrl Pts',(17.1,-24.4,11.));
#142186=CARTESIAN_POINT('Ctrl Pts',(17.1,-24.4,11.2));
#142187=CARTESIAN_POINT('Ctrl Pts',(16.9,-24.4,11.2));
#142188=CARTESIAN_POINT('',(16.9,-24.4,11.2));
#142189=CARTESIAN_POINT('',(16.9,-24.,11.6));
#142190=CARTESIAN_POINT('Origin',(16.9,-24.,11.2));
#142191=CARTESIAN_POINT('Origin',(16.9,-24.,11.));
#142192=CARTESIAN_POINT('Origin',(16.9,-24.4,11.));
#142193=CARTESIAN_POINT('Origin',(7.02412320669191,-24.,11.2));
#142194=CARTESIAN_POINT('',(16.3999999999996,-24.4,11.2));
#142195=CARTESIAN_POINT('',(16.3999999999996,-24.,11.6));
#142196=CARTESIAN_POINT('Origin',(16.3999999999996,-24.,11.2));
#142197=CARTESIAN_POINT('',(7.02412320669191,-24.,11.6));
#142198=CARTESIAN_POINT('',(7.02412320669191,-24.4,11.2));
#142199=CARTESIAN_POINT('Origin',(16.3999999999996,-24.,15.7));
#142200=CARTESIAN_POINT('',(14.5808510638294,-24.4,11.5840921842161));
#142201=CARTESIAN_POINT('',(14.742553191489,-24.,11.9499506567302));
#142202=CARTESIAN_POINT('Origin',(14.5808510638294,-24.,11.5840921842161));
#142203=CARTESIAN_POINT('Origin',(16.3999999999996,-24.,15.7));
#142204=CARTESIAN_POINT('Origin',(16.3999999999996,-24.4,15.7));
#142205=CARTESIAN_POINT('Ctrl Pts',(14.742553191489,-24.,11.9499506567302));
#142206=CARTESIAN_POINT('Ctrl Pts',(14.4450678125079,-24.,12.0814332445142));
#142207=CARTESIAN_POINT('Ctrl Pts',(14.1725339062537,-24.,11.9039212969169));
#142208=CARTESIAN_POINT('Ctrl Pts',(13.8999999999996,-24.,11.7264093493195));
#142209=CARTESIAN_POINT('Ctrl Pts',(13.8999999999996,-24.,11.401162947959));
#142210=CARTESIAN_POINT('Ctrl Pts',(14.742553191489,-24.4,11.9499506567302));
#142211=CARTESIAN_POINT('Ctrl Pts',(14.4450678125079,-24.4,12.0814332445142));
#142212=CARTESIAN_POINT('Ctrl Pts',(14.1725339062537,-24.4,11.9039212969169));
#142213=CARTESIAN_POINT('Ctrl Pts',(13.8999999999996,-24.4,11.7264093493195));
#142214=CARTESIAN_POINT('Ctrl Pts',(13.8999999999996,-24.4,11.401162947959));
#142215=CARTESIAN_POINT('Ctrl Pts',(14.5808510638294,-24.4,11.5840921842161));
#142216=CARTESIAN_POINT('Ctrl Pts',(14.4816892708357,-24.4,11.6279197134774));
#142217=CARTESIAN_POINT('Ctrl Pts',(14.3908446354177,-24.4,11.5687490642783));
#142218=CARTESIAN_POINT('Ctrl Pts',(14.2999999999996,-24.4,11.5095784150792));
#142219=CARTESIAN_POINT('Ctrl Pts',(14.2999999999996,-24.4,11.401162947959));
#142220=CARTESIAN_POINT('',(14.2999999999996,-24.4,11.401162947959));
#142221=CARTESIAN_POINT('',(13.8999999999996,-24.,11.401162947959));
#142222=CARTESIAN_POINT('Origin',(14.2999999999996,-24.,11.401162947959));
#142223=CARTESIAN_POINT('Origin',(14.4999999999996,-24.,11.401162947959));
#142224=CARTESIAN_POINT('Origin',(14.4999999999996,-24.4,11.401162947959));
#142225=CARTESIAN_POINT('Origin',(14.2999999999999,-24.,-0.800000000036603));
#142226=CARTESIAN_POINT('',(14.2999999999997,-24.4,9.24999999996345));
#142227=CARTESIAN_POINT('',(13.8999999999997,-24.,9.24999999996345));
#142228=CARTESIAN_POINT('Origin',(14.2999999999997,-24.,9.24999999996345));
#142229=CARTESIAN_POINT('',(13.8999999999999,-24.,-0.80000000003661));
#142230=CARTESIAN_POINT('',(14.2999999999999,-24.4,-0.800000000036603));
#142231=CARTESIAN_POINT('Origin',(6.09999999999969,-24.,9.2499999999633));
#142232=CARTESIAN_POINT('',(12.8526992139868,-24.4,4.59800544650364));
#142233=CARTESIAN_POINT('',(12.5232992523289,-24.,4.82493201008704));
#142234=CARTESIAN_POINT('Origin',(12.8526992139868,-24.,4.59800544650364));
#142235=CARTESIAN_POINT('Origin',(6.09999999999969,-24.,9.2499999999633));
#142236=CARTESIAN_POINT('Origin',(6.09999999999969,-24.4,9.2499999999633));
#142237=CARTESIAN_POINT('Ctrl Pts',(12.5232992523289,-24.,4.82493201008704));
#142238=CARTESIAN_POINT('Ctrl Pts',(12.3051223920045,-24.,4.50823286173429));
#142239=CARTESIAN_POINT('Ctrl Pts',(12.5017731872981,-24.,4.17773632974227));
#142240=CARTESIAN_POINT('Ctrl Pts',(12.6984239825917,-24.,3.84723979775026));
#142241=CARTESIAN_POINT('Ctrl Pts',(13.080844887153,-24.,3.88790605775575));
#142242=CARTESIAN_POINT('Ctrl Pts',(12.5232992523289,-24.4,4.82493201008704));
#142243=CARTESIAN_POINT('Ctrl Pts',(12.3051223920045,-24.4,4.50823286173429));
#142244=CARTESIAN_POINT('Ctrl Pts',(12.5017731872981,-24.4,4.17773632974227));
#142245=CARTESIAN_POINT('Ctrl Pts',(12.6984239825917,-24.4,3.84723979775026));
#142246=CARTESIAN_POINT('Ctrl Pts',(13.080844887153,-24.4,3.88790605775575));
#142247=CARTESIAN_POINT('Ctrl Pts',(12.8526992139868,-24.4,4.59800544650365));
#142248=CARTESIAN_POINT('Ctrl Pts',(12.7799735938787,-24.4,4.49243906371939));
#142249=CARTESIAN_POINT('Ctrl Pts',(12.8455238589765,-24.4,4.38227355305539));
#142250=CARTESIAN_POINT('Ctrl Pts',(12.9110741240744,-24.4,4.27210804239138));
#142251=CARTESIAN_POINT('Ctrl Pts',(13.0385477589281,-24.4,4.28566346239322));
#142252=CARTESIAN_POINT('',(13.0385477589281,-24.4,4.28566346239322));
#142253=CARTESIAN_POINT('',(13.080844887153,-24.,3.88790605775575));
#142254=CARTESIAN_POINT('Origin',(13.0385477589281,-24.,4.28566346239322));
#142255=CARTESIAN_POINT('Origin',(13.0173991948157,-24.,4.48454216471195));
#142256=CARTESIAN_POINT('Origin',(13.0173991948157,-24.4,4.48454216471195));
#142257=CARTESIAN_POINT('Origin',(15.1,-24.,-15.1));
#142258=CARTESIAN_POINT('',(15.9166307959896,-24.4,4.37785017301522));
#142259=CARTESIAN_POINT('',(15.899875065829,-24.,3.97820127021829));
#142260=CARTESIAN_POINT('Origin',(15.9166307959896,-24.,4.37785017301522));
#142261=CARTESIAN_POINT('Origin',(15.1,-24.,-15.1));
#142262=CARTESIAN_POINT('Origin',(15.1,-24.4,-15.1));
#142263=CARTESIAN_POINT('Ctrl Pts',(15.899875065829,-24.,3.97820127021829));
#142264=CARTESIAN_POINT('Ctrl Pts',(16.2507487943837,-24.,3.9634904941472));
#142265=CARTESIAN_POINT('Ctrl Pts',(16.4990719510994,-24.,4.2118136508629));
#142266=CARTESIAN_POINT('Ctrl Pts',(15.899875065829,-24.4,3.97820127021829));
#142267=CARTESIAN_POINT('Ctrl Pts',(16.2507487943837,-24.4,3.9634904941472));
#142268=CARTESIAN_POINT('Ctrl Pts',(16.4990719510994,-24.4,4.2118136508629));
#142269=CARTESIAN_POINT('Ctrl Pts',(15.9166307959896,-24.4,4.37785017301522));
#142270=CARTESIAN_POINT('Ctrl Pts',(16.0920676602669,-24.4,4.37049478497967));
#142271=CARTESIAN_POINT('Ctrl Pts',(16.2162292386248,-24.4,4.49465636333752));
#142272=CARTESIAN_POINT('',(16.2162292386248,-24.4,4.49465636333752));
#142273=CARTESIAN_POINT('',(16.4990719510994,-24.,4.2118136508629));
#142274=CARTESIAN_POINT('Origin',(16.2162292386248,-24.,4.49465636333752));
#142275=CARTESIAN_POINT('Origin',(15.9333865261502,-24.,4.77749907581214));
#142276=CARTESIAN_POINT('Origin',(15.9333865261502,-24.4,4.77749907581214));
#142277=CARTESIAN_POINT('Origin',(8.90268758620957,-24.,-2.81888528907772));
#142278=CARTESIAN_POINT('',(16.9828427124746,-24.4,5.26126983718734));
#142279=CARTESIAN_POINT('',(17.2656854249492,-24.,4.97842712471272));
#142280=CARTESIAN_POINT('Origin',(16.9828427124746,-24.,5.26126983718734));
#142281=CARTESIAN_POINT('',(9.18553029868418,-24.,-3.10172800155234));
#142282=CARTESIAN_POINT('',(8.90268758620957,-24.4,-2.81888528907772));
#142283=CARTESIAN_POINT('Ctrl Pts',(17.2656854249492,-24.,4.97842712471272));
#142284=CARTESIAN_POINT('Ctrl Pts',(17.5,-24.,5.21274169976348));
#142285=CARTESIAN_POINT('Ctrl Pts',(17.5,-24.,5.54411254966196));
#142286=CARTESIAN_POINT('Ctrl Pts',(17.2656854249492,-24.4,4.97842712471272));
#142287=CARTESIAN_POINT('Ctrl Pts',(17.5,-24.4,5.21274169976348));
#142288=CARTESIAN_POINT('Ctrl Pts',(17.5,-24.4,5.54411254966196));
#142289=CARTESIAN_POINT('Ctrl Pts',(16.9828427124746,-24.4,5.26126983718734));
#142290=CARTESIAN_POINT('Ctrl Pts',(17.1,-24.4,5.37842712471272));
#142291=CARTESIAN_POINT('Ctrl Pts',(17.1,-24.4,5.54411254966196));
#142292=CARTESIAN_POINT('Origin',(16.7,-24.,5.54411254966196));
#142293=CARTESIAN_POINT('Origin',(16.7,-24.4,5.54411254966196));
#142294=CARTESIAN_POINT('Origin',(13.0173991948157,-22.1,4.48454216471195));
#142295=CARTESIAN_POINT('',(13.080844887153,-22.1,3.88790605775575));
#142296=CARTESIAN_POINT('',(13.080844887153,-22.1,3.88790605775575));
#142297=CARTESIAN_POINT('',(12.5232992523289,-22.1,4.82493201008704));
#142298=CARTESIAN_POINT('Origin',(13.0173991948157,-22.1,4.48454216471195));
#142299=CARTESIAN_POINT('',(12.5232992523289,-22.1,4.82493201008704));
#142300=CARTESIAN_POINT('Origin',(15.1,-22.1,-15.1));
#142301=CARTESIAN_POINT('',(15.899875065829,-22.1,3.97820127021829));
#142302=CARTESIAN_POINT('',(15.899875065829,-22.1,3.97820127021829));
#142303=CARTESIAN_POINT('Origin',(15.1,-22.1,-15.1));
#142304=CARTESIAN_POINT('Origin',(15.9333865261502,-22.1,4.77749907581214));
#142305=CARTESIAN_POINT('',(16.4990719510994,-22.1,4.2118136508629));
#142306=CARTESIAN_POINT('',(16.4990719510994,-22.1,4.2118136508629));
#142307=CARTESIAN_POINT('Origin',(15.9333865261502,-22.1,4.77749907581214));
#142308=CARTESIAN_POINT('Origin',(15.4783082405767,-23.,3.19104994034017));
#142309=CARTESIAN_POINT('',(17.2656854249492,-22.1,4.97842712471272));
#142310=CARTESIAN_POINT('',(17.2656854249492,-22.55,4.97842712471272));
#142311=CARTESIAN_POINT('',(14.9000000000107,-22.1,2.61274169977414));
#142312=CARTESIAN_POINT('Origin',(16.7,-22.55,5.54411254966196));
#142313=CARTESIAN_POINT('',(17.5,-22.1,5.54411254966196));
#142314=CARTESIAN_POINT('',(17.5,-22.55,5.54411254966196));
#142315=CARTESIAN_POINT('Origin',(16.7,-22.1,5.54411254966196));
#142316=CARTESIAN_POINT('Origin',(17.5,-22.1,3.84353620177326));
#142317=CARTESIAN_POINT('',(17.5,-22.1,11.));
#142318=CARTESIAN_POINT('',(17.5,-22.1,11.));
#142319=CARTESIAN_POINT('',(17.5,-22.1,1.69676810087534));
#142320=CARTESIAN_POINT('Origin',(-3.45175358661618,-24.4,-3.05000000003699));
#142321=CARTESIAN_POINT('Origin',(0.999999999210583,-24.,-4.75788611936281));
#142322=CARTESIAN_POINT('',(0.599999999210584,-24.,-0.0238638518621566));
#142323=CARTESIAN_POINT('',(0.999999999210584,-24.4,-0.0238638518621564));
#142324=CARTESIAN_POINT('Origin',(0.999999999210584,-24.,-0.0238638518621564));
#142325=CARTESIAN_POINT('',(0.999999999210583,-24.4,-1.85000000003699));
#142326=CARTESIAN_POINT('',(0.999999999210583,-24.4,-4.75788611936281));
#142327=CARTESIAN_POINT('',(0.599999999210584,-24.,-1.85000000003699));
#142328=CARTESIAN_POINT('Origin',(0.999999999210583,-24.,-1.85000000003699));
#142329=CARTESIAN_POINT('',(0.599999999210583,-24.,-4.75788611936281));
#142330=CARTESIAN_POINT('Ctrl Pts',(0.599999999210584,-24.,-1.85000000003699));
#142331=CARTESIAN_POINT('Ctrl Pts',(0.599999999210584,-24.,-2.45000000003699));
#142332=CARTESIAN_POINT('Ctrl Pts',(1.19999999921058,-24.,-2.45000000003699));
#142333=CARTESIAN_POINT('Ctrl Pts',(0.599999999210584,-24.4,-1.85000000003699));
#142334=CARTESIAN_POINT('Ctrl Pts',(0.599999999210584,-24.4,-2.45000000003699));
#142335=CARTESIAN_POINT('Ctrl Pts',(1.19999999921058,-24.4,-2.45000000003699));
#142336=CARTESIAN_POINT('Ctrl Pts',(0.999999999210584,-24.4,-1.85000000003699));
#142337=CARTESIAN_POINT('Ctrl Pts',(0.999999999210584,-24.4,-2.05000000003699));
#142338=CARTESIAN_POINT('Ctrl Pts',(1.19999999921058,-24.4,-2.05000000003699));
#142339=CARTESIAN_POINT('',(1.19999999921058,-24.4,-2.05000000003699));
#142340=CARTESIAN_POINT('',(1.19999999921058,-24.,-2.45000000003699));
#142341=CARTESIAN_POINT('Origin',(1.19999999921058,-24.,-2.05000000003699));
#142342=CARTESIAN_POINT('Origin',(1.19999999921058,-24.,-1.85000000003699));
#142343=CARTESIAN_POINT('Origin',(1.19999999921058,-24.4,-1.85000000003699));
#142344=CARTESIAN_POINT('Origin',(-4.69720428956801,-24.,-2.05000000003699));
#142345=CARTESIAN_POINT('',(4.3,-24.4,-2.05000000003699));
#142346=CARTESIAN_POINT('',(4.3,-24.,-2.45000000003699));
#142347=CARTESIAN_POINT('Origin',(4.3,-24.,-2.05000000003699));
#142348=CARTESIAN_POINT('',(-4.69720428956801,-24.,-2.45000000003699));
#142349=CARTESIAN_POINT('',(-4.69720428956801,-24.4,-2.05000000003699));
#142350=CARTESIAN_POINT('Ctrl Pts',(4.3,-24.,-2.45000000003699));
#142351=CARTESIAN_POINT('Ctrl Pts',(4.9,-24.,-2.45000000003699));
#142352=CARTESIAN_POINT('Ctrl Pts',(4.9,-24.,-1.85000000003699));
#142353=CARTESIAN_POINT('Ctrl Pts',(4.3,-24.4,-2.45000000003699));
#142354=CARTESIAN_POINT('Ctrl Pts',(4.9,-24.4,-2.45000000003699));
#142355=CARTESIAN_POINT('Ctrl Pts',(4.9,-24.4,-1.85000000003699));
#142356=CARTESIAN_POINT('Ctrl Pts',(4.3,-24.4,-2.05000000003699));
#142357=CARTESIAN_POINT('Ctrl Pts',(4.5,-24.4,-2.05000000003699));
#142358=CARTESIAN_POINT('Ctrl Pts',(4.5,-24.4,-1.85000000003699));
#142359=CARTESIAN_POINT('',(4.5,-24.4,-1.85000000003699));
#142360=CARTESIAN_POINT('',(4.9,-24.,-1.85000000003699));
#142361=CARTESIAN_POINT('Origin',(4.5,-24.,-1.85000000003699));
#142362=CARTESIAN_POINT('Origin',(4.3,-24.,-1.85000000003699));
#142363=CARTESIAN_POINT('Origin',(4.3,-24.4,-1.85000000003699));
#142364=CARTESIAN_POINT('Origin',(4.5,-24.,-4.18858360955962));
#142365=CARTESIAN_POINT('',(4.5,-24.4,-0.74199679747406));
#142366=CARTESIAN_POINT('',(4.9,-24.,-0.74199679747406));
#142367=CARTESIAN_POINT('Origin',(4.5,-24.,-0.74199679747406));
#142368=CARTESIAN_POINT('',(4.9,-24.,-4.18858360955962));
#142369=CARTESIAN_POINT('',(4.5,-24.4,-4.18858360955962));
#142370=CARTESIAN_POINT('Origin',(8.6,-24.,-0.741996797474058));
#142371=CARTESIAN_POINT('',(7.60485436893191,-24.4,3.23539998597188));
#142372=CARTESIAN_POINT('',(7.7019417475727,-24.,2.84736127539179));
#142373=CARTESIAN_POINT('Origin',(7.60485436893191,-24.,3.23539998597188));
#142374=CARTESIAN_POINT('Origin',(8.6,-24.,-0.741996797474058));
#142375=CARTESIAN_POINT('Origin',(8.6,-24.4,-0.741996797474058));
#142376=CARTESIAN_POINT('Origin',(6.09999999999969,-24.,9.2499999999633));
#142377=CARTESIAN_POINT('',(11.6600331084108,-24.4,6.50663858859724));
#142378=CARTESIAN_POINT('',(12.0187449218567,-24.,6.32964752979943));
#142379=CARTESIAN_POINT('Origin',(11.6600331084108,-24.,6.50663858859724));
#142380=CARTESIAN_POINT('Origin',(6.09999999999969,-24.,9.2499999999633));
#142381=CARTESIAN_POINT('Origin',(6.09999999999969,-24.4,9.2499999999633));
#142382=CARTESIAN_POINT('Ctrl Pts',(12.0187449218567,-24.,6.32964752979943));
#142383=CARTESIAN_POINT('Ctrl Pts',(12.1810106563356,-24.,6.65851519277877));
#142384=CARTESIAN_POINT('Ctrl Pts',(11.9623390923243,-24.,6.9529075422587));
#142385=CARTESIAN_POINT('Ctrl Pts',(11.7436675283129,-24.,7.24729989173863));
#142386=CARTESIAN_POINT('Ctrl Pts',(11.381945787434,-24.,7.18695512796406));
#142387=CARTESIAN_POINT('Ctrl Pts',(12.0187449218567,-24.4,6.32964752979943));
#142388=CARTESIAN_POINT('Ctrl Pts',(12.1810106563356,-24.4,6.65851519277877));
#142389=CARTESIAN_POINT('Ctrl Pts',(11.9623390923243,-24.4,6.9529075422587));
#142390=CARTESIAN_POINT('Ctrl Pts',(11.7436675283129,-24.4,7.24729989173863));
#142391=CARTESIAN_POINT('Ctrl Pts',(11.381945787434,-24.4,7.18695512796406));
#142392=CARTESIAN_POINT('Ctrl Pts',(11.6600331084108,-24.4,6.50663858859724));
#142393=CARTESIAN_POINT('Ctrl Pts',(11.7141216865704,-24.4,6.61626114292369));
#142394=CARTESIAN_POINT('Ctrl Pts',(11.6412311652333,-24.4,6.71439192608367));
#142395=CARTESIAN_POINT('Ctrl Pts',(11.5683406438962,-24.4,6.81252270924365));
#142396=CARTESIAN_POINT('Ctrl Pts',(11.4477667302699,-24.4,6.79240778798545));
#142397=CARTESIAN_POINT('',(11.4477667302699,-24.4,6.79240778798545));
#142398=CARTESIAN_POINT('',(11.381945787434,-24.,7.18695512796406));
#142399=CARTESIAN_POINT('Origin',(11.4477667302699,-24.,6.79240778798545));
#142400=CARTESIAN_POINT('Origin',(11.4806772016879,-24.,6.59513411799615));
#142401=CARTESIAN_POINT('Origin',(11.4806772016879,-24.4,6.59513411799615));
#142402=CARTESIAN_POINT('Origin',(15.1,-24.,-15.1));
#142403=CARTESIAN_POINT('',(5.40676393843642,-24.4,4.86640932333035));
#142404=CARTESIAN_POINT('',(5.23207139018353,-24.,5.22624611075613));
#142405=CARTESIAN_POINT('Origin',(5.40676393843642,-24.,4.86640932333035));
#142406=CARTESIAN_POINT('Origin',(15.1,-24.,-15.1));
#142407=CARTESIAN_POINT('Origin',(15.1,-24.4,-15.1));
#142408=CARTESIAN_POINT('Origin',(9.25,-24.,-3.05000000003699));
#142409=CARTESIAN_POINT('',(1.01279069686664,-24.4,0.0465114073977232));
#142410=CARTESIAN_POINT('',(0.638372092178764,-24.,0.187261925917483));
#142411=CARTESIAN_POINT('Origin',(1.01279069686664,-24.,0.0465114073977232));
#142412=CARTESIAN_POINT('Origin',(9.25,-24.,-3.05000000003699));
#142413=CARTESIAN_POINT('Origin',(9.25,-24.4,-3.05000000003699));
#142414=CARTESIAN_POINT('Ctrl Pts',(0.638372092178765,-24.,0.187261925917483));
#142415=CARTESIAN_POINT('Ctrl Pts',(0.599999999210585,-24.,0.0851860994182524));
#142416=CARTESIAN_POINT('Ctrl Pts',(0.599999999210585,-24.,-0.0238638518621567));
#142417=CARTESIAN_POINT('Ctrl Pts',(0.638372092178765,-24.4,0.187261925917482));
#142418=CARTESIAN_POINT('Ctrl Pts',(0.599999999210585,-24.4,0.0851860994182523));
#142419=CARTESIAN_POINT('Ctrl Pts',(0.599999999210585,-24.4,-0.0238638518621568));
#142420=CARTESIAN_POINT('Ctrl Pts',(1.01279069686665,-24.4,0.0465114073977229));
#142421=CARTESIAN_POINT('Ctrl Pts',(0.999999999210585,-24.4,0.0124861318979795));
#142422=CARTESIAN_POINT('Ctrl Pts',(0.999999999210585,-24.4,-0.0238638518621568));
#142423=CARTESIAN_POINT('Origin',(1.19999999921058,-24.,-0.0238638518621567));
#142424=CARTESIAN_POINT('Origin',(1.19999999921058,-24.4,-0.0238638518621568));
#142425=CARTESIAN_POINT('Origin',(6.09999999999969,-19.9,9.2499999999633));
#142426=CARTESIAN_POINT('',(12.0187449218567,-20.,6.32964752979944));
#142427=CARTESIAN_POINT('',(12.0187449218567,-19.9,6.32964752979943));
#142428=CARTESIAN_POINT('',(7.7019417475727,-20.,2.84736127539179));
#142429=CARTESIAN_POINT('Origin',(6.09999999999969,-20.,9.2499999999633));
#142430=CARTESIAN_POINT('',(7.7019417475727,-19.9,2.84736127539179));
#142431=CARTESIAN_POINT('Origin',(11.4806772016879,-19.9,6.59513411799615));
#142432=CARTESIAN_POINT('',(11.381945787434,-20.,7.18695512796406));
#142433=CARTESIAN_POINT('',(11.381945787434,-19.9,7.18695512796406));
#142434=CARTESIAN_POINT('Origin',(11.4806772016879,-20.,6.59513411799615));
#142435=CARTESIAN_POINT('Origin',(15.1,-19.9,-15.1));
#142436=CARTESIAN_POINT('',(5.23207139018353,-15.9,5.22624611075614));
#142437=CARTESIAN_POINT('',(5.23207139018353,-19.9,5.22624611075614));
#142438=CARTESIAN_POINT('',(13.3925518029794,-15.9,7.43035544899269));
#142439=CARTESIAN_POINT('Origin',(15.1,-15.9,-15.1));
#142440=CARTESIAN_POINT('',(13.3925518029794,-20.,7.43035544899269));
#142441=CARTESIAN_POINT('',(13.3925518029795,-19.9,7.43035544899269));
#142442=CARTESIAN_POINT('Origin',(15.1,-20.,-15.1));
#142443=CARTESIAN_POINT('Origin',(9.25,-21.1,-3.05000000003699));
#142444=CARTESIAN_POINT('',(0.638372092178764,-20.,0.187261925917484));
#142445=CARTESIAN_POINT('',(0.638372092178764,-21.1,0.187261925917483));
#142446=CARTESIAN_POINT('',(0.159697928570087,-20.,-1.63352259105473));
#142447=CARTESIAN_POINT('Origin',(9.25,-20.,-3.05000000003699));
#142448=CARTESIAN_POINT('',(0.159697928570086,-19.2185290786118,-1.63352259105473));
#142449=CARTESIAN_POINT('',(0.159697928570086,-21.1,-1.63352259105473));
#142450=CARTESIAN_POINT('',(0.184164224908069,-19.1828954869493,-1.48455383390278));
#142451=CARTESIAN_POINT('Ctrl Pts',(0.184164224908773,-19.1828954869485,
-1.48455383389902));
#142452=CARTESIAN_POINT('Ctrl Pts',(0.181353760516264,-19.1834220810812,
-1.50082983826466));
#142453=CARTESIAN_POINT('Ctrl Pts',(0.178601777697792,-19.1849707452015,
-1.51707236850617));
#142454=CARTESIAN_POINT('Ctrl Pts',(0.175910270632949,-19.1875443857133,
-1.53316372260399));
#142455=CARTESIAN_POINT('Ctrl Pts',(0.174241610022826,-19.1891399722911,
-1.54313992110531));
#142456=CARTESIAN_POINT('Ctrl Pts',(0.172597130274316,-19.1911297373904,
-1.55305778148705));
#142457=CARTESIAN_POINT('Ctrl Pts',(0.170986625987962,-19.1935166139609,
-1.56288598586302));
#142458=CARTESIAN_POINT('Ctrl Pts',(0.16828963437131,-19.1975137384361,
-1.57934454796268));
#142459=CARTESIAN_POINT('Ctrl Pts',(0.165686978366581,-19.2026151899126,
-1.59551812123727));
#142460=CARTESIAN_POINT('Ctrl Pts',(0.163189474647243,-19.2088472856758,
-1.61127304108951));
#142461=CARTESIAN_POINT('Ctrl Pts',(0.162001044626545,-19.2118128106676,
-1.61876997476017));
#142462=CARTESIAN_POINT('Ctrl Pts',(0.16083686547626,-19.2150346144176,
-1.62617154830696));
#142463=CARTESIAN_POINT('Ctrl Pts',(0.159700282405873,-19.2185167914062,
-1.63346006998121));
#142464=CARTESIAN_POINT('',(0.506210580792261,-17.3375900928828,-0.188855719761902));
#142465=CARTESIAN_POINT('Ctrl Pts',(0.506210580792261,-17.3375900928828,
-0.188855719761907));
#142466=CARTESIAN_POINT('Ctrl Pts',(0.580278907014156,-17.381066136149,
0.0375005152529757));
#142467=CARTESIAN_POINT('Ctrl Pts',(0.669274719311132,-17.4473071571919,
0.274849655756337));
#142468=CARTESIAN_POINT('Ctrl Pts',(0.792548014213962,-17.586657437599,
0.572772974625153));
#142469=CARTESIAN_POINT('Ctrl Pts',(0.845006682143812,-17.6581943501699,
0.692397462978445));
#142470=CARTESIAN_POINT('Ctrl Pts',(0.914713320592898,-17.7910311183224,
0.844601700992352));
#142471=CARTESIAN_POINT('Ctrl Pts',(0.944350360166487,-17.8608514992075,
0.907096140123004));
#142472=CARTESIAN_POINT('Ctrl Pts',(0.976481807510859,-17.9804818034157,
0.973618150343783));
#142473=CARTESIAN_POINT('Ctrl Pts',(0.985172457114319,-18.0228461575066,
0.991385474329735));
#142474=CARTESIAN_POINT('Ctrl Pts',(0.996932135198067,-18.1102055287159,
1.01534824533723));
#142475=CARTESIAN_POINT('Ctrl Pts',(1.,-18.1551996258224,1.02154761727023));
#142476=CARTESIAN_POINT('Ctrl Pts',(1.,-18.2,1.02154761727023));
#142477=CARTESIAN_POINT('Ctrl Pts',(1.,-18.2593850884882,1.02154761727022));
#142478=CARTESIAN_POINT('Ctrl Pts',(0.994695748169923,-18.3171214241364,
1.01084158300733));
#142479=CARTESIAN_POINT('Ctrl Pts',(0.972999971362076,-18.4411618339318,
0.966468917575704));
#142480=CARTESIAN_POINT('Ctrl Pts',(0.954670937162076,-18.5034679387583,
0.928689483412159));
#142481=CARTESIAN_POINT('Ctrl Pts',(0.8978478687292,-18.6513824418007,0.808562130066912));
#142482=CARTESIAN_POINT('Ctrl Pts',(0.853199148505529,-18.7268262065284,
0.711075214280202));
#142483=CARTESIAN_POINT('Ctrl Pts',(0.703337160928647,-18.9335978311899,
0.365553184470413));
#142484=CARTESIAN_POINT('Ctrl Pts',(0.584646620624056,-19.0181565122869,
0.055144231507496));
#142485=CARTESIAN_POINT('Ctrl Pts',(0.475205795724452,-19.0801011465358,
-0.284823424914531));
#142486=CARTESIAN_POINT('Ctrl Pts',(0.458257453044452,-19.0890086151428,
-0.339186673888201));
#142487=CARTESIAN_POINT('Ctrl Pts',(0.441807997660264,-19.0971096327671,
-0.393733136576476));
#142488=CARTESIAN_POINT('Ctrl Pts',(0.377329500084536,-19.1288639634147,
-0.607544103570025));
#142489=CARTESIAN_POINT('Ctrl Pts',(0.319510142661645,-19.1489487401334,
-0.828054390322394));
#142490=CARTESIAN_POINT('Ctrl Pts',(0.23834220554392,-19.1717559114687,
-1.19207823060078));
#142491=CARTESIAN_POINT('Ctrl Pts',(0.209486143478189,-19.1781509423164,
-1.33790915187365));
#142492=CARTESIAN_POINT('Ctrl Pts',(0.184164224908118,-19.1828954869486,
-1.48455383390281));
#142493=CARTESIAN_POINT('',(0.40335604954683,-17.2099042410653,-0.524749356257178));
#142494=CARTESIAN_POINT('Ctrl Pts',(0.403130429600274,-17.2100443552713,
-0.524549252433244));
#142495=CARTESIAN_POINT('Ctrl Pts',(0.407548590591942,-17.2208124362877,
-0.509132289531301));
#142496=CARTESIAN_POINT('Ctrl Pts',(0.412172338640691,-17.2307118184428,
-0.493157767087332));
#142497=CARTESIAN_POINT('Ctrl Pts',(0.416951623028926,-17.2398480136672,
-0.476819041514874));
#142498=CARTESIAN_POINT('Ctrl Pts',(0.418225874816477,-17.2422839040956,
-0.472462813976238));
#142499=CARTESIAN_POINT('Ctrl Pts',(0.419511363141136,-17.2446655122957,
-0.468080466407649));
#142500=CARTESIAN_POINT('Ctrl Pts',(0.420807513383204,-17.2469947858434,
-0.463675204646474));
#142501=CARTESIAN_POINT('Ctrl Pts',(0.426291621896912,-17.2568501162514,
-0.445036213003789));
#142502=CARTESIAN_POINT('Ctrl Pts',(0.43198280701597,-17.2658022765771,
-0.425926953399594));
#142503=CARTESIAN_POINT('Ctrl Pts',(0.437814431480213,-17.2739660976529,
-0.406566899304107));
#142504=CARTESIAN_POINT('Ctrl Pts',(0.439452911598933,-17.2762598424932,
-0.401127409171076));
#142505=CARTESIAN_POINT('Ctrl Pts',(0.441102768804601,-17.2784913221943,
-0.395667966425912));
#142506=CARTESIAN_POINT('Ctrl Pts',(0.442763141978182,-17.2806630452537,
-0.390193150631224));
#142507=CARTESIAN_POINT('Ctrl Pts',(0.449381559241047,-17.2893197554528,
-0.368369975008351));
#142508=CARTESIAN_POINT('Ctrl Pts',(0.456211562902522,-17.2970896099185,
-0.346146242590313));
#142509=CARTESIAN_POINT('Ctrl Pts',(0.463166341463394,-17.304076867005,
-0.323783362358173));
#142510=CARTESIAN_POINT('Ctrl Pts',(0.465562880074469,-17.3064845973513,
-0.316077364897278));
#142511=CARTESIAN_POINT('Ctrl Pts',(0.467974715975203,-17.3087993719827,
-0.308354963529586));
#142512=CARTESIAN_POINT('Ctrl Pts',(0.470399514304154,-17.3110254971623,
-0.300627410446533));
#142513=CARTESIAN_POINT('Ctrl Pts',(0.477253100275757,-17.3173175422038,
-0.27878582107703));
#142514=CARTESIAN_POINT('Ctrl Pts',(0.484291111603266,-17.322976955946,
-0.256640895596778));
#142515=CARTESIAN_POINT('Ctrl Pts',(0.491434018931853,-17.3280382086754,
-0.234423871949092));
#142516=CARTESIAN_POINT('Ctrl Pts',(0.496316244720445,-17.3314976093734,
-0.219238385030569));
#142517=CARTESIAN_POINT('Ctrl Pts',(0.501248496234294,-17.3346774875366,
-0.204020079963621));
#142518=CARTESIAN_POINT('Ctrl Pts',(0.506210580792283,-17.3375900928828,
-0.188855719761839));
#142519=CARTESIAN_POINT('',(0.159697928570089,-16.4335328638949,-1.63352259105473));
#142520=CARTESIAN_POINT('Origin',(9.25,-15.4417047044218,-3.05000000003699));
#142521=CARTESIAN_POINT('',(0.159697928570088,-15.9,-1.63352259105473));
#142522=CARTESIAN_POINT('',(0.159697928570087,-21.1,-1.63352259105473));
#142523=CARTESIAN_POINT('Origin',(9.25,-15.9,-3.05000000003699));
#142524=CARTESIAN_POINT('Origin',(1.19999999921058,-21.1,-0.0238638518621564));
#142525=CARTESIAN_POINT('',(0.599999999210584,-20.,-0.0238638518621564));
#142526=CARTESIAN_POINT('',(0.599999999210584,-21.1,-0.0238638518621563));
#142527=CARTESIAN_POINT('Origin',(1.19999999921058,-20.,-0.0238638518621563));
#142528=CARTESIAN_POINT('Origin',(0.599999999210582,-19.9,-6.46577223868862));
#142529=CARTESIAN_POINT('',(0.599999999210583,-20.,-1.85000000003699));
#142530=CARTESIAN_POINT('',(0.599999999210583,-19.9,-1.85000000003699));
#142531=CARTESIAN_POINT('',(0.599999999210583,-20.,-3.4578861193556));
#142532=CARTESIAN_POINT('Origin',(-3.45175358661618,-24.4,-3.05000000003699));
#142533=CARTESIAN_POINT('Origin',(-9.35,-24.,-3.05000000003699));
#142534=CARTESIAN_POINT('',(-9.75435462095199,-24.4,-15.093213746397));
#142535=CARTESIAN_POINT('',(-11.6859078763815,-24.4,-14.8714226890816));
#142536=CARTESIAN_POINT('Origin',(-9.35,-24.4,-3.05000000003699));
#142537=CARTESIAN_POINT('',(-11.6083673659622,-24.,-14.479010317661));
#142538=CARTESIAN_POINT('Origin',(-11.6859078763815,-24.,-14.8714226890816));
#142539=CARTESIAN_POINT('',(-9.354354620952,-24.,-14.6999991861862));
#142540=CARTESIAN_POINT('Origin',(-9.35,-24.,-3.05000000003699));
#142541=CARTESIAN_POINT('Ctrl Pts',(-9.35435462095199,-24.,-14.6999991861862));
#142542=CARTESIAN_POINT('Ctrl Pts',(-9.35435462095199,-24.037424083604,
-14.6999991861862));
#142543=CARTESIAN_POINT('Ctrl Pts',(-9.35960040832283,-24.0739958314266,
-14.7052459637971));
#142544=CARTESIAN_POINT('Ctrl Pts',(-9.38066945411349,-24.1485527620938,
-14.7262799468246));
#142545=CARTESIAN_POINT('Ctrl Pts',(-9.39750274952949,-24.1846222324459,
-14.7430693141688));
#142546=CARTESIAN_POINT('Ctrl Pts',(-9.4452457342648,-24.2588372562424,
-14.7905361348673));
#142547=CARTESIAN_POINT('Ctrl Pts',(-9.47880473566812,-24.2934419877695,
-14.8237995352573));
#142548=CARTESIAN_POINT('Ctrl Pts',(-9.5500240810494,-24.3466490845449,
-14.8940310481549));
#142549=CARTESIAN_POINT('Ctrl Pts',(-9.58800870687269,-24.3660751179944,
-14.9313311053489));
#142550=CARTESIAN_POINT('Ctrl Pts',(-9.66746480896846,-24.392789111755,
-15.0089629008643));
#142551=CARTESIAN_POINT('Ctrl Pts',(-9.70955513466183,-24.3996933673943,
-15.0498836464634));
#142552=CARTESIAN_POINT('Ctrl Pts',(-9.75246992778725,-24.399996669763,
-15.0913911669504));
#142553=CARTESIAN_POINT('Ctrl Pts',(-9.75341224988955,-24.4,-15.0923024847155));
#142554=CARTESIAN_POINT('Ctrl Pts',(-9.75435462095199,-24.4,-15.093213746397));
#142555=CARTESIAN_POINT('Ctrl Pts',(-11.6083673659622,-24.,-14.479010317661));
#142556=CARTESIAN_POINT('Ctrl Pts',(-11.9073491418757,-24.,-14.4199316514445));
#142557=CARTESIAN_POINT('Ctrl Pts',(-12.1314036071098,-24.,-14.6265230059077));
#142558=CARTESIAN_POINT('Ctrl Pts',(-12.355458072344,-24.,-14.8331143603709));
#142559=CARTESIAN_POINT('Ctrl Pts',(-12.3207815844978,-24.,-15.1358979998248));
#142560=CARTESIAN_POINT('Ctrl Pts',(-11.6083673659622,-24.4,-14.479010317661));
#142561=CARTESIAN_POINT('Ctrl Pts',(-11.9073491418757,-24.4,-14.4199316514445));
#142562=CARTESIAN_POINT('Ctrl Pts',(-12.1314036071098,-24.4,-14.6265230059077));
#142563=CARTESIAN_POINT('Ctrl Pts',(-12.355458072344,-24.4,-14.8331143603709));
#142564=CARTESIAN_POINT('Ctrl Pts',(-12.3207815844978,-24.4,-15.1358979998248));
#142565=CARTESIAN_POINT('Ctrl Pts',(-11.6859078763815,-24.4,-14.8714226890816));
#142566=CARTESIAN_POINT('Ctrl Pts',(-11.7855684683526,-24.4,-14.8517298003428));
#142567=CARTESIAN_POINT('Ctrl Pts',(-11.8602532900974,-24.4,-14.9205935851638));
#142568=CARTESIAN_POINT('Ctrl Pts',(-11.9349381118421,-24.4,-14.9894573699849));
#142569=CARTESIAN_POINT('Ctrl Pts',(-11.92337928256,-24.4,-15.0903852498028));
#142570=CARTESIAN_POINT('',(-11.92337928256,-24.4,-15.0903852498028));
#142571=CARTESIAN_POINT('',(-12.3207815844978,-24.,-15.1358979998248));
#142572=CARTESIAN_POINT('Origin',(-11.92337928256,-24.,-15.0903852498028));
#142573=CARTESIAN_POINT('Origin',(-11.7246781315911,-24.,-15.0676288747919));
#142574=CARTESIAN_POINT('Origin',(-11.7246781315911,-24.4,-15.0676288747919));
#142575=CARTESIAN_POINT('Origin',(-15.5,-24.,-15.5));
#142576=CARTESIAN_POINT('',(-12.1532274611957,-24.4,-16.8263157895108));
#142577=CARTESIAN_POINT('',(-12.5250910766184,-24.,-16.6789473684541));
#142578=CARTESIAN_POINT('Origin',(-12.1532274611957,-24.,-16.8263157895108));
#142579=CARTESIAN_POINT('Origin',(-15.5,-24.,-15.5));
#142580=CARTESIAN_POINT('Origin',(-15.5,-24.4,-15.5));
#142581=CARTESIAN_POINT('Ctrl Pts',(-12.5250910766184,-24.,-16.6789473684541));
#142582=CARTESIAN_POINT('Ctrl Pts',(-12.642154986228,-24.,-16.9743417843728));
#142583=CARTESIAN_POINT('Ctrl Pts',(-12.4635977686071,-24.,-17.2371708922063));
#142584=CARTESIAN_POINT('Ctrl Pts',(-12.2850405509867,-24.,-17.5000000000395));
#142585=CARTESIAN_POINT('Ctrl Pts',(-11.9672956534844,-24.,-17.5000000000392));
#142586=CARTESIAN_POINT('Ctrl Pts',(-12.5250910766184,-24.4,-16.6789473684541));
#142587=CARTESIAN_POINT('Ctrl Pts',(-12.642154986228,-24.4,-16.9743417843728));
#142588=CARTESIAN_POINT('Ctrl Pts',(-12.4635977686071,-24.4,-17.2371708922063));
#142589=CARTESIAN_POINT('Ctrl Pts',(-12.2850405509867,-24.4,-17.5000000000395));
#142590=CARTESIAN_POINT('Ctrl Pts',(-11.9672956534844,-24.4,-17.5000000000392));
#142591=CARTESIAN_POINT('Ctrl Pts',(-12.1532274611957,-24.4,-16.8263157895108));
#142592=CARTESIAN_POINT('Ctrl Pts',(-12.1922487643989,-24.4,-16.9247805948171));
#142593=CARTESIAN_POINT('Ctrl Pts',(-12.1327296918586,-24.4,-17.0123902974282));
#142594=CARTESIAN_POINT('Ctrl Pts',(-12.0732106193185,-24.4,-17.1000000000393));
#142595=CARTESIAN_POINT('Ctrl Pts',(-11.9672956534844,-24.4,-17.1000000000392));
#142596=CARTESIAN_POINT('',(-11.9672956534841,-24.4,-17.1000000000392));
#142597=CARTESIAN_POINT('',(-11.9672956534834,-24.,-17.5000000000392));
#142598=CARTESIAN_POINT('Origin',(-11.9672956534841,-24.,-17.1000000000392));
#142599=CARTESIAN_POINT('Origin',(-11.9672956534844,-24.,-16.9000000000392));
#142600=CARTESIAN_POINT('Origin',(-11.9672956534844,-24.4,-16.9000000000392));
#142601=CARTESIAN_POINT('Origin',(-11.8235138411924,-24.,-17.1000000000389));
#142602=CARTESIAN_POINT('',(-9.35435462095199,-24.,-17.5000000000348));
#142603=CARTESIAN_POINT('',(-11.8235138411917,-24.,-17.5000000000389));
#142604=CARTESIAN_POINT('',(-9.75435462095199,-24.4,-17.1000000000355));
#142605=CARTESIAN_POINT('',(-11.8235138411924,-24.4,-17.1000000000389));
#142606=CARTESIAN_POINT('Origin',(-9.75435462095199,-24.,-17.1000000000355));
#142607=CARTESIAN_POINT('Origin',(-9.75435462095199,-24.,-15.8999999999905));
#142608=CARTESIAN_POINT('',(-9.75435462095199,-24.4,-15.8999999999905));
#142609=CARTESIAN_POINT('',(-9.35459848714994,-23.9860345609578,-14.6999990924797));
#142610=CARTESIAN_POINT('Ctrl Pts',(-9.35459848714994,-23.9860345609578,
-14.6999990924797));
#142611=CARTESIAN_POINT('Ctrl Pts',(-9.35443500229638,-23.9907142615241,
-14.6999991570104));
#142612=CARTESIAN_POINT('Ctrl Pts',(-9.35435462095199,-23.9953714378489,
-14.6999991861862));
#142613=CARTESIAN_POINT('Ctrl Pts',(-9.35435462095199,-24.,-14.6999991861862));
#142614=CARTESIAN_POINT('',(-9.35459848714835,-23.986034560926,-17.5000000000348));
#142615=CARTESIAN_POINT('',(-9.35459848715105,-23.9860345609261,-15.8999999999905));
#142616=CARTESIAN_POINT('Origin',(-9.75435462095199,-24.,-17.5000000000409));
#142617=CARTESIAN_POINT('Origin',(-11.9672956534844,-10.3,-16.9000000000392));
#142618=CARTESIAN_POINT('',(-11.9672956534834,-10.3,-17.5000000000392));
#142619=CARTESIAN_POINT('',(-11.9672956534834,-10.3,-17.5000000000392));
#142620=CARTESIAN_POINT('',(-12.5250910766184,-10.3,-16.6789473684541));
#142621=CARTESIAN_POINT('Origin',(-11.9672956534844,-10.3,-16.9000000000392));
#142622=CARTESIAN_POINT('',(-12.5250910766184,-10.3,-16.6789473684541));
#142623=CARTESIAN_POINT('Origin',(-13.0020008006734,-10.3,-17.5000000000409));
#142624=CARTESIAN_POINT('',(-3.59005376343034,-20.7879235316574,-17.5000000000251));
#142625=CARTESIAN_POINT('Origin',(-5.65685424948968,-23.8568542494924,-17.5000000000285));
#142626=CARTESIAN_POINT('',(-3.59005376342686,-18.4674209709515,-17.5000000000251));
#142627=CARTESIAN_POINT('',(-3.59005376342686,-10.3,-17.5000000000251));
#142628=CARTESIAN_POINT('',(-1.39005376342686,-14.8791942943342,-17.5000000000433));
#142629=CARTESIAN_POINT('Origin',(-1.26287869055635E-16,-18.2,-17.5000000000409));
#142630=CARTESIAN_POINT('',(-1.39005376342686,-10.3,-17.5000000000213));
#142631=CARTESIAN_POINT('',(-1.39005376342686,-10.3,-17.5000000000213));
#142632=CARTESIAN_POINT('',(-2.22490186899551,-10.3,-17.5000000000227));
#142633=CARTESIAN_POINT('',(-0.170697831157441,-10.3,-17.5000000000193));
#142634=CARTESIAN_POINT('',(-9.08880662998386,-10.3,-17.5000000000343));
#142635=CARTESIAN_POINT('Origin',(-5.65685424948968,-12.5431457505076,-17.5000000000285));
#142636=CARTESIAN_POINT('',(-0.170697831157441,-10.3,-17.5000000000193));
#142637=CARTESIAN_POINT('Origin',(-5.65685424949238,-23.8568542494924,-15.8999999999905));
#142638=CARTESIAN_POINT('',(-3.59005376343416,-20.7879235316642,-13.1764761567201));
#142639=CARTESIAN_POINT('Ctrl Pts',(-9.35459848714994,-23.9860345609578,
-14.6999990924797));
#142640=CARTESIAN_POINT('Ctrl Pts',(-9.35676177374305,-23.9241111885544,
-14.6999982385873));
#142641=CARTESIAN_POINT('Ctrl Pts',(-9.35737145099148,-23.8620802493589,
-14.6999977069853));
#142642=CARTESIAN_POINT('Ctrl Pts',(-9.35641741186418,-23.799999982972,
-14.6999982325186));
#142643=CARTESIAN_POINT('Ctrl Pts',(-9.34952807250257,-23.3517038800543,
-14.7000020275173));
#142644=CARTESIAN_POINT('Ctrl Pts',(-9.25618380964402,-22.8776101099329,
-14.7010327279702));
#142645=CARTESIAN_POINT('Ctrl Pts',(-8.8860287285298,-21.9844435897398,
-14.6922910406182));
#142646=CARTESIAN_POINT('Ctrl Pts',(-8.60117160618611,-21.5685814254056,
-14.6805753032666));
#142647=CARTESIAN_POINT('Ctrl Pts',(-7.93807194307344,-20.905481762293,
-14.6190191278397));
#142648=CARTESIAN_POINT('Ctrl Pts',(-7.51415814075371,-20.6187964801274,
-14.5639150424745));
#142649=CARTESIAN_POINT('Ctrl Pts',(-6.59851020504296,-20.2446694117715,
-14.3800423269859));
#142650=CARTESIAN_POINT('Ctrl Pts',(-6.10725151442864,-20.1568542494924,
-14.2496697959988));
#142651=CARTESIAN_POINT('Ctrl Pts',(-5.16315899376981,-20.1568542494924,
-13.9341089601114));
#142652=CARTESIAN_POINT('Ctrl Pts',(-4.65119667500065,-20.2605684182922,
-13.7228927256965));
#142653=CARTESIAN_POINT('Ctrl Pts',(-3.97775061505936,-20.5518405627531,
-13.3900421583534));
#142654=CARTESIAN_POINT('Ctrl Pts',(-3.77693263646862,-20.6620681829664,
-13.2827729814766));
#142655=CARTESIAN_POINT('Ctrl Pts',(-3.59005376343416,-20.7879235316642,
-13.1764761567201));
#142656=CARTESIAN_POINT('',(-3.59005376342956,-20.7879235316673,-15.8999999999905));
#142657=CARTESIAN_POINT('Origin',(-10.6450268817134,-24.4,-15.5));
#142658=CARTESIAN_POINT('Origin',(-9.35,-10.3,-3.05000000003699));
#142659=CARTESIAN_POINT('',(-11.6083673659622,-10.3,-14.479010317661));
#142660=CARTESIAN_POINT('',(-11.6083673659622,-10.3,-14.479010317661));
#142661=CARTESIAN_POINT('',(-9.15685424949238,-10.3,-14.6983988049827));
#142662=CARTESIAN_POINT('Origin',(-9.35,-10.3,-3.05000000003699));
#142663=CARTESIAN_POINT('',(-8.15685424949238,-11.3,-14.6387403637713));
#142664=CARTESIAN_POINT('Ctrl Pts',(-8.15685424949238,-11.3,-14.6387403637713));
#142665=CARTESIAN_POINT('Ctrl Pts',(-8.15685424949238,-11.1743649985927,
-14.6387403637713));
#142666=CARTESIAN_POINT('Ctrl Pts',(-8.18197680776031,-11.0404139596789,
-14.641412739057));
#142667=CARTESIAN_POINT('Ctrl Pts',(-8.28402198897147,-10.7941000141912,
-14.6512421030957));
#142668=CARTESIAN_POINT('Ctrl Pts',(-8.36093991003168,-10.6817304364779,
-14.6582803730457));
#142669=CARTESIAN_POINT('Ctrl Pts',(-8.53837619979829,-10.5042348482132,
-14.6720346815212));
#142670=CARTESIAN_POINT('Ctrl Pts',(-8.65077495464815,-10.427264453842,
-14.6796516718487));
#142671=CARTESIAN_POINT('Ctrl Pts',(-8.89716064669893,-10.3251447177429,
-14.6918490881968));
#142672=CARTESIAN_POINT('Ctrl Pts',(-9.03115517829841,-10.3,-14.6963145492965));
#142673=CARTESIAN_POINT('Ctrl Pts',(-9.15685424949238,-10.3,-14.6983988049827));
#142674=CARTESIAN_POINT('',(-8.15685424949238,-12.5431457505076,-14.6387403637713));
#142675=CARTESIAN_POINT('',(-8.15685424949238,-10.3,-14.6387403637713));
#142676=CARTESIAN_POINT('',(-3.15685424949238,-12.5431457505076,-12.9174943989697));
#142677=CARTESIAN_POINT('Ctrl Pts',(-8.15685424949238,-12.5431457505076,
-14.6387403637713));
#142678=CARTESIAN_POINT('Ctrl Pts',(-8.15685424949238,-12.8564022173972,
-14.6387403637713));
#142679=CARTESIAN_POINT('Ctrl Pts',(-8.09433479998511,-13.190466093178,
-14.6328369794813));
#142680=CARTESIAN_POINT('Ctrl Pts',(-7.84073632742103,-13.8044918157331,
-14.6025292016044));
#142681=CARTESIAN_POINT('Ctrl Pts',(-7.64965844750753,-14.0844177261518,
-14.5773916287323));
#142682=CARTESIAN_POINT('Ctrl Pts',(-7.20376387556559,-14.5332382695204,
-14.5029020140874));
#142683=CARTESIAN_POINT('Ctrl Pts',(-6.91723165226354,-14.7280486885119,
-14.4476267125339));
#142684=CARTESIAN_POINT('Ctrl Pts',(-6.29717897630526,-14.9828867355091,
-14.2974237235192));
#142685=CARTESIAN_POINT('Ctrl Pts',(-5.96393092697842,-15.0431457505076,
-14.2017652067917));
#142686=CARTESIAN_POINT('Ctrl Pts',(-5.33066040655443,-15.0431457505076,
-13.9900959366778));
#142687=CARTESIAN_POINT('Ctrl Pts',(-4.98833212718866,-14.9759248056554,
-13.8580828066145));
#142688=CARTESIAN_POINT('Ctrl Pts',(-4.363575736342,-14.7094251062448,-13.5844375087381));
#142689=CARTESIAN_POINT('Ctrl Pts',(-4.08079555119357,-14.5103803575851,
-13.4433817276104));
#142690=CARTESIAN_POINT('Ctrl Pts',(-3.65133920193737,-14.064895460083,
-13.2137667708102));
#142691=CARTESIAN_POINT('Ctrl Pts',(-3.46785847818632,-13.7938980371273,
-13.1070248812659));
#142692=CARTESIAN_POINT('Ctrl Pts',(-3.22046675563909,-13.1912956863282,
-12.9581865955658));
#142693=CARTESIAN_POINT('Ctrl Pts',(-3.15685424949238,-12.8592223348356,
-12.9174943989697));
#142694=CARTESIAN_POINT('Ctrl Pts',(-3.15685424949238,-12.5431457505076,
-12.9174943989697));
#142695=CARTESIAN_POINT('',(-3.15685424949238,-11.3,-12.9174943989697));
#142696=CARTESIAN_POINT('',(-3.15685424949238,-10.3,-12.9174943989697));
#142697=CARTESIAN_POINT('',(-2.15685424949238,-10.3,-12.2141232102494));
#142698=CARTESIAN_POINT('Ctrl Pts',(-2.15685424949238,-10.3,-12.2141232102494));
#142699=CARTESIAN_POINT('Ctrl Pts',(-2.28026220008018,-10.3,-12.3109891465738));
#142700=CARTESIAN_POINT('Ctrl Pts',(-2.41580651903231,-10.3241114437069,
-12.4129327889492));
#142701=CARTESIAN_POINT('Ctrl Pts',(-2.67271826515926,-10.4320719373805,
-12.5978509719696));
#142702=CARTESIAN_POINT('Ctrl Pts',(-2.79395836511785,-10.5160800083143,
-12.680909505094));
#142703=CARTESIAN_POINT('Ctrl Pts',(-2.96758654966608,-10.7038187238232,
-12.7965770599196));
#142704=CARTESIAN_POINT('Ctrl Pts',(-3.03762609498192,-10.8096646825789,
-12.8418124725612));
#142705=CARTESIAN_POINT('Ctrl Pts',(-3.13234930878862,-11.0458400668001,
-12.9022320096932));
#142706=CARTESIAN_POINT('Ctrl Pts',(-3.15685424949238,-11.1762211096894,
-12.9174943989697));
#142707=CARTESIAN_POINT('Ctrl Pts',(-3.15685424949238,-11.3,-12.9174943989697));
#142708=CARTESIAN_POINT('',(-1.77992868114481,-10.3,-11.9053102841234));
#142709=CARTESIAN_POINT('Origin',(-9.35,-10.3,-3.05000000003699));
#142710=CARTESIAN_POINT('',(-1.77992868114481,-15.0708061916784,-11.9053102841234));
#142711=CARTESIAN_POINT('',(-1.77992868114481,-10.3,-11.9053102841234));
#142712=CARTESIAN_POINT('',(-3.59005376343415,-18.4674209708535,-13.1764761567201));
#142713=CARTESIAN_POINT('Ctrl Pts',(-3.59005376343416,-18.4674209708535,
-13.1764761567201));
#142714=CARTESIAN_POINT('Ctrl Pts',(-3.59678968275853,-18.3769930868941,
-13.1803075520211));
#142715=CARTESIAN_POINT('Ctrl Pts',(-3.6,-18.2875463035025,-13.1821271212293));
#142716=CARTESIAN_POINT('Ctrl Pts',(-3.6,-17.8815466224465,-13.1821271212293));
#142717=CARTESIAN_POINT('Ctrl Pts',(-3.55476999791657,-17.5382077727571,
-13.1568963520113));
#142718=CARTESIAN_POINT('Ctrl Pts',(-3.36933995170902,-16.8877857922236,
-13.0482873955818));
#142719=CARTESIAN_POINT('Ctrl Pts',(-3.22941756244032,-16.5807035365666,
-12.964430626659));
#142720=CARTESIAN_POINT('Ctrl Pts',(-2.88197413954814,-16.0120984149223,
-12.7421606660272));
#142721=CARTESIAN_POINT('Ctrl Pts',(-2.63436410033982,-15.720213086085,
-12.5756271636011));
#142722=CARTESIAN_POINT('Ctrl Pts',(-2.17431453454083,-15.3198884370908,
-12.2308360831179));
#142723=CARTESIAN_POINT('Ctrl Pts',(-1.97456413725502,-15.1815175288212,
-12.0716968066352));
#142724=CARTESIAN_POINT('Ctrl Pts',(-1.77992868114481,-15.0708061916784,
-11.9053102841234));
#142725=CARTESIAN_POINT('',(-3.59005376343416,-10.3,-13.1764761567201));
#142726=CARTESIAN_POINT('Origin',(-14.5000000000146,-24.,0.715147871306033));
#142727=CARTESIAN_POINT('',(-14.9000000000115,-24.,2.37724133593659));
#142728=CARTESIAN_POINT('',(-14.5000000000115,-24.4,2.37724133593584));
#142729=CARTESIAN_POINT('Origin',(-14.5000000000115,-24.,2.37724133593584));
#142730=CARTESIAN_POINT('',(-14.5000000000318,-24.4,-8.3813708499249));
#142731=CARTESIAN_POINT('',(-14.5000000000146,-24.4,0.715147871306033));
#142732=CARTESIAN_POINT('',(-14.9000000000318,-24.,-8.38137084992414));
#142733=CARTESIAN_POINT('Origin',(-14.5000000000318,-24.,-8.3813708499249));
#142734=CARTESIAN_POINT('',(-14.9000000000146,-24.,0.715147871306786));
#142735=CARTESIAN_POINT('Origin',(-15.7000000000318,-24.,-8.38137084992264));
#142736=CARTESIAN_POINT('',(-14.8514718626079,-24.4,-9.2298989873465));
#142737=CARTESIAN_POINT('',(-15.1343145750825,-24.,-8.94705627487188));
#142738=CARTESIAN_POINT('Origin',(-14.8514718626079,-24.,-9.2298989873465));
#142739=CARTESIAN_POINT('Origin',(-15.7000000000318,-24.,-8.38137084992264));
#142740=CARTESIAN_POINT('Origin',(-15.7000000000318,-24.4,-8.38137084992264));
#142741=CARTESIAN_POINT('Origin',(-10.3394102592575,-24.,-4.71783738399612));
#142742=CARTESIAN_POINT('',(-15.0728809663607,-24.4,-9.45130809109928));
#142743=CARTESIAN_POINT('',(-15.3557236788353,-24.,-9.16846537862467));
#142744=CARTESIAN_POINT('Origin',(-15.0728809663607,-24.,-9.45130809109928));
#142745=CARTESIAN_POINT('',(-10.6222529717321,-24.,-4.4349946715215));
#142746=CARTESIAN_POINT('',(-10.3394102592575,-24.4,-4.71783738399612));
#142747=CARTESIAN_POINT('Ctrl Pts',(-15.3557236788353,-24.,-9.16846537862466));
#142748=CARTESIAN_POINT('Ctrl Pts',(-15.54137387769,-24.,-9.35411557747933));
#142749=CARTESIAN_POINT('Ctrl Pts',(-15.5309901758822,-24.,-9.61645919071648));
#142750=CARTESIAN_POINT('Ctrl Pts',(-15.5206064740745,-24.,-9.87880280395362));
#142751=CARTESIAN_POINT('Ctrl Pts',(-15.3208637689692,-24.,-10.0491989436598));
#142752=CARTESIAN_POINT('Ctrl Pts',(-15.3557236788353,-24.4,-9.16846537862466));
#142753=CARTESIAN_POINT('Ctrl Pts',(-15.54137387769,-24.4,-9.35411557747933));
#142754=CARTESIAN_POINT('Ctrl Pts',(-15.5309901758822,-24.4,-9.61645919071648));
#142755=CARTESIAN_POINT('Ctrl Pts',(-15.5206064740745,-24.4,-9.87880280395362));
#142756=CARTESIAN_POINT('Ctrl Pts',(-15.3208637689692,-24.4,-10.0491989436598));
#142757=CARTESIAN_POINT('Ctrl Pts',(-15.0728809663607,-24.4,-9.45130809109929));
#142758=CARTESIAN_POINT('Ctrl Pts',(-15.1347643659789,-24.4,-9.51319149071751));
#142759=CARTESIAN_POINT('Ctrl Pts',(-15.131303132043,-24.4,-9.60063936179656));
#142760=CARTESIAN_POINT('Ctrl Pts',(-15.1278418981071,-24.4,-9.68808723287561));
#142761=CARTESIAN_POINT('Ctrl Pts',(-15.0612609964053,-24.4,-9.74488594611101));
#142762=CARTESIAN_POINT('',(-15.0612609964053,-24.4,-9.74488594611101));
#142763=CARTESIAN_POINT('',(-15.3208637689692,-24.,-10.0491989436598));
#142764=CARTESIAN_POINT('Origin',(-15.0612609964053,-24.,-9.74488594611101));
#142765=CARTESIAN_POINT('Origin',(-14.9314596101234,-24.,-9.5927294473366));
#142766=CARTESIAN_POINT('Origin',(-14.9314596101234,-24.4,-9.5927294473366));
#142767=CARTESIAN_POINT('Origin',(-9.35,-24.,-3.05000000003699));
#142768=CARTESIAN_POINT('',(-14.7703541221629,-24.4,-9.98251478115012));
#142769=CARTESIAN_POINT('',(-15.0167338549885,-24.,-10.2976290893825));
#142770=CARTESIAN_POINT('Origin',(-14.7703541221629,-24.,-9.98251478115012));
#142771=CARTESIAN_POINT('Origin',(-9.35,-24.,-3.05000000003699));
#142772=CARTESIAN_POINT('Origin',(-9.35,-24.4,-3.05000000003699));
#142773=CARTESIAN_POINT('Ctrl Pts',(-15.0167338549885,-24.,-10.2976290893825));
#142774=CARTESIAN_POINT('Ctrl Pts',(-14.8012729185294,-24.,-10.4660924265662));
#142775=CARTESIAN_POINT('Ctrl Pts',(-14.5327864509729,-24.,-10.4139548407577));
#142776=CARTESIAN_POINT('Ctrl Pts',(-14.2642999834165,-24.,-10.3618172549492));
#142777=CARTESIAN_POINT('Ctrl Pts',(-14.1275490134794,-24.,-10.1249576270339));
#142778=CARTESIAN_POINT('Ctrl Pts',(-15.0167338549885,-24.4,-10.2976290893825));
#142779=CARTESIAN_POINT('Ctrl Pts',(-14.8012729185294,-24.4,-10.4660924265662));
#142780=CARTESIAN_POINT('Ctrl Pts',(-14.5327864509729,-24.4,-10.4139548407577));
#142781=CARTESIAN_POINT('Ctrl Pts',(-14.2642999834165,-24.4,-10.3618172549492));
#142782=CARTESIAN_POINT('Ctrl Pts',(-14.1275490134794,-24.4,-10.1249576270339));
#142783=CARTESIAN_POINT('Ctrl Pts',(-14.7703541221629,-24.4,-9.98251478115011));
#142784=CARTESIAN_POINT('Ctrl Pts',(-14.6985338100098,-24.4,-10.038669226878));
#142785=CARTESIAN_POINT('Ctrl Pts',(-14.6090383208244,-24.4,-10.0212900316085));
#142786=CARTESIAN_POINT('Ctrl Pts',(-14.5195428316389,-24.4,-10.003910836339));
#142787=CARTESIAN_POINT('Ctrl Pts',(-14.4739591749932,-24.4,-9.92495762703391));
#142788=CARTESIAN_POINT('',(-14.4739591749932,-24.4,-9.92495762703391));
#142789=CARTESIAN_POINT('',(-14.1275490134794,-24.,-10.1249576270339));
#142790=CARTESIAN_POINT('Origin',(-14.4739591749932,-24.,-9.92495762703391));
#142791=CARTESIAN_POINT('Origin',(-14.6471642557501,-24.,-9.82495762703391));
#142792=CARTESIAN_POINT('Origin',(-14.6471642557501,-24.4,-9.82495762703391));
#142793=CARTESIAN_POINT('Origin',(-11.8202184969051,-24.,-5.32854394247302));
#142794=CARTESIAN_POINT('',(-12.1762549821757,-24.4,-5.94521722430999));
#142795=CARTESIAN_POINT('',(-11.8298448206619,-24.,-6.14521722430999));
#142796=CARTESIAN_POINT('Origin',(-12.1762549821757,-24.,-5.94521722430999));
#142797=CARTESIAN_POINT('',(-11.4738083353913,-24.,-5.52854394247302));
#142798=CARTESIAN_POINT('',(-11.8202184969051,-24.4,-5.32854394247302));
#142799=CARTESIAN_POINT('Ctrl Pts',(-11.8298448206619,-24.,-6.14521722430999));
#142800=CARTESIAN_POINT('Ctrl Pts',(-11.6079320382025,-24.,-5.76085301024134));
#142801=CARTESIAN_POINT('Ctrl Pts',(-11.9105146878693,-24.,-5.43616104514808));
#142802=CARTESIAN_POINT('Ctrl Pts',(-11.8298448206619,-24.4,-6.14521722430999));
#142803=CARTESIAN_POINT('Ctrl Pts',(-11.6079320382025,-24.4,-5.76085301024134));
#142804=CARTESIAN_POINT('Ctrl Pts',(-11.9105146878693,-24.4,-5.43616104514808));
#142805=CARTESIAN_POINT('Ctrl Pts',(-12.1762549821757,-24.4,-5.94521722430999));
#142806=CARTESIAN_POINT('Ctrl Pts',(-12.1022840546892,-24.4,-5.81709581962044));
#142807=CARTESIAN_POINT('Ctrl Pts',(-12.2031449379115,-24.4,-5.70886516458935));
#142808=CARTESIAN_POINT('',(-12.2031449379115,-24.4,-5.70886516458935));
#142809=CARTESIAN_POINT('',(-11.9105146878693,-24.,-5.43616104514808));
#142810=CARTESIAN_POINT('Origin',(-12.2031449379115,-24.,-5.70886516458935));
#142811=CARTESIAN_POINT('Origin',(-12.3494600629326,-24.,-5.84521722430999));
#142812=CARTESIAN_POINT('Origin',(-12.3494600629326,-24.4,-5.84521722430999));
#142813=CARTESIAN_POINT('Origin',(-9.35,-24.,-3.05000000003699));
#142814=CARTESIAN_POINT('',(-12.2031449379115,-24.4,-0.391134835484633));
#142815=CARTESIAN_POINT('',(-11.9105146878693,-24.,-0.663838954925902));
#142816=CARTESIAN_POINT('Origin',(-12.2031449379115,-24.,-0.391134835484633));
#142817=CARTESIAN_POINT('',(-12.85,-24.,-3.05000000003699));
#142818=CARTESIAN_POINT('Origin',(-9.35,-24.,-3.05000000003699));
#142819=CARTESIAN_POINT('Origin',(-9.35,-24.,-3.05000000003699));
#142820=CARTESIAN_POINT('Origin',(-9.35,-24.4,-3.05000000003699));
#142821=CARTESIAN_POINT('Ctrl Pts',(-11.9105146878693,-24.,-0.663838954925902));
#142822=CARTESIAN_POINT('Ctrl Pts',(-11.6079320382025,-24.,-0.339146989832641));
#142823=CARTESIAN_POINT('Ctrl Pts',(-11.8298448206619,-24.,0.0452172242359999));
#142824=CARTESIAN_POINT('Ctrl Pts',(-11.9105146878693,-24.4,-0.663838954925903));
#142825=CARTESIAN_POINT('Ctrl Pts',(-11.6079320382025,-24.4,-0.339146989832641));
#142826=CARTESIAN_POINT('Ctrl Pts',(-11.8298448206619,-24.4,0.0452172242359998));
#142827=CARTESIAN_POINT('Ctrl Pts',(-12.2031449379115,-24.4,-0.391134835484634));
#142828=CARTESIAN_POINT('Ctrl Pts',(-12.1022840546892,-24.4,-0.282904180453547));
#142829=CARTESIAN_POINT('Ctrl Pts',(-12.1762549821757,-24.4,-0.154782775764001));
#142830=CARTESIAN_POINT('',(-12.1762549821757,-24.4,-0.154782775764));
#142831=CARTESIAN_POINT('',(-11.8298448206619,-24.,0.0452172242359991));
#142832=CARTESIAN_POINT('Origin',(-12.1762549821757,-24.,-0.154782775764));
#142833=CARTESIAN_POINT('Origin',(-12.3494600629326,-24.,-0.254782775764));
#142834=CARTESIAN_POINT('Origin',(-12.3494600629326,-24.4,-0.254782775764001));
#142835=CARTESIAN_POINT('Origin',(-10.3305808539815,-24.,-3.35158414001175));
#142836=CARTESIAN_POINT('',(-13.7535898384977,-24.4,2.57724133593509));
#142837=CARTESIAN_POINT('',(-13.4071796769839,-24.,2.77724133593509));
#142838=CARTESIAN_POINT('Origin',(-13.7535898384977,-24.,2.57724133593509));
#142839=CARTESIAN_POINT('',(-9.98417069246773,-24.,-3.15158414001175));
#142840=CARTESIAN_POINT('',(-10.3305808539815,-24.4,-3.35158414001175));
#142841=CARTESIAN_POINT('Ctrl Pts',(-13.4071796769839,-24.,2.77724133593509));
#142842=CARTESIAN_POINT('Ctrl Pts',(-13.7141104721752,-24.,3.30886106761391));
#142843=CARTESIAN_POINT('Ctrl Pts',(-14.3070552360928,-24.,3.14998199696654));
#142844=CARTESIAN_POINT('Ctrl Pts',(-14.9000000000103,-24.,2.99110292631917));
#142845=CARTESIAN_POINT('Ctrl Pts',(-14.9000000000115,-24.,2.37724133593659));
#142846=CARTESIAN_POINT('Ctrl Pts',(-13.4071796769839,-24.4,2.77724133593509));
#142847=CARTESIAN_POINT('Ctrl Pts',(-13.7141104721752,-24.4,3.30886106761391));
#142848=CARTESIAN_POINT('Ctrl Pts',(-14.3070552360928,-24.4,3.14998199696654));
#142849=CARTESIAN_POINT('Ctrl Pts',(-14.9000000000103,-24.4,2.99110292631917));
#142850=CARTESIAN_POINT('Ctrl Pts',(-14.9000000000115,-24.4,2.37724133593659));
#142851=CARTESIAN_POINT('Ctrl Pts',(-13.7535898384977,-24.4,2.57724133593509));
#142852=CARTESIAN_POINT('Ctrl Pts',(-13.9070552360934,-24.4,2.8430512017745));
#142853=CARTESIAN_POINT('Ctrl Pts',(-14.2035276180521,-24.4,2.76361166645081));
#142854=CARTESIAN_POINT('Ctrl Pts',(-14.5000000000109,-24.4,2.68417213112713));
#142855=CARTESIAN_POINT('Ctrl Pts',(-14.5000000000115,-24.4,2.37724133593584));
#142856=CARTESIAN_POINT('Origin',(-14.1000000000115,-24.,2.37724133593509));
#142857=CARTESIAN_POINT('Origin',(-14.1000000000115,-24.4,2.37724133593509));
#142858=CARTESIAN_POINT('Origin',(-12.3494600629326,-21.1,-5.84521722430998));
#142859=CARTESIAN_POINT('',(-11.9105146878693,-20.,-5.43616104514808));
#142860=CARTESIAN_POINT('',(-11.9105146878693,-21.1,-5.43616104514808));
#142861=CARTESIAN_POINT('',(-11.8298448206619,-20.,-6.14521722430999));
#142862=CARTESIAN_POINT('Origin',(-12.3494600629326,-20.,-5.84521722430998));
#142863=CARTESIAN_POINT('',(-11.8298448206619,-21.1,-6.14521722430999));
#142864=CARTESIAN_POINT('Origin',(-9.35,-21.1,-3.05000000003699));
#142865=CARTESIAN_POINT('',(-12.85,-19.7,-3.05000000003699));
#142866=CARTESIAN_POINT('Origin',(-9.35,-19.7,-3.05000000003699));
#142867=CARTESIAN_POINT('',(-12.85,-21.1,-3.05000000003699));
#142868=CARTESIAN_POINT('',(-11.9105146878693,-20.,-0.663838954925901));
#142869=CARTESIAN_POINT('',(-11.9105146878693,-21.1,-0.663838954925901));
#142870=CARTESIAN_POINT('',(-10.1362187386524,-20.,0.360551288976537));
#142871=CARTESIAN_POINT('Origin',(-9.35,-20.,-3.05000000003699));
#142872=CARTESIAN_POINT('',(-10.1362187386524,-24.,0.360551288976536));
#142873=CARTESIAN_POINT('',(-10.1362187386524,-21.1,0.360551288976537));
#142874=CARTESIAN_POINT('',(-6.00326657347833,-24.,-2.02560975613455));
#142875=CARTESIAN_POINT('Origin',(-9.35,-24.,-3.05000000003699));
#142876=CARTESIAN_POINT('',(-6.00326657347833,-20.,-2.02560975613455));
#142877=CARTESIAN_POINT('',(-6.00326657347833,-21.1,-2.02560975613455));
#142878=CARTESIAN_POINT('',(-6.00326657347833,-20.,-4.07439024393943));
#142879=CARTESIAN_POINT('Origin',(-9.35,-20.,-3.05000000003699));
#142880=CARTESIAN_POINT('',(-6.00326657347833,-24.,-4.07439024393943));
#142881=CARTESIAN_POINT('',(-6.00326657347833,-21.1,-4.07439024393943));
#142882=CARTESIAN_POINT('',(-10.1362187386524,-24.,-6.46055128905052));
#142883=CARTESIAN_POINT('Origin',(-9.35,-24.,-3.05000000003699));
#142884=CARTESIAN_POINT('',(-10.1362187386524,-20.,-6.46055128905052));
#142885=CARTESIAN_POINT('',(-10.1362187386524,-21.1,-6.46055128905052));
#142886=CARTESIAN_POINT('Origin',(-9.35,-20.,-3.05000000003699));
#142887=CARTESIAN_POINT('Origin',(-12.3494600629326,-21.1,-0.254782775764));
#142888=CARTESIAN_POINT('',(-11.8298448206619,-20.,0.0452172242360003));
#142889=CARTESIAN_POINT('',(-11.8298448206619,-21.1,0.0452172242359998));
#142890=CARTESIAN_POINT('Origin',(-12.3494600629326,-20.,-0.254782775764));
#142891=CARTESIAN_POINT('Origin',(-11.5732877460107,-19.9,-0.399152664101091));
#142892=CARTESIAN_POINT('',(-13.4071796769839,-20.,2.77724133593509));
#142893=CARTESIAN_POINT('',(-13.4071796769839,-19.9,2.77724133593509));
#142894=CARTESIAN_POINT('',(-10.9972459287083,-20.,-1.39688635895322));
#142895=CARTESIAN_POINT('Origin',(-14.1000000000115,-19.9,2.37724133593509));
#142896=CARTESIAN_POINT('',(-14.9000000000115,-20.,2.3772413359366));
#142897=CARTESIAN_POINT('',(-14.9000000000115,-19.9,2.3772413359366));
#142898=CARTESIAN_POINT('Origin',(-14.1000000000115,-20.,2.37724133593509));
#142899=CARTESIAN_POINT('Origin',(-14.9000000000075,-22.8,4.48029574262901));
#142900=CARTESIAN_POINT('',(-14.9000000000318,-20.,-8.38137084992414));
#142901=CARTESIAN_POINT('',(-14.9000000000318,-22.8,-8.38137084992414));
#142902=CARTESIAN_POINT('',(-14.9000000000171,-20.,-0.58485212871229));
#142903=CARTESIAN_POINT('Origin',(-3.45175358661618,-24.4,-3.05000000003699));
#142904=CARTESIAN_POINT('Origin',(-9.35,-24.,-3.05000000003699));
#142905=CARTESIAN_POINT('',(-3.36628450305284,-24.4,-9.50253042240576));
#142906=CARTESIAN_POINT('',(-1.01046511708684,-24.4,-5.85929847771334));
#142907=CARTESIAN_POINT('Origin',(-9.35,-24.4,-3.05000000003699));
#142908=CARTESIAN_POINT('',(-0.631395349681702,-24.,-5.98699386306226));
#142909=CARTESIAN_POINT('Origin',(-1.01046511708684,-24.,-5.85929847771334));
#142910=CARTESIAN_POINT('',(-3.34165888869613,-24.,-10.0170536879467));
#142911=CARTESIAN_POINT('Origin',(-9.35,-24.,-3.05000000003699));
#142912=CARTESIAN_POINT('Ctrl Pts',(-3.36628450305284,-24.4,-9.50253042240576));
#142913=CARTESIAN_POINT('Ctrl Pts',(-3.36619187924502,-24.4,-9.50372689824024));
#142914=CARTESIAN_POINT('Ctrl Pts',(-3.36609949462665,-24.3999966844721,
-9.50492339449873));
#142915=CARTESIAN_POINT('Ctrl Pts',(-3.36298725258202,-24.3997727516819,
-9.54533619308514));
#142916=CARTESIAN_POINT('Ctrl Pts',(-3.36022413301821,-24.3959947528393,
-9.58462112336526));
#142917=CARTESIAN_POINT('Ctrl Pts',(-3.35282072422976,-24.3739050476839,
-9.7007017752616));
#142918=CARTESIAN_POINT('Ctrl Pts',(-3.34928303606659,-24.3452366730688,
-9.77290486275007));
#142919=CARTESIAN_POINT('Ctrl Pts',(-3.34497556527484,-24.2733286996026,
-9.88229757161595));
#142920=CARTESIAN_POINT('Ctrl Pts',(-3.3437149391037,-24.2334157755877,
-9.92518249065517));
#142921=CARTESIAN_POINT('Ctrl Pts',(-3.34228518261157,-24.1483727618738,
-9.98306784206126));
#142922=CARTESIAN_POINT('Ctrl Pts',(-3.34194048879486,-24.1068706951224,
-10.0015273168103));
#142923=CARTESIAN_POINT('Ctrl Pts',(-3.34169547356203,-24.0418361742419,
-10.0149184217387));
#142924=CARTESIAN_POINT('Ctrl Pts',(-3.34165888869613,-24.0209215876749,
-10.0170536879467));
#142925=CARTESIAN_POINT('Ctrl Pts',(-3.34165888869614,-23.9999999999998,
-10.0170536879467));
#142926=CARTESIAN_POINT('Ctrl Pts',(-0.631395349681701,-24.,-5.98699386306226));
#142927=CARTESIAN_POINT('Ctrl Pts',(-0.600000000789416,-24.,-5.89379529077492));
#142928=CARTESIAN_POINT('Ctrl Pts',(-0.600000000789416,-24.,-5.79545078503888));
#142929=CARTESIAN_POINT('Ctrl Pts',(-0.631395349681701,-24.4,-5.98699386306226));
#142930=CARTESIAN_POINT('Ctrl Pts',(-0.600000000789416,-24.4,-5.89379529077492));
#142931=CARTESIAN_POINT('Ctrl Pts',(-0.600000000789416,-24.4,-5.79545078503888));
#142932=CARTESIAN_POINT('Ctrl Pts',(-1.01046511708684,-24.4,-5.85929847771334));
#142933=CARTESIAN_POINT('Ctrl Pts',(-1.00000000078942,-24.4,-5.82823228695089));
#142934=CARTESIAN_POINT('Ctrl Pts',(-1.00000000078942,-24.4,-5.79545078503888));
#142935=CARTESIAN_POINT('',(-1.00000000078942,-24.4,-5.79545078503888));
#142936=CARTESIAN_POINT('',(-0.600000000789416,-24.,-5.79545078503888));
#142937=CARTESIAN_POINT('Origin',(-1.00000000078942,-24.,-5.79545078503888));
#142938=CARTESIAN_POINT('Origin',(-1.20000000078942,-24.,-5.79545078503888));
#142939=CARTESIAN_POINT('Origin',(-1.20000000078942,-24.4,-5.79545078503888));
#142940=CARTESIAN_POINT('Origin',(-1.00000000078942,-24.,-1.33262554947194));
#142941=CARTESIAN_POINT('',(-1.00000000078942,-24.4,-4.25000000003699));
#142942=CARTESIAN_POINT('',(-0.600000000789417,-24.,-4.25000000003699));
#142943=CARTESIAN_POINT('Origin',(-1.00000000078942,-24.,-4.25000000003699));
#142944=CARTESIAN_POINT('',(-0.600000000789417,-24.,-1.33262554947194));
#142945=CARTESIAN_POINT('',(-1.00000000078942,-24.4,-1.33262554947194));
#142946=CARTESIAN_POINT('Ctrl Pts',(-0.600000000789416,-24.,-4.25000000003699));
#142947=CARTESIAN_POINT('Ctrl Pts',(-0.600000000789416,-24.,-3.65000000003699));
#142948=CARTESIAN_POINT('Ctrl Pts',(-1.20000000078942,-24.,-3.65000000003699));
#142949=CARTESIAN_POINT('Ctrl Pts',(-0.600000000789416,-24.4,-4.25000000003699));
#142950=CARTESIAN_POINT('Ctrl Pts',(-0.600000000789416,-24.4,-3.65000000003699));
#142951=CARTESIAN_POINT('Ctrl Pts',(-1.20000000078942,-24.4,-3.65000000003699));
#142952=CARTESIAN_POINT('Ctrl Pts',(-1.00000000078942,-24.4,-4.25000000003699));
#142953=CARTESIAN_POINT('Ctrl Pts',(-1.00000000078942,-24.4,-4.05000000003699));
#142954=CARTESIAN_POINT('Ctrl Pts',(-1.20000000078942,-24.4,-4.05000000003699));
#142955=CARTESIAN_POINT('',(-1.20000000078942,-24.4,-4.05000000003699));
#142956=CARTESIAN_POINT('',(-1.20000000078942,-24.,-3.65000000003699));
#142957=CARTESIAN_POINT('Origin',(-1.20000000078942,-24.,-4.05000000003699));
#142958=CARTESIAN_POINT('Origin',(-1.20000000078942,-24.,-4.25000000003699));
#142959=CARTESIAN_POINT('Origin',(-1.20000000078942,-24.4,-4.25000000003699));
#142960=CARTESIAN_POINT('Origin',(-1.71792900372085,-24.,-4.05000000003699));
#142961=CARTESIAN_POINT('',(-5.42954084321747,-24.4,-4.05000000003699));
#142962=CARTESIAN_POINT('',(-5.42954084321747,-24.,-3.65000000003699));
#142963=CARTESIAN_POINT('Origin',(-5.42954084321747,-24.,-4.05000000003699));
#142964=CARTESIAN_POINT('',(-1.71792900372085,-24.,-3.65000000003699));
#142965=CARTESIAN_POINT('',(-1.71792900372085,-24.4,-4.05000000003699));
#142966=CARTESIAN_POINT('Ctrl Pts',(-5.42954084321747,-24.,-3.65000000003699));
#142967=CARTESIAN_POINT('Ctrl Pts',(-5.87336640813625,-24.,-3.65000000003699));
#142968=CARTESIAN_POINT('Ctrl Pts',(-6.00326657347833,-24.,-4.07439024393943));
#142969=CARTESIAN_POINT('Ctrl Pts',(-5.42954084321747,-24.4,-3.65000000003699));
#142970=CARTESIAN_POINT('Ctrl Pts',(-5.87336640813625,-24.4,-3.65000000003699));
#142971=CARTESIAN_POINT('Ctrl Pts',(-6.00326657347833,-24.4,-4.07439024393943));
#142972=CARTESIAN_POINT('Ctrl Pts',(-5.42954084321747,-24.4,-4.05000000003699));
#142973=CARTESIAN_POINT('Ctrl Pts',(-5.57748269819039,-24.4,-4.05000000003699));
#142974=CARTESIAN_POINT('Ctrl Pts',(-5.62078275330442,-24.4,-4.19146341467114));
#142975=CARTESIAN_POINT('',(-5.62078275330442,-24.4,-4.19146341467114));
#142976=CARTESIAN_POINT('Origin',(-5.62078275330442,-24.,-4.19146341467114));
#142977=CARTESIAN_POINT('Origin',(-5.42954084321747,-24.,-4.25000000003699));
#142978=CARTESIAN_POINT('Origin',(-5.42954084321747,-24.4,-4.25000000003699));
#142979=CARTESIAN_POINT('Origin',(-9.35,-24.,-3.05000000003699));
#142980=CARTESIAN_POINT('',(-10.2260723087841,-24.4,-6.8503285792235));
#142981=CARTESIAN_POINT('Origin',(-10.2260723087841,-24.,-6.8503285792235));
#142982=CARTESIAN_POINT('Origin',(-9.35,-24.4,-3.05000000003699));
#142983=CARTESIAN_POINT('Ctrl Pts',(-10.1362187386524,-24.,-6.46055128905052));
#142984=CARTESIAN_POINT('Ctrl Pts',(-10.5687015536612,-24.,-6.36085301024134));
#142985=CARTESIAN_POINT('Ctrl Pts',(-10.7906143361206,-24.,-6.74521722430999));
#142986=CARTESIAN_POINT('Ctrl Pts',(-10.1362187386524,-24.4,-6.46055128905052));
#142987=CARTESIAN_POINT('Ctrl Pts',(-10.5687015536612,-24.4,-6.36085301024134));
#142988=CARTESIAN_POINT('Ctrl Pts',(-10.7906143361206,-24.4,-6.74521722430999));
#142989=CARTESIAN_POINT('Ctrl Pts',(-10.2260723087841,-24.4,-6.8503285792235));
#142990=CARTESIAN_POINT('Ctrl Pts',(-10.3702332471204,-24.4,-6.81709581962044));
#142991=CARTESIAN_POINT('Ctrl Pts',(-10.4442041746068,-24.4,-6.94521722430999));
#142992=CARTESIAN_POINT('',(-10.4442041746068,-24.4,-6.94521722430999));
#142993=CARTESIAN_POINT('',(-10.7906143361206,-24.,-6.74521722430999));
#142994=CARTESIAN_POINT('Origin',(-10.4442041746068,-24.,-6.94521722430999));
#142995=CARTESIAN_POINT('Origin',(-10.2709990938499,-24.,-7.04521722430998));
#142996=CARTESIAN_POINT('Origin',(-10.2709990938499,-24.4,-7.04521722430998));
#142997=CARTESIAN_POINT('Origin',(-8.59853004641263,-24.,-3.74841586006224));
#142998=CARTESIAN_POINT('',(-12.7419083674243,-24.4,-10.9249576270339));
#142999=CARTESIAN_POINT('',(-13.0883185289381,-24.,-10.7249576270339));
#143000=CARTESIAN_POINT('Origin',(-12.7419083674243,-24.,-10.9249576270339));
#143001=CARTESIAN_POINT('',(-8.9449402079264,-24.,-3.54841586006224));
#143002=CARTESIAN_POINT('',(-8.59853004641263,-24.4,-3.74841586006224));
#143003=CARTESIAN_POINT('Ctrl Pts',(-13.0883185289381,-24.,-10.7249576270339));
#143004=CARTESIAN_POINT('Ctrl Pts',(-13.2250694988751,-24.,-10.9618172549492));
#143005=CARTESIAN_POINT('Ctrl Pts',(-13.135978738899,-24.,-11.2204021493297));
#143006=CARTESIAN_POINT('Ctrl Pts',(-13.046887978923,-24.,-11.4789870437101));
#143007=CARTESIAN_POINT('Ctrl Pts',(-12.7932639810861,-24.,-11.5813500196151));
#143008=CARTESIAN_POINT('Ctrl Pts',(-13.0883185289381,-24.4,-10.7249576270339));
#143009=CARTESIAN_POINT('Ctrl Pts',(-13.2250694988751,-24.4,-10.9618172549492));
#143010=CARTESIAN_POINT('Ctrl Pts',(-13.135978738899,-24.4,-11.2204021493297));
#143011=CARTESIAN_POINT('Ctrl Pts',(-13.046887978923,-24.4,-11.4789870437101));
#143012=CARTESIAN_POINT('Ctrl Pts',(-12.7932639810861,-24.4,-11.5813500196151));
#143013=CARTESIAN_POINT('Ctrl Pts',(-12.7419083674243,-24.4,-10.9249576270339));
#143014=CARTESIAN_POINT('Ctrl Pts',(-12.78749202407,-24.4,-11.003910836339));
#143015=CARTESIAN_POINT('Ctrl Pts',(-12.757795104078,-24.4,-11.0901058011325));
#143016=CARTESIAN_POINT('Ctrl Pts',(-12.7280981840859,-24.4,-11.176300765926));
#143017=CARTESIAN_POINT('Ctrl Pts',(-12.6435568514736,-24.4,-11.2104217578943));
#143018=CARTESIAN_POINT('',(-12.6435568514736,-24.4,-11.2104217578943));
#143019=CARTESIAN_POINT('',(-12.7932639810861,-24.,-11.5813500196151));
#143020=CARTESIAN_POINT('Origin',(-12.6435568514736,-24.,-11.2104217578943));
#143021=CARTESIAN_POINT('Origin',(-12.5687032866674,-24.,-11.0249576270339));
#143022=CARTESIAN_POINT('Origin',(-12.5687032866674,-24.4,-11.0249576270339));
#143023=CARTESIAN_POINT('Origin',(-9.35,-24.,-3.05000000003699));
#143024=CARTESIAN_POINT('',(-9.29674553898285,-24.,-12.2498458662666));
#143025=CARTESIAN_POINT('Origin',(-9.35,-24.,-3.05000000003699));
#143026=CARTESIAN_POINT('',(-9.61646521955773,-24.4,-11.845964772975));
#143027=CARTESIAN_POINT('Origin',(-9.35,-24.4,-3.05000000003699));
#143028=CARTESIAN_POINT('Ctrl Pts',(-9.61646521955773,-24.4,-11.845964772975));
#143029=CARTESIAN_POINT('Ctrl Pts',(-9.61574684903454,-24.4,-11.8469292690866));
#143030=CARTESIAN_POINT('Ctrl Pts',(-9.61502828402677,-24.3999966702549,
-11.8478936227214));
#143031=CARTESIAN_POINT('Ctrl Pts',(-9.58516778418947,-24.3997200467267,
-11.887951279054));
#143032=CARTESIAN_POINT('Ctrl Pts',(-9.55564185868478,-24.3939779655324,
-11.9268827633724));
#143033=CARTESIAN_POINT('Ctrl Pts',(-9.49847236767601,-24.3718197176192,
-12.0010201299338));
#143034=CARTESIAN_POINT('Ctrl Pts',(-9.47064424094682,-24.3556254163147,
-12.0364970754362));
#143035=CARTESIAN_POINT('Ctrl Pts',(-9.41249687350933,-24.307908789952,
-12.1095546655319));
#143036=CARTESIAN_POINT('Ctrl Pts',(-9.38271825407688,-24.2737132836985,
-12.146203631867));
#143037=CARTESIAN_POINT('Ctrl Pts',(-9.33855412802582,-24.1981575036158,
-12.1998901428329));
#143038=CARTESIAN_POINT('Ctrl Pts',(-9.32244973805791,-24.1600118608394,
-12.2191999208178));
#143039=CARTESIAN_POINT('Ctrl Pts',(-9.30191813777489,-24.0802759631265,
-12.2437190437141));
#143040=CARTESIAN_POINT('Ctrl Pts',(-9.29674553898285,-24.0405572215704,
-12.2498458662666));
#143041=CARTESIAN_POINT('Ctrl Pts',(-9.29674553898285,-24.,-12.2498458662666));
#143042=CARTESIAN_POINT('Origin',(-5.65685424949238,-24.,-12.900000000019));
#143043=CARTESIAN_POINT('',(-3.34147109452317,-23.9860345655466,-10.0168917310781));
#143044=CARTESIAN_POINT('',(-9.29699352038222,-23.9860345613817,-12.2498472983957));
#143045=CARTESIAN_POINT('Origin',(-5.65685424949238,-23.9860345609261,-12.900000000019));
#143046=CARTESIAN_POINT('Ctrl Pts',(-9.29674553898285,-24.,-12.2498458662666));
#143047=CARTESIAN_POINT('Ctrl Pts',(-9.29674553898285,-23.9953402268027,
-12.2498458662666));
#143048=CARTESIAN_POINT('Ctrl Pts',(-9.29682833839145,-23.9906843935221,
-12.2498463466717));
#143049=CARTESIAN_POINT('Ctrl Pts',(-9.29699352039839,-23.9860345613823,
-12.2498472983958));
#143050=CARTESIAN_POINT('Origin',(-5.65685424949238,-24.4,-12.900000000019));
#143051=CARTESIAN_POINT('Ctrl Pts',(-3.34147109439903,-23.9860345655524,
-10.0168917309711));
#143052=CARTESIAN_POINT('Ctrl Pts',(-3.341509443135,-23.9874600657353,-10.0169248044703));
#143053=CARTESIAN_POINT('Ctrl Pts',(-3.34154193167206,-23.9888862421037,
-10.0169528233557));
#143054=CARTESIAN_POINT('Ctrl Pts',(-3.34162881025419,-23.9935434575362,
-10.0170277488358));
#143055=CARTESIAN_POINT('Ctrl Pts',(-3.34165888869614,-23.9967726737154,
-10.0170536879467));
#143056=CARTESIAN_POINT('Ctrl Pts',(-3.34165888869614,-24.,-10.0170536879467));
#143057=CARTESIAN_POINT('Origin',(-10.5340572614694,-19.9,-6.30084733597289));
#143058=CARTESIAN_POINT('',(-13.0883185289381,-20.,-10.7249576270339));
#143059=CARTESIAN_POINT('',(-13.0883185289381,-19.9,-10.7249576270339));
#143060=CARTESIAN_POINT('',(-10.7906143361206,-20.,-6.74521722430999));
#143061=CARTESIAN_POINT('',(-11.083848469093,-20.,-7.25311364113158));
#143062=CARTESIAN_POINT('',(-10.7906143361206,-21.1,-6.74521722430999));
#143063=CARTESIAN_POINT('Origin',(-12.5687032866674,-19.9,-11.0249576270339));
#143064=CARTESIAN_POINT('',(-12.7932639810861,-20.,-11.5813500196151));
#143065=CARTESIAN_POINT('',(-12.7932639810861,-19.9,-11.5813500196151));
#143066=CARTESIAN_POINT('Origin',(-12.5687032866674,-20.,-11.0249576270339));
#143067=CARTESIAN_POINT('Origin',(-5.65685424949238,-23.8568542494924,-12.900000000019));
#143068=CARTESIAN_POINT('Ctrl Pts',(-3.34147109439903,-23.9860345655524,
-10.0168917309711));
#143069=CARTESIAN_POINT('Ctrl Pts',(-3.33980474884187,-23.9240931491361,
-10.0154546072388));
#143070=CARTESIAN_POINT('Ctrl Pts',(-3.33933631565976,-23.8620596978386,
-10.0150501085589));
#143071=CARTESIAN_POINT('Ctrl Pts',(-3.34007057236773,-23.8,-10.0156836186691));
#143072=CARTESIAN_POINT('Ctrl Pts',(-3.34678531450252,-23.2324670603222,
-10.0214770380324));
#143073=CARTESIAN_POINT('Ctrl Pts',(-3.45749112478326,-22.6438394405351,
-10.1208452048344));
#143074=CARTESIAN_POINT('Ctrl Pts',(-3.79210650744726,-21.8648455084378,
-10.3828564688412));
#143075=CARTESIAN_POINT('Ctrl Pts',(-3.93516684582503,-21.6185652596727,
-10.4905697000702));
#143076=CARTESIAN_POINT('Ctrl Pts',(-4.27387597232643,-21.1849574912198,
-10.7256407182475));
#143077=CARTESIAN_POINT('Ctrl Pts',(-4.46961146676767,-20.9976223772148,
-10.8528595348611));
#143078=CARTESIAN_POINT('Ctrl Pts',(-4.88103383123282,-20.7104988261178,
-11.0948576110964));
#143079=CARTESIAN_POINT('Ctrl Pts',(-5.11310773771486,-20.5923839396418,
-11.2209466582962));
#143080=CARTESIAN_POINT('Ctrl Pts',(-5.60871935569803,-20.4371939821691,
-11.4594259875479));
#143081=CARTESIAN_POINT('Ctrl Pts',(-5.87241302260401,-20.4001685914811,
-11.5715243725022));
#143082=CARTESIAN_POINT('Ctrl Pts',(-6.36784226154627,-20.4001685914811,
-11.7572799449367));
#143083=CARTESIAN_POINT('Ctrl Pts',(-6.64023366360302,-20.4371939821691,
-11.8461805746377));
#143084=CARTESIAN_POINT('Ctrl Pts',(-7.17046372693134,-20.5923839396418,
-11.9923289454911));
#143085=CARTESIAN_POINT('Ctrl Pts',(-7.4282279911993,-20.7104988261178,
-12.0498991631386));
#143086=CARTESIAN_POINT('Ctrl Pts',(-7.89733525228042,-20.9976223772148,
-12.1380456802828));
#143087=CARTESIAN_POINT('Ctrl Pts',(-8.12846146141512,-21.1849574912198,
-12.1708738166254));
#143088=CARTESIAN_POINT('Ctrl Pts',(-8.53822541702071,-21.6185652596727,
-12.2164342890631));
#143089=CARTESIAN_POINT('Ctrl Pts',(-8.71683712981021,-21.8648455084378,
-12.2293283440095));
#143090=CARTESIAN_POINT('Ctrl Pts',(-9.14122841916257,-22.6438394405351,
-12.2518980206493));
#143091=CARTESIAN_POINT('Ctrl Pts',(-9.28997465514599,-23.2324670603222,
-12.2498084550781));
#143092=CARTESIAN_POINT('Ctrl Pts',(-9.29884308443129,-23.8,-12.2498577690457));
#143093=CARTESIAN_POINT('Ctrl Pts',(-9.299812397741,-23.8620309656229,-12.2498631590289));
#143094=CARTESIAN_POINT('Ctrl Pts',(-9.29919497128662,-23.9240642722867,
-12.2498599824283));
#143095=CARTESIAN_POINT('Ctrl Pts',(-9.29699352039839,-23.9860345613823,
-12.2498472983958));
#143096=CARTESIAN_POINT('Origin',(-9.35,-19.9,-3.05000000003699));
#143097=CARTESIAN_POINT('',(-15.0167338549885,-20.,-10.2976290893825));
#143098=CARTESIAN_POINT('',(-15.0167338549885,-19.9,-10.2976290893825));
#143099=CARTESIAN_POINT('Origin',(-9.35,-20.,-3.05000000003699));
#143100=CARTESIAN_POINT('',(-0.631395349681702,-20.,-5.98699386306226));
#143101=CARTESIAN_POINT('',(-0.631395349681702,-19.9,-5.98699386306226));
#143102=CARTESIAN_POINT('',(-0.294290142826895,-20.,-4.67299691398904));
#143103=CARTESIAN_POINT('Origin',(-9.35,-20.,-3.05000000003699));
#143104=CARTESIAN_POINT('',(-0.294290142826894,-19.2199531690376,-4.67299691398904));
#143105=CARTESIAN_POINT('',(-0.294290142826896,-19.9,-4.67299691398904));
#143106=CARTESIAN_POINT('',(-0.298851850326922,-19.2053752002609,-4.69824669658142));
#143107=CARTESIAN_POINT('Origin',(-9.35,-20.1569908742018,-3.05000000003699));
#143108=CARTESIAN_POINT('',(-0.342996093127177,-19.1393368299495,-4.92453477474183));
#143109=CARTESIAN_POINT('Ctrl Pts',(-0.342996093127217,-19.1393368299494,
-4.92453477474201));
#143110=CARTESIAN_POINT('Ctrl Pts',(-0.338919064412081,-19.1408255450474,
-4.90494494687582));
#143111=CARTESIAN_POINT('Ctrl Pts',(-0.334921557723668,-19.1432424146486,
-4.88531258691514));
#143112=CARTESIAN_POINT('Ctrl Pts',(-0.331000810775166,-19.1466300793749,
-4.8658317759892));
#143113=CARTESIAN_POINT('Ctrl Pts',(-0.327439080338206,-19.149707541074,
-4.84813479168418));
#143114=CARTESIAN_POINT('Ctrl Pts',(-0.323940103826726,-19.1535851808526,
-4.83056196821088));
#143115=CARTESIAN_POINT('Ctrl Pts',(-0.320545023409296,-19.1582941278276,
-4.81325056669589));
#143116=CARTESIAN_POINT('Ctrl Pts',(-0.319571527254381,-19.1596443585174,
-4.80828674235626));
#143117=CARTESIAN_POINT('Ctrl Pts',(-0.318606891114168,-19.1610629779184,
-4.8033444026678));
#143118=CARTESIAN_POINT('Ctrl Pts',(-0.317652896980343,-19.1625508569463,
-4.79842681298157));
#143119=CARTESIAN_POINT('Ctrl Pts',(-0.314288911428832,-19.1677974338119,
-4.78108634927618));
#143120=CARTESIAN_POINT('Ctrl Pts',(-0.311033236905911,-19.1739224599097,
-4.76399853811601));
#143121=CARTESIAN_POINT('Ctrl Pts',(-0.30788938154976,-19.1810057026344,
-4.7472968131946));
#143122=CARTESIAN_POINT('Ctrl Pts',(-0.304916277889118,-19.1877042343697,
-4.73150220629397));
#143123=CARTESIAN_POINT('Ctrl Pts',(-0.302043295501447,-19.1952595294941,
-4.71605245153));
#143124=CARTESIAN_POINT('Ctrl Pts',(-0.299306816945607,-19.2037448874674,
-4.70109451849818));
#143125=CARTESIAN_POINT('Ctrl Pts',(-0.299149655135435,-19.2042322197054,
-4.70023545244532));
#143126=CARTESIAN_POINT('Ctrl Pts',(-0.29899295283953,-19.2047226217816,
-4.69937801956356));
#143127=CARTESIAN_POINT('Ctrl Pts',(-0.298836720346318,-19.2052161083662,
-4.69852225182618));
#143128=CARTESIAN_POINT('',(-1.,-18.2,-6.91231795691211));
#143129=CARTESIAN_POINT('Ctrl Pts',(-0.342996093127179,-19.1393368299495,
-4.92453477474183));
#143130=CARTESIAN_POINT('Ctrl Pts',(-0.390027426021725,-19.1221634764483,
-5.15051692500272));
#143131=CARTESIAN_POINT('Ctrl Pts',(-0.444566627282946,-19.0983023390303,
-5.36921499635279));
#143132=CARTESIAN_POINT('Ctrl Pts',(-0.57830980171757,-19.020446191969,
-5.83793682181643));
#143133=CARTESIAN_POINT('Ctrl Pts',(-0.682583950067457,-18.9451070919295,
-6.14520550751075));
#143134=CARTESIAN_POINT('Ctrl Pts',(-0.813666835274515,-18.7846217981295,
-6.48259695343331));
#143135=CARTESIAN_POINT('Ctrl Pts',(-0.860880288003759,-18.7154616839175,
-6.59730399074034));
#143136=CARTESIAN_POINT('Ctrl Pts',(-0.923475479616496,-18.588207088439,
-6.7429762948862));
#143137=CARTESIAN_POINT('Ctrl Pts',(-0.950034610743345,-18.5217732832391,
-6.80269945385084));
#143138=CARTESIAN_POINT('Ctrl Pts',(-0.978869456157098,-18.408184197995,
-6.86637474789097));
#143139=CARTESIAN_POINT('Ctrl Pts',(-0.986675532106876,-18.3679906488546,
-6.8834002020665));
#143140=CARTESIAN_POINT('Ctrl Pts',(-0.997241481275889,-18.2851363950946,
-6.90637026654278));
#143141=CARTESIAN_POINT('Ctrl Pts',(-1.,-18.2424763716807,-6.91231795691211));
#143142=CARTESIAN_POINT('Ctrl Pts',(-1.,-18.2,-6.91231795691211));
#143143=CARTESIAN_POINT('',(-0.707045437301172,-17.4928318802494,-6.20267131609953));
#143144=CARTESIAN_POINT('Ctrl Pts',(-1.,-18.2,-6.91231795691211));
#143145=CARTESIAN_POINT('Ctrl Pts',(-1.,-18.1575236283193,-6.91231795691211));
#143146=CARTESIAN_POINT('Ctrl Pts',(-0.997241481275889,-18.1148636049054,
-6.90637026654278));
#143147=CARTESIAN_POINT('Ctrl Pts',(-0.986675532106877,-18.0320093511454,
-6.88340020206649));
#143148=CARTESIAN_POINT('Ctrl Pts',(-0.978869456157098,-17.991815802005,
-6.86637474789097));
#143149=CARTESIAN_POINT('Ctrl Pts',(-0.950034610743345,-17.8782267167609,
-6.80269945385084));
#143150=CARTESIAN_POINT('Ctrl Pts',(-0.923475479616496,-17.811792911561,
-6.7429762948862));
#143151=CARTESIAN_POINT('Ctrl Pts',(-0.860880288003759,-17.6845383160825,
-6.59730399074034));
#143152=CARTESIAN_POINT('Ctrl Pts',(-0.813666835274515,-17.6153782018705,
-6.48259695343331));
#143153=CARTESIAN_POINT('Ctrl Pts',(-0.75261478687592,-17.5406319380172,
-6.32545638658357));
#143154=CARTESIAN_POINT('Ctrl Pts',(-0.729894647720439,-17.5156771266932,
-6.2653117462773));
#143155=CARTESIAN_POINT('Ctrl Pts',(-0.707045437301173,-17.4928318802494,
-6.20267131609953));
#143156=CARTESIAN_POINT('',(-0.689573580943891,-17.4676466969021,-6.15435407779857));
#143157=CARTESIAN_POINT('Ctrl Pts',(-0.689576769163932,-17.4676488696199,
-6.15435513352118));
#143158=CARTESIAN_POINT('Ctrl Pts',(-0.692251029448898,-17.4728748513358,
-6.16181963780152));
#143159=CARTESIAN_POINT('Ctrl Pts',(-0.695047478275197,-17.4775916434185,
-6.16958981118521));
#143160=CARTESIAN_POINT('Ctrl Pts',(-0.697949233001934,-17.4817806390516,
-6.17760927298781));
#143161=CARTESIAN_POINT('Ctrl Pts',(-0.700891780631754,-17.4860285236359,
-6.18574147248153));
#143162=CARTESIAN_POINT('Ctrl Pts',(-0.70393704643326,-17.48972582708,-6.19411510571193));
#143163=CARTESIAN_POINT('Ctrl Pts',(-0.707067566378145,-17.4928576526749,
-6.20267384590877));
#143164=CARTESIAN_POINT('',(-0.605214914090966,-17.2952175137768,-5.90809968361399));
#143165=CARTESIAN_POINT('Origin',(-9.35,-15.2939545703814,-3.05000000003699));
#143166=CARTESIAN_POINT('',(-0.294290142826895,-16.4303892440217,-4.67299691398904));
#143167=CARTESIAN_POINT('Origin',(-9.35,-15.2939545703814,-3.05000000003699));
#143168=CARTESIAN_POINT('',(-0.294290142826895,-15.9,-4.67299691398904));
#143169=CARTESIAN_POINT('',(-0.294290142826896,-19.9,-4.67299691398904));
#143170=CARTESIAN_POINT('',(-16.5700864372805,-15.9,-8.75178496951782));
#143171=CARTESIAN_POINT('Origin',(-9.35,-15.9,-3.05000000003699));
#143172=CARTESIAN_POINT('',(-16.5700864372805,-20.,-8.75178496951782));
#143173=CARTESIAN_POINT('',(-16.5700864372805,-19.9,-8.75178496951782));
#143174=CARTESIAN_POINT('',(-15.3208637689692,-20.,-10.0491989436598));
#143175=CARTESIAN_POINT('Origin',(-9.35,-20.,-3.05000000003699));
#143176=CARTESIAN_POINT('',(-15.3208637689692,-19.9,-10.0491989436598));
#143177=CARTESIAN_POINT('Origin',(-3.45175358661618,-24.4,-3.05000000003699));
#143178=CARTESIAN_POINT('Origin',(-9.35,-24.,-3.05000000003699));
#143179=CARTESIAN_POINT('',(-0.631395349681703,-24.,-0.11300613701172));
#143180=CARTESIAN_POINT('',(-1.01046511708685,-24.4,-0.240701522360645));
#143181=CARTESIAN_POINT('Origin',(-1.01046511708685,-24.,-0.240701522360645));
#143182=CARTESIAN_POINT('',(-12.6435568514736,-24.4,5.11042175782032));
#143183=CARTESIAN_POINT('Origin',(-9.35,-24.4,-3.05000000003699));
#143184=CARTESIAN_POINT('',(-12.7932639810861,-24.,5.4813500195411));
#143185=CARTESIAN_POINT('Origin',(-12.6435568514736,-24.,5.11042175782032));
#143186=CARTESIAN_POINT('Origin',(-9.35,-24.,-3.05000000003699));
#143187=CARTESIAN_POINT('Ctrl Pts',(-12.7932639810861,-24.,5.4813500195411));
#143188=CARTESIAN_POINT('Ctrl Pts',(-13.046887978923,-24.,5.37898704363615));
#143189=CARTESIAN_POINT('Ctrl Pts',(-13.135978738899,-24.,5.12040214925567));
#143190=CARTESIAN_POINT('Ctrl Pts',(-13.2250694988751,-24.,4.86181725487519));
#143191=CARTESIAN_POINT('Ctrl Pts',(-13.0883185289381,-24.,4.62495762695992));
#143192=CARTESIAN_POINT('Ctrl Pts',(-12.7932639810861,-24.4,5.4813500195411));
#143193=CARTESIAN_POINT('Ctrl Pts',(-13.046887978923,-24.4,5.37898704363615));
#143194=CARTESIAN_POINT('Ctrl Pts',(-13.135978738899,-24.4,5.12040214925567));
#143195=CARTESIAN_POINT('Ctrl Pts',(-13.2250694988751,-24.4,4.86181725487519));
#143196=CARTESIAN_POINT('Ctrl Pts',(-13.0883185289381,-24.4,4.62495762695992));
#143197=CARTESIAN_POINT('Ctrl Pts',(-12.6435568514736,-24.4,5.11042175782032));
#143198=CARTESIAN_POINT('Ctrl Pts',(-12.7280981840859,-24.4,5.076300765852));
#143199=CARTESIAN_POINT('Ctrl Pts',(-12.757795104078,-24.4,4.99010580105851));
#143200=CARTESIAN_POINT('Ctrl Pts',(-12.78749202407,-24.4,4.90391083626501));
#143201=CARTESIAN_POINT('Ctrl Pts',(-12.7419083674243,-24.4,4.82495762695992));
#143202=CARTESIAN_POINT('',(-12.7419083674243,-24.4,4.82495762695992));
#143203=CARTESIAN_POINT('',(-13.0883185289381,-24.,4.62495762695992));
#143204=CARTESIAN_POINT('Origin',(-12.7419083674243,-24.,4.82495762695992));
#143205=CARTESIAN_POINT('Origin',(-12.5687032866674,-24.,4.92495762695992));
#143206=CARTESIAN_POINT('Origin',(-12.5687032866674,-24.4,4.92495762695992));
#143207=CARTESIAN_POINT('Origin',(-10.0881676893362,-24.,0.228543942399029));
#143208=CARTESIAN_POINT('',(-10.4442041746068,-24.4,0.845217224235998));
#143209=CARTESIAN_POINT('',(-10.7906143361206,-24.,0.645217224235999));
#143210=CARTESIAN_POINT('Origin',(-10.4442041746068,-24.,0.845217224235998));
#143211=CARTESIAN_POINT('',(-10.43457785085,-24.,0.0285439423990298));
#143212=CARTESIAN_POINT('',(-10.0881676893362,-24.4,0.228543942399029));
#143213=CARTESIAN_POINT('Ctrl Pts',(-10.7906143361206,-24.,0.645217224236));
#143214=CARTESIAN_POINT('Ctrl Pts',(-10.5687015536612,-24.,0.260853010167357));
#143215=CARTESIAN_POINT('Ctrl Pts',(-10.1362187386524,-24.,0.360551288976537));
#143216=CARTESIAN_POINT('Ctrl Pts',(-10.7906143361206,-24.4,0.645217224236));
#143217=CARTESIAN_POINT('Ctrl Pts',(-10.5687015536612,-24.4,0.260853010167357));
#143218=CARTESIAN_POINT('Ctrl Pts',(-10.1362187386524,-24.4,0.360551288976537));
#143219=CARTESIAN_POINT('Ctrl Pts',(-10.4442041746068,-24.4,0.845217224235999));
#143220=CARTESIAN_POINT('Ctrl Pts',(-10.3702332471204,-24.4,0.717095819546453));
#143221=CARTESIAN_POINT('Ctrl Pts',(-10.2260723087841,-24.4,0.750328579149512));
#143222=CARTESIAN_POINT('',(-10.2260723087841,-24.4,0.750328579149511));
#143223=CARTESIAN_POINT('Origin',(-10.2260723087841,-24.,0.750328579149511));
#143224=CARTESIAN_POINT('Origin',(-10.2709990938499,-24.,0.945217224235998));
#143225=CARTESIAN_POINT('Origin',(-10.2709990938499,-24.4,0.945217224235998));
#143226=CARTESIAN_POINT('Origin',(-9.35,-24.,-3.05000000003699));
#143227=CARTESIAN_POINT('',(-5.62078275330442,-24.4,-1.90853658540285));
#143228=CARTESIAN_POINT('Origin',(-5.62078275330442,-24.,-1.90853658540285));
#143229=CARTESIAN_POINT('Origin',(-9.35,-24.4,-3.05000000003699));
#143230=CARTESIAN_POINT('Ctrl Pts',(-6.00326657347833,-24.,-2.02560975613455));
#143231=CARTESIAN_POINT('Ctrl Pts',(-5.87336640813625,-24.,-2.45000000003699));
#143232=CARTESIAN_POINT('Ctrl Pts',(-5.42954084321747,-24.,-2.45000000003699));
#143233=CARTESIAN_POINT('Ctrl Pts',(-6.00326657347833,-24.4,-2.02560975613455));
#143234=CARTESIAN_POINT('Ctrl Pts',(-5.87336640813625,-24.4,-2.45000000003699));
#143235=CARTESIAN_POINT('Ctrl Pts',(-5.42954084321747,-24.4,-2.45000000003699));
#143236=CARTESIAN_POINT('Ctrl Pts',(-5.62078275330442,-24.4,-1.90853658540285));
#143237=CARTESIAN_POINT('Ctrl Pts',(-5.57748269819039,-24.4,-2.05000000003699));
#143238=CARTESIAN_POINT('Ctrl Pts',(-5.42954084321747,-24.4,-2.05000000003699));
#143239=CARTESIAN_POINT('',(-5.42954084321747,-24.4,-2.05000000003699));
#143240=CARTESIAN_POINT('',(-5.42954084321747,-24.,-2.45000000003699));
#143241=CARTESIAN_POINT('Origin',(-5.42954084321747,-24.,-2.05000000003699));
#143242=CARTESIAN_POINT('Origin',(-5.42954084321747,-24.,-1.85000000003699));
#143243=CARTESIAN_POINT('Origin',(-5.42954084321747,-24.4,-1.85000000003699));
#143244=CARTESIAN_POINT('Origin',(-4.69720428956801,-24.,-2.05000000003699));
#143245=CARTESIAN_POINT('',(-1.20000000078942,-24.4,-2.05000000003699));
#143246=CARTESIAN_POINT('',(-1.20000000078942,-24.,-2.45000000003699));
#143247=CARTESIAN_POINT('Origin',(-1.20000000078942,-24.,-2.05000000003699));
#143248=CARTESIAN_POINT('',(-4.69720428956801,-24.,-2.45000000003699));
#143249=CARTESIAN_POINT('',(-4.69720428956801,-24.4,-2.05000000003699));
#143250=CARTESIAN_POINT('Ctrl Pts',(-1.20000000078942,-24.,-2.45000000003699));
#143251=CARTESIAN_POINT('Ctrl Pts',(-0.600000000789417,-24.,-2.45000000003699));
#143252=CARTESIAN_POINT('Ctrl Pts',(-0.600000000789417,-24.,-1.85000000003699));
#143253=CARTESIAN_POINT('Ctrl Pts',(-1.20000000078942,-24.4,-2.45000000003699));
#143254=CARTESIAN_POINT('Ctrl Pts',(-0.600000000789417,-24.4,-2.45000000003699));
#143255=CARTESIAN_POINT('Ctrl Pts',(-0.600000000789417,-24.4,-1.85000000003699));
#143256=CARTESIAN_POINT('Ctrl Pts',(-1.20000000078942,-24.4,-2.05000000003699));
#143257=CARTESIAN_POINT('Ctrl Pts',(-1.00000000078942,-24.4,-2.05000000003699));
#143258=CARTESIAN_POINT('Ctrl Pts',(-1.00000000078942,-24.4,-1.85000000003699));
#143259=CARTESIAN_POINT('',(-1.00000000078942,-24.4,-1.85000000003699));
#143260=CARTESIAN_POINT('',(-0.600000000789417,-24.,-1.85000000003699));
#143261=CARTESIAN_POINT('Origin',(-1.00000000078942,-24.,-1.85000000003699));
#143262=CARTESIAN_POINT('Origin',(-1.20000000078942,-24.,-1.85000000003699));
#143263=CARTESIAN_POINT('Origin',(-1.20000000078942,-24.4,-1.85000000003699));
#143264=CARTESIAN_POINT('Origin',(-1.00000000078942,-24.,-1.33262554947194));
#143265=CARTESIAN_POINT('',(-1.00000000078942,-24.4,-0.304549215035108));
#143266=CARTESIAN_POINT('',(-0.600000000789418,-24.,-0.304549215035108));
#143267=CARTESIAN_POINT('Origin',(-1.00000000078942,-24.,-0.304549215035108));
#143268=CARTESIAN_POINT('',(-0.600000000789417,-24.,-1.33262554947194));
#143269=CARTESIAN_POINT('',(-1.00000000078942,-24.4,-1.33262554947194));
#143270=CARTESIAN_POINT('Ctrl Pts',(-0.600000000789417,-24.,-0.304549215035108));
#143271=CARTESIAN_POINT('Ctrl Pts',(-0.600000000789417,-24.,-0.206204709299061));
#143272=CARTESIAN_POINT('Ctrl Pts',(-0.631395349681703,-24.,-0.113006137011717));
#143273=CARTESIAN_POINT('Ctrl Pts',(-0.600000000789417,-24.4,-0.304549215035108));
#143274=CARTESIAN_POINT('Ctrl Pts',(-0.600000000789417,-24.4,-0.206204709299061));
#143275=CARTESIAN_POINT('Ctrl Pts',(-0.631395349681703,-24.4,-0.113006137011717));
#143276=CARTESIAN_POINT('Ctrl Pts',(-1.00000000078942,-24.4,-0.304549215035108));
#143277=CARTESIAN_POINT('Ctrl Pts',(-1.00000000078942,-24.4,-0.271767713123092));
#143278=CARTESIAN_POINT('Ctrl Pts',(-1.01046511708685,-24.4,-0.240701522360645));
#143279=CARTESIAN_POINT('Origin',(-1.20000000078942,-24.,-0.304549215035108));
#143280=CARTESIAN_POINT('Origin',(-1.20000000078942,-24.4,-0.304549215035108));
#143281=CARTESIAN_POINT('Origin',(-5.94265499251984,-19.9,-2.45000000003699));
#143282=CARTESIAN_POINT('',(-1.20000000078942,-20.,-2.45000000003699));
#143283=CARTESIAN_POINT('',(-1.20000000078942,-19.9,-2.45000000003699));
#143284=CARTESIAN_POINT('',(-5.42954084321747,-20.,-2.45000000003699));
#143285=CARTESIAN_POINT('',(-4.29148370813747,-20.,-2.45000000003699));
#143286=CARTESIAN_POINT('',(-5.42954084321747,-21.1,-2.45000000003699));
#143287=CARTESIAN_POINT('Origin',(-1.20000000078942,-19.9,-1.85000000003699));
#143288=CARTESIAN_POINT('',(-0.600000000789417,-20.,-1.85000000003699));
#143289=CARTESIAN_POINT('',(-0.600000000789418,-19.9,-1.85000000003699));
#143290=CARTESIAN_POINT('Origin',(-1.20000000078942,-20.,-1.85000000003699));
#143291=CARTESIAN_POINT('Origin',(-0.600000000789418,-19.9,0.384748901093117));
#143292=CARTESIAN_POINT('',(-0.600000000789418,-20.,-0.304549215035106));
#143293=CARTESIAN_POINT('',(-0.600000000789418,-19.9,-0.304549215035106));
#143294=CARTESIAN_POINT('',(-0.600000000789418,-20.,-0.0326255494647287));
#143295=CARTESIAN_POINT('Origin',(-1.20000000078942,-19.9,-0.304549215035106));
#143296=CARTESIAN_POINT('',(-0.631395349681703,-20.,-0.113006137011719));
#143297=CARTESIAN_POINT('',(-0.631395349681703,-19.9,-0.113006137011719));
#143298=CARTESIAN_POINT('Origin',(-1.20000000078942,-20.,-0.304549215035107));
#143299=CARTESIAN_POINT('Origin',(-9.35,-19.9,-3.05000000003699));
#143300=CARTESIAN_POINT('',(-12.7932639810861,-20.,5.4813500195411));
#143301=CARTESIAN_POINT('',(-12.7932639810861,-19.9,5.4813500195411));
#143302=CARTESIAN_POINT('',(-15.8187500000085,-20.,3.49180964541969));
#143303=CARTESIAN_POINT('Origin',(-9.35,-20.,-3.05000000003699));
#143304=CARTESIAN_POINT('',(-15.8187500000085,-15.9,3.49180964541969));
#143305=CARTESIAN_POINT('',(-15.8187500000085,-19.9,3.49180964541969));
#143306=CARTESIAN_POINT('',(-0.259697928570093,-15.9,-1.63352259105473));
#143307=CARTESIAN_POINT('Origin',(-9.35,-15.9,-3.05000000003699));
#143308=CARTESIAN_POINT('',(-0.259697928570093,-16.4335328638949,-1.63352259105473));
#143309=CARTESIAN_POINT('',(-0.259697928570092,-19.9,-1.63352259105473));
#143310=CARTESIAN_POINT('',(-0.522069917640389,-17.2551814608384,-0.460086785087467));
#143311=CARTESIAN_POINT('Origin',(-9.35,-15.4417047044218,-3.05000000003699));
#143312=CARTESIAN_POINT('',(-0.703370836441857,-17.4891769091775,0.092579212634288));
#143313=CARTESIAN_POINT('Ctrl Pts',(-0.703370836454029,-17.4891769091919,
0.0925792126665254));
#143314=CARTESIAN_POINT('Ctrl Pts',(-0.658863507426592,-17.4451361940672,
-0.0298801887081493));
#143315=CARTESIAN_POINT('Ctrl Pts',(-0.616842608901601,-17.4065266547297,
-0.154129592507691));
#143316=CARTESIAN_POINT('Ctrl Pts',(-0.560016497085532,-17.3303629754732,
-0.333206402781313));
#143317=CARTESIAN_POINT('Ctrl Pts',(-0.539569532605825,-17.2969480440437,
-0.400437922534331));
#143318=CARTESIAN_POINT('Ctrl Pts',(-0.522069917640389,-17.2551814608384,
-0.46008678508747));
#143319=CARTESIAN_POINT('',(-1.,-18.2,0.812317956838124));
#143320=CARTESIAN_POINT('Ctrl Pts',(-0.703370836441977,-17.48917690918,
0.092579212633367));
#143321=CARTESIAN_POINT('Ctrl Pts',(-0.727460088883102,-17.5130136104037,
0.158859429802102));
#143322=CARTESIAN_POINT('Ctrl Pts',(-0.751446619517419,-17.5392017461089,
0.222449665429705));
#143323=CARTESIAN_POINT('Ctrl Pts',(-0.813666835274514,-17.6153782018705,
0.382596953359324));
#143324=CARTESIAN_POINT('Ctrl Pts',(-0.860880288003759,-17.6845383160825,
0.497303990666353));
#143325=CARTESIAN_POINT('Ctrl Pts',(-0.923475479616496,-17.811792911561,
0.642976294812216));
#143326=CARTESIAN_POINT('Ctrl Pts',(-0.950034610743346,-17.8782267167609,
0.702699453776853));
#143327=CARTESIAN_POINT('Ctrl Pts',(-0.978869456157099,-17.991815802005,
0.766374747816984));
#143328=CARTESIAN_POINT('Ctrl Pts',(-0.986675532106877,-18.0320093511454,
0.783400201992511));
#143329=CARTESIAN_POINT('Ctrl Pts',(-0.997241481275889,-18.1148636049054,
0.806370266468799));
#143330=CARTESIAN_POINT('Ctrl Pts',(-1.,-18.1575236283193,0.812317956838124));
#143331=CARTESIAN_POINT('Ctrl Pts',(-1.,-18.2,0.812317956838124));
#143332=CARTESIAN_POINT('',(-0.2950380218237,-19.1554855130662,-1.42283572628271));
#143333=CARTESIAN_POINT('Ctrl Pts',(-1.,-18.2,0.812317956838124));
#143334=CARTESIAN_POINT('Ctrl Pts',(-1.,-18.2424763716807,0.812317956838124));
#143335=CARTESIAN_POINT('Ctrl Pts',(-0.997241481275889,-18.2851363950946,
0.806370266468801));
#143336=CARTESIAN_POINT('Ctrl Pts',(-0.986675532106876,-18.3679906488546,
0.783400201992511));
#143337=CARTESIAN_POINT('Ctrl Pts',(-0.978869456157098,-18.408184197995,
0.766374747816981));
#143338=CARTESIAN_POINT('Ctrl Pts',(-0.950034610743345,-18.5217732832391,
0.70269945377685));
#143339=CARTESIAN_POINT('Ctrl Pts',(-0.923475479616496,-18.588207088439,
0.642976294812216));
#143340=CARTESIAN_POINT('Ctrl Pts',(-0.860880288003759,-18.7154616839175,
0.497303990666353));
#143341=CARTESIAN_POINT('Ctrl Pts',(-0.813666835274514,-18.7846217981295,
0.382596953359324));
#143342=CARTESIAN_POINT('Ctrl Pts',(-0.682583950067456,-18.9451070919295,
0.0452055074367616));
#143343=CARTESIAN_POINT('Ctrl Pts',(-0.57830980171757,-19.020446191969,
-0.262063178257554));
#143344=CARTESIAN_POINT('Ctrl Pts',(-0.423429326492426,-19.1106070327523,
-0.804863656734993));
#143345=CARTESIAN_POINT('Ctrl Pts',(-0.351385643958767,-19.1380863052892,
-1.10926838448257));
#143346=CARTESIAN_POINT('Ctrl Pts',(-0.295038021823737,-19.1554855130657,
-1.42283572628275));
#143347=CARTESIAN_POINT('',(-0.260663520072962,-19.2137914246021,-1.62733969108494));
#143348=CARTESIAN_POINT('Ctrl Pts',(-0.260663520072961,-19.2137914246021,
-1.62733969108494));
#143349=CARTESIAN_POINT('Ctrl Pts',(-0.263049439156941,-19.2049905456179,
-1.61209612153309));
#143350=CARTESIAN_POINT('Ctrl Pts',(-0.26556279235318,-19.197231830287,
-1.5962907461053));
#143351=CARTESIAN_POINT('Ctrl Pts',(-0.276256418693354,-19.1697212655996,
-1.53022122955726));
#143352=CARTESIAN_POINT('Ctrl Pts',(-0.285408690980658,-19.1584588901442,
-1.47642172621256));
#143353=CARTESIAN_POINT('Ctrl Pts',(-0.295038021824301,-19.1554855130655,
-1.42283572627961));
#143354=CARTESIAN_POINT('',(-0.259697928570093,-19.217361123564,-1.63352259105473));
#143355=CARTESIAN_POINT('Origin',(-9.35,-20.0351647369409,-3.05000000003699));
#143356=CARTESIAN_POINT('',(-0.259697928570092,-20.,-1.63352259105473));
#143357=CARTESIAN_POINT('',(-0.259697928570092,-19.9,-1.63352259105473));
#143358=CARTESIAN_POINT('Origin',(-9.35,-20.,-3.05000000003699));
#143359=CARTESIAN_POINT('Origin',(-3.45175358661618,-24.4,-3.05000000003699));
#143360=CARTESIAN_POINT('Origin',(-15.7000000000318,-22.8,-8.38137084992264));
#143361=CARTESIAN_POINT('',(-15.1343145750825,-20.,-8.94705627487188));
#143362=CARTESIAN_POINT('',(-15.1343145750825,-22.8,-8.94705627487188));
#143363=CARTESIAN_POINT('Origin',(-15.7000000000318,-20.,-8.38137084992264));
#143364=CARTESIAN_POINT('Origin',(-14.9000000000324,-22.8,-8.71274169982174));
#143365=CARTESIAN_POINT('',(-15.3557236788353,-20.,-9.16846537862466));
#143366=CARTESIAN_POINT('',(-15.3557236788353,-19.9,-9.16846537862467));
#143367=CARTESIAN_POINT('',(-14.4242364691429,-20.,-8.23697816893229));
#143368=CARTESIAN_POINT('Origin',(-14.9314596101234,-19.9,-9.5927294473366));
#143369=CARTESIAN_POINT('Origin',(-14.9314596101234,-20.,-9.5927294473366));
#143370=CARTESIAN_POINT('Origin',(-11.7246781315911,-10.3,-15.0676288747919));
#143371=CARTESIAN_POINT('',(-12.3207815844978,-10.3,-15.1358979998248));
#143372=CARTESIAN_POINT('',(-12.3207815844978,-10.3,-15.1358979998248));
#143373=CARTESIAN_POINT('Origin',(-11.7246781315911,-10.3,-15.0676288747919));
#143374=CARTESIAN_POINT('Origin',(-15.5,-10.3,-15.5));
#143375=CARTESIAN_POINT('Origin',(-15.5,-10.3,-15.5));
#143376=CARTESIAN_POINT('Origin',(-17.9000000000407,-24.4,-10.0156854249824));
#143377=CARTESIAN_POINT('',(-18.1828427125153,-15.9,-9.73284271250775));
#143378=CARTESIAN_POINT('',(-17.5000000000407,-15.9,-10.0156854249794));
#143379=CARTESIAN_POINT('Origin',(-17.9000000000407,-15.9,-10.0156854249824));
#143380=CARTESIAN_POINT('',(-17.5000000000407,-10.3,-10.0156854249794));
#143381=CARTESIAN_POINT('',(-17.5000000000407,-24.4,-10.0156854249794));
#143382=CARTESIAN_POINT('',(-18.1828427125153,-10.3,-9.73284271250775));
#143383=CARTESIAN_POINT('Origin',(-17.9000000000407,-10.3,-10.0156854249824));
#143384=CARTESIAN_POINT('',(-18.1828427125153,-24.4,-9.73284271250775));
#143385=CARTESIAN_POINT('Origin',(-16.5000000000311,-24.4,-8.05000000002354));
#143386=CARTESIAN_POINT('',(-17.1668459513761,-15.9,-8.71684595136846));
#143387=CARTESIAN_POINT('',(-13.2927206125707,-15.9,-4.84272061256308));
#143388=CARTESIAN_POINT('',(-18.8656854249492,-10.3,-10.4156854249416));
#143389=CARTESIAN_POINT('',(-7.38427091436115,-10.3,1.06572908564645));
#143390=CARTESIAN_POINT('',(-18.8656854249492,-25.4,-10.4156854249417));
#143391=CARTESIAN_POINT('',(-18.8656854249492,-24.4,-10.4156854249417));
#143392=CARTESIAN_POINT('',(-16.7343145750813,-25.4,-8.28431457507368));
#143393=CARTESIAN_POINT('',(-10.4750000000288,-25.4,-2.02500000002116));
#143394=CARTESIAN_POINT('',(-16.7343145750813,-20.,-8.28431457507368));
#143395=CARTESIAN_POINT('',(-16.7343145750813,-24.4,-8.28431457507368));
#143396=CARTESIAN_POINT('',(-17.1668459513761,-20.,-8.71684595136846));
#143397=CARTESIAN_POINT('',(-15.7899218940915,-20.,-7.33992189408395));
#143398=CARTESIAN_POINT('',(-17.1668459513761,-19.9,-8.71684595136846));
#143399=CARTESIAN_POINT('Origin',(-17.5000000000421,-22.8,-9.82772085584933));
#143400=CARTESIAN_POINT('',(-17.5000000000302,-15.9,-11.4373755457745));
#143401=CARTESIAN_POINT('',(-17.5000000000467,-15.9,-9.21712743154979));
#143402=CARTESIAN_POINT('',(-17.5000000000302,-10.3,-11.4373755457745));
#143403=CARTESIAN_POINT('',(-17.5000000000302,-10.3,-11.4373755457745));
#143404=CARTESIAN_POINT('',(-17.500000000174,-10.3,7.93725830003194));
#143405=CARTESIAN_POINT('Origin',(-16.8840032389014,-19.9,-8.99968866384308));
#143406=CARTESIAN_POINT('Origin',(-16.8840032389014,-15.9,-8.99968866384308));
#143407=CARTESIAN_POINT('Origin',(-16.8840032389014,-20.,-8.99968866384308));
#143408=CARTESIAN_POINT('Origin',(-14.6471642557501,-19.9,-9.82495762703391));
#143409=CARTESIAN_POINT('',(-14.1275490134794,-20.,-10.1249576270339));
#143410=CARTESIAN_POINT('',(-14.1275490134794,-19.9,-10.1249576270339));
#143411=CARTESIAN_POINT('Origin',(-14.6471642557501,-20.,-9.82495762703391));
#143412=CARTESIAN_POINT('Origin',(-18.3,-24.4,-10.9813708498909));
#143413=CARTESIAN_POINT('',(-19.1,-10.3,-10.9813708498909));
#143414=CARTESIAN_POINT('Origin',(-18.3,-10.3,-10.9813708498909));
#143415=CARTESIAN_POINT('',(-19.1,-25.4,-10.9813708498909));
#143416=CARTESIAN_POINT('',(-19.1,-24.4,-10.9813708498909));
#143417=CARTESIAN_POINT('Origin',(-18.3,-25.4,-10.9813708498909));
#143418=CARTESIAN_POINT('Origin',(-16.7000000000302,-10.3,-11.4373755457685));
#143419=CARTESIAN_POINT('',(-16.4733788179429,-15.9,-12.2046061759114));
#143420=CARTESIAN_POINT('Origin',(-16.7000000000302,-15.9,-11.4373755457685));
#143421=CARTESIAN_POINT('',(-16.4733788179429,-10.3,-12.2046061759113));
#143422=CARTESIAN_POINT('',(-16.4733788179429,-10.3,-12.2046061759113));
#143423=CARTESIAN_POINT('Origin',(-16.7000000000302,-10.3,-11.4373755457685));
#143424=CARTESIAN_POINT('Origin',(-15.5,-10.3,-15.5));
#143425=CARTESIAN_POINT('',(-13.9781746176887,-15.9,-12.419231543135));
#143426=CARTESIAN_POINT('Origin',(-15.5,-15.9,-15.5));
#143427=CARTESIAN_POINT('',(-13.9781746176887,-10.3,-12.419231543135));
#143428=CARTESIAN_POINT('',(-13.9781746176887,-10.3,-12.419231543135));
#143429=CARTESIAN_POINT('Origin',(-15.5,-10.3,-15.5));
#143430=CARTESIAN_POINT('Origin',(-19.1,-24.4,8.48528137429235));
#143431=CARTESIAN_POINT('',(-19.1,-10.3,-15.5));
#143432=CARTESIAN_POINT('',(-19.1,-10.3,9.07476980792574));
#143433=CARTESIAN_POINT('',(-19.1,-25.4,-15.5));
#143434=CARTESIAN_POINT('',(-19.1,-24.4,-15.5));
#143435=CARTESIAN_POINT('',(-19.1,-25.4,4.01764068713489));
#143436=CARTESIAN_POINT('Origin',(-15.5,-24.4,-15.5));
#143437=CARTESIAN_POINT('',(-15.5,-25.4,-19.1000000000451));
#143438=CARTESIAN_POINT('Origin',(-15.5,-25.4,-15.5));
#143439=CARTESIAN_POINT('',(-15.5,-10.3,-19.1000000000451));
#143440=CARTESIAN_POINT('Origin',(-15.5,-10.3,-15.5));
#143441=CARTESIAN_POINT('',(-15.5,-24.4,-19.1000000000451));
#143442=CARTESIAN_POINT('Origin',(-15.5,-20.8,-15.5));
#143443=CARTESIAN_POINT('',(-12.7,-20.8,-15.5));
#143444=CARTESIAN_POINT('Origin',(-15.5,-20.8,-15.5));
#143445=CARTESIAN_POINT('',(-17.1,-20.8,-15.5));
#143446=CARTESIAN_POINT('Origin',(-15.5,-20.8,-15.5));
#143447=CARTESIAN_POINT('Origin',(-15.5,-24.4,-15.5));
#143448=CARTESIAN_POINT('',(-17.1,-10.3,-15.5));
#143449=CARTESIAN_POINT('Origin',(-15.5,-10.3,-15.5));
#143450=CARTESIAN_POINT('',(-17.1,-24.4,-15.5));
#143451=CARTESIAN_POINT('Origin',(-15.5,-24.4,-15.5));
#143452=CARTESIAN_POINT('',(-12.7,-25.4,-15.5));
#143453=CARTESIAN_POINT('Origin',(-15.5,-25.4,-15.5));
#143454=CARTESIAN_POINT('',(-12.7,-24.4,-15.5));
#143455=CARTESIAN_POINT('Origin',(10.9,-22.1,-11.6000000000162));
#143456=CARTESIAN_POINT('',(10.9,-22.1,-12.5077037206369));
#143457=CARTESIAN_POINT('',(10.9,-22.1,-12.5077037206369));
#143458=CARTESIAN_POINT('',(10.9,-22.1,-15.1));
#143459=CARTESIAN_POINT('',(10.9,-22.1,-6.02500000001941));
#143460=CARTESIAN_POINT('',(10.9,-10.3,-15.1));
#143461=CARTESIAN_POINT('',(10.9,-22.1,-15.1));
#143462=CARTESIAN_POINT('',(10.9,-10.3,-13.800000000037));
#143463=CARTESIAN_POINT('',(10.9,-10.3,-11.6000000000162));
#143464=CARTESIAN_POINT('',(10.9,-15.9,-13.800000000037));
#143465=CARTESIAN_POINT('',(10.9,-18.9,-13.800000000037));
#143466=CARTESIAN_POINT('',(10.9,-15.9,-12.650000000037));
#143467=CARTESIAN_POINT('',(10.9,-15.9,-10.1032670035799));
#143468=CARTESIAN_POINT('',(10.9,-20.,-12.650000000037));
#143469=CARTESIAN_POINT('',(10.9,-21.,-12.650000000037));
#143470=CARTESIAN_POINT('',(10.9,-20.,-12.1857384988752));
#143471=CARTESIAN_POINT('',(10.9,-20.,-6.02500000001941));
#143472=CARTESIAN_POINT('',(10.9,-21.,-12.1857384988752));
#143473=CARTESIAN_POINT('Origin',(11.3,-22.1,-12.5077037206369));
#143474=CARTESIAN_POINT('',(11.6304347826087,-22.1,-12.7331207884076));
#143475=CARTESIAN_POINT('',(11.6304347826087,-22.1,-12.7331207884076));
#143476=CARTESIAN_POINT('Origin',(11.3,-22.1,-12.5077037206369));
#143477=CARTESIAN_POINT('Origin',(15.1,-22.1,-15.1));
#143478=CARTESIAN_POINT('',(15.1472108071229,-22.1,-10.9002653488952));
#143479=CARTESIAN_POINT('',(15.1472108071229,-22.1,-10.9002653488952));
#143480=CARTESIAN_POINT('Origin',(15.1,-22.1,-15.1));
#143481=CARTESIAN_POINT('Origin',(15.1562033418129,-22.1,-10.1003158915419));
#143482=CARTESIAN_POINT('Origin',(15.1562033418129,-22.1,-10.1003158915419));
#143483=CARTESIAN_POINT('Origin',(10.5,-21.,-12.650000000037));
#143484=CARTESIAN_POINT('',(10.5,-15.9,-12.250000000037));
#143485=CARTESIAN_POINT('Origin',(10.5,-15.9,-12.650000000037));
#143486=CARTESIAN_POINT('',(10.5,-20.,-12.250000000037));
#143487=CARTESIAN_POINT('',(10.5,-21.,-12.250000000037));
#143488=CARTESIAN_POINT('Origin',(10.5,-20.,-12.650000000037));
#143489=CARTESIAN_POINT('Origin',(18.3,-24.4,-10.9813708499319));
#143490=CARTESIAN_POINT('',(18.8656854249492,-25.4,-10.4156854249827));
#143491=CARTESIAN_POINT('',(19.1,-25.4,-10.9813708499319));
#143492=CARTESIAN_POINT('Origin',(18.3,-25.4,-10.9813708499319));
#143493=CARTESIAN_POINT('',(19.1,-22.1,-10.9813708499319));
#143494=CARTESIAN_POINT('',(19.1,-24.4,-10.9813708499319));
#143495=CARTESIAN_POINT('',(18.8656854249492,-22.1,-10.4156854249827));
#143496=CARTESIAN_POINT('Origin',(18.3,-22.1,-10.9813708499319));
#143497=CARTESIAN_POINT('',(18.8656854249492,-24.4,-10.4156854249827));
#143498=CARTESIAN_POINT('Origin',(19.1,-24.4,-10.6500000000335));
#143499=CARTESIAN_POINT('',(16.734314575042,-22.1,-8.28431457507545));
#143500=CARTESIAN_POINT('',(19.1,-22.1,-10.6500000000335));
#143501=CARTESIAN_POINT('',(16.734314575042,-25.4,-8.28431457507545));
#143502=CARTESIAN_POINT('',(16.734314575042,-24.4,-8.28431457507545));
#143503=CARTESIAN_POINT('',(11.7749999999916,-25.4,-3.3250000000251));
#143504=CARTESIAN_POINT('Origin',(10.6016674012397,-21.,-9.20329141491617));
#143505=CARTESIAN_POINT('',(10.1014821344353,-22.1,-9.53467442424494));
#143506=CARTESIAN_POINT('',(10.1014821344353,-21.,-9.53467442424494));
#143507=CARTESIAN_POINT('Origin',(10.6016674012397,-22.1,-9.20329141491617));
#143508=CARTESIAN_POINT('Origin',(19.1,-24.4,18.2));
#143509=CARTESIAN_POINT('',(19.1,-25.4,-15.1));
#143510=CARTESIAN_POINT('',(19.1,-25.4,8.87499999998871));
#143511=CARTESIAN_POINT('',(19.1,-22.1,-15.1));
#143512=CARTESIAN_POINT('',(19.1,-24.4,-15.1));
#143513=CARTESIAN_POINT('',(19.1,-22.1,8.87499999998871));
#143514=CARTESIAN_POINT('Origin',(15.1,-24.4,-15.1));
#143515=CARTESIAN_POINT('',(15.1,-25.4,-19.1));
#143516=CARTESIAN_POINT('Origin',(15.1,-25.4,-15.1));
#143517=CARTESIAN_POINT('',(15.1,-22.1,-19.1));
#143518=CARTESIAN_POINT('',(15.1,-24.4,-19.1));
#143519=CARTESIAN_POINT('Origin',(15.1,-22.1,-15.1));
#143520=CARTESIAN_POINT('Origin',(11.2581254575403,-22.1,-18.3));
#143521=CARTESIAN_POINT('',(11.2581254575403,-10.3,-19.1000000000102));
#143522=CARTESIAN_POINT('',(11.8728253843338,-10.3,-17.788));
#143523=CARTESIAN_POINT('Origin',(11.2581254575403,-10.3,-18.3));
#143524=CARTESIAN_POINT('',(11.8728253843338,-22.1,-17.788));
#143525=CARTESIAN_POINT('',(11.8728253843338,-22.1,-17.788));
#143526=CARTESIAN_POINT('',(11.2581254575403,-22.1,-19.1));
#143527=CARTESIAN_POINT('Origin',(11.2581254575403,-22.1,-18.3));
#143528=CARTESIAN_POINT('',(11.2581254575403,-22.1,-19.1));
#143529=CARTESIAN_POINT('Origin',(15.1,-22.1,-15.1));
#143530=CARTESIAN_POINT('Origin',(15.1,-10.3,-15.1));
#143531=CARTESIAN_POINT('Origin',(15.1,-22.1,-15.1));
#143532=CARTESIAN_POINT('Origin',(15.1,-24.4,-15.1));
#143533=CARTESIAN_POINT('',(13.55,-22.1,-15.1));
#143534=CARTESIAN_POINT('Origin',(15.1,-22.1,-15.1));
#143535=CARTESIAN_POINT('',(13.55,-25.4,-15.1));
#143536=CARTESIAN_POINT('',(13.55,-24.4,-15.1));
#143537=CARTESIAN_POINT('Origin',(15.1,-25.4,-15.1));
#143538=CARTESIAN_POINT('Origin',(10.5,-18.9,-13.800000000037));
#143539=CARTESIAN_POINT('',(10.5,-10.3,-13.400000000037));
#143540=CARTESIAN_POINT('Origin',(10.5,-10.3,-13.800000000037));
#143541=CARTESIAN_POINT('',(10.5,-15.9,-13.400000000037));
#143542=CARTESIAN_POINT('',(10.5,-18.9,-13.400000000037));
#143543=CARTESIAN_POINT('Origin',(10.5,-15.9,-13.800000000037));
#143544=CARTESIAN_POINT('Origin',(0.0099462365591374,-15.7,-9.20072405893627));
#143545=CARTESIAN_POINT('',(0.634274193548385,-15.9,-8.78513459549712));
#143546=CARTESIAN_POINT('',(0.634274193548384,-10.3,-8.78513459549712));
#143547=CARTESIAN_POINT('',(0.634274193548385,-15.7,-8.78513459549712));
#143548=CARTESIAN_POINT('',(-0.616835877496162,-10.3,-8.7888452157064));
#143549=CARTESIAN_POINT('Origin',(0.0099462365591374,-10.3,-9.20072405893626));
#143550=CARTESIAN_POINT('',(-0.616835877496162,-15.9,-8.7888452157064));
#143551=CARTESIAN_POINT('',(-0.616835877496162,-15.7,-8.7888452157064));
#143552=CARTESIAN_POINT('Origin',(0.0099462365591374,-15.9,-9.20072405893627));
#143553=CARTESIAN_POINT('Origin',(5.65685424949238,-12.5431457505076,-17.500000000019));
#143554=CARTESIAN_POINT('',(3.15685424949238,-12.5431457505076,-12.8620372432944));
#143555=CARTESIAN_POINT('',(8.15685424949238,-12.5431457505076,-14.5481534330082));
#143556=CARTESIAN_POINT('Ctrl Pts',(3.15685424949238,-12.5431457505076,
-12.8620372432944));
#143557=CARTESIAN_POINT('Ctrl Pts',(3.15685424949238,-12.8592320850127,
-12.8620372432944));
#143558=CARTESIAN_POINT('Ctrl Pts',(3.22047042900536,-13.1914168687361,
-12.9023109536184));
#143559=CARTESIAN_POINT('Ctrl Pts',(3.46810331101024,-13.7943820582662,
-13.0496463732524));
#143560=CARTESIAN_POINT('Ctrl Pts',(3.65182681306313,-14.0656238936063,
-13.1553086621643));
#143561=CARTESIAN_POINT('Ctrl Pts',(4.08156538511786,-14.5109362958629,
-13.3821704208394));
#143562=CARTESIAN_POINT('Ctrl Pts',(4.36420178144363,-14.7097688956392,
-13.5212507616241));
#143563=CARTESIAN_POINT('Ctrl Pts',(4.98866328596235,-14.9759892088894,
-13.7905365871133));
#143564=CARTESIAN_POINT('Ctrl Pts',(5.33083836910257,-15.0431457505076,
-13.9201585567324));
#143565=CARTESIAN_POINT('Ctrl Pts',(5.96402984326142,-15.0431457505076,
-14.1274260237179));
#143566=CARTESIAN_POINT('Ctrl Pts',(6.29726352242101,-14.9828471682561,
-14.2207295472445));
#143567=CARTESIAN_POINT('Ctrl Pts',(6.91708557876398,-14.7281135426884,
-14.3664199959765));
#143568=CARTESIAN_POINT('Ctrl Pts',(7.20340848989777,-14.5334551117466,
-14.4195445895854));
#143569=CARTESIAN_POINT('Ctrl Pts',(7.64935577171109,-14.0848586172969,
-14.4907101386031));
#143570=CARTESIAN_POINT('Ctrl Pts',(7.84056457463014,-13.8048197236649,
-14.5143922650254));
#143571=CARTESIAN_POINT('Ctrl Pts',(8.09431374793703,-13.1906049475643,
-14.5427449864562));
#143572=CARTESIAN_POINT('Ctrl Pts',(8.15685424949238,-12.8564634012673,
-14.5481534330082));
#143573=CARTESIAN_POINT('Ctrl Pts',(8.15685424949238,-12.5431457505076,
-14.5481534330082));
#143574=CARTESIAN_POINT('',(3.15685424949238,-12.5431457505076,-11.4163656902917));
#143575=CARTESIAN_POINT('',(3.15685424949238,-12.5431457505076,-17.5000000000137));
#143576=CARTESIAN_POINT('',(8.15685424949238,-12.5431457505076,-13.3421101999983));
#143577=CARTESIAN_POINT('Ctrl Pts',(8.15685424949238,-12.5431457505076,
-13.3421101999983));
#143578=CARTESIAN_POINT('Ctrl Pts',(8.15685424949238,-12.8578774912135,
-13.3421101999983));
#143579=CARTESIAN_POINT('Ctrl Pts',(8.09374219603427,-13.1934037608601,
-13.3360182818923));
#143580=CARTESIAN_POINT('Ctrl Pts',(7.83801789221978,-13.8095513827507,
-13.3040436400873));
#143581=CARTESIAN_POINT('Ctrl Pts',(7.64540523586579,-14.0901286700669,
-13.2773205739759));
#143582=CARTESIAN_POINT('Ctrl Pts',(7.19727521652421,-14.5382586894085,
-13.1970274688756));
#143583=CARTESIAN_POINT('Ctrl Pts',(6.91043414045708,-14.7317662324076,
-13.1371819992974));
#143584=CARTESIAN_POINT('Ctrl Pts',(6.29202188533623,-14.9840644227757,
-12.9734658623863));
#143585=CARTESIAN_POINT('Ctrl Pts',(5.96078348705636,-15.0431457505076,
-12.8687874210152));
#143586=CARTESIAN_POINT('Ctrl Pts',(5.32706036423454,-15.0431457505076,
-12.6341908129028));
#143587=CARTESIAN_POINT('Ctrl Pts',(4.98261630817213,-14.9745611086902,
-12.4857870053569));
#143588=CARTESIAN_POINT('Ctrl Pts',(4.35583159298622,-14.7050239351627,
-12.1764316966991));
#143589=CARTESIAN_POINT('Ctrl Pts',(4.07305532958835,-14.50439870059,-12.0160781324946));
#143590=CARTESIAN_POINT('Ctrl Pts',(3.64746690731458,-14.0589639276313,
-11.755750359458));
#143591=CARTESIAN_POINT('Ctrl Pts',(3.46630265431125,-13.7906444571559,
-11.6345025681409));
#143592=CARTESIAN_POINT('Ctrl Pts',(3.22082631848395,-13.1916327737242,
-11.4639114195569));
#143593=CARTESIAN_POINT('Ctrl Pts',(3.15685424949238,-12.8602908531128,
-11.4163656902917));
#143594=CARTESIAN_POINT('Ctrl Pts',(3.15685424949238,-12.5431457505076,
-11.4163656902917));
#143595=CARTESIAN_POINT('',(8.15685424949238,-12.5431457505076,-17.5000000000052));
#143596=CARTESIAN_POINT('Origin',(-5.65685424949238,-12.5431457505076,-17.500000000019));
#143597=CARTESIAN_POINT('',(-8.15685424949239,-12.5431457505076,-13.4316618717243));
#143598=CARTESIAN_POINT('',(-8.15685424949238,-12.5431457505076,-17.5000000000328));
#143599=CARTESIAN_POINT('',(-3.15685424949238,-12.5431457505076,-11.4670924738648));
#143600=CARTESIAN_POINT('Ctrl Pts',(-3.15685424949238,-12.5431457505076,
-11.4670924738648));
#143601=CARTESIAN_POINT('Ctrl Pts',(-3.15685424949238,-12.8710195758623,
-11.4670924738648));
#143602=CARTESIAN_POINT('Ctrl Pts',(-3.22511540251142,-13.2121346615079,
-11.5183801889379));
#143603=CARTESIAN_POINT('Ctrl Pts',(-3.48502968752171,-13.8253626051227,
-11.7004217329402));
#143604=CARTESIAN_POINT('Ctrl Pts',(-3.6763649683173,-14.0981903752653,
-11.8292149981844));
#143605=CARTESIAN_POINT('Ctrl Pts',(-4.11108111624766,-14.5329065231956,
-12.0956632706648));
#143606=CARTESIAN_POINT('Ctrl Pts',(-4.38898639276768,-14.7231999641409,
-12.253689661289));
#143607=CARTESIAN_POINT('Ctrl Pts',(-5.00163457398632,-14.9784717317639,
-12.5584845046953));
#143608=CARTESIAN_POINT('Ctrl Pts',(-5.33677055768477,-15.0431457505076,
-12.7047172810065));
#143609=CARTESIAN_POINT('Ctrl Pts',(-5.9621407575736,-15.0431457505076,
-12.9409762725843));
#143610=CARTESIAN_POINT('Ctrl Pts',(-6.29493995959754,-14.9835365833956,
-13.0486345344632));
#143611=CARTESIAN_POINT('Ctrl Pts',(-6.9160341250112,-14.7288097484239,
-13.2176887423056));
#143612=CARTESIAN_POINT('Ctrl Pts',(-7.20398399968078,-14.5333922588975,
-13.2798994668974));
#143613=CARTESIAN_POINT('Ctrl Pts',(-7.65043593866441,-14.0832724915651,
-13.3632649111085));
#143614=CARTESIAN_POINT('Ctrl Pts',(-7.84118079530232,-13.8036434650245,
-13.3912900060078));
#143615=CARTESIAN_POINT('Ctrl Pts',(-8.09439086444467,-13.1901020782128,
-13.4250787866805));
#143616=CARTESIAN_POINT('Ctrl Pts',(-8.15685424949238,-12.85623436387,-13.4316618717243));
#143617=CARTESIAN_POINT('Ctrl Pts',(-8.15685424949238,-12.5431457505076,
-13.4316618717243));
#143618=CARTESIAN_POINT('',(-3.15685424949238,-12.5431457505076,-17.5000000000243));
#143619=CARTESIAN_POINT('Origin',(-5.65685424949238,-12.5431457505076,-19.1));
#143620=CARTESIAN_POINT('',(-6.95685424949238,-12.5431457505076,-19.1));
#143621=CARTESIAN_POINT('Origin',(-5.65685424949238,-12.5431457505076,-19.1));
#143622=CARTESIAN_POINT('',(-6.95685424949238,-12.5431457505076,-16.700000000013));
#143623=CARTESIAN_POINT('',(-6.95685424949238,-12.5431457505076,-19.1));
#143624=CARTESIAN_POINT('Origin',(-5.65685424949238,-12.5431457505076,-16.700000000013));
#143625=CARTESIAN_POINT('Origin',(-1.28238570254272E-15,-12.6715728752538,
-15.900000000019));
#143626=CARTESIAN_POINT('',(-4.55308926455237,-10.3,-15.9000000000267));
#143627=CARTESIAN_POINT('',(-6.76061923443239,-10.3,-15.9000000000304));
#143628=CARTESIAN_POINT('',(-2.27654463227754,-10.3,-15.9000000000228));
#143629=CARTESIAN_POINT('Origin',(-5.65685424949238,-12.5431457505076,-15.900000000019));
#143630=CARTESIAN_POINT('',(-7.75685424949508,-12.5431457505076,-15.9000000000321));
#143631=CARTESIAN_POINT('Origin',(-5.65685424949373,-12.5431457505076,-15.9000000000285));
#143632=CARTESIAN_POINT('Origin',(-5.65685424949306,-12.5431457505076,-16.3000000000208));
#143633=CARTESIAN_POINT('',(-7.35685424949373,-12.5431457505076,-16.3000000000225));
#143634=CARTESIAN_POINT('Origin',(5.65685424949238,-12.5431457505076,-19.1));
#143635=CARTESIAN_POINT('',(4.35685424949238,-12.5431457505076,-19.1));
#143636=CARTESIAN_POINT('Origin',(5.65685424949238,-12.5431457505076,-19.1));
#143637=CARTESIAN_POINT('',(4.35685424949238,-12.5431457505076,-16.7000000000321));
#143638=CARTESIAN_POINT('',(4.35685424949238,-12.5431457505076,-19.1));
#143639=CARTESIAN_POINT('Origin',(5.65685424949238,-12.5431457505076,-16.7000000000321));
#143640=CARTESIAN_POINT('Origin',(-1.28238570254272E-15,-12.6715728752538,
-15.900000000019));
#143641=CARTESIAN_POINT('',(6.76061923443239,-10.3,-15.9000000000076));
#143642=CARTESIAN_POINT('',(4.55308926455238,-10.3,-15.9000000000113));
#143643=CARTESIAN_POINT('',(3.38030961721484,-10.3,-15.9000000000133));
#143644=CARTESIAN_POINT('Origin',(5.65685424949238,-12.5431457505076,-15.900000000019));
#143645=CARTESIAN_POINT('',(3.55685424948968,-12.5431457505076,-15.900000000013));
#143646=CARTESIAN_POINT('Origin',(5.65685424949103,-12.5431457505076,-15.9000000000094));
#143647=CARTESIAN_POINT('Origin',(5.65685424949171,-12.5431457505076,-16.3000000000208));
#143648=CARTESIAN_POINT('',(3.95685424949103,-12.5431457505076,-16.3000000000225));
#143649=CARTESIAN_POINT('Origin',(-5.65685424949103,-12.5431457505076,-16.7000000000401));
#143650=CARTESIAN_POINT('Ctrl Pts',(-2.22490186897899,-10.3,-17.5000000000366));
#143651=CARTESIAN_POINT('Ctrl Pts',(-3.67120009961655,-10.3,-16.2893593523635));
#143652=CARTESIAN_POINT('Ctrl Pts',(-4.55308926462462,-10.3,-15.9000000000179));
#143653=CARTESIAN_POINT('Ctrl Pts',(-6.76061923434026,-10.3,-15.9000000000128));
#143654=CARTESIAN_POINT('Ctrl Pts',(-7.64250839935299,-10.3,-16.2893593523584));
#143655=CARTESIAN_POINT('Ctrl Pts',(-9.08880663000172,-10.3,-17.5000000000493));
#143656=CARTESIAN_POINT('Origin',(-1.72162677917566E-16,-23.3784271247462,
-15.900000000019));
#143657=CARTESIAN_POINT('',(-7.08117906942998,-25.4,-15.9));
#143658=CARTESIAN_POINT('',(-4.23252942955478,-25.4,-15.9));
#143659=CARTESIAN_POINT('Origin',(-5.65685424949238,-23.8568542494924,-15.900000000019));
#143660=CARTESIAN_POINT('',(-3.15685424949238,-25.3999994322658,-15.9000000000148));
#143661=CARTESIAN_POINT('',(1.74566039757947E-12,-25.4,-15.9000000000095));
#143662=CARTESIAN_POINT('',(-3.15685424949238,-23.8568542494924,-15.9000000000148));
#143663=CARTESIAN_POINT('',(-3.15685424949238,-24.389213278506,-15.9000000000148));
#143664=CARTESIAN_POINT('',(-8.15685424949238,-23.8568542494924,-15.9000000000232));
#143665=CARTESIAN_POINT('Origin',(-5.65685424949238,-23.8568542494924,-15.900000000019));
#143666=CARTESIAN_POINT('',(-8.15685424949238,-25.3999994322658,-15.9000000000232));
#143667=CARTESIAN_POINT('',(-8.15685424949238,-23.6176406871193,-15.9000000000232));
#143668=CARTESIAN_POINT('',(1.74566039757947E-12,-25.4,-15.9000000000095));
#143669=CARTESIAN_POINT('Origin',(-1.72162677917566E-16,-23.3784271247462,
-15.900000000019));
#143670=CARTESIAN_POINT('',(4.23252942955478,-25.4,-15.9));
#143671=CARTESIAN_POINT('',(7.08117906942998,-25.4,-15.9));
#143672=CARTESIAN_POINT('Origin',(5.65685424949238,-23.8568542494924,-15.900000000019));
#143673=CARTESIAN_POINT('',(8.15685424949238,-25.4,-15.8999999999957));
#143674=CARTESIAN_POINT('',(1.74566039757947E-12,-25.4,-15.9000000000095));
#143675=CARTESIAN_POINT('',(8.15685424949238,-23.8568542494924,-15.8999999999957));
#143676=CARTESIAN_POINT('',(8.15685424949238,-24.3892135623731,-15.8999999999957));
#143677=CARTESIAN_POINT('',(3.15685424949238,-23.8568542494924,-15.9000000000041));
#143678=CARTESIAN_POINT('Origin',(5.65685424949238,-23.8568542494924,-15.900000000019));
#143679=CARTESIAN_POINT('',(3.15685424949238,-25.4,-15.9000000000041));
#143680=CARTESIAN_POINT('',(3.15685424949238,-23.6176406871193,-15.9000000000041));
#143681=CARTESIAN_POINT('',(1.74566039757947E-12,-25.4,-15.9000000000095));
#143682=CARTESIAN_POINT('Origin',(-3.15685424949238,-25.3999994322658,-15.9000000000148));
#143683=CARTESIAN_POINT('',(-3.15685424949238,-25.3999994322658,-12.9000000000148));
#143684=CARTESIAN_POINT('',(-3.15685424949238,-25.4,-8.17500000001868));
#143685=CARTESIAN_POINT('',(-3.15685424949238,-23.8568542494924,-12.9000000000148));
#143686=CARTESIAN_POINT('',(-3.15685424949238,-24.389213278506,-12.9000000000148));
#143687=CARTESIAN_POINT('',(-3.15685424949238,-23.8568542494924,-15.9000000000148));
#143688=CARTESIAN_POINT('Origin',(-5.65685424949238,-23.8568542494924,-15.9000000000095));
#143689=CARTESIAN_POINT('',(-3.42078627199525,-22.7388202607371,-12.9000000000057));
#143690=CARTESIAN_POINT('Origin',(-5.65685424949238,-23.8568542494924,-12.9000000000095));
#143691=CARTESIAN_POINT('',(-8.15685424949238,-23.8568542494924,-12.9000000000232));
#143692=CARTESIAN_POINT('Origin',(-5.65685424949238,-23.8568542494924,-12.9000000000095));
#143693=CARTESIAN_POINT('',(-8.15685424949238,-23.8568542494924,-15.9000000000232));
#143694=CARTESIAN_POINT('Origin',(-8.15685424949238,-23.8568542494924,-15.9000000000232));
#143695=CARTESIAN_POINT('',(-8.15685424949238,-25.3999994322658,-12.9000000000232));
#143696=CARTESIAN_POINT('',(-8.15685424949238,-23.6176406871193,-12.9000000000232));
#143697=CARTESIAN_POINT('',(-8.15685424949238,-25.4,-8.1750000000229));
#143698=CARTESIAN_POINT('Origin',(8.15685424949238,-25.4,-15.8999999999957));
#143699=CARTESIAN_POINT('',(8.15685424949238,-25.4,-12.8999999999957));
#143700=CARTESIAN_POINT('',(8.15685424949238,-25.4,-8.17500000000913));
#143701=CARTESIAN_POINT('',(8.15685424949238,-23.8568542494924,-12.8999999999957));
#143702=CARTESIAN_POINT('',(8.15685424949238,-24.3892135623731,-12.8999999999957));
#143703=CARTESIAN_POINT('',(8.15685424949238,-23.8568542494924,-15.8999999999957));
#143704=CARTESIAN_POINT('Origin',(5.65685424949238,-23.8568542494924,-15.9000000000095));
#143705=CARTESIAN_POINT('',(7.89292222699332,-22.7388202607448,-12.9000000000057));
#143706=CARTESIAN_POINT('Origin',(5.65685424949238,-23.8568542494924,-12.9000000000095));
#143707=CARTESIAN_POINT('',(3.15685424949238,-23.8568542494924,-12.9000000000041));
#143708=CARTESIAN_POINT('Origin',(5.65685424949238,-23.8568542494924,-12.9000000000095));
#143709=CARTESIAN_POINT('',(3.15685424949238,-23.8568542494924,-15.9000000000041));
#143710=CARTESIAN_POINT('Origin',(3.15685424949238,-23.8568542494924,-15.9000000000041));
#143711=CARTESIAN_POINT('',(3.15685424949238,-25.4,-12.9000000000041));
#143712=CARTESIAN_POINT('',(3.15685424949238,-23.6176406871193,-12.9000000000041));
#143713=CARTESIAN_POINT('',(3.15685424949238,-25.4,-8.17500000001335));
#143714=CARTESIAN_POINT('Origin',(5.65685424949238,-23.8568542494924,-12.8999999999999));
#143715=CARTESIAN_POINT('Origin',(5.65685424949238,-23.8568542494924,-12.8999999999999));
#143716=CARTESIAN_POINT('',(7.10022992246644,-22.4134785765183,-11.4566243270258));
#143717=CARTESIAN_POINT('Origin',(5.65685424949238,-23.8568542494924,-12.8999999999999));
#143718=CARTESIAN_POINT('Origin',(5.65685424949238,-24.6284271247462,-12.8999999999999));
#143719=CARTESIAN_POINT('Origin',(5.65685424949238,-25.4,-12.8999999999999));
#143720=CARTESIAN_POINT('Origin',(-5.65685424949238,-23.8568542494924,-12.900000000019));
#143721=CARTESIAN_POINT('Origin',(-5.65685424949238,-23.8568542494924,-12.900000000019));
#143722=CARTESIAN_POINT('',(-4.21347857651832,-22.4134785765183,-11.4566243270449));
#143723=CARTESIAN_POINT('Origin',(-5.65685424949238,-23.8568542494924,-12.900000000019));
#143724=CARTESIAN_POINT('Origin',(-5.65685424949238,-24.6284268408791,-12.900000000019));
#143725=CARTESIAN_POINT('Origin',(-5.65685424949238,-25.4,-12.900000000019));
#143726=CARTESIAN_POINT('Origin',(4.35685424949238,-23.8568542494924,-19.1));
#143727=CARTESIAN_POINT('',(4.35685424949238,-23.8568542494924,-16.7));
#143728=CARTESIAN_POINT('',(4.35685424949238,-25.4,-15.9822540280527));
#143729=CARTESIAN_POINT('Ctrl Pts',(4.35685424949238,-23.8568542494924,
-16.7));
#143730=CARTESIAN_POINT('Ctrl Pts',(4.35685424949238,-24.461508581868,-16.7));
#143731=CARTESIAN_POINT('Ctrl Pts',(4.35685424949238,-25.4,-15.9822540280527));
#143732=CARTESIAN_POINT('',(4.35685424949238,-25.4,-19.1));
#143733=CARTESIAN_POINT('',(4.35685424949238,-25.4,-9.77500000001129));
#143734=CARTESIAN_POINT('',(4.35685424949238,-23.8568542494924,-19.1));
#143735=CARTESIAN_POINT('',(4.35685424949238,-24.1284271247462,-19.1));
#143736=CARTESIAN_POINT('',(4.35685424949238,-23.8568542494924,-19.1));
#143737=CARTESIAN_POINT('Origin',(5.65685424949238,-23.8568542494924,-19.1));
#143738=CARTESIAN_POINT('',(6.95685424949238,-23.8568542494924,-16.7));
#143739=CARTESIAN_POINT('Origin',(5.65685424949238,-23.8568542494924,-16.7));
#143740=CARTESIAN_POINT('',(6.95685424949238,-23.8568542494924,-19.1));
#143741=CARTESIAN_POINT('Origin',(5.65685424949238,-23.8568542494924,-19.1));
#143742=CARTESIAN_POINT('',(6.95685424949238,-23.8568542494924,-19.1));
#143743=CARTESIAN_POINT('Origin',(6.95685424949238,-25.4,-19.1));
#143744=CARTESIAN_POINT('',(6.95685424949238,-25.4,-15.9822540280527));
#143745=CARTESIAN_POINT('Ctrl Pts',(6.95685424949238,-25.4,-15.9822540280527));
#143746=CARTESIAN_POINT('Ctrl Pts',(6.95685424949238,-24.4615085818681,
-16.7));
#143747=CARTESIAN_POINT('Ctrl Pts',(6.95685424949238,-23.8568542494924,
-16.7));
#143748=CARTESIAN_POINT('',(6.95685424949238,-25.4,-19.1));
#143749=CARTESIAN_POINT('',(6.95685424949238,-24.9,-19.1));
#143750=CARTESIAN_POINT('',(6.95685424949238,-25.4,-9.77500000001129));
#143751=CARTESIAN_POINT('Origin',(5.65685424949238,-23.8568542494924,-16.3));
#143752=CARTESIAN_POINT('Ctrl Pts',(7.08117906942999,-25.4,-15.9));
#143753=CARTESIAN_POINT('Ctrl Pts',(7.01777493434072,-25.4,-15.9430038491878));
#143754=CARTESIAN_POINT('Ctrl Pts',(6.95685424949238,-25.4,-15.9822540280527));
#143755=CARTESIAN_POINT('Ctrl Pts',(4.35685424949238,-25.4,-15.9822540280527));
#143756=CARTESIAN_POINT('Ctrl Pts',(4.29593356464403,-25.4,-15.9430038491878));
#143757=CARTESIAN_POINT('Ctrl Pts',(4.23252942955477,-25.4,-15.9));
#143758=CARTESIAN_POINT('Origin',(-6.95685424949238,-23.8568542494924,-19.1));
#143759=CARTESIAN_POINT('',(-6.95685424949238,-23.8568542494924,-16.7));
#143760=CARTESIAN_POINT('',(-6.95685424949238,-25.4,-15.9822540280527));
#143761=CARTESIAN_POINT('Ctrl Pts',(-6.95685424949238,-23.8568542494924,
-16.7));
#143762=CARTESIAN_POINT('Ctrl Pts',(-6.95685424949238,-24.4615085818681,
-16.7));
#143763=CARTESIAN_POINT('Ctrl Pts',(-6.95685424949238,-25.4,-15.9822540280527));
#143764=CARTESIAN_POINT('',(-6.95685424949238,-25.3999994322658,-19.1));
#143765=CARTESIAN_POINT('',(-6.95685424949238,-25.4,-9.77500000001129));
#143766=CARTESIAN_POINT('',(-6.95685424949238,-23.8568542494924,-19.1));
#143767=CARTESIAN_POINT('',(-6.95685424949238,-24.1284271247462,-19.1));
#143768=CARTESIAN_POINT('',(-6.95685424949238,-23.8568542494924,-19.1));
#143769=CARTESIAN_POINT('Origin',(-5.65685424949238,-23.8568542494924,-19.1));
#143770=CARTESIAN_POINT('',(-4.35685424949238,-23.8568542494924,-16.7));
#143771=CARTESIAN_POINT('Origin',(-5.65685424949238,-23.8568542494924,-16.7));
#143772=CARTESIAN_POINT('',(-4.35685424949238,-23.8568542494924,-19.1));
#143773=CARTESIAN_POINT('Origin',(-5.65685424949238,-23.8568542494924,-19.1));
#143774=CARTESIAN_POINT('',(-4.35685424949238,-23.8568542494924,-19.1));
#143775=CARTESIAN_POINT('Origin',(-4.35685424949238,-25.3999994322658,-19.1));
#143776=CARTESIAN_POINT('',(-4.35685424949238,-25.4,-15.9822540280527));
#143777=CARTESIAN_POINT('Ctrl Pts',(-4.35685424949238,-25.4,-15.9822540280527));
#143778=CARTESIAN_POINT('Ctrl Pts',(-4.35685424949238,-24.4615085818681,
-16.7));
#143779=CARTESIAN_POINT('Ctrl Pts',(-4.35685424949238,-23.8568542494924,
-16.7));
#143780=CARTESIAN_POINT('',(-4.35685424949238,-25.3999994322658,-19.1));
#143781=CARTESIAN_POINT('',(-4.35685424949238,-24.8999997161328,-19.1));
#143782=CARTESIAN_POINT('',(-4.35685424949239,-25.4,-9.77500000001129));
#143783=CARTESIAN_POINT('Origin',(-5.65685424949238,-23.8568542494924,-16.3));
#143784=CARTESIAN_POINT('Ctrl Pts',(-4.23252942955477,-25.4,-15.9));
#143785=CARTESIAN_POINT('Ctrl Pts',(-4.29593356464405,-25.4,-15.9430038491878));
#143786=CARTESIAN_POINT('Ctrl Pts',(-4.35685424949239,-25.4,-15.9822540280527));
#143787=CARTESIAN_POINT('Ctrl Pts',(-6.95685424949238,-25.4,-15.9822540280527));
#143788=CARTESIAN_POINT('Ctrl Pts',(-7.01777493434072,-25.4,-15.9430038491878));
#143789=CARTESIAN_POINT('Ctrl Pts',(-7.08117906942999,-25.4,-15.9));
#143790=CARTESIAN_POINT('Origin',(10.9,-15.7,-13.400000000037));
#143791=CARTESIAN_POINT('',(9.25,-10.3,-13.400000000037));
#143792=CARTESIAN_POINT('',(4.12984378812245,-10.3,-13.400000000037));
#143793=CARTESIAN_POINT('',(9.25,-15.9,-13.400000000037));
#143794=CARTESIAN_POINT('',(9.25,-21.1,-13.400000000037));
#143795=CARTESIAN_POINT('',(3.8928257784653,-15.9,-13.400000000037));
#143796=CARTESIAN_POINT('Origin',(10.9,-19.9,-12.250000000037));
#143797=CARTESIAN_POINT('',(3.8928257784653,-15.9,-12.250000000037));
#143798=CARTESIAN_POINT('',(4.12984378812245,-20.,-12.250000000037));
#143799=CARTESIAN_POINT('Origin',(-1.26287869055635E-16,-18.2,-19.1));
#143800=CARTESIAN_POINT('',(-0.790053763424162,-14.6877621021777,-16.9000000000203));
#143801=CARTESIAN_POINT('Ctrl Pts',(-0.790053763427873,-14.6877621021785,
-16.9000000000213));
#143802=CARTESIAN_POINT('Ctrl Pts',(-0.790053763427873,-14.6877621021785,
-16.9749752755816));
#143803=CARTESIAN_POINT('Ctrl Pts',(-0.804989255950869,-14.6910185364364,
-17.0548386220574));
#143804=CARTESIAN_POINT('Ctrl Pts',(-0.865223395403298,-14.7053831241914,
-17.2013777360166));
#143805=CARTESIAN_POINT('Ctrl Pts',(-0.910511782222757,-14.7166346855472,
-17.2680436277885));
#143806=CARTESIAN_POINT('Ctrl Pts',(-1.01708168610465,-14.7461903939279,
-17.3764937169279));
#143807=CARTESIAN_POINT('Ctrl Pts',(-1.08648661407425,-14.7669551355699,
-17.4238310868093));
#143808=CARTESIAN_POINT('Ctrl Pts',(-1.23615012040654,-14.8179616954849,
-17.485547331143));
#143809=CARTESIAN_POINT('Ctrl Pts',(-1.31633318766185,-14.8483356495151,
-17.5000000000213));
#143810=CARTESIAN_POINT('Ctrl Pts',(-1.39005376342787,-14.8791942943346,
-17.5000000000213));
#143811=CARTESIAN_POINT('',(-3.59005376342416,-18.4674209709877,-19.1));
#143812=CARTESIAN_POINT('',(-0.790053763435527,-14.6877621021802,-12.3613777665646));
#143813=CARTESIAN_POINT('Ctrl Pts',(-0.79005376343553,-14.6877621021802,
-12.3613777665646));
#143814=CARTESIAN_POINT('Ctrl Pts',(-0.790053763435658,-14.6877621021803,
-12.2855065251448));
#143815=CARTESIAN_POINT('Ctrl Pts',(-0.805345661260487,-14.6910942468679,
-12.2047540470466));
#143816=CARTESIAN_POINT('Ctrl Pts',(-0.866899513458881,-14.7057924400671,
-12.0568713431911));
#143817=CARTESIAN_POINT('Ctrl Pts',(-0.913151482487876,-14.7173085072149,
-11.9897519100894));
#143818=CARTESIAN_POINT('Ctrl Pts',(-1.02061424285241,-14.7472351076383,
-11.8822891497248));
#143819=CARTESIAN_POINT('Ctrl Pts',(-1.08953284953172,-14.767936670379,
-11.8359268093953));
#143820=CARTESIAN_POINT('Ctrl Pts',(-1.2378422455355,-14.8185968721662,
-11.7755081825809));
#143821=CARTESIAN_POINT('Ctrl Pts',(-1.31715971249138,-14.8486816239716,
-11.7613777665656));
#143822=CARTESIAN_POINT('Ctrl Pts',(-1.46598670564076,-14.910979012095,
-11.7613777665656));
#143823=CARTESIAN_POINT('Ctrl Pts',(-1.54605981512051,-14.9478478813323,
-11.7765606781301));
#143824=CARTESIAN_POINT('Ctrl Pts',(-1.67832189315571,-15.0144783588798,
-11.8313482828004));
#143825=CARTESIAN_POINT('Ctrl Pts',(-1.73301170809371,-15.0441191690517,
-11.865202730501));
#143826=CARTESIAN_POINT('Ctrl Pts',(-1.77992868114481,-15.0708061916784,
-11.9053102841234));
#143827=CARTESIAN_POINT('',(-0.790053763424162,-14.6877621021777,-19.1));
#143828=CARTESIAN_POINT('Origin',(-3.59005376342686,-10.3,-17.5000000000251));
#143829=CARTESIAN_POINT('Origin',(-0.790053763426861,-10.3,-17.5000000000203));
#143830=CARTESIAN_POINT('',(-0.790053763427873,-10.3,-16.9000000000203));
#143831=CARTESIAN_POINT('',(-0.790053763427873,-10.3,-16.9000000000203));
#143832=CARTESIAN_POINT('',(-0.790053763435531,-10.3,-12.3613777665646));
#143833=CARTESIAN_POINT('',(-0.79005376343553,-10.3,-12.3613777665646));
#143834=CARTESIAN_POINT('',(-0.790053763449776,-10.3,-3.91787087923316));
#143835=CARTESIAN_POINT('Origin',(1.40994623656442,-10.3,-12.3320287107467));
#143836=CARTESIAN_POINT('',(0.809946236564421,-10.3,-12.3320287107477));
#143837=CARTESIAN_POINT('',(1.79710938537606,-10.3,-11.8736569225635));
#143838=CARTESIAN_POINT('Origin',(1.40994623656442,-10.3,-12.3320287107467));
#143839=CARTESIAN_POINT('',(1.79710938537606,-15.0806414350073,-11.8736569225635));
#143840=CARTESIAN_POINT('',(1.79710938537606,-10.3,-11.8736569225635));
#143841=CARTESIAN_POINT('',(0.809946236564415,-14.6922960367392,-12.3320287107477));
#143842=CARTESIAN_POINT('Ctrl Pts',(1.79710938537606,-15.0806414350073,
-11.8736569225635));
#143843=CARTESIAN_POINT('Ctrl Pts',(1.75079494773061,-15.0539589908968,
-11.8345374916201));
#143844=CARTESIAN_POINT('Ctrl Pts',(1.69707204519075,-15.0244494752567,
-11.8015240531292));
#143845=CARTESIAN_POINT('Ctrl Pts',(1.5659413296006,-14.9573677420981,-11.7472096227115));
#143846=CARTESIAN_POINT('Ctrl Pts',(1.48587960880272,-14.9199127536573,
-11.7320287107467));
#143847=CARTESIAN_POINT('Ctrl Pts',(1.33711320367574,-14.8565894593461,
-11.7320287107467));
#143848=CARTESIAN_POINT('Ctrl Pts',(1.25782749360031,-14.825976274775,-11.7461351698937));
#143849=CARTESIAN_POINT('Ctrl Pts',(1.10951031289533,-14.7743390479818,
-11.8065293086185));
#143850=CARTESIAN_POINT('Ctrl Pts',(1.04055362922102,-14.7531894409119,
-11.8528931806663));
#143851=CARTESIAN_POINT('Ctrl Pts',(0.933070797095156,-14.7225913145941,
-11.9603760127921));
#143852=CARTESIAN_POINT('Ctrl Pts',(0.8868166131236,-14.710793680294,-12.0274791631079));
#143853=CARTESIAN_POINT('Ctrl Pts',(0.825248988139974,-14.695721396081,
-12.1753628835624));
#143854=CARTESIAN_POINT('Ctrl Pts',(0.809946236564421,-14.6922960367393,
-12.2561325049032));
#143855=CARTESIAN_POINT('Ctrl Pts',(0.809946236564421,-14.6922960367393,
-12.3320287107467));
#143856=CARTESIAN_POINT('',(0.80994623656442,-10.3,-12.3320287107477));
#143857=CARTESIAN_POINT('Origin',(1.70994623656809,-18.2,-14.5048933931961));
#143858=CARTESIAN_POINT('',(3.6,-18.2,-17.5000000000129));
#143859=CARTESIAN_POINT('',(3.60994623657314,-18.2,-17.5000000000129));
#143860=CARTESIAN_POINT('',(-5.64602728205014,-18.2,-17.5000000000285));
#143861=CARTESIAN_POINT('',(3.60000000001663,-18.2,-13.1237282076557));
#143862=CARTESIAN_POINT('',(3.6,-18.2,-19.1));
#143863=CARTESIAN_POINT('',(3.60994623658205,-18.2,-13.1293002508741));
#143864=CARTESIAN_POINT('Origin',(9.25,-18.2,-3.05000000003699));
#143865=CARTESIAN_POINT('',(3.6099462365668,-18.2,-13.7451470201718));
#143866=CARTESIAN_POINT('Origin',(3.60994623656552,-10.3,-12.9854006471506));
#143867=CARTESIAN_POINT('',(3.60994623657554,-20.7746200619787,-17.5000000000129));
#143868=CARTESIAN_POINT('',(3.60994623657314,-10.3,-17.5000000000129));
#143869=CARTESIAN_POINT('',(3.60994623656576,-20.7746200619886,-13.1293002508268));
#143870=CARTESIAN_POINT('',(3.60994623656576,-10.3,-13.1293002508268));
#143871=CARTESIAN_POINT('',(3.60994623657044,-20.7746200619855,-15.8999999999905));
#143872=CARTESIAN_POINT('Origin',(-1.26287869055635E-16,-18.2,-19.1));
#143873=CARTESIAN_POINT('',(1.40994623657314,-14.8875912676765,-17.5000000000386));
#143874=CARTESIAN_POINT('',(0.809946236575839,-14.6922960367419,-16.9000000000176));
#143875=CARTESIAN_POINT('Ctrl Pts',(1.40994623657213,-14.887591267676,-17.5000000000166));
#143876=CARTESIAN_POINT('Ctrl Pts',(1.33625361239476,-14.8562235692673,
-17.5000000000166));
#143877=CARTESIAN_POINT('Ctrl Pts',(1.25606667560244,-14.8253033748672,
-17.4855585585683));
#143878=CARTESIAN_POINT('Ctrl Pts',(1.1063385789953,-14.7732966653415,-17.4238130856251));
#143879=CARTESIAN_POINT('Ctrl Pts',(1.03687453723727,-14.7520783114986,
-17.3764332109703));
#143880=CARTESIAN_POINT('Ctrl Pts',(0.930320256457108,-14.7218724492534,
-17.2679197801565));
#143881=CARTESIAN_POINT('Ctrl Pts',(0.885069824864685,-14.710356559554,
-17.2012887424176));
#143882=CARTESIAN_POINT('Ctrl Pts',(0.824877328391394,-14.6956402424863,
-17.0548048739472));
#143883=CARTESIAN_POINT('Ctrl Pts',(0.809946236572128,-14.692296036741,
-16.9749620143834));
#143884=CARTESIAN_POINT('Ctrl Pts',(0.809946236572128,-14.692296036741,
-16.9000000000166));
#143885=CARTESIAN_POINT('',(0.809946236575839,-14.6922960367419,-19.1));
#143886=CARTESIAN_POINT('Ctrl Pts',(1.79710938537606,-15.0806414350073,
-11.8736569225635));
#143887=CARTESIAN_POINT('Ctrl Pts',(1.98632462279995,-15.1896511791408,
-12.0334773325729));
#143888=CARTESIAN_POINT('Ctrl Pts',(2.17985487135821,-15.3247214343457,
-12.1860629633352));
#143889=CARTESIAN_POINT('Ctrl Pts',(2.63411012231677,-15.7199744539229,
-12.5234615495083));
#143890=CARTESIAN_POINT('Ctrl Pts',(2.88145248890814,-16.0115207345657,
-12.6881804314593));
#143891=CARTESIAN_POINT('Ctrl Pts',(3.22898189906331,-16.5797619219656,
-12.9082317714475));
#143892=CARTESIAN_POINT('Ctrl Pts',(3.36909827503896,-16.8871060729476,
-12.9912776188885));
#143893=CARTESIAN_POINT('Ctrl Pts',(3.5547431222469,-17.5379457491925,-13.0987837118773));
#143894=CARTESIAN_POINT('Ctrl Pts',(3.6,-17.8814386363522,-13.1237282076074));
#143895=CARTESIAN_POINT('Ctrl Pts',(3.6,-18.2,-13.1237282076074));
#143896=CARTESIAN_POINT('Origin',(-1.26287869055635E-16,-18.2,-17.5000000000409));
#143897=CARTESIAN_POINT('Origin',(0.,-18.2,-12.1));
#143898=CARTESIAN_POINT('',(-2.,-18.2,-12.1));
#143899=CARTESIAN_POINT('Origin',(0.,-18.2,-12.1));
#143900=CARTESIAN_POINT('',(-1.,-18.2,-12.1));
#143901=CARTESIAN_POINT('Origin',(0.,-18.2,-12.1));
#143902=CARTESIAN_POINT('Origin',(0.,-18.2,-19.1));
#143903=CARTESIAN_POINT('',(-2.,-18.2,-19.1));
#143904=CARTESIAN_POINT('Origin',(0.,-18.2,-19.1));
#143905=CARTESIAN_POINT('',(-2.,-18.2,-19.1));
#143906=CARTESIAN_POINT('Origin',(5.65685424949373,-12.5431457505076,-16.7000000000401));
#143907=CARTESIAN_POINT('',(8.95833898688851,-14.9742357383029,-17.5000000000039));
#143908=CARTESIAN_POINT('',(9.07509596432602,-10.3,-17.4885302101201));
#143909=CARTESIAN_POINT('Ctrl Pts',(8.95833898688868,-14.974235738303,-17.5000000000039));
#143910=CARTESIAN_POINT('Ctrl Pts',(8.96684937916237,-14.9626783996845,
-17.5000000000039));
#143911=CARTESIAN_POINT('Ctrl Pts',(8.97504674785079,-14.9511132665156,
-17.4998189890635));
#143912=CARTESIAN_POINT('Ctrl Pts',(9.09671999843394,-14.7737137436823,
-17.4948316381137));
#143913=CARTESIAN_POINT('Ctrl Pts',(9.17373133832194,-14.590460376238,-17.464473403876));
#143914=CARTESIAN_POINT('Ctrl Pts',(9.29933180973145,-14.2051637392862,
-17.3987460174418));
#143915=CARTESIAN_POINT('Ctrl Pts',(9.34518631085098,-14.0026171612565,
-17.3611498632386));
#143916=CARTESIAN_POINT('Ctrl Pts',(9.44789375510663,-13.3797508448848,
-17.2599642528778));
#143917=CARTESIAN_POINT('Ctrl Pts',(9.47008652427947,-12.9456743678109,
-17.2132322747989));
#143918=CARTESIAN_POINT('Ctrl Pts',(9.47008652427947,-12.5431457505076,
-17.2132322747989));
#143919=CARTESIAN_POINT('Ctrl Pts',(9.47008652427947,-12.1406171332043,
-17.2132322747989));
#143920=CARTESIAN_POINT('Ctrl Pts',(9.44789375510637,-11.7065406561306,
-17.2599642528782));
#143921=CARTESIAN_POINT('Ctrl Pts',(9.34518631085064,-11.0836743397588,
-17.3611498632388));
#143922=CARTESIAN_POINT('Ctrl Pts',(9.29933180973091,-10.8811277617293,
-17.3987460174422));
#143923=CARTESIAN_POINT('Ctrl Pts',(9.19248941207167,-10.5533740834192,
-17.4546572053516));
#143924=CARTESIAN_POINT('Ctrl Pts',(9.14049576625509,-10.4233085064875,
-17.4755557135403));
#143925=CARTESIAN_POINT('Ctrl Pts',(9.07509596432527,-10.3000000000004,
-17.4885302101202));
#143926=CARTESIAN_POINT('Ctrl Pts',(9.07509596432612,-10.3,-17.4885302101202));
#143927=CARTESIAN_POINT('Ctrl Pts',(7.63884118065615,-10.3,-16.2877402533004));
#143928=CARTESIAN_POINT('Ctrl Pts',(6.76061923425244,-10.3,-15.8999999999894));
#143929=CARTESIAN_POINT('',(2.22490186900091,-10.3,-17.5000000000152));
#143930=CARTESIAN_POINT('Ctrl Pts',(4.55308926471108,-10.3,-15.9000000000025));
#143931=CARTESIAN_POINT('Ctrl Pts',(3.67120009968434,-10.3,-16.2893593523261));
#143932=CARTESIAN_POINT('Ctrl Pts',(2.22490186900091,-10.3,-17.5000000000152));
#143933=CARTESIAN_POINT('Origin',(5.65685424949508,-12.5431457505076,-17.5000000000095));
#143934=CARTESIAN_POINT('Origin',(0.809946236563033,-10.3,-11.5097867863747));
#143935=CARTESIAN_POINT('',(0.809946236572127,-10.3,-16.9000000000176));
#143936=CARTESIAN_POINT('',(0.809946236572127,-10.3,-16.9000000000176));
#143937=CARTESIAN_POINT('',(0.809946236545172,-10.3,-0.922764272408981));
#143938=CARTESIAN_POINT('Origin',(1.40994623657213,-10.3,-16.9000000000166));
#143939=CARTESIAN_POINT('',(1.40994623657314,-10.3,-17.5000000000166));
#143940=CARTESIAN_POINT('',(1.40994623657314,-10.3,-17.5000000000166));
#143941=CARTESIAN_POINT('Origin',(1.40994623657213,-10.3,-16.9000000000166));
#143942=CARTESIAN_POINT('Origin',(-13.0020008006734,-10.3,-17.5000000000409));
#143943=CARTESIAN_POINT('',(8.95833898688851,-22.1864655136712,-17.5000000000039));
#143944=CARTESIAN_POINT('',(8.95833898688851,-10.3,-17.5000000000039));
#143945=CARTESIAN_POINT('',(1.52930216884256,-10.3,-17.5000000000164));
#143946=CARTESIAN_POINT('Origin',(5.65685424949508,-23.8568542494924,-17.5000000000094));
#143947=CARTESIAN_POINT('Origin',(5.65685424949238,-23.8568542494924,-15.8999999999905));
#143948=CARTESIAN_POINT('',(9.2027052186294,-22.8,-17.4479827960698));
#143949=CARTESIAN_POINT('',(9.20270521923383,-22.800000001014,-14.8591068129788));
#143950=CARTESIAN_POINT('',(9.20270521862939,-22.8,-15.8999999999905));
#143951=CARTESIAN_POINT('Ctrl Pts',(9.2027052186294,-22.8,-17.4479827960698));
#143952=CARTESIAN_POINT('Ctrl Pts',(9.19834579112383,-22.7853736877598,
-17.4499268294952));
#143953=CARTESIAN_POINT('Ctrl Pts',(9.19389700182971,-22.7707783400677,
-17.4518486125093));
#143954=CARTESIAN_POINT('Ctrl Pts',(9.12772044053632,-22.5583820195644,
-17.4794535144052));
#143955=CARTESIAN_POINT('Ctrl Pts',(9.04959436224867,-22.3668296543679,
-17.5000000000041));
#143956=CARTESIAN_POINT('Ctrl Pts',(8.95833898688636,-22.1864655136723,
-17.5000000000039));
#143957=CARTESIAN_POINT('',(8.72773006566549,-21.7929449196905,-14.5881859109889));
#143958=CARTESIAN_POINT('Ctrl Pts',(3.60994623656577,-20.7746200619886,
-13.1293002508268));
#143959=CARTESIAN_POINT('Ctrl Pts',(3.79140355647922,-20.6541144743078,
-13.2308379582684));
#143960=CARTESIAN_POINT('Ctrl Pts',(3.98575528452356,-20.5483144915821,
-13.3330605413595));
#143961=CARTESIAN_POINT('Ctrl Pts',(4.6518611362006,-20.2604272228388,-13.6577712706292));
#143962=CARTESIAN_POINT('Ctrl Pts',(5.16353509300209,-20.1568542494924,
-13.8653938802152));
#143963=CARTESIAN_POINT('Ctrl Pts',(6.10748558781039,-20.1568542494924,
-14.1743845031205));
#143964=CARTESIAN_POINT('Ctrl Pts',(6.59875708310373,-20.2447590781236,
-14.3012528646996));
#143965=CARTESIAN_POINT('Ctrl Pts',(7.51405499583234,-20.6187655438616,
-14.4783102296068));
#143966=CARTESIAN_POINT('Ctrl Pts',(7.93762194150675,-20.9052246256443,
-14.5301152590098));
#143967=CARTESIAN_POINT('Ctrl Pts',(8.43699112950463,-21.4043064481664,
-14.572534597221));
#143968=CARTESIAN_POINT('Ctrl Pts',(8.5915440810246,-21.5903147747047,-14.5820215238136));
#143969=CARTESIAN_POINT('Ctrl Pts',(8.72773006566549,-21.7929449196905,
-14.5881859109889));
#143970=CARTESIAN_POINT('Ctrl Pts',(9.20270521923383,-22.800000002028,-14.8591068129788));
#143971=CARTESIAN_POINT('Ctrl Pts',(9.19840087688139,-22.7855585059171,
-14.8525270133598));
#143972=CARTESIAN_POINT('Ctrl Pts',(9.19406217050678,-22.7713252500284,
-14.8461774792127));
#143973=CARTESIAN_POINT('Ctrl Pts',(9.09405266484628,-22.4499690063357,
-14.7054086990967));
#143974=CARTESIAN_POINT('Ctrl Pts',(8.92474937148254,-22.0860885247979,
-14.5971038865447));
#143975=CARTESIAN_POINT('Ctrl Pts',(8.72773006566549,-21.7929449196905,
-14.5881859109889));
#143976=CARTESIAN_POINT('Origin',(8.9583389868875,-10.3,-16.9000000000039));
#143977=CARTESIAN_POINT('',(9.5341197068668,-22.8,-16.7312500000035));
#143978=CARTESIAN_POINT('Origin',(8.9583389868875,-22.8,-16.9000000000039));
#143979=CARTESIAN_POINT('',(9.5341197068668,-10.3,-16.7312500000035));
#143980=CARTESIAN_POINT('',(9.5341197068668,-10.3,-16.7312500000035));
#143981=CARTESIAN_POINT('Origin',(8.9583389868875,-10.3,-16.9000000000039));
#143982=CARTESIAN_POINT('Origin',(8.89557956784908,-22.8,-16.359209486979));
#143983=CARTESIAN_POINT('',(9.30054298873711,-22.8,-15.1793622990701));
#143984=CARTESIAN_POINT('Origin',(8.70059915998578,-22.8,-15.1875721920774));
#143985=CARTESIAN_POINT('Origin',(15.1,-22.8,-15.1));
#143986=CARTESIAN_POINT('Origin',(-1.39005376342787,-10.3,-16.9000000000213));
#143987=CARTESIAN_POINT('Origin',(-1.39005376342787,-10.3,-16.9000000000213));
#143988=CARTESIAN_POINT('Origin',(15.1,-10.3,-15.1));
#143989=CARTESIAN_POINT('',(9.30054298873711,-10.3,-15.1793622990701));
#143990=CARTESIAN_POINT('Origin',(15.1,-10.3,-15.1));
#143991=CARTESIAN_POINT('',(9.30054298873711,-10.3,-15.1793622990701));
#143992=CARTESIAN_POINT('Origin',(8.70059915998578,-10.3,-15.1875721920774));
#143993=CARTESIAN_POINT('',(9.15685424949238,-10.3,-14.7979168401324));
#143994=CARTESIAN_POINT('',(8.72773006566549,-10.3967544991228,-14.5881859109889));
#143995=CARTESIAN_POINT('Ctrl Pts',(9.15685424949238,-10.3,-14.7979168401324));
#143996=CARTESIAN_POINT('Ctrl Pts',(9.13480845676445,-10.3,-14.7721029892919));
#143997=CARTESIAN_POINT('Ctrl Pts',(9.11081400901224,-10.3007417728394,
-14.7484812900472));
#143998=CARTESIAN_POINT('Ctrl Pts',(9.02751618170135,-10.3066884459713,
-14.6787793388689));
#143999=CARTESIAN_POINT('Ctrl Pts',(8.94804409342239,-10.3193411582955,
-14.6360996007727));
#144000=CARTESIAN_POINT('Ctrl Pts',(8.82976691205054,-10.3536628217986,
-14.599453582636));
#144001=CARTESIAN_POINT('Ctrl Pts',(8.77818765688933,-10.3727825306704,
-14.5904698473944));
#144002=CARTESIAN_POINT('Ctrl Pts',(8.72773006566549,-10.3967544991228,
-14.5881859109889));
#144003=CARTESIAN_POINT('Origin',(8.70059915998578,-10.3,-15.1875721920774));
#144004=CARTESIAN_POINT('',(8.72773006566549,-10.3,-14.5881859109889));
#144005=CARTESIAN_POINT('Origin',(8.15685424949238,-12.5431457505076,-17.5000000000052));
#144006=CARTESIAN_POINT('',(8.15685424949238,-11.3,-14.5481534330082));
#144007=CARTESIAN_POINT('',(8.15685424949238,-11.3,-13.3421101999983));
#144008=CARTESIAN_POINT('',(8.15685424949238,-11.3,-3.91787087922305));
#144009=CARTESIAN_POINT('',(8.15685424949238,-10.3,-14.5481534330082));
#144010=CARTESIAN_POINT('',(8.15685424949238,-21.1,-13.3421101999983));
#144011=CARTESIAN_POINT('Origin',(9.15685424949238,-11.3,-3.91787087922305));
#144012=CARTESIAN_POINT('',(9.15685424949238,-10.3,-13.3995808547945));
#144013=CARTESIAN_POINT('Ctrl Pts',(8.15685424949238,-11.3,-13.3421101999983));
#144014=CARTESIAN_POINT('Ctrl Pts',(8.15685424949238,-11.1743492779575,
-13.3421101999983));
#144015=CARTESIAN_POINT('Ctrl Pts',(8.18198270554795,-11.040386423148,-13.3448758442539));
#144016=CARTESIAN_POINT('Ctrl Pts',(8.28404532921617,-10.7940569805527,
-13.3549532338642));
#144017=CARTESIAN_POINT('Ctrl Pts',(8.36097444345056,-10.6816828441367,
-13.362131196164));
#144018=CARTESIAN_POINT('Ctrl Pts',(8.53841888019012,-10.5042052130985,
-13.3758933767352));
#144019=CARTESIAN_POINT('Ctrl Pts',(8.65080793814199,-10.4272469229557,
-13.3833767702998));
#144020=CARTESIAN_POINT('Ctrl Pts',(8.8971770787256,-10.3251417681012,-13.3947195510483));
#144021=CARTESIAN_POINT('Ctrl Pts',(9.03116520852081,-10.3,-13.3984496592208));
#144022=CARTESIAN_POINT('Ctrl Pts',(9.15685424949238,-10.3,-13.3995808547945));
#144023=CARTESIAN_POINT('',(9.15685424949238,-10.3,-3.91787087922305));
#144024=CARTESIAN_POINT('Ctrl Pts',(8.72773006566549,-10.3967544991228,
-14.5881859109889));
#144025=CARTESIAN_POINT('Ctrl Pts',(8.62263035139291,-10.4466864711768,
-14.5834286275394));
#144026=CARTESIAN_POINT('Ctrl Pts',(8.52719773482439,-10.5154313193455,
-14.5776230261749));
#144027=CARTESIAN_POINT('Ctrl Pts',(8.36097192174538,-10.6816820908159,
-14.566077401997));
#144028=CARTESIAN_POINT('Ctrl Pts',(8.28403667557063,-10.7940707929597,
-14.5596498341489));
#144029=CARTESIAN_POINT('Ctrl Pts',(8.181975807613,-11.0404101457541,-14.5506281907869));
#144030=CARTESIAN_POINT('Ctrl Pts',(8.15685424949238,-11.1743668352713,
-14.5481534330082));
#144031=CARTESIAN_POINT('Ctrl Pts',(8.15685424949238,-11.3,-14.5481534330082));
#144032=CARTESIAN_POINT('Origin',(3.15685424949238,-10.3,-17.5000000000137));
#144033=CARTESIAN_POINT('',(3.15685424949238,-11.3,-11.4163656902917));
#144034=CARTESIAN_POINT('',(3.15685424949238,-11.3,-12.8620372432944));
#144035=CARTESIAN_POINT('',(3.15685424949238,-11.3,-3.91787087922727));
#144036=CARTESIAN_POINT('',(3.15685424949238,-21.1,-11.4163656902917));
#144037=CARTESIAN_POINT('',(3.15685424949238,-10.3,-12.8620372432944));
#144038=CARTESIAN_POINT('Origin',(9.25,-10.3,-3.05000000003698));
#144039=CARTESIAN_POINT('',(2.15685424949238,-10.3,-12.1653597494959));
#144040=CARTESIAN_POINT('Ctrl Pts',(3.15685424949238,-11.3,-12.8620372432944));
#144041=CARTESIAN_POINT('Ctrl Pts',(3.15685424949238,-11.1762015590292,
-12.8620372432944));
#144042=CARTESIAN_POINT('Ctrl Pts',(3.13234244232117,-11.0457637590431,
-12.8469337261833));
#144043=CARTESIAN_POINT('Ctrl Pts',(3.03750402279937,-10.8094195852156,
-12.7870703131628));
#144044=CARTESIAN_POINT('Ctrl Pts',(2.96735248349465,-10.7034637280328,
-12.7422285875942));
#144045=CARTESIAN_POINT('Ctrl Pts',(2.79365250694672,-10.5158786289393,
-12.6276596027851));
#144046=CARTESIAN_POINT('Ctrl Pts',(2.67252340826556,-10.4319701706144,
-12.5454812826689));
#144047=CARTESIAN_POINT('Ctrl Pts',(2.41575853688544,-10.3241111824561,
-12.3623845936079));
#144048=CARTESIAN_POINT('Ctrl Pts',(2.28025089968914,-10.3,-12.2613812394894));
#144049=CARTESIAN_POINT('Ctrl Pts',(2.15685424949238,-10.3,-12.1653597494959));
#144050=CARTESIAN_POINT('Origin',(9.25,-10.3,-3.05000000003698));
#144051=CARTESIAN_POINT('Origin',(-1.39005376343553,-10.3,-12.3613777665656));
#144052=CARTESIAN_POINT('Origin',(-1.39005376343553,-10.3,-12.3613777665656));
#144053=CARTESIAN_POINT('Origin',(-3.15685424949238,-12.5431457505076,-17.5000000000243));
#144054=CARTESIAN_POINT('',(-3.15685424949238,-11.3,-11.4670924738648));
#144055=CARTESIAN_POINT('',(-3.15685424949238,-11.3,-3.9178708792326));
#144056=CARTESIAN_POINT('',(-3.15685424949238,-15.9,-11.4670924738648));
#144057=CARTESIAN_POINT('Origin',(-9.35,-15.9,-3.05000000003699));
#144058=CARTESIAN_POINT('Origin',(-9.35,-15.9,-3.05000000003699));
#144059=CARTESIAN_POINT('',(-2.15685424949238,-10.3,-10.6303135959217));
#144060=CARTESIAN_POINT('Origin',(-9.35,-10.3,-3.05000000003699));
#144061=CARTESIAN_POINT('Ctrl Pts',(-3.15685424949238,-11.3,-11.4670924738648));
#144062=CARTESIAN_POINT('Ctrl Pts',(-3.15685424949238,-11.1669531550595,
-11.4670924738648));
#144063=CARTESIAN_POINT('Ctrl Pts',(-3.12859247195756,-11.0286485309897,
-11.4464839092837));
#144064=CARTESIAN_POINT('Ctrl Pts',(-3.02305868401783,-10.7827027578499,
-11.3672511996362));
#144065=CARTESIAN_POINT('Ctrl Pts',(-2.94605369112082,-10.6749858792553,
-11.3085067616158));
#144066=CARTESIAN_POINT('Ctrl Pts',(-2.76593743750536,-10.4948696256399,
-11.1659256985317));
#144067=CARTESIAN_POINT('Ctrl Pts',(-2.64696217816639,-10.4182896302278,
-11.0686275519228));
#144068=CARTESIAN_POINT('Ctrl Pts',(-2.39997354427981,-10.3209637887529,
-10.8555260063351));
#144069=CARTESIAN_POINT('Ctrl Pts',(-2.27209385158697,-10.3,-10.7396672847383));
#144070=CARTESIAN_POINT('Ctrl Pts',(-2.15685424949238,-10.3,-10.6303135959217));
#144071=CARTESIAN_POINT('',(-8.15685424949239,-11.3,-13.4316618717243));
#144072=CARTESIAN_POINT('',(-8.15685424949239,-15.9,-13.4316618717243));
#144073=CARTESIAN_POINT('',(-9.15685424949239,-10.3,-13.4982149058982));
#144074=CARTESIAN_POINT('Ctrl Pts',(-9.15685424949239,-10.3,-13.4982149058982));
#144075=CARTESIAN_POINT('Ctrl Pts',(-9.03112180920881,-10.3,-13.4958906154084));
#144076=CARTESIAN_POINT('Ctrl Pts',(-8.89711190098953,-10.3251571822744,
-13.4909106549527));
#144077=CARTESIAN_POINT('Ctrl Pts',(-8.65072463395046,-10.4272930525798,
-13.4773072697496));
#144078=CARTESIAN_POINT('Ctrl Pts',(-8.53833784786347,-10.5042659905921,
-13.4688117245097));
#144079=CARTESIAN_POINT('Ctrl Pts',(-8.36093460719447,-10.6817429599976,
-13.4534691379964));
#144080=CARTESIAN_POINT('Ctrl Pts',(-8.28402699211168,-10.7940934369191,
-13.4456161349629));
#144081=CARTESIAN_POINT('Ctrl Pts',(-8.1819838951961,-11.0403913536937,
-13.4346459578849));
#144082=CARTESIAN_POINT('Ctrl Pts',(-8.15685424949239,-11.174347121187,
-13.4316618717243));
#144083=CARTESIAN_POINT('Ctrl Pts',(-8.15685424949239,-11.3,-13.4316618717243));
#144084=CARTESIAN_POINT('Origin',(-9.35,-10.3,-3.05000000003699));
#144085=CARTESIAN_POINT('Origin',(-8.15685424949238,-10.3,-17.5000000000328));
#144086=CARTESIAN_POINT('',(-8.15685424949239,-11.3,-3.91787087923682));
#144087=CARTESIAN_POINT('Origin',(9.25,-21.1,-3.05000000003699));
#144088=CARTESIAN_POINT('',(2.15685424949238,-10.3,-10.5872265033375));
#144089=CARTESIAN_POINT('Ctrl Pts',(2.15685424949238,-10.3,-10.5872265033375));
#144090=CARTESIAN_POINT('Ctrl Pts',(2.27216752689059,-10.3,-10.6957457157024));
#144091=CARTESIAN_POINT('Ctrl Pts',(2.4001077317982,-10.3209951024604,-10.8106623925262));
#144092=CARTESIAN_POINT('Ctrl Pts',(2.64710933942602,-10.4183692065858,
-11.0218717794871));
#144093=CARTESIAN_POINT('Ctrl Pts',(2.76603569567595,-10.4949678838105,
-11.1182210617341));
#144094=CARTESIAN_POINT('Ctrl Pts',(2.94615370539162,-10.6750858935261,
-11.259441539498));
#144095=CARTESIAN_POINT('Ctrl Pts',(3.02316861067196,-10.7828869566871,
-11.3176108509303));
#144096=CARTESIAN_POINT('Ctrl Pts',(3.12864992256832,-11.0288545184812,
-11.3960105022376));
#144097=CARTESIAN_POINT('Ctrl Pts',(3.15685424949238,-11.1670935229091,
-11.4163656902917));
#144098=CARTESIAN_POINT('Ctrl Pts',(3.15685424949238,-11.3,-11.4163656902917));
#144099=CARTESIAN_POINT('Origin',(9.25,-10.3,-3.05000000003699));
#144100=CARTESIAN_POINT('Origin',(9.25,-15.9,-3.05000000003699));
#144101=CARTESIAN_POINT('Origin',(9.25,-10.3,-3.05000000003699));
#144102=CARTESIAN_POINT('Origin',(2.15685424949238,-11.3,-3.91787087922727));
#144103=CARTESIAN_POINT('',(2.15685424949238,-10.3,-3.91787087922727));
#144104=CARTESIAN_POINT('Origin',(-2.15685424949238,-11.3,-3.9178708792326));
#144105=CARTESIAN_POINT('',(-2.15685424949238,-10.3,-3.9178708792326));
#144106=CARTESIAN_POINT('Origin',(-9.15685424949239,-11.3,-3.91787087923682));
#144107=CARTESIAN_POINT('',(-9.15685424949239,-10.3,-3.91787087923682));
#144108=CARTESIAN_POINT('Origin',(2.24865810106615,-10.3,9.66425824155912));
#144109=CARTESIAN_POINT('',(13.8193751525349,-10.3,-19.1000000000069));
#144110=CARTESIAN_POINT('Origin',(19.1,-24.4,-19.1));
#144111=CARTESIAN_POINT('',(9.54999999998871,-25.4,-19.1));
#144112=CARTESIAN_POINT('',(9.54999999998871,-25.4,-19.1));
#144113=CARTESIAN_POINT('',(9.54999999998871,-25.4,-19.1));
#144114=CARTESIAN_POINT('',(-69.9000013262034,-22.1,-19.1));
#144115=CARTESIAN_POINT('Origin',(11.2998162594733,-10.3,10.1607140398676));
#144116=CARTESIAN_POINT('',(10.69984250812,-11.3,10.1663263198865));
#144117=CARTESIAN_POINT('',(11.3890749660464,-10.5645232201992,9.56739044915099));
#144118=CARTESIAN_POINT('Ctrl Pts',(10.69984250812,-11.3,10.1663263198865));
#144119=CARTESIAN_POINT('Ctrl Pts',(10.6992150492722,-11.3,10.0992486193006));
#144120=CARTESIAN_POINT('Ctrl Pts',(10.7105416393666,-11.2859681238687,
10.0298809986402));
#144121=CARTESIAN_POINT('Ctrl Pts',(10.7531080502661,-11.2354954752618,
9.90483916612018));
#144122=CARTESIAN_POINT('Ctrl Pts',(10.78415813957,-11.1993829121916,9.84896825061679));
#144123=CARTESIAN_POINT('Ctrl Pts',(10.8663746357755,-11.1058434210861,
9.73764581751491));
#144124=CARTESIAN_POINT('Ctrl Pts',(10.9287151162477,-11.0366106450061,
9.68269383698243));
#144125=CARTESIAN_POINT('Ctrl Pts',(11.0648458019447,-10.8905755867573,
9.60303292733449));
#144126=CARTESIAN_POINT('Ctrl Pts',(11.1386925567721,-10.8137589718382,
9.57844696758312));
#144127=CARTESIAN_POINT('Ctrl Pts',(11.2085510069148,-10.7430780618347,
9.56769578241224));
#144128=CARTESIAN_POINT('Ctrl Pts',(11.2653388943385,-10.68562159734,9.55895615117352));
#144129=CARTESIAN_POINT('Ctrl Pts',(11.3269631854058,-10.6246068030101,
9.55804644650272));
#144130=CARTESIAN_POINT('Ctrl Pts',(11.3890749660464,-10.5645232201992,
9.56739044915099));
#144131=CARTESIAN_POINT('',(11.3890749660464,-10.3,9.56739044915099));
#144132=CARTESIAN_POINT('',(11.3890749660464,-10.3,9.56739044915099));
#144133=CARTESIAN_POINT('',(10.69984250812,-10.3,10.1663263198865));
#144134=CARTESIAN_POINT('Origin',(11.2998162594733,-10.3,10.1607140398676));
#144135=CARTESIAN_POINT('',(10.69984250812,-10.3,10.1663263198865));
#144136=CARTESIAN_POINT('Origin',(3.68732223444763,-10.3,7.75181077763493));
#144137=CARTESIAN_POINT('',(4.17484762952654,-11.3,8.10155209511566));
#144138=CARTESIAN_POINT('Ctrl Pts',(3.96202237101816,-10.5713843344211,
7.21838802318202));
#144139=CARTESIAN_POINT('Ctrl Pts',(4.01561068343958,-10.6292415447907,
7.24598474007845));
#144140=CARTESIAN_POINT('Ctrl Pts',(4.06327615070688,-10.6878073192481,
7.28094613908644));
#144141=CARTESIAN_POINT('Ctrl Pts',(4.15407930627617,-10.8137589718382,
7.36823076389991));
#144142=CARTESIAN_POINT('Ctrl Pts',(4.20033921266016,-10.8905755867573,
7.43082336471489));
#144143=CARTESIAN_POINT('Ctrl Pts',(4.26586151345588,-11.0366106450061,
7.57429549515384));
#144144=CARTESIAN_POINT('Ctrl Pts',(4.28524090449668,-11.1058434210861,
7.65510697251215));
#144145=CARTESIAN_POINT('Ctrl Pts',(4.28844947659775,-11.1993829121916,
7.79346137766468));
#144146=CARTESIAN_POINT('Ctrl Pts',(4.28170596499445,-11.2354954752618,
7.85702388466544));
#144147=CARTESIAN_POINT('Ctrl Pts',(4.24458994202194,-11.2859681238687,
7.98379044198844));
#144148=CARTESIAN_POINT('Ctrl Pts',(4.21394907908761,-11.3,8.04704623980883));
#144149=CARTESIAN_POINT('Ctrl Pts',(4.17484762952654,-11.3,8.10155209511565));
#144150=CARTESIAN_POINT('',(4.17484762952654,-10.3,8.10155209511566));
#144151=CARTESIAN_POINT('',(4.17484762952654,-10.3,8.10155209511566));
#144152=CARTESIAN_POINT('Origin',(3.68732223444763,-10.3,7.75181077763493));
#144153=CARTESIAN_POINT('Origin',(7.47499999999962,-14.8,14.199999999963));
#144154=CARTESIAN_POINT('',(7.64999999999965,-11.7199299841877,13.3321470759639));
#144155=CARTESIAN_POINT('',(7.41177157822234,-12.1000000000004,12.9825884501688));
#144156=CARTESIAN_POINT('Ctrl Pts',(7.64999999999965,-11.7199299841877,
13.3321470759639));
#144157=CARTESIAN_POINT('Ctrl Pts',(7.61868756556843,-11.7633272734221,
13.2935842063427));
#144158=CARTESIAN_POINT('Ctrl Pts',(7.58861560393998,-11.8067445070237,
13.2545025807997));
#144159=CARTESIAN_POINT('Ctrl Pts',(7.50520657393635,-11.9331277607182,
13.1393811397357));
#144160=CARTESIAN_POINT('Ctrl Pts',(7.455490303221,-12.0162549490882,13.0619591119168));
#144161=CARTESIAN_POINT('Ctrl Pts',(7.41177157822295,-12.1000000000003,
12.9825884501684));
#144162=CARTESIAN_POINT('',(7.29999999999962,-12.2182788550814,12.9928480087538));
#144163=CARTESIAN_POINT('Ctrl Pts',(7.41177157822255,-12.1000000000006,
12.9825884501688));
#144164=CARTESIAN_POINT('Ctrl Pts',(7.3743512628699,-12.1391578411027,12.9867811617336));
#144165=CARTESIAN_POINT('Ctrl Pts',(7.33707673963459,-12.1785907678552,
12.9901928882805));
#144166=CARTESIAN_POINT('Ctrl Pts',(7.29999999999961,-12.2182788550814,
12.9928480087538));
#144167=CARTESIAN_POINT('',(7.29999999999956,-12.5535531013342,15.9538461538416));
#144168=CARTESIAN_POINT('Origin',(7.29999999999959,-14.8,14.199999999963));
#144169=CARTESIAN_POINT('Ctrl Pts',(7.29999999999956,-12.5535531013342,
15.9538461538416));
#144170=CARTESIAN_POINT('Ctrl Pts',(7.29999999999956,-12.5814935453447,
15.9896341981098));
#144171=CARTESIAN_POINT('Ctrl Pts',(7.30941758154832,-12.6038504815788,
16.0316406923603));
#144172=CARTESIAN_POINT('Ctrl Pts',(7.34336734883734,-12.6320030732815,
16.1165268946216));
#144173=CARTESIAN_POINT('Ctrl Pts',(7.36769238401017,-12.6379779471448,
16.1594297908438));
#144174=CARTESIAN_POINT('Ctrl Pts',(7.43072186332663,-12.6386585391172,
16.2530509386545));
#144175=CARTESIAN_POINT('Ctrl Pts',(7.47734347162638,-12.6270638876253,
16.3079691869699));
#144176=CARTESIAN_POINT('Ctrl Pts',(7.57576120928368,-12.585316726708,16.4059033715659));
#144177=CARTESIAN_POINT('Ctrl Pts',(7.62758928926194,-12.5550504765137,
16.4488386620803));
#144178=CARTESIAN_POINT('Ctrl Pts',(7.67529068457363,-12.5213497005712,
16.482597821068));
#144179=CARTESIAN_POINT('Ctrl Pts',(7.7264149551059,-12.485230681931,16.5187794121043));
#144180=CARTESIAN_POINT('Ctrl Pts',(7.78179221084198,-12.4388020333086,
16.5507601268268));
#144181=CARTESIAN_POINT('Ctrl Pts',(7.87967710828239,-12.3400773625447,
16.5899436813847));
#144182=CARTESIAN_POINT('Ctrl Pts',(7.92296055726618,-12.2894858062932,
16.6));
#144183=CARTESIAN_POINT('Ctrl Pts',(7.9603418636975,-12.238262308539,16.6));
#144184=CARTESIAN_POINT('',(7.64999999999961,-12.1392658583161,15.9777777777737));
#144185=CARTESIAN_POINT('Ctrl Pts',(7.64999999999963,-12.1392658583161,
15.9777777777737));
#144186=CARTESIAN_POINT('Ctrl Pts',(7.64999999999963,-12.1647190199888,
16.0158725819284));
#144187=CARTESIAN_POINT('Ctrl Pts',(7.65945587523489,-12.1840248468099,
16.0598458438056));
#144188=CARTESIAN_POINT('Ctrl Pts',(7.6935871828228,-12.2057670409854,16.1474492768948));
#144189=CARTESIAN_POINT('Ctrl Pts',(7.71806257389703,-12.208379932636,16.1911133687284));
#144190=CARTESIAN_POINT('Ctrl Pts',(7.78149608588271,-12.2015215184701,
16.2853111664178));
#144191=CARTESIAN_POINT('Ctrl Pts',(7.82839529686648,-12.1853531341838,
16.3395239080143));
#144192=CARTESIAN_POINT('Ctrl Pts',(7.92745916770871,-12.1352560207032,
16.4343503422875));
#144193=CARTESIAN_POINT('Ctrl Pts',(7.97965638032824,-12.101215923928,16.4748711334417));
#144194=CARTESIAN_POINT('Ctrl Pts',(8.02770876399932,-12.0644749514664,
16.5058409981337));
#144195=CARTESIAN_POINT('Ctrl Pts',(8.07847474046147,-12.0256591591853,
16.5385597792197));
#144196=CARTESIAN_POINT('Ctrl Pts',(8.13347864575108,-11.9770409104891,
16.5663042200272));
#144197=CARTESIAN_POINT('Ctrl Pts',(8.22123438481492,-11.8859917604215,
16.5939479694972));
#144198=CARTESIAN_POINT('Ctrl Pts',(8.2555385114276,-11.8465704328685,16.6));
#144199=CARTESIAN_POINT('Ctrl Pts',(8.28666521865376,-11.8066740906056,
16.6));
#144200=CARTESIAN_POINT('Origin',(7.64999999999965,-14.8,14.199999999963));
#144201=CARTESIAN_POINT('Origin',(7.1,-24.4,10.2));
#144202=CARTESIAN_POINT('',(9.89635480722185,-12.1,10.0571721591311));
#144203=CARTESIAN_POINT('',(9.89635480722185,-17.7372583002031,10.0571721591311));
#144204=CARTESIAN_POINT('',(9.89635480722185,-10.3,10.0571721591311));
#144205=CARTESIAN_POINT('',(8.7218665882827,-12.1000000000115,12.4824435961951));
#144206=CARTESIAN_POINT('Origin',(7.1,-12.1,10.2));
#144207=CARTESIAN_POINT('Ctrl Pts',(9.32485954600978,-17.0248595463278,
11.9000000001556));
#144208=CARTESIAN_POINT('Ctrl Pts',(9.34001112247009,-17.0043603546528,
11.8801705122017));
#144209=CARTESIAN_POINT('Ctrl Pts',(9.35447849265797,-16.9836680437391,
11.8606864486227));
#144210=CARTESIAN_POINT('Ctrl Pts',(9.54024107063934,-16.703804134771,11.6040173789117));
#144211=CARTESIAN_POINT('Ctrl Pts',(9.64482709960529,-16.3646990093396,
11.3790747377687));
#144212=CARTESIAN_POINT('Ctrl Pts',(9.76404695970622,-15.608125281439,11.0770456465201));
#144213=CARTESIAN_POINT('Ctrl Pts',(9.78328157301077,-15.1913725392454,
10.999999999963));
#144214=CARTESIAN_POINT('Ctrl Pts',(9.78328157301077,-14.4086274607546,
10.999999999963));
#144215=CARTESIAN_POINT('Ctrl Pts',(9.76404695970622,-13.991874718561,11.0770456465201));
#144216=CARTESIAN_POINT('Ctrl Pts',(9.64482709960529,-13.2353009906604,
11.3790747377687));
#144217=CARTESIAN_POINT('Ctrl Pts',(9.54024107063934,-12.896195865229,11.6040173789117));
#144218=CARTESIAN_POINT('Ctrl Pts',(9.22419326738574,-12.4200484376874,
12.0407021866206));
#144219=CARTESIAN_POINT('Ctrl Pts',(8.98968945737333,-12.2245160908571,
12.2888237365864));
#144220=CARTESIAN_POINT('Ctrl Pts',(8.73475193252056,-12.1058672399844,
12.4732461679086));
#144221=CARTESIAN_POINT('Ctrl Pts',(8.72832975141059,-12.1029215104077,
12.4778509796025));
#144222=CARTESIAN_POINT('Ctrl Pts',(8.72186658827967,-12.1000000000216,
12.4824435961973));
#144223=CARTESIAN_POINT('Origin',(7.1,-17.7372583002031,10.2));
#144224=CARTESIAN_POINT('Origin',(7.1,-10.3,10.2));
#144225=CARTESIAN_POINT('Origin',(7.1,-10.3,10.2));
#144226=CARTESIAN_POINT('Origin',(7.1,-11.3,10.2));
#144227=CARTESIAN_POINT('Origin',(8.49999999999956,-12.238262308539,16.2));
#144228=CARTESIAN_POINT('',(8.49999999999956,-12.5535531013342,15.9538461538416));
#144229=CARTESIAN_POINT('Origin',(15.1,-10.3,-15.1000000000002));
#144230=CARTESIAN_POINT('',(4.67225419943745,-11.3140320785605,7.56083038410859));
#144231=CARTESIAN_POINT('',(4.67225419942505,-18.5232262216426,7.56083038411999));
#144232=CARTESIAN_POINT('',(4.67225419943745,-10.3,7.56083038410859));
#144233=CARTESIAN_POINT('',(4.65844715578268,-11.3,7.55447175239154));
#144234=CARTESIAN_POINT('Ctrl Pts',(4.65844715578268,-11.3,7.55447175239154));
#144235=CARTESIAN_POINT('Ctrl Pts',(4.66304985477283,-11.3046805476178,
7.55659315805736));
#144236=CARTESIAN_POINT('Ctrl Pts',(4.66765219994199,-11.3093579116597,
7.558712699977));
#144237=CARTESIAN_POINT('Ctrl Pts',(4.67225419943745,-11.3140320785604,
7.56083038410858));
#144238=CARTESIAN_POINT('Ctrl Pts',(4.20575266919785,-10.8312625177592,
7.34028723688267));
#144239=CARTESIAN_POINT('Ctrl Pts',(4.35718070025283,-10.9906489469993,
7.41380209013365));
#144240=CARTESIAN_POINT('Ctrl Pts',(4.5080049398014,-11.1470132508919,7.48513222572595));
#144241=CARTESIAN_POINT('Ctrl Pts',(4.65844715578268,-11.3,7.55447175239154));
#144242=CARTESIAN_POINT('Ctrl Pts',(4.20575266919785,-19.0059957824439,
7.34028723688266));
#144243=CARTESIAN_POINT('Ctrl Pts',(4.36181367819661,-18.8417328861054,
7.41605129519349));
#144244=CARTESIAN_POINT('Ctrl Pts',(4.51723285276396,-18.6806785743082,
7.48949481655117));
#144245=CARTESIAN_POINT('Ctrl Pts',(4.67225419943426,-18.5232262216458,
7.56083038410712));
#144246=CARTESIAN_POINT('Origin',(-2.356826353498,-10.3,7.0077344540968));
#144247=CARTESIAN_POINT('',(-2.6993491429948,-16.3017075537437,6.51511072479082));
#144248=CARTESIAN_POINT('',(-2.87773485737152,-16.5848708742773,7.30548322503002));
#144249=CARTESIAN_POINT('Ctrl Pts',(-2.69934914221477,-16.3017075545574,
6.51511072424847));
#144250=CARTESIAN_POINT('Ctrl Pts',(-2.74531797479244,-16.3670746844141,
6.54707299438395));
#144251=CARTESIAN_POINT('Ctrl Pts',(-2.78651988585169,-16.4308362330594,
6.58526323998097));
#144252=CARTESIAN_POINT('Ctrl Pts',(-2.85722586073441,-16.547448699515,
6.67196627688682));
#144253=CARTESIAN_POINT('Ctrl Pts',(-2.89124061589894,-16.6082776579722,
6.72661902786091));
#144254=CARTESIAN_POINT('Ctrl Pts',(-2.92845981168729,-16.6785516418896,
6.8221836431129));
#144255=CARTESIAN_POINT('Ctrl Pts',(-2.93858697485447,-16.6983485015077,
6.85634795597679));
#144256=CARTESIAN_POINT('Ctrl Pts',(-2.9527704395822,-16.7264359005426,
6.92887841593282));
#144257=CARTESIAN_POINT('Ctrl Pts',(-2.95682635349799,-16.7346748090408,
6.96726462231166));
#144258=CARTESIAN_POINT('Ctrl Pts',(-2.95682635349799,-16.7346748090408,
7.04820428588195));
#144259=CARTESIAN_POINT('Ctrl Pts',(-2.9527704395822,-16.7264359005426,
7.08659049226079));
#144260=CARTESIAN_POINT('Ctrl Pts',(-2.93858697485447,-16.6983485015077,
7.15912095221682));
#144261=CARTESIAN_POINT('Ctrl Pts',(-2.92845981168729,-16.6785516418896,
7.1932852650807));
#144262=CARTESIAN_POINT('Ctrl Pts',(-2.90488679928763,-16.6340431709469,
7.25381171689106));
#144263=CARTESIAN_POINT('Ctrl Pts',(-2.89191125967647,-16.6101294913542,
7.28068175067744));
#144264=CARTESIAN_POINT('Ctrl Pts',(-2.87773485721227,-16.5848708746402,
7.30548322530863));
#144265=CARTESIAN_POINT('',(-2.69934914434707,-10.3,6.51511072573106));
#144266=CARTESIAN_POINT('',(-2.69934914434707,-10.3,6.51511072573106));
#144267=CARTESIAN_POINT('',(-2.87773485773448,-10.3,7.30548322439503));
#144268=CARTESIAN_POINT('Origin',(-2.356826353498,-10.3,7.0077344540968));
#144269=CARTESIAN_POINT('',(-2.87773485773448,-10.3,7.30548322439503));
#144270=CARTESIAN_POINT('Origin',(-8.4775012782713,-10.3,10.5062825050979));
#144271=CARTESIAN_POINT('',(-4.07042440724209,-10.3,15.2158656557344));
#144272=CARTESIAN_POINT('Origin',(-8.4775012782713,-10.3,10.5062825050979));
#144273=CARTESIAN_POINT('',(-4.07042440724209,-15.4372006646508,15.2158656557344));
#144274=CARTESIAN_POINT('',(-4.07042440724209,-10.3,15.2158656557344));
#144275=CARTESIAN_POINT('',(-3.33223732524944,-14.0144660545858,14.3958530281318));
#144276=CARTESIAN_POINT('Ctrl Pts',(-4.07042440724209,-15.4372006646508,
15.2158656557344));
#144277=CARTESIAN_POINT('Ctrl Pts',(-4.03861146906795,-15.3625014535314,
15.1860961284658));
#144278=CARTESIAN_POINT('Ctrl Pts',(-4.0059205861772,-15.2886209362891,
15.1548999501354));
#144279=CARTESIAN_POINT('Ctrl Pts',(-3.77494925612046,-14.7841712702143,
14.929484770533));
#144280=CARTESIAN_POINT('Ctrl Pts',(-3.5505954637745,-14.3821453612863,
14.6847050369457));
#144281=CARTESIAN_POINT('Ctrl Pts',(-3.33223732524944,-14.0144660545858,
14.3958530281318));
#144282=CARTESIAN_POINT('',(-2.06491552545779,-13.264554338996,11.2));
#144283=CARTESIAN_POINT('Ctrl Pts',(-3.33223732524944,-14.0144660545858,
14.3958530281318));
#144284=CARTESIAN_POINT('Ctrl Pts',(-2.97652069716172,-13.7312686798221,
13.9252982629844));
#144285=CARTESIAN_POINT('Ctrl Pts',(-2.64594985001838,-13.5429439336592,
13.343649108976));
#144286=CARTESIAN_POINT('Ctrl Pts',(-2.23928412359358,-13.3371720517063,
12.2247807719029));
#144287=CARTESIAN_POINT('Ctrl Pts',(-2.12002313078455,-13.2876105243186,
11.7094036800094));
#144288=CARTESIAN_POINT('Ctrl Pts',(-2.06491552545779,-13.264554338996,
11.2));
#144289=CARTESIAN_POINT('',(-2.17171046614589,-15.7153121622159,9.14999999999999));
#144290=CARTESIAN_POINT('Ctrl Pts',(-2.06491552545779,-13.264554338996,
11.2));
#144291=CARTESIAN_POINT('Ctrl Pts',(-2.01806542640658,-13.7144020133522,
10.7669270561843));
#144292=CARTESIAN_POINT('Ctrl Pts',(-2.01903789024593,-14.176467536479,
10.3450743353087));
#144293=CARTESIAN_POINT('Ctrl Pts',(-2.06556093124264,-14.8558616960581,
9.77835970509417));
#144294=CARTESIAN_POINT('Ctrl Pts',(-2.09659729559528,-15.1499390919158,
9.54682356160579));
#144295=CARTESIAN_POINT('Ctrl Pts',(-2.14186392109874,-15.5009332716129,
9.29495491302226));
#144296=CARTESIAN_POINT('Ctrl Pts',(-2.15622982991206,-15.6061897771793,
9.22197442521173));
#144297=CARTESIAN_POINT('Ctrl Pts',(-2.17171046614589,-15.7153121622159,
9.14999999999999));
#144298=CARTESIAN_POINT('Ctrl Pts',(-2.17171046614589,-15.7153121622159,
9.14999999999999));
#144299=CARTESIAN_POINT('Ctrl Pts',(-2.21590083179177,-15.7539362010656,
8.94454486758705));
#144300=CARTESIAN_POINT('Ctrl Pts',(-2.26974837175159,-15.8029699038511,
8.74353599076851));
#144301=CARTESIAN_POINT('Ctrl Pts',(-2.42818675997411,-15.9610882759758,
8.24557800636064));
#144302=CARTESIAN_POINT('Ctrl Pts',(-2.54447355256091,-16.0886251879561,
7.96074874984413));
#144303=CARTESIAN_POINT('Ctrl Pts',(-2.73607614870722,-16.3511725332041,
7.56266001973146));
#144304=CARTESIAN_POINT('Ctrl Pts',(-2.80802393475142,-16.460664364867,
7.42744178898432));
#144305=CARTESIAN_POINT('Ctrl Pts',(-2.87773485721227,-16.5848708746402,
7.30548322530863));
#144306=CARTESIAN_POINT('Origin',(0.0177419354838726,-10.3,5.45105352468434));
#144307=CARTESIAN_POINT('',(-0.722791023811509,-16.12212292569,4.77903348316978));
#144308=CARTESIAN_POINT('Ctrl Pts',(0.753380028237917,-16.1330170457761,
4.77367874179883));
#144309=CARTESIAN_POINT('Ctrl Pts',(0.74409769330423,-16.1296337930307,
4.76359800165401));
#144310=CARTESIAN_POINT('Ctrl Pts',(0.734669071608476,-16.126268178292,
4.75377451472814));
#144311=CARTESIAN_POINT('Ctrl Pts',(0.637473178290217,-16.092336359572,
4.65650419393023));
#144312=CARTESIAN_POINT('Ctrl Pts',(0.526282739188228,-16.0602162963568,
4.57976205448264));
#144313=CARTESIAN_POINT('Ctrl Pts',(0.280340152199377,-16.0143519898035,
4.47698741133051));
#144314=CARTESIAN_POINT('Ctrl Pts',(0.145454989338261,-16.0011015187019,
4.45105352468434));
#144315=CARTESIAN_POINT('Ctrl Pts',(-0.109580731505419,-15.9990447121329,
4.45105352468434));
#144316=CARTESIAN_POINT('Ctrl Pts',(-0.244282057994744,-16.0100526854273,
4.4768451524154));
#144317=CARTESIAN_POINT('Ctrl Pts',(-0.490127096915344,-16.0516707912072,
4.57938413049508));
#144318=CARTESIAN_POINT('Ctrl Pts',(-0.601393492215431,-16.0817799830708,
4.65603999011667));
#144319=CARTESIAN_POINT('Ctrl Pts',(-0.700521533797108,-16.1144751009463,
4.75509513111577));
#144320=CARTESIAN_POINT('Ctrl Pts',(-0.7117644146194,-16.118287311821,4.76688270338414));
#144321=CARTESIAN_POINT('Ctrl Pts',(-0.72279102380988,-16.1221229257004,
4.77903348316799));
#144322=CARTESIAN_POINT('',(-0.722791023842917,-10.3,4.77903348320439));
#144323=CARTESIAN_POINT('Origin',(0.0177419354838726,-10.3,5.45105352468434));
#144324=CARTESIAN_POINT('',(-0.722791023842917,-10.3,4.77903348320439));
#144325=CARTESIAN_POINT('Origin',(-9.35,-10.3,-3.05000000003699));
#144326=CARTESIAN_POINT('',(-2.26762751619799,-15.8025293645632,6.19999999999999));
#144327=CARTESIAN_POINT('Ctrl Pts',(-2.69934914221477,-16.3017075545574,
6.51511072424847));
#144328=CARTESIAN_POINT('Ctrl Pts',(-2.5724485882362,-16.1212564853078,
6.42687637939889));
#144329=CARTESIAN_POINT('Ctrl Pts',(-2.42570115325786,-15.9520419899461,
6.32103095973219));
#144330=CARTESIAN_POINT('Ctrl Pts',(-2.26762751619799,-15.8025293645632,
6.19999999999999));
#144331=CARTESIAN_POINT('',(-1.02533784472924,-16.2535462234705,5.09999999999999));
#144332=CARTESIAN_POINT('Ctrl Pts',(-2.26762751619799,-15.8025293645632,
6.19999999999999));
#144333=CARTESIAN_POINT('Ctrl Pts',(-1.8764893960922,-15.8447934730179,
5.90052044765489));
#144334=CARTESIAN_POINT('Ctrl Pts',(-1.50140793289236,-15.9797824776671,
5.57275424042926));
#144335=CARTESIAN_POINT('Ctrl Pts',(-1.11481261265353,-16.1987537307299,
5.19064987199639));
#144336=CARTESIAN_POINT('Ctrl Pts',(-1.06975596859005,-16.2256644836538,
5.14537004597675));
#144337=CARTESIAN_POINT('Ctrl Pts',(-1.02533784472924,-16.2535462234705,
5.09999999999999));
#144338=CARTESIAN_POINT('Ctrl Pts',(-1.02533784472924,-16.2535462234705,
5.09999999999999));
#144339=CARTESIAN_POINT('Ctrl Pts',(-1.0092117726784,-16.2450514561352,
5.083528331078));
#144340=CARTESIAN_POINT('Ctrl Pts',(-0.993056266977858,-16.2367972149681,
5.0669287615527));
#144341=CARTESIAN_POINT('Ctrl Pts',(-0.892245880391997,-16.1868384475464,
4.96272194243645));
#144342=CARTESIAN_POINT('Ctrl Pts',(-0.807070308040803,-16.1514395348919,
4.87190509994976));
#144343=CARTESIAN_POINT('Ctrl Pts',(-0.722791023809883,-16.1221229257004,
4.77903348316799));
#144344=CARTESIAN_POINT('Origin',(-9.35,-10.3,-3.05000000003699));
#144345=CARTESIAN_POINT('Origin',(1.68452938230201E-16,-18.2,11.8));
#144346=CARTESIAN_POINT('',(4.15,-18.2,12.));
#144347=CARTESIAN_POINT('Origin',(1.9309146098219E-16,-18.2,12.));
#144348=CARTESIAN_POINT('',(3.75,-18.2,11.6));
#144349=CARTESIAN_POINT('',(3.95,-18.2,11.8));
#144350=CARTESIAN_POINT('Origin',(1.43814415478212E-16,-18.2,11.6));
#144351=CARTESIAN_POINT('Origin',(1.7735870188571E-16,-18.2,11.6));
#144352=CARTESIAN_POINT('',(2.4,-18.2,11.6));
#144353=CARTESIAN_POINT('Origin',(3.59031095959199E-16,-18.2,11.6));
#144354=CARTESIAN_POINT('Origin',(1.04273619012177E-16,-18.2,11.6));
#144355=CARTESIAN_POINT('',(4.15,-18.2,14.1));
#144356=CARTESIAN_POINT('',(4.15,-18.2,11.6));
#144357=CARTESIAN_POINT('Origin',(6.59385131324756E-16,-18.2,14.1));
#144358=CARTESIAN_POINT('Origin',(3.46711834583204E-16,-18.2,11.5));
#144359=CARTESIAN_POINT('',(2.1,-18.2,11.4));
#144360=CARTESIAN_POINT('',(2.25,-18.2,11.5));
#144361=CARTESIAN_POINT('Origin',(3.3439257320721E-16,-18.2,11.4));
#144362=CARTESIAN_POINT('Origin',(7.1,-24.4,10.2));
#144363=CARTESIAN_POINT('',(9.9,-25.4,10.2));
#144364=CARTESIAN_POINT('Origin',(7.1,-25.4,10.2));
#144365=CARTESIAN_POINT('',(9.9,-20.8,10.2));
#144366=CARTESIAN_POINT('',(9.9,-24.4,10.2));
#144367=CARTESIAN_POINT('Origin',(7.1,-20.8,10.2));
#144368=CARTESIAN_POINT('Origin',(8.49999999999959,-14.8,14.199999999963));
#144369=CARTESIAN_POINT('Ctrl Pts',(7.29999999999962,-12.2182788550814,
12.9928480087538));
#144370=CARTESIAN_POINT('Ctrl Pts',(7.23242869523073,-12.2160163080132,
12.9976868903941));
#144371=CARTESIAN_POINT('Ctrl Pts',(7.16556025075935,-12.2149468090407,
13.));
#144372=CARTESIAN_POINT('Ctrl Pts',(6.84067152517238,-12.2149468090407,
13.));
#144373=CARTESIAN_POINT('Ctrl Pts',(6.56105708740227,-12.231704090976,12.9613548244849));
#144374=CARTESIAN_POINT('Ctrl Pts',(6.03441613857713,-12.3138039205035,
12.8038566188284));
#144375=CARTESIAN_POINT('Ctrl Pts',(5.78755856457603,-12.3805717968042,
12.6851850087052));
#144376=CARTESIAN_POINT('Ctrl Pts',(5.55598060272308,-12.4860759700654,
12.5360460877507));
#144377=CARTESIAN_POINT('Ctrl Pts',(5.52791362209311,-12.4996785494448,
12.517261610228));
#144378=CARTESIAN_POINT('Ctrl Pts',(5.49999999999963,-12.5141521334422,
12.4978250586149));
#144379=CARTESIAN_POINT('Origin',(7.1,-24.4,10.2));
#144380=CARTESIAN_POINT('',(8.7,-20.8,10.2));
#144381=CARTESIAN_POINT('Origin',(7.1,-20.8,10.2));
#144382=CARTESIAN_POINT('',(8.7,-10.3,10.2));
#144383=CARTESIAN_POINT('',(8.7,-24.4,10.2));
#144384=CARTESIAN_POINT('Origin',(7.1,-10.3,10.2));
#144385=CARTESIAN_POINT('Origin',(11.4999886762478,-10.3,10.1900175708635));
#144386=CARTESIAN_POINT('',(11.5845457335763,-19.4622952671594,9.59600569888119));
#144387=CARTESIAN_POINT('',(11.5845457335763,-10.3,9.59600569888119));
#144388=CARTESIAN_POINT('Ctrl Pts',(11.5845457335763,-19.4622952671594,
9.59600569888118));
#144389=CARTESIAN_POINT('Ctrl Pts',(11.526887976094,-19.4062489738839,9.58779816880506));
#144390=CARTESIAN_POINT('Ctrl Pts',(11.4697992967847,-19.3496507368366,
9.58839463648441));
#144391=CARTESIAN_POINT('Ctrl Pts',(11.4168221802075,-19.2961572437437,
9.59580941378689));
#144392=CARTESIAN_POINT('Ctrl Pts',(11.3465401866327,-19.2251902002209,
9.60564621436044));
#144393=CARTESIAN_POINT('Ctrl Pts',(11.272077928651,-19.1480722446802,9.62936914383039));
#144394=CARTESIAN_POINT('Ctrl Pts',(11.1344342252255,-19.0015084112899,
9.70768993967275));
#144395=CARTESIAN_POINT('Ctrl Pts',(11.0711979486242,-18.9320481917235,
9.76216454706022));
#144396=CARTESIAN_POINT('Ctrl Pts',(10.9874224914153,-18.8381784329961,
9.87316070906256));
#144397=CARTESIAN_POINT('Ctrl Pts',(10.9556614086042,-18.8019424520368,
9.92903001551857));
#144398=CARTESIAN_POINT('Ctrl Pts',(10.9117741849865,-18.7513211403521,
10.0543325101422));
#144399=CARTESIAN_POINT('Ctrl Pts',(10.8998372689763,-18.7372583002031,
10.1239619024751));
#144400=CARTESIAN_POINT('Ctrl Pts',(10.8999902203958,-18.7372583002031,
10.1913788112003));
#144401=CARTESIAN_POINT('Origin',(13.7499999999997,-14.8,14.199999999963));
#144402=CARTESIAN_POINT('',(13.8999999999996,-14.8,11.899999999963));
#144403=CARTESIAN_POINT('Origin',(13.8999999999996,-14.8,14.199999999963));
#144404=CARTESIAN_POINT('',(13.5999999999997,-14.8,12.199999999963));
#144405=CARTESIAN_POINT('',(13.7499999999997,-14.8,12.049999999963));
#144406=CARTESIAN_POINT('Origin',(13.5999999999997,-14.8,14.199999999963));
#144407=CARTESIAN_POINT('Origin',(13.8999999999996,-14.8,14.199999999963));
#144408=CARTESIAN_POINT('',(8.49999999999959,-14.8,12.199999999963));
#144409=CARTESIAN_POINT('',(13.8999999999996,-14.8,12.199999999963));
#144410=CARTESIAN_POINT('Origin',(8.49999999999959,-14.8,14.199999999963));
#144411=CARTESIAN_POINT('Origin',(13.4954867544557,-19.9,8.99159012270411));
#144412=CARTESIAN_POINT('',(13.5220680886962,-10.3,8.59247430909859));
#144413=CARTESIAN_POINT('',(13.8952427952371,-10.3,8.97762202123065));
#144414=CARTESIAN_POINT('Origin',(13.4954867544557,-10.3,8.99159012270412));
#144415=CARTESIAN_POINT('',(13.8952427952371,-15.9,8.97762202123065));
#144416=CARTESIAN_POINT('',(13.8952427952371,-19.9,8.97762202123064));
#144417=CARTESIAN_POINT('',(13.5220680886962,-15.9,8.59247430909859));
#144418=CARTESIAN_POINT('Origin',(13.4954867544557,-15.9,8.99159012270412));
#144419=CARTESIAN_POINT('',(13.5220680886962,-19.9,8.59247430909859));
#144420=CARTESIAN_POINT('Origin',(9.25,-21.1,-3.05000000003699));
#144421=CARTESIAN_POINT('',(0.634274193548384,-10.3,2.68513459542314));
#144422=CARTESIAN_POINT('',(0.634274193548383,-15.9,2.68513459542314));
#144423=CARTESIAN_POINT('',(0.634274193548383,-15.7,2.68513459542314));
#144424=CARTESIAN_POINT('',(4.72983031395648,-10.3,6.26077687460528));
#144425=CARTESIAN_POINT('Origin',(9.25,-10.3,-3.05000000003699));
#144426=CARTESIAN_POINT('',(4.72983031395648,-15.9,6.26077687460528));
#144427=CARTESIAN_POINT('',(4.72983031395648,-15.7,6.26077687460528));
#144428=CARTESIAN_POINT('Origin',(9.25,-15.9,-3.05000000003699));
#144429=CARTESIAN_POINT('Origin',(0.0099462365591374,-15.7,3.10072405886228));
#144430=CARTESIAN_POINT('',(-0.616835877496162,-15.9,2.68884521563242));
#144431=CARTESIAN_POINT('',(-0.616835877496162,-10.3,2.68884521563242));
#144432=CARTESIAN_POINT('',(-0.616835877496162,-15.7,2.68884521563242));
#144433=CARTESIAN_POINT('Origin',(0.0099462365591374,-10.3,3.10072405886228));
#144434=CARTESIAN_POINT('Origin',(0.0099462365591374,-15.9,3.10072405886228));
#144435=CARTESIAN_POINT('Origin',(-5.41858467284464,-21.1,25.4463470699242));
#144436=CARTESIAN_POINT('',(-0.459727007153424,-10.3,16.7624694423079));
#144437=CARTESIAN_POINT('',(-0.459727007153423,-21.1,16.7624694423079));
#144438=CARTESIAN_POINT('Origin',(-5.41858467284464,-10.3,25.4463470699242));
#144439=CARTESIAN_POINT('Origin',(0.748897957688959,-10.3,17.4526448948953));
#144440=CARTESIAN_POINT('',(0.748897957688964,-10.3,17.4526448948953));
#144441=CARTESIAN_POINT('',(0.748897957688964,-10.3,17.4526448948953));
#144442=CARTESIAN_POINT('',(-0.362541436325646,-10.3,16.8179664718101));
#144443=CARTESIAN_POINT('Origin',(0.550543651061315,-10.3,17.8));
#144444=CARTESIAN_POINT('',(0.550543651061315,-10.3,18.2));
#144445=CARTESIAN_POINT('Origin',(0.550543651061315,-10.3,17.8));
#144446=CARTESIAN_POINT('',(0.550543651061315,-10.3,18.2));
#144447=CARTESIAN_POINT('Origin',(8.6,-19.9,-0.741996797474057));
#144448=CARTESIAN_POINT('',(6.1,-20.,-0.741996797474058));
#144449=CARTESIAN_POINT('',(6.09999999999987,-23.,-0.741996797474058));
#144450=CARTESIAN_POINT('',(7.99320388349507,-20.,1.68324514365152));
#144451=CARTESIAN_POINT('Origin',(8.6,-20.,-0.741996797474057));
#144452=CARTESIAN_POINT('',(7.99320388349492,-22.1690497294436,1.68324514365148));
#144453=CARTESIAN_POINT('',(7.99320388349507,-19.9,1.68324514365152));
#144454=CARTESIAN_POINT('',(7.14318637525862,-22.1759507871132,1.28967592783578));
#144455=CARTESIAN_POINT('Ctrl Pts',(7.14318637525862,-22.1759507871132,
1.28967592783578));
#144456=CARTESIAN_POINT('Ctrl Pts',(7.27634231486309,-22.1482114428875,
1.38515557109449));
#144457=CARTESIAN_POINT('Ctrl Pts',(7.41971691376916,-22.1341795264265,
1.46792856779323));
#144458=CARTESIAN_POINT('Ctrl Pts',(7.70527732150551,-22.1341795264265,
1.59720438867895));
#144459=CARTESIAN_POINT('Ctrl Pts',(7.84789476028797,-22.1458682109901,
1.64688876610433));
#144460=CARTESIAN_POINT('Ctrl Pts',(7.99320388349492,-22.1690497294436,
1.68324514365148));
#144461=CARTESIAN_POINT('',(6.10539366127889,-23.,-0.57786509787753));
#144462=CARTESIAN_POINT('Ctrl Pts',(6.10539366127889,-23.,-0.577865097877531));
#144463=CARTESIAN_POINT('Ctrl Pts',(6.11813237646687,-22.890355013293,-0.384251799939226));
#144464=CARTESIAN_POINT('Ctrl Pts',(6.15396251435404,-22.7894964256895,
-0.191486226472621));
#144465=CARTESIAN_POINT('Ctrl Pts',(6.29596367302553,-22.562167115317,0.272007126052555));
#144466=CARTESIAN_POINT('Ctrl Pts',(6.4444684430105,-22.4335682956343,0.56671497320216));
#144467=CARTESIAN_POINT('Ctrl Pts',(6.79236654041548,-22.2678733559761,
0.999597022742));
#144468=CARTESIAN_POINT('Ctrl Pts',(6.96001166618957,-22.2141101536678,
1.15833025953227));
#144469=CARTESIAN_POINT('Ctrl Pts',(7.14318637525862,-22.1759507871132,
1.28967592783578));
#144470=CARTESIAN_POINT('',(6.10539366127889,-23.,-0.57786509787753));
#144471=CARTESIAN_POINT('Origin',(3.34425313716315E-18,-18.2,18.2));
#144472=CARTESIAN_POINT('',(3.1,-18.2,18.2));
#144473=CARTESIAN_POINT('Origin',(3.34425313716343E-18,-18.2,18.2));
#144474=CARTESIAN_POINT('',(3.1,-18.2,16.1));
#144475=CARTESIAN_POINT('',(3.1,-18.2,18.2));
#144476=CARTESIAN_POINT('Origin',(8.48627692340407E-16,-18.2,16.1));
#144477=CARTESIAN_POINT('Origin',(6.1,-22.1,2.59986263839934));
#144478=CARTESIAN_POINT('',(6.1,-20.,-5.32716721908225));
#144479=CARTESIAN_POINT('',(6.09999999999996,-23.,-5.32716721908225));
#144480=CARTESIAN_POINT('',(6.1,-20.,1.07493131918839));
#144481=CARTESIAN_POINT('Origin',(8.6,-21.,-5.32716721908225));
#144482=CARTESIAN_POINT('',(7.74383561643836,-22.1349879358347,-7.67599299983325));
#144483=CARTESIAN_POINT('Ctrl Pts',(7.74383561643836,-22.1349879358347,
-7.67599299983324));
#144484=CARTESIAN_POINT('Ctrl Pts',(7.56929610419344,-22.1414472919843,
-7.61237205564362));
#144485=CARTESIAN_POINT('Ctrl Pts',(7.3994612412714,-22.1582279470408,-7.52800380534636));
#144486=CARTESIAN_POINT('Ctrl Pts',(6.96320155009549,-22.2327613073737,
-7.24588019257465));
#144487=CARTESIAN_POINT('Ctrl Pts',(6.72532955663053,-22.3135747988836,
-7.00860235960015));
#144488=CARTESIAN_POINT('Ctrl Pts',(6.55177992406772,-22.4120688591538,
-6.76062266678474));
#144489=CARTESIAN_POINT('Ctrl Pts',(6.36059256319116,-22.5205728021874,
-6.48744097045821));
#144490=CARTESIAN_POINT('Ctrl Pts',(6.22126616693759,-22.6644734037083,
-6.16555726477482));
#144491=CARTESIAN_POINT('Ctrl Pts',(6.13107715207365,-22.8859742655692,
-5.73441170350023));
#144492=CARTESIAN_POINT('Ctrl Pts',(6.11613067119341,-22.9421215186625,
-5.6292985619738));
#144493=CARTESIAN_POINT('Ctrl Pts',(6.10786135295693,-23.,-5.52527063630252));
#144494=CARTESIAN_POINT('',(7.74383561643836,-20.,-7.67599299983325));
#144495=CARTESIAN_POINT('',(7.74383561643836,-21.,-7.67599299983325));
#144496=CARTESIAN_POINT('Origin',(8.6,-20.,-5.32716721908225));
#144497=CARTESIAN_POINT('Origin',(-5.42954084321747,-21.1,-4.25000000003699));
#144498=CARTESIAN_POINT('',(-5.42954084321747,-20.,-3.65000000003699));
#144499=CARTESIAN_POINT('Origin',(-5.42954084321747,-20.,-4.25000000003699));
#144500=CARTESIAN_POINT('',(-5.42954084321747,-21.1,-3.65000000003699));
#144501=CARTESIAN_POINT('Origin',(9.25,-22.55,-3.05000000003699));
#144502=CARTESIAN_POINT('',(7.5030745174711,-23.,0.548367874220887));
#144503=CARTESIAN_POINT('Origin',(9.25,-23.,-3.05000000003699));
#144504=CARTESIAN_POINT('Origin',(9.25,-22.55,-3.05000000003699));
#144505=CARTESIAN_POINT('',(11.3899837160979,-22.1,-7.4580006460029));
#144506=CARTESIAN_POINT('',(10.9969254825289,-23.,-6.64836787429488));
#144507=CARTESIAN_POINT('',(8.05573019712722,-22.1,-7.8022331212071));
#144508=CARTESIAN_POINT('Origin',(9.25,-22.1,-3.05000000003699));
#144509=CARTESIAN_POINT('Ctrl Pts',(8.05573019725203,-22.0999999999764,
-7.80223312126278));
#144510=CARTESIAN_POINT('Ctrl Pts',(7.95316899134432,-22.1193813623634,
-7.75647475434377));
#144511=CARTESIAN_POINT('Ctrl Pts',(7.84883301855934,-22.1311021932522,
-7.7142653301181));
#144512=CARTESIAN_POINT('Ctrl Pts',(7.74383561643836,-22.1349879358347,
-7.67599299983325));
#144513=CARTESIAN_POINT('Origin',(-10.2709990938499,-21.1,-7.04521722430998));
#144514=CARTESIAN_POINT('Origin',(-10.2709990938499,-20.,-7.04521722430998));
#144515=CARTESIAN_POINT('Origin',(-9.35,-19.7,-3.05000000003699));
#144516=CARTESIAN_POINT('',(-10.9,-19.7,-3.05000000003699));
#144517=CARTESIAN_POINT('Origin',(-9.35,-19.7,-3.05000000003699));
#144518=CARTESIAN_POINT('Origin',(-8.47750127826606,-18.3,10.5062825051013));
#144519=CARTESIAN_POINT('',(-11.5275012782661,-18.3,10.5062825051013));
#144520=CARTESIAN_POINT('Origin',(-8.47750127826606,-18.3,10.5062825051013));
#144521=CARTESIAN_POINT('',(-6.47750127826606,-18.3,10.5062825051013));
#144522=CARTESIAN_POINT('Origin',(-8.47750127826606,-18.3,10.5062825051013));
#144523=CARTESIAN_POINT('Origin',(-9.35,-22.1,-3.05000000003699));
#144524=CARTESIAN_POINT('',(-10.9,-23.2,-3.05000000003699));
#144525=CARTESIAN_POINT('',(-10.9,-22.1,-3.05000000003699));
#144526=CARTESIAN_POINT('Origin',(-9.35,-23.2,-3.05000000003699));
#144527=CARTESIAN_POINT('Origin',(-8.47750127826606,-18.5,10.5062825051013));
#144528=CARTESIAN_POINT('',(-6.47750127826606,-24.4,10.5062825051013));
#144529=CARTESIAN_POINT('',(-6.47750127826606,-18.5,10.5062825051013));
#144530=CARTESIAN_POINT('Origin',(-8.47750127826606,-24.4,10.5062825051013));
#144531=CARTESIAN_POINT('Origin',(-0.100000000022575,-23.2,-0.450000000022577));
#144532=CARTESIAN_POINT('Origin',(-8.47750127826606,-24.4,10.5062825051013));
#144533=CARTESIAN_POINT('Origin',(15.1,-22.55,-15.1));
#144534=CARTESIAN_POINT('',(16.4999999999948,-23.,-5.80993508719201));
#144535=CARTESIAN_POINT('',(16.4999999999931,-22.1,-6.72119489704348));
#144536=CARTESIAN_POINT('Ctrl Pts',(16.4999999999948,-23.0000000000039,
-5.80993508718805));
#144537=CARTESIAN_POINT('Ctrl Pts',(16.4999999999939,-22.5267915597811,
-6.2884866616241));
#144538=CARTESIAN_POINT('Ctrl Pts',(16.4999999999931,-22.1,-6.72119489704349));
#144539=CARTESIAN_POINT('Origin',(15.1,-22.1,-15.1));
#144540=CARTESIAN_POINT('Origin',(15.1,-23.,-15.1));
#144541=CARTESIAN_POINT('Origin',(15.1,-15.7,-15.1));
#144542=CARTESIAN_POINT('Origin',(15.1,-10.3,-15.1));
#144543=CARTESIAN_POINT('Origin',(15.1,-15.9,-15.1));
#144544=CARTESIAN_POINT('Origin',(8.49999999999959,-14.8,14.199999999963));
#144545=CARTESIAN_POINT('',(8.49999999999962,-14.8,12.549999999963));
#144546=CARTESIAN_POINT('Origin',(8.49999999999959,-14.8,14.199999999963));
#144547=CARTESIAN_POINT('',(8.49999999999962,-14.8,12.549999999963));
#144548=CARTESIAN_POINT('Origin',(8.49999999999959,-14.8,14.199999999963));
#144549=CARTESIAN_POINT('Origin',(7.25435078580463E-16,-18.2,15.1));
#144550=CARTESIAN_POINT('',(3.625,-18.2,15.1));
#144551=CARTESIAN_POINT('Origin',(-2.57959738503056E-16,-18.2,6.59999999999999));
#144552=CARTESIAN_POINT('',(2.1,-18.2,6.59999999999999));
#144553=CARTESIAN_POINT('Origin',(-1.98514478612865E-16,-18.2,6.59999999999999));
#144554=CARTESIAN_POINT('',(1.2,-18.2,6.59999999999999));
#144555=CARTESIAN_POINT('Origin',(1.14718080875314E-15,-18.2,6.59999999999999));
#144556=CARTESIAN_POINT('Origin',(1.12870191668915E-15,-18.2,6.44999999999999));
#144557=CARTESIAN_POINT('',(-1.,-18.2,6.29999999999999));
#144558=CARTESIAN_POINT('',(1.,-18.2,6.29999999999999));
#144559=CARTESIAN_POINT('Origin',(1.11022302462516E-15,-18.2,6.29999999999999));
#144560=CARTESIAN_POINT('',(1.1,-18.2,6.44999999999999));
#144561=CARTESIAN_POINT('Origin',(1.11022302462516E-15,-18.2,6.29999999999999));
#144562=CARTESIAN_POINT('Origin',(7.1,-19.3686291501015,10.2));
#144563=CARTESIAN_POINT('',(5.32995029238257,-17.7372583002031,12.369544660191));
#144564=CARTESIAN_POINT('Origin',(7.1,-17.7372583002031,10.2));
#144565=CARTESIAN_POINT('Ctrl Pts',(5.32295533692169,-18.7372583002029,
13.5588855689683));
#144566=CARTESIAN_POINT('Ctrl Pts',(5.34297156764967,-18.5389449337303,
13.3451179243545));
#144567=CARTESIAN_POINT('Ctrl Pts',(5.350772928081,-18.3486971007653,13.1310218147186));
#144568=CARTESIAN_POINT('Ctrl Pts',(5.34926297347848,-18.0331996694862,
12.755024908149));
#144569=CARTESIAN_POINT('Ctrl Pts',(5.34159640421336,-17.8714005164436,
12.5521693415744));
#144570=CARTESIAN_POINT('Ctrl Pts',(5.32995029238257,-17.7372583002031,
12.369544660191));
#144571=CARTESIAN_POINT('Origin',(7.1,-19.3686291501015,10.2));
#144572=CARTESIAN_POINT('',(4.89412386071569,-17.7372583002031,8.47543905351648));
#144573=CARTESIAN_POINT('Ctrl Pts',(4.89412386071568,-17.7372583002031,
8.47543905351647));
#144574=CARTESIAN_POINT('Ctrl Pts',(4.93436452953714,-17.7372583002031,
8.42396744193725));
#144575=CARTESIAN_POINT('Ctrl Pts',(4.9669696527347,-17.7511306117407,8.36381545146218));
#144576=CARTESIAN_POINT('Ctrl Pts',(5.00922761570301,-17.8008285638029,
8.24239426982826));
#144577=CARTESIAN_POINT('Ctrl Pts',(5.01915235870633,-17.8362967472096,
8.18107382133259));
#144578=CARTESIAN_POINT('Ctrl Pts',(5.0239204625628,-17.9281186662182,8.04624688172536));
#144579=CARTESIAN_POINT('Ctrl Pts',(5.01003668161719,-17.9961660277199,
7.96621461494606));
#144580=CARTESIAN_POINT('Ctrl Pts',(4.95550714282828,-18.139449903377,7.82176351540889));
#144581=CARTESIAN_POINT('Ctrl Pts',(4.91473826352193,-18.2147014671034,
7.75740612148749));
#144582=CARTESIAN_POINT('Ctrl Pts',(4.86860064468514,-18.2838984063394,
7.70583542702161));
#144583=CARTESIAN_POINT('Ctrl Pts',(4.81723293471555,-18.3609394066135,
7.64841875613479));
#144584=CARTESIAN_POINT('Ctrl Pts',(4.75012706774148,-18.444132170492,7.59666483773002));
#144585=CARTESIAN_POINT('Ctrl Pts',(4.67225419943427,-18.5232262216458,
7.56083038410712));
#144586=CARTESIAN_POINT('',(4.30011215770157,-17.7372583002031,10.1749386642522));
#144587=CARTESIAN_POINT('Ctrl Pts',(4.30011215770158,-17.7372583002031,
10.1749386642522));
#144588=CARTESIAN_POINT('Ctrl Pts',(4.19159461984128,-17.8468421420048,
10.0553192575359));
#144589=CARTESIAN_POINT('Ctrl Pts',(4.08369135164002,-17.9632436979253,
9.9388527734317));
#144590=CARTESIAN_POINT('Ctrl Pts',(3.78934767167766,-18.2915555175059,
9.63507652193826));
#144591=CARTESIAN_POINT('Ctrl Pts',(3.60197212932834,-18.5118359362721,
9.45659171009935));
#144592=CARTESIAN_POINT('Ctrl Pts',(3.40807692379815,-18.7372583002031,
9.30016445979934));
#144593=CARTESIAN_POINT('Origin',(7.1,-17.7372583002031,10.2));
#144594=CARTESIAN_POINT('Origin',(7.1,-19.3686291501015,10.2));
#144595=CARTESIAN_POINT('',(10.6037224484923,-18.5232262216426,9.43639346681366));
#144596=CARTESIAN_POINT('Ctrl Pts',(10.6037224531807,-18.5232262260405,
9.4363934676728));
#144597=CARTESIAN_POINT('Ctrl Pts',(10.5194042997935,-18.4441321735666,
9.42094222224999));
#144598=CARTESIAN_POINT('Ctrl Pts',(10.4347432389821,-18.3609394080404,
9.42470659861854));
#144599=CARTESIAN_POINT('Ctrl Pts',(10.3597035517405,-18.2838984063394,
9.4421525517822));
#144600=CARTESIAN_POINT('Ctrl Pts',(10.2923041596806,-18.2147014671034,
9.4578222151345));
#144601=CARTESIAN_POINT('Ctrl Pts',(10.2219460850893,-18.139449903377,9.4870406513017));
#144602=CARTESIAN_POINT('Ctrl Pts',(10.0942809753824,-17.9961660277199,
9.57388079479276));
#144603=CARTESIAN_POINT('Ctrl Pts',(10.0369085244781,-17.9281186662182,
9.63138144675786));
#144604=CARTESIAN_POINT('Ctrl Pts',(9.96329423056347,-17.8362967472096,
9.74443884010165));
#144605=CARTESIAN_POINT('Ctrl Pts',(9.93615995461258,-17.8008285638029,
9.80031753904868));
#144606=CARTESIAN_POINT('Ctrl Pts',(9.90092737860809,-17.7511306117407,
9.92396018691622));
#144607=CARTESIAN_POINT('Ctrl Pts',(9.89302208195365,-17.7372583002031,
9.9919223992231));
#144608=CARTESIAN_POINT('Ctrl Pts',(9.89635480722185,-17.7372583002031,
10.0571721591311));
#144609=CARTESIAN_POINT('Ctrl Pts',(10.6037224484923,-18.5232262216426,
9.43639346681366));
#144610=CARTESIAN_POINT('Ctrl Pts',(10.9243634589968,-18.8240012734338,
9.4951507156968));
#144611=CARTESIAN_POINT('Ctrl Pts',(11.2507529726933,-19.1378316080336,
9.54849059868016));
#144612=CARTESIAN_POINT('Ctrl Pts',(11.5845457335763,-19.4622952671594,
9.59600569888119));
#144613=CARTESIAN_POINT('Origin',(7.1,-20.8,10.2));
#144614=CARTESIAN_POINT('Origin',(3.56597033699713E-16,-18.2,11.6));
#144615=CARTESIAN_POINT('',(2.1,-18.2,11.6));
#144616=CARTESIAN_POINT('Origin',(1.04273619012177E-16,-18.2,11.6));
#144617=CARTESIAN_POINT('',(4.4846606338756,-15.2827548956307,11.2));
#144618=CARTESIAN_POINT('Ctrl Pts',(4.48466063387559,-15.2827548956307,
11.2));
#144619=CARTESIAN_POINT('Ctrl Pts',(4.54827264874599,-15.3805452042008,
11.366367006649));
#144620=CARTESIAN_POINT('Ctrl Pts',(4.62296913595049,-15.5030834282367,
11.5130892578383));
#144621=CARTESIAN_POINT('Ctrl Pts',(4.80528294110503,-15.8368475963683,
11.8187844172933));
#144622=CARTESIAN_POINT('Ctrl Pts',(4.93705801232801,-16.1205392330633,
11.9835651254983));
#144623=CARTESIAN_POINT('Ctrl Pts',(5.12599278618915,-16.6428387391747,
12.19077642575));
#144624=CARTESIAN_POINT('Ctrl Pts',(5.21110280172174,-16.9473520403291,
12.2682274318723));
#144625=CARTESIAN_POINT('Ctrl Pts',(5.29517632124998,-17.4195096846515,
12.3410243821726));
#144626=CARTESIAN_POINT('Ctrl Pts',(5.3162453081633,-17.5794015851531,12.3583632801737));
#144627=CARTESIAN_POINT('Ctrl Pts',(5.32995029238257,-17.7372583002031,
12.369544660191));
#144628=CARTESIAN_POINT('Origin',(1.54557770421648E-17,-18.2,11.2));
#144629=CARTESIAN_POINT('Origin',(7.25077700072151E-16,-18.2,14.3958530281318));
#144630=CARTESIAN_POINT('Origin',(1.54557770421648E-17,-18.2,11.2));
#144631=CARTESIAN_POINT('Origin',(3.56597033699713E-16,-18.2,11.6));
#144632=CARTESIAN_POINT('Origin',(8.45923926665497E-17,-18.2,9.14999999999999));
#144633=CARTESIAN_POINT('Origin',(-2.42923399597872E-16,-18.2,6.19999999999999));
#144634=CARTESIAN_POINT('Origin',(-2.42923399597872E-16,-18.2,6.19999999999999));
#144635=CARTESIAN_POINT('Origin',(1.17797896219313E-15,-18.2,5.64999999999999));
#144636=CARTESIAN_POINT('Ctrl Pts',(2.3,-20.5664319132398,6.19999999999999));
#144637=CARTESIAN_POINT('Ctrl Pts',(2.27958604839685,-20.5471301887928,
6.17193081654566));
#144638=CARTESIAN_POINT('Ctrl Pts',(2.2595024242038,-20.5281396051547,6.14431583328021));
#144639=CARTESIAN_POINT('Origin',(1.17797896219313E-15,-18.2,5.64999999999999));
#144640=CARTESIAN_POINT('Origin',(1.11022302462516E-15,-18.2,5.09999999999999));
#144641=CARTESIAN_POINT('Origin',(1.11022302462516E-15,-18.2,-19.1));
#144642=CARTESIAN_POINT('Origin',(-5.536176502776,-10.3,16.5874694585077));
#144643=CARTESIAN_POINT('',(-4.16287082888301,-15.6648219347062,15.302374052251));
#144644=CARTESIAN_POINT('',(-4.16287082888302,-10.3,15.302374052251));
#144645=CARTESIAN_POINT('',(-4.16287082888302,-10.3,15.302374052251));
#144646=CARTESIAN_POINT('Origin',(4.4806864735526,-18.2,7.21401033669983));
#144647=CARTESIAN_POINT('',(-1.73395719574401,-10.3,13.0294745722009));
#144648=CARTESIAN_POINT('Origin',(-3.65042002992564,-10.3,15.85));
#144649=CARTESIAN_POINT('',(-4.18196358468572,-17.1622932649853,16.3791138340594));
#144650=CARTESIAN_POINT('Ctrl Pts',(-4.18187625800635,-17.1623114267662,
16.3792076522946));
#144651=CARTESIAN_POINT('Ctrl Pts',(-4.19394811587314,-17.1587260110058,
16.3670919708574));
#144652=CARTESIAN_POINT('Ctrl Pts',(-4.21680216810472,-17.1442366946548,
16.3422127058649));
#144653=CARTESIAN_POINT('Ctrl Pts',(-4.24674448939413,-17.1067250534971,
16.305735840826));
#144654=CARTESIAN_POINT('Ctrl Pts',(-4.28111161194148,-17.0288513854137,
16.2575852802216));
#144655=CARTESIAN_POINT('Ctrl Pts',(-4.3164940870397,-16.8690652334165,
16.197184839744));
#144656=CARTESIAN_POINT('Ctrl Pts',(-4.33114148592674,-16.682242226022,
16.164479258454));
#144657=CARTESIAN_POINT('Ctrl Pts',(-4.33276019641122,-16.4943822165373,
16.1612288892188));
#144658=CARTESIAN_POINT('Ctrl Pts',(-4.32419391032616,-16.3065945433838,
16.1795042852215));
#144659=CARTESIAN_POINT('Ctrl Pts',(-4.29214178574177,-16.075454478799,
16.2446281088384));
#144660=CARTESIAN_POINT('Ctrl Pts',(-4.15704520376224,-15.7158195120752,
16.4317690537223));
#144661=CARTESIAN_POINT('Ctrl Pts',(-3.89740878663184,-15.4677167334541,
16.6));
#144662=CARTESIAN_POINT('Ctrl Pts',(-3.65042002992564,-15.3215437309242,
16.6));
#144663=CARTESIAN_POINT('Ctrl Pts',(-4.16287082888297,-15.6648219347062,
15.302374052251));
#144664=CARTESIAN_POINT('Ctrl Pts',(-4.25484771496768,-15.9027259587502,
15.3884430724526));
#144665=CARTESIAN_POINT('Ctrl Pts',(-4.3183020446404,-16.1518334302826,
15.4924169890107));
#144666=CARTESIAN_POINT('Ctrl Pts',(-4.39472128107487,-16.6187968527348,
15.7017962064845));
#144667=CARTESIAN_POINT('Ctrl Pts',(-4.41570619245039,-16.912665600934,
15.8343457381435));
#144668=CARTESIAN_POINT('Ctrl Pts',(-4.38320717254138,-17.174369879551,
16.0121523282015));
#144669=CARTESIAN_POINT('Ctrl Pts',(-4.37587758335711,-17.2167793786262,
16.0437248374513));
#144670=CARTESIAN_POINT('Ctrl Pts',(-4.35929935835897,-17.2687407400561,
16.0956008187188));
#144671=CARTESIAN_POINT('Ctrl Pts',(-4.35285886199348,-17.2840306332906,
16.1136122575154));
#144672=CARTESIAN_POINT('Ctrl Pts',(-4.33744597327384,-17.3076885865545,
16.1515317596741));
#144673=CARTESIAN_POINT('Ctrl Pts',(-4.32848093244943,-17.3160588866582,
16.1714414131769));
#144674=CARTESIAN_POINT('Ctrl Pts',(-4.31735930687918,-17.3183300903997,
16.1930626777379));
#144675=CARTESIAN_POINT('Ctrl Pts',(-4.31061548133341,-17.3197072813252,
16.2061731745225));
#144676=CARTESIAN_POINT('Ctrl Pts',(-4.30342160786703,-17.3186208202269,
16.2191885665456));
#144677=CARTESIAN_POINT('Ctrl Pts',(-4.28859108025688,-17.3118976847781,
16.2442727939903));
#144678=CARTESIAN_POINT('Ctrl Pts',(-4.28095308507075,-17.3062247464623,
16.2563311027636));
#144679=CARTESIAN_POINT('Ctrl Pts',(-4.25810464024748,-17.2846822200441,
16.2904427701345));
#144680=CARTESIAN_POINT('Ctrl Pts',(-4.24290182089397,-17.2638318647245,
16.3103432232216));
#144681=CARTESIAN_POINT('Ctrl Pts',(-4.2135428425112,-17.2188943338578,
16.3459997875122));
#144682=CARTESIAN_POINT('Ctrl Pts',(-4.19780490989408,-17.1914425505379,
16.3631997645882));
#144683=CARTESIAN_POINT('Ctrl Pts',(-4.18196358468572,-17.1622932649853,
16.3791138340594));
#144684=CARTESIAN_POINT('Origin',(-3.65042002992564,-10.3,15.85));
#144685=CARTESIAN_POINT('Origin',(11.2999999999996,-10.3,12.6));
#144686=CARTESIAN_POINT('',(11.7999999999996,-11.8066740905561,12.6));
#144687=CARTESIAN_POINT('',(11.8999999999998,-11.8066740905561,12.6));
#144688=CARTESIAN_POINT('',(13.8999999999996,-11.8066740905561,12.6000000000001));
#144689=CARTESIAN_POINT('',(11.7999999999996,-10.3,12.6));
#144690=CARTESIAN_POINT('',(11.7999999999996,-10.3,12.6));
#144691=CARTESIAN_POINT('',(11.8999999999996,-10.3,12.6));
#144692=CARTESIAN_POINT('',(11.2999999999996,-10.3,12.6));
#144693=CARTESIAN_POINT('',(11.8999999999996,-10.3,12.6));
#144694=CARTESIAN_POINT('Origin',(11.2999999999996,-10.3,16.6));
#144695=CARTESIAN_POINT('',(11.2999999999996,-10.3,16.2));
#144696=CARTESIAN_POINT('',(11.2999999999996,-11.8066740906056,16.2));
#144697=CARTESIAN_POINT('',(11.2999999999996,-10.3,16.2));
#144698=CARTESIAN_POINT('',(11.2999999999996,-10.3,13.1));
#144699=CARTESIAN_POINT('',(11.2999999999996,-10.3,16.6));
#144700=CARTESIAN_POINT('',(11.2999999999996,-11.3721726997876,13.1));
#144701=CARTESIAN_POINT('',(11.2999999999996,-10.3,13.1));
#144702=CARTESIAN_POINT('Origin',(11.2999999999996,-14.8,14.199999999963));
#144703=CARTESIAN_POINT('Origin',(11.7999999999996,-10.3,13.1));
#144704=CARTESIAN_POINT('Ctrl Pts',(11.2999999999996,-11.3721726997876,
13.1));
#144705=CARTESIAN_POINT('Ctrl Pts',(11.2999999999996,-11.4587530856937,
12.950109792686));
#144706=CARTESIAN_POINT('Ctrl Pts',(11.4173949896311,-11.6750919324497,
12.702604689212));
#144707=CARTESIAN_POINT('Ctrl Pts',(11.6819358373965,-11.8066740905561,
12.6));
#144708=CARTESIAN_POINT('Ctrl Pts',(11.7999999999996,-11.8066740905561,
12.6));
#144709=CARTESIAN_POINT('Origin',(11.7999999999996,-10.3,13.1));
#144710=CARTESIAN_POINT('Origin',(11.8999999999997,-14.8,14.199999999963));
#144711=CARTESIAN_POINT('',(11.8999999999998,-12.1392658582721,12.4222222222182));
#144712=CARTESIAN_POINT('Origin',(11.8999999999998,-11.8066740905561,12.2000000000001));
#144713=CARTESIAN_POINT('Origin',(11.8999999999997,-14.8,14.199999999963));
#144714=CARTESIAN_POINT('Origin',(13.8999999999996,-14.8,14.199999999963));
#144715=CARTESIAN_POINT('',(10.8999999999996,-11.7530423998112,13.2222222222181));
#144716=CARTESIAN_POINT('',(10.8999999999996,-12.1392658583161,15.9777777777737));
#144717=CARTESIAN_POINT('Origin',(10.8999999999996,-14.8,14.199999999963));
#144718=CARTESIAN_POINT('',(11.7999999999996,-12.1392658582721,12.4222222222181));
#144719=CARTESIAN_POINT('Ctrl Pts',(11.7999999999996,-12.1392658582721,
12.4222222222181));
#144720=CARTESIAN_POINT('Ctrl Pts',(11.587484507314,-12.1392658582721,12.4222222222181));
#144721=CARTESIAN_POINT('Ctrl Pts',(11.1113109813363,-12.0223039399553,
12.5863897249574));
#144722=CARTESIAN_POINT('Ctrl Pts',(10.8999999999996,-11.8300027428388,
12.9823978905158));
#144723=CARTESIAN_POINT('Ctrl Pts',(10.8999999999996,-11.7530423998112,
13.2222222222181));
#144724=CARTESIAN_POINT('',(13.8999999999996,-12.1392658582721,12.4222222222182));
#144725=CARTESIAN_POINT('Ctrl Pts',(8.72186658824407,-12.1000000000251,
12.4824435961918));
#144726=CARTESIAN_POINT('Ctrl Pts',(8.70882337879446,-12.0731544895491,
12.5246447594989));
#144727=CARTESIAN_POINT('Ctrl Pts',(8.69229019349259,-12.0478221085961,
12.5666605881537));
#144728=CARTESIAN_POINT('Ctrl Pts',(8.6341741057584,-11.9787672316304,12.6870768342024));
#144729=CARTESIAN_POINT('Ctrl Pts',(8.57970250797918,-11.9362210326303,
12.7697041881164));
#144730=CARTESIAN_POINT('Ctrl Pts',(8.44647017591476,-11.86550775675,12.9210429686623));
#144731=CARTESIAN_POINT('Ctrl Pts',(8.36788263061954,-11.8370629769507,
12.9897769287426));
#144732=CARTESIAN_POINT('Ctrl Pts',(8.13014000727059,-11.770919657986,13.1608510380605));
#144733=CARTESIAN_POINT('Ctrl Pts',(7.93448701836192,-11.7429091928131,
13.2523731799822));
#144734=CARTESIAN_POINT('Ctrl Pts',(7.70170765487302,-11.7236773606694,
13.3189227526333));
#144735=CARTESIAN_POINT('Ctrl Pts',(7.67591374269582,-11.7217258906158,
13.3257732799122));
#144736=CARTESIAN_POINT('Ctrl Pts',(7.64999999999965,-11.7199299841877,
13.3321470759639));
#144737=CARTESIAN_POINT('',(13.8999999999996,-12.1392658583161,15.9777777777737));
#144738=CARTESIAN_POINT('Origin',(13.8999999999996,-11.8066740906056,16.2));
#144739=CARTESIAN_POINT('Origin',(10.8999999999996,-11.8066740906056,16.2));
#144740=CARTESIAN_POINT('Origin',(11.8999999999998,-11.8066740905561,12.2000000000001));
#144741=CARTESIAN_POINT('Origin',(11.8999999999997,-11.8066740905561,12.2));
#144742=CARTESIAN_POINT('Origin',(11.8999999999998,-11.8066740905561,12.2000000000001));
#144743=CARTESIAN_POINT('Origin',(11.8999999999997,-10.3,12.2));
#144744=CARTESIAN_POINT('Origin',(11.8999999999997,-10.3,12.2));
#144745=CARTESIAN_POINT('Origin',(10.8999999999996,-11.8066740906056,16.2));
#144746=CARTESIAN_POINT('Origin',(10.8999999999996,-11.8066740906056,16.2));
#144747=CARTESIAN_POINT('Origin',(10.8999999999996,-11.8066740906056,16.2));
#144748=CARTESIAN_POINT('Origin',(13.8999999999996,-11.8066740905561,12.2000000000001));
#144749=CARTESIAN_POINT('Origin',(11.7999999999996,-11.8066740905561,12.2));
#144750=CARTESIAN_POINT('Ctrl Pts',(11.7999999999996,-11.8066740905561,
12.6));
#144751=CARTESIAN_POINT('Ctrl Pts',(11.6819358373965,-11.8066740905561,
12.6));
#144752=CARTESIAN_POINT('Ctrl Pts',(11.4173949896311,-11.6750919324497,
12.702604689212));
#144753=CARTESIAN_POINT('Ctrl Pts',(11.2999999999996,-11.4587530856937,
12.950109792686));
#144754=CARTESIAN_POINT('Ctrl Pts',(11.2999999999996,-11.3721726997876,
13.1));
#144755=CARTESIAN_POINT('Ctrl Pts',(11.7999999999996,-11.8721251143289,
12.6));
#144756=CARTESIAN_POINT('Ctrl Pts',(11.6716366670667,-11.8721251143289,
12.6));
#144757=CARTESIAN_POINT('Ctrl Pts',(11.3853622217568,-11.7474710537238,
12.7239006626482));
#144758=CARTESIAN_POINT('Ctrl Pts',(11.2901909346614,-11.5500696929581,
12.9883381875986));
#144759=CARTESIAN_POINT('Ctrl Pts',(11.2999999999996,-11.471884154085,13.1319977029522));
#144760=CARTESIAN_POINT('Ctrl Pts',(11.7999999999996,-12.0029536410931,
12.5672054150641));
#144761=CARTESIAN_POINT('Ctrl Pts',(11.6432129484504,-12.0029536410931,
12.5672054150641));
#144762=CARTESIAN_POINT('Ctrl Pts',(11.2939898772465,-11.8923755833045,
12.7224346897746));
#144763=CARTESIAN_POINT('Ctrl Pts',(11.1953517025113,-11.732454125104,13.0376950947528));
#144764=CARTESIAN_POINT('Ctrl Pts',(11.2132967619966,-11.670485809188,13.1957295661626));
#144765=CARTESIAN_POINT('Ctrl Pts',(11.7999999999996,-12.102904178399,12.4766434014566));
#144766=CARTESIAN_POINT('Ctrl Pts',(11.6060763489285,-12.1029041783991,
12.4766434014566));
#144767=CARTESIAN_POINT('Ctrl Pts',(11.172110277341,-11.9919204949165,12.6401816400886));
#144768=CARTESIAN_POINT('Ctrl Pts',(10.9985531508785,-11.8206425682432,
13.0109145504288));
#144769=CARTESIAN_POINT('Ctrl Pts',(11.0047197551193,-11.7530423998112,
13.2222222222181));
#144770=CARTESIAN_POINT('Ctrl Pts',(11.7999999999996,-12.1392658582721,
12.4222222222181));
#144771=CARTESIAN_POINT('Ctrl Pts',(11.587484507314,-12.1392658582721,12.4222222222181));
#144772=CARTESIAN_POINT('Ctrl Pts',(11.1113109813363,-12.0223039399553,
12.5863897249574));
#144773=CARTESIAN_POINT('Ctrl Pts',(10.8999999999996,-11.8300027428388,
12.9823978905158));
#144774=CARTESIAN_POINT('Ctrl Pts',(10.8999999999996,-11.7530423998112,
13.2222222222181));
#144775=CARTESIAN_POINT('Origin',(10.8999999999996,-11.3721726997876,13.1));
#144776=CARTESIAN_POINT('Origin',(10.8999999999996,-14.8,14.199999999963));
#144777=CARTESIAN_POINT('Origin',(10.8999999999996,-10.3,16.2));
#144778=CARTESIAN_POINT('Origin',(10.8999999999996,-10.3,16.2));
#144779=CARTESIAN_POINT('Origin',(7.1,-24.4,10.2));
#144780=CARTESIAN_POINT('',(4.89412386071569,-12.1,8.47543905351648));
#144781=CARTESIAN_POINT('',(4.89412386071569,-10.3,8.47543905351648));
#144782=CARTESIAN_POINT('Ctrl Pts',(4.30011215770157,-17.7372583002031,
10.1749386642522));
#144783=CARTESIAN_POINT('Ctrl Pts',(4.30001128733287,-17.6309935487308,
10.1862080443775));
#144784=CARTESIAN_POINT('Ctrl Pts',(4.29993438568727,-17.5236929545511,
10.2015325229438));
#144785=CARTESIAN_POINT('Ctrl Pts',(4.30043239221638,-17.1514858680764,
10.2686927199916));
#144786=CARTESIAN_POINT('Ctrl Pts',(4.30231487297464,-16.8903956938801,
10.3420198077238));
#144787=CARTESIAN_POINT('Ctrl Pts',(4.31743469546803,-16.3800007039129,
10.5281842790581));
#144788=CARTESIAN_POINT('Ctrl Pts',(4.33744031191061,-16.0600796813261,
10.6822846029848));
#144789=CARTESIAN_POINT('Ctrl Pts',(4.39372574524066,-15.6586384458731,
10.9243170138561));
#144790=CARTESIAN_POINT('Ctrl Pts',(4.42716844435502,-15.4866311493459,
11.0416565744492));
#144791=CARTESIAN_POINT('Ctrl Pts',(4.47109045903957,-15.3281474321327,
11.1639384262309));
#144792=CARTESIAN_POINT('Ctrl Pts',(4.47769342258432,-15.3054612836516,
11.1817783780378));
#144793=CARTESIAN_POINT('Ctrl Pts',(4.4846606338756,-15.2827548956307,11.2));
#144794=CARTESIAN_POINT('Origin',(7.1,-12.1,10.2));
#144795=CARTESIAN_POINT('Origin',(4.42143611658333,-10.3,8.10589027927001));
#144796=CARTESIAN_POINT('Ctrl Pts',(4.67225419943745,-11.3140320785605,
7.56083038410858));
#144797=CARTESIAN_POINT('Ctrl Pts',(4.75012706774333,-11.3931261297133,
7.59666483773142));
#144798=CARTESIAN_POINT('Ctrl Pts',(4.81723293471625,-11.4763188935906,
7.64841875613557));
#144799=CARTESIAN_POINT('Ctrl Pts',(4.86860064468514,-11.5533598938637,
7.70583542702161));
#144800=CARTESIAN_POINT('Ctrl Pts',(4.91473826352193,-11.6225568330996,
7.75740612148749));
#144801=CARTESIAN_POINT('Ctrl Pts',(4.95550714282828,-11.6978083968261,
7.82176351540889));
#144802=CARTESIAN_POINT('Ctrl Pts',(5.01003668161719,-11.8410922724832,
7.96621461494606));
#144803=CARTESIAN_POINT('Ctrl Pts',(5.0239204625628,-11.9091396339848,8.04624688172536));
#144804=CARTESIAN_POINT('Ctrl Pts',(5.01915235870633,-12.0009615529934,
8.18107382133259));
#144805=CARTESIAN_POINT('Ctrl Pts',(5.00922761570301,-12.0364297364002,
8.24239426982826));
#144806=CARTESIAN_POINT('Ctrl Pts',(4.9669696527347,-12.0861276884624,8.36381545146218));
#144807=CARTESIAN_POINT('Ctrl Pts',(4.93436452953714,-12.1,8.42396744193725));
#144808=CARTESIAN_POINT('Ctrl Pts',(4.89412386071568,-12.1,8.47543905351647));
#144809=CARTESIAN_POINT('Origin',(15.1,-10.3,-15.1000000000002));
#144810=CARTESIAN_POINT('',(11.7798591918362,-10.3,9.6230212796182));
#144811=CARTESIAN_POINT('',(11.7798591918362,-10.3,9.6230212796182));
#144812=CARTESIAN_POINT('Origin',(15.1,-10.3,-15.1000000000002));
#144813=CARTESIAN_POINT('',(10.6037224484923,-11.3140320785605,9.43639346681366));
#144814=CARTESIAN_POINT('Ctrl Pts',(10.6037224484923,-11.3140320785605,
9.43639346681366));
#144815=CARTESIAN_POINT('Ctrl Pts',(10.608707598078,-11.309355793944,9.43730699211245));
#144816=CARTESIAN_POINT('Ctrl Pts',(10.6136918678395,-11.3046784029656,
9.43821878587495));
#144817=CARTESIAN_POINT('Ctrl Pts',(10.618675187344,-11.3,9.43912883747022));
#144818=CARTESIAN_POINT('Ctrl Pts',(10.8716162365519,-11.0625357648361,
9.48532081956795));
#144819=CARTESIAN_POINT('Ctrl Pts',(11.1281188708098,-10.8169580561747,
9.52813260756565));
#144820=CARTESIAN_POINT('Ctrl Pts',(11.3890749660464,-10.5645232201992,
9.56739044915099));
#144821=CARTESIAN_POINT('',(10.6037224484923,-10.3,9.43639346681366));
#144822=CARTESIAN_POINT('Origin',(7.1,-11.7,10.2));
#144823=CARTESIAN_POINT('Ctrl Pts',(9.89635480722185,-12.1,10.0571721591311));
#144824=CARTESIAN_POINT('Ctrl Pts',(9.89302208195365,-12.1,9.99192239922311));
#144825=CARTESIAN_POINT('Ctrl Pts',(9.90092737860809,-12.0861276884624,
9.92396018691622));
#144826=CARTESIAN_POINT('Ctrl Pts',(9.93615995461258,-12.0364297364002,
9.80031753904868));
#144827=CARTESIAN_POINT('Ctrl Pts',(9.96329423056347,-12.0009615529934,
9.74443884010165));
#144828=CARTESIAN_POINT('Ctrl Pts',(10.0369085244781,-11.9091396339848,
9.63138144675786));
#144829=CARTESIAN_POINT('Ctrl Pts',(10.0942809753824,-11.8410922724832,
9.57388079479276));
#144830=CARTESIAN_POINT('Ctrl Pts',(10.2219460850893,-11.6978083968261,
9.48704065130171));
#144831=CARTESIAN_POINT('Ctrl Pts',(10.2923041596806,-11.6225568330996,
9.4578222151345));
#144832=CARTESIAN_POINT('Ctrl Pts',(10.3597035517405,-11.5533598938637,
9.4421525517822));
#144833=CARTESIAN_POINT('Ctrl Pts',(10.4347432375913,-11.4763188935906,
9.4247065989419));
#144834=CARTESIAN_POINT('Ctrl Pts',(10.5194042966525,-11.3931261297133,
9.42094222236673));
#144835=CARTESIAN_POINT('Ctrl Pts',(10.6037224484923,-11.3140320785605,
9.43639346681366));
#144836=CARTESIAN_POINT('Origin',(10.4955736944837,-10.3,10.0265661932306));
#144837=CARTESIAN_POINT('Ctrl Pts',(-4.15558608030974,-17.0949638327396,
16.3958525879769));
#144838=CARTESIAN_POINT('Ctrl Pts',(-4.15558499113943,-17.0949600091324,
16.3958530281318));
#144839=CARTESIAN_POINT('Ctrl Pts',(-4.15225602908945,-17.082431601768,
16.3958530281318));
#144840=CARTESIAN_POINT('Ctrl Pts',(-4.14264067399083,-17.0470960648441,
16.3958530281318));
#144841=CARTESIAN_POINT('Ctrl Pts',(-4.12242181413037,-16.9757326797749,
16.3958530281318));
#144842=CARTESIAN_POINT('Ctrl Pts',(-4.07716739275611,-16.8287774262104,
16.3958530281318));
#144843=CARTESIAN_POINT('Ctrl Pts',(-4.0172093385339,-16.6621227828839,
16.3958530281318));
#144844=CARTESIAN_POINT('Ctrl Pts',(-3.9509934453542,-16.5015111868501,
16.3958530281318));
#144845=CARTESIAN_POINT('Ctrl Pts',(-3.88102031079464,-16.3453037878245,
16.3958530281318));
#144846=CARTESIAN_POINT('Ctrl Pts',(-3.7880821209169,-16.1604212714353,
16.3958530281318));
#144847=CARTESIAN_POINT('Ctrl Pts',(-3.62588443732701,-15.8785354637891,
16.3958530281318));
#144848=CARTESIAN_POINT('Ctrl Pts',(-3.48316325575844,-15.6727047931632,
16.3958530281318));
#144849=CARTESIAN_POINT('Ctrl Pts',(-3.37654926102705,-15.5374983403089,
16.3958530281318));
#144850=CARTESIAN_POINT('Ctrl Pts',(-4.15864956755341,-17.106484576438,
16.3958530281318));
#144851=CARTESIAN_POINT('Ctrl Pts',(-4.16166551294798,-17.1061109850393,
16.3930613132255));
#144852=CARTESIAN_POINT('Ctrl Pts',(-4.1640449424804,-17.0929074595252,
16.3888332106743));
#144853=CARTESIAN_POINT('Ctrl Pts',(-4.16285653706035,-17.0565722710498,
16.3842705686255));
#144854=CARTESIAN_POINT('Ctrl Pts',(-4.1546283879313,-16.9836856368366,
16.3802789513044));
#144855=CARTESIAN_POINT('Ctrl Pts',(-4.12819280007378,-16.8338876916016,
16.3795050583179));
#144856=CARTESIAN_POINT('Ctrl Pts',(-4.084909445423,-16.6638724411723,16.3868078748572));
#144857=CARTESIAN_POINT('Ctrl Pts',(-4.03044710954714,-16.500694908825,
16.3993030153564));
#144858=CARTESIAN_POINT('Ctrl Pts',(-3.96829324310505,-16.3426975171319,
16.4144180987784));
#144859=CARTESIAN_POINT('Ctrl Pts',(-3.87688666777836,-16.1572121716626,
16.436082235871));
#144860=CARTESIAN_POINT('Ctrl Pts',(-3.69817616932894,-15.8750570428302,
16.4661169180521));
#144861=CARTESIAN_POINT('Ctrl Pts',(-3.52791761123353,-15.6602065606675,
16.472559675109));
#144862=CARTESIAN_POINT('Ctrl Pts',(-3.40369690428402,-15.516091679354,
16.4574186477821));
#144863=CARTESIAN_POINT('Ctrl Pts',(-4.16407740090863,-17.1297201895698,
16.3950704330864));
#144864=CARTESIAN_POINT('Ctrl Pts',(-4.17309867009879,-17.1286064742394,
16.3866195493542));
#144865=CARTESIAN_POINT('Ctrl Pts',(-4.18636378592173,-17.1141977739953,
16.3731958794539));
#144866=CARTESIAN_POINT('Ctrl Pts',(-4.2007971294629,-17.0762147421848,
16.3573798048861));
#144867=CARTESIAN_POINT('Ctrl Pts',(-4.21449765860984,-17.00093000886,16.3407443488439));
#144868=CARTESIAN_POINT('Ctrl Pts',(-4.22313388349631,-16.8464676114765,
16.3272957665252));
#144869=CARTESIAN_POINT('Ctrl Pts',(-4.21459807528536,-16.6696778592131,
16.3338317080614));
#144870=CARTESIAN_POINT('Ctrl Pts',(-4.19048552821278,-16.4985546366527,
16.356892527142));
#144871=CARTESIAN_POINT('Ctrl Pts',(-4.15397606217355,-16.3321688812547,
16.390284419557));
#144872=CARTESIAN_POINT('Ctrl Pts',(-4.08234299653493,-16.135908034094,
16.4481217202394));
#144873=CARTESIAN_POINT('Ctrl Pts',(-3.89286548876974,-15.8363272941988,
16.5528979639547));
#144874=CARTESIAN_POINT('Ctrl Pts',(-3.65781260387296,-15.6050158945688,
16.5971927661982));
#144875=CARTESIAN_POINT('Ctrl Pts',(-3.484171134057,-15.4526355429943,16.5617031069992));
#144876=CARTESIAN_POINT('Ctrl Pts',(-4.16805924125643,-17.1531430391027,
16.3927289346864));
#144877=CARTESIAN_POINT('Ctrl Pts',(-4.18298182306529,-17.1512963280167,
16.3785132377752));
#144878=CARTESIAN_POINT('Ctrl Pts',(-4.20588345022822,-17.1358278214066,
16.3545595711711));
#144879=CARTESIAN_POINT('Ctrl Pts',(-4.23261434468994,-17.0965546016377,
16.3238807136553));
#144880=CARTESIAN_POINT('Ctrl Pts',(-4.26155471740868,-17.0195426579297,
16.2870832365073));
#144881=CARTESIAN_POINT('Ctrl Pts',(-4.29142198289111,-16.8615280733557,
16.2438785345673));
#144882=CARTESIAN_POINT('Ctrl Pts',(-4.30284255427461,-16.6780413458487,
16.2257886933808));
#144883=CARTESIAN_POINT('Ctrl Pts',(-4.30015587581447,-16.495765620729,
16.2332149212329));
#144884=CARTESIAN_POINT('Ctrl Pts',(-4.28596701049521,-16.3151284088004,
16.2588392704518));
#144885=CARTESIAN_POINT('Ctrl Pts',(-4.24322921026512,-16.0956649254156,
16.3252794120497));
#144886=CARTESIAN_POINT('Ctrl Pts',(-4.08618086693028,-15.7561566065747,
16.4925437736698));
#144887=CARTESIAN_POINT('Ctrl Pts',(-3.82169923706759,-15.5135583824825,
16.6184335132367));
#144888=CARTESIAN_POINT('Ctrl Pts',(-3.59497510060098,-15.3652635777075,
16.6));
#144889=CARTESIAN_POINT('Ctrl Pts',(-4.16968069936174,-17.1648544705749,
16.3911731305015));
#144890=CARTESIAN_POINT('Ctrl Pts',(-4.18751555020898,-17.1626412633014,
16.3740604246625));
#144891=CARTESIAN_POINT('Ctrl Pts',(-4.21488136238738,-17.1466430737096,
16.344552703831));
#144892=CARTESIAN_POINT('Ctrl Pts',(-4.24674448939413,-17.1067250534971,
16.305735840826));
#144893=CARTESIAN_POINT('Ctrl Pts',(-4.28111161194148,-17.0288513854137,
16.2575852802216));
#144894=CARTESIAN_POINT('Ctrl Pts',(-4.3164940870397,-16.8690652334165,
16.197184839744));
#144895=CARTESIAN_POINT('Ctrl Pts',(-4.33114148592674,-16.682242226022,
16.164479258454));
#144896=CARTESIAN_POINT('Ctrl Pts',(-4.33276019641122,-16.4943822165373,
16.1612288892188));
#144897=CARTESIAN_POINT('Ctrl Pts',(-4.32419391032616,-16.3065945433838,
16.1795042852215));
#144898=CARTESIAN_POINT('Ctrl Pts',(-4.29214178574177,-16.075454478799,
16.2446281088384));
#144899=CARTESIAN_POINT('Ctrl Pts',(-4.15704520376224,-15.7158195120752,
16.4317690537223));
#144900=CARTESIAN_POINT('Ctrl Pts',(-3.89740878663184,-15.4677167334541,
16.6));
#144901=CARTESIAN_POINT('Ctrl Pts',(-3.65042002992564,-15.3215437309242,
16.6));
#144902=CARTESIAN_POINT('',(-4.15558499113943,-17.0949600091324,16.3958530281318));
#144903=CARTESIAN_POINT('Ctrl Pts',(-4.18187625800635,-17.1623114267662,
16.3792076522946));
#144904=CARTESIAN_POINT('Ctrl Pts',(-4.17634967961608,-17.1520585558519,
16.3847557199795));
#144905=CARTESIAN_POINT('Ctrl Pts',(-4.17124056639269,-17.14091999511,16.3890221165494));
#144906=CARTESIAN_POINT('Ctrl Pts',(-4.16669365147873,-17.1291585903885,
16.3918453420656));
#144907=CARTESIAN_POINT('Ctrl Pts',(-4.1624355815674,-17.1181443346773,
16.3944892207946));
#144908=CARTESIAN_POINT('Ctrl Pts',(-4.15869481542099,-17.1066547384278,
16.3958530346329));
#144909=CARTESIAN_POINT('Ctrl Pts',(-4.15558608030974,-17.0949638327396,
16.3958525879769));
#144910=CARTESIAN_POINT('',(-3.37654926102705,-15.5374983403089,16.3958530281318));
#144911=CARTESIAN_POINT('Origin',(-3.65042002992564,-15.3215437309242,16.2));
#144912=CARTESIAN_POINT('Origin',(8.85953015492336E-16,-18.2,16.3958530281318));
#144913=CARTESIAN_POINT('Origin',(1.07729948100197E-15,-18.2,16.2));
#144914=CARTESIAN_POINT('Origin',(8.85953015492336E-16,-18.2,16.3958530281318));
#144915=CARTESIAN_POINT('Origin',(17.5,-22.1,11.6));
#144916=CARTESIAN_POINT('',(16.3999999999996,-22.1,11.6));
#144917=CARTESIAN_POINT('',(16.3999999999996,-22.1,11.6));
#144918=CARTESIAN_POINT('',(16.9,-22.1,11.6));
#144919=CARTESIAN_POINT('',(8.74999999998871,-22.1,11.6));
#144920=CARTESIAN_POINT('',(16.9,-22.1,11.6));
#144921=CARTESIAN_POINT('Origin',(16.9,-22.1,11.));
#144922=CARTESIAN_POINT('Origin',(16.9,-22.1,11.));
#144923=CARTESIAN_POINT('Origin',(16.3999999999996,-22.1,15.7));
#144924=CARTESIAN_POINT('',(14.742553191489,-22.1,11.9499506567302));
#144925=CARTESIAN_POINT('',(14.742553191489,-22.1,11.9499506567302));
#144926=CARTESIAN_POINT('Origin',(16.3999999999996,-22.1,15.7));
#144927=CARTESIAN_POINT('Origin',(11.6999999999997,-10.3,10.2176829561026));
#144928=CARTESIAN_POINT('Origin',(11.6999999999997,-10.3,10.2176829561026));
#144929=CARTESIAN_POINT('Origin',(0.,-24.4,18.2));
#144930=CARTESIAN_POINT('',(-9.16862915008378,-25.4,18.2));
#144931=CARTESIAN_POINT('',(-9.16862915008378,-24.4,18.2));
#144932=CARTESIAN_POINT('',(12.8999999999995,-25.4,18.2));
#144933=CARTESIAN_POINT('',(-1.12865534254263E-11,-25.4,18.2));
#144934=CARTESIAN_POINT('',(12.8999999999995,-10.3,18.2));
#144935=CARTESIAN_POINT('',(12.8999999999995,-22.15,18.2));
#144936=CARTESIAN_POINT('',(-5.79396237474835,-10.3,18.2));
#144937=CARTESIAN_POINT('Origin',(12.8999999999995,-22.15,17.2));
#144938=CARTESIAN_POINT('',(13.8999999999995,-25.4,17.2));
#144939=CARTESIAN_POINT('Origin',(12.8999999999995,-25.4,17.2));
#144940=CARTESIAN_POINT('',(13.8999999999997,-10.3,17.2));
#144941=CARTESIAN_POINT('',(13.8999999999995,-22.15,17.2));
#144942=CARTESIAN_POINT('Origin',(12.8999999999995,-10.3,17.2));
#144943=CARTESIAN_POINT('Origin',(16.3999999999996,-22.15,15.7));
#144944=CARTESIAN_POINT('',(16.3999999999996,-25.4,13.2));
#144945=CARTESIAN_POINT('',(13.8999999999996,-25.4,15.6999999999999));
#144946=CARTESIAN_POINT('Origin',(16.3999999999996,-25.4,15.7));
#144947=CARTESIAN_POINT('',(16.3999999999996,-22.1,13.2));
#144948=CARTESIAN_POINT('',(16.3999999999996,-22.15,13.2));
#144949=CARTESIAN_POINT('',(13.8999999999996,-22.1,15.6999999999999));
#144950=CARTESIAN_POINT('Origin',(16.3999999999996,-22.1,15.7));
#144951=CARTESIAN_POINT('',(13.8999999999996,-22.15,15.6999999999999));
#144952=CARTESIAN_POINT('Origin',(19.1,-24.4,13.2));
#144953=CARTESIAN_POINT('',(18.1,-25.4,13.2));
#144954=CARTESIAN_POINT('',(9.54999999998872,-25.4,13.2));
#144955=CARTESIAN_POINT('',(18.1,-22.1,13.2));
#144956=CARTESIAN_POINT('',(18.1,-24.4,13.2));
#144957=CARTESIAN_POINT('',(9.54999999998872,-22.1,13.2));
#144958=CARTESIAN_POINT('Origin',(18.1,-24.4,12.2));
#144959=CARTESIAN_POINT('',(19.1,-25.4,12.2));
#144960=CARTESIAN_POINT('Origin',(18.1,-25.4,12.2));
#144961=CARTESIAN_POINT('',(19.1,-22.1,12.2));
#144962=CARTESIAN_POINT('',(19.1,-24.4,12.2));
#144963=CARTESIAN_POINT('Origin',(18.1,-22.1,12.2));
#144964=CARTESIAN_POINT('Origin',(15.1,-22.55,-15.1));
#144965=CARTESIAN_POINT('',(17.5765623826223,-22.1,3.02656238258888));
#144966=CARTESIAN_POINT('',(16.7650854557587,-23.,2.2150854557252));
#144967=CARTESIAN_POINT('Ctrl Pts',(17.5765623826223,-22.1,3.02656238258888));
#144968=CARTESIAN_POINT('Ctrl Pts',(17.1605923305092,-22.568450440311,2.61059233047568));
#144969=CARTESIAN_POINT('Ctrl Pts',(16.7650854557587,-23.,2.21508545572519));
#144970=CARTESIAN_POINT('Origin',(15.1,-23.,-15.1));
#144971=CARTESIAN_POINT('',(9.9082087163681,-22.1,2.44283125131488));
#144972=CARTESIAN_POINT('Ctrl Pts',(7.99320388349492,-22.1690497294436,
1.68324514365148));
#144973=CARTESIAN_POINT('Ctrl Pts',(8.26898312988902,-22.2130454645242,
1.75224517737468));
#144974=CARTESIAN_POINT('Ctrl Pts',(8.54092388752982,-22.2349444050467,
1.83645502172102));
#144975=CARTESIAN_POINT('Ctrl Pts',(9.18093316499991,-22.2349444050467,
2.07300875877398));
#144976=CARTESIAN_POINT('Ctrl Pts',(9.55380073243788,-22.1895443581543,
2.24456092434208));
#144977=CARTESIAN_POINT('Ctrl Pts',(9.9082087163681,-22.1,2.44283125131488));
#144978=CARTESIAN_POINT('Origin',(15.1,-22.1,-15.1));
#144979=CARTESIAN_POINT('Origin',(-2.25752749827279E-11,-22.1,-0.450000000022577));
#144980=CARTESIAN_POINT('Origin',(6.1,-22.1,-12.1857384988752));
#144981=CARTESIAN_POINT('',(16.4999999999912,-22.1,-7.7186291501247));
#144982=CARTESIAN_POINT('',(16.4999999999906,-22.1,-8.05000000002406));
#144983=CARTESIAN_POINT('Origin',(17.2999999999912,-22.1,-7.71862915012621));
#144984=CARTESIAN_POINT('Origin',(14.4999999999996,-22.1,11.401162947959));
#144985=CARTESIAN_POINT('',(13.8999999999996,-22.1,11.401162947959));
#144986=CARTESIAN_POINT('',(13.8999999999996,-22.1,11.401162947959));
#144987=CARTESIAN_POINT('Origin',(14.4999999999996,-22.1,11.401162947959));
#144988=CARTESIAN_POINT('Origin',(-13.9260346165329,-15.9,10.3798528337676));
#144989=CARTESIAN_POINT('Origin',(-13.9260346165329,-15.7,10.3798528337676));
#144990=CARTESIAN_POINT('Origin',(-12.3362327337785,-22.8,13.1010255664155));
#144991=CARTESIAN_POINT('',(-9.07157287523651,-15.7,16.3656854249499));
#144992=CARTESIAN_POINT('',(-9.07157287523651,-16.55,16.3656854249499));
#144993=CARTESIAN_POINT('',(-11.0195632919613,-15.7,14.4176950082296));
#144994=CARTESIAN_POINT('Origin',(-8.50588745028793,-16.55,15.8));
#144995=CARTESIAN_POINT('Origin',(-8.50588745028793,-15.7,15.8));
#144996=CARTESIAN_POINT('Origin',(-4.89034568556533,-10.3,14.3396641393448));
#144997=CARTESIAN_POINT('',(-7.07515042368407,-15.7,16.3841343442657));
#144998=CARTESIAN_POINT('',(-4.89034568556533,-15.7,14.3396641393448));
#144999=CARTESIAN_POINT('',(-7.07515042368407,-15.7,16.3841343442657));
#145000=CARTESIAN_POINT('',(-7.07515042368407,-10.3,16.3841343442657));
#145001=CARTESIAN_POINT('',(-7.07515042368407,-10.3,16.3841343442657));
#145002=CARTESIAN_POINT('',(-4.89034568556533,-10.3,14.3396641393448));
#145003=CARTESIAN_POINT('',(-1.82100242629958,-10.3,11.4674711544254));
#145004=CARTESIAN_POINT('',(-4.89034568556533,-21.1,14.3396641393448));
#145005=CARTESIAN_POINT('Origin',(-7.62176460923847,-10.3,15.8));
#145006=CARTESIAN_POINT('Origin',(-7.62176460923847,-15.7,15.8));
#145007=CARTESIAN_POINT('Origin',(-7.62176460923847,-10.3,15.8));
#145008=CARTESIAN_POINT('Origin',(-16.5000000000123,-24.4,1.94999999997646));
#145009=CARTESIAN_POINT('',(-16.5000000000305,-20.,-7.71862915012594));
#145010=CARTESIAN_POINT('',(-16.5000000000089,-20.,3.77623615174464));
#145011=CARTESIAN_POINT('',(-16.5000000000195,-20.,-1.85000000003706));
#145012=CARTESIAN_POINT('',(-16.5000000000305,-25.4,-7.71862915012594));
#145013=CARTESIAN_POINT('',(-16.5000000000305,-24.4,-7.71862915012594));
#145014=CARTESIAN_POINT('',(-16.4999999999955,-25.4,10.8686291501049));
#145015=CARTESIAN_POINT('',(-16.5000000000146,-25.4,0.749999999992473));
#145016=CARTESIAN_POINT('',(-16.4999999999955,-24.4,10.8686291501049));
#145017=CARTESIAN_POINT('',(-16.5000000000054,-15.9,5.6354763829797));
#145018=CARTESIAN_POINT('',(-16.5000000000054,-22.8,5.6354763829797));
#145019=CARTESIAN_POINT('',(-16.5000000000089,-15.9,3.77623615174464));
#145020=CARTESIAN_POINT('',(-16.4999999999949,-15.9,11.2000000000031));
#145021=CARTESIAN_POINT('',(-16.5000000000089,-19.9,3.77623615174464));
#145022=CARTESIAN_POINT('Origin',(-15.6999999999955,-24.4,10.8686291501034));
#145023=CARTESIAN_POINT('',(-16.2656854249441,-25.4,11.4343145750533));
#145024=CARTESIAN_POINT('Origin',(-15.6999999999955,-25.4,10.8686291501034));
#145025=CARTESIAN_POINT('',(-16.2656854249441,-24.4,11.4343145750533));
#145026=CARTESIAN_POINT('Origin',(-10.6033654998821,-24.4,17.0966345001022));
#145027=CARTESIAN_POINT('',(-9.73431457503237,-25.4,17.9656854249499));
#145028=CARTESIAN_POINT('',(-9.73431457503237,-24.4,17.9656854249499));
#145029=CARTESIAN_POINT('',(-12.3391827499422,-25.4,15.3608172500461));
#145030=CARTESIAN_POINT('Origin',(-9.16862915008378,-24.4,17.4));
#145031=CARTESIAN_POINT('Origin',(-9.16862915008378,-25.4,17.4));
#145032=CARTESIAN_POINT('Origin',(-2.25752749827279E-11,-22.1,-0.450000000022577));
#145033=CARTESIAN_POINT('',(18.8656854249492,-22.1,4.31568542491577));
#145034=CARTESIAN_POINT('',(19.1,-22.1,4.88137084986501));
#145035=CARTESIAN_POINT('Origin',(18.3,-22.1,4.881370849865));
#145036=CARTESIAN_POINT('',(11.7750000000018,-22.1,-2.77500000003169));
#145037=CARTESIAN_POINT('Origin',(6.09999999999969,-22.1,9.2499999999633));
#145038=CARTESIAN_POINT('',(13.8999999999997,-22.1,6.04557695250827));
#145039=CARTESIAN_POINT('',(19.1,-22.1,-19.1));
#145040=CARTESIAN_POINT('Origin',(19.1,-24.4,18.2));
#145041=CARTESIAN_POINT('',(19.1,-25.4,4.881370849865));
#145042=CARTESIAN_POINT('',(19.1,-24.4,4.881370849865));
#145043=CARTESIAN_POINT('',(19.1,-25.4,8.87499999998871));
#145044=CARTESIAN_POINT('Origin',(18.3,-24.4,4.881370849865));
#145045=CARTESIAN_POINT('',(18.8656854249492,-25.4,4.31568542491577));
#145046=CARTESIAN_POINT('Origin',(18.3,-25.4,4.881370849865));
#145047=CARTESIAN_POINT('',(18.8656854249492,-24.4,4.31568542491577));
#145048=CARTESIAN_POINT('Origin',(17.2999999999912,-24.4,-7.71862915012621));
#145049=CARTESIAN_POINT('',(16.4999999999912,-25.4,-7.7186291501247));
#145050=CARTESIAN_POINT('',(16.4999999999912,-24.4,-7.7186291501247));
#145051=CARTESIAN_POINT('Origin',(17.2999999999912,-25.4,-7.71862915012621));
#145052=CARTESIAN_POINT('Origin',(-8.47750127826606,-21.1,10.5062825051013));
#145053=CARTESIAN_POINT('',(-4.68280159094393,-15.7,6.87823147417057));
#145054=CARTESIAN_POINT('',(-4.68280159094394,-10.3,6.87823147417058));
#145055=CARTESIAN_POINT('',(-4.68280159094394,-15.7,6.87823147417058));
#145056=CARTESIAN_POINT('Origin',(-8.47750127826606,-15.7,10.5062825051013));
#145057=CARTESIAN_POINT('Origin',(-8.47750127826606,-10.3,10.5062825051013));
#145058=CARTESIAN_POINT('Origin',(2.24865810106615,-10.3,9.66425824155912));
#145059=CARTESIAN_POINT('',(-4.57640302989081,-10.3,6.24598149558596));
#145060=CARTESIAN_POINT('Origin',(-4.39368161476701,-10.3,6.60180853848062));
#145061=CARTESIAN_POINT('',(13.8999999999997,-10.3,9.24999999996345));
#145062=CARTESIAN_POINT('',(13.8999999999997,-10.3,7.8549175970337));
#145063=CARTESIAN_POINT('Origin',(6.09999999999969,-10.3,9.2499999999633));
#145064=CARTESIAN_POINT('Origin',(-9.35,-10.3,-3.05000000003699));
#145065=CARTESIAN_POINT('Origin',(-4.39368161476701,-15.7,6.60180853848062));
#145066=CARTESIAN_POINT('',(-4.57640302989081,-15.7,6.24598149558596));
#145067=CARTESIAN_POINT('',(-4.57640302989081,-15.7,6.24598149558596));
#145068=CARTESIAN_POINT('Origin',(-4.39368161476701,-15.7,6.60180853848062));
#145069=CARTESIAN_POINT('Origin',(-9.35,-15.7,-3.05000000003699));
#145070=CARTESIAN_POINT('',(-9.43222590492927,-15.7,7.39967649737471));
#145071=CARTESIAN_POINT('',(-7.92889383452772,-15.7,7.30292022888666));
#145072=CARTESIAN_POINT('Ctrl Pts',(-9.43222590492927,-15.7,7.39967649737471));
#145073=CARTESIAN_POINT('Ctrl Pts',(-9.19930785473307,-15.7701742479532,
7.40150927157174));
#145074=CARTESIAN_POINT('Ctrl Pts',(-8.95201593280048,-15.8156689756711,
7.39600675444461));
#145075=CARTESIAN_POINT('Ctrl Pts',(-8.40561223809871,-15.8156689756711,
7.36083955244824));
#145076=CARTESIAN_POINT('Ctrl Pts',(-8.15965523600794,-15.7701742479532,
7.33459597284539));
#145077=CARTESIAN_POINT('Ctrl Pts',(-7.92889383452772,-15.7,7.30292022888666));
#145078=CARTESIAN_POINT('Origin',(-9.35,-15.7,-3.05000000003699));
#145079=CARTESIAN_POINT('',(-11.4725028070433,-15.9,7.18217874322649));
#145080=CARTESIAN_POINT('Origin',(-9.35,-15.9,-3.05000000003699));
#145081=CARTESIAN_POINT('',(-11.4725028070433,-15.7,7.18217874322649));
#145082=CARTESIAN_POINT('',(-11.4725028070433,-15.7,7.18217874322649));
#145083=CARTESIAN_POINT('Origin',(-9.35,-15.7,-3.05000000003699));
#145084=CARTESIAN_POINT('Origin',(-11.5537469336287,-15.7,7.57384108746624));
#145085=CARTESIAN_POINT('Origin',(-11.5537469336287,-15.7,7.57384108746624));
#145086=CARTESIAN_POINT('Origin',(-11.5537469336287,-15.9,7.57384108746624));
#145087=CARTESIAN_POINT('Origin',(-8.47750127826606,-24.4,10.5062825051013));
#145088=CARTESIAN_POINT('',(-5.42750127826606,-15.9,10.5062825051013));
#145089=CARTESIAN_POINT('',(-11.5275012782661,-15.9,10.5062825051013));
#145090=CARTESIAN_POINT('Origin',(-8.47750127826606,-15.9,10.5062825051013));
#145091=CARTESIAN_POINT('Origin',(-8.47750127826606,-15.9,10.5062825051013));
#145092=CARTESIAN_POINT('',(-11.5275012782661,-24.4,10.5062825051013));
#145093=CARTESIAN_POINT('Origin',(-8.85961065987377,-15.7,11.5466726141172));
#145094=CARTESIAN_POINT('',(-5.22750127826606,-15.7,10.5062825051013));
#145095=CARTESIAN_POINT('Origin',(-8.47750127826606,-15.7,10.5062825051013));
#145096=CARTESIAN_POINT('Origin',(-8.47750127826606,-15.7,10.5062825051013));
#145097=CARTESIAN_POINT('Origin',(-8.47750127826606,-15.8,10.5062825051013));
#145098=CARTESIAN_POINT('',(-5.32750127826606,-15.8,10.5062825051013));
#145099=CARTESIAN_POINT('Origin',(-13.5133325473166,-19.9,5.36110350072047));
#145100=CARTESIAN_POINT('',(-10.7906143361206,-20.,0.645217224236));
#145101=CARTESIAN_POINT('',(-10.7906143361206,-21.1,0.645217224236));
#145102=CARTESIAN_POINT('',(-13.0883185289381,-20.,4.62495762695992));
#145103=CARTESIAN_POINT('',(-11.4476530870906,-20.,1.78324172345756));
#145104=CARTESIAN_POINT('',(-13.0883185289381,-19.9,4.62495762695993));
#145105=CARTESIAN_POINT('Origin',(-2.6403124237551,-20.,-0.450000000022575));
#145106=CARTESIAN_POINT('',(-0.00257311493774171,-20.,-4.50827945559669));
#145107=CARTESIAN_POINT('Origin',(-0.00257311493774171,-20.,-4.70827945559669));
#145108=CARTESIAN_POINT('',(-0.0974268850622617,-20.,-4.50827945559669));
#145109=CARTESIAN_POINT('',(8.27360890601114,-20.,-4.50827945559669));
#145110=CARTESIAN_POINT('Origin',(-0.0974268850622617,-20.,-4.70827945559669));
#145111=CARTESIAN_POINT('',(-0.600000000789417,-20.,-5.79545078503888));
#145112=CARTESIAN_POINT('Origin',(-1.20000000078942,-20.,-5.79545078503888));
#145113=CARTESIAN_POINT('',(-0.600000000789417,-20.,-4.25000000003699));
#145114=CARTESIAN_POINT('',(-0.600000000789418,-20.,-0.0326255494647287));
#145115=CARTESIAN_POINT('',(-1.20000000078942,-20.,-3.65000000003699));
#145116=CARTESIAN_POINT('Origin',(-1.20000000078942,-20.,-4.25000000003699));
#145117=CARTESIAN_POINT('',(-1.31220842229031,-20.,-3.65000000003699));
#145118=CARTESIAN_POINT('Origin',(-5.42954084321747,-20.,-1.85000000003699));
#145119=CARTESIAN_POINT('',(-0.0620826661477014,-20.,-1.80272960390294));
#145120=CARTESIAN_POINT('Origin',(-0.0620826661477014,-20.,-1.60272960390294));
#145121=CARTESIAN_POINT('',(-0.037917333852302,-20.,-1.80272960390294));
#145122=CARTESIAN_POINT('',(8.27360890601114,-20.,-1.80272960390295));
#145123=CARTESIAN_POINT('Origin',(-0.037917333852302,-20.,-1.60272960390295));
#145124=CARTESIAN_POINT('',(1.19999999921058,-20.,-2.45000000003699));
#145125=CARTESIAN_POINT('Origin',(1.19999999921058,-20.,-1.85000000003699));
#145126=CARTESIAN_POINT('',(4.3,-20.,-2.45000000003699));
#145127=CARTESIAN_POINT('',(-4.29148370813747,-20.,-2.45000000003699));
#145128=CARTESIAN_POINT('',(4.9,-20.,-1.85000000003699));
#145129=CARTESIAN_POINT('Origin',(4.3,-20.,-1.85000000003699));
#145130=CARTESIAN_POINT('',(4.9,-20.,-0.741996797474059));
#145131=CARTESIAN_POINT('',(4.9,-20.,-2.88858360955241));
#145132=CARTESIAN_POINT('Origin',(8.6,-20.,-0.741996797474057));
#145133=CARTESIAN_POINT('',(13.7548828365128,-20.,7.75241235336064));
#145134=CARTESIAN_POINT('Origin',(13.3623247423326,-20.,7.82921171985308));
#145135=CARTESIAN_POINT('Origin',(6.09999999999969,-20.,9.2499999999633));
#145136=CARTESIAN_POINT('Origin',(6.1,-20.,-12.1857384988752));
#145137=CARTESIAN_POINT('Origin',(-12.5687032866674,-19.9,4.92495762695992));
#145138=CARTESIAN_POINT('Origin',(-12.5687032866674,-20.,4.92495762695992));
#145139=CARTESIAN_POINT('Origin',(0.,-18.2,-19.1));
#145140=CARTESIAN_POINT('Origin',(0.,-18.2,1.41228796703553));
#145141=CARTESIAN_POINT('Origin',(0.,-18.2,0.728598564603416));
#145142=CARTESIAN_POINT('',(-1.,-18.2,-19.1));
#145143=CARTESIAN_POINT('Origin',(19.1875302357774,-18.9150528379807,-5.20109977862422));
#145144=CARTESIAN_POINT('',(0.192158240549244,-19.225912103606,-4.66267573655754));
#145145=CARTESIAN_POINT('Origin',(-7.13578540802763E-18,-17.9401923788647,
-6.889607624103));
#145146=CARTESIAN_POINT('',(-0.0974268850622617,-19.3150528379807,-4.50827945559669));
#145147=CARTESIAN_POINT('Origin',(-0.0974268850622617,-19.1995827841427,
-4.70827945559669));
#145148=CARTESIAN_POINT('',(-0.00257311493774059,-19.3150528379807,-4.50827945559669));
#145149=CARTESIAN_POINT('',(19.1875302357774,-19.3150528379807,-4.50827945559669));
#145150=CARTESIAN_POINT('Origin',(-0.00257311493774171,-19.1995827841427,
-4.70827945559669));
#145151=CARTESIAN_POINT('Origin',(19.1875302357774,-16.3150528379807,-1.80272960390295));
#145152=CARTESIAN_POINT('',(-0.0620826661477025,-15.9,-1.80272960390294));
#145153=CARTESIAN_POINT('',(-0.0620826661477025,-16.3150528379807,-1.80272960390294));
#145154=CARTESIAN_POINT('',(-0.0620826661477026,-19.9,-1.80272960390294));
#145155=CARTESIAN_POINT('',(-0.0379173338523009,-15.9,-1.80272960390294));
#145156=CARTESIAN_POINT('',(8.03659089635399,-15.9,-1.80272960390294));
#145157=CARTESIAN_POINT('',(-0.037917333852302,-16.3150528379807,-1.80272960390294));
#145158=CARTESIAN_POINT('',(-0.0379173338523009,-21.1,-1.80272960390294));
#145159=CARTESIAN_POINT('',(19.1875302357774,-16.3150528379807,-1.80272960390295));
#145160=CARTESIAN_POINT('Origin',(19.1875302357774,-15.8150528379807,-4.50827945559669));
#145161=CARTESIAN_POINT('',(-0.0974268850622617,-16.3150528379807,-4.50827945559669));
#145162=CARTESIAN_POINT('',(-0.0974268850622628,-15.9,-4.50827945559669));
#145163=CARTESIAN_POINT('',(-0.0974268850622628,-19.9,-4.50827945559669));
#145164=CARTESIAN_POINT('',(-0.00257311493774059,-16.3150528379807,-4.50827945559669));
#145165=CARTESIAN_POINT('',(19.1875302357774,-16.3150528379807,-4.50827945559669));
#145166=CARTESIAN_POINT('',(-0.00257311493774171,-15.9,-4.50827945559669));
#145167=CARTESIAN_POINT('',(-0.00257311493774168,-21.1,-4.50827945559669));
#145168=CARTESIAN_POINT('',(8.03659089635399,-15.9,-4.50827945559669));
#145169=CARTESIAN_POINT('Origin',(19.1875302357774,-16.3150528379807,-4.50827945559669));
#145170=CARTESIAN_POINT('Origin',(4.54783644736696E-17,-18.4457456132867,
-7.55122409562988));
#145171=CARTESIAN_POINT('Origin',(-0.00257311493774171,-16.4550943456226,
-4.70827945559669));
#145172=CARTESIAN_POINT('Origin',(-0.0974268850622628,-16.4550943456226,
-4.70827945559669));
#145173=CARTESIAN_POINT('Origin',(19.1875302357774,-19.3150528379807,-4.50827945559669));
#145174=CARTESIAN_POINT('',(-0.00257311493774168,-21.1,-4.50827945559669));
#145175=CARTESIAN_POINT('',(-0.0974268850622617,-19.9,-4.50827945559669));
#145176=CARTESIAN_POINT('Origin',(-0.0974268850622617,-19.9,-4.70827945559669));
#145177=CARTESIAN_POINT('Origin',(-0.00257311493774171,-21.1,-4.70827945559669));
#145178=CARTESIAN_POINT('Ctrl Pts',(0.192159868891087,-19.2258247671933,
-4.6628270076618));
#145179=CARTESIAN_POINT('Ctrl Pts',(0.192955152312465,-19.2238679775077,
-4.66621855530548));
#145180=CARTESIAN_POINT('Ctrl Pts',(0.193667594328148,-19.2219578017748,
-4.6696565646564));
#145181=CARTESIAN_POINT('Ctrl Pts',(0.194292330138919,-19.2200994892544,
-4.67313792326465));
#145182=CARTESIAN_POINT('Origin',(-0.00257311493774171,-21.1,-4.70827945559669));
#145183=CARTESIAN_POINT('Origin',(-0.00257311493774171,-15.9,-4.70827945559669));
#145184=CARTESIAN_POINT('Origin',(-0.0974268850622628,-19.9,-4.70827945559669));
#145185=CARTESIAN_POINT('Origin',(-0.0974268850622628,-15.9,-4.70827945559669));
#145186=CARTESIAN_POINT('Origin',(-0.0379173338523009,-21.1,-1.60272960390294));
#145187=CARTESIAN_POINT('Origin',(-0.0379173338523009,-15.9,-1.60272960390294));
#145188=CARTESIAN_POINT('Origin',(-0.0379173338523009,-16.4550943456226,
-1.60272960390294));
#145189=CARTESIAN_POINT('Origin',(-0.0620826661477025,-19.9,-1.60272960390294));
#145190=CARTESIAN_POINT('Origin',(-0.0620826661477025,-15.9,-1.60272960390294));
#145191=CARTESIAN_POINT('Origin',(-0.0620826661477025,-16.4550943456226,
-1.60272960390294));
#145192=CARTESIAN_POINT('Origin',(19.1875302357774,-19.9150528379807,-1.80272960390295));
#145193=CARTESIAN_POINT('',(-0.0620826661477025,-19.3150528379807,-1.80272960390294));
#145194=CARTESIAN_POINT('',(-0.0620826661477014,-19.9,-1.80272960390294));
#145195=CARTESIAN_POINT('',(-0.037917333852302,-19.3150528379807,-1.80272960390294));
#145196=CARTESIAN_POINT('',(19.1875302357774,-19.3150528379807,-1.80272960390295));
#145197=CARTESIAN_POINT('',(-0.037917333852302,-21.1,-1.80272960390295));
#145198=CARTESIAN_POINT('Origin',(-0.0620826661477014,-19.9,-1.60272960390294));
#145199=CARTESIAN_POINT('Origin',(-0.0620826661477014,-19.1995827841427,
-1.60272960390294));
#145200=CARTESIAN_POINT('Origin',(-0.037917333852302,-21.1,-1.60272960390295));
#145201=CARTESIAN_POINT('',(0.154550859259101,-19.2309727753312,-1.65709866349047));
#145202=CARTESIAN_POINT('Ctrl Pts',(0.159700282405874,-19.2185167914062,
-1.63346006998121));
#145203=CARTESIAN_POINT('Ctrl Pts',(0.158439401477663,-19.2223797827423,
-1.64154567165289));
#145204=CARTESIAN_POINT('Ctrl Pts',(0.156704150703268,-19.2265376018115,
-1.64941336612285));
#145205=CARTESIAN_POINT('Ctrl Pts',(0.1545517600316,-19.2309315391986,-1.65702724041366));
#145206=CARTESIAN_POINT('Origin',(-0.037917333852302,-19.1995827841427,
-1.60272960390295));
#145207=CARTESIAN_POINT('Origin',(19.1875302357774,-19.3150528379807,-1.80272960390295));
#145208=CARTESIAN_POINT('Origin',(-4.41432195622002E-17,-17.9401923788647,
0.578598564603414));
#145209=CARTESIAN_POINT('Ctrl Pts',(0.239413492381404,-19.2179565118977,
-1.63455383389902));
#145210=CARTESIAN_POINT('Ctrl Pts',(0.0329622508010724,-19.256639091472,
-1.70155402708951));
#145211=CARTESIAN_POINT('Ctrl Pts',(-0.182855485725863,-19.2442944946718,
-1.68017255823251));
#145212=CARTESIAN_POINT('Ctrl Pts',(-0.38354942837159,-19.1823235458498,
-1.57283572627961));
#145213=CARTESIAN_POINT('Ctrl Pts',(0.220025619949421,-19.1920879531095,
-1.58974817575931));
#145214=CARTESIAN_POINT('Ctrl Pts',(0.0304801589848503,-19.2302536493785,
-1.6557966353406));
#145215=CARTESIAN_POINT('Ctrl Pts',(-0.168404518381573,-19.2180965784821,
-1.63469104263094));
#145216=CARTESIAN_POINT('Ctrl Pts',(-0.35222244035206,-19.1569603036518,
-1.52890530214794));
#145217=CARTESIAN_POINT('Ctrl Pts',(0.200667423514428,-19.1798032977788,
-1.53719128952209));
#145218=CARTESIAN_POINT('Ctrl Pts',(0.0279861671460582,-19.2149481765117,
-1.60369891136253));
#145219=CARTESIAN_POINT('Ctrl Pts',(-0.15394211994542,-19.2036985468328,
-1.58245502005562));
#145220=CARTESIAN_POINT('Ctrl Pts',(-0.320960312691724,-19.1474811411372,
-1.4759254735363));
#145221=CARTESIAN_POINT('Ctrl Pts',(0.184164224908773,-19.1828954869485,
-1.48455383389902));
#145222=CARTESIAN_POINT('Ctrl Pts',(0.0253555775392867,-19.2126513173903,
-1.55155402708952));
#145223=CARTESIAN_POINT('Ctrl Pts',(-0.140658065942972,-19.2031554736978,
-1.53017255823251));
#145224=CARTESIAN_POINT('Ctrl Pts',(-0.295038021824301,-19.1554855130655,
-1.42283572627961));
#145225=CARTESIAN_POINT('Ctrl Pts',(-0.445894921065382,-19.1613302577989,
-4.77453477474201));
#145226=CARTESIAN_POINT('Ctrl Pts',(-0.210103453700173,-19.2474288217223,
-4.62540768756798));
#145227=CARTESIAN_POINT('Ctrl Pts',(0.0508640605567958,-19.2632280647536,
-4.59804259591671));
#145228=CARTESIAN_POINT('Ctrl Pts',(0.295320308048652,-19.2062041938388,
-4.69681083758541));
#145229=CARTESIAN_POINT('Ctrl Pts',(-0.409289944973037,-19.1362684546969,
-4.81794309104411));
#145230=CARTESIAN_POINT('Ctrl Pts',(-0.193645890390995,-19.2212017125735,
-4.67099311891243));
#145231=CARTESIAN_POINT('Ctrl Pts',(0.0470734714362628,-19.2367613684955,
-4.64397201463185));
#145232=CARTESIAN_POINT('Ctrl Pts',(0.271337754375829,-19.180501426813,
-4.7413293359692));
#145233=CARTESIAN_POINT('Ctrl Pts',(-0.37277385892892,-19.1284635659547,
-4.8711741434902));
#145234=CARTESIAN_POINT('Ctrl Pts',(-0.177157130011096,-19.2064969954954,
-4.72318393045555));
#145235=CARTESIAN_POINT('Ctrl Pts',(0.0432613162406244,-19.2209198881668,
-4.69598856904055));
#145236=CARTESIAN_POINT('Ctrl Pts',(0.247395954893676,-19.1691370458623,
-4.79402523679034));
#145237=CARTESIAN_POINT('Ctrl Pts',(-0.342996093127217,-19.1393368299494,
-4.92453477474201));
#145238=CARTESIAN_POINT('Ctrl Pts',(-0.161618041307826,-19.2055664945059,
-4.77540768756798));
#145239=CARTESIAN_POINT('Ctrl Pts',(0.0391262004283044,-19.2177197583761,
-4.74804259591671));
#145240=CARTESIAN_POINT('Ctrl Pts',(0.227169467729732,-19.1738552422878,
-4.84681083758542));
#145241=CARTESIAN_POINT('Origin',(0.,-18.2,-7.039607624103));
#145242=CARTESIAN_POINT('Ctrl Pts',(-0.605214914090967,-17.2952175137768,
-5.90809968361399));
#145243=CARTESIAN_POINT('Ctrl Pts',(-0.623018660594374,-17.3333600838434,
-5.96257291902663));
#145244=CARTESIAN_POINT('Ctrl Pts',(-0.648851205478286,-17.3868815961198,
-6.03900956010202));
#145245=CARTESIAN_POINT('Ctrl Pts',(-0.678920665712354,-17.4468307073562,
-6.12462576382018));
#145246=CARTESIAN_POINT('Ctrl Pts',(-0.689573580943891,-17.4676466969021,
-6.15435407779857));
#145247=CARTESIAN_POINT('Ctrl Pts',(-0.689576769163932,-17.4676488696199,
-6.15435513352118));
#145248=CARTESIAN_POINT('Ctrl Pts',(-0.55385925080104,-17.3273362577698,
-5.95397000382664));
#145249=CARTESIAN_POINT('Ctrl Pts',(-0.579124049415806,-17.3542551168377,
-6.00899666937624));
#145250=CARTESIAN_POINT('Ctrl Pts',(-0.618927029183115,-17.3956063549456,
-6.08234407992258));
#145251=CARTESIAN_POINT('Ctrl Pts',(-0.669540381817794,-17.4504718858759,
-6.15513440299772));
#145252=CARTESIAN_POINT('Ctrl Pts',(-0.690350066847747,-17.4737712704258,
-6.17528093750827));
#145253=CARTESIAN_POINT('Ctrl Pts',(-0.694897793055846,-17.478047099637,
-6.16920739223372));
#145254=CARTESIAN_POINT('Ctrl Pts',(-0.502781108682595,-17.3345631845704,
-6.01690035049276));
#145255=CARTESIAN_POINT('Ctrl Pts',(-0.539605351320391,-17.3562694270032,
-6.06711859772466));
#145256=CARTESIAN_POINT('Ctrl Pts',(-0.594604834126566,-17.393599725971,
-6.131228060911));
#145257=CARTESIAN_POINT('Ctrl Pts',(-0.663199682814476,-17.4507778603678,
-6.18690214327408));
#145258=CARTESIAN_POINT('Ctrl Pts',(-0.692581332696088,-17.4785619697096,
-6.19661963035754));
#145259=CARTESIAN_POINT('Ctrl Pts',(-0.701612310120372,-17.4873509901404,
-6.1843296238416));
#145260=CARTESIAN_POINT('Ctrl Pts',(-0.465549933916129,-17.3149783849924,
-6.0801726145193));
#145261=CARTESIAN_POINT('Ctrl Pts',(-0.511817975000622,-17.3393168679221,
-6.12535925716751));
#145262=CARTESIAN_POINT('Ctrl Pts',(-0.578223751373194,-17.3811061564651,
-6.18014514262514));
#145263=CARTESIAN_POINT('Ctrl Pts',(-0.66000814405107,-17.4476866284114,
-6.21866263408644));
#145264=CARTESIAN_POINT('Ctrl Pts',(-0.696213461155708,-17.4819138991659,
-6.21795888300343));
#145265=CARTESIAN_POINT('Ctrl Pts',(-0.709597871030093,-17.4953931156811,
-6.19945217637467));
#145266=CARTESIAN_POINT('',(-0.465549933916128,-17.3149783849924,-6.0801726145193));
#145267=CARTESIAN_POINT('Ctrl Pts',(-0.707067566378144,-17.4928576526749,
-6.20267384590878));
#145268=CARTESIAN_POINT('Ctrl Pts',(-0.693980570416363,-17.4798073798581,
-6.21798592469554));
#145269=CARTESIAN_POINT('Ctrl Pts',(-0.658926778537658,-17.4468062914195,
-6.218153350034));
#145270=CARTESIAN_POINT('Ctrl Pts',(-0.578223751373194,-17.3811061564651,
-6.18014514262514));
#145271=CARTESIAN_POINT('Ctrl Pts',(-0.511817975000622,-17.3393168679221,
-6.12535925716751));
#145272=CARTESIAN_POINT('Ctrl Pts',(-0.465549933916129,-17.3149783849924,
-6.0801726145193));
#145273=CARTESIAN_POINT('Origin',(-0.605214914090966,-17.0494719004901,
-6.0801726145193));
#145274=CARTESIAN_POINT('Ctrl Pts',(0.838117322977332,-17.4519854043201,
-6.13198743401459));
#145275=CARTESIAN_POINT('Ctrl Pts',(0.669902960334304,-17.3101168025864,
-5.92937807322927));
#145276=CARTESIAN_POINT('Ctrl Pts',(0.191478511893925,-17.080317816636,
-5.6011911094929));
#145277=CARTESIAN_POINT('Ctrl Pts',(-0.345547509129884,-17.1586240778992,
-5.71302404043138));
#145278=CARTESIAN_POINT('Ctrl Pts',(-0.605214914090966,-17.2952175137768,
-5.90809968361399));
#145279=CARTESIAN_POINT('Ctrl Pts',(0.764181235176186,-17.4808267723045,
-6.17317717621315));
#145280=CARTESIAN_POINT('Ctrl Pts',(0.613605800021816,-17.3417952320759,
-5.97506916075729));
#145281=CARTESIAN_POINT('Ctrl Pts',(0.176871355450469,-17.1164577820709,
-5.65299097316032));
#145282=CARTESIAN_POINT('Ctrl Pts',(-0.317987318062742,-17.1933294614096,
-5.76290031980275));
#145283=CARTESIAN_POINT('Ctrl Pts',(-0.553859250801039,-17.3273362577698,
-5.95397000382664));
#145284=CARTESIAN_POINT('Ctrl Pts',(0.691003313955543,-17.4746156005897,
-6.23828151084433));
#145285=CARTESIAN_POINT('Ctrl Pts',(0.557421428927607,-17.3481757435076,
-6.03813220065825));
#145286=CARTESIAN_POINT('Ctrl Pts',(0.162193315798326,-17.1406373153018,
-5.71309101023175));
#145287=CARTESIAN_POINT('Ctrl Pts',(-0.29035089633337,-17.2118747949918,
-5.82396153717806));
#145288=CARTESIAN_POINT('Ctrl Pts',(-0.502781108682595,-17.3345631845704,
-6.01690035049276));
#145289=CARTESIAN_POINT('Ctrl Pts',(0.644705633059487,-17.4355690700257,
-6.3040603649199));
#145290=CARTESIAN_POINT('Ctrl Pts',(0.515309969487927,-17.3264393763844,
-6.10145100413458));
#145291=CARTESIAN_POINT('Ctrl Pts',(0.147291162995327,-17.1496709256533,
-5.77326404039821));
#145292=CARTESIAN_POINT('Ctrl Pts',(-0.265805776253758,-17.2099065112404,
-5.88509697133669));
#145293=CARTESIAN_POINT('Ctrl Pts',(-0.465549933916129,-17.3149783849924,
-6.0801726145193));
#145294=CARTESIAN_POINT('Origin',(0.,-18.2,-7.72329702653519));
#145295=CARTESIAN_POINT('Origin',(19.1875302357774,-17.3150528379807,-0.374581597160819));
#145296=CARTESIAN_POINT('Origin',(3.02518007237845E-18,-18.4457456132867,
1.24021503613021));
#145297=CARTESIAN_POINT('Ctrl Pts',(-0.914382087390238,-17.5216755952362,
-0.0794937182387867));
#145298=CARTESIAN_POINT('Ctrl Pts',(-0.683643791787282,-17.293356355078,
-0.405567385971643));
#145299=CARTESIAN_POINT('Ctrl Pts',(-0.125022675737884,-17.054213772593,
-0.747098388474721));
#145300=CARTESIAN_POINT('Ctrl Pts',(0.448115403944561,-17.2013730333212,
-0.536933183592055));
#145301=CARTESIAN_POINT('Ctrl Pts',(0.658073755029969,-17.3246127340343,
-0.360928650667152));
#145302=CARTESIAN_POINT('Ctrl Pts',(-0.832254441336071,-17.5489810332648,
-0.0404975113449715));
#145303=CARTESIAN_POINT('Ctrl Pts',(-0.627393047499884,-17.3253518030282,
-0.359056762504974));
#145304=CARTESIAN_POINT('Ctrl Pts',(-0.115018286391046,-17.0908909725833,
-0.694774811887389));
#145305=CARTESIAN_POINT('Ctrl Pts',(0.41157768336954,-17.235251291275,-0.488248529886861));
#145306=CARTESIAN_POINT('Ctrl Pts',(0.601833509913226,-17.3561346296068,
-0.315910718336575));
#145307=CARTESIAN_POINT('Ctrl Pts',(-0.751191480614262,-17.5364962027232,
0.0256067422309708));
#145308=CARTESIAN_POINT('Ctrl Pts',(-0.570929837813018,-17.3337638916996,
-0.296314833667629));
#145309=CARTESIAN_POINT('Ctrl Pts',(-0.105131601746012,-17.1167802483211,
-0.634963805784064));
#145310=CARTESIAN_POINT('Ctrl Pts',(0.375028796817523,-17.2503715095973,
-0.426620170382907));
#145311=CARTESIAN_POINT('Ctrl Pts',(0.545941211667053,-17.3609108659448,
-0.252580344646373));
#145312=CARTESIAN_POINT('Ctrl Pts',(-0.703370836454029,-17.4891769091919,
0.0925792126665251));
#145313=CARTESIAN_POINT('Ctrl Pts',(-0.525879839836371,-17.3135467244548,
-0.233494455066332));
#145314=CARTESIAN_POINT('Ctrl Pts',(-0.096171289029141,-17.1295908917741,
-0.575025457569408));
#145315=CARTESIAN_POINT('Ctrl Pts',(0.344704156880431,-17.2427903231035,
-0.364860252686742));
#145316=CARTESIAN_POINT('Ctrl Pts',(0.506210580792283,-17.3375900928828,
-0.188855719761839));
#145317=CARTESIAN_POINT('Origin',(13.3623247423326,-19.9,7.82921171985308));
#145318=CARTESIAN_POINT('',(13.7548828365128,-15.9,7.75241235336064));
#145319=CARTESIAN_POINT('Origin',(13.3623247423326,-15.9,7.82921171985308));
#145320=CARTESIAN_POINT('',(13.7548828365128,-19.9,7.75241235336064));
#145321=CARTESIAN_POINT('Origin',(1.19999999921058,-19.9,-1.85000000003699));
#145322=CARTESIAN_POINT('',(1.19999999921058,-19.9,-2.45000000003699));
#145323=CARTESIAN_POINT('Origin',(4.3,-19.9,-1.85000000003699));
#145324=CARTESIAN_POINT('',(4.9,-19.9,-1.85000000003699));
#145325=CARTESIAN_POINT('',(4.3,-19.9,-2.45000000003699));
#145326=CARTESIAN_POINT('Origin',(-5.94265499251984,-19.9,-2.45000000003699));
#145327=CARTESIAN_POINT('Origin',(-10.2709990938499,-21.1,0.945217224235999));
#145328=CARTESIAN_POINT('Origin',(-10.2709990938499,-20.,0.945217224235999));
#145329=CARTESIAN_POINT('Origin',(-15.3000000000043,-22.8,6.20189169841846));
#145330=CARTESIAN_POINT('',(-14.9000000000043,-15.9,6.20189169841771));
#145331=CARTESIAN_POINT('',(-14.9000000000043,-22.8,6.20189169841771));
#145332=CARTESIAN_POINT('',(-15.0836363636405,-15.9,5.86545927302008));
#145333=CARTESIAN_POINT('Origin',(-15.3000000000043,-15.9,6.20189169841846));
#145334=CARTESIAN_POINT('',(-15.0836363636405,-22.8,5.86545927302008));
#145335=CARTESIAN_POINT('Origin',(-9.35,-22.8,-3.05000000003699));
#145336=CARTESIAN_POINT('',(-15.8545454545506,-15.9,5.31964087814201));
#145337=CARTESIAN_POINT('',(-15.8545454545506,-22.8,5.31964087814201));
#145338=CARTESIAN_POINT('Origin',(-9.35,-15.9,-3.05000000003699));
#145339=CARTESIAN_POINT('Origin',(-16.1000000000054,-22.8,5.63547638297895));
#145340=CARTESIAN_POINT('Origin',(-16.1000000000054,-15.9,5.63547638297895));
#145341=CARTESIAN_POINT('Origin',(-3.1143484430694,-15.9,-8.60653400714346));
#145342=CARTESIAN_POINT('Origin',(-16.1000000000089,-15.9,3.77623615174389));
#145343=CARTESIAN_POINT('',(-14.9000000000142,-15.9,0.96536214654126));
#145344=CARTESIAN_POINT('Origin',(6.09999999999969,-15.9,9.2499999999633));
#145345=CARTESIAN_POINT('Origin',(-16.1000000000089,-19.9,3.77623615174389));
#145346=CARTESIAN_POINT('Origin',(-16.1000000000089,-20.,3.77623615174389));
#145347=CARTESIAN_POINT('Origin',(-5.42954084321747,-21.1,-1.85000000003699));
#145348=CARTESIAN_POINT('Origin',(0.0158955791744741,-19.9,-3.65000000003699));
#145349=CARTESIAN_POINT('',(-1.20000000078942,-19.9,-3.65000000003699));
#145350=CARTESIAN_POINT('Origin',(-1.20000000078942,-19.9,-4.25000000003699));
#145351=CARTESIAN_POINT('',(-0.600000000789417,-19.9,-4.25000000003699));
#145352=CARTESIAN_POINT('Origin',(-0.600000000789418,-19.9,0.384748901093117));
#145353=CARTESIAN_POINT('',(-0.600000000789417,-19.9,-5.79545078503888));
#145354=CARTESIAN_POINT('Origin',(-1.20000000078942,-19.9,-5.79545078503888));
#145355=CARTESIAN_POINT('Origin',(6.1,-21.,-12.1857384988752));
#145356=CARTESIAN_POINT('Origin',(8.6,-19.9,-0.741996797474057));
#145357=CARTESIAN_POINT('',(4.9,-19.9,-0.741996797474059));
#145358=CARTESIAN_POINT('Origin',(4.9,-19.9,-5.32716721908225));
#145359=CARTESIAN_POINT('Origin',(6.09999999999969,-19.9,9.2499999999633));
#145360=CARTESIAN_POINT('',(13.8999999999997,-19.9,9.24999999996345));
#145361=CARTESIAN_POINT('Origin',(13.8999999999998,-19.9,1.44999999996345));
#145362=CARTESIAN_POINT('',(13.8999999999998,-25.4,0.499999999970565));
#145363=CARTESIAN_POINT('Origin',(-14.8999999999961,-22.8,10.5372583002038));
#145364=CARTESIAN_POINT('',(-14.8999999999968,-22.8,10.2058874503056));
#145365=CARTESIAN_POINT('Origin',(-14.0999999999968,-22.8,10.2058874503041));
#145366=CARTESIAN_POINT('Origin',(7.94152002157416E-16,-18.2,15.6578006787879));
#145367=CARTESIAN_POINT('Origin',(2.10864821770493E-16,-18.2,10.175));
#145368=CARTESIAN_POINT('Origin',(3.04851216033843,-24.4,10.2415765003998));
#145369=CARTESIAN_POINT('Origin',(2.3,-22.8,6.19999999999999));
#145370=CARTESIAN_POINT('Origin',(16.5000000000094,-24.4,1.94999999997594));
#145371=CARTESIAN_POINT('',(16.7343145750595,-25.4,2.18431457502608));
#145372=CARTESIAN_POINT('',(11.7750000000018,-25.4,-2.77500000003169));
#145373=CARTESIAN_POINT('',(16.7343145750595,-23.,2.18431457502608));
#145374=CARTESIAN_POINT('',(16.7343145750595,-24.4,2.18431457502608));
#145375=CARTESIAN_POINT('',(16.7650854557587,-23.,2.2150854557252));
#145376=CARTESIAN_POINT('Origin',(17.3000000000088,-24.4,1.61862915007684));
#145377=CARTESIAN_POINT('',(16.5000000000088,-25.4,1.61862915007834));
#145378=CARTESIAN_POINT('Origin',(17.3000000000088,-25.4,1.61862915007684));
#145379=CARTESIAN_POINT('',(16.5000000000088,-23.,1.61862915007834));
#145380=CARTESIAN_POINT('',(16.5000000000088,-24.,1.61862915007834));
#145381=CARTESIAN_POINT('Origin',(17.3000000000088,-23.,1.61862915007684));
#145382=CARTESIAN_POINT('Origin',(16.4999999999906,-24.4,-8.05000000002406));
#145383=CARTESIAN_POINT('',(16.4999999999977,-25.4,-4.25000000003885));
#145384=CARTESIAN_POINT('',(16.5000000000088,-23.,1.61862915007834));
#145385=CARTESIAN_POINT('Origin',(9.25,-23.,-3.05000000003699));
#145386=CARTESIAN_POINT('Origin',(15.8325427278768,-23.,-1.75748667391245));
#145387=CARTESIAN_POINT('Origin',(0.,-18.2,-19.1));
#145388=CARTESIAN_POINT('',(-1.,-18.2,-19.1));
#145389=CARTESIAN_POINT('Origin',(-2.25752749827279E-11,-25.4,-0.450000000022578));
#145390=CARTESIAN_POINT('Origin',(-17.3000000000305,-25.4,-7.71862915012444));
#145391=CARTESIAN_POINT('Origin',(-17.3000000000305,-24.4,-7.71862915012444));
#145392=CARTESIAN_POINT('Origin',(-17.3000000000305,-20.,-7.71862915012444));
#145393=CARTESIAN_POINT('Origin',(-16.0596875762449,-20.,-5.65000000005141));
#145394=CARTESIAN_POINT('Origin',(-14.5525630318579,-19.9,-10.8611035007945));
#145395=CARTESIAN_POINT('',(-13.6127165965579,-20.,-9.23324172354236));
#145396=CARTESIAN_POINT('Origin',(-16.0596875762449,-20.,-5.65000000005141));
#145397=CARTESIAN_POINT('Origin',(-3.1143484430694,-15.9,-8.60653400714346));
#145398=CARTESIAN_POINT('',(0.,0.,0.));
#145399=CARTESIAN_POINT('Origin',(3.99999981302311,0.199999999999988,2.50184806546842));
#145400=CARTESIAN_POINT('',(3.99999981302311,11.9,2.50184806546842));
#145401=CARTESIAN_POINT('',(-0.600000000002621,11.9,7.10184787849414));
#145402=CARTESIAN_POINT('',(-0.849538123856316,11.9,7.35138600234784));
#145403=CARTESIAN_POINT('',(3.99999981302311,14.4,2.50184806546842));
#145404=CARTESIAN_POINT('',(3.99999957308175,7.29999999999999,2.50184830540978));
#145405=CARTESIAN_POINT('',(-0.600000000002621,14.4,7.10184787849414));
#145406=CARTESIAN_POINT('',(-1.18078817722572,14.4,7.68263605571724));
#145407=CARTESIAN_POINT('',(-0.600000000002621,0.199999999999988,7.10184787849414));
#145408=CARTESIAN_POINT('Origin',(3.99999981302311,0.199999999999988,2.50184806546842));
#145409=CARTESIAN_POINT('',(-0.600000000002621,2.1,7.10184787849414));
#145410=CARTESIAN_POINT('',(3.99999981302311,2.1,2.50184806546842));
#145411=CARTESIAN_POINT('',(-0.849538123856316,2.1,7.35138600234784));
#145412=CARTESIAN_POINT('',(-0.600000000002621,0.199999999999988,7.10184787849414));
#145413=CARTESIAN_POINT('',(-0.600000000002621,0.199999999999988,7.10184787849414));
#145414=CARTESIAN_POINT('',(3.99999981302311,0.199999999999988,2.50184806546842));
#145415=CARTESIAN_POINT('',(-1.18078817722572,0.199999999999988,7.68263605571724));
#145416=CARTESIAN_POINT('',(3.99999957308175,7.29999999999999,2.50184830540978));
#145417=CARTESIAN_POINT('Origin',(-2.20000021345912,14.4,17.0249999999815));
#145418=CARTESIAN_POINT('',(-0.599999999994357,14.4,15.0499999999722));
#145419=CARTESIAN_POINT('',(-0.600000000010333,14.4,12.0634239392391));
#145420=CARTESIAN_POINT('',(3.99999957308175,14.4,0.00184806546839056));
#145421=CARTESIAN_POINT('',(3.99999957308175,14.4,-4.44089209850063E-15));
#145422=CARTESIAN_POINT('',(-3.99999999999999,14.4,-4.44089209850063E-15));
#145423=CARTESIAN_POINT('Origin',(1.33226762955019E-14,14.4,-4.44089209850063E-15));
#145424=CARTESIAN_POINT('',(-3.99999999999999,14.4,3.08613054156667));
#145425=CARTESIAN_POINT('',(-3.99999999999999,14.4,-4.44089209850063E-15));
#145426=CARTESIAN_POINT('',(-6.0957241205081,14.4,7.15616513795545));
#145427=CARTESIAN_POINT('Origin',(-8.99999999999999,14.4,3.08613054156667));
#145428=CARTESIAN_POINT('',(-5.25380888164337,14.4,16.9135949821128));
#145429=CARTESIAN_POINT('Origin',(-5.84999999999999,14.4,12.049999999963));
#145430=CARTESIAN_POINT('',(-0.899999999999987,14.4,24.0343597112987));
#145431=CARTESIAN_POINT('Origin',(-8.89999999999999,14.4,24.0343597112987));
#145432=CARTESIAN_POINT('',(-0.899999999999987,14.4,32.4000004268813));
#145433=CARTESIAN_POINT('',(-0.899999999999987,14.4,16.049999999963));
#145434=CARTESIAN_POINT('',(-4.26918251861252E-7,14.4,33.299999999963));
#145435=CARTESIAN_POINT('',(-4.61875037354885,14.4,28.6812500533325));
#145436=CARTESIAN_POINT('',(-4.26918254081698E-7,14.4,36.3857864375899));
#145437=CARTESIAN_POINT('',(-4.2691824742036E-7,14.4,27.6624999999723));
#145438=CARTESIAN_POINT('',(0.292892791895201,14.4,37.0928932187765));
#145439=CARTESIAN_POINT('Origin',(0.999999573081747,14.4,36.3857864375899));
#145440=CARTESIAN_POINT('',(1.20710635426829,14.4,38.0071067811496));
#145441=CARTESIAN_POINT('',(-5.11875037354885,14.4,31.6812500533324));
#145442=CARTESIAN_POINT('',(1.91421313545483,14.4,38.299999999963));
#145443=CARTESIAN_POINT('Origin',(1.91421313545483,14.4,37.299999999963));
#145444=CARTESIAN_POINT('',(3.99999957308175,14.4,38.299999999963));
#145445=CARTESIAN_POINT('',(0.899999679811312,14.4,38.299999999963));
#145446=CARTESIAN_POINT('',(4.,14.4,19.6499999999665));
#145447=CARTESIAN_POINT('',(3.99999957308175,14.4,-4.44089209850063E-15));
#145448=CARTESIAN_POINT('',(0.493749946643665,14.4,16.1437499466102));
#145449=CARTESIAN_POINT('Origin',(-5.84999999999999,2.1,12.049999999963));
#145450=CARTESIAN_POINT('',(-0.599999999994357,2.09999999999999,15.0499999999722));
#145451=CARTESIAN_POINT('',(-0.600000000006467,2.1,9.57592393923266));
#145452=CARTESIAN_POINT('',(1.75042009953066,2.1,3.59666921959181));
#145453=CARTESIAN_POINT('',(-2.98516557716169,2.1,5.90137500303677));
#145454=CARTESIAN_POINT('',(0.461099356094962,2.09999999999999,3.97333454214578));
#145455=CARTESIAN_POINT('Origin',(1.33226762955019E-14,2.09999999999999,
-2.49800183849383E-15));
#145456=CARTESIAN_POINT('',(-3.40729205497977,2.09999999999999,2.09531879485477));
#145457=CARTESIAN_POINT('Origin',(-5.84999999999999,2.1,12.049999999963));
#145458=CARTESIAN_POINT('',(-3.99999999999999,2.09999999999999,-1.99840144432528E-13));
#145459=CARTESIAN_POINT('Origin',(1.33226762955019E-14,2.09999999999999,
-2.49800183849383E-15));
#145460=CARTESIAN_POINT('',(-3.99999999999999,2.1,3.08613054156667));
#145461=CARTESIAN_POINT('',(-3.99999999999999,2.09999999999999,9.87500000569498));
#145462=CARTESIAN_POINT('',(-6.74999999999999,2.1,7.5512733164396));
#145463=CARTESIAN_POINT('Origin',(-8.99999999999999,2.1,3.08613054156667));
#145464=CARTESIAN_POINT('',(-7.66385919120079,2.1,8.26187185607765));
#145465=CARTESIAN_POINT('Origin',(-5.39999999999999,2.1,10.2303589813634));
#145466=CARTESIAN_POINT('',(-7.1474157554001,2.1,16.0445853799042));
#145467=CARTESIAN_POINT('Origin',(-5.84999999999999,2.1,12.049999999963));
#145468=CARTESIAN_POINT('',(-6.35454545454544,2.1,16.4501220332571));
#145469=CARTESIAN_POINT('Origin',(-5.39999999999999,2.1,13.6060329039916));
#145470=CARTESIAN_POINT('',(-0.899999999999982,2.09999999999999,24.0343597112987));
#145471=CARTESIAN_POINT('Origin',(-8.89999999999999,2.09999999999999,24.0343597112987));
#145472=CARTESIAN_POINT('',(-0.899999999999987,2.09999999999999,25.399999999963));
#145473=CARTESIAN_POINT('',(-0.899999999999987,2.09999999999999,25.049999999963));
#145474=CARTESIAN_POINT('',(1.10000000000001,2.09999999999999,23.399999999963));
#145475=CARTESIAN_POINT('',(1.70000000000002,2.09999999999999,22.799999999963));
#145476=CARTESIAN_POINT('',(4.,2.09999999999999,23.399999999963));
#145477=CARTESIAN_POINT('',(3.,2.09999999999999,23.399999999963));
#145478=CARTESIAN_POINT('',(4.,2.09999999999999,19.6499999999665));
#145479=CARTESIAN_POINT('',(3.99999957308175,2.09999999999999,10.4499999999815));
#145480=CARTESIAN_POINT('',(3.38750000000382,2.09999999999999,19.0374999999704));
#145481=CARTESIAN_POINT('Origin',(1.75042009953066,0.199999999999991,3.59666921959181));
#145482=CARTESIAN_POINT('',(3.99999957308175,8.24999999999999,2.50184818224262));
#145483=CARTESIAN_POINT('',(1.75042009953066,11.9,3.59666921959181));
#145484=CARTESIAN_POINT('',(3.92607865052219,11.9,2.53782387550884));
#145485=CARTESIAN_POINT('',(1.75042009953066,11.9,3.59666921959181));
#145486=CARTESIAN_POINT('Origin',(-5.84999999999999,11.9,12.049999999963));
#145487=CARTESIAN_POINT('',(-0.599999999994357,11.9,15.0499999999722));
#145488=CARTESIAN_POINT('',(-0.600000000006467,11.9,9.57592393923266));
#145489=CARTESIAN_POINT('',(4.,11.9,19.6499999999665));
#145490=CARTESIAN_POINT('',(2.2000000000047,11.9,17.8499999999712));
#145491=CARTESIAN_POINT('',(4.,11.9,23.399999999963));
#145492=CARTESIAN_POINT('',(3.99999957308175,11.9,8.07499999998326));
#145493=CARTESIAN_POINT('',(1.10000000000001,11.9,23.399999999963));
#145494=CARTESIAN_POINT('',(1.99999957308175,11.9,23.399999999963));
#145495=CARTESIAN_POINT('',(-0.899999999999987,11.9,25.399999999963));
#145496=CARTESIAN_POINT('',(1.70000000000002,11.9,22.799999999963));
#145497=CARTESIAN_POINT('',(-0.899999999999982,11.9,24.0343597112987));
#145498=CARTESIAN_POINT('',(-0.899999999999987,11.9,25.049999999963));
#145499=CARTESIAN_POINT('',(-6.35454545454544,11.9,16.4501220332571));
#145500=CARTESIAN_POINT('Origin',(-8.89999999999999,11.9,24.0343597112987));
#145501=CARTESIAN_POINT('',(-7.1474157554001,11.9,16.0445853799042));
#145502=CARTESIAN_POINT('Origin',(-5.39999999999999,11.9,13.6060329039916));
#145503=CARTESIAN_POINT('',(-7.66385919120079,11.9,8.26187185607765));
#145504=CARTESIAN_POINT('Origin',(-5.84999999999999,11.9,12.049999999963));
#145505=CARTESIAN_POINT('',(-6.74999999999999,11.9,7.55127331643961));
#145506=CARTESIAN_POINT('Origin',(-5.39999999999999,11.9,10.2303589813634));
#145507=CARTESIAN_POINT('',(-3.99999999999999,11.9,3.08613054156667));
#145508=CARTESIAN_POINT('Origin',(-8.99999999999999,11.9,3.08613054156667));
#145509=CARTESIAN_POINT('',(-3.99999999999999,11.9,-2.00427047043497E-13));
#145510=CARTESIAN_POINT('',(-3.99999999999999,11.9,9.87500000569498));
#145511=CARTESIAN_POINT('',(-3.40729205497977,11.9,2.09531879485477));
#145512=CARTESIAN_POINT('Origin',(1.33226762955019E-14,11.9,-2.49800183849383E-15));
#145513=CARTESIAN_POINT('',(0.461099356094962,11.9,3.97333454214578));
#145514=CARTESIAN_POINT('Origin',(-5.84999999999999,11.9,12.049999999963));
#145515=CARTESIAN_POINT('Origin',(1.33226762955019E-14,11.9,-2.49800183849383E-15));
#145516=CARTESIAN_POINT('Origin',(0.100000000000013,13.15,24.399999999963));
#145517=CARTESIAN_POINT('',(1.10000000000001,13.15,23.399999999963));
#145518=CARTESIAN_POINT('',(-0.899999999999987,13.15,25.399999999963));
#145519=CARTESIAN_POINT('Origin',(-0.899999999999987,14.4,38.049999999963));
#145520=CARTESIAN_POINT('',(-0.899999999999987,0.199999999999987,24.0343597112987));
#145521=CARTESIAN_POINT('',(-0.899999999999987,14.4,24.0343597112987));
#145522=CARTESIAN_POINT('',(-0.899999999999987,0.199999999999982,32.4000004268813));
#145523=CARTESIAN_POINT('',(-0.899999999999987,0.199999999999982,27.5374999999723));
#145524=CARTESIAN_POINT('',(-0.899999999999987,6.72554492441848,32.4000004268813));
#145525=CARTESIAN_POINT('',(-0.899999999999987,7.29999999999999,32.4000004268813));
#145526=CARTESIAN_POINT('',(-0.900000426918255,5.59999999999999,30.799999999963));
#145527=CARTESIAN_POINT('Origin',(-0.899999999999987,7.29999999999998,30.799999999963));
#145528=CARTESIAN_POINT('',(-0.900000426918255,5.59999999999999,27.799999999963));
#145529=CARTESIAN_POINT('',(-0.899999999999987,5.59999999999999,32.924999999963));
#145530=CARTESIAN_POINT('',(-0.900000426918255,8.99999999999999,27.799999999963));
#145531=CARTESIAN_POINT('Origin',(-0.899999999999987,7.29999999999999,27.799999999963));
#145532=CARTESIAN_POINT('',(-0.900000426918255,8.99999999999998,30.799999999963));
#145533=CARTESIAN_POINT('',(-0.899999999999987,8.99999999999998,34.424999999963));
#145534=CARTESIAN_POINT('',(-0.899999999999987,7.87445507558149,32.4000004268813));
#145535=CARTESIAN_POINT('Origin',(-0.899999999999987,7.29999999999998,30.799999999963));
#145536=CARTESIAN_POINT('',(-0.899999999999987,7.29999999999999,32.4000004268813));
#145537=CARTESIAN_POINT('',(-0.899999999999987,14.4,24.0343597112987));
#145538=CARTESIAN_POINT('Origin',(3.99999957308175,14.4,-2.5));
#145539=CARTESIAN_POINT('',(3.99999957308175,13.15,23.399999999963));
#145540=CARTESIAN_POINT('',(3.99999957308175,6.09999999999999,19.6499995730483));
#145541=CARTESIAN_POINT('',(3.99999957308175,0.199999999999987,38.299999999963));
#145542=CARTESIAN_POINT('',(3.99999957308175,14.4,38.299999999963));
#145543=CARTESIAN_POINT('',(4.,0.199999999999987,19.6499999999665));
#145544=CARTESIAN_POINT('',(3.99999957308175,0.199999999999987,7.26249999999075));
#145545=CARTESIAN_POINT('',(3.99999957308175,6.09999999999999,19.6499995730483));
#145546=CARTESIAN_POINT('',(3.99999957308175,10.7,30.799999999963));
#145547=CARTESIAN_POINT('',(3.99999957308175,3.89999999999998,30.799999999963));
#145548=CARTESIAN_POINT('Origin',(3.99999957308175,7.29999999999998,30.799999999963));
#145549=CARTESIAN_POINT('',(3.99999957308175,10.7,27.799999999963));
#145550=CARTESIAN_POINT('',(3.99999957308175,10.7,14.1499999999815));
#145551=CARTESIAN_POINT('',(3.99999957308175,3.89999999999999,27.799999999963));
#145552=CARTESIAN_POINT('Origin',(3.99999957308175,7.29999999999999,27.799999999963));
#145553=CARTESIAN_POINT('',(3.99999957308175,3.89999999999999,12.6499999999815));
#145554=CARTESIAN_POINT('Origin',(1.40000000000941,-2.2,17.0499999999759));
#145555=CARTESIAN_POINT('',(-0.599999999994357,-2.2,15.0499999999722));
#145556=CARTESIAN_POINT('Origin',(1.99999957308175,11.9,23.399999999963));
#145557=CARTESIAN_POINT('Origin',(-8.89999999999999,14.4,24.0343597112987));
#145558=CARTESIAN_POINT('',(-6.35454545129335,14.8710452666677,16.4501220343486));
#145559=CARTESIAN_POINT('Ctrl Pts',(-5.25380888164336,14.4,16.9135949821128));
#145560=CARTESIAN_POINT('Ctrl Pts',(-5.33338146986815,14.4501241917611,
16.8728497987675));
#145561=CARTESIAN_POINT('Ctrl Pts',(-5.41464812969736,14.4979663578989,
16.8329226337617));
#145562=CARTESIAN_POINT('Ctrl Pts',(-5.76835566322084,14.6899428683665,
16.6667013086606));
#145563=CARTESIAN_POINT('Ctrl Pts',(-6.05674662065273,14.8056725793831,
16.5500705618533));
#145564=CARTESIAN_POINT('Ctrl Pts',(-6.35454545128526,14.8710452666659,
16.4501220343513));
#145565=CARTESIAN_POINT('',(-6.35454545454544,14.4,16.4501220332571));
#145566=CARTESIAN_POINT('Origin',(1.33226762955019E-14,11.9,-2.49800183849383E-15));
#145567=CARTESIAN_POINT('',(0.461099356094962,11.9,3.97333454214578));
#145568=CARTESIAN_POINT('Origin',(-3.99999999999999,14.4,8.04999999996301));
#145569=CARTESIAN_POINT('',(-3.99999999999999,14.4,3.08613054156667));
#145570=CARTESIAN_POINT('',(-3.99999999999999,14.4,-4.44089209850063E-15));
#145571=CARTESIAN_POINT('Origin',(-5.84999999999999,11.6,12.049999999963));
#145572=CARTESIAN_POINT('',(-3.40729205497977,11.9,2.09531879485477));
#145573=CARTESIAN_POINT('Origin',(1.40000000000941,-2.2,17.0499999999759));
#145574=CARTESIAN_POINT('',(-0.599999999994357,0.199999999999987,15.0499999999722));
#145575=CARTESIAN_POINT('',(0.493749946643668,0.199999999999987,16.1437499466102));
#145576=CARTESIAN_POINT('',(-0.599999999994357,-2.2,15.0499999999722));
#145577=CARTESIAN_POINT('Origin',(-0.600000000009414,-2.19999999999999,
7.0499999999797));
#145578=CARTESIAN_POINT('',(-0.600000000010333,0.199999999999987,12.0634239392391));
#145579=CARTESIAN_POINT('Origin',(-0.600000000009414,-2.19999999999999,
7.0499999999797));
#145580=CARTESIAN_POINT('Origin',(3.99999957308175,14.4,-2.5));
#145581=CARTESIAN_POINT('',(3.99999957308175,0.199999999999991,0.00184806546839056));
#145582=CARTESIAN_POINT('',(3.99999957308175,0.199999999999987,7.26249999999075));
#145583=CARTESIAN_POINT('',(4.00000000000001,0.199999999999991,-4.44089209850063E-15));
#145584=CARTESIAN_POINT('',(3.99999957308175,0.199999999999987,7.26249999999075));
#145585=CARTESIAN_POINT('',(3.99999957308175,0.199999999999991,-2.5));
#145586=CARTESIAN_POINT('',(3.99999957308175,0.199999999999987,7.26249999999075));
#145587=CARTESIAN_POINT('',(3.99999957308175,14.4,-2.5));
#145588=CARTESIAN_POINT('',(3.99999957308175,14.4,-2.5));
#145589=CARTESIAN_POINT('',(4.00000000000001,14.4,-4.44089209850063E-15));
#145590=CARTESIAN_POINT('',(3.99999957308175,14.4,-4.44089209850063E-15));
#145591=CARTESIAN_POINT('Origin',(1.33226762955019E-14,14.4,-4.44089209850063E-15));
#145592=CARTESIAN_POINT('Origin',(0.999999573081747,3.74999999999998,36.3857864375899));
#145593=CARTESIAN_POINT('',(-4.26918254081698E-7,0.199999999999987,36.3857864375899));
#145594=CARTESIAN_POINT('',(0.292892791895201,0.199999999999987,37.0928932187765));
#145595=CARTESIAN_POINT('Origin',(0.999999573081747,0.199999999999987,36.3857864375899));
#145596=CARTESIAN_POINT('',(0.292892791895198,3.74999999999998,37.0928932187765));
#145597=CARTESIAN_POINT('',(-4.26918254081698E-7,3.74999999999998,36.3857864375899));
#145598=CARTESIAN_POINT('Origin',(0.749999573081743,7.29999999999999,37.549999999963));
#145599=CARTESIAN_POINT('',(1.20710635426829,0.199999999999987,38.0071067811496));
#145600=CARTESIAN_POINT('',(-5.11875037354885,0.199999999999982,31.6812500533324));
#145601=CARTESIAN_POINT('',(1.20710635426828,10.85,38.0071067811496));
#145602=CARTESIAN_POINT('Origin',(-2.20000021345912,0.199999999999987,17.0249999999815));
#145603=CARTESIAN_POINT('',(1.91421313545483,0.199999999999987,38.299999999963));
#145604=CARTESIAN_POINT('',(0.899999679811312,0.199999999999987,38.299999999963));
#145605=CARTESIAN_POINT('Origin',(1.91421313545483,0.199999999999987,37.299999999963));
#145606=CARTESIAN_POINT('',(-4.26918251861252E-7,0.199999999999987,33.299999999963));
#145607=CARTESIAN_POINT('',(-4.2691824742036E-7,0.199999999999982,27.6624999999723));
#145608=CARTESIAN_POINT('',(-4.61875037354885,0.199999999999982,28.6812500533325));
#145609=CARTESIAN_POINT('',(-5.25380888164337,0.199999999999987,16.9135949821128));
#145610=CARTESIAN_POINT('Origin',(-8.89999999999999,0.199999999999987,24.0343597112987));
#145611=CARTESIAN_POINT('',(-6.0957241205081,0.199999999999987,7.15616513795545));
#145612=CARTESIAN_POINT('Origin',(-5.84999999999999,0.199999999999987,12.049999999963));
#145613=CARTESIAN_POINT('',(-3.99999999999999,0.199999999999991,3.08613054156667));
#145614=CARTESIAN_POINT('Origin',(-8.99999999999999,0.199999999999991,3.08613054156667));
#145615=CARTESIAN_POINT('',(-3.99999999999999,0.199999999999991,-4.44089209850063E-15));
#145616=CARTESIAN_POINT('',(-3.99999999999999,0.199999999999987,12.5374999999723));
#145617=CARTESIAN_POINT('Origin',(1.33226762955019E-14,0.199999999999991,
-4.44089209850063E-15));
#145618=CARTESIAN_POINT('Origin',(1.91421313545483,10.85,37.299999999963));
#145619=CARTESIAN_POINT('',(1.91421313545483,10.85,38.299999999963));
#145620=CARTESIAN_POINT('Origin',(-4.26918256302145E-7,0.199999999999987,
38.299999999963));
#145621=CARTESIAN_POINT('',(-4.26918251861252E-7,0.199999999999987,33.299999999963));
#145622=CARTESIAN_POINT('Origin',(-4.26918251861252E-7,0.199999999999987,
33.299999999963));
#145623=CARTESIAN_POINT('Origin',(-2.50000042691827,7.29999999999998,30.799999999963));
#145624=CARTESIAN_POINT('Origin',(3.99999957308175,7.29999999999998,30.799999999963));
#145625=CARTESIAN_POINT('',(1.99999957308175,8.99999999999998,30.799999999963));
#145626=CARTESIAN_POINT('',(3.99999957308175,8.99999999999998,30.799999999963));
#145627=CARTESIAN_POINT('',(1.99999957308175,5.59999999999999,30.799999999963));
#145628=CARTESIAN_POINT('Origin',(1.99999957308175,7.29999999999998,30.799999999963));
#145629=CARTESIAN_POINT('',(3.99999957308175,5.59999999999999,30.799999999963));
#145630=CARTESIAN_POINT('Origin',(3.89999957308174,7.29999999999998,30.799999999963));
#145631=CARTESIAN_POINT('',(3.79999957308174,10.5,30.799999999963));
#145632=CARTESIAN_POINT('',(3.79999957308174,10.5,30.799999999963));
#145633=CARTESIAN_POINT('',(3.79999957308174,4.09999999999998,30.799999999963));
#145634=CARTESIAN_POINT('',(3.99999957308175,3.89999999999998,30.799999999963));
#145635=CARTESIAN_POINT('Origin',(3.79999957308174,7.29999999999998,30.799999999963));
#145636=CARTESIAN_POINT('Origin',(3.89999957308174,10.6,14.1499999999815));
#145637=CARTESIAN_POINT('',(3.79999957308174,10.5,27.799999999963));
#145638=CARTESIAN_POINT('',(3.79999957308174,10.5,27.799999999963));
#145639=CARTESIAN_POINT('',(3.79999957308174,10.5,14.1499999999815));
#145640=CARTESIAN_POINT('Origin',(3.89999957308174,7.29999999999999,27.799999999963));
#145641=CARTESIAN_POINT('',(3.79999957308174,4.09999999999999,27.799999999963));
#145642=CARTESIAN_POINT('',(3.79999957308174,4.09999999999999,27.799999999963));
#145643=CARTESIAN_POINT('Origin',(3.79999957308174,7.29999999999999,27.799999999963));
#145644=CARTESIAN_POINT('Origin',(3.89999957308174,3.99999999999999,12.6499999999815));
#145645=CARTESIAN_POINT('',(3.79999957308174,4.09999999999999,12.6499999999815));
#145646=CARTESIAN_POINT('Origin',(3.99999957308175,10.5,30.799999999963));
#145647=CARTESIAN_POINT('',(1.99999957308175,10.5,30.799999999963));
#145648=CARTESIAN_POINT('',(3.99999957308175,10.5,30.799999999963));
#145649=CARTESIAN_POINT('',(1.99999957308175,10.5,27.799999999963));
#145650=CARTESIAN_POINT('',(1.99999957308175,10.5,27.799999999963));
#145651=CARTESIAN_POINT('',(3.99999957308175,10.5,27.799999999963));
#145652=CARTESIAN_POINT('Origin',(3.99999957308175,7.29999999999998,30.799999999963));
#145653=CARTESIAN_POINT('',(1.99999957308175,4.09999999999998,30.799999999963));
#145654=CARTESIAN_POINT('',(3.99999957308175,4.09999999999998,30.799999999963));
#145655=CARTESIAN_POINT('Origin',(1.99999957308175,7.29999999999998,30.799999999963));
#145656=CARTESIAN_POINT('Origin',(3.99999957308175,4.09999999999999,27.799999999963));
#145657=CARTESIAN_POINT('',(1.99999957308175,4.09999999999999,27.799999999963));
#145658=CARTESIAN_POINT('',(3.99999957308175,4.09999999999999,27.799999999963));
#145659=CARTESIAN_POINT('',(1.99999957308175,4.09999999999998,30.799999999963));
#145660=CARTESIAN_POINT('Origin',(3.99999957308175,7.29999999999999,27.799999999963));
#145661=CARTESIAN_POINT('Origin',(1.99999957308175,7.29999999999999,27.799999999963));
#145662=CARTESIAN_POINT('Origin',(1.99999957308175,7.29999999999999,29.299999999963));
#145663=CARTESIAN_POINT('',(1.99999957308175,8.99999999999999,27.799999999963));
#145664=CARTESIAN_POINT('',(1.99999957308174,8.99999999999999,30.049999999963));
#145665=CARTESIAN_POINT('',(1.99999957308175,5.59999999999999,27.799999999963));
#145666=CARTESIAN_POINT('Origin',(1.99999957308175,7.29999999999999,27.799999999963));
#145667=CARTESIAN_POINT('',(1.99999957308174,5.59999999999999,28.549999999963));
#145668=CARTESIAN_POINT('Origin',(3.99999957308175,8.99999999999998,30.799999999963));
#145669=CARTESIAN_POINT('',(3.99999957308175,8.99999999999999,27.799999999963));
#145670=CARTESIAN_POINT('Origin',(3.99999957308175,5.59999999999999,27.799999999963));
#145671=CARTESIAN_POINT('',(3.99999957308175,5.59999999999999,27.799999999963));
#145672=CARTESIAN_POINT('Origin',(3.99999957308175,7.29999999999999,27.799999999963));
#145673=CARTESIAN_POINT('Origin',(-5.84999999999999,14.85,12.049999999963));
#145674=CARTESIAN_POINT('',(-6.74999999999999,14.7121310205014,7.55127331643961));
#145675=CARTESIAN_POINT('Ctrl Pts',(-6.74999999999999,14.7121310205014,
7.5512733164396));
#145676=CARTESIAN_POINT('Ctrl Pts',(-6.59752601769717,14.6667024782955,
7.47444117971334));
#145677=CARTESIAN_POINT('Ctrl Pts',(-6.45066441870419,14.6042854333858,
7.39054870820519));
#145678=CARTESIAN_POINT('Ctrl Pts',(-6.23747959335272,14.4896253048058,
7.25461326047292));
#145679=CARTESIAN_POINT('Ctrl Pts',(-6.16538230807449,14.4461506137646,
7.20587149527676));
#145680=CARTESIAN_POINT('Ctrl Pts',(-6.0957241205081,14.4,7.15616513795545));
#145681=CARTESIAN_POINT('',(-7.94554708839804,15.3,8.64284834494288));
#145682=CARTESIAN_POINT('Ctrl Pts',(-6.74999999999999,14.7121310205014,
7.55127331643961));
#145683=CARTESIAN_POINT('Ctrl Pts',(-7.00710332219316,14.788733132856,7.68082851861365));
#145684=CARTESIAN_POINT('Ctrl Pts',(-7.24069578776386,14.8797238094481,
7.84718696018165));
#145685=CARTESIAN_POINT('Ctrl Pts',(-7.62292890725893,15.0675098561581,
8.1991278933308));
#145686=CARTESIAN_POINT('Ctrl Pts',(-7.80142030539744,15.1786537405669,
8.4117434285975));
#145687=CARTESIAN_POINT('Ctrl Pts',(-7.94554708839804,15.3,8.64284834494288));
#145688=CARTESIAN_POINT('',(-7.59791508502123,15.3,15.6478872766235));
#145689=CARTESIAN_POINT('Origin',(-5.84999999999999,15.3,12.049999999963));
#145690=CARTESIAN_POINT('Ctrl Pts',(-7.59791508502124,15.3,15.6478872766235));
#145691=CARTESIAN_POINT('Ctrl Pts',(-7.52392855362119,15.2606953607031,
15.7275286632141));
#145692=CARTESIAN_POINT('Ctrl Pts',(-7.4466010458344,15.2236063588331,15.8020015711092));
#145693=CARTESIAN_POINT('Ctrl Pts',(-7.17008331211839,15.1023689555337,
16.0423295793347));
#145694=CARTESIAN_POINT('Ctrl Pts',(-6.92898212028428,15.0179793780072,
16.2033520572508));
#145695=CARTESIAN_POINT('Ctrl Pts',(-6.56497369958393,14.9197507369652,
16.372867478824));
#145696=CARTESIAN_POINT('Ctrl Pts',(-6.4603790510634,14.8942778184954,16.4146017054756));
#145697=CARTESIAN_POINT('Ctrl Pts',(-6.35454545129335,14.8710452666677,
16.4501220343486));
#145698=CARTESIAN_POINT('Origin',(-5.84999999999999,-0.250000000000012,
12.049999999963));
#145699=CARTESIAN_POINT('',(-6.7499999280398,-0.112130999061391,7.55127328017863));
#145700=CARTESIAN_POINT('Ctrl Pts',(-6.0957241205081,0.199999999999987,
7.15616513795545));
#145701=CARTESIAN_POINT('Ctrl Pts',(-6.16538230807449,0.153849386235404,
7.20587149527676));
#145702=CARTESIAN_POINT('Ctrl Pts',(-6.23747959335272,0.110374695194135,
7.25461326047291));
#145703=CARTESIAN_POINT('Ctrl Pts',(-6.45066439686828,-0.00428542164149448,
7.39054869428171));
#145704=CARTESIAN_POINT('Ctrl Pts',(-6.59752597145899,-0.0667024587113867,
7.47444115333255));
#145705=CARTESIAN_POINT('Ctrl Pts',(-6.7499999280398,-0.112130999061384,
7.55127328017863));
#145706=CARTESIAN_POINT('',(-6.35454550078494,-0.271045277532096,16.450122017738));
#145707=CARTESIAN_POINT('Ctrl Pts',(-6.35454550078344,-0.271045277531764,
16.4501220177385));
#145708=CARTESIAN_POINT('Ctrl Pts',(-6.0567466526599,-0.205672592100444,
16.5500705489484));
#145709=CARTESIAN_POINT('Ctrl Pts',(-5.76835567822078,-0.0899428765078181,
16.6667013016116));
#145710=CARTESIAN_POINT('Ctrl Pts',(-5.41464812969736,0.102033642101067,
16.8329226337617));
#145711=CARTESIAN_POINT('Ctrl Pts',(-5.33338146986815,0.149875808238858,
16.8728497987674));
#145712=CARTESIAN_POINT('Ctrl Pts',(-5.25380888164336,0.199999999999991,
16.9135949821128));
#145713=CARTESIAN_POINT('',(-7.59791508502123,-0.700000000000012,15.6478872766235));
#145714=CARTESIAN_POINT('Ctrl Pts',(-6.35454550078494,-0.271045277532095,
16.450122017738));
#145715=CARTESIAN_POINT('Ctrl Pts',(-6.46037908367833,-0.294277826431993,
16.4146016924801));
#145716=CARTESIAN_POINT('Ctrl Pts',(-6.56497371540389,-0.319750741234298,
16.3728674714568));
#145717=CARTESIAN_POINT('Ctrl Pts',(-6.92898212028428,-0.417979378007196,
16.2033520572508));
#145718=CARTESIAN_POINT('Ctrl Pts',(-7.17008331211839,-0.502368955533736,
16.0423295793347));
#145719=CARTESIAN_POINT('Ctrl Pts',(-7.4466010458344,-0.623606358833087,
15.8020015711092));
#145720=CARTESIAN_POINT('Ctrl Pts',(-7.52392855362119,-0.660695360703133,
15.7275286632141));
#145721=CARTESIAN_POINT('Ctrl Pts',(-7.59791508502124,-0.700000000000011,
15.6478872766235));
#145722=CARTESIAN_POINT('',(-7.94554708839804,-0.700000000000012,8.64284834494287));
#145723=CARTESIAN_POINT('Origin',(-5.84999999999999,-0.700000000000012,
12.049999999963));
#145724=CARTESIAN_POINT('Ctrl Pts',(-7.94554708839804,-0.70000000000001,
8.64284834494287));
#145725=CARTESIAN_POINT('Ctrl Pts',(-7.80142030539744,-0.578653740566923,
8.4117434285975));
#145726=CARTESIAN_POINT('Ctrl Pts',(-7.62292890725893,-0.467509856158084,
8.1991278933308));
#145727=CARTESIAN_POINT('Ctrl Pts',(-7.24069576991161,-0.279723800677587,
7.8471869437442));
#145728=CARTESIAN_POINT('Ctrl Pts',(-7.00710327840368,-0.188733116017182,
7.68082848788949));
#145729=CARTESIAN_POINT('Ctrl Pts',(-6.7499999280464,-0.112130999063354,
7.55127328018196));
#145730=CARTESIAN_POINT('Origin',(-5.12499999999999,15.3,12.049999999963));
#145731=CARTESIAN_POINT('',(-8.39999999999999,15.3,10.2303589813634));
#145732=CARTESIAN_POINT('',(-8.39999999999999,15.3,13.6060329039916));
#145733=CARTESIAN_POINT('',(-8.39999999999999,15.3,11.1401794906632));
#145734=CARTESIAN_POINT('Origin',(-5.39999999999998,15.3,13.6060329039916));
#145735=CARTESIAN_POINT('Origin',(-5.4,15.3,10.2303589813634));
#145736=CARTESIAN_POINT('',(-4.34999999999999,15.3,12.049999999963));
#145737=CARTESIAN_POINT('Origin',(-5.84999999999999,15.3,12.049999999963));
#145738=CARTESIAN_POINT('Origin',(-5.12499999999999,-0.700000000000012,
12.049999999963));
#145739=CARTESIAN_POINT('',(-8.39999999999999,-0.700000000000012,13.6060329039916));
#145740=CARTESIAN_POINT('Origin',(-5.39999999999998,-0.700000000000012,
13.6060329039916));
#145741=CARTESIAN_POINT('',(-8.39999999999999,-0.700000000000012,10.2303589813634));
#145742=CARTESIAN_POINT('',(-8.39999999999999,-0.700000000000012,12.8280164519773));
#145743=CARTESIAN_POINT('Origin',(-5.4,-0.700000000000012,10.2303589813634));
#145744=CARTESIAN_POINT('',(-4.34999999999999,-0.700000000000012,12.049999999963));
#145745=CARTESIAN_POINT('Origin',(-5.84999999999999,-0.700000000000012,
12.049999999963));
#145746=CARTESIAN_POINT('Origin',(-5.84999999999999,2.19999999999999,12.049999999963));
#145747=CARTESIAN_POINT('',(-7.94554708839804,2.3,8.64284834494287));
#145748=CARTESIAN_POINT('Ctrl Pts',(-7.6638591912008,2.09999999999999,8.26187185607765));
#145749=CARTESIAN_POINT('Ctrl Pts',(-7.76664216185284,2.16222477820042,
8.38007744138255));
#145750=CARTESIAN_POINT('Ctrl Pts',(-7.86173330152362,2.22943372970385,
8.50845432184085));
#145751=CARTESIAN_POINT('Ctrl Pts',(-7.94554708839804,2.29999999999999,
8.64284834494287));
#145752=CARTESIAN_POINT('',(-7.59791508502123,2.29999999999999,15.6478872766235));
#145753=CARTESIAN_POINT('Origin',(-5.84999999999999,2.29999999999999,12.049999999963));
#145754=CARTESIAN_POINT('Ctrl Pts',(-7.59791508502124,2.29999999999999,
15.6478872766235));
#145755=CARTESIAN_POINT('Ctrl Pts',(-7.52392855362119,2.26069536070311,
15.7275286632141));
#145756=CARTESIAN_POINT('Ctrl Pts',(-7.4466010458344,2.22360635883307,15.8020015711092));
#145757=CARTESIAN_POINT('Ctrl Pts',(-7.29927642305898,2.15901283541843,
15.9300448350199));
#145758=CARTESIAN_POINT('Ctrl Pts',(-7.2255360033652,2.12910947683608,15.9886060423839));
#145759=CARTESIAN_POINT('Ctrl Pts',(-7.1474157554001,2.09999999999999,16.0445853799042));
#145760=CARTESIAN_POINT('Origin',(-5.84999999999999,11.8,12.049999999963));
#145761=CARTESIAN_POINT('',(-7.59791508502123,11.7,15.6478872766235));
#145762=CARTESIAN_POINT('Ctrl Pts',(-7.1474157554001,11.9,16.0445853799042));
#145763=CARTESIAN_POINT('Ctrl Pts',(-7.2255360033652,11.8708905231639,15.9886060423839));
#145764=CARTESIAN_POINT('Ctrl Pts',(-7.29927642305897,11.8409871645816,
15.9300448350199));
#145765=CARTESIAN_POINT('Ctrl Pts',(-7.4466010458344,11.7763936411669,15.8020015711092));
#145766=CARTESIAN_POINT('Ctrl Pts',(-7.52392855362119,11.7393046392969,
15.7275286632141));
#145767=CARTESIAN_POINT('Ctrl Pts',(-7.59791508502124,11.7,15.6478872766235));
#145768=CARTESIAN_POINT('',(-7.94554708839804,11.7,8.64284834494287));
#145769=CARTESIAN_POINT('Origin',(-5.84999999999999,11.7,12.049999999963));
#145770=CARTESIAN_POINT('Ctrl Pts',(-7.94554708839804,11.7,8.64284834494287));
#145771=CARTESIAN_POINT('Ctrl Pts',(-7.86174205772034,11.7705588980944,
8.50846836225769));
#145772=CARTESIAN_POINT('Ctrl Pts',(-7.76664825426621,11.8377715334544,
8.38008444796432));
#145773=CARTESIAN_POINT('Ctrl Pts',(-7.66385919120079,11.9,8.26187185607765));
#145774=CARTESIAN_POINT('Origin',(-5.12499999999999,11.7,12.049999999963));
#145775=CARTESIAN_POINT('',(-8.39999999999999,11.7,13.6060329039916));
#145776=CARTESIAN_POINT('',(-8.39999999999999,11.7,10.2303589813634));
#145777=CARTESIAN_POINT('',(-8.39999999999999,11.7,11.1401794906632));
#145778=CARTESIAN_POINT('Origin',(-5.4,11.7,10.2303589813634));
#145779=CARTESIAN_POINT('Origin',(-5.39999999999998,11.7,13.6060329039916));
#145780=CARTESIAN_POINT('',(-4.34999999999999,11.7,12.049999999963));
#145781=CARTESIAN_POINT('Origin',(-5.84999999999999,11.7,12.049999999963));
#145782=CARTESIAN_POINT('Origin',(-5.12499999999999,2.29999999999999,12.049999999963));
#145783=CARTESIAN_POINT('',(-8.39999999999999,2.29999999999999,13.6060329039916));
#145784=CARTESIAN_POINT('Origin',(-5.39999999999998,2.29999999999999,13.6060329039916));
#145785=CARTESIAN_POINT('',(-8.39999999999999,2.29999999999999,10.2303589813634));
#145786=CARTESIAN_POINT('Origin',(-5.4,2.29999999999999,10.2303589813634));
#145787=CARTESIAN_POINT('',(-8.39999999999999,2.29999999999999,13.6060329039916));
#145788=CARTESIAN_POINT('',(-4.34999999999999,2.29999999999999,12.049999999963));
#145789=CARTESIAN_POINT('Origin',(-5.84999999999999,2.29999999999999,12.049999999963));
#145790=CARTESIAN_POINT('Origin',(-8.89999999999999,14.4,24.0343597112987));
#145791=CARTESIAN_POINT('',(-6.35454545454544,14.4,16.4501220332571));
#145792=CARTESIAN_POINT('Origin',(-5.39999999999999,14.4,10.2303589813634));
#145793=CARTESIAN_POINT('',(-8.39999999999999,14.4,10.2303589813634));
#145794=CARTESIAN_POINT('',(-6.74999999999999,14.4,7.55127331643961));
#145795=CARTESIAN_POINT('Origin',(-8.39999999999999,14.4,16.049999999963));
#145796=CARTESIAN_POINT('',(-8.39999999999999,11.9,13.6060329039916));
#145797=CARTESIAN_POINT('Origin',(-5.39999999999999,14.4,13.6060329039916));
#145798=CARTESIAN_POINT('Origin',(1.33226762955019E-14,0.0999999999999934,
-4.44089209850063E-15));
#145799=CARTESIAN_POINT('',(4.00000000000001,0.0999999999999934,-4.44089209850063E-15));
#145800=CARTESIAN_POINT('Origin',(1.33226762955019E-14,0.0999999999999934,
-4.44089209850063E-15));
#145801=CARTESIAN_POINT('',(1.60000000000001,0.0999999999999934,-4.44089209850063E-15));
#145802=CARTESIAN_POINT('Origin',(1.33226762955019E-14,0.0999999999999934,
-4.44089209850063E-15));
#145803=CARTESIAN_POINT('Origin',(-2.20000021345912,0.199999999999987,17.0249999999815));
#145804=CARTESIAN_POINT('',(1.75280925781799,0.199999999999987,-3.59550548681377));
#145805=CARTESIAN_POINT('Origin',(1.33226762955019E-14,0.199999999999991,
-4.44089209850063E-15));
#145806=CARTESIAN_POINT('',(4.21701869329868,0.199999999999991,-2.3942031587951));
#145807=CARTESIAN_POINT('Origin',(1.33226762955019E-14,14.5,-4.44089209850063E-15));
#145808=CARTESIAN_POINT('',(4.00000000000001,14.5,-4.44089209850063E-15));
#145809=CARTESIAN_POINT('Origin',(1.33226762955019E-14,14.5,-4.44089209850063E-15));
#145810=CARTESIAN_POINT('',(1.60000000000001,14.5,-4.44089209850063E-15));
#145811=CARTESIAN_POINT('Origin',(1.33226762955019E-14,14.5,-4.44089209850063E-15));
#145812=CARTESIAN_POINT('Origin',(-2.20000021345912,14.4,17.0249999999815));
#145813=CARTESIAN_POINT('',(1.75280925781799,14.4,-3.59550548681377));
#145814=CARTESIAN_POINT('Origin',(1.33226762955019E-14,14.4,-4.44089209850063E-15));
#145815=CARTESIAN_POINT('',(3.99999957308175,14.4,-2.5));
#145816=CARTESIAN_POINT('Origin',(-3.99999999999999,14.4,8.04999999996301));
#145817=CARTESIAN_POINT('',(-3.99999999999999,14.4,-4.44089209850063E-15));
#145818=CARTESIAN_POINT('',(-3.99999999999999,14.4,3.08613054156667));
#145819=CARTESIAN_POINT('Origin',(-8.39999999999999,14.4,16.049999999963));
#145820=CARTESIAN_POINT('',(-8.39999999999999,14.4,10.2303589813634));
#145821=CARTESIAN_POINT('',(-8.39999999999999,14.4,13.6060329039916));
#145822=CARTESIAN_POINT('Origin',(-8.99999999999999,14.4,3.08613054156667));
#145823=CARTESIAN_POINT('Origin',(-8.99999999999999,14.4,3.08613054156667));
#145824=CARTESIAN_POINT('',(-6.74999999999999,14.4,7.55127331643961));
#145825=CARTESIAN_POINT('Origin',(-5.39999999999999,14.4,10.2303589813634));
#145826=CARTESIAN_POINT('Origin',(-5.84999999999999,14.4,12.049999999963));
#145827=CARTESIAN_POINT('',(-4.34999999999999,14.4,12.049999999963));
#145828=CARTESIAN_POINT('Origin',(-5.39999999999999,14.4,13.6060329039916));
#145829=CARTESIAN_POINT('Origin',(3.99999957308175,14.4,38.299999999963));
#145830=CARTESIAN_POINT('Origin',(1.75280925781799,14.4,-3.59550548681377));
#145831=CARTESIAN_POINT('',(1.75280925781799,14.4,-3.59550548681377));
#145832=CARTESIAN_POINT('Origin',(1.33226762955019E-14,14.4,-4.44089209850063E-15));
#145833=CARTESIAN_POINT('',(1.60000000000001,14.4,-4.24494861063705E-15));
#145834=CARTESIAN_POINT('Origin',(-5.84999999999999,14.4,12.049999999963));
#145835=CARTESIAN_POINT('',(-4.34999999999999,14.4,12.049999999963));
#145836=CARTESIAN_POINT('Origin',(1.33226762955019E-14,14.4,-4.44089209850063E-15));
#145837=CARTESIAN_POINT('',(4.00000000000001,14.4,-3.95103337884168E-15));
#145838=CARTESIAN_POINT('',(4.00000000000001,14.4,-3.95103337884168E-15));
#145839=CARTESIAN_POINT('',(0.,0.,0.));
#145840=CARTESIAN_POINT('Origin',(4.44089209850063E-15,0.,0.1));
#145841=CARTESIAN_POINT('',(1.30000000000001,0.,0.));
#145842=CARTESIAN_POINT('Origin',(4.44089209850063E-15,0.,0.));
#145843=CARTESIAN_POINT('',(1.50000000000001,0.,0.2));
#145844=CARTESIAN_POINT('',(1.40000000000001,-1.7145055188063E-16,0.1));
#145845=CARTESIAN_POINT('Origin',(4.44089209850063E-15,0.,0.2));
#145846=CARTESIAN_POINT('Origin',(4.44089209850063E-15,2.22044604925031E-15,
24.));
#145847=CARTESIAN_POINT('',(1.50000000000001,2.22044604925031E-15,23.8));
#145848=CARTESIAN_POINT('',(1.50000000000001,2.03674902937821E-15,24.));
#145849=CARTESIAN_POINT('Origin',(4.44089209850063E-15,2.22044604925031E-15,
23.8));
#145850=CARTESIAN_POINT('Origin',(4.44089209850063E-15,0.,0.));
#145851=CARTESIAN_POINT('Origin',(4.44089209850063E-15,2.22044604925031E-15,
23.9));
#145852=CARTESIAN_POINT('',(1.30000000000001,2.22044604925031E-15,24.));
#145853=CARTESIAN_POINT('Origin',(4.44089209850063E-15,2.22044604925031E-15,
24.));
#145854=CARTESIAN_POINT('',(1.40000000000001,2.39189660113094E-15,23.9));
#145855=CARTESIAN_POINT('Origin',(4.44089209850063E-15,2.22044604925031E-15,
24.));
#145856=CARTESIAN_POINT('',(0.,0.,0.));
#145857=CARTESIAN_POINT('Origin',(-8.84687992363536,110.965520572543,16.0678367667527));
#145858=CARTESIAN_POINT('',(-10.2468799236354,111.015520572543,16.0678367667527));
#145859=CARTESIAN_POINT('Origin',(-8.84687992363536,111.015520572543,16.0678367667527));
#145860=CARTESIAN_POINT('',(-10.3468799236354,110.915520572543,16.0678367667527));
#145861=CARTESIAN_POINT('',(-10.2968799236354,110.965520572543,16.0678367667527));
#145862=CARTESIAN_POINT('Origin',(-8.84687992363536,110.915520572543,16.0678367667527));
#145863=CARTESIAN_POINT('Origin',(-8.84687992363537,98.5155205725429,16.0678367667527));
#145864=CARTESIAN_POINT('',(-10.3468799236354,95.1155205725429,16.0678367667528));
#145865=CARTESIAN_POINT('Origin',(-8.84687992363537,95.1155205725429,16.0678367667528));
#145866=CARTESIAN_POINT('',(-10.3468799236354,98.5155205725429,16.0678367667527));
#145867=CARTESIAN_POINT('Origin',(-8.84687992363536,111.015520572543,16.0678367667527));
#145868=CARTESIAN_POINT('Origin',(-8.84687992363537,95.065520572543,16.0678367667528));
#145869=CARTESIAN_POINT('',(-10.2468799236354,95.0155205725429,16.0678367667528));
#145870=CARTESIAN_POINT('Origin',(-8.84687992363537,95.0155205725429,16.0678367667528));
#145871=CARTESIAN_POINT('',(-10.2968799236354,95.065520572543,16.0678367667528));
#145872=CARTESIAN_POINT('Origin',(-8.84687992363537,95.0155205725429,16.0678367667528));
#145873=CARTESIAN_POINT('',(0.,0.,0.));
#145874=CARTESIAN_POINT('Origin',(1.11022302462516E-15,-1.77635683940025E-14,
2.22044604925031E-15));
#145875=CARTESIAN_POINT('',(8.993316745,-1.00000000000002,-0.346776472999999));
#145876=CARTESIAN_POINT('',(8.993316745,0.999999999999982,-0.346776472999999));
#145877=CARTESIAN_POINT('Ctrl Pts',(8.99331674501319,-0.999999999990532,
-0.346776473489777));
#145878=CARTESIAN_POINT('Ctrl Pts',(8.92005828617723,-0.888963444672732,
-0.346598504102869));
#145879=CARTESIAN_POINT('Ctrl Pts',(8.85904637943913,-0.76995646962542,
-0.346446577592176));
#145880=CARTESIAN_POINT('Ctrl Pts',(8.72757931577561,-0.424051722950309,
-0.34611575375876));
#145881=CARTESIAN_POINT('Ctrl Pts',(8.68754893604535,-0.18879105880841,
-0.346011201242058));
#145882=CARTESIAN_POINT('Ctrl Pts',(8.69992957774455,0.283921315910095,
-0.346043086203101));
#145883=CARTESIAN_POINT('Ctrl Pts',(8.75224857096735,0.516830885584916,
-0.346179200855117));
#145884=CARTESIAN_POINT('Ctrl Pts',(8.88881765021319,0.826237684539586,
-0.346520446328741));
#145885=CARTESIAN_POINT('Ctrl Pts',(8.93754891983208,0.915473689936097,
-0.346640994723032));
#145886=CARTESIAN_POINT('Ctrl Pts',(8.99331674501319,0.999999999990496,
-0.346776473489776));
#145887=CARTESIAN_POINT('',(8.988197099,-1.00000000000002,-0.460774244));
#145888=CARTESIAN_POINT('Origin',(1.11022302462516E-15,-1.00000000000002,
2.22044604925031E-15));
#145889=CARTESIAN_POINT('',(8.988197099,0.999999999999982,-0.460774244));
#145890=CARTESIAN_POINT('Ctrl Pts',(8.9881970991918,0.999999999893166,-0.460774243665515));
#145891=CARTESIAN_POINT('Ctrl Pts',(8.91521760434871,0.888963444601223,
-0.454384658959212));
#145892=CARTESIAN_POINT('Ctrl Pts',(8.85443769504401,0.76995646958464,-0.449066908687326));
#145893=CARTESIAN_POINT('Ctrl Pts',(8.72347022432541,0.424051722946438,
-0.43761178395344));
#145894=CARTESIAN_POINT('Ctrl Pts',(8.6835916231211,0.18879105880802,-0.434127619986626));
#145895=CARTESIAN_POINT('Ctrl Pts',(8.69592528214153,-0.28392131590547,
-0.435205655554323));
#145896=CARTESIAN_POINT('Ctrl Pts',(8.74804585570079,-0.516830885578334,
-0.439759927270131));
#145897=CARTESIAN_POINT('Ctrl Pts',(8.88409573697414,-0.826237684498686,
-0.451662013470527));
#145898=CARTESIAN_POINT('Ctrl Pts',(8.93264163468216,-0.915473689865194,
-0.455910187711914));
#145899=CARTESIAN_POINT('Ctrl Pts',(8.9881970991918,-0.999999999893202,
-0.460774243665515));
#145900=CARTESIAN_POINT('Origin',(1.11022302462516E-15,0.999999999999982,
2.22044604925031E-15));
#145901=CARTESIAN_POINT('Origin',(1.11022302462516E-15,-1.77635683940025E-14,
2.22044604925031E-15));
#145902=CARTESIAN_POINT('',(8.926027492,-1.00000000000002,-1.151535151));
#145903=CARTESIAN_POINT('',(8.926027492,0.999999999999982,-1.151535151));
#145904=CARTESIAN_POINT('Ctrl Pts',(8.92602749221155,-0.999999999831737,
-1.15153515148245));
#145905=CARTESIAN_POINT('Ctrl Pts',(8.85307990349065,-0.88896344455843,
-1.14479106093982));
#145906=CARTESIAN_POINT('Ctrl Pts',(8.79232723137321,-0.769956469564023,
-1.1391706808964));
#145907=CARTESIAN_POINT('Ctrl Pts',(8.66141907029811,-0.42405172294863,
-1.12705657215028));
#145908=CARTESIAN_POINT('Ctrl Pts',(8.6215592131229,-0.188791058808235,
-1.12336414496197));
#145909=CARTESIAN_POINT('Ctrl Pts',(8.63388715585244,0.283921315908099,
-1.1245056937277));
#145910=CARTESIAN_POINT('Ctrl Pts',(8.68598332696715,0.516830885582071,
-1.1293310988108));
#145911=CARTESIAN_POINT('Ctrl Pts',(8.82197203021842,0.826237684479057,
-1.14191292839256));
#145912=CARTESIAN_POINT('Ctrl Pts',(8.87049631616405,0.915473689823285,
-1.14640122881592));
#145913=CARTESIAN_POINT('Ctrl Pts',(8.92602749221155,0.999999999831702,
-1.15153515148245));
#145914=CARTESIAN_POINT('',(8.910709775,-1.00000000000002,-1.264615079));
#145915=CARTESIAN_POINT('Origin',(1.11022302462516E-15,-1.00000000000002,
2.22044604925031E-15));
#145916=CARTESIAN_POINT('',(8.910709775,0.999999999999982,-1.264615079));
#145917=CARTESIAN_POINT('Ctrl Pts',(8.9107097753288,0.999999999842809,-1.26461507851505));
#145918=CARTESIAN_POINT('Ctrl Pts',(8.83859683244853,0.888963444565197,
-1.25170938491645));
#145919=CARTESIAN_POINT('Ctrl Pts',(8.7785382846604,0.769956469565656,-1.24096477327833));
#145920=CARTESIAN_POINT('Ctrl Pts',(8.64912487994753,0.424051722946349,
-1.21781592994151));
#145921=CARTESIAN_POINT('Ctrl Pts',(8.6097191363179,0.188791058808013,-1.21077110194112));
#145922=CARTESIAN_POINT('Ctrl Pts',(8.6219065092898,-0.28392131590536,-1.21295037832583));
#145923=CARTESIAN_POINT('Ctrl Pts',(8.67340901897361,-0.516830885578179,
-1.22215836807797));
#145924=CARTESIAN_POINT('Ctrl Pts',(8.8078443086326,-0.82623768448008,-1.24620795731553));
#145925=CARTESIAN_POINT('Ctrl Pts',(8.85581397141433,-0.915473689829693,
-1.25479065037674));
#145926=CARTESIAN_POINT('Ctrl Pts',(8.9107097753288,-0.999999999842844,
-1.26461507851505));
#145927=CARTESIAN_POINT('Origin',(1.11022302462516E-15,0.999999999999982,
2.22044604925031E-15));
#145928=CARTESIAN_POINT('Origin',(1.11022302462516E-15,-1.77635683940025E-14,
2.22044604925031E-15));
#145929=CARTESIAN_POINT('',(8.786871115,-1.00000000000002,-1.947022345));
#145930=CARTESIAN_POINT('',(8.786871115,0.999999999999982,-1.947022345));
#145931=CARTESIAN_POINT('Ctrl Pts',(8.78687111484236,-1.00000000011924,
-1.9470223448582));
#145932=CARTESIAN_POINT('Ctrl Pts',(8.71482172720569,-0.888963444765539,
-1.93376643256629));
#145933=CARTESIAN_POINT('Ctrl Pts',(8.65481743440953,-0.769956469675546,
-1.92272285094909));
#145934=CARTESIAN_POINT('Ctrl Pts',(8.52552217140722,-0.424051722951982,
-1.89892299290974));
#145935=CARTESIAN_POINT('Ctrl Pts',(8.48615376492162,-0.188791058808556,
-1.89167242028617));
#145936=CARTESIAN_POINT('Ctrl Pts',(8.49832975133559,0.283921315912148,
-1.89391444178229));
#145937=CARTESIAN_POINT('Ctrl Pts',(8.54978365260218,0.516830885587828,
-1.90339028599331));
#145938=CARTESIAN_POINT('Ctrl Pts',(8.68409707884376,0.826237684589113,
-1.92811139825368));
#145939=CARTESIAN_POINT('Ctrl Pts',(8.73202369219063,0.915473690027751,
-1.9369313135815));
#145940=CARTESIAN_POINT('Ctrl Pts',(8.78687111484236,1.0000000001192,-1.9470223448582));
#145941=CARTESIAN_POINT('',(8.761478656,-1.00000000000002,-2.058273976));
#145942=CARTESIAN_POINT('Origin',(1.11022302462516E-15,-1.00000000000002,
2.22044604925031E-15));
#145943=CARTESIAN_POINT('',(8.761478656,0.999999999999982,-2.058273976));
#145944=CARTESIAN_POINT('Ctrl Pts',(8.76147865610178,1.00000000003545,-2.05827397542385));
#145945=CARTESIAN_POINT('Ctrl Pts',(8.69081287612847,0.888963444702555,
-2.03895608197732));
#145946=CARTESIAN_POINT('Ctrl Pts',(8.63195924591628,0.769956469637271,
-2.02287111825923));
#145947=CARTESIAN_POINT('Ctrl Pts',(8.50514186781519,0.424051722945794,
-1.9882149371944));
#145948=CARTESIAN_POINT('Ctrl Pts',(8.4665262536374,0.188791058807998,-1.97766616597551));
#145949=CARTESIAN_POINT('Ctrl Pts',(8.47846921499966,-0.283921315904603,
-1.98092913692443));
#145950=CARTESIAN_POINT('Ctrl Pts',(8.52893899288346,-0.516830885577122,
-1.9947167073906));
#145951=CARTESIAN_POINT('Ctrl Pts',(8.66067729706199,-0.826237684549968,
-2.03072016651486));
#145952=CARTESIAN_POINT('Ctrl Pts',(8.70768450145157,-0.915473689964895,
-2.04356827560745));
#145953=CARTESIAN_POINT('Ctrl Pts',(8.76147865610178,-1.00000000003548,
-2.05827397542385));
#145954=CARTESIAN_POINT('Origin',(1.11022302462516E-15,0.999999999999982,
2.22044604925031E-15));
#145955=CARTESIAN_POINT('Origin',(1.11022302462516E-15,-1.77635683940025E-14,
2.22044604925031E-15));
#145956=CARTESIAN_POINT('',(8.576968018,-1.00000000000002,-2.726833259));
#145957=CARTESIAN_POINT('',(8.576968018,0.999999999999982,-2.726833259));
#145958=CARTESIAN_POINT('Ctrl Pts',(8.57696801776425,-1.00000000013926,
-2.72683325905983));
#145959=CARTESIAN_POINT('Ctrl Pts',(8.50639693059222,-0.88896344478025,
-2.70717225385519));
#145960=CARTESIAN_POINT('Ctrl Pts',(8.44762413645845,-0.769956469683949,
-2.69079438711029));
#145961=CARTESIAN_POINT('Ctrl Pts',(8.32098278099789,-0.42405172295278,
-2.65550040227742));
#145962=CARTESIAN_POINT('Ctrl Pts',(8.28242279646211,-0.188791058808601,
-2.64475006157633));
#145963=CARTESIAN_POINT('Ctrl Pts',(8.29434879267705,0.283921315913182,
-2.64807450436084));
#145964=CARTESIAN_POINT('Ctrl Pts',(8.34474614753761,0.51683088558928,-2.66212449376052));
#145965=CARTESIAN_POINT('Ctrl Pts',(8.47630288399607,0.826237684597597,
-2.69878584880073));
#145966=CARTESIAN_POINT('Ctrl Pts',(8.52324594777668,0.915473690042371,
-2.71186636624358));
#145967=CARTESIAN_POINT('Ctrl Pts',(8.57696801776425,1.00000000013922,-2.72683325905983));
#145968=CARTESIAN_POINT('',(8.541705262,-1.00000000000002,-2.835360862));
#145969=CARTESIAN_POINT('Origin',(1.11022302462516E-15,-1.00000000000002,
2.22044604925031E-15));
#145970=CARTESIAN_POINT('',(8.541705262,0.999999999999982,-2.835360862));
#145971=CARTESIAN_POINT('Ctrl Pts',(8.54170526175661,1.00000000003763,-2.83536086248987));
#145972=CARTESIAN_POINT('Ctrl Pts',(8.47305560404579,0.888963444707527,
-2.80978630556046));
#145973=CARTESIAN_POINT('Ctrl Pts',(8.41588074626889,0.769956469645603,
-2.78849049646969));
#145974=CARTESIAN_POINT('Ctrl Pts',(8.29268045374403,0.424051722952562,
-2.74260600893571));
#145975=CARTESIAN_POINT('Ctrl Pts',(8.25516587923031,0.188791058808566,
-2.72863822702008));
#145976=CARTESIAN_POINT('Ctrl Pts',(8.26676827128391,-0.283921315912958,
-2.73295862100441));
#145977=CARTESIAN_POINT('Ctrl Pts',(8.31579896440192,-0.516830885588957,
-2.75121476275006));
#145978=CARTESIAN_POINT('Ctrl Pts',(8.44377960372841,-0.826237684560067,
-2.7988822130079));
#145979=CARTESIAN_POINT('Ctrl Pts',(8.48944587531942,-0.915473689970773,
-2.81589229268048));
#145980=CARTESIAN_POINT('Ctrl Pts',(8.54170526175661,-1.00000000003766,
-2.83536086248987));
#145981=CARTESIAN_POINT('Origin',(1.11022302462516E-15,0.999999999999982,
2.22044604925031E-15));
#145982=CARTESIAN_POINT('Origin',(1.11022302462516E-15,-1.77635683940025E-14,
2.22044604925031E-15));
#145983=CARTESIAN_POINT('',(8.298008217,-1.00000000000002,-3.484689316));
#145984=CARTESIAN_POINT('',(8.298008217,0.999999999999982,-3.484689317));
#145985=CARTESIAN_POINT('Ctrl Pts',(8.29800821680649,-0.999999999999693,
-3.48468931651321));
#145986=CARTESIAN_POINT('Ctrl Pts',(8.22948362702784,-0.888963444677954,
-3.4587815172934));
#145987=CARTESIAN_POINT('Ctrl Pts',(8.17241553555906,-0.769956469625942,
-3.43720123040944));
#145988=CARTESIAN_POINT('Ctrl Pts',(8.04944772937248,-0.424051722947685,
-3.39069728525703));
#145989=CARTESIAN_POINT('Ctrl Pts',(8.0120066291036,-0.188791058808186,
-3.37653373191683));
#145990=CARTESIAN_POINT('Ctrl Pts',(8.02358661401111,0.283921315906866,
-3.38091382952584));
#145991=CARTESIAN_POINT('Ctrl Pts',(8.07252165260454,0.516830885580342,
-3.39942484183956));
#145992=CARTESIAN_POINT('Ctrl Pts',(8.2002624818134,0.826237684599015,-3.4477312639312));
#145993=CARTESIAN_POINT('Ctrl Pts',(8.24584403809067,0.915473690055275,
-3.4649670668361));
#145994=CARTESIAN_POINT('Ctrl Pts',(8.29800821690682,1.00000000016222,-3.48468931655114));
#145995=CARTESIAN_POINT('',(8.253159079,-1.00000000000002,-3.58961909));
#145996=CARTESIAN_POINT('Origin',(1.11022302462516E-15,-1.00000000000002,
2.22044604925031E-15));
#145997=CARTESIAN_POINT('',(8.253159079,0.999999999999982,-3.58961909));
#145998=CARTESIAN_POINT('Ctrl Pts',(8.25315907930141,0.999999999897839,
-3.58961908972884));
#145999=CARTESIAN_POINT('Ctrl Pts',(8.18707827057777,0.888963444607218,
-3.55799378058502));
#146000=CARTESIAN_POINT('Ctrl Pts',(8.13204252360867,0.769956469592238,
-3.53165858743165));
#146001=CARTESIAN_POINT('Ctrl Pts',(8.01345125301593,0.424051722951706,
-3.47491522827454));
#146002=CARTESIAN_POINT('Ctrl Pts',(7.97733976346943,0.188791058808487,
-3.45764089600619));
#146003=CARTESIAN_POINT('Ctrl Pts',(7.98850817057213,-0.283921315911917,
-3.46298392776071));
#146004=CARTESIAN_POINT('Ctrl Pts',(8.03570501260313,-0.516830885587481,
-3.48556165309702));
#146005=CARTESIAN_POINT('Ctrl Pts',(8.15889756217779,-0.826237684507598,
-3.54450930427714));
#146006=CARTESIAN_POINT('Ctrl Pts',(8.20285522296936,-0.915473689871846,
-3.56554439938598));
#146007=CARTESIAN_POINT('Ctrl Pts',(8.25315907930141,-0.999999999897875,
-3.58961908972884));
#146008=CARTESIAN_POINT('Origin',(1.11022302462516E-15,0.999999999999982,
2.22044604925031E-15));
#146009=CARTESIAN_POINT('Origin',(1.11022302462516E-15,-1.77635683940025E-14,
2.22044604925031E-15));
#146010=CARTESIAN_POINT('',(7.952237733,-1.00000000000002,-4.214488703));
#146011=CARTESIAN_POINT('',(7.952237733,0.999999999999982,-4.214488703));
#146012=CARTESIAN_POINT('Ctrl Pts',(7.95223773319635,-0.999999999775502,
-4.21448870337516));
#146013=CARTESIAN_POINT('Ctrl Pts',(7.88631136054351,-0.888963444517432,
-4.18254270450202));
#146014=CARTESIAN_POINT('Ctrl Pts',(7.83140745047794,-0.769956469541136,
-4.15593374925552));
#146015=CARTESIAN_POINT('Ctrl Pts',(7.71310325805549,-0.424051722947019,
-4.0985942661749));
#146016=CARTESIAN_POINT('Ctrl Pts',(7.6770824957803,-0.188791058808112,
-4.08113153678696));
#146017=CARTESIAN_POINT('Ctrl Pts',(7.68822323415081,0.283921315906083,
-4.08653202325389));
#146018=CARTESIAN_POINT('Ctrl Pts',(7.73530196031659,0.516830885579221,
-4.10935501871067));
#146019=CARTESIAN_POINT('Ctrl Pts',(7.85819838815941,0.826237684456182,
-4.1689175729596));
#146020=CARTESIAN_POINT('Ctrl Pts',(7.90205144095589,0.915473689782661,
-4.19016988875141));
#146021=CARTESIAN_POINT('Ctrl Pts',(7.95223773319635,0.999999999775467,
-4.21448870337516));
#146022=CARTESIAN_POINT('',(7.898163313,-1.00000000000002,-4.314975815));
#146023=CARTESIAN_POINT('Origin',(1.11022302462516E-15,-1.00000000000002,
2.22044604925031E-15));
#146024=CARTESIAN_POINT('',(7.898163313,0.999999999999982,-4.314975815));
#146025=CARTESIAN_POINT('Ctrl Pts',(7.89816331271264,1.00000000009806,-4.31497581519262));
#146026=CARTESIAN_POINT('Ctrl Pts',(7.83518339669397,0.88896344475189,-4.277554382208));
#146027=CARTESIAN_POINT('Ctrl Pts',(7.78272987593037,0.769956469670873,
-4.24639184046861));
#146028=CARTESIAN_POINT('Ctrl Pts',(7.66970245438489,0.424051722954895,
-4.17924647387125));
#146029=CARTESIAN_POINT('Ctrl Pts',(7.63528479827936,0.188791058808738,
-4.15880467402876));
#146030=CARTESIAN_POINT('Ctrl Pts',(7.64592929898681,-0.283921315915892,
-4.16512732459995));
#146031=CARTESIAN_POINT('Ctrl Pts',(7.69091228871913,-0.516830885593102,
-4.19184485094197));
#146032=CARTESIAN_POINT('Ctrl Pts',(7.80832487464018,-0.826237684585495,
-4.26159809119923));
#146033=CARTESIAN_POINT('Ctrl Pts',(7.85022000346808,-0.915473690014823,
-4.28648883954431));
#146034=CARTESIAN_POINT('Ctrl Pts',(7.89816331271264,-1.00000000009809,
-4.31497581519262));
#146035=CARTESIAN_POINT('Origin',(1.11022302462516E-15,0.999999999999982,
2.22044604925031E-15));
#146036=CARTESIAN_POINT('Origin',(1.11022302462516E-15,-1.77635683940025E-14,
2.22044604925031E-15));
#146037=CARTESIAN_POINT('',(7.542440507,-1.00000000000002,-4.910355505));
#146038=CARTESIAN_POINT('',(7.542440507,0.999999999999982,-4.910355506));
#146039=CARTESIAN_POINT('Ctrl Pts',(7.54244050699415,-0.999999999713361,
-4.91035550585342));
#146040=CARTESIAN_POINT('Ctrl Pts',(7.47964315180284,-0.888963444471707,
-4.87262851771894));
#146041=CARTESIAN_POINT('Ctrl Pts',(7.42734547710069,-0.769956469514917,
-4.84120513376688));
#146042=CARTESIAN_POINT('Ctrl Pts',(7.31465741420511,-0.424051722944403,
-4.77349177656747));
#146043=CARTESIAN_POINT('Ctrl Pts',(7.2803470079185,-0.18879105880792,-4.75287047076504));
#146044=CARTESIAN_POINT('Ctrl Pts',(7.29095880107796,0.283921315902789,
-4.75924786454684));
#146045=CARTESIAN_POINT('Ctrl Pts',(7.33580216459886,0.516830885574571,
-4.78619908580148));
#146046=CARTESIAN_POINT('Ctrl Pts',(7.4528647013947,0.826237684516619,-4.85653820956603));
#146047=CARTESIAN_POINT('Ctrl Pts',(7.49463617183292,0.915473689903834,
-4.88163592714012));
#146048=CARTESIAN_POINT('Ctrl Pts',(7.54244050712803,0.99999999995005,-4.91035550593385));
#146049=CARTESIAN_POINT('',(7.47957618,-1.00000000000002,-5.005590891));
#146050=CARTESIAN_POINT('Origin',(1.11022302462516E-15,-1.00000000000002,
2.22044604925031E-15));
#146051=CARTESIAN_POINT('',(7.47957618,0.999999999999982,-5.005590891));
#146052=CARTESIAN_POINT('Ctrl Pts',(7.47957617982888,1.00000000003923,-5.00559089113518));
#146053=CARTESIAN_POINT('Ctrl Pts',(7.42020423385493,0.888963444707324,
-4.96267462967732));
#146054=CARTESIAN_POINT('Ctrl Pts',(7.37075526427221,0.769956469643232,
-4.92693564180633));
#146055=CARTESIAN_POINT('Ctrl Pts',(7.2642017221897,0.424051722949885,-4.84992888272495));
#146056=CARTESIAN_POINT('Ctrl Pts',(7.23175501026859,0.188791058808343,
-4.82648420063957));
#146057=CARTESIAN_POINT('Ctrl Pts',(7.24178990131453,-0.283921315909651,
-4.83373556376861));
#146058=CARTESIAN_POINT('Ctrl Pts',(7.28419686214625,-0.516830885584273,
-4.8643777773319));
#146059=CARTESIAN_POINT('Ctrl Pts',(7.39488414722774,-0.826237684556975,
-4.94437499464598));
#146060=CARTESIAN_POINT('Ctrl Pts',(7.43437942908497,-0.915473689970184,
-4.9729209905592));
#146061=CARTESIAN_POINT('Ctrl Pts',(7.47957617982888,-1.00000000003927,
-5.00559089113518));
#146062=CARTESIAN_POINT('Origin',(1.11022302462516E-15,0.999999999999982,
2.22044604925031E-15));
#146063=CARTESIAN_POINT('Origin',(1.11022302462516E-15,-1.77635683940025E-14,
2.22044604925031E-15));
#146064=CARTESIAN_POINT('',(7.071915986,-1.00000000000002,-5.566687012));
#146065=CARTESIAN_POINT('',(7.071915985,0.999999999999982,-5.566687013));
#146066=CARTESIAN_POINT('Ctrl Pts',(7.07191598537279,-1.00000000011093,
-5.56668701257384));
#146067=CARTESIAN_POINT('Ctrl Pts',(7.01275325493728,-0.888963444757714,
-5.52348279059387));
#146068=CARTESIAN_POINT('Ctrl Pts',(6.96348288566105,-0.769956469668278,
-5.48749798046137));
#146069=CARTESIAN_POINT('Ctrl Pts',(6.85731825030078,-0.424051722948234,
-5.4099559371812));
#146070=CARTESIAN_POINT('Ctrl Pts',(6.82499444723148,-0.188791058808213,
-5.38634208557447));
#146071=CARTESIAN_POINT('Ctrl Pts',(6.83499185525839,0.283921315907583,
-5.39364503965271));
#146072=CARTESIAN_POINT('Ctrl Pts',(6.87723880372388,0.516830885581344,
-5.4245074913437));
#146073=CARTESIAN_POINT('Ctrl Pts',(6.98752493069896,0.826237684544213,
-5.50505685541548));
#146074=CARTESIAN_POINT('Ctrl Pts',(7.02687849941884,0.915473689949043,
-5.53379790271953));
#146075=CARTESIAN_POINT('Ctrl Pts',(7.07191598531944,1.00000000001076,-5.56668701253488));
#146076=CARTESIAN_POINT('',(7.000767897,-1.00000000000002,-5.655903894));
#146077=CARTESIAN_POINT('Origin',(1.11022302462516E-15,-1.00000000000002,
2.22044604925031E-15));
#146078=CARTESIAN_POINT('',(7.000767897,0.999999999999982,-5.655903894));
#146079=CARTESIAN_POINT('Ctrl Pts',(7.00076789681102,1.00000000017972,-5.65590389380216));
#146080=CARTESIAN_POINT('Ctrl Pts',(6.94548194883083,0.888963444807022,
-5.60783834035334));
#146081=CARTESIAN_POINT('Ctrl Pts',(6.89943566441819,0.769956469694419,
-5.56781065565214));
#146082=CARTESIAN_POINT('Ctrl Pts',(6.8002139082344,0.424051722948536,-5.48156251723961));
#146083=CARTESIAN_POINT('Ctrl Pts',(6.76999938234043,0.188791058808216,
-5.4553037157138));
#146084=CARTESIAN_POINT('Ctrl Pts',(6.77934386868416,-0.283921315908016,
-5.46342540768646));
#146085=CARTESIAN_POINT('Ctrl Pts',(6.81883336470601,-0.516830885581949,
-5.49774559537489));
#146086=CARTESIAN_POINT('Ctrl Pts',(6.92190416004712,-0.826237684606703,
-5.58734269918266));
#146087=CARTESIAN_POINT('Ctrl Pts',(6.958681602184,-0.9154736900682,-5.61931410710659));
#146088=CARTESIAN_POINT('Ctrl Pts',(7.00076789681102,-1.00000000017975,
-5.65590389380216));
#146089=CARTESIAN_POINT('Origin',(1.11022302462516E-15,0.999999999999982,
2.22044604925031E-15));
#146090=CARTESIAN_POINT('Origin',(1.11022302462516E-15,-1.77635683940025E-14,
2.22044604925031E-15));
#146091=CARTESIAN_POINT('',(6.544452554,-1.00000000000002,-6.178198829));
#146092=CARTESIAN_POINT('',(6.544452554,0.999999999999982,-6.178198829));
#146093=CARTESIAN_POINT('Ctrl Pts',(6.54445255416351,-1.0000000000805,-6.17819882862886));
#146094=CARTESIAN_POINT('Ctrl Pts',(6.4894007921,-0.888963444736671,-6.12986522787583));
#146095=CARTESIAN_POINT('Ctrl Pts',(6.44355442436668,-0.769956469658398,
-6.08960872015794));
#146096=CARTESIAN_POINT('Ctrl Pts',(6.34476799180017,-0.424051722949613,
-6.00286231379505));
#146097=CARTESIAN_POINT('Ctrl Pts',(6.31469104420046,-0.188791058808339,
-5.97644604124083));
#146098=CARTESIAN_POINT('Ctrl Pts',(6.32399357384459,0.283921315909266,
-5.98461575652057));
#146099=CARTESIAN_POINT('Ctrl Pts',(6.36330395967154,0.516830885583735,
-6.01914095232269));
#146100=CARTESIAN_POINT('Ctrl Pts',(6.46592571779309,0.826237684571677,
-6.10925202055844));
#146101=CARTESIAN_POINT('Ctrl Pts',(6.50254453300505,0.915473689998984,
-6.14140499157264));
#146102=CARTESIAN_POINT('Ctrl Pts',(6.54445255416351,1.00000000008047,-6.17819882862886));
#146103=CARTESIAN_POINT('',(6.465593548,-1.00000000000002,-6.260678883));
#146104=CARTESIAN_POINT('Origin',(1.11022302462516E-15,-1.00000000000002,
2.22044604925031E-15));
#146105=CARTESIAN_POINT('',(6.465593547,0.999999999999982,-6.260678883));
#146106=CARTESIAN_POINT('Ctrl Pts',(6.46559354762128,0.99999999981135,-6.26067888279958));
#146107=CARTESIAN_POINT('Ctrl Pts',(6.41483872768217,0.888963444543264,
-6.20785103304572));
#146108=CARTESIAN_POINT('Ctrl Pts',(6.37256586612411,0.769956469555061,
-6.1638569309814));
#146109=CARTESIAN_POINT('Ctrl Pts',(6.28147477111903,0.424051722947445,
-6.06906183260181));
#146110=CARTESIAN_POINT('Ctrl Pts',(6.25373570084517,0.18879105880813,-6.04020033207072));
#146111=CARTESIAN_POINT('Ctrl Pts',(6.26231454617831,-0.283921315906656,
-6.04912696179709));
#146112=CARTESIAN_POINT('Ctrl Pts',(6.29856863119255,-0.516830885580026,
-6.08684879763255));
#146113=CARTESIAN_POINT('Ctrl Pts',(6.39319307134218,-0.826237684586883,
-6.18532440469951));
#146114=CARTESIAN_POINT('Ctrl Pts',(6.4269565633907,-0.915473690032379,
-6.22046380962379));
#146115=CARTESIAN_POINT('Ctrl Pts',(6.46559354776685,-1.00000000012986,
-6.26067888295109));
#146116=CARTESIAN_POINT('Origin',(1.11022302462516E-15,0.999999999999982,
2.22044604925031E-15));
#146117=CARTESIAN_POINT('Origin',(1.11022302462516E-15,-1.77635683940025E-14,
2.22044604925031E-15));
#146118=CARTESIAN_POINT('',(5.964297039,-1.00000000000002,-6.739967421));
#146119=CARTESIAN_POINT('',(5.964297039,0.999999999999982,-6.73996742));
#146120=CARTESIAN_POINT('Ctrl Pts',(5.96429703935934,-1.00000000016049,
-6.73996742032238));
#146121=CARTESIAN_POINT('Ctrl Pts',(5.91379949005691,-0.888963444794065,
-6.68689359451439));
#146122=CARTESIAN_POINT('Ctrl Pts',(5.87174625183969,-0.769956469688926,
-6.64268951092948));
#146123=CARTESIAN_POINT('Ctrl Pts',(5.78113339231567,-0.42405172295009,
-6.54743717254365));
#146124=CARTESIAN_POINT('Ctrl Pts',(5.75354546207986,-0.188791058808368,
-6.51843116733989));
#146125=CARTESIAN_POINT('Ctrl Pts',(5.76207821484305,0.283921315909877,
-6.52740186607613));
#146126=CARTESIAN_POINT('Ctrl Pts',(5.79813553392257,0.516830885584594,
-6.56531182940824));
#146127=CARTESIAN_POINT('Ctrl Pts',(5.89226667310739,0.826237684479476,
-6.66425908042156));
#146128=CARTESIAN_POINT('Ctrl Pts',(5.92585590159545,0.915473689821208,
-6.69956509827456));
#146129=CARTESIAN_POINT('Ctrl Pts',(5.96429703920789,0.999999999827432,
-6.7399674201632));
#146130=CARTESIAN_POINT('',(5.87836204,-1.00000000000002,-6.815046568));
#146131=CARTESIAN_POINT('Origin',(1.11022302462516E-15,-1.00000000000002,
2.22044604925031E-15));
#146132=CARTESIAN_POINT('',(5.87836204,0.999999999999982,-6.815046568));
#146133=CARTESIAN_POINT('Ctrl Pts',(5.87836203971057,0.999999999954793,
-6.81504656831974));
#146134=CARTESIAN_POINT('Ctrl Pts',(5.8325469956454,0.888963444648912,-6.75788176096771));
#146135=CARTESIAN_POINT('Ctrl Pts',(5.79438791306315,0.769956469615795,
-6.71027545612482));
#146136=CARTESIAN_POINT('Ctrl Pts',(5.7121608910693,0.424051722953685,-6.60769663216305));
#146137=CARTESIAN_POINT('Ctrl Pts',(5.68712061508326,0.188791058808652,
-6.57646480847093));
#146138=CARTESIAN_POINT('Ctrl Pts',(5.69486474759318,-0.283921315914366,
-6.58612450397438));
#146139=CARTESIAN_POINT('Ctrl Pts',(5.72759152504514,-0.516830885590948,
-6.62694427389891));
#146140=CARTESIAN_POINT('Ctrl Pts',(5.81300774969049,-0.826237684531224,
-6.73350551647852));
#146141=CARTESIAN_POINT('Ctrl Pts',(5.84348544786606,-0.915473689913203,
-6.77152999653492));
#146142=CARTESIAN_POINT('Ctrl Pts',(5.87836203971057,-0.999999999954828,
-6.81504656831974));
#146143=CARTESIAN_POINT('Origin',(1.11022302462516E-15,0.999999999999982,
2.22044604925031E-15));
#146144=CARTESIAN_POINT('Origin',(1.11022302462516E-15,-1.77635683940025E-14,
2.22044604925031E-15));
#146145=CARTESIAN_POINT('',(5.336120511,-1.00000000000002,-7.247469758));
#146146=CARTESIAN_POINT('',(5.33612051,0.999999999999982,-7.247469758));
#146147=CARTESIAN_POINT('Ctrl Pts',(5.3361205102212,-1.00000000007198,-7.24746975847874));
#146148=CARTESIAN_POINT('Ctrl Pts',(5.29058375025361,-0.888963444727195,
-7.19008302691189));
#146149=CARTESIAN_POINT('Ctrl Pts',(5.25266222949664,-0.769956469647748,
-7.14228727279495));
#146150=CARTESIAN_POINT('Ctrl Pts',(5.17095250443963,-0.42405172294289,
-7.03929591826978));
#146151=CARTESIAN_POINT('Ctrl Pts',(5.14607571334355,-0.18879105880775,
-7.00793371972911));
#146152=CARTESIAN_POINT('Ctrl Pts',(5.15376998852219,0.28392131590102,-7.01763317512497));
#146153=CARTESIAN_POINT('Ctrl Pts',(5.18628392854452,0.516830885572041,
-7.05862267723458));
#146154=CARTESIAN_POINT('Ctrl Pts',(5.27116656029511,0.826237684454488,
-7.16560944591632));
#146155=CARTESIAN_POINT('Ctrl Pts',(5.30145576140191,0.915473689787592,
-7.20378424732816));
#146156=CARTESIAN_POINT('Ctrl Pts',(5.33612051010402,0.999999999786219,
-7.24746975833107));
#146157=CARTESIAN_POINT('',(5.243801419,-1.00000000000002,-7.314543504));
#146158=CARTESIAN_POINT('Origin',(1.11022302462516E-15,-1.00000000000002,
2.22044604925031E-15));
#146159=CARTESIAN_POINT('',(5.243801419,0.999999999999982,-7.314543505));
#146160=CARTESIAN_POINT('Ctrl Pts',(5.24380141936078,1.00000000025759,-7.31454350429201));
#146161=CARTESIAN_POINT('Ctrl Pts',(5.20329502701867,0.888963444859878,
-7.25350199664624));
#146162=CARTESIAN_POINT('Ctrl Pts',(5.16955695795366,0.769956469717499,
-7.20266678690974));
#146163=CARTESIAN_POINT('Ctrl Pts',(5.09685605273472,0.424051722943023,
-7.09313014161181));
#146164=CARTESIAN_POINT('Ctrl Pts',(5.07471618065862,0.188791058807761,
-7.05977945500722));
#146165=CARTESIAN_POINT('Ctrl Pts',(5.08156324912866,-0.283921315901189,
-7.07009444210696));
#146166=CARTESIAN_POINT('Ctrl Pts',(5.11049922219244,-0.516830885572283,
-7.11368348937601));
#146167=CARTESIAN_POINT('Ctrl Pts',(5.18601950998405,-0.826237684487119,
-7.22747239912402));
#146168=CARTESIAN_POINT('Ctrl Pts',(5.21296602575133,-0.915473689849889,
-7.26807580361716));
#146169=CARTESIAN_POINT('Ctrl Pts',(5.24380141922105,-0.999999999874605,
-7.31454350408144));
#146170=CARTESIAN_POINT('Origin',(1.11022302462516E-15,0.999999999999982,
2.22044604925031E-15));
#146171=CARTESIAN_POINT('Origin',(1.11022302462516E-15,-1.77635683940025E-14,
2.22044604925031E-15));
#146172=CARTESIAN_POINT('',(4.664980679,-1.00000000000002,-7.69661973));
#146173=CARTESIAN_POINT('',(4.664980679,0.999999999999982,-7.69661973));
#146174=CARTESIAN_POINT('Ctrl Pts',(4.6649806790278,-1.00000000012153,-7.69661972976142));
#146175=CARTESIAN_POINT('Ctrl Pts',(4.62477134369037,-0.888963444769274,
-7.6353821365611));
#146176=CARTESIAN_POINT('Ctrl Pts',(4.59128686224838,-0.769956469681019,
-7.58437953514421));
#146177=CARTESIAN_POINT('Ctrl Pts',(4.51913815048226,-0.424051722956118,
-7.47447839016348));
#146178=CARTESIAN_POINT('Ctrl Pts',(4.49717279187256,-0.188791058808884,
-7.44101250822752));
#146179=CARTESIAN_POINT('Ctrl Pts',(4.50396663967298,0.283921315917304,
-7.45136262598658));
#146180=CARTESIAN_POINT('Ctrl Pts',(4.53267541744313,0.516830885595124,
-7.49510164355729));
#146181=CARTESIAN_POINT('Ctrl Pts',(4.60762611656944,0.826237684595681,
-7.60926653553599));
#146182=CARTESIAN_POINT('Ctrl Pts',(4.6343714194336,0.915473690032042,-7.65000275956128));
#146183=CARTESIAN_POINT('Ctrl Pts',(4.6649806790278,1.0000000001215,-7.69661972976142));
#146184=CARTESIAN_POINT('',(4.567020791,-1.00000000000002,-7.755148038));
#146185=CARTESIAN_POINT('Origin',(1.11022302462516E-15,-1.00000000000002,
2.22044604925031E-15));
#146186=CARTESIAN_POINT('',(4.56702079017615,1.00000000014985,-7.75514803858119));
#146187=CARTESIAN_POINT('Ctrl Pts',(4.56702079103465,1.0000000001046,-7.7551480381945));
#146188=CARTESIAN_POINT('Ctrl Pts',(4.53214918409692,0.888963444751377,
-7.69072130073945));
#146189=CARTESIAN_POINT('Ctrl Pts',(4.50310376766113,0.769956469661911,
-7.63706648144992));
#146190=CARTESIAN_POINT('Ctrl Pts',(4.44051432410008,0.424051722944636,
-7.5214539396054));
#146191=CARTESIAN_POINT('Ctrl Pts',(4.42145311313639,0.188791058807902,
-7.48625291022913));
#146192=CARTESIAN_POINT('Ctrl Pts',(4.42734798900763,-0.283921315903169,
-7.49714013870893));
#146193=CARTESIAN_POINT('Ctrl Pts',(4.45226018228089,-0.516830885575091,
-7.54314750991511));
#146194=CARTESIAN_POINT('Ctrl Pts',(4.5172764883787,-0.826237684515359,
-7.66324792537742));
#146195=CARTESIAN_POINT('Ctrl Pts',(4.54047486428761,-0.915473689900841,
-7.7061033395637));
#146196=CARTESIAN_POINT('Ctrl Pts',(4.56702079098469,-0.999999999945535,
-7.75514803810218));
#146197=CARTESIAN_POINT('Origin',(1.11022302462516E-15,0.999999999999982,
2.22044604925031E-15));
#146198=CARTESIAN_POINT('Origin',(1.11022302462516E-15,-1.77635683940025E-14,
2.22044604925031E-15));
#146199=CARTESIAN_POINT('',(3.956281164,-1.00000000000002,-8.083801046));
#146200=CARTESIAN_POINT('',(3.956281165,0.999999999999982,-8.083801046));
#146201=CARTESIAN_POINT('Ctrl Pts',(3.95628116468507,-1.00000000001549,
-8.08380104560689));
#146202=CARTESIAN_POINT('Ctrl Pts',(3.92172299585936,-0.888963444693514,
-8.01920563994906));
#146203=CARTESIAN_POINT('Ctrl Pts',(3.89294515105064,-0.769956469641267,
-7.96540683425602));
#146204=CARTESIAN_POINT('Ctrl Pts',(3.83093835147929,-0.424051722956149,
-7.84948075832601));
#146205=CARTESIAN_POINT('Ctrl Pts',(3.81206127747473,-0.188791058808902,
-7.81418064062605));
#146206=CARTESIAN_POINT('Ctrl Pts',(3.81789999783811,0.283921315917307,
-7.82509808767561));
#146207=CARTESIAN_POINT('Ctrl Pts',(3.8425724672014,0.516830885595135,-7.87123445981978));
#146208=CARTESIAN_POINT('Ctrl Pts',(3.90698777483689,0.826237684636356,
-7.99165828639557));
#146209=CARTESIAN_POINT('Ctrl Pts',(3.92997384201674,0.91547369011003,-8.0346279488464));
#146210=CARTESIAN_POINT('Ctrl Pts',(3.95628116475256,1.0000000002323,-8.08380104573303));
#146211=CARTESIAN_POINT('',(3.853469197,-1.00000000000002,-8.133312679));
#146212=CARTESIAN_POINT('Origin',(1.11022302462516E-15,-1.00000000000002,
2.22044604925031E-15));
#146213=CARTESIAN_POINT('',(3.853469197,0.999999999999982,-8.13331268));
#146214=CARTESIAN_POINT('Ctrl Pts',(3.85346919706807,1.0000000001062,-8.13331267979544));
#146215=CARTESIAN_POINT('Ctrl Pts',(3.82451314113869,0.888963444756582,
-8.06601943872399));
#146216=CARTESIAN_POINT('Ctrl Pts',(3.80039423388955,0.769956469671447,
-8.00997700692796));
#146217=CARTESIAN_POINT('Ctrl Pts',(3.74842018528737,0.424051722952665,
-7.88921941276124));
#146218=CARTESIAN_POINT('Ctrl Pts',(3.73259110507323,0.18879105880854,-7.85245145861414));
#146219=CARTESIAN_POINT('Ctrl Pts',(3.73748632627965,-0.283921315913163,
-7.86382327090975));
#146220=CARTESIAN_POINT('Ctrl Pts',(3.758174161464,-0.516830885589227,-7.91187854173883));
#146221=CARTESIAN_POINT('Ctrl Pts',(3.81216301286461,-0.82623768443046,
-8.0373234849023));
#146222=CARTESIAN_POINT('Ctrl Pts',(3.83142646923125,-0.91547368972195,
-8.08208586210271));
#146223=CARTESIAN_POINT('Ctrl Pts',(3.85346919695796,-0.999999999683993,
-8.13331267953954));
#146224=CARTESIAN_POINT('Origin',(1.11022302462516E-15,0.999999999999982,
2.22044604925031E-15));
#146225=CARTESIAN_POINT('Origin',(1.11022302462516E-15,-1.77635683940025E-14,
2.22044604925031E-15));
#146226=CARTESIAN_POINT('',(3.215728,-1.00000000000002,-8.405896349));
#146227=CARTESIAN_POINT('',(3.215728,0.999999999999982,-8.405896349));
#146228=CARTESIAN_POINT('Ctrl Pts',(3.21572799910164,-1.00000000004898,
-8.40589634930077));
#146229=CARTESIAN_POINT('Ctrl Pts',(3.18709923874645,-0.888963444711018,
-8.33846321539938));
#146230=CARTESIAN_POINT('Ctrl Pts',(3.16325973277762,-0.769956469639689,
-8.28230136177404));
#146231=CARTESIAN_POINT('Ctrl Pts',(3.11189408755156,-0.424051722943416,
-8.16128372353288));
#146232=CARTESIAN_POINT('Ctrl Pts',(3.09625728521347,-0.188791058807824,
-8.12443358587799));
#146233=CARTESIAN_POINT('Ctrl Pts',(3.10109386820783,0.283921315901602,
-8.13583046134637));
#146234=CARTESIAN_POINT('Ctrl Pts',(3.12153138099901,0.516830885572883,
-8.18399272510011));
#146235=CARTESIAN_POINT('Ctrl Pts',(3.17489266307679,0.826237684551582,
-8.30970590433157));
#146236=CARTESIAN_POINT('Ctrl Pts',(3.19393442429636,0.915473689972814,
-8.35456303867882));
#146237=CARTESIAN_POINT('Ctrl Pts',(3.21572799910164,1.00000000004895,-8.40589634930077));
#146238=CARTESIAN_POINT('',(3.108891736,-1.00000000000002,-8.445992669));
#146239=CARTESIAN_POINT('Origin',(1.11022302462516E-15,-1.00000000000002,
2.22044604925031E-15));
#146240=CARTESIAN_POINT('',(3.108891736,0.999999999999982,-8.44599267));
#146241=CARTESIAN_POINT('Ctrl Pts',(3.10889173624931,1.00000000023755,-8.44599266953941));
#146242=CARTESIAN_POINT('Ctrl Pts',(3.08608436854417,0.888963444846535,
-8.37637473037447));
#146243=CARTESIAN_POINT('Ctrl Pts',(3.06708616180808,0.76995646971212,-8.31839590671147));
#146244=CARTESIAN_POINT('Ctrl Pts',(3.0261459728075,0.424051722944944,-8.19346552927423));
#146245=CARTESIAN_POINT('Ctrl Pts',(3.01367646984111,0.188791058807912,
-8.15542668428225));
#146246=CARTESIAN_POINT('Ctrl Pts',(3.01753262292283,-0.283921315903587,
-8.16719152125182));
#146247=CARTESIAN_POINT('Ctrl Pts',(3.03382953366586,-0.516830885575674,
-8.21690777894712));
#146248=CARTESIAN_POINT('Ctrl Pts',(3.07635624373366,-0.826237684462671,
-8.34668724102495));
#146249=CARTESIAN_POINT('Ctrl Pts',(3.09152968251005,-0.915473689799155,
-8.39299618100886));
#146250=CARTESIAN_POINT('Ctrl Pts',(3.10889173615958,-0.999999999800758,
-8.44599266926553));
#146251=CARTESIAN_POINT('Origin',(1.11022302462516E-15,0.999999999999982,
2.22044604925031E-15));
#146252=CARTESIAN_POINT('Origin',(1.11022302462516E-15,-1.77635683940025E-14,
2.22044604925031E-15));
#146253=CARTESIAN_POINT('',(2.449283685,-1.00000000000002,-8.660312317));
#146254=CARTESIAN_POINT('',(2.449283685,0.999999999999982,-8.660312317));
#146255=CARTESIAN_POINT('Ctrl Pts',(2.44928368492003,-0.999999999970373,
-8.66031231707298));
#146256=CARTESIAN_POINT('Ctrl Pts',(2.42681483511176,-0.88896344465865,
-8.5905843868621));
#146257=CARTESIAN_POINT('Ctrl Pts',(2.40810560977552,-0.76995646961857,
-8.53251166751632));
#146258=CARTESIAN_POINT('Ctrl Pts',(2.36779468507835,-0.42405172295094,
-8.40737682975315));
#146259=CARTESIAN_POINT('Ctrl Pts',(2.35552405280636,-0.188791058808441,
-8.36927336775524));
#146260=CARTESIAN_POINT('Ctrl Pts',(2.35931955709161,0.283921315910929,
-8.38105791071449));
#146261=CARTESIAN_POINT('Ctrl Pts',(2.37535756239453,0.516830885586086,
-8.4308582918873));
#146262=CARTESIAN_POINT('Ctrl Pts',(2.41723518504276,0.826237684533091,
-8.56084865527989));
#146263=CARTESIAN_POINT('Ctrl Pts',(2.4321793271706,0.915473689922331,-8.6072320982976));
#146264=CARTESIAN_POINT('Ctrl Pts',(2.44928368492003,0.999999999970337,
-8.66031231707298));
#146265=CARTESIAN_POINT('',(2.339283306,-1.00000000000002,-8.690670493));
#146266=CARTESIAN_POINT('Origin',(1.11022302462516E-15,-1.00000000000002,
2.22044604925031E-15));
#146267=CARTESIAN_POINT('',(2.339283305,0.999999999999982,-8.690670493));
#146268=CARTESIAN_POINT('Ctrl Pts',(2.33928330561053,1.00000000001403,-8.69067049283723));
#146269=CARTESIAN_POINT('Ctrl Pts',(2.322808257611,0.888963444688627,-8.61928837841982));
#146270=CARTESIAN_POINT('Ctrl Pts',(2.30908371374843,0.769956469632264,
-8.5598399743875));
#146271=CARTESIAN_POINT('Ctrl Pts',(2.27950701057719,0.424051722948505,
-8.4317426797122));
#146272=CARTESIAN_POINT('Ctrl Pts',(2.27049748192907,0.188791058808199,
-8.39273921030103));
#146273=CARTESIAN_POINT('Ctrl Pts',(2.27328351942049,-0.283921315908009,
-8.40480234839289));
#146274=CARTESIAN_POINT('Ctrl Pts',(2.28505829262577,-0.516830885581933,
-8.45577930686427));
#146275=CARTESIAN_POINT('Ctrl Pts',(2.31578046142091,-0.826237684583821,
-8.58884837992317));
#146276=CARTESIAN_POINT('Ctrl Pts',(2.32674171504669,-0.91547369002434,
-8.63633103035858));
#146277=CARTESIAN_POINT('Ctrl Pts',(2.33928330562587,-1.00000000011744,
-8.69067049290369));
#146278=CARTESIAN_POINT('Origin',(1.11022302462516E-15,0.999999999999982,
2.22044604925031E-15));
#146279=CARTESIAN_POINT('Origin',(1.11022302462516E-15,-1.77635683940025E-14,
2.22044604925031E-15));
#146280=CARTESIAN_POINT('',(1.663119178,-1.00000000000002,-8.845000543));
#146281=CARTESIAN_POINT('',(1.663119178,0.999999999999982,-8.845000543));
#146282=CARTESIAN_POINT('Ctrl Pts',(1.66311917835389,-1.00000000017414,
-8.84500054264957));
#146283=CARTESIAN_POINT('Ctrl Pts',(1.64699114496605,-0.888963444802729,
-8.77353922436293));
#146284=CARTESIAN_POINT('Ctrl Pts',(1.6335628358678,-0.769956469691643,
-8.71402320664169));
#146285=CARTESIAN_POINT('Ctrl Pts',(1.60463119142803,-0.424051722947924,
-8.58577868149685));
#146286=CARTESIAN_POINT('Ctrl Pts',(1.5958255251009,-0.188791058808183,
-8.54672868184126));
#146287=CARTESIAN_POINT('Ctrl Pts',(1.59854939151922,0.28392131590721,-8.55880601007474));
#146288=CARTESIAN_POINT('Ctrl Pts',(1.61005876079406,0.516830885580814,
-8.60984354526128));
#146289=CARTESIAN_POINT('Ctrl Pts',(1.64011555016049,0.826237684603748,
-8.74306448684239));
#146290=CARTESIAN_POINT('Ctrl Pts',(1.65084175181585,0.915473690063816,
-8.79060078636947));
#146291=CARTESIAN_POINT('Ctrl Pts',(1.66311917835389,1.00000000017411,-8.84500054264957));
#146292=CARTESIAN_POINT('',(1.550840341,-1.00000000000002,-8.865376147));
#146293=CARTESIAN_POINT('Origin',(1.11022302462516E-15,-1.00000000000002,
2.22044604925031E-15));
#146294=CARTESIAN_POINT('',(1.550840341,0.999999999999982,-8.865376147));
#146295=CARTESIAN_POINT('Ctrl Pts',(1.55084034140624,0.999999999808245,
-8.86537614723733));
#146296=CARTESIAN_POINT('Ctrl Pts',(1.54083026051303,0.888963444542273,
-8.7928045843712));
#146297=CARTESIAN_POINT('Ctrl Pts',(1.53248988148326,0.769956469556595,
-8.73236524355606));
#146298=CARTESIAN_POINT('Ctrl Pts',(1.51451479838375,0.424051722949861,
-8.60213239572781));
#146299=CARTESIAN_POINT('Ctrl Pts',(1.50903778348876,0.188791058808314,
-8.56247833489648));
#146300=CARTESIAN_POINT('Ctrl Pts',(1.51073127385162,-0.283921315909679,
-8.5747426488163));
#146301=CARTESIAN_POINT('Ctrl Pts',(1.51788910595866,-0.516830885584297,
-8.62656987157201));
#146302=CARTESIAN_POINT('Ctrl Pts',(1.53655937659348,-0.826237684472212,
-8.76185716159183));
#146303=CARTESIAN_POINT('Ctrl Pts',(1.54322019145936,-0.915473689807618,
-8.81013121996665));
#146304=CARTESIAN_POINT('Ctrl Pts',(1.55084034140624,-0.99999999980828,
-8.86537614723733));
#146305=CARTESIAN_POINT('Origin',(1.11022302462516E-15,0.999999999999982,
2.22044604925031E-15));
#146306=CARTESIAN_POINT('Origin',(1.11022302462516E-15,-1.77635683940025E-14,
2.22044604925031E-15));
#146307=CARTESIAN_POINT('',(0.863564213,-1.00000000000002,-8.958474025));
#146308=CARTESIAN_POINT('',(0.863564213,0.999999999999982,-8.958474025));
#146309=CARTESIAN_POINT('Ctrl Pts',(0.863564213524502,-1.00000000018892,
-8.95847402464141));
#146310=CARTESIAN_POINT('Ctrl Pts',(0.853906850043781,-0.888963444813415,
-8.88585468284159));
#146311=CARTESIAN_POINT('Ctrl Pts',(0.845867574068788,-0.769956469697459,
-8.82537455475955));
#146312=CARTESIAN_POINT('Ctrl Pts',(0.828548150532186,-0.424051722948203,
-8.69505289175402));
#146313=CARTESIAN_POINT('Ctrl Pts',(0.823278348211899,-0.188791058808255,
-8.65537076207234));
#146314=CARTESIAN_POINT('Ctrl Pts',(0.824908645788199,0.283921315907445,
-8.6676436360364));
#146315=CARTESIAN_POINT('Ctrl Pts',(0.831796712342162,0.516830885581175,
-8.71950740101901));
#146316=CARTESIAN_POINT('Ctrl Pts',(0.849790668772453,0.826237684609472,
-8.8548863040852));
#146317=CARTESIAN_POINT('Ctrl Pts',(0.856212568854875,0.915473690074354,
-8.90319272575271));
#146318=CARTESIAN_POINT('Ctrl Pts',(0.863564213524502,1.00000000018889,
-8.95847402464141));
#146319=CARTESIAN_POINT('',(0.749910923000001,-1.00000000000002,-8.968703006));
#146320=CARTESIAN_POINT('Origin',(1.11022302462516E-15,-1.00000000000002,
2.22044604925031E-15));
#146321=CARTESIAN_POINT('',(0.749910923000001,0.999999999999982,-8.968703006));
#146322=CARTESIAN_POINT('Ctrl Pts',(0.749910923421742,1.0000000000954,-8.96870300583525));
#146323=CARTESIAN_POINT('Ctrl Pts',(0.746446404937194,0.888963444745312,
-8.89552629792414));
#146324=CARTESIAN_POINT('Ctrl Pts',(0.743557342583251,0.76995646965958,
-8.83458264224673));
#146325=CARTESIAN_POINT('Ctrl Pts',(0.737328604408766,0.424051722945632,
-8.70326279950605));
#146326=CARTESIAN_POINT('Ctrl Pts',(0.735428200989169,0.188791058807976,
-8.66327741843499));
#146327=CARTESIAN_POINT('Ctrl Pts',(0.736015509228912,-0.283921315904421,
-8.67564416313782));
#146328=CARTESIAN_POINT('Ctrl Pts',(0.738498769557774,-0.516830885576862,
-8.72790436785553));
#146329=CARTESIAN_POINT('Ctrl Pts',(0.744966819940245,-0.826237684571764,
-8.86432062122607));
#146330=CARTESIAN_POINT('Ctrl Pts',(0.747273567077169,-0.91547369000699,
-8.91299741334236));
#146331=CARTESIAN_POINT('Ctrl Pts',(0.749910923421742,-1.00000000009543,
-8.96870300583525));
#146332=CARTESIAN_POINT('Origin',(1.11022302462516E-15,0.999999999999982,
2.22044604925031E-15));
#146333=CARTESIAN_POINT('Origin',(1.11022302462516E-15,-1.77635683940025E-14,
2.22044604925031E-15));
#146334=CARTESIAN_POINT('',(0.057056338,-1.00000000000002,-8.999819141));
#146335=CARTESIAN_POINT('',(0.057056338,0.999999999999982,-8.999819141));
#146336=CARTESIAN_POINT('Ctrl Pts',(0.0570563383389186,-0.999999999933197,
-8.99981914108697));
#146337=CARTESIAN_POINT('Ctrl Pts',(0.0539474002202264,-0.888963444633974,
-8.92662646409639));
#146338=CARTESIAN_POINT('Ctrl Pts',(0.0513618849266559,-0.76995646960878,
-8.86566917614543));
#146339=CARTESIAN_POINT('Ctrl Pts',(0.0457941281782637,-0.424051722954681,
-8.73431964871831));
#146340=CARTESIAN_POINT('Ctrl Pts',(0.0441026192351812,-0.188791058808771,
-8.69432488618503));
#146341=CARTESIAN_POINT('Ctrl Pts',(0.0446262217656046,0.283921315915514,
-8.70669449191622));
#146342=CARTESIAN_POINT('Ctrl Pts',(0.0468375269099042,0.516830885592592,
-8.75896691015616));
#146343=CARTESIAN_POINT('Ctrl Pts',(0.0526237735737155,0.82623768452456,
-8.89541378333879));
#146344=CARTESIAN_POINT('Ctrl Pts',(0.054689666691092,0.915473689898555,
-8.94410139218079));
#146345=CARTESIAN_POINT('Ctrl Pts',(0.0570563383389185,0.999999999933161,
-8.99981914108697));
#146346=CARTESIAN_POINT('',(-0.0570563369999999,-1.00000000000002,-8.999819141));
#146347=CARTESIAN_POINT('Origin',(1.11022302462516E-15,-1.00000000000002,
2.22044604925031E-15));
#146348=CARTESIAN_POINT('',(-0.0570563369999999,0.999999999999982,-8.999819141));
#146349=CARTESIAN_POINT('Ctrl Pts',(-0.0570563367490442,0.999999999940042,
-8.99981914110159));
#146350=CARTESIAN_POINT('Ctrl Pts',(-0.0539473986136921,0.888963444636815,
-8.92662646410728));
#146351=CARTESIAN_POINT('Ctrl Pts',(-0.0513618833063578,0.769956469606837,
-8.86566917615349));
#146352=CARTESIAN_POINT('Ctrl Pts',(-0.0457941265286543,0.424051722950587,
-8.73431964872652));
#146353=CARTESIAN_POINT('Ctrl Pts',(-0.0441026175767645,0.188791058808359,
-8.69432488619385));
#146354=CARTESIAN_POINT('Ctrl Pts',(-0.0446262201098946,-0.283921315910611,
-8.70669449192419));
#146355=CARTESIAN_POINT('Ctrl Pts',(-0.0468375252657083,-0.51683088558561,
-8.75896691016323));
#146356=CARTESIAN_POINT('Ctrl Pts',(-0.0526237719600614,-0.826237684521612,
-8.89541378334643));
#146357=CARTESIAN_POINT('Ctrl Pts',(-0.0546896650884917,-0.91547368990086,
-8.94410139219154));
#146358=CARTESIAN_POINT('Ctrl Pts',(-0.0570563367490442,-0.999999999940079,
-8.99981914110159));
#146359=CARTESIAN_POINT('Origin',(1.11022302462516E-15,0.999999999999982,
2.22044604925031E-15));
#146360=CARTESIAN_POINT('Origin',(1.11022302462516E-15,-1.77635683940025E-14,
2.22044604925031E-15));
#146361=CARTESIAN_POINT('',(-0.749910922999999,-1.00000000000002,-8.968703006));
#146362=CARTESIAN_POINT('',(-0.749910922999999,0.999999999999982,-8.968703006));
#146363=CARTESIAN_POINT('Ctrl Pts',(-0.749910923031043,-1.00000000008893,
-8.96870300586362));
#146364=CARTESIAN_POINT('Ctrl Pts',(-0.746446404541414,-0.888963444741282,
-8.89552629795534));
#146365=CARTESIAN_POINT('Ctrl Pts',(-0.743557342183263,-0.769956469658455,
-8.83458264228013));
#146366=CARTESIAN_POINT('Ctrl Pts',(-0.737328603999571,-0.424051722946837,
-8.70326279954085));
#146367=CARTESIAN_POINT('Ctrl Pts',(-0.735428200577178,-0.188791058808127,
-8.66327741846985));
#146368=CARTESIAN_POINT('Ctrl Pts',(-0.736015508817798,0.28392131590579,
-8.67564416317284));
#146369=CARTESIAN_POINT('Ctrl Pts',(-0.738498769150314,0.516830885578821,
-8.72790436789049));
#146370=CARTESIAN_POINT('Ctrl Pts',(-0.744966819542354,0.826237684570914,
-8.86432062125932));
#146371=CARTESIAN_POINT('Ctrl Pts',(-0.747273566682627,0.915473690003112,
-8.91299741337342));
#146372=CARTESIAN_POINT('Ctrl Pts',(-0.749910923031043,1.00000000008889,
-8.96870300586362));
#146373=CARTESIAN_POINT('',(-0.863564211999999,-1.00000000000002,-8.958474025));
#146374=CARTESIAN_POINT('Origin',(1.11022302462516E-15,-1.00000000000002,
2.22044604925031E-15));
#146375=CARTESIAN_POINT('',(-0.863564212999999,0.999999999999982,-8.958474025));
#146376=CARTESIAN_POINT('Ctrl Pts',(-0.863564212376334,1.00000000020806,
-8.95847402476479));
#146377=CARTESIAN_POINT('Ctrl Pts',(-0.85390684889901,0.888963444826714,
-8.88585468295841));
#146378=CARTESIAN_POINT('Ctrl Pts',(-0.845867572926913,0.76995646970382,
-8.82537455487132));
#146379=CARTESIAN_POINT('Ctrl Pts',(-0.82854814939751,0.424051722947429,
-8.69505289186206));
#146380=CARTESIAN_POINT('Ctrl Pts',(-0.823278347079534,0.188791058808129,
-8.65537076218012));
#146381=CARTESIAN_POINT('Ctrl Pts',(-0.824908644655102,-0.283921315906636,
-8.66764363614415));
#146382=CARTESIAN_POINT('Ctrl Pts',(-0.831796711206042,-0.516830885579999,
-8.7195074011271));
#146383=CARTESIAN_POINT('Ctrl Pts',(-0.849790667627615,-0.826237684593336,
-8.8548863041878));
#146384=CARTESIAN_POINT('Ctrl Pts',(-0.856212567706076,-0.915473690044782,
-8.90319272584691));
#146385=CARTESIAN_POINT('Ctrl Pts',(-0.863564212371063,-1.00000000014749,
-8.95847402472516));
#146386=CARTESIAN_POINT('Origin',(1.11022302462516E-15,0.999999999999982,
2.22044604925031E-15));
#146387=CARTESIAN_POINT('Origin',(1.11022302462516E-15,-1.77635683940025E-14,
2.22044604925031E-15));
#146388=CARTESIAN_POINT('',(-1.550840341,-1.00000000000002,-8.865376147));
#146389=CARTESIAN_POINT('',(-1.550840341,0.999999999999982,-8.865376147));
#146390=CARTESIAN_POINT('Ctrl Pts',(-1.55084034103818,-0.999999999802089,
-8.86537614729757));
#146391=CARTESIAN_POINT('Ctrl Pts',(-1.54083026013964,-0.888963444538492,
-8.79280458443473));
#146392=CARTESIAN_POINT('Ctrl Pts',(-1.53248988110543,-0.769956469555648,
-8.73236524362217));
#146393=CARTESIAN_POINT('Ctrl Pts',(-1.51451479799595,-0.424051722951105,
-8.60213239579622));
#146394=CARTESIAN_POINT('Ctrl Pts',(-1.50903778309791,-0.188791058808463,
-8.56247833496524));
#146395=CARTESIAN_POINT('Ctrl Pts',(-1.51073127346174,0.283921315911108,
-8.57474264888515));
#146396=CARTESIAN_POINT('Ctrl Pts',(-1.51788910557278,0.516830885586346,
-8.62656987164042));
#146397=CARTESIAN_POINT('Ctrl Pts',(-1.53655937621794,0.826237684471543,
-8.76185716165758));
#146398=CARTESIAN_POINT('Ctrl Pts',(-1.54322019108732,0.915473689803992,
-8.81013122002992));
#146399=CARTESIAN_POINT('Ctrl Pts',(-1.55084034103818,0.999999999802054,
-8.86537614729757));
#146400=CARTESIAN_POINT('',(-1.663119178,-1.00000000000002,-8.845000543));
#146401=CARTESIAN_POINT('Origin',(1.11022302462516E-15,-1.00000000000002,
2.22044604925031E-15));
#146402=CARTESIAN_POINT('',(-1.663119178,0.999999999999982,-8.845000543));
#146403=CARTESIAN_POINT('Ctrl Pts',(-1.66311917779156,1.00000000018363,
-8.84500054276169));
#146404=CARTESIAN_POINT('Ctrl Pts',(-1.64699114441794,0.888963444810215,
-8.77353922446984));
#146405=CARTESIAN_POINT('Ctrl Pts',(-1.63356283533152,0.769956469696761,
-8.71402320674444));
#146406=CARTESIAN_POINT('Ctrl Pts',(-1.60463119091762,0.424051722949323,
-8.58577868159241));
#146407=CARTESIAN_POINT('Ctrl Pts',(-1.5958255245984,0.188791058808294,
-8.54672868193495));
#146408=CARTESIAN_POINT('Ctrl Pts',(-1.59854939101432,-0.283921315908962,
-8.55880601016923));
#146409=CARTESIAN_POINT('Ctrl Pts',(-1.61005876027881,-0.516830885583298,
-8.60984354535825));
#146410=CARTESIAN_POINT('Ctrl Pts',(-1.64011554961833,-0.826237684609204,
-8.74306448694674));
#146411=CARTESIAN_POINT('Ctrl Pts',(-1.65084175126428,-0.915473690071452,
-8.79060078647737));
#146412=CARTESIAN_POINT('Ctrl Pts',(-1.66311917779156,-1.00000000018366,
-8.84500054276169));
#146413=CARTESIAN_POINT('Origin',(1.11022302462516E-15,0.999999999999982,
2.22044604925031E-15));
#146414=CARTESIAN_POINT('Origin',(1.11022302462516E-15,-1.77635683940025E-14,
2.22044604925031E-15));
#146415=CARTESIAN_POINT('',(-2.339283305,-1.00000000000002,-8.690670493));
#146416=CARTESIAN_POINT('',(-2.339283305,0.999999999999982,-8.690670493));
#146417=CARTESIAN_POINT('Ctrl Pts',(-2.33928330447186,-0.999999999994548,
-8.6906704931304));
#146418=CARTESIAN_POINT('Ctrl Pts',(-2.32280825646114,-0.888963444676296,
-8.61928837872337));
#146419=CARTESIAN_POINT('Ctrl Pts',(-2.30908371258921,-0.769956469628456,
-8.55983997469919));
#146420=CARTESIAN_POINT('Ctrl Pts',(-2.27950700939569,-0.424051722951681,
-8.43174268003197));
#146421=CARTESIAN_POINT('Ctrl Pts',(-2.27049748074064,-0.188791058808523,
-8.39273921062221));
#146422=CARTESIAN_POINT('Ctrl Pts',(-2.27328351823432,0.2839213159118,-8.40480234871414));
#146423=CARTESIAN_POINT('Ctrl Pts',(-2.2850582914487,0.516830885587333,
-8.45577930718373));
#146424=CARTESIAN_POINT('Ctrl Pts',(-2.31578046026309,0.82623768454295,
-8.58884838021716));
#146425=CARTESIAN_POINT('Ctrl Pts',(-2.32674171389091,0.915473689939805,
-8.63633103062244));
#146426=CARTESIAN_POINT('Ctrl Pts',(-2.33928330447186,0.999999999994512,
-8.6906704931304));
#146427=CARTESIAN_POINT('',(-2.449283685,-1.00000000000002,-8.660312317));
#146428=CARTESIAN_POINT('Origin',(1.11022302462516E-15,-1.00000000000002,
2.22044604925031E-15));
#146429=CARTESIAN_POINT('',(-2.449283685,0.999999999999982,-8.660312317));
#146430=CARTESIAN_POINT('Ctrl Pts',(-2.44928368526842,0.999999999964309,
-8.66031231697031));
#146431=CARTESIAN_POINT('Ctrl Pts',(-2.42681483546961,0.88896344465514,
-8.59058438675928));
#146432=CARTESIAN_POINT('Ctrl Pts',(-2.40810561014116,0.769956469618107,
-8.53251166741322));
#146433=CARTESIAN_POINT('Ctrl Pts',(-2.36779468545961,0.424051722952562,
-8.40737682964596));
#146434=CARTESIAN_POINT('Ctrl Pts',(-2.35552405319222,0.188791058808562,
-8.36927336764646));
#146435=CARTESIAN_POINT('Ctrl Pts',(-2.35931955747613,-0.283921315912972,
-8.38105791060647));
#146436=CARTESIAN_POINT('Ctrl Pts',(-2.37535756277304,-0.516830885588973,
-8.43085829178138));
#146437=CARTESIAN_POINT('Ctrl Pts',(-2.41723518540491,-0.826237684533162,
-8.56084865517789));
#146438=CARTESIAN_POINT('Ctrl Pts',(-2.43217932752638,-0.915473689919173,
-8.60723209819538));
#146439=CARTESIAN_POINT('Ctrl Pts',(-2.44928368526842,-0.999999999964344,
-8.66031231697031));
#146440=CARTESIAN_POINT('Origin',(1.11022302462516E-15,0.999999999999982,
2.22044604925031E-15));
#146441=CARTESIAN_POINT('Origin',(1.11022302462516E-15,-1.77635683940025E-14,
2.22044604925031E-15));
#146442=CARTESIAN_POINT('',(-3.108891735,-1.00000000000002,-8.44599267));
#146443=CARTESIAN_POINT('',(-3.108891735,0.999999999999982,-8.44599267));
#146444=CARTESIAN_POINT('Ctrl Pts',(-3.10889173544937,-1.0000000000809,
-8.44599266972378));
#146445=CARTESIAN_POINT('Ctrl Pts',(-3.08608436775725,-0.888963444735185,
-8.37637473060366));
#146446=CARTESIAN_POINT('Ctrl Pts',(-3.06708616103101,-0.769956469654648,
-8.31839590697488));
#146447=CARTESIAN_POINT('Ctrl Pts',(-3.02614597203477,-0.424051722946105,
-8.19346552955976));
#146448=CARTESIAN_POINT('Ctrl Pts',(-3.01367646906759,-0.188791058808043,
-8.15542668456797));
#146449=CARTESIAN_POINT('Ctrl Pts',(-3.01753262214961,0.283921315904936,
-8.16719152153766));
#146450=CARTESIAN_POINT('Ctrl Pts',(-3.03382953289371,0.516830885577599,
-8.21690777923272));
#146451=CARTESIAN_POINT('Ctrl Pts',(-3.07635624297832,0.826237684567004,
-8.34668724135259));
#146452=CARTESIAN_POINT('Ctrl Pts',(-3.0915296817749,0.915473689997013,
-8.39299618139483));
#146453=CARTESIAN_POINT('Ctrl Pts',(-3.10889173544937,1.00000000008087,
-8.44599266972378));
#146454=CARTESIAN_POINT('',(-3.215728,-1.00000000000002,-8.405896349));
#146455=CARTESIAN_POINT('Origin',(1.11022302462516E-15,-1.00000000000002,
2.22044604925031E-15));
#146456=CARTESIAN_POINT('',(-3.215728,0.999999999999982,-8.405896349));
#146457=CARTESIAN_POINT('Ctrl Pts',(-3.21572799949971,1.00000000004184,
-8.40589634914347));
#146458=CARTESIAN_POINT('Ctrl Pts',(-3.1870992391518,0.888963444706609,
-8.33846321524215));
#146459=CARTESIAN_POINT('Ctrl Pts',(-3.16325973318893,0.769956469638536,
-8.28230136161672));
#146460=CARTESIAN_POINT('Ctrl Pts',(-3.11189408797419,0.424051722944788,
-8.1612837233719));
#146461=CARTESIAN_POINT('Ctrl Pts',(-3.09625728563935,0.188791058807923,
-8.12443358571553));
#146462=CARTESIAN_POINT('Ctrl Pts',(-3.10109386863279,-0.283921315903343,
-8.13583046118458));
#146463=CARTESIAN_POINT('Ctrl Pts',(-3.12153138141973,-0.516830885575342,
-8.18399272494027));
#146464=CARTESIAN_POINT('Ctrl Pts',(-3.17489266348559,-0.826237684550909,
-8.30970590417526));
#146465=CARTESIAN_POINT('Ctrl Pts',(-3.19393442470021,-0.915473689968737,
-8.35456303852214));
#146466=CARTESIAN_POINT('Ctrl Pts',(-3.21572799949971,-1.00000000004188,
-8.40589634914347));
#146467=CARTESIAN_POINT('Origin',(1.11022302462516E-15,0.999999999999982,
2.22044604925031E-15));
#146468=CARTESIAN_POINT('Origin',(1.11022302462516E-15,-1.77635683940025E-14,
2.22044604925031E-15));
#146469=CARTESIAN_POINT('',(-3.85346919675118,-0.999999999914645,-8.13331268017501));
#146470=CARTESIAN_POINT('',(-3.853469196,0.999999999999982,-8.13331268));
#146471=CARTESIAN_POINT('Ctrl Pts',(-3.85346919578197,-1.00000000005209,
-8.13331268036528));
#146472=CARTESIAN_POINT('Ctrl Pts',(-3.82451313984361,-0.888963444719943,
-8.06601943931758));
#146473=CARTESIAN_POINT('Ctrl Pts',(-3.8003942325866,-0.769956469655612,
-8.00997700754015));
#146474=CARTESIAN_POINT('Ctrl Pts',(-3.74842018395872,-0.424051722956698,
-7.889219413393));
#146475=CARTESIAN_POINT('Ctrl Pts',(-3.73259110373581,-0.188791058808942,
-7.85245145924943));
#146476=CARTESIAN_POINT('Ctrl Pts',(-3.73748632494522,0.283921315917998,
-7.86382327154454));
#146477=CARTESIAN_POINT('Ctrl Pts',(-3.75817416014108,0.516830885596111,
-7.9118785423691));
#146478=CARTESIAN_POINT('Ctrl Pts',(-3.81216301158527,0.826237684515586,
-8.03732348555132));
#146479=CARTESIAN_POINT('Ctrl Pts',(-3.83142646798091,0.915473689877324,
-8.08208586278962));
#146480=CARTESIAN_POINT('Ctrl Pts',(-3.85346919574261,0.999999999901152,
-8.13331268027382));
#146481=CARTESIAN_POINT('',(-3.956281164,-1.00000000000002,-8.083801046));
#146482=CARTESIAN_POINT('Origin',(1.11022302462516E-15,-1.00000000000002,
2.22044604925031E-15));
#146483=CARTESIAN_POINT('',(-3.956281164,0.999999999999982,-8.083801046));
#146484=CARTESIAN_POINT('Ctrl Pts',(-3.95628116427791,1.00000000002303,
-8.08380104581171));
#146485=CARTESIAN_POINT('Ctrl Pts',(-3.92172299544629,0.888963444698272,
-8.01920564015371));
#146486=CARTESIAN_POINT('Ctrl Pts',(-3.89294515063276,0.769956469642722,
-7.96540683446067));
#146487=CARTESIAN_POINT('Ctrl Pts',(-3.83093835105285,0.424051722954888,
-7.84948075853399));
#146488=CARTESIAN_POINT('Ctrl Pts',(-3.8120612770459,0.18879105880875,-7.81418064083539));
#146489=CARTESIAN_POINT('Ctrl Pts',(-3.81789999740993,-0.283921315915858,
-7.82509808788435));
#146490=CARTESIAN_POINT('Ctrl Pts',(-3.84257246677633,-0.516830885593061,
-7.87123446002671));
#146491=CARTESIAN_POINT('Ctrl Pts',(-3.9069877744043,-0.826237684557927,
-7.99165828656834));
#146492=CARTESIAN_POINT('Ctrl Pts',(-3.92997384156548,-0.915473689962003,
-8.03462794897708));
#146493=CARTESIAN_POINT('Ctrl Pts',(-3.95628116427791,-1.00000000002306,
-8.08380104581171));
#146494=CARTESIAN_POINT('Origin',(1.11022302462516E-15,0.999999999999982,
2.22044604925031E-15));
#146495=CARTESIAN_POINT('Origin',(1.11022302462516E-15,-1.77635683940025E-14,
2.22044604925031E-15));
#146496=CARTESIAN_POINT('',(-4.56702079,-1.00000000000002,-7.755148038));
#146497=CARTESIAN_POINT('',(-4.567020791,0.999999999999982,-7.755148038));
#146498=CARTESIAN_POINT('Ctrl Pts',(-4.5670207907231,-0.999999999723034,
-7.75514803808598));
#146499=CARTESIAN_POINT('Ctrl Pts',(-4.53214918384362,-0.888963444478476,
-7.69072130072636));
#146500=CARTESIAN_POINT('Ctrl Pts',(-4.5031037674526,-0.769956469518228,
-7.63706648150941));
#146501=CARTESIAN_POINT('Ctrl Pts',(-4.44051432392658,-0.424051722944118,
-7.52145393970776));
#146502=CARTESIAN_POINT('Ctrl Pts',(-4.42145311296568,-0.188791058807883,
-7.48625291033001));
#146503=CARTESIAN_POINT('Ctrl Pts',(-4.42734798883601,0.283921315902463,
-7.49714013881019));
#146504=CARTESIAN_POINT('Ctrl Pts',(-4.45226018210561,0.516830885574101,
-7.54314751001829));
#146505=CARTESIAN_POINT('Ctrl Pts',(-4.5172764881937,0.82623768451322,-7.66324792548531));
#146506=CARTESIAN_POINT('Ctrl Pts',(-4.54047486409895,0.915473689897858,
-7.70610333967294));
#146507=CARTESIAN_POINT('Ctrl Pts',(-4.56702079079182,0.999999999941809,
-7.75514803821294));
#146508=CARTESIAN_POINT('',(-4.664980679,-1.00000000000002,-7.69661973));
#146509=CARTESIAN_POINT('Origin',(1.11022302462516E-15,-1.00000000000002,
2.22044604925031E-15));
#146510=CARTESIAN_POINT('',(-4.664980678,0.999999999999982,-7.69661973));
#146511=CARTESIAN_POINT('Ctrl Pts',(-4.66498067874573,0.999999999872924,
-7.69661972974073));
#146512=CARTESIAN_POINT('Ctrl Pts',(-4.62477134343723,0.888963444590632,
-7.63538213660728));
#146513=CARTESIAN_POINT('Ctrl Pts',(-4.59128686201658,0.769956469585573,
-7.58437953524182));
#146514=CARTESIAN_POINT('Ctrl Pts',(-4.51913815025123,0.424051722954113,
-7.47447839030291));
#146515=CARTESIAN_POINT('Ctrl Pts',(-4.49717279163596,0.188791058808665,
-7.44101250837074));
#146516=CARTESIAN_POINT('Ctrl Pts',(-4.50396663943793,-0.283921315914944,
-7.45136262612836));
#146517=CARTESIAN_POINT('Ctrl Pts',(-4.53267541721535,-0.516830885591754,
-7.49510164369407));
#146518=CARTESIAN_POINT('Ctrl Pts',(-4.60762611636159,-0.826237684594402,
-7.60926653566084));
#146519=CARTESIAN_POINT('Ctrl Pts',(-4.63437141923369,-0.915473690033446,
-7.65000275968309));
#146520=CARTESIAN_POINT('Ctrl Pts',(-4.66498067883709,-1.00000000012526,
-7.69661972987988));
#146521=CARTESIAN_POINT('Origin',(1.11022302462516E-15,0.999999999999982,
2.22044604925031E-15));
#146522=CARTESIAN_POINT('Origin',(1.11022302462516E-15,-1.77635683940025E-14,
2.22044604925031E-15));
#146523=CARTESIAN_POINT('',(-5.243801418,-1.00000000000002,-7.314543505));
#146524=CARTESIAN_POINT('',(-5.243801418,0.999999999999982,-7.314543505));
#146525=CARTESIAN_POINT('Ctrl Pts',(-5.2438014182955,-0.999999999983744,
-7.31454350483351));
#146526=CARTESIAN_POINT('Ctrl Pts',(-5.20329502600418,-0.888963444664369,
-7.25350199725071));
#146527=CARTESIAN_POINT('Ctrl Pts',(-5.16955695697835,-0.769956469615146,
-7.20266678756193));
#146528=CARTESIAN_POINT('Ctrl Pts',(-5.09685605179224,-0.424051722943349,
-7.09313014228908));
#146529=CARTESIAN_POINT('Ctrl Pts',(-5.07471617971955,-0.188791058807812,
-7.0597794556822));
#146530=CARTESIAN_POINT('Ctrl Pts',(-5.08156324818856,0.283921315901536,
-7.0700944427827));
#146531=CARTESIAN_POINT('Ctrl Pts',(-5.11049922124789,0.516830885572785,
-7.11368349005474));
#146532=CARTESIAN_POINT('Ctrl Pts',(-5.18601950903758,0.826237684527553,
-7.22747239982518));
#146533=CARTESIAN_POINT('Ctrl Pts',(-5.21296602481403,0.91547368992686,
-7.26807580434118));
#146534=CARTESIAN_POINT('Ctrl Pts',(-5.2438014182955,0.999999999983708,
-7.31454350483351));
#146535=CARTESIAN_POINT('',(-5.336120511,-1.00000000000002,-7.247469758));
#146536=CARTESIAN_POINT('Origin',(1.11022302462516E-15,-1.00000000000002,
2.22044604925031E-15));
#146537=CARTESIAN_POINT('',(-5.336120511,0.999999999999982,-7.247469758));
#146538=CARTESIAN_POINT('Ctrl Pts',(-5.3361205105636,1.00000000006483,-7.24746975822081));
#146539=CARTESIAN_POINT('Ctrl Pts',(-5.29058375060566,0.888963444722998,
-7.19008302665036));
#146540=CARTESIAN_POINT('Ctrl Pts',(-5.25266222985656,0.769956469647075,
-7.1422872725303));
#146541=CARTESIAN_POINT('Ctrl Pts',(-5.17095250481387,0.424051722944707,
-7.03929591799513));
#146542=CARTESIAN_POINT('Ctrl Pts',(-5.14607571372182,0.1887910588079,-7.0079337194511));
#146543=CARTESIAN_POINT('Ctrl Pts',(-5.1537699888994,-0.283921315903279,
-7.01763317484824));
#146544=CARTESIAN_POINT('Ctrl Pts',(-5.18628392891646,-0.516830885575241,
-7.05862267696227));
#146545=CARTESIAN_POINT('Ctrl Pts',(-5.27116656068067,-0.826237684559263,
-7.16560944569037));
#146546=CARTESIAN_POINT('Ctrl Pts',(-5.30145576182033,-0.915473689984878,
-7.20378424715405));
#146547=CARTESIAN_POINT('Ctrl Pts',(-5.3361205105636,-1.00000000006487,
-7.24746975822081));
#146548=CARTESIAN_POINT('Origin',(1.11022302462516E-15,0.999999999999982,
2.22044604925031E-15));
#146549=CARTESIAN_POINT('Origin',(1.11022302462516E-15,-1.77635683940025E-14,
2.22044604925031E-15));
#146550=CARTESIAN_POINT('',(-5.87836204,-1.00000000000002,-6.815046568));
#146551=CARTESIAN_POINT('',(-5.878362039,0.999999999999982,-6.815046569));
#146552=CARTESIAN_POINT('Ctrl Pts',(-5.8783620393509,-0.999999999947016,
-6.81504656862317));
#146553=CARTESIAN_POINT('Ctrl Pts',(-5.83254699529058,-0.888963444643322,
-6.75788176127013));
#146554=CARTESIAN_POINT('Ctrl Pts',(-5.79438791271225,-0.769956469612807,
-6.71027545642628));
#146555=CARTESIAN_POINT('Ctrl Pts',(-5.71216089072527,-0.424051722953643,
-6.60769663246045));
#146556=CARTESIAN_POINT('Ctrl Pts',(-5.6871206147411,-0.188791058808675,
-6.57646480876682));
#146557=CARTESIAN_POINT('Ctrl Pts',(-5.69486474725043,0.283921315914249,
-6.58612450427073));
#146558=CARTESIAN_POINT('Ctrl Pts',(-5.72759152469995,0.516830885590793,
-6.62694427419722));
#146559=CARTESIAN_POINT('Ctrl Pts',(-5.81300774934533,0.826237684554357,
-6.73350551678999));
#146560=CARTESIAN_POINT('Ctrl Pts',(-5.84348544752745,0.915473689957745,
-6.77152999685925));
#146561=CARTESIAN_POINT('Ctrl Pts',(-5.87836203938029,1.0000000000182,-6.81504656865983));
#146562=CARTESIAN_POINT('',(-5.964297039,-1.00000000000002,-6.739967421));
#146563=CARTESIAN_POINT('Origin',(1.11022302462516E-15,-1.00000000000002,
2.22044604925031E-15));
#146564=CARTESIAN_POINT('',(-5.964297039,0.999999999999982,-6.739967421));
#146565=CARTESIAN_POINT('Ctrl Pts',(-5.96429703907415,1.00000000016684,
-6.73996742058037));
#146566=CARTESIAN_POINT('Ctrl Pts',(-5.91379948977288,0.888963444798608,
-6.68689359476871));
#146567=CARTESIAN_POINT('Ctrl Pts',(-5.87174625155671,0.769956469691324,
-6.64268951118085));
#146568=CARTESIAN_POINT('Ctrl Pts',(-5.78113339203643,0.424051722950086,
-6.54743717279022));
#146569=CARTESIAN_POINT('Ctrl Pts',(-5.75354546180194,0.18879105880834,
-6.51843116758519));
#146570=CARTESIAN_POINT('Ctrl Pts',(-5.76207821456473,-0.28392131590995,
-6.52740186632182));
#146571=CARTESIAN_POINT('Ctrl Pts',(-5.79813553364252,-0.516830885584689,
-6.56531182965558));
#146572=CARTESIAN_POINT('Ctrl Pts',(-5.8922666728607,-0.826237684604123,
-6.66425908071305));
#146573=CARTESIAN_POINT('Ctrl Pts',(-5.92585590139914,-0.91547369006014,
-6.69956509862226));
#146574=CARTESIAN_POINT('Ctrl Pts',(-5.96429703907415,-1.00000000016687,
-6.73996742058037));
#146575=CARTESIAN_POINT('Origin',(1.11022302462516E-15,0.999999999999982,
2.22044604925031E-15));
#146576=CARTESIAN_POINT('Origin',(1.11022302462516E-15,-1.77635683940025E-14,
2.22044604925031E-15));
#146577=CARTESIAN_POINT('',(-6.465593547,-1.00000000000002,-6.260678884));
#146578=CARTESIAN_POINT('',(-6.465593547,0.999999999999982,-6.260678883));
#146579=CARTESIAN_POINT('Ctrl Pts',(-6.465593547415,-1.00000000013442,-6.26067888331879));
#146580=CARTESIAN_POINT('Ctrl Pts',(-6.41483872740882,-0.888963444774572,
-6.20785103349866));
#146581=CARTESIAN_POINT('Ctrl Pts',(-6.37256586579951,-0.769956469677245,
-6.16385693138393));
#146582=CARTESIAN_POINT('Ctrl Pts',(-6.2814747707594,-0.424051722948395,
-6.06906183297416));
#146583=CARTESIAN_POINT('Ctrl Pts',(-6.25373570048456,-0.18879105880825,
-6.04020033244393));
#146584=CARTESIAN_POINT('Ctrl Pts',(-6.26231454581811,0.283921315907737,
-6.04912696217015));
#146585=CARTESIAN_POINT('Ctrl Pts',(-6.29856863083365,0.516830885581577,
-6.08684879800449));
#146586=CARTESIAN_POINT('Ctrl Pts',(-6.39319307094973,0.826237684468098,
-6.18532440503001));
#146587=CARTESIAN_POINT('Ctrl Pts',(-6.42695656294875,0.915473689802836,
-6.22046380990041));
#146588=CARTESIAN_POINT('Ctrl Pts',(-6.46559354726348,0.999999999802907,
-6.26067888316109));
#146589=CARTESIAN_POINT('',(-6.544452554,-1.00000000000002,-6.178198829));
#146590=CARTESIAN_POINT('Origin',(1.11022302462516E-15,-1.00000000000002,
2.22044604925031E-15));
#146591=CARTESIAN_POINT('',(-6.544452554,0.999999999999982,-6.178198829));
#146592=CARTESIAN_POINT('Ctrl Pts',(-6.54445255390455,1.0000000000868,-6.17819882890926));
#146593=CARTESIAN_POINT('Ctrl Pts',(-6.48940079184017,0.888963444741018,
-6.12986522815414));
#146594=CARTESIAN_POINT('Ctrl Pts',(-6.44355442410624,0.769956469660418,
-6.0896087204346));
#146595=CARTESIAN_POINT('Ctrl Pts',(-6.34476799154022,0.424051722949282,
-6.00286231406975));
#146596=CARTESIAN_POINT('Ctrl Pts',(-6.31469104394089,0.188791058808275,
-5.97644604151514));
#146597=CARTESIAN_POINT('Ctrl Pts',(-6.32399357358486,-0.283921315908946,
-5.98461575679496));
#146598=CARTESIAN_POINT('Ctrl Pts',(-6.36330395941132,-0.516830885583268,
-6.01914095259761));
#146599=CARTESIAN_POINT('Ctrl Pts',(-6.46592571753245,-0.82623768457364,
-6.10925202083548));
#146600=CARTESIAN_POINT('Ctrl Pts',(-6.50254453274514,-0.915473690003293,
-6.1414049918512));
#146601=CARTESIAN_POINT('Ctrl Pts',(-6.54445255390455,-1.00000000008684,
-6.17819882890926));
#146602=CARTESIAN_POINT('Origin',(1.11022302462516E-15,0.999999999999982,
2.22044604925031E-15));
#146603=CARTESIAN_POINT('Origin',(1.11022302462516E-15,-1.77635683940025E-14,
2.22044604925031E-15));
#146604=CARTESIAN_POINT('',(-7.000767897,-1.00000000000002,-5.655903894));
#146605=CARTESIAN_POINT('',(-7.000767897,0.999999999999982,-5.655903894));
#146606=CARTESIAN_POINT('Ctrl Pts',(-7.00076789655177,-1.00000000017299,
-5.65590389411597));
#146607=CARTESIAN_POINT('Ctrl Pts',(-6.94548194857316,-0.888963444802471,
-5.60783834066879));
#146608=CARTESIAN_POINT('Ctrl Pts',(-6.89943566416173,-0.769956469692456,
-5.56781065596884));
#146609=CARTESIAN_POINT('Ctrl Pts',(-6.80021390797847,-0.42405172294906,
-5.4815625175572));
#146610=CARTESIAN_POINT('Ctrl Pts',(-6.76999938208442,-0.1887910588083,
-5.45530371603143));
#146611=CARTESIAN_POINT('Ctrl Pts',(-6.77934386842823,0.283921315908572,
-5.46342540800412));
#146612=CARTESIAN_POINT('Ctrl Pts',(-6.81883336445019,0.516830885582756,
-5.49774559569251));
#146613=CARTESIAN_POINT('Ctrl Pts',(-6.92190415979063,0.826237684604844,
-5.58734269949925));
#146614=CARTESIAN_POINT('Ctrl Pts',(-6.95868160192628,0.915473690063716,
-5.61931410742192));
#146615=CARTESIAN_POINT('Ctrl Pts',(-7.00076789655177,1.00000000017296,
-5.65590389411597));
#146616=CARTESIAN_POINT('',(-7.071915985,-1.00000000000002,-5.566687013));
#146617=CARTESIAN_POINT('Origin',(1.11022302462516E-15,-1.00000000000002,
2.22044604925031E-15));
#146618=CARTESIAN_POINT('',(-7.07191598509133,1.00000000000236,-5.56668701279559));
#146619=CARTESIAN_POINT('Ctrl Pts',(-7.07191598491097,1.00000000000174,
-5.56668701304417));
#146620=CARTESIAN_POINT('Ctrl Pts',(-7.01275325449934,0.888963444679146,
-5.52348279108474));
#146621=CARTESIAN_POINT('Ctrl Pts',(-6.96348288524122,0.769956469626119,
-5.48749798096801));
#146622=CARTESIAN_POINT('Ctrl Pts',(-6.85731824989088,0.424051722947136,
-5.40995593770057));
#146623=CARTESIAN_POINT('Ctrl Pts',(-6.82499444682085,0.188791058808089,
-5.38634208609494));
#146624=CARTESIAN_POINT('Ctrl Pts',(-6.83499185484783,-0.283921315906313,
-5.39364504017274));
#146625=CARTESIAN_POINT('Ctrl Pts',(-6.87723880331428,-0.516830885579532,
-5.42450749186227));
#146626=CARTESIAN_POINT('Ctrl Pts',(-6.98752493029364,-0.826237684546756,
-5.50505685593148));
#146627=CARTESIAN_POINT('Ctrl Pts',(-7.02687849901688,-0.915473689956015,
-5.53379790323594));
#146628=CARTESIAN_POINT('Ctrl Pts',(-7.07191598492155,-1.00000000002162,
-5.5666870130519));
#146629=CARTESIAN_POINT('Origin',(1.11022302462516E-15,0.999999999999982,
2.22044604925031E-15));
#146630=CARTESIAN_POINT('Origin',(1.11022302462516E-15,-1.77635683940025E-14,
2.22044604925031E-15));
#146631=CARTESIAN_POINT('',(-7.47957618,-1.00000000000002,-5.005590892));
#146632=CARTESIAN_POINT('',(-7.47957618,0.999999999999982,-5.005590892));
#146633=CARTESIAN_POINT('Ctrl Pts',(-7.47957617967883,-1.00000000029992,
-5.00559089166839));
#146634=CARTESIAN_POINT('Ctrl Pts',(-7.4202042336451,-0.888963444893636,
-4.96267463016275));
#146635=CARTESIAN_POINT('Ctrl Pts',(-7.37075526401692,-0.769956469741096,
-4.92693564225511));
#146636=CARTESIAN_POINT('Ctrl Pts',(-7.26420172190818,-0.424051722949988,
-4.84992888314661));
#146637=CARTESIAN_POINT('Ctrl Pts',(-7.23175500998826,-0.188791058808376,
-4.82648420105959));
#146638=CARTESIAN_POINT('Ctrl Pts',(-7.24178990103384,0.283921315909722,
-4.83373556418914));
#146639=CARTESIAN_POINT('Ctrl Pts',(-7.28419686186403,0.516830885584386,
-4.86437777775459));
#146640=CARTESIAN_POINT('Ctrl Pts',(-7.3948841469757,0.82623768465271,-4.94437499509896));
#146641=CARTESIAN_POINT('Ctrl Pts',(-7.43437942887842,0.915473690153646,
-4.9729209910481));
#146642=CARTESIAN_POINT('Ctrl Pts',(-7.47957617967883,1.00000000029988,
-5.00559089166839));
#146643=CARTESIAN_POINT('',(-7.542440507,-1.00000000000002,-4.910355506));
#146644=CARTESIAN_POINT('Origin',(1.11022302462516E-15,-1.00000000000002,
2.22044604925031E-15));
#146645=CARTESIAN_POINT('',(-7.542440507,0.999999999999982,-4.910355506));
#146646=CARTESIAN_POINT('Ctrl Pts',(-7.54244050680655,0.999999999960002,
-4.91035550643967));
#146647=CARTESIAN_POINT('Ctrl Pts',(-7.47964315154329,0.888963444646453,
-4.87262851828103));
#146648=CARTESIAN_POINT('Ctrl Pts',(-7.42734547678568,0.769956469604148,
-4.84120513431145));
#146649=CARTESIAN_POINT('Ctrl Pts',(-7.31465741384491,0.424051722941438,
-4.77349177711883));
#146650=CARTESIAN_POINT('Ctrl Pts',(-7.28034700755391,0.188791058807605,
-4.75287047132402));
#146651=CARTESIAN_POINT('Ctrl Pts',(-7.29095880071433,-0.28392131589928,
-4.75924786510321));
#146652=CARTESIAN_POINT('Ctrl Pts',(-7.33580216424091,-0.516830885569566,
-4.78619908634786));
#146653=CARTESIAN_POINT('Ctrl Pts',(-7.45286470105418,-0.826237684516339,
-4.85653821008756));
#146654=CARTESIAN_POINT('Ctrl Pts',(-7.49463617150114,-0.915473689909019,
-4.88163592765425));
#146655=CARTESIAN_POINT('Ctrl Pts',(-7.54244050680655,-0.999999999960038,
-4.91035550643967));
#146656=CARTESIAN_POINT('Origin',(1.11022302462516E-15,0.999999999999982,
2.22044604925031E-15));
#146657=CARTESIAN_POINT('Origin',(1.11022302462516E-15,-1.77635683940025E-14,
2.22044604925031E-15));
#146658=CARTESIAN_POINT('',(-7.898163313,-1.00000000000002,-4.314975815));
#146659=CARTESIAN_POINT('',(-7.898163313,0.999999999999982,-4.314975815));
#146660=CARTESIAN_POINT('Ctrl Pts',(-7.89816331281296,-1.0000000001015,
-4.31497581501368));
#146661=CARTESIAN_POINT('Ctrl Pts',(-7.8351833967921,-0.888963444754436,
-4.27755438203096));
#146662=CARTESIAN_POINT('Ctrl Pts',(-7.78272987602674,-0.769956469672355,
-4.24639184029317));
#146663=CARTESIAN_POINT('Ctrl Pts',(-7.66970245447833,-0.424051722955077,
-4.1792464736998));
#146664=CARTESIAN_POINT('Ctrl Pts',(-7.63528479837203,-0.188791058808791,
-4.15880467385859));
#146665=CARTESIAN_POINT('Ctrl Pts',(-7.64592929907974,0.283921315916024,
-4.16512732442939));
#146666=CARTESIAN_POINT('Ctrl Pts',(-7.69091228881307,0.516830885593306,
-4.19184485076974));
#146667=CARTESIAN_POINT('Ctrl Pts',(-7.80832487473718,0.826237684586908,
-4.26159809102287));
#146668=CARTESIAN_POINT('Ctrl Pts',(-7.8502200035666,0.915473690017277,
-4.28648883936674));
#146669=CARTESIAN_POINT('Ctrl Pts',(-7.89816331281296,1.00000000010146,
-4.31497581501368));
#146670=CARTESIAN_POINT('',(-7.952237733,-1.00000000000002,-4.214488703));
#146671=CARTESIAN_POINT('Origin',(1.11022302462516E-15,-1.00000000000002,
2.22044604925031E-15));
#146672=CARTESIAN_POINT('',(-7.952237734,0.999999999999982,-4.214488703));
#146673=CARTESIAN_POINT('Ctrl Pts',(-7.9522377334233,1.00000000018981,-4.21448870353033));
#146674=CARTESIAN_POINT('Ctrl Pts',(-7.8863113606651,0.888963444813991,
-4.18254270459723));
#146675=CARTESIAN_POINT('Ctrl Pts',(-7.83140745051944,0.769956469697667,
-4.15593374930452));
#146676=CARTESIAN_POINT('Ctrl Pts',(-7.71310325805011,0.424051722948052,
-4.09859426618526));
#146677=CARTESIAN_POINT('Ctrl Pts',(-7.67708249577676,0.188791058808185,
-4.08113153679338));
#146678=CARTESIAN_POINT('Ctrl Pts',(-7.68822323414686,-0.283921315907398,
-4.08653202326161));
#146679=CARTESIAN_POINT('Ctrl Pts',(-7.73530196031026,-0.516830885581081,
-4.10935501872354));
#146680=CARTESIAN_POINT('Ctrl Pts',(-7.8581983881465,-0.8262376844579,-4.16891757298584));
#146681=CARTESIAN_POINT('Ctrl Pts',(-7.90205144094031,-0.915473689783842,
-4.19016988878227));
#146682=CARTESIAN_POINT('Ctrl Pts',(-7.95223773317769,-0.999999999776178,
-4.21448870341132));
#146683=CARTESIAN_POINT('Origin',(1.11022302462516E-15,0.999999999999982,
2.22044604925031E-15));
#146684=CARTESIAN_POINT('Origin',(1.11022302462516E-15,-1.77635683940025E-14,
2.22044604925031E-15));
#146685=CARTESIAN_POINT('',(-8.253159079,-1.00000000000002,-3.58961909));
#146686=CARTESIAN_POINT('',(-8.253159079,0.999999999999982,-3.58961909));
#146687=CARTESIAN_POINT('Ctrl Pts',(-8.25315907914881,-0.999999999891681,
-3.58961909006943));
#146688=CARTESIAN_POINT('Ctrl Pts',(-8.18707827043164,-0.888963444602147,
-3.55799378091446));
#146689=CARTESIAN_POINT('Ctrl Pts',(-8.13204252346783,-0.76995646958845,
-3.5316585877518));
#146690=CARTESIAN_POINT('Ctrl Pts',(-8.01345125288575,-0.424051722950383,
-3.47491522857435));
#146691=CARTESIAN_POINT('Ctrl Pts',(-7.97733976334233,-0.188791058808387,
-3.45764089629977));
#146692=CARTESIAN_POINT('Ctrl Pts',(-7.98850817044388,0.283921315910252,
-3.46298392805613));
#146693=CARTESIAN_POINT('Ctrl Pts',(-8.03570501247084,0.516830885585125,
-3.48556165340058));
#146694=CARTESIAN_POINT('Ctrl Pts',(-8.15889756203451,0.826237684503461,
-3.5445093046019));
#146695=CARTESIAN_POINT('Ctrl Pts',(-8.20285522282177,0.915473689866596,
-3.56554439971813));
#146696=CARTESIAN_POINT('Ctrl Pts',(-8.25315907914881,0.999999999891645,
-3.58961909006943));
#146697=CARTESIAN_POINT('',(-8.298008217,-1.00000000000002,-3.484689316));
#146698=CARTESIAN_POINT('Origin',(1.11022302462516E-15,-1.00000000000002,
2.22044604925031E-15));
#146699=CARTESIAN_POINT('',(-8.298008217,0.999999999999982,-3.484689316));
#146700=CARTESIAN_POINT('Ctrl Pts',(-8.29800821680407,0.999999999999763,
-3.48468931651914));
#146701=CARTESIAN_POINT('Ctrl Pts',(-8.22948362702398,0.888963444677762,
-3.4587815173023));
#146702=CARTESIAN_POINT('Ctrl Pts',(-8.17241553555401,0.769956469625439,
-3.43720123042082));
#146703=CARTESIAN_POINT('Ctrl Pts',(-8.04944772936533,0.424051722947192,
-3.39069728527389));
#146704=CARTESIAN_POINT('Ctrl Pts',(-8.01200662909584,0.188791058808111,
-3.37653373193536));
#146705=CARTESIAN_POINT('Ctrl Pts',(-8.02358661400347,-0.28392131590634,
-3.38091382954382));
#146706=CARTESIAN_POINT('Ctrl Pts',(-8.07252165259768,-0.51683088557958,
-3.39942484185536));
#146707=CARTESIAN_POINT('Ctrl Pts',(-8.20026248178415,-0.826237684538798,
-3.447731263932));
#146708=CARTESIAN_POINT('Ctrl Pts',(-8.24584403802863,-0.915473689940681,
-3.46496706682217));
#146709=CARTESIAN_POINT('Ctrl Pts',(-8.29800821680408,-0.999999999999801,
-3.48468931651914));
#146710=CARTESIAN_POINT('Origin',(1.11022302462516E-15,0.999999999999982,
2.22044604925031E-15));
#146711=CARTESIAN_POINT('Origin',(1.11022302462516E-15,-1.77635683940025E-14,
2.22044604925031E-15));
#146712=CARTESIAN_POINT('',(-8.541705262,-1.00000000000002,-2.835360862));
#146713=CARTESIAN_POINT('',(-8.541705262,0.999999999999982,-2.835360862));
#146714=CARTESIAN_POINT('Ctrl Pts',(-8.54170526179937,-1.00000000003984,
-2.83536086236564));
#146715=CARTESIAN_POINT('Ctrl Pts',(-8.47305560408872,-0.888963444708826,
-2.80978630543292));
#146716=CARTESIAN_POINT('Ctrl Pts',(-8.41588074631203,-0.76995646964581,
-2.78849049633943));
#146717=CARTESIAN_POINT('Ctrl Pts',(-8.29268045378883,-0.424051722952022,
-2.74260600880005));
#146718=CARTESIAN_POINT('Ctrl Pts',(-8.25516587927573,-0.188791058808552,
-2.72863822688283));
#146719=CARTESIAN_POINT('Ctrl Pts',(-8.26676827132905,0.283921315912211,
-2.73295862086762));
#146720=CARTESIAN_POINT('Ctrl Pts',(-8.31579896444622,0.51683088558791,
-2.75121476261534));
#146721=CARTESIAN_POINT('Ctrl Pts',(-8.4437796037711,0.826237684560039,
-2.79888221287883));
#146722=CARTESIAN_POINT('Ctrl Pts',(-8.48944587536211,0.915473689971902,
-2.81589229255365));
#146723=CARTESIAN_POINT('Ctrl Pts',(-8.54170526179937,1.00000000003981,
-2.83536086236564));
#146724=CARTESIAN_POINT('',(-8.576968018,-1.00000000000002,-2.726833259));
#146725=CARTESIAN_POINT('Origin',(1.11022302462516E-15,-1.00000000000002,
2.22044604925031E-15));
#146726=CARTESIAN_POINT('',(-8.576968018,0.999999999999982,-2.726833259));
#146727=CARTESIAN_POINT('Ctrl Pts',(-8.57696801766623,1.00000000014478,
-2.72683325938025));
#146728=CARTESIAN_POINT('Ctrl Pts',(-8.50639693048896,0.888963444783311,
-2.70717225418446));
#146729=CARTESIAN_POINT('Ctrl Pts',(-8.447624136351,0.769956469684066,-2.69079438744693));
#146730=CARTESIAN_POINT('Ctrl Pts',(-8.32098278088487,0.424051722950983,
-2.65550040263088));
#146731=CARTESIAN_POINT('Ctrl Pts',(-8.28242279634777,0.188791058808389,
-2.64475006193496));
#146732=CARTESIAN_POINT('Ctrl Pts',(-8.29434879256285,-0.283921315911112,
-2.64807450471779));
#146733=CARTESIAN_POINT('Ctrl Pts',(-8.34474614742513,-0.51683088558632,
-2.66212449411069));
#146734=CARTESIAN_POINT('Ctrl Pts',(-8.4763028838897,-0.826237684597308,
-2.6987858491335));
#146735=CARTESIAN_POINT('Ctrl Pts',(-8.52324594767412,-0.915473690045215,
-2.71186636657059));
#146736=CARTESIAN_POINT('Ctrl Pts',(-8.57696801766623,-1.00000000014482,
-2.72683325938025));
#146737=CARTESIAN_POINT('Origin',(1.11022302462516E-15,0.999999999999982,
2.22044604925031E-15));
#146738=CARTESIAN_POINT('Origin',(1.11022302462516E-15,-1.77635683940025E-14,
2.22044604925031E-15));
#146739=CARTESIAN_POINT('',(-8.761478656,-1.00000000000002,-2.058273977));
#146740=CARTESIAN_POINT('',(-8.761478656,0.999999999999982,-2.058273976));
#146741=CARTESIAN_POINT('Ctrl Pts',(-8.76147865594458,-1.00000000014044,
-2.0582739763956));
#146742=CARTESIAN_POINT('Ctrl Pts',(-8.69081287594316,-0.888963444777773,
-2.03895608293596));
#146743=CARTESIAN_POINT('Ctrl Pts',(-8.63195924570962,-0.76995646967708,
-2.02287111920752));
#146744=CARTESIAN_POINT('Ctrl Pts',(-8.50514186759658,-0.424051722946195,
-1.9882149381297));
#146745=CARTESIAN_POINT('Ctrl Pts',(-8.46652625341952,-0.188791058808052,
-1.97766616690805));
#146746=CARTESIAN_POINT('Ctrl Pts',(-8.47846921478163,0.283921315905045,
-1.98092913785784));
#146747=CARTESIAN_POINT('Ctrl Pts',(-8.52893899266448,0.516830885577757,
-1.99471670832764));
#146748=CARTESIAN_POINT('Ctrl Pts',(-8.66067729683783,0.82623768454449,
-2.03072016746058));
#146749=CARTESIAN_POINT('Ctrl Pts',(-8.70768450122283,0.915473689953664,
-2.04356827655552));
#146750=CARTESIAN_POINT('Ctrl Pts',(-8.76147865586744,1.00000000001919,
-2.05827397637451));
#146751=CARTESIAN_POINT('',(-8.786871115,-1.00000000000002,-1.947022346));
#146752=CARTESIAN_POINT('Origin',(1.11022302462516E-15,-1.00000000000002,
2.22044604925031E-15));
#146753=CARTESIAN_POINT('',(-8.786871115,0.999999999999982,-1.947022345));
#146754=CARTESIAN_POINT('Ctrl Pts',(-8.78687111468735,1.00000000013172,
-1.94702234559588));
#146755=CARTESIAN_POINT('Ctrl Pts',(-8.71482172704382,0.888963444773288,
-1.93376643331344));
#146756=CARTESIAN_POINT('Ctrl Pts',(-8.65481743424227,0.769956469677657,
-1.92272285170412));
#146757=CARTESIAN_POINT('Ctrl Pts',(-8.52552217123474,0.424051722949631,
-1.89892299368291));
#146758=CARTESIAN_POINT('Ctrl Pts',(-8.48615376474826,0.188791058808297,
-1.89167242106493));
#146759=CARTESIAN_POINT('Ctrl Pts',(-8.49832975116214,-0.283921315909391,
-1.89391444255924));
#146760=CARTESIAN_POINT('Ctrl Pts',(-8.54978365242985,-0.516830885583895,
-1.90339028676294));
#146761=CARTESIAN_POINT('Ctrl Pts',(-8.68409707869062,-0.826237684621147,
-1.92811139900698));
#146762=CARTESIAN_POINT('Ctrl Pts',(-8.73202369206082,-0.915473690093675,
-1.93693131433199));
#146763=CARTESIAN_POINT('Ctrl Pts',(-8.78687111474132,-1.00000000021493,
-1.94702234560581));
#146764=CARTESIAN_POINT('Origin',(1.11022302462516E-15,0.999999999999982,
2.22044604925031E-15));
#146765=CARTESIAN_POINT('Origin',(1.11022302462516E-15,-1.77635683940025E-14,
2.22044604925031E-15));
#146766=CARTESIAN_POINT('',(-8.910709775,-1.00000000000002,-1.264615079));
#146767=CARTESIAN_POINT('',(-8.910709775,0.999999999999982,-1.264615079));
#146768=CARTESIAN_POINT('Ctrl Pts',(-8.91070977524219,-0.999999999833344,
-1.26461507908072));
#146769=CARTESIAN_POINT('Ctrl Pts',(-8.83859683236404,-0.88896344455949,
-1.25170938549311));
#146770=CARTESIAN_POINT('Ctrl Pts',(-8.77853828457743,-0.769956469564433,
-1.24096477386405));
#146771=CARTESIAN_POINT('Ctrl Pts',(-8.64912487986267,-0.424051722948457,
-1.21781593054578));
#146772=CARTESIAN_POINT('Ctrl Pts',(-8.60971913623194,-0.188791058808239,
-1.21077110255088));
#146773=CARTESIAN_POINT('Ctrl Pts',(-8.62190650920452,0.283921315907843,
-1.21295037893394));
#146774=CARTESIAN_POINT('Ctrl Pts',(-8.67340901888981,0.516830885581718,
-1.2221583686789));
#146775=CARTESIAN_POINT('Ctrl Pts',(-8.80784430855032,0.826237684479383,
-1.24620795789709));
#146776=CARTESIAN_POINT('Ctrl Pts',(-8.85581397133016,0.915473689824291,
-1.25479065095093));
#146777=CARTESIAN_POINT('Ctrl Pts',(-8.91070977524219,0.999999999833308,
-1.26461507908072));
#146778=CARTESIAN_POINT('',(-8.926027492,-1.00000000000002,-1.151535151));
#146779=CARTESIAN_POINT('Origin',(1.11022302462516E-15,-1.00000000000002,
2.22044604925031E-15));
#146780=CARTESIAN_POINT('',(-8.926027492,0.999999999999982,-1.151535151));
#146781=CARTESIAN_POINT('Ctrl Pts',(-8.92602749223077,0.999999999828974,
-1.15153515131936));
#146782=CARTESIAN_POINT('Ctrl Pts',(-8.85307990351357,0.888963444557654,
-1.14479106076095));
#146783=CARTESIAN_POINT('Ctrl Pts',(-8.79232723139907,0.769956469565621,
-1.13917068070444));
#146784=CARTESIAN_POINT('Ctrl Pts',(-8.66141907032706,0.424051722951004,
-1.12705657192987));
#146785=CARTESIAN_POINT('Ctrl Pts',(-8.6215592131525,0.188791058808435,
-1.12336414473294));
#146786=CARTESIAN_POINT('Ctrl Pts',(-8.63388715588222,-0.28392131591104,
-1.12450569350138));
#146787=CARTESIAN_POINT('Ctrl Pts',(-8.68598332699613,-0.516830885586241,
-1.12933109859575));
#146788=CARTESIAN_POINT('Ctrl Pts',(-8.82197203024378,-0.826237684481343,
-1.14191292820707));
#146789=CARTESIAN_POINT('Ctrl Pts',(-8.87049631618663,-0.915473689822921,
-1.14640122864087));
#146790=CARTESIAN_POINT('Ctrl Pts',(-8.92602749223077,-0.999999999829011,
-1.15153515131936));
#146791=CARTESIAN_POINT('Origin',(1.11022302462516E-15,0.999999999999982,
2.22044604925031E-15));
#146792=CARTESIAN_POINT('Origin',(1.11022302462516E-15,-1.77635683940025E-14,
2.22044604925031E-15));
#146793=CARTESIAN_POINT('',(-8.988197099,-1.00000000000002,-0.460774244));
#146794=CARTESIAN_POINT('',(-8.988197099,0.999999999999982,-0.460774244));
#146795=CARTESIAN_POINT('Ctrl Pts',(-8.98819709915994,-0.999999999884686,
-0.4607742441774));
#146796=CARTESIAN_POINT('Ctrl Pts',(-8.91521760431959,-0.888963444596554,
-0.454384659487097));
#146797=CARTESIAN_POINT('Ctrl Pts',(-8.85443769501692,-0.769956469584521,
-0.449066909228443));
#146798=CARTESIAN_POINT('Ctrl Pts',(-8.72347022429716,-0.42405172294922,
-0.437611784522527));
#146799=CARTESIAN_POINT('Ctrl Pts',(-8.68359162309196,-0.188791058808321,
-0.434127620564106));
#146800=CARTESIAN_POINT('Ctrl Pts',(-8.69592528211311,0.283921315908748,
-0.435205656129234));
#146801=CARTESIAN_POINT('Ctrl Pts',(-8.74804585567359,0.51683088558301,
-0.439759927834076));
#146802=CARTESIAN_POINT('Ctrl Pts',(-8.88409573694761,0.82623768449924,
-0.451662014005326));
#146803=CARTESIAN_POINT('Ctrl Pts',(-8.93264163465328,0.915473689860902,
-0.455910188236057));
#146804=CARTESIAN_POINT('Ctrl Pts',(-8.98819709915994,0.999999999884654,
-0.460774244177401));
#146805=CARTESIAN_POINT('',(-8.993316745,-1.00000000000002,-0.346776472999999));
#146806=CARTESIAN_POINT('Origin',(1.11022302462516E-15,-1.00000000000002,
2.22044604925031E-15));
#146807=CARTESIAN_POINT('',(-8.993316745,0.999999999999982,-0.346776472999999));
#146808=CARTESIAN_POINT('Ctrl Pts',(-8.99331674501375,0.999999999990158,
-0.3467764734695));
#146809=CARTESIAN_POINT('Ctrl Pts',(-8.92005828617789,0.888963444672462,
-0.346598504082613));
#146810=CARTESIAN_POINT('Ctrl Pts',(-8.85904637943988,0.769956469625277,
-0.346446577571944));
#146811=CARTESIAN_POINT('Ctrl Pts',(-8.7275793157764,0.42405172295028,-0.346115753738565));
#146812=CARTESIAN_POINT('Ctrl Pts',(-8.68754893604615,0.188791058808367,
-0.34601120122187));
#146813=CARTESIAN_POINT('Ctrl Pts',(-8.69992957774535,-0.283921315910156,
-0.346043086182908));
#146814=CARTESIAN_POINT('Ctrl Pts',(-8.75224857096815,-0.516830885584984,
-0.346179200834906));
#146815=CARTESIAN_POINT('Ctrl Pts',(-8.88881765021394,-0.826237684539528,
-0.346520446308492));
#146816=CARTESIAN_POINT('Ctrl Pts',(-8.93754891983274,-0.915473689935909,
-0.346640994702772));
#146817=CARTESIAN_POINT('Ctrl Pts',(-8.99331674501375,-0.999999999990196,
-0.346776473469499));
#146818=CARTESIAN_POINT('Origin',(1.11022302462516E-15,0.999999999999982,
2.22044604925031E-15));
#146819=CARTESIAN_POINT('Origin',(1.11022302462516E-15,-1.77635683940025E-14,
2.22044604925031E-15));
#146820=CARTESIAN_POINT('',(-8.993316745,-1.00000000000002,0.346776472999999));
#146821=CARTESIAN_POINT('',(-8.993316745,0.999999999999982,0.346776472999999));
#146822=CARTESIAN_POINT('Ctrl Pts',(-8.99331674501319,-0.999999999990532,
0.346776473489777));
#146823=CARTESIAN_POINT('Ctrl Pts',(-8.92005828617723,-0.888963444672731,
0.34659850410287));
#146824=CARTESIAN_POINT('Ctrl Pts',(-8.85904637943913,-0.76995646962542,
0.346446577592178));
#146825=CARTESIAN_POINT('Ctrl Pts',(-8.72757931577561,-0.424051722950311,
0.346115753758762));
#146826=CARTESIAN_POINT('Ctrl Pts',(-8.68754893604535,-0.188791058808411,
0.346011201242062));
#146827=CARTESIAN_POINT('Ctrl Pts',(-8.69992957774455,0.283921315910098,
0.346043086203105));
#146828=CARTESIAN_POINT('Ctrl Pts',(-8.75224857096735,0.516830885584921,
0.346179200855117));
#146829=CARTESIAN_POINT('Ctrl Pts',(-8.88881765021319,0.826237684539586,
0.346520446328741));
#146830=CARTESIAN_POINT('Ctrl Pts',(-8.93754891983208,0.915473689936097,
0.346640994723034));
#146831=CARTESIAN_POINT('Ctrl Pts',(-8.99331674501319,0.999999999990497,
0.346776473489777));
#146832=CARTESIAN_POINT('',(-8.988197099,-1.00000000000002,0.460774244000002));
#146833=CARTESIAN_POINT('Origin',(1.11022302462516E-15,-1.00000000000002,
2.22044604925031E-15));
#146834=CARTESIAN_POINT('',(-8.988197099,0.999999999999982,0.460774244000002));
#146835=CARTESIAN_POINT('Ctrl Pts',(-8.9881970991918,0.999999999893167,
0.460774243665518));
#146836=CARTESIAN_POINT('Ctrl Pts',(-8.91521760434871,0.888963444601223,
0.454384658959215));
#146837=CARTESIAN_POINT('Ctrl Pts',(-8.85443769504401,0.76995646958464,
0.449066908687328));
#146838=CARTESIAN_POINT('Ctrl Pts',(-8.72347022432541,0.424051722946442,
0.437611783953442));
#146839=CARTESIAN_POINT('Ctrl Pts',(-8.6835916231211,0.188791058808023,
0.434127619986628));
#146840=CARTESIAN_POINT('Ctrl Pts',(-8.69592528214153,-0.283921315905468,
0.435205655554325));
#146841=CARTESIAN_POINT('Ctrl Pts',(-8.74804585570079,-0.516830885578331,
0.439759927270136));
#146842=CARTESIAN_POINT('Ctrl Pts',(-8.88409573697414,-0.826237684498686,
0.451662013470531));
#146843=CARTESIAN_POINT('Ctrl Pts',(-8.93264163468216,-0.915473689865192,
0.455910187711916));
#146844=CARTESIAN_POINT('Ctrl Pts',(-8.9881970991918,-0.9999999998932,0.460774243665518));
#146845=CARTESIAN_POINT('Origin',(1.11022302462516E-15,0.999999999999982,
2.22044604925031E-15));
#146846=CARTESIAN_POINT('Origin',(1.11022302462516E-15,-1.77635683940025E-14,
2.22044604925031E-15));
#146847=CARTESIAN_POINT('',(-8.926027492,-1.00000000000002,1.151535151));
#146848=CARTESIAN_POINT('',(-8.926027492,0.999999999999982,1.151535151));
#146849=CARTESIAN_POINT('Ctrl Pts',(-8.92602749221154,-0.999999999831735,
1.15153515148245));
#146850=CARTESIAN_POINT('Ctrl Pts',(-8.85307990349065,-0.888963444558428,
1.14479106093982));
#146851=CARTESIAN_POINT('Ctrl Pts',(-8.79232723137321,-0.769956469564023,
1.1391706808964));
#146852=CARTESIAN_POINT('Ctrl Pts',(-8.66141907029811,-0.424051722948626,
1.12705657215028));
#146853=CARTESIAN_POINT('Ctrl Pts',(-8.6215592131229,-0.188791058808234,
1.12336414496198));
#146854=CARTESIAN_POINT('Ctrl Pts',(-8.63388715585244,0.283921315908096,
1.1245056937277));
#146855=CARTESIAN_POINT('Ctrl Pts',(-8.68598332696715,0.516830885582066,
1.12933109881079));
#146856=CARTESIAN_POINT('Ctrl Pts',(-8.82197203021842,0.826237684479056,
1.14191292839256));
#146857=CARTESIAN_POINT('Ctrl Pts',(-8.87049631616405,0.915473689823283,
1.14640122881592));
#146858=CARTESIAN_POINT('Ctrl Pts',(-8.92602749221154,0.999999999831699,
1.15153515148245));
#146859=CARTESIAN_POINT('',(-8.910709775,-1.00000000000002,1.264615079));
#146860=CARTESIAN_POINT('Origin',(1.11022302462516E-15,-1.00000000000002,
2.22044604925031E-15));
#146861=CARTESIAN_POINT('',(-8.910709775,0.999999999999982,1.264615079));
#146862=CARTESIAN_POINT('Ctrl Pts',(-8.9107097753288,0.999999999842807,
1.26461507851505));
#146863=CARTESIAN_POINT('Ctrl Pts',(-8.83859683244852,0.888963444565195,
1.25170938491645));
#146864=CARTESIAN_POINT('Ctrl Pts',(-8.7785382846604,0.769956469565655,
1.24096477327833));
#146865=CARTESIAN_POINT('Ctrl Pts',(-8.64912487994753,0.424051722946345,
1.21781592994151));
#146866=CARTESIAN_POINT('Ctrl Pts',(-8.6097191363179,0.18879105880801,1.21077110194113));
#146867=CARTESIAN_POINT('Ctrl Pts',(-8.6219065092898,-0.28392131590536,
1.21295037832583));
#146868=CARTESIAN_POINT('Ctrl Pts',(-8.6734090189736,-0.516830885578178,
1.22215836807797));
#146869=CARTESIAN_POINT('Ctrl Pts',(-8.80784430863259,-0.82623768448008,
1.24620795731554));
#146870=CARTESIAN_POINT('Ctrl Pts',(-8.85581397141432,-0.915473689829693,
1.25479065037675));
#146871=CARTESIAN_POINT('Ctrl Pts',(-8.9107097753288,-0.999999999842844,
1.26461507851505));
#146872=CARTESIAN_POINT('Origin',(1.11022302462516E-15,0.999999999999982,
2.22044604925031E-15));
#146873=CARTESIAN_POINT('Origin',(1.11022302462516E-15,-1.77635683940025E-14,
2.22044604925031E-15));
#146874=CARTESIAN_POINT('',(-8.786871115,-1.00000000000002,1.947022345));
#146875=CARTESIAN_POINT('',(-8.786871115,0.999999999999982,1.947022345));
#146876=CARTESIAN_POINT('Ctrl Pts',(-8.78687111484236,-1.00000000011924,
1.9470223448582));
#146877=CARTESIAN_POINT('Ctrl Pts',(-8.71482172720569,-0.88896344476554,
1.93376643256629));
#146878=CARTESIAN_POINT('Ctrl Pts',(-8.65481743440953,-0.769956469675547,
1.92272285094909));
#146879=CARTESIAN_POINT('Ctrl Pts',(-8.52552217140722,-0.424051722951982,
1.89892299290974));
#146880=CARTESIAN_POINT('Ctrl Pts',(-8.48615376492161,-0.188791058808557,
1.89167242028618));
#146881=CARTESIAN_POINT('Ctrl Pts',(-8.49832975133559,0.283921315912148,
1.89391444178229));
#146882=CARTESIAN_POINT('Ctrl Pts',(-8.54978365260218,0.51683088558783,
1.90339028599331));
#146883=CARTESIAN_POINT('Ctrl Pts',(-8.68409707884375,0.826237684589113,
1.92811139825368));
#146884=CARTESIAN_POINT('Ctrl Pts',(-8.73202369219063,0.91547369002775,
1.9369313135815));
#146885=CARTESIAN_POINT('Ctrl Pts',(-8.78687111484236,1.0000000001192,1.9470223448582));
#146886=CARTESIAN_POINT('',(-8.761478656,-1.00000000000002,2.058273976));
#146887=CARTESIAN_POINT('Origin',(1.11022302462516E-15,-1.00000000000002,
2.22044604925031E-15));
#146888=CARTESIAN_POINT('',(-8.761478656,0.999999999999982,2.058273976));
#146889=CARTESIAN_POINT('Ctrl Pts',(-8.76147865610178,1.00000000003545,
2.05827397542386));
#146890=CARTESIAN_POINT('Ctrl Pts',(-8.69081287612847,0.888963444702555,
2.03895608197732));
#146891=CARTESIAN_POINT('Ctrl Pts',(-8.63195924591628,0.769956469637271,
2.02287111825923));
#146892=CARTESIAN_POINT('Ctrl Pts',(-8.50514186781518,0.424051722945794,
1.9882149371944));
#146893=CARTESIAN_POINT('Ctrl Pts',(-8.4665262536374,0.188791058807997,
1.97766616597551));
#146894=CARTESIAN_POINT('Ctrl Pts',(-8.47846921499966,-0.283921315904604,
1.98092913692443));
#146895=CARTESIAN_POINT('Ctrl Pts',(-8.52893899288346,-0.516830885577124,
1.9947167073906));
#146896=CARTESIAN_POINT('Ctrl Pts',(-8.66067729706199,-0.826237684549968,
2.03072016651486));
#146897=CARTESIAN_POINT('Ctrl Pts',(-8.70768450145157,-0.915473689964894,
2.04356827560746));
#146898=CARTESIAN_POINT('Ctrl Pts',(-8.76147865610178,-1.00000000003548,
2.05827397542386));
#146899=CARTESIAN_POINT('Origin',(1.11022302462516E-15,0.999999999999982,
2.22044604925031E-15));
#146900=CARTESIAN_POINT('Origin',(1.11022302462516E-15,-1.77635683940025E-14,
2.22044604925031E-15));
#146901=CARTESIAN_POINT('',(-8.576968018,-1.00000000000002,2.726833259));
#146902=CARTESIAN_POINT('',(-8.576968018,0.999999999999982,2.726833259));
#146903=CARTESIAN_POINT('Ctrl Pts',(-8.57696801776425,-1.00000000013926,
2.72683325905983));
#146904=CARTESIAN_POINT('Ctrl Pts',(-8.50639693059222,-0.888963444780249,
2.70717225385519));
#146905=CARTESIAN_POINT('Ctrl Pts',(-8.44762413645845,-0.769956469683948,
2.69079438711029));
#146906=CARTESIAN_POINT('Ctrl Pts',(-8.32098278099788,-0.424051722952772,
2.65550040227742));
#146907=CARTESIAN_POINT('Ctrl Pts',(-8.28242279646211,-0.188791058808596,
2.64475006157632));
#146908=CARTESIAN_POINT('Ctrl Pts',(-8.29434879267705,0.283921315913186,
2.64807450436084));
#146909=CARTESIAN_POINT('Ctrl Pts',(-8.34474614753761,0.516830885589286,
2.66212449376052));
#146910=CARTESIAN_POINT('Ctrl Pts',(-8.47630288399607,0.826237684597596,
2.69878584880073));
#146911=CARTESIAN_POINT('Ctrl Pts',(-8.52324594777668,0.91547369004237,
2.71186636624358));
#146912=CARTESIAN_POINT('Ctrl Pts',(-8.57696801776425,1.00000000013922,
2.72683325905983));
#146913=CARTESIAN_POINT('',(-8.541705262,-1.00000000000002,2.835360862));
#146914=CARTESIAN_POINT('Origin',(1.11022302462516E-15,-1.00000000000002,
2.22044604925031E-15));
#146915=CARTESIAN_POINT('',(-8.541705262,0.999999999999982,2.835360862));
#146916=CARTESIAN_POINT('Ctrl Pts',(-8.54170526175661,1.00000000003763,
2.83536086248987));
#146917=CARTESIAN_POINT('Ctrl Pts',(-8.47305560404579,0.888963444707527,
2.80978630556046));
#146918=CARTESIAN_POINT('Ctrl Pts',(-8.41588074626889,0.769956469645605,
2.78849049646969));
#146919=CARTESIAN_POINT('Ctrl Pts',(-8.29268045374403,0.424051722952567,
2.74260600893571));
#146920=CARTESIAN_POINT('Ctrl Pts',(-8.2551658792303,0.18879105880857,2.72863822702008));
#146921=CARTESIAN_POINT('Ctrl Pts',(-8.2667682712839,-0.28392131591296,
2.73295862100442));
#146922=CARTESIAN_POINT('Ctrl Pts',(-8.31579896440192,-0.516830885588963,
2.75121476275007));
#146923=CARTESIAN_POINT('Ctrl Pts',(-8.4437796037284,-0.826237684560064,
2.7988822130079));
#146924=CARTESIAN_POINT('Ctrl Pts',(-8.48944587531942,-0.915473689970771,
2.81589229268048));
#146925=CARTESIAN_POINT('Ctrl Pts',(-8.54170526175661,-1.00000000003766,
2.83536086248987));
#146926=CARTESIAN_POINT('Origin',(1.11022302462516E-15,0.999999999999982,
2.22044604925031E-15));
#146927=CARTESIAN_POINT('Origin',(1.11022302462516E-15,-1.77635683940025E-14,
2.22044604925031E-15));
#146928=CARTESIAN_POINT('',(-8.298008217,-1.00000000000002,3.484689316));
#146929=CARTESIAN_POINT('',(-8.298008217,0.999999999999982,3.484689317));
#146930=CARTESIAN_POINT('Ctrl Pts',(-8.29800821680649,-0.999999999999694,
3.48468931651321));
#146931=CARTESIAN_POINT('Ctrl Pts',(-8.22948362702784,-0.888963444677954,
3.4587815172934));
#146932=CARTESIAN_POINT('Ctrl Pts',(-8.17241553555906,-0.769956469625944,
3.43720123040945));
#146933=CARTESIAN_POINT('Ctrl Pts',(-8.04944772937249,-0.424051722947701,
3.39069728525703));
#146934=CARTESIAN_POINT('Ctrl Pts',(-8.0120066291036,-0.188791058808198,
3.37653373191682));
#146935=CARTESIAN_POINT('Ctrl Pts',(-8.02358661401112,0.28392131590686,
3.38091382952583));
#146936=CARTESIAN_POINT('Ctrl Pts',(-8.07252165260454,0.516830885580335,
3.39942484183956));
#146937=CARTESIAN_POINT('Ctrl Pts',(-8.2002624818134,0.826237684599012,
3.4477312639312));
#146938=CARTESIAN_POINT('Ctrl Pts',(-8.24584403809067,0.915473690055274,
3.4649670668361));
#146939=CARTESIAN_POINT('Ctrl Pts',(-8.29800821690682,1.00000000016222,
3.48468931655114));
#146940=CARTESIAN_POINT('',(-8.253159079,-1.00000000000002,3.58961909));
#146941=CARTESIAN_POINT('Origin',(1.11022302462516E-15,-1.00000000000002,
2.22044604925031E-15));
#146942=CARTESIAN_POINT('',(-8.253159079,0.999999999999982,3.58961909));
#146943=CARTESIAN_POINT('Ctrl Pts',(-8.2531590793014,0.999999999897838,
3.58961908972884));
#146944=CARTESIAN_POINT('Ctrl Pts',(-8.18707827057777,0.888963444607217,
3.55799378058502));
#146945=CARTESIAN_POINT('Ctrl Pts',(-8.13204252360867,0.769956469592236,
3.53165858743165));
#146946=CARTESIAN_POINT('Ctrl Pts',(-8.01345125301592,0.424051722951699,
3.47491522827454));
#146947=CARTESIAN_POINT('Ctrl Pts',(-7.97733976346943,0.188791058808483,
3.45764089600619));
#146948=CARTESIAN_POINT('Ctrl Pts',(-7.98850817057213,-0.283921315911911,
3.46298392776071));
#146949=CARTESIAN_POINT('Ctrl Pts',(-8.03570501260313,-0.51683088558747,
3.48556165309702));
#146950=CARTESIAN_POINT('Ctrl Pts',(-8.15889756217778,-0.826237684507599,
3.54450930427714));
#146951=CARTESIAN_POINT('Ctrl Pts',(-8.20285522296936,-0.915473689871845,
3.56554439938598));
#146952=CARTESIAN_POINT('Ctrl Pts',(-8.2531590793014,-0.999999999897872,
3.58961908972884));
#146953=CARTESIAN_POINT('Origin',(1.11022302462516E-15,0.999999999999982,
2.22044604925031E-15));
#146954=CARTESIAN_POINT('Origin',(1.11022302462516E-15,-1.77635683940025E-14,
2.22044604925031E-15));
#146955=CARTESIAN_POINT('',(-7.952237733,-1.00000000000002,4.214488703));
#146956=CARTESIAN_POINT('',(-7.952237733,0.999999999999982,4.214488703));
#146957=CARTESIAN_POINT('Ctrl Pts',(-7.95223773319635,-0.999999999775504,
4.21448870337516));
#146958=CARTESIAN_POINT('Ctrl Pts',(-7.88631136054351,-0.888963444517433,
4.18254270450202));
#146959=CARTESIAN_POINT('Ctrl Pts',(-7.83140745047794,-0.769956469541135,
4.15593374925552));
#146960=CARTESIAN_POINT('Ctrl Pts',(-7.71310325805549,-0.424051722947019,
4.0985942661749));
#146961=CARTESIAN_POINT('Ctrl Pts',(-7.6770824957803,-0.188791058808112,
4.08113153678696));
#146962=CARTESIAN_POINT('Ctrl Pts',(-7.68822323415081,0.283921315906088,
4.08653202325389));
#146963=CARTESIAN_POINT('Ctrl Pts',(-7.7353019603166,0.516830885579229,
4.10935501871067));
#146964=CARTESIAN_POINT('Ctrl Pts',(-7.85819838815941,0.826237684456182,
4.1689175729596));
#146965=CARTESIAN_POINT('Ctrl Pts',(-7.90205144095589,0.915473689782662,
4.19016988875141));
#146966=CARTESIAN_POINT('Ctrl Pts',(-7.95223773319635,0.999999999775469,
4.21448870337516));
#146967=CARTESIAN_POINT('',(-7.898163313,-1.00000000000002,4.314975815));
#146968=CARTESIAN_POINT('Origin',(1.11022302462516E-15,-1.00000000000002,
2.22044604925031E-15));
#146969=CARTESIAN_POINT('',(-7.898163313,0.999999999999982,4.314975815));
#146970=CARTESIAN_POINT('Ctrl Pts',(-7.89816331271264,1.00000000009806,
4.31497581519263));
#146971=CARTESIAN_POINT('Ctrl Pts',(-7.83518339669397,0.888963444751888,
4.277554382208));
#146972=CARTESIAN_POINT('Ctrl Pts',(-7.78272987593037,0.769956469670872,
4.24639184046861));
#146973=CARTESIAN_POINT('Ctrl Pts',(-7.66970245438489,0.424051722954907,
4.17924647387126));
#146974=CARTESIAN_POINT('Ctrl Pts',(-7.63528479827936,0.188791058808747,
4.15880467402877));
#146975=CARTESIAN_POINT('Ctrl Pts',(-7.64592929898681,-0.283921315915896,
4.16512732459995));
#146976=CARTESIAN_POINT('Ctrl Pts',(-7.69091228871914,-0.51683088559311,
4.19184485094197));
#146977=CARTESIAN_POINT('Ctrl Pts',(-7.80832487464018,-0.826237684585493,
4.26159809119923));
#146978=CARTESIAN_POINT('Ctrl Pts',(-7.85022000346807,-0.915473690014822,
4.28648883954432));
#146979=CARTESIAN_POINT('Ctrl Pts',(-7.89816331271264,-1.00000000009809,
4.31497581519263));
#146980=CARTESIAN_POINT('Origin',(1.11022302462516E-15,0.999999999999982,
2.22044604925031E-15));
#146981=CARTESIAN_POINT('Origin',(1.11022302462516E-15,-1.77635683940025E-14,
2.22044604925031E-15));
#146982=CARTESIAN_POINT('',(-7.542440507,-1.00000000000002,4.910355505));
#146983=CARTESIAN_POINT('',(-7.542440507,0.999999999999982,4.910355506));
#146984=CARTESIAN_POINT('Ctrl Pts',(-7.54244050699415,-0.999999999713363,
4.91035550585342));
#146985=CARTESIAN_POINT('Ctrl Pts',(-7.47964315180284,-0.888963444471708,
4.87262851771894));
#146986=CARTESIAN_POINT('Ctrl Pts',(-7.42734547710069,-0.769956469514917,
4.84120513376689));
#146987=CARTESIAN_POINT('Ctrl Pts',(-7.31465741420512,-0.424051722944422,
4.77349177656748));
#146988=CARTESIAN_POINT('Ctrl Pts',(-7.28034700791849,-0.18879105880793,
4.75287047076504));
#146989=CARTESIAN_POINT('Ctrl Pts',(-7.29095880107796,0.283921315902793,
4.75924786454684));
#146990=CARTESIAN_POINT('Ctrl Pts',(-7.33580216459887,0.516830885574576,
4.78619908580148));
#146991=CARTESIAN_POINT('Ctrl Pts',(-7.4528647013947,0.82623768451662,4.85653820956603));
#146992=CARTESIAN_POINT('Ctrl Pts',(-7.49463617183292,0.915473689903834,
4.88163592714012));
#146993=CARTESIAN_POINT('Ctrl Pts',(-7.54244050712803,0.999999999950053,
4.91035550593385));
#146994=CARTESIAN_POINT('',(-7.47957618,-1.00000000000002,5.005590891));
#146995=CARTESIAN_POINT('Origin',(1.11022302462516E-15,-1.00000000000002,
2.22044604925031E-15));
#146996=CARTESIAN_POINT('',(-7.47957618,0.999999999999982,5.005590891));
#146997=CARTESIAN_POINT('Ctrl Pts',(-7.47957617982888,1.00000000003923,
5.00559089113518));
#146998=CARTESIAN_POINT('Ctrl Pts',(-7.42020423385493,0.888963444707323,
4.96267462967732));
#146999=CARTESIAN_POINT('Ctrl Pts',(-7.37075526427221,0.769956469643229,
4.92693564180633));
#147000=CARTESIAN_POINT('Ctrl Pts',(-7.2642017221897,0.4240517229499,4.84992888272496));
#147001=CARTESIAN_POINT('Ctrl Pts',(-7.2317550102686,0.188791058808352,
4.82648420063956));
#147002=CARTESIAN_POINT('Ctrl Pts',(-7.24178990131453,-0.283921315909654,
4.83373556376861));
#147003=CARTESIAN_POINT('Ctrl Pts',(-7.28419686214626,-0.516830885584279,
4.8643777773319));
#147004=CARTESIAN_POINT('Ctrl Pts',(-7.39488414722774,-0.826237684556974,
4.94437499464598));
#147005=CARTESIAN_POINT('Ctrl Pts',(-7.43437942908497,-0.915473689970183,
4.9729209905592));
#147006=CARTESIAN_POINT('Ctrl Pts',(-7.47957617982888,-1.00000000003927,
5.00559089113518));
#147007=CARTESIAN_POINT('Origin',(1.11022302462516E-15,0.999999999999982,
2.22044604925031E-15));
#147008=CARTESIAN_POINT('Origin',(1.11022302462516E-15,-1.77635683940025E-14,
2.22044604925031E-15));
#147009=CARTESIAN_POINT('',(-7.071915986,-1.00000000000002,5.566687012));
#147010=CARTESIAN_POINT('',(-7.071915985,0.999999999999982,5.566687013));
#147011=CARTESIAN_POINT('Ctrl Pts',(-7.07191598537279,-1.00000000011093,
5.56668701257385));
#147012=CARTESIAN_POINT('Ctrl Pts',(-7.01275325493728,-0.888963444757717,
5.52348279059388));
#147013=CARTESIAN_POINT('Ctrl Pts',(-6.96348288566105,-0.76995646966828,
5.48749798046137));
#147014=CARTESIAN_POINT('Ctrl Pts',(-6.85731825030078,-0.424051722948235,
5.40995593718119));
#147015=CARTESIAN_POINT('Ctrl Pts',(-6.82499444723148,-0.188791058808213,
5.38634208557447));
#147016=CARTESIAN_POINT('Ctrl Pts',(-6.83499185525838,0.283921315907589,
5.39364503965271));
#147017=CARTESIAN_POINT('Ctrl Pts',(-6.87723880372388,0.516830885581356,
5.42450749134371));
#147018=CARTESIAN_POINT('Ctrl Pts',(-6.98752493069895,0.826237684544213,
5.50505685541549));
#147019=CARTESIAN_POINT('Ctrl Pts',(-7.02687849941884,0.915473689949042,
5.53379790271954));
#147020=CARTESIAN_POINT('Ctrl Pts',(-7.07191598531943,1.00000000001076,
5.56668701253488));
#147021=CARTESIAN_POINT('',(-7.000767897,-1.00000000000002,5.655903894));
#147022=CARTESIAN_POINT('Origin',(1.11022302462516E-15,-1.00000000000002,
2.22044604925031E-15));
#147023=CARTESIAN_POINT('',(-7.000767897,0.999999999999982,5.655903894));
#147024=CARTESIAN_POINT('Ctrl Pts',(-7.00076789681103,1.00000000017972,
5.65590389380216));
#147025=CARTESIAN_POINT('Ctrl Pts',(-6.94548194883083,0.888963444807022,
5.60783834035334));
#147026=CARTESIAN_POINT('Ctrl Pts',(-6.89943566441819,0.76995646969442,
5.56781065565214));
#147027=CARTESIAN_POINT('Ctrl Pts',(-6.8002139082344,0.42405172294853,5.48156251723961));
#147028=CARTESIAN_POINT('Ctrl Pts',(-6.76999938234043,0.188791058808214,
5.4553037157138));
#147029=CARTESIAN_POINT('Ctrl Pts',(-6.77934386868416,-0.283921315908009,
5.46342540768646));
#147030=CARTESIAN_POINT('Ctrl Pts',(-6.818833364706,-0.516830885581938,
5.49774559537489));
#147031=CARTESIAN_POINT('Ctrl Pts',(-6.92190416004712,-0.826237684606702,
5.58734269918266));
#147032=CARTESIAN_POINT('Ctrl Pts',(-6.958681602184,-0.915473690068199,
5.61931410710659));
#147033=CARTESIAN_POINT('Ctrl Pts',(-7.00076789681103,-1.00000000017975,
5.65590389380216));
#147034=CARTESIAN_POINT('Origin',(1.11022302462516E-15,0.999999999999982,
2.22044604925031E-15));
#147035=CARTESIAN_POINT('Origin',(1.11022302462516E-15,-1.77635683940025E-14,
2.22044604925031E-15));
#147036=CARTESIAN_POINT('',(-6.544452554,-1.00000000000002,6.178198829));
#147037=CARTESIAN_POINT('',(-6.544452554,0.999999999999982,6.178198829));
#147038=CARTESIAN_POINT('Ctrl Pts',(-6.54445255416351,-1.0000000000805,
6.17819882862887));
#147039=CARTESIAN_POINT('Ctrl Pts',(-6.4894007921,-0.88896344473667,6.12986522787584));
#147040=CARTESIAN_POINT('Ctrl Pts',(-6.44355442436669,-0.769956469658397,
6.08960872015794));
#147041=CARTESIAN_POINT('Ctrl Pts',(-6.34476799180017,-0.424051722949622,
6.00286231379506));
#147042=CARTESIAN_POINT('Ctrl Pts',(-6.31469104420046,-0.188791058808342,
5.97644604124084));
#147043=CARTESIAN_POINT('Ctrl Pts',(-6.32399357384458,0.283921315909262,
5.98461575652057));
#147044=CARTESIAN_POINT('Ctrl Pts',(-6.36330395967153,0.516830885583727,
6.01914095232269));
#147045=CARTESIAN_POINT('Ctrl Pts',(-6.46592571779309,0.826237684571677,
6.10925202055845));
#147046=CARTESIAN_POINT('Ctrl Pts',(-6.50254453300505,0.915473689998982,
6.14140499157264));
#147047=CARTESIAN_POINT('Ctrl Pts',(-6.54445255416351,1.00000000008046,
6.17819882862886));
#147048=CARTESIAN_POINT('',(-6.465593548,-1.00000000000002,6.260678883));
#147049=CARTESIAN_POINT('Origin',(1.11022302462516E-15,-1.00000000000002,
2.22044604925031E-15));
#147050=CARTESIAN_POINT('',(-6.465593547,0.999999999999982,6.260678883));
#147051=CARTESIAN_POINT('Ctrl Pts',(-6.46559354762128,0.999999999811353,
6.26067888279958));
#147052=CARTESIAN_POINT('Ctrl Pts',(-6.41483872768217,0.888963444543266,
6.20785103304572));
#147053=CARTESIAN_POINT('Ctrl Pts',(-6.37256586612412,0.769956469555061,
6.1638569309814));
#147054=CARTESIAN_POINT('Ctrl Pts',(-6.28147477111903,0.424051722947448,
6.06906183260181));
#147055=CARTESIAN_POINT('Ctrl Pts',(-6.25373570084517,0.188791058808131,
6.04020033207072));
#147056=CARTESIAN_POINT('Ctrl Pts',(-6.26231454617831,-0.283921315906657,
6.04912696179709));
#147057=CARTESIAN_POINT('Ctrl Pts',(-6.29856863119255,-0.516830885580028,
6.08684879763255));
#147058=CARTESIAN_POINT('Ctrl Pts',(-6.39319307134218,-0.826237684586883,
6.18532440469952));
#147059=CARTESIAN_POINT('Ctrl Pts',(-6.42695656339071,-0.91547369003238,
6.22046380962379));
#147060=CARTESIAN_POINT('Ctrl Pts',(-6.46559354776686,-1.00000000012986,
6.26067888295109));
#147061=CARTESIAN_POINT('Origin',(1.11022302462516E-15,0.999999999999982,
2.22044604925031E-15));
#147062=CARTESIAN_POINT('Origin',(1.11022302462516E-15,-1.77635683940025E-14,
2.22044604925031E-15));
#147063=CARTESIAN_POINT('',(-5.964297039,-1.00000000000002,6.739967421));
#147064=CARTESIAN_POINT('',(-5.964297039,0.999999999999982,6.73996742));
#147065=CARTESIAN_POINT('Ctrl Pts',(-5.96429703935934,-1.00000000016049,
6.73996742032238));
#147066=CARTESIAN_POINT('Ctrl Pts',(-5.91379949005691,-0.888963444794064,
6.68689359451439));
#147067=CARTESIAN_POINT('Ctrl Pts',(-5.87174625183969,-0.769956469688926,
6.64268951092948));
#147068=CARTESIAN_POINT('Ctrl Pts',(-5.78113339231567,-0.424051722950078,
6.54743717254365));
#147069=CARTESIAN_POINT('Ctrl Pts',(-5.75354546207987,-0.188791058808362,
6.51843116733989));
#147070=CARTESIAN_POINT('Ctrl Pts',(-5.76207821484306,0.283921315909882,
6.52740186607612));
#147071=CARTESIAN_POINT('Ctrl Pts',(-5.79813553392257,0.516830885584602,
6.56531182940825));
#147072=CARTESIAN_POINT('Ctrl Pts',(-5.89226667310739,0.826237684479476,
6.66425908042156));
#147073=CARTESIAN_POINT('Ctrl Pts',(-5.92585590159545,0.915473689821207,
6.69956509827457));
#147074=CARTESIAN_POINT('Ctrl Pts',(-5.96429703920789,0.999999999827432,
6.7399674201632));
#147075=CARTESIAN_POINT('',(-5.87836204,-1.00000000000002,6.815046568));
#147076=CARTESIAN_POINT('Origin',(1.11022302462516E-15,-1.00000000000002,
2.22044604925031E-15));
#147077=CARTESIAN_POINT('',(-5.87836204,0.999999999999982,6.815046568));
#147078=CARTESIAN_POINT('Ctrl Pts',(-5.87836203971057,0.999999999954792,
6.81504656831974));
#147079=CARTESIAN_POINT('Ctrl Pts',(-5.8325469956454,0.888963444648911,
6.75788176096771));
#147080=CARTESIAN_POINT('Ctrl Pts',(-5.79438791306314,0.769956469615795,
6.71027545612482));
#147081=CARTESIAN_POINT('Ctrl Pts',(-5.7121608910693,0.424051722953674,
6.60769663216305));
#147082=CARTESIAN_POINT('Ctrl Pts',(-5.68712061508326,0.188791058808645,
6.57646480847093));
#147083=CARTESIAN_POINT('Ctrl Pts',(-5.69486474759318,-0.28392131591436,
6.58612450397438));
#147084=CARTESIAN_POINT('Ctrl Pts',(-5.72759152504513,-0.516830885590938,
6.62694427389891));
#147085=CARTESIAN_POINT('Ctrl Pts',(-5.81300774969049,-0.826237684531225,
6.73350551647852));
#147086=CARTESIAN_POINT('Ctrl Pts',(-5.84348544786606,-0.915473689913203,
6.77152999653492));
#147087=CARTESIAN_POINT('Ctrl Pts',(-5.87836203971057,-0.999999999954829,
6.81504656831974));
#147088=CARTESIAN_POINT('Origin',(1.11022302462516E-15,0.999999999999982,
2.22044604925031E-15));
#147089=CARTESIAN_POINT('Origin',(1.11022302462516E-15,-1.77635683940025E-14,
2.22044604925031E-15));
#147090=CARTESIAN_POINT('',(-5.336120511,-1.00000000000002,7.247469758));
#147091=CARTESIAN_POINT('',(-5.33612051,0.999999999999982,7.247469758));
#147092=CARTESIAN_POINT('Ctrl Pts',(-5.3361205102212,-1.00000000007198,
7.24746975847874));
#147093=CARTESIAN_POINT('Ctrl Pts',(-5.29058375025361,-0.888963444727199,
7.1900830269119));
#147094=CARTESIAN_POINT('Ctrl Pts',(-5.25266222949664,-0.769956469647752,
7.14228727279496));
#147095=CARTESIAN_POINT('Ctrl Pts',(-5.17095250443963,-0.424051722942908,
7.03929591826979));
#147096=CARTESIAN_POINT('Ctrl Pts',(-5.14607571334354,-0.18879105880776,
7.00793371972911));
#147097=CARTESIAN_POINT('Ctrl Pts',(-5.15376998852218,0.283921315901019,
7.01763317512498));
#147098=CARTESIAN_POINT('Ctrl Pts',(-5.18628392854453,0.516830885572041,
7.05862267723458));
#147099=CARTESIAN_POINT('Ctrl Pts',(-5.27116656029511,0.826237684454485,
7.16560944591632));
#147100=CARTESIAN_POINT('Ctrl Pts',(-5.30145576140191,0.915473689787588,
7.20378424732816));
#147101=CARTESIAN_POINT('Ctrl Pts',(-5.33612051010402,0.999999999786214,
7.24746975833107));
#147102=CARTESIAN_POINT('',(-5.243801419,-1.00000000000002,7.314543504));
#147103=CARTESIAN_POINT('Origin',(1.11022302462516E-15,-1.00000000000002,
2.22044604925031E-15));
#147104=CARTESIAN_POINT('',(-5.243801419,0.999999999999982,7.314543505));
#147105=CARTESIAN_POINT('Ctrl Pts',(-5.24380141936077,1.00000000025758,
7.31454350429201));
#147106=CARTESIAN_POINT('Ctrl Pts',(-5.20329502701867,0.888963444859877,
7.25350199664625));
#147107=CARTESIAN_POINT('Ctrl Pts',(-5.16955695795366,0.769956469717498,
7.20266678690975));
#147108=CARTESIAN_POINT('Ctrl Pts',(-5.09685605273471,0.424051722943015,
7.09313014161181));
#147109=CARTESIAN_POINT('Ctrl Pts',(-5.07471618065861,0.188791058807757,
7.05977945500723));
#147110=CARTESIAN_POINT('Ctrl Pts',(-5.08156324912865,-0.283921315901173,
7.07009444210697));
#147111=CARTESIAN_POINT('Ctrl Pts',(-5.11049922219243,-0.516830885572257,
7.113683489376));
#147112=CARTESIAN_POINT('Ctrl Pts',(-5.18601950998405,-0.826237684487118,
7.22747239912401));
#147113=CARTESIAN_POINT('Ctrl Pts',(-5.21296602575132,-0.915473689849885,
7.26807580361716));
#147114=CARTESIAN_POINT('Ctrl Pts',(-5.24380141922105,-0.999999999874601,
7.31454350408145));
#147115=CARTESIAN_POINT('Origin',(1.11022302462516E-15,0.999999999999982,
2.22044604925031E-15));
#147116=CARTESIAN_POINT('Origin',(1.11022302462516E-15,-1.77635683940025E-14,
2.22044604925031E-15));
#147117=CARTESIAN_POINT('',(-4.664980679,-1.00000000000002,7.69661973));
#147118=CARTESIAN_POINT('',(-4.664980679,0.999999999999982,7.69661973));
#147119=CARTESIAN_POINT('Ctrl Pts',(-4.6649806790278,-1.00000000012154,
7.69661972976142));
#147120=CARTESIAN_POINT('Ctrl Pts',(-4.62477134369037,-0.888963444769277,
7.6353821365611));
#147121=CARTESIAN_POINT('Ctrl Pts',(-4.59128686224838,-0.769956469681022,
7.58437953514422));
#147122=CARTESIAN_POINT('Ctrl Pts',(-4.51913815048226,-0.424051722956112,
7.47447839016348));
#147123=CARTESIAN_POINT('Ctrl Pts',(-4.49717279187257,-0.188791058808881,
7.44101250822753));
#147124=CARTESIAN_POINT('Ctrl Pts',(-4.50396663967298,0.283921315917288,
7.45136262598659));
#147125=CARTESIAN_POINT('Ctrl Pts',(-4.53267541744312,0.516830885595098,
7.49510164355728));
#147126=CARTESIAN_POINT('Ctrl Pts',(-4.60762611656943,0.826237684595678,
7.609266535536));
#147127=CARTESIAN_POINT('Ctrl Pts',(-4.6343714194336,0.915473690032038,
7.65000275956128));
#147128=CARTESIAN_POINT('Ctrl Pts',(-4.6649806790278,1.00000000012149,7.69661972976142));
#147129=CARTESIAN_POINT('',(-4.567020791,-1.00000000000002,7.755148038));
#147130=CARTESIAN_POINT('Origin',(1.11022302462516E-15,-1.00000000000002,
2.22044604925031E-15));
#147131=CARTESIAN_POINT('',(-4.56702079017615,1.00000000014985,7.75514803858119));
#147132=CARTESIAN_POINT('Ctrl Pts',(-4.56702079103465,1.0000000001046,7.7551480381945));
#147133=CARTESIAN_POINT('Ctrl Pts',(-4.53214918409692,0.888963444751377,
7.69072130073945));
#147134=CARTESIAN_POINT('Ctrl Pts',(-4.50310376766113,0.769956469661912,
7.63706648144992));
#147135=CARTESIAN_POINT('Ctrl Pts',(-4.44051432410009,0.42405172294464,
7.5214539396054));
#147136=CARTESIAN_POINT('Ctrl Pts',(-4.42145311313639,0.188791058807904,
7.48625291022913));
#147137=CARTESIAN_POINT('Ctrl Pts',(-4.42734798900763,-0.283921315903176,
7.49714013870893));
#147138=CARTESIAN_POINT('Ctrl Pts',(-4.45226018228089,-0.516830885575103,
7.54314750991512));
#147139=CARTESIAN_POINT('Ctrl Pts',(-4.5172764883787,-0.826237684515357,
7.66324792537743));
#147140=CARTESIAN_POINT('Ctrl Pts',(-4.5404748642876,-0.915473689900839,
7.7061033395637));
#147141=CARTESIAN_POINT('Ctrl Pts',(-4.56702079098469,-0.999999999945533,
7.75514803810219));
#147142=CARTESIAN_POINT('Origin',(1.11022302462516E-15,0.999999999999982,
2.22044604925031E-15));
#147143=CARTESIAN_POINT('Origin',(1.11022302462516E-15,-1.77635683940025E-14,
2.22044604925031E-15));
#147144=CARTESIAN_POINT('',(-3.956281164,-1.00000000000002,8.083801046));
#147145=CARTESIAN_POINT('',(-3.956281165,0.999999999999982,8.083801046));
#147146=CARTESIAN_POINT('Ctrl Pts',(-3.95628116468507,-1.00000000001549,
8.08380104560689));
#147147=CARTESIAN_POINT('Ctrl Pts',(-3.92172299585936,-0.888963444693512,
8.01920563994907));
#147148=CARTESIAN_POINT('Ctrl Pts',(-3.89294515105064,-0.769956469641267,
7.96540683425602));
#147149=CARTESIAN_POINT('Ctrl Pts',(-3.83093835147929,-0.424051722956145,
7.84948075832601));
#147150=CARTESIAN_POINT('Ctrl Pts',(-3.81206127747473,-0.188791058808899,
7.81418064062606));
#147151=CARTESIAN_POINT('Ctrl Pts',(-3.81789999783811,0.28392131591731,
7.82509808767561));
#147152=CARTESIAN_POINT('Ctrl Pts',(-3.84257246720139,0.516830885595139,
7.87123445981979));
#147153=CARTESIAN_POINT('Ctrl Pts',(-3.90698777483688,0.826237684636356,
7.99165828639558));
#147154=CARTESIAN_POINT('Ctrl Pts',(-3.92997384201674,0.915473690110029,
8.03462794884641));
#147155=CARTESIAN_POINT('Ctrl Pts',(-3.95628116475256,1.0000000002323,8.08380104573304));
#147156=CARTESIAN_POINT('',(-3.853469197,-1.00000000000002,8.133312679));
#147157=CARTESIAN_POINT('Origin',(1.11022302462516E-15,-1.00000000000002,
2.22044604925031E-15));
#147158=CARTESIAN_POINT('',(-3.853469197,0.999999999999982,8.13331268));
#147159=CARTESIAN_POINT('Ctrl Pts',(-3.85346919706807,1.0000000001062,8.13331267979544));
#147160=CARTESIAN_POINT('Ctrl Pts',(-3.82451314113869,0.888963444756583,
8.06601943872399));
#147161=CARTESIAN_POINT('Ctrl Pts',(-3.80039423388956,0.769956469671448,
8.00997700692796));
#147162=CARTESIAN_POINT('Ctrl Pts',(-3.74842018528738,0.424051722952648,
7.88921941276123));
#147163=CARTESIAN_POINT('Ctrl Pts',(-3.73259110507324,0.188791058808531,
7.85245145861415));
#147164=CARTESIAN_POINT('Ctrl Pts',(-3.73748632627966,-0.283921315913158,
7.86382327090975));
#147165=CARTESIAN_POINT('Ctrl Pts',(-3.758174161464,-0.51683088558922,7.91187854173883));
#147166=CARTESIAN_POINT('Ctrl Pts',(-3.81216301286461,-0.826237684430458,
8.0373234849023));
#147167=CARTESIAN_POINT('Ctrl Pts',(-3.83142646923125,-0.915473689721949,
8.08208586210271));
#147168=CARTESIAN_POINT('Ctrl Pts',(-3.85346919695796,-0.999999999683992,
8.13331267953955));
#147169=CARTESIAN_POINT('Origin',(1.11022302462516E-15,0.999999999999982,
2.22044604925031E-15));
#147170=CARTESIAN_POINT('Origin',(1.11022302462516E-15,-1.77635683940025E-14,
2.22044604925031E-15));
#147171=CARTESIAN_POINT('',(-3.215728,-1.00000000000002,8.405896349));
#147172=CARTESIAN_POINT('',(-3.215728,0.999999999999982,8.405896349));
#147173=CARTESIAN_POINT('Ctrl Pts',(-3.21572799910164,-1.00000000004898,
8.40589634930078));
#147174=CARTESIAN_POINT('Ctrl Pts',(-3.18709923874645,-0.888963444711017,
8.33846321539938));
#147175=CARTESIAN_POINT('Ctrl Pts',(-3.16325973277762,-0.769956469639689,
8.28230136177404));
#147176=CARTESIAN_POINT('Ctrl Pts',(-3.11189408755156,-0.424051722943413,
8.16128372353288));
#147177=CARTESIAN_POINT('Ctrl Pts',(-3.09625728521347,-0.188791058807823,
8.12443358587799));
#147178=CARTESIAN_POINT('Ctrl Pts',(-3.10109386820782,0.283921315901608,
8.13583046134637));
#147179=CARTESIAN_POINT('Ctrl Pts',(-3.12153138099901,0.516830885572894,
8.18399272510012));
#147180=CARTESIAN_POINT('Ctrl Pts',(-3.17489266307678,0.82623768455158,
8.30970590433158));
#147181=CARTESIAN_POINT('Ctrl Pts',(-3.19393442429636,0.915473689972812,
8.35456303867883));
#147182=CARTESIAN_POINT('Ctrl Pts',(-3.21572799910164,1.00000000004894,
8.40589634930078));
#147183=CARTESIAN_POINT('',(-3.108891736,-1.00000000000002,8.445992669));
#147184=CARTESIAN_POINT('Origin',(1.11022302462516E-15,-1.00000000000002,
2.22044604925031E-15));
#147185=CARTESIAN_POINT('',(-3.108891736,0.999999999999982,8.44599267));
#147186=CARTESIAN_POINT('Ctrl Pts',(-3.10889173624931,1.00000000023756,
8.44599266953942));
#147187=CARTESIAN_POINT('Ctrl Pts',(-3.08608436854417,0.888963444846536,
8.37637473037447));
#147188=CARTESIAN_POINT('Ctrl Pts',(-3.06708616180808,0.769956469712122,
8.31839590671147));
#147189=CARTESIAN_POINT('Ctrl Pts',(-3.0261459728075,0.424051722944941,
8.19346552927423));
#147190=CARTESIAN_POINT('Ctrl Pts',(-3.01367646984111,0.188791058807912,
8.15542668428226));
#147191=CARTESIAN_POINT('Ctrl Pts',(-3.01753262292282,-0.283921315903578,
8.16719152125183));
#147192=CARTESIAN_POINT('Ctrl Pts',(-3.03382953366587,-0.51683088557566,
8.21690777894712));
#147193=CARTESIAN_POINT('Ctrl Pts',(-3.07635624373367,-0.826237684462668,
8.34668724102495));
#147194=CARTESIAN_POINT('Ctrl Pts',(-3.09152968251005,-0.915473689799155,
8.39299618100886));
#147195=CARTESIAN_POINT('Ctrl Pts',(-3.10889173615958,-0.999999999800759,
8.44599266926553));
#147196=CARTESIAN_POINT('Origin',(1.11022302462516E-15,0.999999999999982,
2.22044604925031E-15));
#147197=CARTESIAN_POINT('Origin',(1.11022302462516E-15,-1.77635683940025E-14,
2.22044604925031E-15));
#147198=CARTESIAN_POINT('',(-2.449283685,-1.00000000000002,8.660312317));
#147199=CARTESIAN_POINT('',(-2.449283685,0.999999999999982,8.660312317));
#147200=CARTESIAN_POINT('Ctrl Pts',(-2.44928368492003,-0.999999999970374,
8.66031231707298));
#147201=CARTESIAN_POINT('Ctrl Pts',(-2.42681483511176,-0.888963444658655,
8.5905843868621));
#147202=CARTESIAN_POINT('Ctrl Pts',(-2.40810560977551,-0.769956469618574,
8.53251166751632));
#147203=CARTESIAN_POINT('Ctrl Pts',(-2.36779468507834,-0.424051722950929,
8.40737682975315));
#147204=CARTESIAN_POINT('Ctrl Pts',(-2.35552405280636,-0.188791058808435,
8.36927336775524));
#147205=CARTESIAN_POINT('Ctrl Pts',(-2.35931955709161,0.283921315910924,
8.3810579107145));
#147206=CARTESIAN_POINT('Ctrl Pts',(-2.37535756239453,0.516830885586079,
8.4308582918873));
#147207=CARTESIAN_POINT('Ctrl Pts',(-2.41723518504276,0.826237684533093,
8.56084865527989));
#147208=CARTESIAN_POINT('Ctrl Pts',(-2.4321793271706,0.915473689922331,
8.6072320982976));
#147209=CARTESIAN_POINT('Ctrl Pts',(-2.44928368492003,0.999999999970338,
8.66031231707298));
#147210=CARTESIAN_POINT('',(-2.339283306,-1.00000000000002,8.690670493));
#147211=CARTESIAN_POINT('Origin',(1.11022302462516E-15,-1.00000000000002,
2.22044604925031E-15));
#147212=CARTESIAN_POINT('',(-2.339283305,0.999999999999982,8.690670493));
#147213=CARTESIAN_POINT('Ctrl Pts',(-2.33928330561053,1.00000000001403,
8.69067049283724));
#147214=CARTESIAN_POINT('Ctrl Pts',(-2.322808257611,0.888963444688627,8.61928837841982));
#147215=CARTESIAN_POINT('Ctrl Pts',(-2.30908371374843,0.769956469632263,
8.55983997438751));
#147216=CARTESIAN_POINT('Ctrl Pts',(-2.27950701057719,0.424051722948508,
8.4317426797122));
#147217=CARTESIAN_POINT('Ctrl Pts',(-2.27049748192908,0.188791058808201,
8.39273921030103));
#147218=CARTESIAN_POINT('Ctrl Pts',(-2.27328351942049,-0.283921315908011,
8.40480234839289));
#147219=CARTESIAN_POINT('Ctrl Pts',(-2.28505829262577,-0.516830885581936,
8.45577930686427));
#147220=CARTESIAN_POINT('Ctrl Pts',(-2.31578046142091,-0.826237684583821,
8.58884837992318));
#147221=CARTESIAN_POINT('Ctrl Pts',(-2.32674171504669,-0.91547369002434,
8.63633103035859));
#147222=CARTESIAN_POINT('Ctrl Pts',(-2.33928330562587,-1.00000000011744,
8.6906704929037));
#147223=CARTESIAN_POINT('Origin',(1.11022302462516E-15,0.999999999999982,
2.22044604925031E-15));
#147224=CARTESIAN_POINT('Origin',(1.11022302462516E-15,-1.77635683940025E-14,
2.22044604925031E-15));
#147225=CARTESIAN_POINT('',(-1.663119178,-1.00000000000002,8.845000543));
#147226=CARTESIAN_POINT('',(-1.663119178,0.999999999999982,8.845000543));
#147227=CARTESIAN_POINT('Ctrl Pts',(-1.66311917835389,-1.00000000017415,
8.84500054264958));
#147228=CARTESIAN_POINT('Ctrl Pts',(-1.64699114496605,-0.888963444802729,
8.77353922436293));
#147229=CARTESIAN_POINT('Ctrl Pts',(-1.6335628358678,-0.769956469691642,
8.7140232066417));
#147230=CARTESIAN_POINT('Ctrl Pts',(-1.60463119142804,-0.424051722947916,
8.58577868149686));
#147231=CARTESIAN_POINT('Ctrl Pts',(-1.5958255251009,-0.188791058808179,
8.54672868184127));
#147232=CARTESIAN_POINT('Ctrl Pts',(-1.59854939151922,0.283921315907216,
8.55880601007475));
#147233=CARTESIAN_POINT('Ctrl Pts',(-1.61005876079405,0.516830885580825,
8.6098435452613));
#147234=CARTESIAN_POINT('Ctrl Pts',(-1.64011555016048,0.826237684603746,
8.7430644868424));
#147235=CARTESIAN_POINT('Ctrl Pts',(-1.65084175181584,0.915473690063816,
8.79060078636947));
#147236=CARTESIAN_POINT('Ctrl Pts',(-1.66311917835389,1.00000000017411,
8.84500054264958));
#147237=CARTESIAN_POINT('',(-1.550840341,-1.00000000000002,8.865376147));
#147238=CARTESIAN_POINT('Origin',(1.11022302462516E-15,-1.00000000000002,
2.22044604925031E-15));
#147239=CARTESIAN_POINT('',(-1.550840341,0.999999999999982,8.865376147));
#147240=CARTESIAN_POINT('Ctrl Pts',(-1.55084034140624,0.999999999808246,
8.86537614723733));
#147241=CARTESIAN_POINT('Ctrl Pts',(-1.54083026051303,0.88896344454227,
8.7928045843712));
#147242=CARTESIAN_POINT('Ctrl Pts',(-1.53248988148326,0.769956469556594,
8.73236524355607));
#147243=CARTESIAN_POINT('Ctrl Pts',(-1.51451479838375,0.424051722949868,
8.60213239572782));
#147244=CARTESIAN_POINT('Ctrl Pts',(-1.50903778348876,0.188791058808319,
8.56247833489648));
#147245=CARTESIAN_POINT('Ctrl Pts',(-1.51073127385161,-0.283921315909671,
8.57474264881631));
#147246=CARTESIAN_POINT('Ctrl Pts',(-1.51788910595866,-0.516830885584286,
8.62656987157201));
#147247=CARTESIAN_POINT('Ctrl Pts',(-1.53655937659347,-0.82623768447221,
8.76185716159184));
#147248=CARTESIAN_POINT('Ctrl Pts',(-1.54322019145936,-0.915473689807616,
8.81013121996666));
#147249=CARTESIAN_POINT('Ctrl Pts',(-1.55084034140624,-0.999999999808279,
8.86537614723733));
#147250=CARTESIAN_POINT('Origin',(1.11022302462516E-15,0.999999999999982,
2.22044604925031E-15));
#147251=CARTESIAN_POINT('Origin',(1.11022302462516E-15,-1.77635683940025E-14,
2.22044604925031E-15));
#147252=CARTESIAN_POINT('',(-0.863564212999999,-1.00000000000002,8.958474025));
#147253=CARTESIAN_POINT('',(-0.863564212999999,0.999999999999982,8.958474025));
#147254=CARTESIAN_POINT('Ctrl Pts',(-0.863564213524501,-1.00000000018892,
8.95847402464142));
#147255=CARTESIAN_POINT('Ctrl Pts',(-0.853906850043781,-0.888963444813406,
8.88585468284159));
#147256=CARTESIAN_POINT('Ctrl Pts',(-0.845867574068782,-0.769956469697448,
8.82537455475955));
#147257=CARTESIAN_POINT('Ctrl Pts',(-0.828548150532178,-0.42405172294816,
8.69505289175401));
#147258=CARTESIAN_POINT('Ctrl Pts',(-0.823278348211893,-0.188791058808215,
8.65537076207235));
#147259=CARTESIAN_POINT('Ctrl Pts',(-0.824908645788194,0.283921315907471,
8.66764363603641));
#147260=CARTESIAN_POINT('Ctrl Pts',(-0.83179671234216,0.516830885581191,
8.71950740101902));
#147261=CARTESIAN_POINT('Ctrl Pts',(-0.84979066877245,0.82623768460948,
8.8548863040852));
#147262=CARTESIAN_POINT('Ctrl Pts',(-0.856212568854875,0.915473690074359,
8.90319272575272));
#147263=CARTESIAN_POINT('Ctrl Pts',(-0.863564213524501,1.00000000018888,
8.95847402464141));
#147264=CARTESIAN_POINT('',(-0.749910922999999,-1.00000000000002,8.968703006));
#147265=CARTESIAN_POINT('Origin',(1.11022302462516E-15,-1.00000000000002,
2.22044604925031E-15));
#147266=CARTESIAN_POINT('',(-0.749910922999999,0.999999999999982,8.968703006));
#147267=CARTESIAN_POINT('Ctrl Pts',(-0.749910923421741,1.0000000000954,
8.96870300583526));
#147268=CARTESIAN_POINT('Ctrl Pts',(-0.746446404937193,0.888963444745311,
8.89552629792414));
#147269=CARTESIAN_POINT('Ctrl Pts',(-0.743557342583254,0.769956469659581,
8.83458264224674));
#147270=CARTESIAN_POINT('Ctrl Pts',(-0.737328604408769,0.424051722945646,
8.70326279950606));
#147271=CARTESIAN_POINT('Ctrl Pts',(-0.73542820098917,0.188791058807986,
8.66327741843499));
#147272=CARTESIAN_POINT('Ctrl Pts',(-0.736015509228913,-0.283921315904419,
8.67564416313782));
#147273=CARTESIAN_POINT('Ctrl Pts',(-0.738498769557774,-0.516830885576862,
8.72790436785554));
#147274=CARTESIAN_POINT('Ctrl Pts',(-0.744966819940244,-0.826237684571763,
8.86432062122608));
#147275=CARTESIAN_POINT('Ctrl Pts',(-0.747273567077168,-0.91547369000699,
8.91299741334237));
#147276=CARTESIAN_POINT('Ctrl Pts',(-0.749910923421741,-1.00000000009543,
8.96870300583526));
#147277=CARTESIAN_POINT('Origin',(1.11022302462516E-15,0.999999999999982,
2.22044604925031E-15));
#147278=CARTESIAN_POINT('Origin',(1.11022302462516E-15,-1.77635683940025E-14,
2.22044604925031E-15));
#147279=CARTESIAN_POINT('',(-0.057056338,-1.00000000000002,8.999819141));
#147280=CARTESIAN_POINT('',(-0.057056338,0.999999999999982,8.999819141));
#147281=CARTESIAN_POINT('Ctrl Pts',(-0.0570563383389178,-0.999999999933198,
8.99981914108698));
#147282=CARTESIAN_POINT('Ctrl Pts',(-0.0539474002202254,-0.88896344463397,
8.92662646409639));
#147283=CARTESIAN_POINT('Ctrl Pts',(-0.0513618849266572,-0.769956469608777,
8.86566917614544));
#147284=CARTESIAN_POINT('Ctrl Pts',(-0.0457941281782648,-0.424051722954678,
8.73431964871832));
#147285=CARTESIAN_POINT('Ctrl Pts',(-0.0441026192351823,-0.188791058808769,
8.69432488618504));
#147286=CARTESIAN_POINT('Ctrl Pts',(-0.0446262217656057,0.283921315915507,
8.70669449191623));
#147287=CARTESIAN_POINT('Ctrl Pts',(-0.0468375269099042,0.516830885592579,
8.75896691015616));
#147288=CARTESIAN_POINT('Ctrl Pts',(-0.0526237735737156,0.82623768452456,
8.89541378333879));
#147289=CARTESIAN_POINT('Ctrl Pts',(-0.0546896666910911,0.915473689898557,
8.9441013921808));
#147290=CARTESIAN_POINT('Ctrl Pts',(-0.0570563383389176,0.999999999933163,
8.99981914108698));
#147291=CARTESIAN_POINT('',(0.0570563369999999,-1.00000000000002,8.999819141));
#147292=CARTESIAN_POINT('Origin',(1.11022302462516E-15,-1.00000000000002,
2.22044604925031E-15));
#147293=CARTESIAN_POINT('',(0.0570563369999999,0.999999999999982,8.999819141));
#147294=CARTESIAN_POINT('Ctrl Pts',(0.0570563367490446,0.999999999940043,
8.99981914110159));
#147295=CARTESIAN_POINT('Ctrl Pts',(0.0539473986136925,0.888963444636815,
8.92662646410728));
#147296=CARTESIAN_POINT('Ctrl Pts',(0.0513618833063579,0.769956469606838,
8.86566917615349));
#147297=CARTESIAN_POINT('Ctrl Pts',(0.0457941265286543,0.424051722950573,
8.73431964872651));
#147298=CARTESIAN_POINT('Ctrl Pts',(0.0441026175767656,0.188791058808352,
8.69432488619386));
#147299=CARTESIAN_POINT('Ctrl Pts',(0.0446262201098957,-0.2839213159106,
8.70669449192419));
#147300=CARTESIAN_POINT('Ctrl Pts',(0.0468375252657094,-0.516830885585594,
8.75896691016323));
#147301=CARTESIAN_POINT('Ctrl Pts',(0.0526237719600633,-0.826237684521612,
8.89541378334644));
#147302=CARTESIAN_POINT('Ctrl Pts',(0.0546896650884921,-0.91547368990086,
8.94410139219155));
#147303=CARTESIAN_POINT('Ctrl Pts',(0.0570563367490447,-0.999999999940079,
8.9998191411016));
#147304=CARTESIAN_POINT('Origin',(1.11022302462516E-15,0.999999999999982,
2.22044604925031E-15));
#147305=CARTESIAN_POINT('Origin',(1.11022302462516E-15,-1.77635683940025E-14,
2.22044604925031E-15));
#147306=CARTESIAN_POINT('',(0.749910923000001,-1.00000000000002,8.968703006));
#147307=CARTESIAN_POINT('',(0.749910923000001,0.999999999999982,8.968703006));
#147308=CARTESIAN_POINT('Ctrl Pts',(0.749910923031046,-1.00000000008893,
8.96870300586362));
#147309=CARTESIAN_POINT('Ctrl Pts',(0.746446404541417,-0.888963444741279,
8.89552629795535));
#147310=CARTESIAN_POINT('Ctrl Pts',(0.743557342183267,-0.769956469658455,
8.83458264228014));
#147311=CARTESIAN_POINT('Ctrl Pts',(0.737328603999575,-0.424051722946827,
8.70326279954085));
#147312=CARTESIAN_POINT('Ctrl Pts',(0.735428200577185,-0.188791058808123,
8.66327741846986));
#147313=CARTESIAN_POINT('Ctrl Pts',(0.736015508817804,0.283921315905779,
8.67564416317285));
#147314=CARTESIAN_POINT('Ctrl Pts',(0.73849876915032,0.516830885578806,
8.72790436789049));
#147315=CARTESIAN_POINT('Ctrl Pts',(0.74496681954236,0.826237684570912,
8.86432062125932));
#147316=CARTESIAN_POINT('Ctrl Pts',(0.747273566682631,0.91547369000311,
8.91299741337342));
#147317=CARTESIAN_POINT('Ctrl Pts',(0.749910923031046,1.00000000008889,
8.96870300586362));
#147318=CARTESIAN_POINT('',(0.863564212000001,-1.00000000000002,8.958474025));
#147319=CARTESIAN_POINT('Origin',(1.11022302462516E-15,-1.00000000000002,
2.22044604925031E-15));
#147320=CARTESIAN_POINT('',(0.863564213,0.999999999999982,8.958474025));
#147321=CARTESIAN_POINT('Ctrl Pts',(0.863564212376334,1.00000000020806,
8.95847402476479));
#147322=CARTESIAN_POINT('Ctrl Pts',(0.85390684889901,0.888963444826714,
8.88585468295841));
#147323=CARTESIAN_POINT('Ctrl Pts',(0.845867572926911,0.769956469703821,
8.82537455487133));
#147324=CARTESIAN_POINT('Ctrl Pts',(0.828548149397508,0.424051722947431,
8.69505289186206));
#147325=CARTESIAN_POINT('Ctrl Pts',(0.823278347079537,0.188791058808132,
8.65537076218013));
#147326=CARTESIAN_POINT('Ctrl Pts',(0.824908644655106,-0.283921315906622,
8.66764363614415));
#147327=CARTESIAN_POINT('Ctrl Pts',(0.83179671120604,-0.516830885579978,
8.71950740112709));
#147328=CARTESIAN_POINT('Ctrl Pts',(0.849790667627614,-0.826237684593335,
8.8548863041878));
#147329=CARTESIAN_POINT('Ctrl Pts',(0.856212567706076,-0.915473690044782,
8.90319272584691));
#147330=CARTESIAN_POINT('Ctrl Pts',(0.863564212371063,-1.00000000014749,
8.95847402472516));
#147331=CARTESIAN_POINT('Origin',(1.11022302462516E-15,0.999999999999982,
2.22044604925031E-15));
#147332=CARTESIAN_POINT('Origin',(1.11022302462516E-15,-1.77635683940025E-14,
2.22044604925031E-15));
#147333=CARTESIAN_POINT('',(1.550840341,-1.00000000000002,8.865376147));
#147334=CARTESIAN_POINT('',(1.550840341,0.999999999999982,8.865376147));
#147335=CARTESIAN_POINT('Ctrl Pts',(1.55084034103818,-0.999999999802086,
8.86537614729757));
#147336=CARTESIAN_POINT('Ctrl Pts',(1.54083026013964,-0.888963444538492,
8.79280458443474));
#147337=CARTESIAN_POINT('Ctrl Pts',(1.53248988110544,-0.769956469555649,
8.73236524362217));
#147338=CARTESIAN_POINT('Ctrl Pts',(1.51451479799596,-0.424051722951098,
8.60213239579622));
#147339=CARTESIAN_POINT('Ctrl Pts',(1.50903778309792,-0.188791058808459,
8.56247833496524));
#147340=CARTESIAN_POINT('Ctrl Pts',(1.51073127346174,0.283921315911105,
8.57474264888516));
#147341=CARTESIAN_POINT('Ctrl Pts',(1.51788910557278,0.516830885586341,
8.62656987164042));
#147342=CARTESIAN_POINT('Ctrl Pts',(1.53655937621794,0.826237684471544,
8.76185716165758));
#147343=CARTESIAN_POINT('Ctrl Pts',(1.54322019108732,0.91547368980399,8.81013122002992));
#147344=CARTESIAN_POINT('Ctrl Pts',(1.55084034103818,0.99999999980205,8.86537614729757));
#147345=CARTESIAN_POINT('',(1.663119178,-1.00000000000002,8.845000543));
#147346=CARTESIAN_POINT('Origin',(1.11022302462516E-15,-1.00000000000002,
2.22044604925031E-15));
#147347=CARTESIAN_POINT('',(1.663119178,0.999999999999982,8.845000543));
#147348=CARTESIAN_POINT('Ctrl Pts',(1.66311917779156,1.00000000018363,8.84500054276169));
#147349=CARTESIAN_POINT('Ctrl Pts',(1.64699114441794,0.888963444810215,
8.77353922446985));
#147350=CARTESIAN_POINT('Ctrl Pts',(1.63356283533152,0.769956469696762,
8.71402320674444));
#147351=CARTESIAN_POINT('Ctrl Pts',(1.60463119091762,0.424051722949316,
8.58577868159241));
#147352=CARTESIAN_POINT('Ctrl Pts',(1.5958255245984,0.188791058808291,8.54672868193495));
#147353=CARTESIAN_POINT('Ctrl Pts',(1.59854939101432,-0.28392131590896,
8.55880601016923));
#147354=CARTESIAN_POINT('Ctrl Pts',(1.61005876027881,-0.516830885583296,
8.60984354535825));
#147355=CARTESIAN_POINT('Ctrl Pts',(1.64011554961833,-0.826237684609203,
8.74306448694674));
#147356=CARTESIAN_POINT('Ctrl Pts',(1.65084175126428,-0.915473690071451,
8.79060078647738));
#147357=CARTESIAN_POINT('Ctrl Pts',(1.66311917779156,-1.00000000018366,
8.84500054276169));
#147358=CARTESIAN_POINT('Origin',(1.11022302462516E-15,0.999999999999982,
2.22044604925031E-15));
#147359=CARTESIAN_POINT('Origin',(1.11022302462516E-15,-1.77635683940025E-14,
2.22044604925031E-15));
#147360=CARTESIAN_POINT('',(2.339283305,-1.00000000000002,8.690670493));
#147361=CARTESIAN_POINT('',(2.339283305,0.999999999999982,8.690670493));
#147362=CARTESIAN_POINT('Ctrl Pts',(2.33928330447186,-0.999999999994545,
8.6906704931304));
#147363=CARTESIAN_POINT('Ctrl Pts',(2.32280825646114,-0.888963444676295,
8.61928837872337));
#147364=CARTESIAN_POINT('Ctrl Pts',(2.30908371258922,-0.769956469628457,
8.55983997469919));
#147365=CARTESIAN_POINT('Ctrl Pts',(2.2795070093957,-0.424051722951687,
8.43174268003198));
#147366=CARTESIAN_POINT('Ctrl Pts',(2.27049748074064,-0.188791058808529,
8.39273921062222));
#147367=CARTESIAN_POINT('Ctrl Pts',(2.27328351823432,0.283921315911797,
8.40480234871414));
#147368=CARTESIAN_POINT('Ctrl Pts',(2.2850582914487,0.51683088558733,8.45577930718374));
#147369=CARTESIAN_POINT('Ctrl Pts',(2.31578046026309,0.826237684542946,
8.58884838021717));
#147370=CARTESIAN_POINT('Ctrl Pts',(2.32674171389092,0.915473689939803,
8.63633103062244));
#147371=CARTESIAN_POINT('Ctrl Pts',(2.33928330447186,0.99999999999451,8.6906704931304));
#147372=CARTESIAN_POINT('',(2.449283685,-1.00000000000002,8.660312317));
#147373=CARTESIAN_POINT('Origin',(1.11022302462516E-15,-1.00000000000002,
2.22044604925031E-15));
#147374=CARTESIAN_POINT('',(2.449283685,0.999999999999982,8.660312317));
#147375=CARTESIAN_POINT('Ctrl Pts',(2.44928368526842,0.999999999964307,
8.66031231697032));
#147376=CARTESIAN_POINT('Ctrl Pts',(2.42681483546961,0.888963444655136,
8.59058438675928));
#147377=CARTESIAN_POINT('Ctrl Pts',(2.40810561014116,0.769956469618104,
8.53251166741322));
#147378=CARTESIAN_POINT('Ctrl Pts',(2.36779468545961,0.424051722952564,
8.40737682964597));
#147379=CARTESIAN_POINT('Ctrl Pts',(2.35552405319223,0.188791058808564,
8.36927336764647));
#147380=CARTESIAN_POINT('Ctrl Pts',(2.35931955747614,-0.283921315912966,
8.38105791060647));
#147381=CARTESIAN_POINT('Ctrl Pts',(2.37535756277304,-0.516830885588967,
8.43085829178138));
#147382=CARTESIAN_POINT('Ctrl Pts',(2.41723518540491,-0.826237684533161,
8.5608486551779));
#147383=CARTESIAN_POINT('Ctrl Pts',(2.43217932752638,-0.915473689919173,
8.60723209819538));
#147384=CARTESIAN_POINT('Ctrl Pts',(2.44928368526842,-0.999999999964343,
8.66031231697032));
#147385=CARTESIAN_POINT('Origin',(1.11022302462516E-15,0.999999999999982,
2.22044604925031E-15));
#147386=CARTESIAN_POINT('Origin',(1.11022302462516E-15,-1.77635683940025E-14,
2.22044604925031E-15));
#147387=CARTESIAN_POINT('',(3.108891735,-1.00000000000002,8.44599267));
#147388=CARTESIAN_POINT('',(3.108891735,0.999999999999982,8.44599267));
#147389=CARTESIAN_POINT('Ctrl Pts',(3.10889173544937,-1.0000000000809,8.44599266972378));
#147390=CARTESIAN_POINT('Ctrl Pts',(3.08608436775726,-0.888963444735186,
8.37637473060366));
#147391=CARTESIAN_POINT('Ctrl Pts',(3.06708616103102,-0.769956469654649,
8.31839590697489));
#147392=CARTESIAN_POINT('Ctrl Pts',(3.02614597203478,-0.424051722946102,
8.19346552955976));
#147393=CARTESIAN_POINT('Ctrl Pts',(3.0136764690676,-0.188791058808042,
8.15542668456797));
#147394=CARTESIAN_POINT('Ctrl Pts',(3.01753262214962,0.283921315904921,
8.16719152153767));
#147395=CARTESIAN_POINT('Ctrl Pts',(3.03382953289371,0.516830885577575,
8.21690777923271));
#147396=CARTESIAN_POINT('Ctrl Pts',(3.07635624297832,0.826237684567004,
8.34668724135259));
#147397=CARTESIAN_POINT('Ctrl Pts',(3.0915296817749,0.915473689997012,8.39299618139483));
#147398=CARTESIAN_POINT('Ctrl Pts',(3.10889173544937,1.00000000008087,8.44599266972378));
#147399=CARTESIAN_POINT('',(3.215728,-1.00000000000002,8.405896349));
#147400=CARTESIAN_POINT('Origin',(1.11022302462516E-15,-1.00000000000002,
2.22044604925031E-15));
#147401=CARTESIAN_POINT('',(3.215728,0.999999999999982,8.405896349));
#147402=CARTESIAN_POINT('Ctrl Pts',(3.21572799949971,1.00000000004184,8.40589634914348));
#147403=CARTESIAN_POINT('Ctrl Pts',(3.1870992391518,0.888963444706611,8.33846321524216));
#147404=CARTESIAN_POINT('Ctrl Pts',(3.16325973318893,0.769956469638538,
8.28230136161672));
#147405=CARTESIAN_POINT('Ctrl Pts',(3.11189408797419,0.424051722944791,
8.16128372337191));
#147406=CARTESIAN_POINT('Ctrl Pts',(3.09625728563936,0.188791058807925,
8.12443358571553));
#147407=CARTESIAN_POINT('Ctrl Pts',(3.10109386863279,-0.283921315903338,
8.13583046118458));
#147408=CARTESIAN_POINT('Ctrl Pts',(3.12153138141972,-0.516830885575335,
8.18399272494027));
#147409=CARTESIAN_POINT('Ctrl Pts',(3.17489266348559,-0.826237684550909,
8.30970590417526));
#147410=CARTESIAN_POINT('Ctrl Pts',(3.19393442470021,-0.915473689968736,
8.35456303852214));
#147411=CARTESIAN_POINT('Ctrl Pts',(3.21572799949971,-1.00000000004187,
8.40589634914348));
#147412=CARTESIAN_POINT('Origin',(1.11022302462516E-15,0.999999999999982,
2.22044604925031E-15));
#147413=CARTESIAN_POINT('Origin',(1.11022302462516E-15,-1.77635683940025E-14,
2.22044604925031E-15));
#147414=CARTESIAN_POINT('',(3.85346919675118,-0.999999999914645,8.13331268017501));
#147415=CARTESIAN_POINT('',(3.853469196,0.999999999999982,8.13331268));
#147416=CARTESIAN_POINT('Ctrl Pts',(3.85346919578197,-1.00000000005208,
8.13331268036528));
#147417=CARTESIAN_POINT('Ctrl Pts',(3.82451313984361,-0.888963444719939,
8.06601943931758));
#147418=CARTESIAN_POINT('Ctrl Pts',(3.8003942325866,-0.76995646965561,8.00997700754015));
#147419=CARTESIAN_POINT('Ctrl Pts',(3.74842018395873,-0.424051722956707,
7.88921941339301));
#147420=CARTESIAN_POINT('Ctrl Pts',(3.73259110373581,-0.188791058808946,
7.85245145924944));
#147421=CARTESIAN_POINT('Ctrl Pts',(3.73748632494522,0.283921315918004,
7.86382327154455));
#147422=CARTESIAN_POINT('Ctrl Pts',(3.75817416014108,0.51683088559612,7.91187854236911));
#147423=CARTESIAN_POINT('Ctrl Pts',(3.81216301158527,0.826237684515584,
8.03732348555132));
#147424=CARTESIAN_POINT('Ctrl Pts',(3.83142646798092,0.91547368987732,8.08208586278962));
#147425=CARTESIAN_POINT('Ctrl Pts',(3.85346919574262,0.999999999901147,
8.13331268027382));
#147426=CARTESIAN_POINT('',(3.956281164,-1.00000000000002,8.083801046));
#147427=CARTESIAN_POINT('Origin',(1.11022302462516E-15,-1.00000000000002,
2.22044604925031E-15));
#147428=CARTESIAN_POINT('',(3.956281164,0.999999999999982,8.083801046));
#147429=CARTESIAN_POINT('Ctrl Pts',(3.95628116427791,1.00000000002302,8.08380104581171));
#147430=CARTESIAN_POINT('Ctrl Pts',(3.92172299544629,0.88896344469827,8.01920564015371));
#147431=CARTESIAN_POINT('Ctrl Pts',(3.89294515063276,0.76995646964272,7.96540683446068));
#147432=CARTESIAN_POINT('Ctrl Pts',(3.83093835105285,0.424051722954895,
7.849480758534));
#147433=CARTESIAN_POINT('Ctrl Pts',(3.8120612770459,0.188791058808754,7.8141806408354));
#147434=CARTESIAN_POINT('Ctrl Pts',(3.81789999740993,-0.28392131591586,
7.82509808788435));
#147435=CARTESIAN_POINT('Ctrl Pts',(3.84257246677632,-0.516830885593063,
7.87123446002672));
#147436=CARTESIAN_POINT('Ctrl Pts',(3.9069877744043,-0.826237684557924,
7.99165828656834));
#147437=CARTESIAN_POINT('Ctrl Pts',(3.92997384156548,-0.915473689961999,
8.03462794897708));
#147438=CARTESIAN_POINT('Ctrl Pts',(3.95628116427791,-1.00000000002306,
8.08380104581171));
#147439=CARTESIAN_POINT('Origin',(1.11022302462516E-15,0.999999999999982,
2.22044604925031E-15));
#147440=CARTESIAN_POINT('Origin',(1.11022302462516E-15,-1.77635683940025E-14,
2.22044604925031E-15));
#147441=CARTESIAN_POINT('',(4.56702079,-1.00000000000002,7.755148038));
#147442=CARTESIAN_POINT('',(4.567020791,0.999999999999982,7.755148038));
#147443=CARTESIAN_POINT('Ctrl Pts',(4.56702079072311,-0.999999999723031,
7.75514803808598));
#147444=CARTESIAN_POINT('Ctrl Pts',(4.53214918384362,-0.888963444478469,
7.69072130072636));
#147445=CARTESIAN_POINT('Ctrl Pts',(4.50310376745261,-0.769956469518223,
7.63706648150941));
#147446=CARTESIAN_POINT('Ctrl Pts',(4.44051432392658,-0.424051722944125,
7.52145393970777));
#147447=CARTESIAN_POINT('Ctrl Pts',(4.42145311296569,-0.188791058807886,
7.48625291033002));
#147448=CARTESIAN_POINT('Ctrl Pts',(4.42734798883602,0.283921315902461,
7.49714013881019));
#147449=CARTESIAN_POINT('Ctrl Pts',(4.45226018210562,0.516830885574096,
7.54314751001828));
#147450=CARTESIAN_POINT('Ctrl Pts',(4.51727648819371,0.82623768451322,7.66324792548531));
#147451=CARTESIAN_POINT('Ctrl Pts',(4.54047486409896,0.915473689897855,
7.70610333967294));
#147452=CARTESIAN_POINT('Ctrl Pts',(4.56702079079182,0.999999999941805,
7.75514803821294));
#147453=CARTESIAN_POINT('',(4.664980679,-1.00000000000002,7.69661973));
#147454=CARTESIAN_POINT('Origin',(1.11022302462516E-15,-1.00000000000002,
2.22044604925031E-15));
#147455=CARTESIAN_POINT('',(4.664980678,0.999999999999982,7.69661973));
#147456=CARTESIAN_POINT('Ctrl Pts',(4.66498067874573,0.999999999872922,
7.69661972974073));
#147457=CARTESIAN_POINT('Ctrl Pts',(4.62477134343723,0.888963444590633,
7.63538213660728));
#147458=CARTESIAN_POINT('Ctrl Pts',(4.59128686201659,0.769956469585573,
7.58437953524182));
#147459=CARTESIAN_POINT('Ctrl Pts',(4.51913815025123,0.424051722954107,
7.47447839030291));
#147460=CARTESIAN_POINT('Ctrl Pts',(4.49717279163596,0.188791058808661,
7.44101250837075));
#147461=CARTESIAN_POINT('Ctrl Pts',(4.50396663943793,-0.28392131591495,
7.45136262612837));
#147462=CARTESIAN_POINT('Ctrl Pts',(4.53267541721536,-0.516830885591761,
7.49510164369408));
#147463=CARTESIAN_POINT('Ctrl Pts',(4.6076261163616,-0.826237684594402,
7.60926653566084));
#147464=CARTESIAN_POINT('Ctrl Pts',(4.63437141923369,-0.915473690033447,
7.6500027596831));
#147465=CARTESIAN_POINT('Ctrl Pts',(4.66498067883709,-1.00000000012526,
7.69661972987988));
#147466=CARTESIAN_POINT('Origin',(1.11022302462516E-15,0.999999999999982,
2.22044604925031E-15));
#147467=CARTESIAN_POINT('Origin',(1.11022302462516E-15,-1.77635683940025E-14,
2.22044604925031E-15));
#147468=CARTESIAN_POINT('',(5.243801418,-1.00000000000002,7.314543505));
#147469=CARTESIAN_POINT('',(5.243801418,0.999999999999982,7.314543505));
#147470=CARTESIAN_POINT('Ctrl Pts',(5.24380141829551,-0.999999999983744,
7.31454350483351));
#147471=CARTESIAN_POINT('Ctrl Pts',(5.20329502600419,-0.888963444664367,
7.25350199725071));
#147472=CARTESIAN_POINT('Ctrl Pts',(5.16955695697835,-0.769956469615145,
7.20266678756194));
#147473=CARTESIAN_POINT('Ctrl Pts',(5.09685605179224,-0.424051722943348,
7.09313014228908));
#147474=CARTESIAN_POINT('Ctrl Pts',(5.07471617971955,-0.188791058807811,
7.05977945568221));
#147475=CARTESIAN_POINT('Ctrl Pts',(5.08156324818856,0.283921315901524,
7.0700944427827));
#147476=CARTESIAN_POINT('Ctrl Pts',(5.11049922124789,0.516830885572765,
7.11368349005473));
#147477=CARTESIAN_POINT('Ctrl Pts',(5.18601950903758,0.826237684527554,
7.22747239982517));
#147478=CARTESIAN_POINT('Ctrl Pts',(5.21296602481403,0.915473689926858,
7.26807580434118));
#147479=CARTESIAN_POINT('Ctrl Pts',(5.24380141829551,0.999999999983706,
7.31454350483351));
#147480=CARTESIAN_POINT('',(5.336120511,-1.00000000000002,7.247469758));
#147481=CARTESIAN_POINT('Origin',(1.11022302462516E-15,-1.00000000000002,
2.22044604925031E-15));
#147482=CARTESIAN_POINT('',(5.336120511,0.999999999999982,7.247469758));
#147483=CARTESIAN_POINT('Ctrl Pts',(5.3361205105636,1.00000000006483,7.24746975822081));
#147484=CARTESIAN_POINT('Ctrl Pts',(5.29058375060566,0.888963444722995,
7.19008302665037));
#147485=CARTESIAN_POINT('Ctrl Pts',(5.25266222985656,0.769956469647073,
7.1422872725303));
#147486=CARTESIAN_POINT('Ctrl Pts',(5.17095250481386,0.424051722944686,
7.03929591799513));
#147487=CARTESIAN_POINT('Ctrl Pts',(5.14607571372183,0.188791058807888,
7.0079337194511));
#147488=CARTESIAN_POINT('Ctrl Pts',(5.1537699888994,-0.283921315903273,
7.01763317484824));
#147489=CARTESIAN_POINT('Ctrl Pts',(5.18628392891646,-0.51683088557523,
7.05862267696227));
#147490=CARTESIAN_POINT('Ctrl Pts',(5.27116656068068,-0.826237684559263,
7.16560944569038));
#147491=CARTESIAN_POINT('Ctrl Pts',(5.30145576182033,-0.915473689984878,
7.20378424715405));
#147492=CARTESIAN_POINT('Ctrl Pts',(5.3361205105636,-1.00000000006487,7.24746975822082));
#147493=CARTESIAN_POINT('Origin',(1.11022302462516E-15,0.999999999999982,
2.22044604925031E-15));
#147494=CARTESIAN_POINT('Origin',(1.11022302462516E-15,-1.77635683940025E-14,
2.22044604925031E-15));
#147495=CARTESIAN_POINT('',(5.87836204,-1.00000000000002,6.815046568));
#147496=CARTESIAN_POINT('',(5.878362039,0.999999999999982,6.815046569));
#147497=CARTESIAN_POINT('Ctrl Pts',(5.8783620393509,-0.999999999947016,
6.81504656862317));
#147498=CARTESIAN_POINT('Ctrl Pts',(5.83254699529058,-0.888963444643323,
6.75788176127013));
#147499=CARTESIAN_POINT('Ctrl Pts',(5.79438791271225,-0.769956469612809,
6.71027545642629));
#147500=CARTESIAN_POINT('Ctrl Pts',(5.71216089072527,-0.424051722953641,
6.60769663246045));
#147501=CARTESIAN_POINT('Ctrl Pts',(5.68712061474111,-0.188791058808674,
6.57646480876682));
#147502=CARTESIAN_POINT('Ctrl Pts',(5.69486474725044,0.283921315914245,
6.58612450427073));
#147503=CARTESIAN_POINT('Ctrl Pts',(5.72759152469994,0.516830885590786,
6.62694427419722));
#147504=CARTESIAN_POINT('Ctrl Pts',(5.81300774934532,0.826237684554357,
6.73350551678999));
#147505=CARTESIAN_POINT('Ctrl Pts',(5.84348544752745,0.915473689957744,
6.77152999685925));
#147506=CARTESIAN_POINT('Ctrl Pts',(5.87836203938029,1.0000000000182,6.81504656865984));
#147507=CARTESIAN_POINT('',(5.964297039,-1.00000000000002,6.739967421));
#147508=CARTESIAN_POINT('Origin',(1.11022302462516E-15,-1.00000000000002,
2.22044604925031E-15));
#147509=CARTESIAN_POINT('',(5.964297039,0.999999999999982,6.739967421));
#147510=CARTESIAN_POINT('Ctrl Pts',(5.96429703907415,1.00000000016684,6.73996742058037));
#147511=CARTESIAN_POINT('Ctrl Pts',(5.91379948977288,0.888963444798607,
6.68689359476872));
#147512=CARTESIAN_POINT('Ctrl Pts',(5.87174625155671,0.769956469691321,
6.64268951118086));
#147513=CARTESIAN_POINT('Ctrl Pts',(5.78113339203642,0.424051722950071,
6.54743717279022));
#147514=CARTESIAN_POINT('Ctrl Pts',(5.75354546180195,0.188791058808329,
6.5184311675852));
#147515=CARTESIAN_POINT('Ctrl Pts',(5.76207821456473,-0.283921315909946,
6.52740186632183));
#147516=CARTESIAN_POINT('Ctrl Pts',(5.79813553364251,-0.516830885584677,
6.56531182965559));
#147517=CARTESIAN_POINT('Ctrl Pts',(5.89226667286069,-0.826237684604124,
6.66425908071306));
#147518=CARTESIAN_POINT('Ctrl Pts',(5.92585590139914,-0.91547369006014,
6.69956509862226));
#147519=CARTESIAN_POINT('Ctrl Pts',(5.96429703907415,-1.00000000016687,
6.73996742058037));
#147520=CARTESIAN_POINT('Origin',(1.11022302462516E-15,0.999999999999982,
2.22044604925031E-15));
#147521=CARTESIAN_POINT('Origin',(1.11022302462516E-15,-1.77635683940025E-14,
2.22044604925031E-15));
#147522=CARTESIAN_POINT('',(6.465593547,-1.00000000000002,6.260678884));
#147523=CARTESIAN_POINT('',(6.465593547,0.999999999999982,6.260678883));
#147524=CARTESIAN_POINT('Ctrl Pts',(6.465593547415,-1.00000000013442,6.26067888331879));
#147525=CARTESIAN_POINT('Ctrl Pts',(6.41483872740882,-0.888963444774573,
6.20785103349867));
#147526=CARTESIAN_POINT('Ctrl Pts',(6.37256586579951,-0.769956469677246,
6.16385693138393));
#147527=CARTESIAN_POINT('Ctrl Pts',(6.28147477075941,-0.424051722948395,
6.06906183297416));
#147528=CARTESIAN_POINT('Ctrl Pts',(6.25373570048457,-0.188791058808251,
6.04020033244393));
#147529=CARTESIAN_POINT('Ctrl Pts',(6.26231454581812,0.283921315907732,
6.04912696217015));
#147530=CARTESIAN_POINT('Ctrl Pts',(6.29856863083365,0.516830885581569,
6.08684879800449));
#147531=CARTESIAN_POINT('Ctrl Pts',(6.39319307094974,0.826237684468099,
6.18532440503001));
#147532=CARTESIAN_POINT('Ctrl Pts',(6.42695656294875,0.915473689802837,
6.22046380990041));
#147533=CARTESIAN_POINT('Ctrl Pts',(6.46559354726348,0.999999999802907,
6.26067888316109));
#147534=CARTESIAN_POINT('',(6.544452554,-1.00000000000002,6.178198829));
#147535=CARTESIAN_POINT('Origin',(1.11022302462516E-15,-1.00000000000002,
2.22044604925031E-15));
#147536=CARTESIAN_POINT('',(6.544452554,0.999999999999982,6.178198829));
#147537=CARTESIAN_POINT('Ctrl Pts',(6.54445255390455,1.0000000000868,6.17819882890926));
#147538=CARTESIAN_POINT('Ctrl Pts',(6.48940079184017,0.888963444741015,
6.12986522815415));
#147539=CARTESIAN_POINT('Ctrl Pts',(6.44355442410623,0.769956469660416,
6.0896087204346));
#147540=CARTESIAN_POINT('Ctrl Pts',(6.34476799154022,0.424051722949287,
6.00286231406977));
#147541=CARTESIAN_POINT('Ctrl Pts',(6.3146910439409,0.188791058808277,5.97644604151514));
#147542=CARTESIAN_POINT('Ctrl Pts',(6.32399357358487,-0.28392131590895,
5.98461575679496));
#147543=CARTESIAN_POINT('Ctrl Pts',(6.36330395941132,-0.516830885583272,
6.01914095259762));
#147544=CARTESIAN_POINT('Ctrl Pts',(6.46592571753245,-0.82623768457364,
6.10925202083549));
#147545=CARTESIAN_POINT('Ctrl Pts',(6.50254453274514,-0.915473690003291,
6.1414049918512));
#147546=CARTESIAN_POINT('Ctrl Pts',(6.54445255390455,-1.00000000008684,
6.17819882890926));
#147547=CARTESIAN_POINT('Origin',(1.11022302462516E-15,0.999999999999982,
2.22044604925031E-15));
#147548=CARTESIAN_POINT('Origin',(1.11022302462516E-15,-1.77635683940025E-14,
2.22044604925031E-15));
#147549=CARTESIAN_POINT('',(7.000767897,-1.00000000000002,5.655903894));
#147550=CARTESIAN_POINT('',(7.000767897,0.999999999999982,5.655903894));
#147551=CARTESIAN_POINT('Ctrl Pts',(7.00076789655178,-1.00000000017299,
5.65590389411597));
#147552=CARTESIAN_POINT('Ctrl Pts',(6.94548194857317,-0.888963444802474,
5.60783834066879));
#147553=CARTESIAN_POINT('Ctrl Pts',(6.89943566416173,-0.769956469692457,
5.56781065596884));
#147554=CARTESIAN_POINT('Ctrl Pts',(6.80021390797847,-0.424051722949051,
5.4815625175572));
#147555=CARTESIAN_POINT('Ctrl Pts',(6.76999938208442,-0.188791058808294,
5.45530371603143));
#147556=CARTESIAN_POINT('Ctrl Pts',(6.77934386842824,0.283921315908569,
5.46342540800412));
#147557=CARTESIAN_POINT('Ctrl Pts',(6.8188333644502,0.516830885582751,5.4977455956925));
#147558=CARTESIAN_POINT('Ctrl Pts',(6.92190415979063,0.826237684604844,
5.58734269949924));
#147559=CARTESIAN_POINT('Ctrl Pts',(6.95868160192628,0.915473690063715,
5.61931410742192));
#147560=CARTESIAN_POINT('Ctrl Pts',(7.00076789655177,1.00000000017296,5.65590389411597));
#147561=CARTESIAN_POINT('',(7.071915985,-1.00000000000002,5.566687013));
#147562=CARTESIAN_POINT('Origin',(1.11022302462516E-15,-1.00000000000002,
2.22044604925031E-15));
#147563=CARTESIAN_POINT('',(7.07191598509134,1.00000000000236,5.5666870127956));
#147564=CARTESIAN_POINT('Ctrl Pts',(7.07191598491098,1.00000000000174,5.56668701304418));
#147565=CARTESIAN_POINT('Ctrl Pts',(7.01275325449934,0.888963444679149,
5.52348279108474));
#147566=CARTESIAN_POINT('Ctrl Pts',(6.96348288524122,0.769956469626121,
5.48749798096801));
#147567=CARTESIAN_POINT('Ctrl Pts',(6.85731824989088,0.424051722947126,
5.40995593770058));
#147568=CARTESIAN_POINT('Ctrl Pts',(6.82499444682085,0.188791058808083,
5.38634208609495));
#147569=CARTESIAN_POINT('Ctrl Pts',(6.83499185484784,-0.283921315906306,
5.39364504017274));
#147570=CARTESIAN_POINT('Ctrl Pts',(6.87723880331427,-0.516830885579519,
5.42450749186227));
#147571=CARTESIAN_POINT('Ctrl Pts',(6.98752493029364,-0.826237684546757,
5.50505685593149));
#147572=CARTESIAN_POINT('Ctrl Pts',(7.02687849901688,-0.915473689956015,
5.53379790323594));
#147573=CARTESIAN_POINT('Ctrl Pts',(7.07191598492155,-1.00000000002162,
5.5666870130519));
#147574=CARTESIAN_POINT('Origin',(1.11022302462516E-15,0.999999999999982,
2.22044604925031E-15));
#147575=CARTESIAN_POINT('Origin',(1.11022302462516E-15,-1.77635683940025E-14,
2.22044604925031E-15));
#147576=CARTESIAN_POINT('',(7.47957618,-1.00000000000002,5.005590892));
#147577=CARTESIAN_POINT('',(7.47957618,0.999999999999982,5.005590892));
#147578=CARTESIAN_POINT('Ctrl Pts',(7.47957617967883,-1.00000000029992,
5.00559089166839));
#147579=CARTESIAN_POINT('Ctrl Pts',(7.4202042336451,-0.888963444893634,
4.96267463016275));
#147580=CARTESIAN_POINT('Ctrl Pts',(7.37075526401692,-0.769956469741095,
4.92693564225512));
#147581=CARTESIAN_POINT('Ctrl Pts',(7.26420172190819,-0.424051722949997,
4.84992888314662));
#147582=CARTESIAN_POINT('Ctrl Pts',(7.23175500998827,-0.188791058808381,
4.82648420105958));
#147583=CARTESIAN_POINT('Ctrl Pts',(7.24178990103385,0.283921315909722,
4.83373556418914));
#147584=CARTESIAN_POINT('Ctrl Pts',(7.28419686186404,0.516830885584386,
4.86437777775458));
#147585=CARTESIAN_POINT('Ctrl Pts',(7.39488414697571,0.82623768465271,4.94437499509896));
#147586=CARTESIAN_POINT('Ctrl Pts',(7.43437942887843,0.915473690153646,
4.9729209910481));
#147587=CARTESIAN_POINT('Ctrl Pts',(7.47957617967883,1.00000000029988,5.00559089166839));
#147588=CARTESIAN_POINT('',(7.542440507,-1.00000000000002,4.910355506));
#147589=CARTESIAN_POINT('Origin',(1.11022302462516E-15,-1.00000000000002,
2.22044604925031E-15));
#147590=CARTESIAN_POINT('',(7.542440507,0.999999999999982,4.910355506));
#147591=CARTESIAN_POINT('Ctrl Pts',(7.54244050680655,0.99999999996,4.91035550643967));
#147592=CARTESIAN_POINT('Ctrl Pts',(7.47964315154329,0.888963444646452,
4.87262851828103));
#147593=CARTESIAN_POINT('Ctrl Pts',(7.42734547678568,0.769956469604149,
4.84120513431145));
#147594=CARTESIAN_POINT('Ctrl Pts',(7.31465741384491,0.42405172294144,4.77349177711884));
#147595=CARTESIAN_POINT('Ctrl Pts',(7.28034700755391,0.188791058807607,
4.75287047132403));
#147596=CARTESIAN_POINT('Ctrl Pts',(7.29095880071433,-0.283921315899282,
4.75924786510322));
#147597=CARTESIAN_POINT('Ctrl Pts',(7.33580216424092,-0.51683088556957,
4.78619908634786));
#147598=CARTESIAN_POINT('Ctrl Pts',(7.45286470105419,-0.826237684516338,
4.85653821008756));
#147599=CARTESIAN_POINT('Ctrl Pts',(7.49463617150114,-0.915473689909017,
4.88163592765426));
#147600=CARTESIAN_POINT('Ctrl Pts',(7.54244050680656,-0.999999999960036,
4.91035550643967));
#147601=CARTESIAN_POINT('Origin',(1.11022302462516E-15,0.999999999999982,
2.22044604925031E-15));
#147602=CARTESIAN_POINT('Origin',(1.11022302462516E-15,-1.77635683940025E-14,
2.22044604925031E-15));
#147603=CARTESIAN_POINT('',(7.898163313,-1.00000000000002,4.314975815));
#147604=CARTESIAN_POINT('',(7.898163313,0.999999999999982,4.314975815));
#147605=CARTESIAN_POINT('Ctrl Pts',(7.89816331281297,-1.0000000001015,4.31497581501367));
#147606=CARTESIAN_POINT('Ctrl Pts',(7.83518339679211,-0.888963444754433,
4.27755438203095));
#147607=CARTESIAN_POINT('Ctrl Pts',(7.78272987602675,-0.769956469672351,
4.24639184029318));
#147608=CARTESIAN_POINT('Ctrl Pts',(7.66970245447833,-0.424051722955082,
4.1792464736998));
#147609=CARTESIAN_POINT('Ctrl Pts',(7.63528479837203,-0.188791058808791,
4.1588046738586));
#147610=CARTESIAN_POINT('Ctrl Pts',(7.64592929907975,0.283921315916036,
4.16512732442939));
#147611=CARTESIAN_POINT('Ctrl Pts',(7.69091228881308,0.516830885593324,
4.19184485076974));
#147612=CARTESIAN_POINT('Ctrl Pts',(7.80832487473718,0.826237684586909,
4.26159809102288));
#147613=CARTESIAN_POINT('Ctrl Pts',(7.8502200035666,0.915473690017278,4.28648883936673));
#147614=CARTESIAN_POINT('Ctrl Pts',(7.89816331281297,1.00000000010146,4.31497581501367));
#147615=CARTESIAN_POINT('',(7.952237733,-1.00000000000002,4.214488703));
#147616=CARTESIAN_POINT('Origin',(1.11022302462516E-15,-1.00000000000002,
2.22044604925031E-15));
#147617=CARTESIAN_POINT('',(7.952237734,0.999999999999982,4.214488703));
#147618=CARTESIAN_POINT('Ctrl Pts',(7.9522377334233,1.00000000018981,4.21448870353033));
#147619=CARTESIAN_POINT('Ctrl Pts',(7.8863113606651,0.888963444813986,4.18254270459723));
#147620=CARTESIAN_POINT('Ctrl Pts',(7.83140745051944,0.769956469697662,
4.15593374930452));
#147621=CARTESIAN_POINT('Ctrl Pts',(7.71310325805012,0.424051722948053,
4.09859426618527));
#147622=CARTESIAN_POINT('Ctrl Pts',(7.67708249577676,0.188791058808183,
4.08113153679339));
#147623=CARTESIAN_POINT('Ctrl Pts',(7.68822323414686,-0.283921315907404,
4.08653202326162));
#147624=CARTESIAN_POINT('Ctrl Pts',(7.73530196031026,-0.516830885581086,
4.10935501872354));
#147625=CARTESIAN_POINT('Ctrl Pts',(7.8581983881465,-0.826237684457902,
4.16891757298585));
#147626=CARTESIAN_POINT('Ctrl Pts',(7.90205144094032,-0.915473689783842,
4.19016988878228));
#147627=CARTESIAN_POINT('Ctrl Pts',(7.95223773317769,-0.999999999776177,
4.21448870341132));
#147628=CARTESIAN_POINT('Origin',(1.11022302462516E-15,0.999999999999982,
2.22044604925031E-15));
#147629=CARTESIAN_POINT('Origin',(1.11022302462516E-15,-1.77635683940025E-14,
2.22044604925031E-15));
#147630=CARTESIAN_POINT('',(8.253159079,-1.00000000000002,3.58961909));
#147631=CARTESIAN_POINT('',(8.253159079,0.999999999999982,3.58961909));
#147632=CARTESIAN_POINT('Ctrl Pts',(8.25315907914881,-0.999999999891678,
3.58961909006944));
#147633=CARTESIAN_POINT('Ctrl Pts',(8.18707827043164,-0.888963444602143,
3.55799378091446));
#147634=CARTESIAN_POINT('Ctrl Pts',(8.13204252346783,-0.769956469588448,
3.5316585877518));
#147635=CARTESIAN_POINT('Ctrl Pts',(8.01345125288576,-0.424051722950382,
3.47491522857436));
#147636=CARTESIAN_POINT('Ctrl Pts',(7.97733976334233,-0.188791058808387,
3.45764089629978));
#147637=CARTESIAN_POINT('Ctrl Pts',(7.98850817044388,0.283921315910249,
3.46298392805613));
#147638=CARTESIAN_POINT('Ctrl Pts',(8.03570501247084,0.516830885585118,
3.48556165340058));
#147639=CARTESIAN_POINT('Ctrl Pts',(8.15889756203452,0.826237684503458,
3.5445093046019));
#147640=CARTESIAN_POINT('Ctrl Pts',(8.20285522282177,0.915473689866593,
3.56554439971813));
#147641=CARTESIAN_POINT('Ctrl Pts',(8.25315907914881,0.999999999891641,
3.58961909006944));
#147642=CARTESIAN_POINT('',(8.298008217,-1.00000000000002,3.484689316));
#147643=CARTESIAN_POINT('Origin',(1.11022302462516E-15,-1.00000000000002,
2.22044604925031E-15));
#147644=CARTESIAN_POINT('',(8.298008217,0.999999999999982,3.484689316));
#147645=CARTESIAN_POINT('Ctrl Pts',(8.29800821680408,0.999999999999766,
3.48468931651914));
#147646=CARTESIAN_POINT('Ctrl Pts',(8.22948362702398,0.888963444677765,
3.45878151730231));
#147647=CARTESIAN_POINT('Ctrl Pts',(8.17241553555401,0.769956469625439,
3.43720123042083));
#147648=CARTESIAN_POINT('Ctrl Pts',(8.04944772936533,0.424051722947189,
3.39069728527389));
#147649=CARTESIAN_POINT('Ctrl Pts',(8.01200662909584,0.188791058808109,
3.37653373193536));
#147650=CARTESIAN_POINT('Ctrl Pts',(8.02358661400347,-0.28392131590634,
3.38091382954382));
#147651=CARTESIAN_POINT('Ctrl Pts',(8.07252165259768,-0.51683088557958,
3.39942484185536));
#147652=CARTESIAN_POINT('Ctrl Pts',(8.20026248178416,-0.826237684538796,
3.447731263932));
#147653=CARTESIAN_POINT('Ctrl Pts',(8.24584403802863,-0.915473689940678,
3.46496706682217));
#147654=CARTESIAN_POINT('Ctrl Pts',(8.29800821680408,-0.999999999999798,
3.48468931651914));
#147655=CARTESIAN_POINT('Origin',(1.11022302462516E-15,0.999999999999982,
2.22044604925031E-15));
#147656=CARTESIAN_POINT('Origin',(1.11022302462516E-15,-1.77635683940025E-14,
2.22044604925031E-15));
#147657=CARTESIAN_POINT('',(8.541705262,-1.00000000000002,2.835360862));
#147658=CARTESIAN_POINT('',(8.541705262,0.999999999999982,2.835360862));
#147659=CARTESIAN_POINT('Ctrl Pts',(8.54170526179937,-1.00000000003984,
2.83536086236564));
#147660=CARTESIAN_POINT('Ctrl Pts',(8.47305560408873,-0.888963444708827,
2.80978630543292));
#147661=CARTESIAN_POINT('Ctrl Pts',(8.41588074631203,-0.769956469645811,
2.78849049633942));
#147662=CARTESIAN_POINT('Ctrl Pts',(8.29268045378883,-0.424051722952013,
2.74260600880004));
#147663=CARTESIAN_POINT('Ctrl Pts',(8.25516587927574,-0.188791058808545,
2.72863822688282));
#147664=CARTESIAN_POINT('Ctrl Pts',(8.26676827132905,0.283921315912221,
2.73295862086762));
#147665=CARTESIAN_POINT('Ctrl Pts',(8.31579896444623,0.516830885587926,
2.75121476261534));
#147666=CARTESIAN_POINT('Ctrl Pts',(8.44377960377111,0.826237684560039,
2.79888221287883));
#147667=CARTESIAN_POINT('Ctrl Pts',(8.48944587536212,0.915473689971902,
2.81589229255365));
#147668=CARTESIAN_POINT('Ctrl Pts',(8.54170526179937,1.00000000003981,2.83536086236564));
#147669=CARTESIAN_POINT('',(8.576968018,-1.00000000000002,2.726833259));
#147670=CARTESIAN_POINT('Origin',(1.11022302462516E-15,-1.00000000000002,
2.22044604925031E-15));
#147671=CARTESIAN_POINT('',(8.576968018,0.999999999999982,2.726833259));
#147672=CARTESIAN_POINT('Ctrl Pts',(8.57696801766623,1.00000000014478,2.72683325938026));
#147673=CARTESIAN_POINT('Ctrl Pts',(8.50639693048896,0.888963444783309,
2.70717225418446));
#147674=CARTESIAN_POINT('Ctrl Pts',(8.44762413635101,0.769956469684064,
2.69079438744694));
#147675=CARTESIAN_POINT('Ctrl Pts',(8.32098278088488,0.424051722950995,
2.65550040263089));
#147676=CARTESIAN_POINT('Ctrl Pts',(8.28242279634777,0.188791058808397,
2.64475006193496));
#147677=CARTESIAN_POINT('Ctrl Pts',(8.29434879256285,-0.283921315911108,
2.6480745047178));
#147678=CARTESIAN_POINT('Ctrl Pts',(8.34474614742513,-0.516830885586315,
2.6621244941107));
#147679=CARTESIAN_POINT('Ctrl Pts',(8.4763028838897,-0.826237684597308,
2.69878584913351));
#147680=CARTESIAN_POINT('Ctrl Pts',(8.52324594767412,-0.915473690045216,
2.71186636657059));
#147681=CARTESIAN_POINT('Ctrl Pts',(8.57696801766623,-1.00000000014482,
2.72683325938026));
#147682=CARTESIAN_POINT('Origin',(1.11022302462516E-15,0.999999999999982,
2.22044604925031E-15));
#147683=CARTESIAN_POINT('Origin',(1.11022302462516E-15,-1.77635683940025E-14,
2.22044604925031E-15));
#147684=CARTESIAN_POINT('',(8.761478656,-1.00000000000002,2.058273977));
#147685=CARTESIAN_POINT('',(8.761478656,0.999999999999982,2.058273976));
#147686=CARTESIAN_POINT('Ctrl Pts',(8.76147865594458,-1.00000000014044,
2.0582739763956));
#147687=CARTESIAN_POINT('Ctrl Pts',(8.69081287594316,-0.888963444777774,
2.03895608293596));
#147688=CARTESIAN_POINT('Ctrl Pts',(8.63195924570963,-0.769956469677081,
2.02287111920753));
#147689=CARTESIAN_POINT('Ctrl Pts',(8.50514186759659,-0.424051722946206,
1.98821493812971));
#147690=CARTESIAN_POINT('Ctrl Pts',(8.46652625341953,-0.188791058808058,
1.97766616690805));
#147691=CARTESIAN_POINT('Ctrl Pts',(8.47846921478163,0.283921315905046,
1.98092913785784));
#147692=CARTESIAN_POINT('Ctrl Pts',(8.52893899266448,0.516830885577759,
1.99471670832763));
#147693=CARTESIAN_POINT('Ctrl Pts',(8.66067729683783,0.82623768454449,2.03072016746057));
#147694=CARTESIAN_POINT('Ctrl Pts',(8.70768450122283,0.915473689953662,
2.04356827655552));
#147695=CARTESIAN_POINT('Ctrl Pts',(8.76147865586744,1.00000000001919,2.05827397637451));
#147696=CARTESIAN_POINT('',(8.786871115,-1.00000000000002,1.947022346));
#147697=CARTESIAN_POINT('Origin',(1.11022302462516E-15,-1.00000000000002,
2.22044604925031E-15));
#147698=CARTESIAN_POINT('',(8.786871115,0.999999999999982,1.947022345));
#147699=CARTESIAN_POINT('Ctrl Pts',(8.78687111468735,1.00000000013172,1.94702234559588));
#147700=CARTESIAN_POINT('Ctrl Pts',(8.71482172704381,0.888963444773286,
1.93376643331344));
#147701=CARTESIAN_POINT('Ctrl Pts',(8.65481743424227,0.769956469677654,
1.92272285170413));
#147702=CARTESIAN_POINT('Ctrl Pts',(8.52552217123475,0.424051722949642,
1.89892299368291));
#147703=CARTESIAN_POINT('Ctrl Pts',(8.48615376474826,0.188791058808303,
1.89167242106493));
#147704=CARTESIAN_POINT('Ctrl Pts',(8.49832975116214,-0.283921315909392,
1.89391444255924));
#147705=CARTESIAN_POINT('Ctrl Pts',(8.54978365242985,-0.516830885583896,
1.90339028676294));
#147706=CARTESIAN_POINT('Ctrl Pts',(8.68409707869062,-0.826237684621147,
1.92811139900698));
#147707=CARTESIAN_POINT('Ctrl Pts',(8.73202369206082,-0.915473690093674,
1.93693131433199));
#147708=CARTESIAN_POINT('Ctrl Pts',(8.78687111474133,-1.00000000021493,
1.94702234560581));
#147709=CARTESIAN_POINT('Origin',(1.11022302462516E-15,0.999999999999982,
2.22044604925031E-15));
#147710=CARTESIAN_POINT('Origin',(1.11022302462516E-15,-1.77635683940025E-14,
2.22044604925031E-15));
#147711=CARTESIAN_POINT('',(8.910709775,-1.00000000000002,1.264615079));
#147712=CARTESIAN_POINT('',(8.910709775,0.999999999999982,1.264615079));
#147713=CARTESIAN_POINT('Ctrl Pts',(8.91070977524219,-0.999999999833344,
1.26461507908072));
#147714=CARTESIAN_POINT('Ctrl Pts',(8.83859683236404,-0.888963444559491,
1.25170938549312));
#147715=CARTESIAN_POINT('Ctrl Pts',(8.77853828457744,-0.769956469564432,
1.24096477386405));
#147716=CARTESIAN_POINT('Ctrl Pts',(8.64912487986268,-0.424051722948475,
1.21781593054578));
#147717=CARTESIAN_POINT('Ctrl Pts',(8.60971913623194,-0.188791058808248,
1.21077110255089));
#147718=CARTESIAN_POINT('Ctrl Pts',(8.62190650920452,0.283921315907853,
1.21295037893395));
#147719=CARTESIAN_POINT('Ctrl Pts',(8.67340901888982,0.516830885581736,
1.2221583686789));
#147720=CARTESIAN_POINT('Ctrl Pts',(8.80784430855032,0.826237684479382,
1.24620795789709));
#147721=CARTESIAN_POINT('Ctrl Pts',(8.85581397133016,0.915473689824291,
1.25479065095093));
#147722=CARTESIAN_POINT('Ctrl Pts',(8.91070977524219,0.999999999833308,
1.26461507908072));
#147723=CARTESIAN_POINT('',(8.926027492,-1.00000000000002,1.151535151));
#147724=CARTESIAN_POINT('Origin',(1.11022302462516E-15,-1.00000000000002,
2.22044604925031E-15));
#147725=CARTESIAN_POINT('',(8.926027492,0.999999999999982,1.151535151));
#147726=CARTESIAN_POINT('Ctrl Pts',(8.92602749223077,0.999999999828974,
1.15153515131936));
#147727=CARTESIAN_POINT('Ctrl Pts',(8.85307990351357,0.888963444557652,
1.14479106076096));
#147728=CARTESIAN_POINT('Ctrl Pts',(8.79232723139907,0.769956469565621,
1.13917068070444));
#147729=CARTESIAN_POINT('Ctrl Pts',(8.66141907032706,0.424051722951004,
1.12705657192987));
#147730=CARTESIAN_POINT('Ctrl Pts',(8.6215592131525,0.188791058808435,1.12336414473294));
#147731=CARTESIAN_POINT('Ctrl Pts',(8.63388715588223,-0.283921315911035,
1.12450569350138));
#147732=CARTESIAN_POINT('Ctrl Pts',(8.68598332699613,-0.516830885586233,
1.12933109859576));
#147733=CARTESIAN_POINT('Ctrl Pts',(8.82197203024378,-0.826237684481341,
1.14191292820709));
#147734=CARTESIAN_POINT('Ctrl Pts',(8.87049631618663,-0.915473689822919,
1.14640122864087));
#147735=CARTESIAN_POINT('Ctrl Pts',(8.92602749223077,-0.99999999982901,
1.15153515131936));
#147736=CARTESIAN_POINT('Origin',(1.11022302462516E-15,0.999999999999982,
2.22044604925031E-15));
#147737=CARTESIAN_POINT('Origin',(1.11022302462516E-15,-1.77635683940025E-14,
2.22044604925031E-15));
#147738=CARTESIAN_POINT('',(8.988197099,-1.00000000000002,0.460774244000002));
#147739=CARTESIAN_POINT('',(8.988197099,0.999999999999982,0.460774244000002));
#147740=CARTESIAN_POINT('Ctrl Pts',(8.98819709915994,-0.999999999884687,
0.460774244177401));
#147741=CARTESIAN_POINT('Ctrl Pts',(8.91521760431959,-0.888963444596554,
0.454384659487097));
#147742=CARTESIAN_POINT('Ctrl Pts',(8.85443769501692,-0.76995646958452,
0.449066909228441));
#147743=CARTESIAN_POINT('Ctrl Pts',(8.72347022429716,-0.424051722949224,
0.437611784522525));
#147744=CARTESIAN_POINT('Ctrl Pts',(8.68359162309196,-0.188791058808323,
0.434127620564111));
#147745=CARTESIAN_POINT('Ctrl Pts',(8.69592528211311,0.283921315908744,
0.435205656129238));
#147746=CARTESIAN_POINT('Ctrl Pts',(8.74804585567359,0.516830885583003,
0.439759927834071));
#147747=CARTESIAN_POINT('Ctrl Pts',(8.88409573694761,0.826237684499239,
0.451662014005322));
#147748=CARTESIAN_POINT('Ctrl Pts',(8.93264163465328,0.9154736898609,0.455910188236056));
#147749=CARTESIAN_POINT('Ctrl Pts',(8.98819709915994,0.999999999884651,
0.4607742441774));
#147750=CARTESIAN_POINT('',(8.993316745,-1.00000000000002,0.346776472999999));
#147751=CARTESIAN_POINT('Origin',(1.11022302462516E-15,-1.00000000000002,
2.22044604925031E-15));
#147752=CARTESIAN_POINT('',(8.993316745,0.999999999999982,0.346776472999999));
#147753=CARTESIAN_POINT('Ctrl Pts',(8.99331674501375,0.999999999990159,
0.346776473469501));
#147754=CARTESIAN_POINT('Ctrl Pts',(8.9200582861779,0.888963444672463,0.346598504082614));
#147755=CARTESIAN_POINT('Ctrl Pts',(8.85904637943988,0.769956469625277,
0.34644657757194));
#147756=CARTESIAN_POINT('Ctrl Pts',(8.72757931577641,0.424051722950287,
0.346115753738563));
#147757=CARTESIAN_POINT('Ctrl Pts',(8.68754893604615,0.18879105880837,0.346011201221874));
#147758=CARTESIAN_POINT('Ctrl Pts',(8.69992957774535,-0.283921315910157,
0.346043086182914));
#147759=CARTESIAN_POINT('Ctrl Pts',(8.75224857096816,-0.516830885584986,
0.346179200834908));
#147760=CARTESIAN_POINT('Ctrl Pts',(8.88881765021394,-0.826237684539527,
0.346520446308495));
#147761=CARTESIAN_POINT('Ctrl Pts',(8.93754891983274,-0.915473689935908,
0.346640994702773));
#147762=CARTESIAN_POINT('Ctrl Pts',(8.99331674501375,-0.999999999990195,
0.346776473469501));
#147763=CARTESIAN_POINT('Origin',(1.11022302462516E-15,0.999999999999982,
2.22044604925031E-15));
#147764=CARTESIAN_POINT('Origin',(1.11022302462516E-15,-1.50000000000002,
2.22044604925031E-15));
#147765=CARTESIAN_POINT('',(2.50000000035605,-1.09999999964397,2.52660774908075E-15));
#147766=CARTESIAN_POINT('',(-2.5,-1.10000000000002,2.52660774903715E-15));
#147767=CARTESIAN_POINT('Origin',(1.11022302462516E-15,-1.10000000000002,
2.22044604925031E-15));
#147768=CARTESIAN_POINT('',(2.9,-1.50000000000002,2.57559362100305E-15));
#147769=CARTESIAN_POINT('',(2.9,-1.50000000000002,2.57559362100305E-15));
#147770=CARTESIAN_POINT('Origin',(1.11022302462516E-15,-1.50000000000002,
2.22044604925031E-15));
#147771=CARTESIAN_POINT('Origin',(1.11022302462516E-15,-1.10000000000002,
2.22044604925031E-15));
#147772=CARTESIAN_POINT('Origin',(-6.,-1.30000000000002,2.22044604925031E-15));
#147773=CARTESIAN_POINT('',(-4.5,-1.30000000000002,2.40414306912242E-15));
#147774=CARTESIAN_POINT('',(-7.5,-1.30000000000002,2.40414306912242E-15));
#147775=CARTESIAN_POINT('Origin',(-6.,-1.30000000000002,2.22044604925031E-15));
#147776=CARTESIAN_POINT('',(-4.30000000017802,-1.50000000017804,2.42863600508356E-15));
#147777=CARTESIAN_POINT('',(-4.5,-1.30000000000002,2.40414306912242E-15));
#147778=CARTESIAN_POINT('Origin',(-6.,-1.50000000000002,2.22044604925031E-15));
#147779=CARTESIAN_POINT('Origin',(-6.,-1.30000000000002,2.22044604925031E-15));
#147780=CARTESIAN_POINT('Origin',(6.,-1.30000000000002,2.22044604925031E-15));
#147781=CARTESIAN_POINT('',(7.5,-1.30000000000002,2.40414306912242E-15));
#147782=CARTESIAN_POINT('',(4.5,-1.30000000000002,2.40414306912242E-15));
#147783=CARTESIAN_POINT('Origin',(6.,-1.30000000000002,2.22044604925031E-15));
#147784=CARTESIAN_POINT('',(7.69999999982198,-1.50000000017804,2.42863600508356E-15));
#147785=CARTESIAN_POINT('',(7.5,-1.30000000000002,2.40414306912242E-15));
#147786=CARTESIAN_POINT('Origin',(6.,-1.50000000000002,2.22044604925031E-15));
#147787=CARTESIAN_POINT('Origin',(6.,-1.30000000000002,2.22044604925031E-15));
#147788=CARTESIAN_POINT('Origin',(1.11022302462516E-15,2.49999999999998,
2.22044604925031E-15));
#147789=CARTESIAN_POINT('',(8.99999999982198,2.29999999982196,3.32262816846113E-15));
#147790=CARTESIAN_POINT('',(-9.,2.29999999999998,3.32262816848293E-15));
#147791=CARTESIAN_POINT('Origin',(1.11022302462516E-15,2.29999999999998,
2.22044604925031E-15));
#147792=CARTESIAN_POINT('',(8.8,2.49999999999998,3.29813523249998E-15));
#147793=CARTESIAN_POINT('',(8.8,2.49999999999998,3.29813523249998E-15));
#147794=CARTESIAN_POINT('Origin',(1.11022302462516E-15,2.49999999999998,
2.22044604925031E-15));
#147795=CARTESIAN_POINT('Origin',(1.11022302462516E-15,2.29999999999998,
2.22044604925031E-15));
#147796=CARTESIAN_POINT('Origin',(6.,2.49999999999998,2.22044604925031E-15));
#147797=CARTESIAN_POINT('',(4.49999999982198,2.29999999982196,2.40414306914422E-15));
#147798=CARTESIAN_POINT('Origin',(6.,2.29999999999998,2.22044604925031E-15));
#147799=CARTESIAN_POINT('',(4.3,2.49999999999998,2.42863600510536E-15));
#147800=CARTESIAN_POINT('',(4.3,2.49999999999998,2.42863600510536E-15));
#147801=CARTESIAN_POINT('Origin',(6.,2.49999999999998,2.22044604925031E-15));
#147802=CARTESIAN_POINT('Origin',(-6.,2.49999999999998,2.22044604925031E-15));
#147803=CARTESIAN_POINT('',(-7.50000000017802,2.29999999982196,2.40414306914422E-15));
#147804=CARTESIAN_POINT('Origin',(-6.,2.29999999999998,2.22044604925031E-15));
#147805=CARTESIAN_POINT('',(-7.7,2.49999999999998,2.42863600510536E-15));
#147806=CARTESIAN_POINT('',(-7.7,2.49999999999998,2.42863600510536E-15));
#147807=CARTESIAN_POINT('Origin',(-6.,2.49999999999998,2.22044604925031E-15));
#147808=CARTESIAN_POINT('Origin',(1.11022302462516E-15,4.99999999999998,
2.22044604925031E-15));
#147809=CARTESIAN_POINT('',(3.49999999982198,4.79999999982196,2.64907242893008E-15));
#147810=CARTESIAN_POINT('',(-3.5,4.79999999999998,2.64907242895189E-15));
#147811=CARTESIAN_POINT('Origin',(1.11022302462516E-15,4.79999999999998,
2.22044604925031E-15));
#147812=CARTESIAN_POINT('',(3.3,4.99999999999998,2.62457949296894E-15));
#147813=CARTESIAN_POINT('',(3.3,4.99999999999998,2.62457949296894E-15));
#147814=CARTESIAN_POINT('Origin',(1.11022302462516E-15,4.99999999999998,
2.22044604925031E-15));
#147815=CARTESIAN_POINT('Origin',(1.11022302462516E-15,4.79999999999998,
2.22044604925031E-15));
#147816=CARTESIAN_POINT('Origin',(1.11022302462516E-15,4.79999999999998,
2.22044604925031E-15));
#147817=CARTESIAN_POINT('',(-2.5,4.79999999999998,2.52660774903715E-15));
#147818=CARTESIAN_POINT('Origin',(1.11022302462516E-15,4.79999999999998,
2.22044604925031E-15));
#147819=CARTESIAN_POINT('',(-2.69999999982198,5.00000000017801,2.5511006849983E-15));
#147820=CARTESIAN_POINT('',(-2.5,4.79999999999998,2.52660774903715E-15));
#147821=CARTESIAN_POINT('Origin',(1.11022302462516E-15,4.99999999999998,
2.22044604925031E-15));
#147822=CARTESIAN_POINT('Origin',(-6.,-1.50000000000002,2.22044604925031E-15));
#147823=CARTESIAN_POINT('',(-7.5,-1.50000000000002,2.40414306912242E-15));
#147824=CARTESIAN_POINT('Origin',(6.,-1.50000000000002,2.22044604925031E-15));
#147825=CARTESIAN_POINT('',(4.5,-1.50000000000002,2.40414306912242E-15));
#147826=CARTESIAN_POINT('Origin',(1.11022302462516E-15,-1.00000000000002,
2.22044604925031E-15));
#147827=CARTESIAN_POINT('',(8.671878177,-1.32768940200002,0.0866025400000026));
#147828=CARTESIAN_POINT('',(8.671878177,-1.32768940200002,-0.0866025400000003));
#147829=CARTESIAN_POINT('Ctrl Pts',(8.67187817702724,-1.32768940206672,
0.0866025400494723));
#147830=CARTESIAN_POINT('Ctrl Pts',(8.66616846994706,-1.3334449271527,0.0819858522682004));
#147831=CARTESIAN_POINT('Ctrl Pts',(8.66092780725788,-1.33873894467796,
0.0762673294526388));
#147832=CARTESIAN_POINT('Ctrl Pts',(8.64993438117684,-1.34985996696303,
0.0603505832064055));
#147833=CARTESIAN_POINT('Ctrl Pts',(8.64487598591024,-1.35499086504381,
0.0494502637821226));
#147834=CARTESIAN_POINT('Ctrl Pts',(8.63800999226789,-1.36196031874185,
0.0255744021040338));
#147835=CARTESIAN_POINT('Ctrl Pts',(8.63624826494697,-1.36375173570061,
0.0128536662840273));
#147836=CARTESIAN_POINT('Ctrl Pts',(8.63624826494697,-1.36375173570061,
2.22044604925031E-15));
#147837=CARTESIAN_POINT('Ctrl Pts',(8.63624826494697,-1.36375173570061,
-0.00730777731083654));
#147838=CARTESIAN_POINT('Ctrl Pts',(8.63681787290187,-1.36317274212995,
-0.0145911248958308));
#147839=CARTESIAN_POINT('Ctrl Pts',(8.63907576227445,-1.3608789882621,-0.0288572911900964));
#147840=CARTESIAN_POINT('Ctrl Pts',(8.64075793401352,-1.35917045581577,
-0.0357924289474276));
#147841=CARTESIAN_POINT('Ctrl Pts',(8.64690488602001,-1.35293307609673,
-0.0542397254755866));
#147842=CARTESIAN_POINT('Ctrl Pts',(8.65245472483424,-1.34730670087632,
-0.0648458367127547));
#147843=CARTESIAN_POINT('Ctrl Pts',(8.66314315367645,-1.33650155461798,
-0.0786155019109556));
#147844=CARTESIAN_POINT('Ctrl Pts',(8.66736782138124,-1.33223595142604,
-0.0829556097415421));
#147845=CARTESIAN_POINT('Ctrl Pts',(8.67187817702726,-1.3276894020667,-0.0866025400494835));
#147846=CARTESIAN_POINT('Ctrl Pts',(8.99331674490455,-1.00000000018596,
0.346776473354771));
#147847=CARTESIAN_POINT('Ctrl Pts',(8.88752172769541,-1.10901473823108,
0.261175104387876));
#147848=CARTESIAN_POINT('Ctrl Pts',(8.78035308155774,-1.21834403191783,
0.174311900770753));
#147849=CARTESIAN_POINT('Ctrl Pts',(8.67187817714367,-1.32768940195315,
0.0866025397638899));
#147850=CARTESIAN_POINT('',(8.644730737,-1.32768940200002,0.691087263000001));
#147851=CARTESIAN_POINT('Ctrl Pts',(8.64473073694086,-1.32768940194368,
0.69108726299106));
#147852=CARTESIAN_POINT('Ctrl Pts',(8.76063136896071,-1.21834383455991,
0.61345446945312));
#147853=CARTESIAN_POINT('Ctrl Pts',(8.87515482087759,-1.10901465443497,
0.53654755682168));
#147854=CARTESIAN_POINT('Ctrl Pts',(8.9881970992204,-1.00000000007974,0.460774244214116));
#147855=CARTESIAN_POINT('',(8.629204753,-1.32768940200002,0.863595070000001));
#147856=CARTESIAN_POINT('Ctrl Pts',(8.64473073689486,-1.3276894020015,0.691087262840869));
#147857=CARTESIAN_POINT('Ctrl Pts',(8.63991163031322,-1.33223595135028,
0.694315206512238));
#147858=CARTESIAN_POINT('Ctrl Pts',(8.63531492562229,-1.33650155453273,
0.698259146043817));
#147859=CARTESIAN_POINT('Ctrl Pts',(8.62343522198836,-1.34730670078397,
0.711015275232578));
#147860=CARTESIAN_POINT('Ctrl Pts',(8.6169570007115,-1.35293307600527,0.721081205667737));
#147861=CARTESIAN_POINT('Ctrl Pts',(8.60918119161373,-1.35917045572572,
0.738903230273293));
#147862=CARTESIAN_POINT('Ctrl Pts',(8.60688413084748,-1.36087898817255,
0.745659660492595));
#147863=CARTESIAN_POINT('Ctrl Pts',(8.6033565217857,-1.36317274204141,0.759665999752384));
#147864=CARTESIAN_POINT('Ctrl Pts',(8.6021363326606,-1.36375173561258,0.766868967457794));
#147865=CARTESIAN_POINT('Ctrl Pts',(8.6014812685525,-1.36375173561308,0.774147325805647));
#147866=CARTESIAN_POINT('Ctrl Pts',(8.60032907478934,-1.36375173561396,
0.786949247007953));
#147867=CARTESIAN_POINT('Ctrl Pts',(8.60094343194574,-1.36196031865609,
0.799776692904925));
#147868=CARTESIAN_POINT('Ctrl Pts',(8.60564156937475,-1.35499086495975,
0.82417190030865));
#147869=CARTESIAN_POINT('Ctrl Pts',(8.60970250392851,-1.3498599668798,0.835481769307738));
#147870=CARTESIAN_POINT('Ctrl Pts',(8.61922490753858,-1.33873894463695,
0.852319882468268));
#147871=CARTESIAN_POINT('Ctrl Pts',(8.62393186837942,-1.33344492716415,
0.858485153528086));
#147872=CARTESIAN_POINT('Ctrl Pts',(8.6292047530988,-1.3276894021372,0.863595070052561));
#147873=CARTESIAN_POINT('Ctrl Pts',(8.92602749216612,-1.00000000026639,
1.1515351511352));
#147874=CARTESIAN_POINT('Ctrl Pts',(8.8283316221154,-1.10901473835186,1.0567949958371));
#147875=CARTESIAN_POINT('Ctrl Pts',(8.72938076294725,-1.2183440320791,0.960674954515168));
#147876=CARTESIAN_POINT('Ctrl Pts',(8.6292047530771,-1.32768940215461,0.863595070094576));
#147877=CARTESIAN_POINT('',(8.547981008,-1.32768940200002,1.463212838));
#147878=CARTESIAN_POINT('Ctrl Pts',(8.54798100788837,-1.32768940187192,
1.46321283800514));
#147879=CARTESIAN_POINT('Ctrl Pts',(8.67037400794378,-1.21834383453907,
1.39628182386026));
#147880=CARTESIAN_POINT('Ctrl Pts',(8.79133030455683,-1.10901465446516,
1.32995031896543));
#147881=CARTESIAN_POINT('Ctrl Pts',(8.91070977524376,-1.00000000016074,
1.26461507917722));
#147882=CARTESIAN_POINT('',(8.517054046,-1.32768940200002,1.633634441));
#147883=CARTESIAN_POINT('Ctrl Pts',(8.54798100783859,-1.32768940196088,
1.4632128377687));
#147884=CARTESIAN_POINT('Ctrl Pts',(8.5428919508647,-1.33223595136504,1.46599580531845));
#147885=CARTESIAN_POINT('Ctrl Pts',(8.53796021908521,-1.33650155459769,
1.4695118223078));
#147886=CARTESIAN_POINT('Ctrl Pts',(8.52498488898969,-1.34730670089114,
1.48115171069211));
#147887=CARTESIAN_POINT('Ctrl Pts',(8.5176304440792,-1.3529330761124,1.49059641537225));
#147888=CARTESIAN_POINT('Ctrl Pts',(8.50828838413339,-1.35917045583282,
1.50764967559236));
#147889=CARTESIAN_POINT('Ctrl Pts',(8.50539492892274,-1.36087898827965,
1.51417299947031));
#147890=CARTESIAN_POINT('Ctrl Pts',(8.50062600240598,-1.36317274214851,
1.52780674088759));
#147891=CARTESIAN_POINT('Ctrl Pts',(8.49876505635617,-1.36375173571968,
1.53487133465274));
#147892=CARTESIAN_POINT('Ctrl Pts',(8.4974602023311,-1.36375173572018,1.54206167297575));
#147893=CARTESIAN_POINT('Ctrl Pts',(8.49516509159167,-1.36375173572105,
1.55470877555439));
#147894=CARTESIAN_POINT('Ctrl Pts',(8.49462713214117,-1.36196031876316,
1.56753965247642));
#147895=CARTESIAN_POINT('Ctrl Pts',(8.49711958671715,-1.35499086506676,
1.59225778973971));
#147896=CARTESIAN_POINT('Ctrl Pts',(8.50015036430107,-1.34985996698678,
1.6038861478983));
#147897=CARTESIAN_POINT('Ctrl Pts',(8.50812507669321,-1.33873894473423,
1.62151005745983));
#147898=CARTESIAN_POINT('Ctrl Pts',(8.51226043806651,-1.33344492724917,
1.62807243767969));
#147899=CARTESIAN_POINT('Ctrl Pts',(8.51705404632889,-1.3276894022084,1.63363444093218));
#147900=CARTESIAN_POINT('Ctrl Pts',(8.78687111486193,-0.999999999752185,
1.94702234585691));
#147901=CARTESIAN_POINT('Ctrl Pts',(8.69806098154262,-1.10901473805156,
1.84390619609545));
#147902=CARTESIAN_POINT('Ctrl Pts',(8.60812460334816,-1.2183440319946,1.73930321896202));
#147903=CARTESIAN_POINT('Ctrl Pts',(8.51705404621577,-1.327689402286,1.63363444110997));
#147904=CARTESIAN_POINT('',(8.382407962,-1.32768940200002,2.223557482));
#147905=CARTESIAN_POINT('Ctrl Pts',(8.38240796213464,-1.32768940171091,
2.22355748287687));
#147906=CARTESIAN_POINT('Ctrl Pts',(8.51030789375738,-1.21834383440846,
2.16786713730407));
#147907=CARTESIAN_POINT('Ctrl Pts',(8.63672316609019,-1.10901465436549,
2.11264510242942));
#147908=CARTESIAN_POINT('Ctrl Pts',(8.7614786558207,-1.00000000009201,2.05827397640414));
#147909=CARTESIAN_POINT('',(8.336329029,-1.32768940200002,2.390520747));
#147910=CARTESIAN_POINT('Ctrl Pts',(8.38240796207935,-1.32768940188413,
2.22355748240969));
#147911=CARTESIAN_POINT('Ctrl Pts',(8.37708992878106,-1.33223595136664,
2.22587306701158));
#147912=CARTESIAN_POINT('Ctrl Pts',(8.37186287728827,-1.33650155467049,
2.22893285255653));
#147913=CARTESIAN_POINT('Ctrl Pts',(8.3578963904289,-1.34730670102585,2.23936278260429));
#147914=CARTESIAN_POINT('Ctrl Pts',(8.34972493555017,-1.35293307624908,
2.24811021831966));
#147915=CARTESIAN_POINT('Ctrl Pts',(8.3388918415288,-1.35917045597279,2.26425741132905));
#147916=CARTESIAN_POINT('Ctrl Pts',(8.33542528827331,-1.36087898842084,
2.27049510689713));
#147917=CARTESIAN_POINT('Ctrl Pts',(8.32945344089288,-1.36317274229213,
2.28364647960213));
#147918=CARTESIAN_POINT('Ctrl Pts',(8.32696672116126,-1.36375173586451,
2.29051581947185));
#147919=CARTESIAN_POINT('Ctrl Pts',(8.32502258313609,-1.36375173586619,
2.29756024539374));
#147920=CARTESIAN_POINT('Ctrl Pts',(8.32160303430179,-1.36375173586915,
2.30995070231481));
#147921=CARTESIAN_POINT('Ctrl Pts',(8.31991708957669,-1.36196031891332,
2.32268170358541));
#147922=CARTESIAN_POINT('Ctrl Pts',(8.32018379351913,-1.35499086522079,
2.34752375480154));
#147923=CARTESIAN_POINT('Ctrl Pts',(8.32216001209317,-1.3498599671427,2.3593769774175));
#147924=CARTESIAN_POINT('Ctrl Pts',(8.32852282561185,-1.3387389448062,2.37764478615217));
#147925=CARTESIAN_POINT('Ctrl Pts',(8.33205329208909,-1.33344492721209,
2.3845514392093));
#147926=CARTESIAN_POINT('Ctrl Pts',(8.33632902867257,-1.32768940204801,
2.39052074728081));
#147927=CARTESIAN_POINT('Ctrl Pts',(8.57696801758913,-1.00000000005396,
2.72683325934723));
#147928=CARTESIAN_POINT('Ctrl Pts',(8.4977586683085,-1.10901473814976,2.61617134608161));
#147929=CARTESIAN_POINT('Ctrl Pts',(8.41756088626376,-1.21834403188794,
2.50392763516743));
#147930=CARTESIAN_POINT('Ctrl Pts',(8.33632902879468,-1.32768940197433,
2.3905207471223));
#147931=CARTESIAN_POINT('',(8.149344695,-1.32768940200002,2.965999351));
#147932=CARTESIAN_POINT('Ctrl Pts',(8.1493446952874,-1.32768940216563,2.96599935145307));
#147933=CARTESIAN_POINT('Ctrl Pts',(8.281721783784,-1.21834383463976,2.92199806015237));
#147934=CARTESIAN_POINT('Ctrl Pts',(8.41257821073727,-1.10901465437208,
2.87833011043717));
#147935=CARTESIAN_POINT('Ctrl Pts',(8.54170526199449,-0.999999999874976,
2.83536086230067));
#147936=CARTESIAN_POINT('',(8.088484791,-1.32768940200002,3.128159987));
#147937=CARTESIAN_POINT('Ctrl Pts',(8.14934469528429,-1.32768940220673,
2.96599935134145));
#147938=CARTESIAN_POINT('Ctrl Pts',(8.14384050348253,-1.33223595163132,
2.96782890925026));
#147939=CARTESIAN_POINT('Ctrl Pts',(8.13836021756285,-1.33650155488223,
2.97040782769713));
#147940=CARTESIAN_POINT('Ctrl Pts',(8.12351502401358,-1.3473067011882,2.97954382365383));
#147941=CARTESIAN_POINT('Ctrl Pts',(8.11459235092013,-1.35293307640658,
2.98752356120022));
#147942=CARTESIAN_POINT('Ctrl Pts',(8.10235544453278,-1.35917045612245,
3.00263467930046));
#147943=CARTESIAN_POINT('Ctrl Pts',(8.09834370388334,-1.36087898856765,
3.00853652430322));
#147944=CARTESIAN_POINT('Ctrl Pts',(8.09121701744786,-1.36317274243324,
3.02109964117804));
#147945=CARTESIAN_POINT('Ctrl Pts',(8.08812454564212,-1.36375173600275,
3.02771841926748));
#147946=CARTESIAN_POINT('Ctrl Pts',(8.08555677667574,-1.36375173600163,
3.03456021521294));
#147947=CARTESIAN_POINT('Ctrl Pts',(8.08104032194735,-1.36375173599966,
3.04659426580439));
#147948=CARTESIAN_POINT('Ctrl Pts',(8.07821996618797,-1.36196031903889,
3.05912288888715));
#147949=CARTESIAN_POINT('Ctrl Pts',(8.0762587721631,-1.35499086533698,3.08388884046511));
#147950=CARTESIAN_POINT('Ctrl Pts',(8.07716452038241,-1.34985996725432,
3.09587149235794));
#147951=CARTESIAN_POINT('Ctrl Pts',(8.08186420533724,-1.33873894491981,
3.11463611845345));
#147952=CARTESIAN_POINT('Ctrl Pts',(8.08476135158299,-1.33344492733438,
3.12183143591672));
#147953=CARTESIAN_POINT('Ctrl Pts',(8.08848479065032,-1.32768940218083,
3.12815998737018));
#147954=CARTESIAN_POINT('Ctrl Pts',(8.29800821672472,-1.00000000020416,
3.48468931635154));
#147955=CARTESIAN_POINT('Ctrl Pts',(8.22903739841269,-1.10901473827415,
3.3673726241933));
#147956=CARTESIAN_POINT('Ctrl Pts',(8.15922391772688,-1.21834403198615,
3.2483918998115));
#147957=CARTESIAN_POINT('Ctrl Pts',(8.0884847908968,-1.32768940204711,3.12815998710355));
#147958=CARTESIAN_POINT('',(7.850667698,-1.32768940200002,3.684560736));
#147959=CARTESIAN_POINT('Ctrl Pts',(7.85066769785711,-1.32768940157742,
3.68456073683881));
#147960=CARTESIAN_POINT('Ctrl Pts',(7.98645612010734,-1.21834383433082,
3.65260277261618));
#147961=CARTESIAN_POINT('Ctrl Pts',(8.12070012204856,-1.109014654343,3.62084049699315));
#147962=CARTESIAN_POINT('Ctrl Pts',(8.25315907913426,-1.00000000012426,
3.58961909013581));
#147963=CARTESIAN_POINT('',(7.77551683,-1.32768940200002,3.840613121));
#147964=CARTESIAN_POINT('Ctrl Pts',(7.85066769791922,-1.32768940194829,
3.68456073583356));
#147965=CARTESIAN_POINT('Ctrl Pts',(7.84502166401928,-1.3322359514189,3.68588953652913));
#147966=CARTESIAN_POINT('Ctrl Pts',(7.83933226760092,-1.33650155471162,
3.68796682397788));
#147967=CARTESIAN_POINT('Ctrl Pts',(7.82372789202242,-1.34730670105384,
3.69573532823493));
#147968=CARTESIAN_POINT('Ctrl Pts',(7.81412584082864,-1.35293307627325,
3.70288311945405));
#147969=CARTESIAN_POINT('Ctrl Pts',(7.80058364644547,-1.35917045599075,
3.71683649680359));
#147970=CARTESIAN_POINT('Ctrl Pts',(7.79605901857717,-1.36087898843652,
3.7223549730541));
#147971=CARTESIAN_POINT('Ctrl Pts',(7.78783487297178,-1.36317274230327,
3.73422868326695));
#147972=CARTESIAN_POINT('Ctrl Pts',(7.78416154785463,-1.36375173587338,
3.74054360906622));
#147973=CARTESIAN_POINT('Ctrl Pts',(7.78099082211099,-1.36375173587283,
3.74712768891714));
#147974=CARTESIAN_POINT('Ctrl Pts',(7.7754138253233,-1.36375173587187,3.75870844207817));
#147975=CARTESIAN_POINT('Ctrl Pts',(7.77148176637241,-1.36196031891213,
3.77093381386658));
#147976=CARTESIAN_POINT('Ctrl Pts',(7.76730846475425,-1.3549908652122,3.7954242649276));
#147977=CARTESIAN_POINT('Ctrl Pts',(7.76713645006289,-1.3498599671305,3.80743986883125));
#147978=CARTESIAN_POINT('Ctrl Pts',(7.77013516735406,-1.33873894479117,
3.82655023058136));
#147979=CARTESIAN_POINT('Ctrl Pts',(7.77237566726015,-1.33344492719834,
3.83397628000857));
#147980=CARTESIAN_POINT('Ctrl Pts',(7.77551682988422,-1.32768940203628,
3.84061312108624));
#147981=CARTESIAN_POINT('Ctrl Pts',(7.95223773319059,-1.00000000030882,
4.2144887031835));
#147982=CARTESIAN_POINT('Ctrl Pts',(7.8940607583389,-1.10901473835463,4.09146179706751));
#147983=CARTESIAN_POINT('Ctrl Pts',(7.83519367612302,-1.21834403204217,
3.96670202196033));
#147984=CARTESIAN_POINT('Ctrl Pts',(7.77551682979918,-1.32768940207848,
3.8406131211631));
#147985=CARTESIAN_POINT('',(7.488781739,-1.32768940200002,4.373456205));
#147986=CARTESIAN_POINT('Ctrl Pts',(7.48878173910531,-1.32768940203771,
4.3734562055302));
#147987=CARTESIAN_POINT('Ctrl Pts',(7.62688820723029,-1.2183438345691,4.3537988749128));
#147988=CARTESIAN_POINT('Ctrl Pts',(7.76343893103024,-1.1090146543582,4.33419800434109));
#147989=CARTESIAN_POINT('Ctrl Pts',(7.89816331292909,-0.999999999917447,
4.3149758149713));
#147990=CARTESIAN_POINT('',(7.399944978,-1.32768940200002,4.522143898));
#147991=CARTESIAN_POINT('Ctrl Pts',(7.48878173912938,-1.32768940209639,
4.37345620537261));
#147992=CARTESIAN_POINT('Ctrl Pts',(7.48303932181701,-1.33223595148124,
4.37427355014363));
#147993=CARTESIAN_POINT('Ctrl Pts',(7.47718662272123,-1.33650155469588,
4.37583248146923));
#147994=CARTESIAN_POINT('Ctrl Pts',(7.46094870251594,-1.34730670096865,
4.38217094653701));
#147995=CARTESIAN_POINT('Ctrl Pts',(7.45074458329346,-1.35293307618431,
4.38842924161994));
#147996=CARTESIAN_POINT('Ctrl Pts',(7.43600613470365,-1.35917045589565,
4.40111253383242));
#147997=CARTESIAN_POINT('Ctrl Pts',(7.43100504926068,-1.36087898833917,
4.40620320980585));
#147998=CARTESIAN_POINT('Ctrl Pts',(7.42174966047235,-1.3631727422014,4.41729191322548));
#147999=CARTESIAN_POINT('Ctrl Pts',(7.41752505749903,-1.36375173576924,
4.42325214266577));
#148000=CARTESIAN_POINT('Ctrl Pts',(7.41377690379883,-1.36375173576648,
4.42952549528285));
#148001=CARTESIAN_POINT('Ctrl Pts',(7.4071842676527,-1.36375173576164,4.44055970959978));
#148002=CARTESIAN_POINT('Ctrl Pts',(7.4021721641394,-1.36196031879803,4.45238339858913));
#148003=CARTESIAN_POINT('Ctrl Pts',(7.39582035590394,-1.3549908650908,4.47640116642154));
#148004=CARTESIAN_POINT('Ctrl Pts',(7.39457196326603,-1.34985996700553,
4.48835297975807));
#148005=CARTESIAN_POINT('Ctrl Pts',(7.39584556898714,-1.33873894466817,
4.5076552117413));
#148006=CARTESIAN_POINT('Ctrl Pts',(7.39741138335892,-1.33344492708259,
4.51525220292776));
#148007=CARTESIAN_POINT('Ctrl Pts',(7.39994497873345,-1.32768940192929,
4.52214389767129));
#148008=CARTESIAN_POINT('Ctrl Pts',(7.54244050677706,-1.00000000021305,
4.91035550626368));
#148009=CARTESIAN_POINT('Ctrl Pts',(7.49552578212922,-1.10901473827983,
4.78260892651342));
#148010=CARTESIAN_POINT('Ctrl Pts',(7.44807906146581,-1.21834403198914,
4.65307459304683));
#148011=CARTESIAN_POINT('Ctrl Pts',(7.39994497847541,-1.32768940204821,
4.52214389786548));
#148012=CARTESIAN_POINT('',(7.066600514,-1.32768940200002,5.027139175));
#148013=CARTESIAN_POINT('Ctrl Pts',(7.06660051407375,-1.32768940204712,
5.02713917571187));
#148014=CARTESIAN_POINT('Ctrl Pts',(7.20591307568901,-1.21834383453908,
5.01994074814748));
#148015=CARTESIAN_POINT('Ctrl Pts',(7.34367109490997,-1.10901465428964,
5.01265909749143));
#148016=CARTESIAN_POINT('Ctrl Pts',(7.47957617982504,-0.999999999810885,
5.00559089155299));
#148017=CARTESIAN_POINT('',(6.964793122,-1.32768940200002,5.167265029));
#148018=CARTESIAN_POINT('Ctrl Pts',(7.06660051416282,-1.32768940218437,
5.0271391753499));
#148019=CARTESIAN_POINT('Ctrl Pts',(7.06080794801293,-1.33223595147841,
5.0274384834299));
#148020=CARTESIAN_POINT('Ctrl Pts',(7.05483906874339,-1.33650155461117,
5.02846650704578));
#148021=CARTESIAN_POINT('Ctrl Pts',(7.0380983421117,-1.34730670081975,5.0333238993322));
#148022=CARTESIAN_POINT('Ctrl Pts',(7.02737431242565,-1.35293307604024,
5.03864231015989));
#148023=CARTESIAN_POINT('Ctrl Pts',(7.01155827494509,-1.35917045575939,
5.04995339881578));
#148024=CARTESIAN_POINT('Ctrl Pts',(7.00612099772445,-1.36087898820575,
5.05457528737984));
#148025=CARTESIAN_POINT('Ctrl Pts',(6.99590888469631,-1.36317274207367,
5.06478970428213));
#148026=CARTESIAN_POINT('Ctrl Pts',(6.99116701788302,-1.36375173564436,
5.07034724909893));
#148027=CARTESIAN_POINT('Ctrl Pts',(6.9868716141528,-1.36375173564439,5.07625936513458));
#148028=CARTESIAN_POINT('Ctrl Pts',(6.9793164186734,-1.36375173564445,5.08665819959848));
#148029=CARTESIAN_POINT('Ctrl Pts',(6.97326462510242,-1.36196031868576,
5.09798500839568));
#148030=CARTESIAN_POINT('Ctrl Pts',(6.96478545126267,-1.35499086498787,
5.121336716054));
#148031=CARTESIAN_POINT('Ctrl Pts',(6.96247073199497,-1.34985996690716,
5.13312850985036));
#148032=CARTESIAN_POINT('Ctrl Pts',(6.96200897181235,-1.33873894460026,
5.15246720181947));
#148033=CARTESIAN_POINT('Ctrl Pts',(6.9628874936231,-1.33344492704721,5.16017396823523));
#148034=CARTESIAN_POINT('Ctrl Pts',(6.96479312271032,-1.32768940192987,
5.16726502875217));
#148035=CARTESIAN_POINT('Ctrl Pts',(7.07191598493006,-1.0000000000433,5.56668701305468));
#148036=CARTESIAN_POINT('Ctrl Pts',(7.03664124030446,-1.1090147382238,5.43524929978373));
#148037=CARTESIAN_POINT('Ctrl Pts',(7.00099689432893,-1.21834403204728,
5.30198334200609));
#148038=CARTESIAN_POINT('Ctrl Pts',(6.96479312204206,-1.32768940221948,
5.16726502916683));
#148039=CARTESIAN_POINT('',(6.587523177,-1.32768940200002,5.640346578));
#148040=CARTESIAN_POINT('Ctrl Pts',(6.58752317677662,-1.3276894017101,5.64034657789402));
#148041=CARTESIAN_POINT('Ctrl Pts',(6.72692016891382,-1.2183438343021,5.64566501082948));
#148042=CARTESIAN_POINT('Ctrl Pts',(6.86477633685045,-1.10901465415312,
5.6507612075996));
#148043=CARTESIAN_POINT('Ctrl Pts',(7.00076789681646,-0.999999999774394,
5.65590389407081));
#148044=CARTESIAN_POINT('',(6.473564847,-1.32768940200002,5.770782381));
#148045=CARTESIAN_POINT('Ctrl Pts',(6.58752317690416,-1.32768940185458,
5.64034657752293));
#148046=CARTESIAN_POINT('Ctrl Pts',(6.58172709993427,-1.33223595135912,
5.64012543898217));
#148047=CARTESIAN_POINT('Ctrl Pts',(6.57569009804838,-1.33650155468271,
5.64061427785487));
#148048=CARTESIAN_POINT('Ctrl Pts',(6.55858135111834,-1.34730670105205,
5.64395148859084));
#148049=CARTESIAN_POINT('Ctrl Pts',(6.5474237545518,-1.35293307627263,5.64828719444978));
#148050=CARTESIAN_POINT('Ctrl Pts',(6.53065746961772,-1.359170455992,5.65813500931785));
#148051=CARTESIAN_POINT('Ctrl Pts',(6.52482777837964,-1.36087898843847,
5.66225089774472));
#148052=CARTESIAN_POINT('Ctrl Pts',(6.51374116304361,-1.36317274230659,
5.6715087876528));
#148053=CARTESIAN_POINT('Ctrl Pts',(6.50852021111509,-1.36375173587738,
5.67661890176379));
#148054=CARTESIAN_POINT('Ctrl Pts',(6.50371214142148,-1.36375173587751,
5.6821221803364));
#148055=CARTESIAN_POINT('Ctrl Pts',(6.49525521660246,-1.36375173587774,
5.69180190964827));
#148056=CARTESIAN_POINT('Ctrl Pts',(6.48821245845978,-1.36196031891918,
5.7025406414498));
#148057=CARTESIAN_POINT('Ctrl Pts',(6.47767418834347,-1.35499086522148,
5.72503827471508));
#148058=CARTESIAN_POINT('Ctrl Pts',(6.47431177920769,-1.34985996714087,
5.73657510838082));
#148059=CARTESIAN_POINT('Ctrl Pts',(6.47211837095175,-1.33873894483526,
5.7557945565959));
#148060=CARTESIAN_POINT('Ctrl Pts',(6.47230252687583,-1.33344492728374,
5.76354904792197));
#148061=CARTESIAN_POINT('Ctrl Pts',(6.47356484669523,-1.32768940216811,
5.77078238118694));
#148062=CARTESIAN_POINT('Ctrl Pts',(6.54445255389812,-0.999999999960807,
6.17819882898586));
#148063=CARTESIAN_POINT('Ctrl Pts',(6.52110180080846,-1.10901473814172,
6.04412824156698));
#148064=CARTESIAN_POINT('Ctrl Pts',(6.49754681684949,-1.21834403196544,
5.90820363880618));
#148065=CARTESIAN_POINT('Ctrl Pts',(6.47356484676908,-1.32768940213768,
5.77078238114983));
#148066=CARTESIAN_POINT('',(6.055406976,-1.32768940200002,6.208141225));
#148067=CARTESIAN_POINT('Ctrl Pts',(6.05540697605073,-1.32768940208598,
6.20814122513386));
#148068=CARTESIAN_POINT('Ctrl Pts',(6.19376605621082,-1.21834383468118,
6.22593369766439));
#148069=CARTESIAN_POINT('Ctrl Pts',(6.33061043617276,-1.10901465453519,
6.24336671027083));
#148070=CARTESIAN_POINT('Ctrl Pts',(6.46559354722401,-1.00000000015905,
6.26067888325481));
#148071=CARTESIAN_POINT('',(5.930215234,-1.32768940200002,6.327836787));
#148072=CARTESIAN_POINT('Ctrl Pts',(6.05540697612598,-1.3276894021538,6.20814122496572));
#148073=CARTESIAN_POINT('Ctrl Pts',(6.04965405520633,-1.33223595161668,
6.20740142034682));
#148074=CARTESIAN_POINT('Ctrl Pts',(6.04359753738465,-1.33650155490257,
6.20734713862694));
#148075=CARTESIAN_POINT('Ctrl Pts',(6.02625852002746,-1.34730670124086,
6.2091372984766));
#148076=CARTESIAN_POINT('Ctrl Pts',(6.01475719098768,-1.35293307646214,
6.21245539081279));
#148077=CARTESIAN_POINT('Ctrl Pts',(5.99717565086845,-1.35917045618277,
6.22076064307861));
#148078=CARTESIAN_POINT('Ctrl Pts',(5.99100048285915,-1.36087898862972,
6.22433739265493));
#148079=CARTESIAN_POINT('Ctrl Pts',(5.97912862812348,-1.3631727424988,6.23256421648311));
#148080=CARTESIAN_POINT('Ctrl Pts',(5.97347062711498,-1.36375173607007,
6.23718575625434));
#148081=CARTESIAN_POINT('Ctrl Pts',(5.96818860320827,-1.36375173607066,
6.24223588820087));
#148082=CARTESIAN_POINT('Ctrl Pts',(5.95889803923611,-1.36375173607169,
6.25111857687207));
#148083=CARTESIAN_POINT('Ctrl Pts',(5.95092102066963,-1.36196031911392,
6.26118276972391));
#148084=CARTESIAN_POINT('Ctrl Pts',(5.93840850223206,-1.35499086541765,
6.28264519088178));
#148085=CARTESIAN_POINT('Ctrl Pts',(5.93402547536983,-1.34985996733775,
6.29383417661584));
#148086=CARTESIAN_POINT('Ctrl Pts',(5.93011807903562,-1.33873894492255,
6.31277963757132));
#148087=CARTESIAN_POINT('Ctrl Pts',(5.92960638637303,-1.33344492723105,
6.32051941938347));
#148088=CARTESIAN_POINT('Ctrl Pts',(5.93021523353628,-1.32768940195741,
6.32783678700507));
#148089=CARTESIAN_POINT('Ctrl Pts',(5.96429703904196,-0.999999999791277,
6.73996742082874));
#148090=CARTESIAN_POINT('Ctrl Pts',(5.95305828402978,-1.10901473792973,
6.60434341685274));
#148091=CARTESIAN_POINT('Ctrl Pts',(5.94178231297559,-1.21834403171087,
6.46685455414235));
#148092=CARTESIAN_POINT('Ctrl Pts',(5.93021523383119,-1.32768940184066,
6.3278367868887));
#148093=CARTESIAN_POINT('',(5.474536198,-1.32768940200002,6.725951571));
#148094=CARTESIAN_POINT('Ctrl Pts',(5.47453619793898,-1.32768940194877,
6.72595157108985));
#148095=CARTESIAN_POINT('Ctrl Pts',(5.61074338033991,-1.21834383447162,
6.75607482866063));
#148096=CARTESIAN_POINT('Ctrl Pts',(5.74547418201546,-1.10901465425249,
6.78570429670652));
#148097=CARTESIAN_POINT('Ctrl Pts',(5.87836203967684,-0.999999999803763,
6.81504656873444));
#148098=CARTESIAN_POINT('',(5.339119014,-1.32768940200002,6.833943172));
#148099=CARTESIAN_POINT('Ctrl Pts',(5.47453619794346,-1.3276894019521,6.72595157108191));
#148100=CARTESIAN_POINT('Ctrl Pts',(5.46887275217696,-1.33223595140147,
6.72469905685192));
#148101=CARTESIAN_POINT('Ctrl Pts',(5.46284548190358,-1.33650155467468,
6.72410209158784));
#148102=CARTESIAN_POINT('Ctrl Pts',(5.44541579765377,-1.34730670099757,
6.72433078725384));
#148103=CARTESIAN_POINT('Ctrl Pts',(5.43366333807954,-1.35293307621405,
6.7266045507431));
#148104=CARTESIAN_POINT('Ctrl Pts',(5.41540809900001,-1.35917045592674,
6.73330037140443));
#148105=CARTESIAN_POINT('Ctrl Pts',(5.40893717304231,-1.36087898837075,
6.73630918424745));
#148106=CARTESIAN_POINT('Ctrl Pts',(5.39637566410318,-1.36317274223397,
6.74343870445049));
#148107=CARTESIAN_POINT('Ctrl Pts',(5.39032616891342,-1.36375173580231,
6.74753445996235));
#148108=CARTESIAN_POINT('Ctrl Pts',(5.38461271854601,-1.36375173580003,
6.75209078459071));
#148109=CARTESIAN_POINT('Ctrl Pts',(5.37456331758125,-1.36375173579604,
6.76010491443722));
#148110=CARTESIAN_POINT('Ctrl Pts',(5.36571626485717,-1.36196031883328,
6.76941353737756));
#148111=CARTESIAN_POINT('Ctrl Pts',(5.35133024154627,-1.35499086512764,
6.78966794363456));
#148112=CARTESIAN_POINT('Ctrl Pts',(5.34596188651656,-1.34985996704315,
6.80041899430357));
#148113=CARTESIAN_POINT('Ctrl Pts',(5.34037196225801,-1.33873894475413,
6.81893792987469));
#148114=CARTESIAN_POINT('Ctrl Pts',(5.33916854083174,-1.33344492722887,
6.82660068560842));
#148115=CARTESIAN_POINT('Ctrl Pts',(5.33911901311749,-1.32768940214345,
6.83394317210648));
#148116=CARTESIAN_POINT('Ctrl Pts',(5.33612051055408,-1.00000000012717,
7.24746975809871));
#148117=CARTESIAN_POINT('Ctrl Pts',(5.33708424139336,-1.10901473818033,
7.11138430241068));
#148118=CARTESIAN_POINT('Ctrl Pts',(5.33817807065952,-1.21834403187569,
6.97343815934646));
#148119=CARTESIAN_POINT('Ctrl Pts',(5.33911901369835,-1.32768940192048,
6.83394317193563));
#148120=CARTESIAN_POINT('',(4.84958767583258,-1.32768940194837,7.18960850739358));
#148121=CARTESIAN_POINT('Ctrl Pts',(4.8495876755192,-1.32768940181776,7.18960850804234));
#148122=CARTESIAN_POINT('Ctrl Pts',(4.9825462995355,-1.21834383449911,7.2318200159394));
#148123=CARTESIAN_POINT('Ctrl Pts',(5.11407874926017,-1.10901465444024,
7.27340738041884));
#148124=CARTESIAN_POINT('Ctrl Pts',(5.24380141818337,-1.00000000015116,
7.31454350482227));
#148125=CARTESIAN_POINT('',(4.705035349,-1.32768940200002,7.285026664));
#148126=CARTESIAN_POINT('Ctrl Pts',(4.84958767607712,-1.32768940218148,
7.18960850722729));
#148127=CARTESIAN_POINT('Ctrl Pts',(4.84405930425442,-1.33223595156484,
7.18785336792304));
#148128=CARTESIAN_POINT('Ctrl Pts',(4.83810980963135,-1.33650155477901,
7.18671852554355));
#148129=CARTESIAN_POINT('Ctrl Pts',(4.82072979213366,-1.34730670106102,
7.1853839156919));
#148130=CARTESIAN_POINT('Ctrl Pts',(4.80882082591909,-1.35293307628648,
7.18659504331653));
#148131=CARTESIAN_POINT('Ctrl Pts',(4.79003886832668,-1.35917045601382,
7.19162752154787));
#148132=CARTESIAN_POINT('Ctrl Pts',(4.78332428450956,-1.36087898846319,
7.19404417246096));
#148133=CARTESIAN_POINT('Ctrl Pts',(4.77017425924559,-1.36317274233714,
7.20001898632598));
#148134=CARTESIAN_POINT('Ctrl Pts',(4.76378197684948,-1.36375173591085,
7.20355598095978));
#148135=CARTESIAN_POINT('Ctrl Pts',(4.75768310136027,-1.36375173591383,
7.20758181342034));
#148136=CARTESIAN_POINT('Ctrl Pts',(4.74695577526567,-1.36375173591908,
7.2146628593743));
#148137=CARTESIAN_POINT('Ctrl Pts',(4.73730991964322,-1.36196031896553,
7.22314096483992));
#148138=CARTESIAN_POINT('Ctrl Pts',(4.72116621924342,-1.35499086527729,
7.24202427961917));
#148139=CARTESIAN_POINT('Ctrl Pts',(4.71485575887476,-1.3498599672013,7.25225083408192));
#148140=CARTESIAN_POINT('Ctrl Pts',(4.70762831330155,-1.33873894475924,
7.27019414118161));
#148141=CARTESIAN_POINT('Ctrl Pts',(4.70574285233601,-1.33344492702836,
7.27771817531577));
#148142=CARTESIAN_POINT('Ctrl Pts',(4.70503534864307,-1.32768940170969,
7.28502666373681));
#148143=CARTESIAN_POINT('Ctrl Pts',(4.66498067879555,-0.999999999952129,
7.6966197299416));
#148144=CARTESIAN_POINT('Ctrl Pts',(4.67813913625212,-1.10901473800108,
7.56116850237982));
#148145=CARTESIAN_POINT('Ctrl Pts',(4.6915939591275,-1.21834403169194,7.42387573995099));
#148146=CARTESIAN_POINT('Ctrl Pts',(4.70503534858688,-1.32768940173079,
7.28502666374798));
#148147=CARTESIAN_POINT('',(4.185593123,-1.32768940200002,7.595378945));
#148148=CARTESIAN_POINT('Ctrl Pts',(4.18559312299156,-1.32768940217896,
7.59537894538274));
#148149=CARTESIAN_POINT('Ctrl Pts',(4.31423268431486,-1.21834383483831,
7.64933884133742));
#148150=CARTESIAN_POINT('Ctrl Pts',(4.44150776048922,-1.10901465475701,
7.70254926521416));
#148151=CARTESIAN_POINT('Ctrl Pts',(4.56702079035568,-1.00000000044527,
7.75514803807409));
#148152=CARTESIAN_POINT('',(4.033069504,-1.32768940200002,7.677455405));
#148153=CARTESIAN_POINT('Ctrl Pts',(4.18559312312533,-1.32768940225632,
7.5953789452207));
#148154=CARTESIAN_POINT('Ctrl Pts',(4.18024433645438,-1.33223595154869,
7.5931353122223));
#148155=CARTESIAN_POINT('Ctrl Pts',(4.17442051933056,-1.33650155468029,
7.59147172983892));
#148156=CARTESIAN_POINT('Ctrl Pts',(4.15723010228811,-1.34730670089189,
7.58858455999571));
#148157=CARTESIAN_POINT('Ctrl Pts',(4.1452605134269,-1.35293307611646,7.58872330047544));
#148158=CARTESIAN_POINT('Ctrl Pts',(4.12610305860312,-1.35917045584226,
7.59205191773052));
#148159=CARTESIAN_POINT('Ctrl Pts',(4.11919887880873,-1.36087898829106,
7.59385694926454));
#148160=CARTESIAN_POINT('Ctrl Pts',(4.10556621349489,-1.36317274216386,
7.59862895110864));
#148161=CARTESIAN_POINT('Ctrl Pts',(4.09888261079392,-1.363751735737,7.6015787070655));
#148162=CARTESIAN_POINT('Ctrl Pts',(4.09244741474498,-1.36375173573942,
7.60504163372407));
#148163=CARTESIAN_POINT('Ctrl Pts',(4.0811285336459,-1.36375173574369,7.61113258337114));
#148164=CARTESIAN_POINT('Ctrl Pts',(4.07076153788779,-1.36196031878918,
7.61871191064466));
#148165=CARTESIAN_POINT('Ctrl Pts',(4.0529901399933,-1.35499086509918,7.63607209660278));
#148166=CARTESIAN_POINT('Ctrl Pts',(4.04578838240849,-1.34985996702232,
7.64569181665736));
#148167=CARTESIAN_POINT('Ctrl Pts',(4.03698160687458,-1.33873894472513,
7.66291502582498));
#148168=CARTESIAN_POINT('Ctrl Pts',(4.03442928704495,-1.33344492717922,
7.67023975875926));
#148169=CARTESIAN_POINT('Ctrl Pts',(4.03306950367077,-1.32768940206933,
7.67745540499325));
#148170=CARTESIAN_POINT('Ctrl Pts',(3.95628116425374,-0.999999999912974,
8.08380104597694));
#148171=CARTESIAN_POINT('Ctrl Pts',(3.98152840407528,-1.10901473807425,
7.95007462013823));
#148172=CARTESIAN_POINT('Ctrl Pts',(4.00723589014992,-1.21834403187787,
7.81454063889855));
#148173=CARTESIAN_POINT('Ctrl Pts',(4.03306950377905,-1.32768940202923,
7.67745540498167));
#148174=CARTESIAN_POINT('',(3.48789863553934,-1.3276894017749,7.93999585849295));
#148175=CARTESIAN_POINT('Ctrl Pts',(3.48789863503969,-1.32768940145685,
7.93999585890388));
#148176=CARTESIAN_POINT('Ctrl Pts',(3.61118340371515,-1.21834383408035,
8.00526968952849));
#148177=CARTESIAN_POINT('Ctrl Pts',(3.73317636241191,-1.10901465396194,
8.06967475372053));
#148178=CARTESIAN_POINT('Ctrl Pts',(3.8534691962495,-0.999999999613144,
8.13331268060684));
#148179=CARTESIAN_POINT('',(3.328631754,-1.32768940200002,8.00806979));
#148180=CARTESIAN_POINT('Ctrl Pts',(3.48789863549781,-1.32768940169677,
7.93999585844058));
#148181=CARTESIAN_POINT('Ctrl Pts',(3.48277249902714,-1.3322359511742,7.93728179597329));
#148182=CARTESIAN_POINT('Ctrl Pts',(3.47712124905877,-1.33650155447281,
7.93510286764403));
#148183=CARTESIAN_POINT('Ctrl Pts',(3.46025883926026,-1.34730670081657,
7.93068638354843));
#148184=CARTESIAN_POINT('Ctrl Pts',(3.44832499984238,-1.35293307603251,
7.92975161983458));
#148185=CARTESIAN_POINT('Ctrl Pts',(3.42894629234951,-1.35917045574422,
7.93134957605619));
#148186=CARTESIAN_POINT('Ctrl Pts',(3.42190810497448,-1.36087898818788,
7.93252845516265));
#148187=CARTESIAN_POINT('Ctrl Pts',(3.40790256181813,-1.36317274205037,
7.93605922364059));
#148188=CARTESIAN_POINT('Ctrl Pts',(3.400981451253,-1.36375173561834,7.9383979912236));
#148189=CARTESIAN_POINT('Ctrl Pts',(3.39426174706129,-1.36375173561571,
7.94127013063417));
#148190=CARTESIAN_POINT('Ctrl Pts',(3.38244244393533,-1.3637517356111,7.94632194323559));
#148191=CARTESIAN_POINT('Ctrl Pts',(3.37143777699997,-1.36196031864773,
7.95294146803599));
#148192=CARTESIAN_POINT('Ctrl Pts',(3.35218176646765,-1.35499086494101,
7.96863875117293));
#148193=CARTESIAN_POINT('Ctrl Pts',(3.34414669599052,-1.34985996685599,
7.97757418449405));
#148194=CARTESIAN_POINT('Ctrl Pts',(3.33383149747034,-1.33873894463069,
7.99393862469351));
#148195=CARTESIAN_POINT('Ctrl Pts',(3.33063286857535,-1.33344492718698,
8.00100508209111));
#148196=CARTESIAN_POINT('Ctrl Pts',(3.32863175374708,-1.32768940219364,
8.0080697900861));
#148197=CARTESIAN_POINT('Ctrl Pts',(3.21572799953932,-1.00000000015765,
8.4058963490006));
#148198=CARTESIAN_POINT('Ctrl Pts',(3.25286074564109,-1.10901473828874,
8.27497141166348));
#148199=CARTESIAN_POINT('Ctrl Pts',(3.29061391319593,-1.21834403206225,
8.14228745177371));
#148200=CARTESIAN_POINT('Ctrl Pts',(3.32863175377034,-1.32768940218508,
8.00806979008571));
#148201=CARTESIAN_POINT('',(2.76212164,-1.32768940200002,8.220684592));
#148202=CARTESIAN_POINT('Ctrl Pts',(2.76212164018736,-1.3276894021635,8.22068459194698));
#148203=CARTESIAN_POINT('Ctrl Pts',(2.87905899951266,-1.21834383472095,
8.29674681085366));
#148204=CARTESIAN_POINT('Ctrl Pts',(2.99478762493089,-1.10901465453746,
8.37182796377343));
#148205=CARTESIAN_POINT('Ctrl Pts',(3.10889173535243,-1.00000000012429,
8.44599266964046));
#148206=CARTESIAN_POINT('',(2.59739382,-1.32768940200002,8.274207905));
#148207=CARTESIAN_POINT('Ctrl Pts',(2.76212164024878,-1.32768940219308,
8.22068459189514));
#148208=CARTESIAN_POINT('Ctrl Pts',(2.7572594268428,-1.33223595159149,8.21752195217762));
#148209=CARTESIAN_POINT('Ctrl Pts',(2.75182624485655,-1.33650155481904,
8.21484522147967));
#148210=CARTESIAN_POINT('Ctrl Pts',(2.73542760884484,-1.34730670110944,
8.20893498211433));
#148211=CARTESIAN_POINT('Ctrl Pts',(2.72362560313124,-1.35293307633198,
8.20693424036016));
#148212=CARTESIAN_POINT('Ctrl Pts',(2.7041816689267,-1.3591704560546,8.20678866972344));
#148213=CARTESIAN_POINT('Ctrl Pts',(2.69706614131622,-1.36087898850225,
8.20733190475376));
#148214=CARTESIAN_POINT('Ctrl Pts',(2.68280048471137,-1.36317274237276,
8.20959301218039));
#148215=CARTESIAN_POINT('Ctrl Pts',(2.67569759099157,-1.36375173594474,
8.21130196100192));
#148216=CARTESIAN_POINT('Ctrl Pts',(2.66874748175985,-1.36375173594604,
8.21356018838122));
#148217=CARTESIAN_POINT('Ctrl Pts',(2.65652291868142,-1.36375173594831,
8.21753218970139));
#148218=CARTESIAN_POINT('Ctrl Pts',(2.64496918366811,-1.36196031899179,
8.22313861549781));
#148219=CARTESIAN_POINT('Ctrl Pts',(2.62438359855294,-1.35499086529792,
8.23704661050358));
#148220=CARTESIAN_POINT('Ctrl Pts',(2.61557990883475,-1.34985996721918,
8.24522581422891));
#148221=CARTESIAN_POINT('Ctrl Pts',(2.60383933905131,-1.33873894490892,
8.26059972886249));
#148222=CARTESIAN_POINT('Ctrl Pts',(2.60002015447877,-1.33344492734899,
8.26735101603766));
#148223=CARTESIAN_POINT('Ctrl Pts',(2.59739381999828,-1.32768940222356,
8.27420790518699));
#148224=CARTESIAN_POINT('Ctrl Pts',(2.44928368525819,-0.999999999982718,
8.66031231708415));
#148225=CARTESIAN_POINT('Ctrl Pts',(2.49800296686794,-1.10901473814178,
8.53324299868092));
#148226=CARTESIAN_POINT('Ctrl Pts',(2.54749784986341,-1.21834403194323,
8.40447735317845));
#148227=CARTESIAN_POINT('Ctrl Pts',(2.59739382035255,-1.32768940209275,
8.27420790521288));
#148228=CARTESIAN_POINT('',(2.0141056646537,-1.3276894019719,8.43518520740466));
#148229=CARTESIAN_POINT('Ctrl Pts',(2.01410566413619,-1.32768940192452,
8.43518520800257));
#148230=CARTESIAN_POINT('Ctrl Pts',(2.12375410335396,-1.21834383447808,
8.52142340685227));
#148231=CARTESIAN_POINT('Ctrl Pts',(2.23228661674759,-1.10901465429013,
8.606576139125));
#148232=CARTESIAN_POINT('Ctrl Pts',(2.33928330464296,-0.999999999872262,
8.69067049328867));
#148233=CARTESIAN_POINT('',(1.845243197,-1.32768940200002,8.473726964));
#148234=CARTESIAN_POINT('Ctrl Pts',(2.01410566493824,-1.32768940228522,
8.43518520744022));
#148235=CARTESIAN_POINT('Ctrl Pts',(2.00954652218687,-1.33223595171976,
8.43159945409989));
#148236=CARTESIAN_POINT('Ctrl Pts',(2.00437515284886,-1.33650155497982,
8.42844647242926));
#148237=CARTESIAN_POINT('Ctrl Pts',(1.98857232265249,-1.34730670129488,
8.42109006353587));
#148238=CARTESIAN_POINT('Ctrl Pts',(1.97699717345129,-1.35293307651467,
8.41803945254678));
#148239=CARTESIAN_POINT('Ctrl Pts',(1.95764456366011,-1.3591704562329,8.41615152711446));
#148240=CARTESIAN_POINT('Ctrl Pts',(1.95050898585904,-1.36087898867897,
8.41605474426427));
#148241=CARTESIAN_POINT('Ctrl Pts',(1.93609807448668,-1.3631727425463,8.41702798554097));
#148242=CARTESIAN_POINT('Ctrl Pts',(1.92887058593775,-1.36375173611669,
8.41809335615413));
#148243=CARTESIAN_POINT('Ctrl Pts',(1.92174602986137,-1.36375173611642,
8.41971948958691));
#148244=CARTESIAN_POINT('Ctrl Pts',(1.90921463182692,-1.36375173611594,
8.422579699414));
#148245=CARTESIAN_POINT('Ctrl Pts',(1.89720485262119,-1.36196031915664,
8.42712788656892));
#148246=CARTESIAN_POINT('Ctrl Pts',(1.87545543596194,-1.3549908654575,8.43913461445686));
#148247=CARTESIAN_POINT('Ctrl Pts',(1.8659540091429,-1.34985996737619,8.4464917344525));
#148248=CARTESIAN_POINT('Ctrl Pts',(1.85288259622497,-1.3387389449445,8.46075134181751));
#148249=CARTESIAN_POINT('Ctrl Pts',(1.8484736057682,-1.33344492723396,8.4671331014014));
#148250=CARTESIAN_POINT('Ctrl Pts',(1.84524319731389,-1.32768940193907,
8.47372696410058));
#148251=CARTESIAN_POINT('Ctrl Pts',(1.66311917770952,-0.999999999928505,
8.84500054279377));
#148252=CARTESIAN_POINT('Ctrl Pts',(1.7230327356253,-1.10901473804792,8.72280993090161));
#148253=CARTESIAN_POINT('Ctrl Pts',(1.78387083017168,-1.21834403180964,
8.59899934519942));
#148254=CARTESIAN_POINT('Ctrl Pts',(1.84524319736451,-1.32768940192018,
8.47372696410889));
#148255=CARTESIAN_POINT('',(1.249873295,-1.32768940200002,8.581770672));
#148256=CARTESIAN_POINT('Ctrl Pts',(1.24987329474725,-1.32768940183712,
8.58177067208187));
#148257=CARTESIAN_POINT('Ctrl Pts',(1.35134998891948,-1.21834383452832,
8.67749051148483));
#148258=CARTESIAN_POINT('Ctrl Pts',(1.45181255013311,-1.10901465447807,
8.7720292232633));
#148259=CARTESIAN_POINT('Ctrl Pts',(1.55084034091679,-1.00000000019697,
8.86537614731829));
#148260=CARTESIAN_POINT('',(1.078235761,-1.32768940200002,8.605020555));
#148261=CARTESIAN_POINT('Ctrl Pts',(1.24987329478272,-1.32768940185216,
8.5817706720615));
#148262=CARTESIAN_POINT('Ctrl Pts',(1.24565393021003,-1.33223595135743,
8.57779067543879));
#148263=CARTESIAN_POINT('Ctrl Pts',(1.24078601032253,-1.33650155468153,
8.5741868287156));
#148264=CARTESIAN_POINT('Ctrl Pts',(1.22570622100733,-1.34730670104963,
8.56544347974055));
#148265=CARTESIAN_POINT('Ctrl Pts',(1.21445112461428,-1.3529330762685,8.56136756123979));
#148266=CARTESIAN_POINT('Ctrl Pts',(1.19534565507141,-1.35917045598511,
8.55775248147335));
#148267=CARTESIAN_POINT('Ctrl Pts',(1.18824747855661,-1.36087898843056,
8.55701645997985));
#148268=CARTESIAN_POINT('Ctrl Pts',(1.17380734060152,-1.36317274229666,
8.55669399913736));
#148269=CARTESIAN_POINT('Ctrl Pts',(1.1665134487113,-1.36375173586643,8.55710721380306));
#148270=CARTESIAN_POINT('Ctrl Pts',(1.15927180852621,-1.36375173586557,
8.55808816061781));
#148271=CARTESIAN_POINT('Ctrl Pts',(1.14653447098409,-1.36375173586405,
8.55981355022169));
#148272=CARTESIAN_POINT('Ctrl Pts',(1.1341653432657,-1.36196031890375,8.56326687940421));
#148273=CARTESIAN_POINT('Ctrl Pts',(1.11142720857434,-1.35499086520276,
8.5732756690572));
#148274=CARTESIAN_POINT('Ctrl Pts',(1.10130454455473,-1.34985996712054,
8.57975147011711));
#148275=CARTESIAN_POINT('Ctrl Pts',(1.08700753210465,-1.33873894480506,
8.59278195993714));
#148276=CARTESIAN_POINT('Ctrl Pts',(1.0820442345278,-1.33344492724318,8.59874280941312));
#148277=CARTESIAN_POINT('Ctrl Pts',(1.07823576149092,-1.32768940211611,
8.60502055540426));
#148278=CARTESIAN_POINT('Ctrl Pts',(0.863564212198985,-0.999999999788603,
8.9584740249227));
#148279=CARTESIAN_POINT('Ctrl Pts',(0.934189657823288,-1.10901473803966,
8.84214592630361));
#148280=CARTESIAN_POINT('Ctrl Pts',(1.00588113150084,-1.2183440319341,8.72428725023411));
#148281=CARTESIAN_POINT('Ctrl Pts',(1.07823576132974,-1.32768940217741,
8.60502055536268));
#148282=CARTESIAN_POINT('',(0.475577681,-1.32768940200002,8.659260764));
#148283=CARTESIAN_POINT('Ctrl Pts',(0.475577680456158,-1.32768940202431,
8.65926076450709));
#148284=CARTESIAN_POINT('Ctrl Pts',(0.568065599076004,-1.21834383457737,
8.76369156484591));
#148285=CARTESIAN_POINT('Ctrl Pts',(0.659649342801168,-1.10901465438963,
8.86685508625391));
#148286=CARTESIAN_POINT('Ctrl Pts',(0.749910923085495,-0.999999999972138,
8.96870300589438));
#148287=CARTESIAN_POINT('',(0.302547006,-1.32768940200002,8.667031581));
#148288=CARTESIAN_POINT('Ctrl Pts',(0.475577681121856,-1.32768940229424,
8.6592607642002));
#148289=CARTESIAN_POINT('Ctrl Pts',(0.471732066689365,-1.33223595165813,
8.65491856908753));
#148290=CARTESIAN_POINT('Ctrl Pts',(0.467206790057779,-1.33650155485448,
8.65089287353958));
#148291=CARTESIAN_POINT('Ctrl Pts',(0.452971455449953,-1.34730670111979,
8.64083298092142));
#148292=CARTESIAN_POINT('Ctrl Pts',(0.442127031285838,-1.35293307634352,
8.63576457180456));
#148293=CARTESIAN_POINT('Ctrl Pts',(0.423422528000211,-1.35917045606807,
8.63045144419511));
#148294=CARTESIAN_POINT('Ctrl Pts',(0.416418903115651,-1.36087898851643,
8.62908211006862));
#148295=CARTESIAN_POINT('Ctrl Pts',(0.402065802077876,-1.36317274238836,
8.62746654336826));
#148296=CARTESIAN_POINT('Ctrl Pts',(0.394764232974746,-1.36375173596106,
8.62722427512315));
#148297=CARTESIAN_POINT('Ctrl Pts',(0.387463814108889,-1.36375173596304,
8.62755213731119));
#148298=CARTESIAN_POINT('Ctrl Pts',(0.374623090611254,-1.36375173596654,
8.62812881486619));
#148299=CARTESIAN_POINT('Ctrl Pts',(0.361994203322082,-1.36196031901124,
8.63045948189726));
#148300=CARTESIAN_POINT('Ctrl Pts',(0.338450424685213,-1.35499086531967,
8.63838974842051));
#148301=CARTESIAN_POINT('Ctrl Pts',(0.327788025201015,-1.34985996724206,
8.64393209119936));
#148302=CARTESIAN_POINT('Ctrl Pts',(0.312380524047815,-1.33873894481487,
8.65562854990332));
#148303=CARTESIAN_POINT('Ctrl Pts',(0.306902880703474,-1.33344492710504,
8.66112049633992));
#148304=CARTESIAN_POINT('Ctrl Pts',(0.302547006590515,-1.32768940181038,
8.66703158125051));
#148305=CARTESIAN_POINT('Ctrl Pts',(0.0570563368422528,-1.00000000016179,
8.99981914104469));
#148306=CARTESIAN_POINT('Ctrl Pts',(0.13782503550806,-1.10901473824052,
8.89029016145374));
#148307=CARTESIAN_POINT('Ctrl Pts',(0.219792670612582,-1.21834403196144,
8.77933232408725));
#148308=CARTESIAN_POINT('Ctrl Pts',(0.302547006027248,-1.32768940203058,
8.66703158104984));
#148309=CARTESIAN_POINT('',(-0.302547007,-1.32768940200002,8.667031581));
#148310=CARTESIAN_POINT('Ctrl Pts',(-0.302547007479097,-1.32768940183626,
8.6670315811936));
#148311=CARTESIAN_POINT('Ctrl Pts',(-0.219792522734839,-1.21834383445799,
8.77933252688754));
#148312=CARTESIAN_POINT('Ctrl Pts',(-0.137824974935764,-1.10901465433772,
8.89029024572902));
#148313=CARTESIAN_POINT('Ctrl Pts',(-0.057056338302778,-0.999999999986948,
8.99981914121027));
#148314=CARTESIAN_POINT('',(-0.475577681,-1.32768940200002,8.659260764));
#148315=CARTESIAN_POINT('Ctrl Pts',(-0.302547006808484,-1.32768940209839,
8.66703158095471));
#148316=CARTESIAN_POINT('Ctrl Pts',(-0.305987908599572,-1.33223595155284,
8.6623621479303));
#148317=CARTESIAN_POINT('Ctrl Pts',(-0.310134107298285,-1.33650155483069,
8.65794701589456));
#148318=CARTESIAN_POINT('Ctrl Pts',(-0.323410372907654,-1.34730670115792,
8.64665157582216));
#148319=CARTESIAN_POINT('Ctrl Pts',(-0.333756811921427,-1.35293307637481,
8.64063148394742));
#148320=CARTESIAN_POINT('Ctrl Pts',(-0.35190975129218,-1.35917045608826,
8.63366308668714));
#148321=CARTESIAN_POINT('Ctrl Pts',(-0.358762435478124,-1.36087898853258,
8.63167146500544));
#148322=CARTESIAN_POINT('Ctrl Pts',(-0.372912936869241,-1.3631727423964,
8.62877580004926));
#148323=CARTESIAN_POINT('Ctrl Pts',(-0.380163395243697,-1.36375173596503,
8.6278799994992));
#148324=CARTESIAN_POINT('Ctrl Pts',(-0.387463814108889,-1.36375173596304,
8.62755213731119));
#148325=CARTESIAN_POINT('Ctrl Pts',(-0.400304537606773,-1.36375173595955,
8.62697545975618));
#148326=CARTESIAN_POINT('Ctrl Pts',(-0.413091504089375,-1.36196031899726,
8.62816469948271));
#148327=CARTESIAN_POINT('Ctrl Pts',(-0.437251366001838,-1.35499086529249,
8.63395259304714));
#148328=CARTESIAN_POINT('Ctrl Pts',(-0.448367653573954,-1.34985996720843,
8.63851685386684));
#148329=CARTESIAN_POINT('Ctrl Pts',(-0.464761590912138,-1.33873894491584,
8.64878510818524));
#148330=CARTESIAN_POINT('Ctrl Pts',(-0.470709476999125,-1.33344492738548,
8.65376393332434));
#148331=CARTESIAN_POINT('Ctrl Pts',(-0.475577681121838,-1.32768940229425,
8.65926076420018));
#148332=CARTESIAN_POINT('Ctrl Pts',(-0.749910923381223,-1.00000000008659,
8.9687030057548));
#148333=CARTESIAN_POINT('Ctrl Pts',(-0.659649273775829,-1.10901473822727,
8.86685500789799));
#148334=CARTESIAN_POINT('Ctrl Pts',(-0.568065432473346,-1.21834403201054,
8.76369137626223));
#148335=CARTESIAN_POINT('Ctrl Pts',(-0.475577680748764,-1.32768940214297,
8.65926076437218));
#148336=CARTESIAN_POINT('',(-1.07823576159075,-1.32768940191118,8.60502055527694));
#148337=CARTESIAN_POINT('Ctrl Pts',(-1.07823576225904,-1.32768940182398,
8.60502055560243));
#148338=CARTESIAN_POINT('Ctrl Pts',(-1.00588100192119,-1.21834383435451,
8.72428746560446));
#148339=CARTESIAN_POINT('Ctrl Pts',(-0.934189604625298,-1.10901465414413,
8.8421460157062));
#148340=CARTESIAN_POINT('Ctrl Pts',(-0.86356421329429,-0.999999999704432,
8.95847402490167));
#148341=CARTESIAN_POINT('',(-1.249873295,-1.32768940200002,8.581770672));
#148342=CARTESIAN_POINT('Ctrl Pts',(-1.07823576149091,-1.32768940211609,
8.60502055540429));
#148343=CARTESIAN_POINT('Ctrl Pts',(-1.08124424645351,-1.33223595151502,
8.60006148014486));
#148344=CARTESIAN_POINT('Ctrl Pts',(-1.08497798435395,-1.33650155474298,
8.59529245980227));
#148345=CARTESIAN_POINT('Ctrl Pts',(-1.09718828812372,-1.34730670103304,
8.58285241662335));
#148346=CARTESIAN_POINT('Ctrl Pts',(-1.10695343853787,-1.35293307625488,
8.5759291122228));
#148347=CARTESIAN_POINT('Ctrl Pts',(-1.12440865719427,-1.35917045597631,
8.5673615507366));
#148348=CARTESIAN_POINT('Ctrl Pts',(-1.13105522689638,-1.36087898842353,
8.56476367686195));
#148349=CARTESIAN_POINT('Ctrl Pts',(-1.14488919712259,-1.36317274229316,
8.56061122783271));
#148350=CARTESIAN_POINT('Ctrl Pts',(-1.15203016834083,-1.3637517358647,
8.5590691074326));
#148351=CARTESIAN_POINT('Ctrl Pts',(-1.1592718085262,-1.36375173586557,
8.55808816061781));
#148352=CARTESIAN_POINT('Ctrl Pts',(-1.17200914606821,-1.36375173586709,
8.55636277101395));
#148353=CARTESIAN_POINT('Ctrl Pts',(-1.18485123861067,-1.36196031890983,
8.55640100836933));
#148354=CARTESIAN_POINT('Ctrl Pts',(-1.20943266280315,-1.35499086521458,
8.55999992824462));
#148355=CARTESIAN_POINT('Ctrl Pts',(-1.22091333665684,-1.34985996713517,
8.56354935835334));
#148356=CARTESIAN_POINT('Ctrl Pts',(-1.23816171620794,-1.3387389447467,
8.57230673456117));
#148357=CARTESIAN_POINT('Ctrl Pts',(-1.24453195642251,-1.33344492708842,
8.57673235212775));
#148358=CARTESIAN_POINT('Ctrl Pts',(-1.2498732947827,-1.32768940185218,
8.58177067206149));
#148359=CARTESIAN_POINT('Ctrl Pts',(-1.5508403411853,-1.00000000030594,
8.86537614716069));
#148360=CARTESIAN_POINT('Ctrl Pts',(-1.4518124743483,-1.1090147383101,8.77202915141815));
#148361=CARTESIAN_POINT('Ctrl Pts',(-1.35134980606935,-1.21834403195577,
8.6774903386024));
#148362=CARTESIAN_POINT('Ctrl Pts',(-1.24987329501286,-1.32768940194995,
8.58177067192916));
#148363=CARTESIAN_POINT('',(-1.845243197,-1.32768940200002,8.473726964));
#148364=CARTESIAN_POINT('Ctrl Pts',(-1.84524319784118,-1.3276894017423,
8.47372696418715));
#148365=CARTESIAN_POINT('Ctrl Pts',(-1.78387071989928,-1.21834383431895,
8.59899957133592));
#148366=CARTESIAN_POINT('Ctrl Pts',(-1.72303269008614,-1.1090146541547,
8.72281002482354));
#148367=CARTESIAN_POINT('Ctrl Pts',(-1.66311917818115,-0.999999999760975,
8.84500054287555));
#148368=CARTESIAN_POINT('',(-2.014105665,-1.32768940200002,8.435185207));
#148369=CARTESIAN_POINT('Ctrl Pts',(-1.84524319731387,-1.32768940193905,
8.4737269641006));
#148370=CARTESIAN_POINT('Ctrl Pts',(-1.8477950429561,-1.33223595150089,
8.46851817393294));
#148371=CARTESIAN_POINT('Ctrl Pts',(-1.85108625832112,-1.33650155487643,
8.46343366240974));
#148372=CARTESIAN_POINT('Ctrl Pts',(-1.86213229025263,-1.34730670128967,
8.44994917584068));
#148373=CARTESIAN_POINT('Ctrl Pts',(-1.87123752882059,-1.35293307651039,
8.44217840129406));
#148374=CARTESIAN_POINT('Ctrl Pts',(-1.88785448760807,-1.35917045623014,
8.43208065655475));
#148375=CARTESIAN_POINT('Ctrl Pts',(-1.89424142855602,-1.36087898867676,
8.42889744704194));
#148376=CARTESIAN_POINT('Ctrl Pts',(-1.9076474846242,-1.3631727425452,8.42352164702133));
#148377=CARTESIAN_POINT('Ctrl Pts',(-1.9146214737849,-1.36375173611614,
8.42134562301972));
#148378=CARTESIAN_POINT('Ctrl Pts',(-1.92174602986137,-1.36375173611642,
8.41971948958691));
#148379=CARTESIAN_POINT('Ctrl Pts',(-1.93427742789579,-1.36375173611689,
8.41685927975983));
#148380=CARTESIAN_POINT('Ctrl Pts',(-1.94707124951948,-1.36196031915856,
8.41574620688258));
#148381=CARTESIAN_POINT('Ctrl Pts',(-1.9718763208155,-1.35499086546122,
8.41712717668837));
#148382=CARTESIAN_POINT('Ctrl Pts',(-1.98362894531338,-1.34985996738079,
8.41963319816523));
#148383=CARTESIAN_POINT('Ctrl Pts',(-2.00159289302696,-1.33873894504213,
8.42680918689579));
#148384=CARTESIAN_POINT('Ctrl Pts',(-2.00833419776163,-1.33344492744846,
8.43064596424567));
#148385=CARTESIAN_POINT('Ctrl Pts',(-2.01410566493822,-1.32768940228524,
8.43518520744021));
#148386=CARTESIAN_POINT('Ctrl Pts',(-2.33928330581808,-0.999999999832172,
8.69067049301388));
#148387=CARTESIAN_POINT('Ctrl Pts',(-2.23228653562601,-1.10901473810327,
8.60657607417562));
#148388=CARTESIAN_POINT('Ctrl Pts',(-2.12375390641409,-1.21834403201796,
8.5214232507742));
#148389=CARTESIAN_POINT('Ctrl Pts',(-2.01410566492906,-1.32768940228112,
8.43518520744663));
#148390=CARTESIAN_POINT('',(-2.59739382,-1.32768940200002,8.274207905));
#148391=CARTESIAN_POINT('Ctrl Pts',(-2.59739382005672,-1.32768940220198,
8.27420790519126));
#148392=CARTESIAN_POINT('Ctrl Pts',(-2.54749775952752,-1.21834383473538,
8.40447758822955));
#148393=CARTESIAN_POINT('Ctrl Pts',(-2.49800292915253,-1.10901465452695,
8.53324309624464));
#148394=CARTESIAN_POINT('Ctrl Pts',(-2.44928368495601,-1.00000000008884,
8.66031231705933));
#148395=CARTESIAN_POINT('',(-2.762121641,-1.32768940200002,8.220684592));
#148396=CARTESIAN_POINT('Ctrl Pts',(-2.59739381999827,-1.32768940222354,
8.27420790518701));
#148397=CARTESIAN_POINT('Ctrl Pts',(-2.59946848029277,-1.33223595162173,
8.26879133857389));
#148398=CARTESIAN_POINT('Ctrl Pts',(-2.60229067402789,-1.33650155484869,
8.26343227370457));
#148399=CARTESIAN_POINT('Ctrl Pts',(-2.61208349771735,-1.34730670113423,
8.24901191321329));
#148400=CARTESIAN_POINT('Ctrl Pts',(-2.62045551441409,-1.35293307635233,
8.24045623422956));
#148401=CARTESIAN_POINT('Ctrl Pts',(-2.63610042335359,-1.35917045606773,
8.22890960734339));
#148402=CARTESIAN_POINT('Ctrl Pts',(-2.64217631165495,-1.36087898851275,
8.22516669152494));
#148403=CARTESIAN_POINT('Ctrl Pts',(-2.65504651588519,-1.36317274237799,
8.21861082329637));
#148404=CARTESIAN_POINT('Ctrl Pts',(-2.66179737252854,-1.36375173594733,
8.21581841576039));
#148405=CARTESIAN_POINT('Ctrl Pts',(-2.66874748175985,-1.36375173594604,
8.21356018838122));
#148406=CARTESIAN_POINT('Ctrl Pts',(-2.68097204483843,-1.36375173594376,
8.20958818706101));
#148407=CARTESIAN_POINT('Ctrl Pts',(-2.6936145872141,-1.3619603189827,8.20733276576193));
#148408=CARTESIAN_POINT('Ctrl Pts',(-2.71844358976387,-1.35499086528025,
8.20648466674614));
#148409=CARTESIAN_POINT('Ctrl Pts',(-2.73037353968324,-1.34985996719732,
8.20792710258216));
#148410=CARTESIAN_POINT('Ctrl Pts',(-2.74890842063211,-1.33873894477131,
8.2134639270796));
#148411=CARTESIAN_POINT('Ctrl Pts',(-2.7559665130382,-1.33344492707015,
8.21668097286978));
#148412=CARTESIAN_POINT('Ctrl Pts',(-2.76212164068402,-1.32768940178609,
8.22068459217825));
#148413=CARTESIAN_POINT('Ctrl Pts',(-3.10889173601996,-1.00000000022005,
8.44599266929272));
#148414=CARTESIAN_POINT('Ctrl Pts',(-2.99478753806051,-1.10901473827084,
8.37182790653102));
#148415=CARTESIAN_POINT('Ctrl Pts',(-2.87905878935271,-1.21834403196374,
8.29674667337776));
#148416=CARTESIAN_POINT('Ctrl Pts',(-2.76212164114016,-1.32768940200595,
8.22068459179305));
#148417=CARTESIAN_POINT('',(-3.328631754,-1.32768940200002,8.00806979));
#148418=CARTESIAN_POINT('Ctrl Pts',(-3.32863175341881,-1.32768940231455,
8.00806979009162));
#148419=CARTESIAN_POINT('Ctrl Pts',(-3.29061384423879,-1.21834383487425,
8.14228769397692));
#148420=CARTESIAN_POINT('Ctrl Pts',(-3.25286071676859,-1.10901465469334,
8.27497151221575));
#148421=CARTESIAN_POINT('Ctrl Pts',(-3.21572799918201,-1.00000000028271,
8.40589634900339));
#148422=CARTESIAN_POINT('',(-3.487898636,-1.32768940200002,7.939995858));
#148423=CARTESIAN_POINT('Ctrl Pts',(-3.32863175374707,-1.32768940219362,
8.00806979008613));
#148424=CARTESIAN_POINT('Ctrl Pts',(-3.3302125247748,-1.33223595146223,
8.00248905800613));
#148425=CARTESIAN_POINT('Ctrl Pts',(-3.3325429742706,-1.33650155457232,
7.99689858780651));
#148426=CARTESIAN_POINT('Ctrl Pts',(-3.34100374369261,-1.3473067007662,
7.9816584576379));
#148427=CARTESIAN_POINT('Ctrl Pts',(-3.3485751319546,-1.35293307599117,
7.97238675950792));
#148428=CARTESIAN_POINT('Ctrl Pts',(-3.36312202742945,-1.35917045571755,
7.95948421711507));
#148429=CARTESIAN_POINT('Ctrl Pts',(-3.3688379436014,-1.36087898816654,
7.95521173074453));
#148430=CARTESIAN_POINT('Ctrl Pts',(-3.38106867267251,-1.36317274203975,
7.94752857829612));
#148431=CARTESIAN_POINT('Ctrl Pts',(-3.38754204286878,-1.36375173561309,
7.94414227004508));
#148432=CARTESIAN_POINT('Ctrl Pts',(-3.39426174706129,-1.36375173561571,
7.94127013063417));
#148433=CARTESIAN_POINT('Ctrl Pts',(-3.40608105018694,-1.36375173562033,
7.93621831803288));
#148434=CARTESIAN_POINT('Ctrl Pts',(-3.4184705229962,-1.3619603186662,7.93283870763021));
#148435=CARTESIAN_POINT('Ctrl Pts',(-3.44312354827155,-1.35499086497692,
7.9297683681713));
#148436=CARTESIAN_POINT('Ctrl Pts',(-3.45513477067233,-1.34985996690043,
7.93013560471274));
#148437=CARTESIAN_POINT('Ctrl Pts',(-3.47409135267749,-1.33873894453579,
7.93398868563539));
#148438=CARTESIAN_POINT('Ctrl Pts',(-3.48140940496856,-1.3334449269038,
7.93656009797619));
#148439=CARTESIAN_POINT('Ctrl Pts',(-3.48789863549779,-1.32768940169679,
7.93999585844057));
#148440=CARTESIAN_POINT('Ctrl Pts',(-3.8534691968536,-1.00000000021841,
8.13331267965086));
#148441=CARTESIAN_POINT('Ctrl Pts',(-3.73317627069964,-1.10901473822962,
8.06967470393504));
#148442=CARTESIAN_POINT('Ctrl Pts',(-3.61118318198707,-1.21834403188243,
8.00526957087236));
#148443=CARTESIAN_POINT('Ctrl Pts',(-3.48789863585382,-1.32768940188326,
7.93999585808051));
#148444=CARTESIAN_POINT('',(-4.033069504,-1.32768940200002,7.677455405));
#148445=CARTESIAN_POINT('Ctrl Pts',(-4.03306950415229,-1.327689401891,7.67745540494174));
#148446=CARTESIAN_POINT('Ctrl Pts',(-4.00723584390747,-1.2183438344254,
7.81454088623289));
#148447=CARTESIAN_POINT('Ctrl Pts',(-3.98152838506235,-1.1090146542176,
7.9500747228005));
#148448=CARTESIAN_POINT('Ctrl Pts',(-3.95628116463241,-0.999999999779801,
8.08380104593988));
#148449=CARTESIAN_POINT('',(-4.185593123,-1.32768940200002,7.595378945));
#148450=CARTESIAN_POINT('Ctrl Pts',(-4.03306950367076,-1.32768940206931,
7.67745540499327));
#148451=CARTESIAN_POINT('Ctrl Pts',(-4.03414365800827,-1.33223595145271,
7.67175543994932));
#148452=CARTESIAN_POINT('Ctrl Pts',(-4.03596359994506,-1.33650155466611,
7.66597857532337));
#148453=CARTESIAN_POINT('Ctrl Pts',(-4.04302419413378,-1.34730670093839,
7.65004137978482));
#148454=CARTESIAN_POINT('Ctrl Pts',(-4.04973399360729,-1.35293307615463,
7.64012831277831));
#148455=CARTESIAN_POINT('Ctrl Pts',(-4.06306575258347,-1.3591704558669,
7.6259737385784));
#148456=CARTESIAN_POINT('Ctrl Pts',(-4.0683756754347,-1.36087898831076,
7.62120608120941));
#148457=CARTESIAN_POINT('Ctrl Pts',(-4.0798684547153,-1.36317274217366,
7.61245750477904));
#148458=CARTESIAN_POINT('Ctrl Pts',(-4.08601221869673,-1.36375173574185,
7.60850456038226));
#148459=CARTESIAN_POINT('Ctrl Pts',(-4.09244741474498,-1.36375173573942,
7.60504163372406));
#148460=CARTESIAN_POINT('Ctrl Pts',(-4.10376629584433,-1.36375173573516,
7.59895068407684));
#148461=CARTESIAN_POINT('Ctrl Pts',(-4.11580294633933,-1.36196031877213,
7.59447409521846));
#148462=CARTESIAN_POINT('Ctrl Pts',(-4.1400815026765,-1.35499086506602,
7.58920623590949));
#148463=CARTESIAN_POINT('Ctrl Pts',(-4.15207729025624,-1.3498599669813,
7.5884953163971));
#148464=CARTESIAN_POINT('Ctrl Pts',(-4.17130294590846,-1.33873894473932,
7.59063363102621));
#148465=CARTESIAN_POINT('Ctrl Pts',(-4.17882203729309,-1.33344492727405,
7.59253870638845));
#148466=CARTESIAN_POINT('Ctrl Pts',(-4.1855931231253,-1.32768940225634,
7.59537894522069));
#148467=CARTESIAN_POINT('Ctrl Pts',(-4.5670207909907,-1.00000000006023,
7.75514803814698));
#148468=CARTESIAN_POINT('Ctrl Pts',(-4.44150766456477,-1.10901473824446,
7.7025492248208));
#148469=CARTESIAN_POINT('Ctrl Pts',(-4.314232452478,-1.21834403207158,7.64933874389548));
#148470=CARTESIAN_POINT('Ctrl Pts',(-4.18559312311081,-1.32768940224796,
7.59537894523824));
#148471=CARTESIAN_POINT('',(-4.705035349,-1.32768940200002,7.285026664));
#148472=CARTESIAN_POINT('Ctrl Pts',(-4.70503534876328,-1.32768940166456,
7.2850266637129));
#148473=CARTESIAN_POINT('Ctrl Pts',(-4.6915939350508,-1.21834383431014,
7.42387599047203));
#148474=CARTESIAN_POINT('Ctrl Pts',(-4.67813912632766,-1.10901465421366,
7.56116860636961));
#148475=CARTESIAN_POINT('Ctrl Pts',(-4.66498067897969,-0.999999999886532,
7.69661972990669));
#148476=CARTESIAN_POINT('',(-4.849587676,-1.32768940200002,7.189608507));
#148477=CARTESIAN_POINT('Ctrl Pts',(-4.70503534864306,-1.32768940170967,
7.28502666373683));
#148478=CARTESIAN_POINT('Ctrl Pts',(-4.70559423778767,-1.33223595129557,
7.27925335840597));
#148479=CARTESIAN_POINT('Ctrl Pts',(-4.70688901904333,-1.33650155469243,
7.27333661116777));
#148480=CARTESIAN_POINT('Ctrl Pts',(-4.71249259024252,-1.34730670111821,
7.25683066707283));
#148481=CARTESIAN_POINT('Ctrl Pts',(-4.71828677756059,-1.35293307633343,
7.24635604537204));
#148482=CARTESIAN_POINT('Ctrl Pts',(-4.73029606054557,-1.35917045604412,
7.23106340366536));
#148483=CARTESIAN_POINT('Ctrl Pts',(-4.7351572376969,-1.36087898848742,
7.22583896166849));
#148484=CARTESIAN_POINT('Ctrl Pts',(-4.74581953408189,-1.3631727423492,
7.21609539964255));
#148485=CARTESIAN_POINT('Ctrl Pts',(-4.75158422587188,-1.36375173591682,
7.21160764588035));
#148486=CARTESIAN_POINT('Ctrl Pts',(-4.75768310136027,-1.36375173591383,
7.20758181342034));
#148487=CARTESIAN_POINT('Ctrl Pts',(-4.76841042745518,-1.36375173590859,
7.20050076746617));
#148488=CARTESIAN_POINT('Ctrl Pts',(-4.77999734360254,-1.36196031894457,
7.19496324300642));
#148489=CARTESIAN_POINT('Ctrl Pts',(-4.80370595434182,-1.35499086523651,
7.18754027753896));
#148490=CARTESIAN_POINT('Ctrl Pts',(-4.81558972407364,-1.34985996715084,
7.18575692587118));
#148491=CARTESIAN_POINT('Ctrl Pts',(-4.83492966004746,-1.33873894484204,
7.18616325779104));
#148492=CARTESIAN_POINT('Ctrl Pts',(-4.84258925152041,-1.33344492729326,
7.18738665775673));
#148493=CARTESIAN_POINT('Ctrl Pts',(-4.84958767607709,-1.3276894021815,
7.18960850722728));
#148494=CARTESIAN_POINT('Ctrl Pts',(-5.24380141911386,-1.00000000018046,
7.31454350411914));
#148495=CARTESIAN_POINT('Ctrl Pts',(-5.11407865044419,-1.10901473830268,
7.2734073480866));
#148496=CARTESIAN_POINT('Ctrl Pts',(-4.98254606029434,-1.21834403206745,
7.23181993899048));
#148497=CARTESIAN_POINT('Ctrl Pts',(-4.84958767607749,-1.32768940218177,
7.18960850722668));
#148498=CARTESIAN_POINT('',(-5.339119013,-1.32768940200002,6.833943172));
#148499=CARTESIAN_POINT('Ctrl Pts',(-5.33911901336203,-1.3276894020463,
6.83394317203873));
#148500=CARTESIAN_POINT('Ctrl Pts',(-5.33817806862293,-1.21834383468527,
6.97343841116911));
#148501=CARTESIAN_POINT('Ctrl Pts',(-5.33708424031203,-1.10901465458379,
7.11138440702185));
#148502=CARTESIAN_POINT('Ctrl Pts',(-5.33612051020986,-1.00000000025242,
7.24746975819661));
#148503=CARTESIAN_POINT('',(-5.474536199,-1.32768940200002,6.725951571));
#148504=CARTESIAN_POINT('Ctrl Pts',(-5.33911901311747,-1.32768940214016,
6.83394317211069));
#148505=CARTESIAN_POINT('Ctrl Pts',(-5.33915813729677,-1.33223595149941,
6.82814301021648));
#148506=CARTESIAN_POINT('Ctrl Pts',(-5.33991733300375,-1.33650155469162,
6.82213401903261));
#148507=CARTESIAN_POINT('Ctrl Pts',(-5.34401876437182,-1.34730670095398,
6.80519222304139));
#148508=CARTESIAN_POINT('Ctrl Pts',(-5.34885068813799,-1.35293307617826,
6.79424038213928));
#148509=CARTESIAN_POINT('Ctrl Pts',(-5.35944080343791,-1.35917045590364,
6.77793280028018));
#148510=CARTESIAN_POINT('Ctrl Pts',(-5.36381409554641,-1.36087898835228,
6.77229363778862));
#148511=CARTESIAN_POINT('Ctrl Pts',(-5.37356006248996,-1.36317274222478,
6.76163353959512));
#148512=CARTESIAN_POINT('Ctrl Pts',(-5.37889926817801,-1.36375173579776,
6.75664710921955));
#148513=CARTESIAN_POINT('Ctrl Pts',(-5.38461271854601,-1.36375173580003,
6.75209078459071));
#148514=CARTESIAN_POINT('Ctrl Pts',(-5.39466211951056,-1.36375173580403,
6.74407665474437));
#148515=CARTESIAN_POINT('Ctrl Pts',(-5.40570601027229,-1.36196031884925,
6.73752277956918));
#148516=CARTESIAN_POINT('Ctrl Pts',(-5.42865378761812,-1.35499086515872,
6.72800447328541));
#148517=CARTESIAN_POINT('Ctrl Pts',(-5.4403298583754,-1.34985996708161,
6.72516304795477));
#148518=CARTESIAN_POINT('Ctrl Pts',(-5.4596283610753,-1.33873894460838,
6.72383412557344));
#148519=CARTESIAN_POINT('Ctrl Pts',(-5.46736678229439,-1.33344492683944,
6.72436600006063));
#148520=CARTESIAN_POINT('Ctrl Pts',(-5.47453619853397,-1.32768940147805,
6.72595157121251));
#148521=CARTESIAN_POINT('Ctrl Pts',(-5.87836203986568,-0.999999999941251,
6.81504656838998));
#148522=CARTESIAN_POINT('Ctrl Pts',(-5.74547408034092,-1.10901473795678,
6.78570427387046));
#148523=CARTESIAN_POINT('Ctrl Pts',(-5.61074313513168,-1.21834403161385,
6.75607477404509));
#148524=CARTESIAN_POINT('Ctrl Pts',(-5.47453619872126,-1.32768940161921,
6.72595157087805));
#148525=CARTESIAN_POINT('',(-5.93021523354241,-1.32768940189191,6.32783678686983));
#148526=CARTESIAN_POINT('Ctrl Pts',(-5.93021523412515,-1.32768940176286,
6.32783678671984));
#148527=CARTESIAN_POINT('Ctrl Pts',(-5.94178233414468,-1.21834383430549,
6.46685480485237));
#148528=CARTESIAN_POINT('Ctrl Pts',(-5.95305829295893,-1.10901465410688,
6.60434352087773));
#148529=CARTESIAN_POINT('Ctrl Pts',(-5.96429703934163,-0.999999999678912,
6.73996742071359));
#148530=CARTESIAN_POINT('',(-6.055406976,-1.32768940200002,6.208141225));
#148531=CARTESIAN_POINT('Ctrl Pts',(-5.93021523353202,-1.32768940199765,
6.32783678695391));
#148532=CARTESIAN_POINT('Ctrl Pts',(-5.92973427764573,-1.33223595152411,
6.32205646756782));
#148533=CARTESIAN_POINT('Ctrl Pts',(-5.92995177522349,-1.33650155486746,
6.31600361284212));
#148534=CARTESIAN_POINT('Ctrl Pts',(-5.93251804458815,-1.34730670125214,
6.29876236986105));
#148535=CARTESIAN_POINT('Ctrl Pts',(-5.93634880100404,-1.35293307647141,
6.28742148754437));
#148536=CARTESIAN_POINT('Ctrl Pts',(-5.94543448325041,-1.35917045618876,
6.27023026460104));
#148537=CARTESIAN_POINT('Ctrl Pts',(-5.94928467914374,-1.3608789886345,
6.26422178483839));
#148538=CARTESIAN_POINT('Ctrl Pts',(-5.95803584785762,-1.36317274250118,
6.25273097932687));
#148539=CARTESIAN_POINT('Ctrl Pts',(-5.9629065793017,-1.36375173607124,
6.24728602014727));
#148540=CARTESIAN_POINT('Ctrl Pts',(-5.96818860320827,-1.36375173607065,
6.24223588820087));
#148541=CARTESIAN_POINT('Ctrl Pts',(-5.97747916718048,-1.36375173606962,
6.23335319952962));
#148542=CARTESIAN_POINT('Ctrl Pts',(-5.98789111364512,-1.36196031910978,
6.22583574159617));
#148543=CARTESIAN_POINT('Ctrl Pts',(-6.00989329559083,-1.3549908654096,
6.21429873031894));
#148544=CARTESIAN_POINT('Ctrl Pts',(-6.02126765851763,-1.34985996732778,
6.21042210882142));
#148545=CARTESIAN_POINT('Ctrl Pts',(-6.0403693472299,-1.33873894496681,
6.20736863188564));
#148546=CARTESIAN_POINT('Ctrl Pts',(-6.04812429250931,-1.33344492734667,
6.20720469845112));
#148547=CARTESIAN_POINT('Ctrl Pts',(-6.05540697612596,-1.32768940215382,
6.20814122496572));
#148548=CARTESIAN_POINT('Ctrl Pts',(-6.46559354791635,-0.999999999885754,
6.26067888293268));
#148549=CARTESIAN_POINT('Ctrl Pts',(-6.33061033303081,-1.10901473812568,
6.24336669663294));
#148550=CARTESIAN_POINT('Ctrl Pts',(-6.19376580688885,-1.21834403200888,
6.22593366519494));
#148551=CARTESIAN_POINT('Ctrl Pts',(-6.05540697622249,-1.32768940224085,
6.20814122474999));
#148552=CARTESIAN_POINT('',(-6.473564847,-1.32768940200002,5.770782381));
#148553=CARTESIAN_POINT('Ctrl Pts',(-6.47356484705234,-1.32768940202094,
5.77078238100751));
#148554=CARTESIAN_POINT('Ctrl Pts',(-6.49754686040969,-1.21834383453442,
5.90820388664413));
#148555=CARTESIAN_POINT('Ctrl Pts',(-6.52110181902666,-1.10901465430655,
6.04412834439049));
#148556=CARTESIAN_POINT('Ctrl Pts',(-6.54445255418411,-0.999999999849286,
6.17819882884537));
#148557=CARTESIAN_POINT('',(-6.587523177,-1.32768940200002,5.640346578));
#148558=CARTESIAN_POINT('Ctrl Pts',(-6.47356484669524,-1.32768940216809,
5.77078238118696));
#148559=CARTESIAN_POINT('Ctrl Pts',(-6.47256768322408,-1.33223595155632,
5.76506844435758));
#148560=CARTESIAN_POINT('Ctrl Pts',(-6.47224173153327,-1.33650155477443,
5.75902046047074));
#148561=CARTESIAN_POINT('Ctrl Pts',(-6.47325217673578,-1.3473067010545,
5.74161858722323));
#148562=CARTESIAN_POINT('Ctrl Pts',(-6.47605092279891,-1.35293307627464,
5.72997997360681));
#148563=CARTESIAN_POINT('Ctrl Pts',(-6.48355901941539,-1.3591704559933,
5.71204352319526));
#148564=CARTESIAN_POINT('Ctrl Pts',(-6.48685511957833,-1.3608789884395,
5.70571410290666));
#148565=CARTESIAN_POINT('Ctrl Pts',(-6.49454103079465,-1.36317274230711,
5.69348510728424));
#148566=CARTESIAN_POINT('Ctrl Pts',(-6.49890407172791,-1.36375173587764,
5.68762545890897));
#148567=CARTESIAN_POINT('Ctrl Pts',(-6.50371214142148,-1.36375173587751,
5.6821221803364));
#148568=CARTESIAN_POINT('Ctrl Pts',(-6.51216906624052,-1.36375173587729,
5.67244245102451));
#148569=CARTESIAN_POINT('Ctrl Pts',(-6.52186523753564,-1.36196031891828,
5.6640219364811));
#148570=CARTESIAN_POINT('Ctrl Pts',(-6.54274467544731,-1.35499086521973,
5.65055910943509));
#148571=CARTESIAN_POINT('Ctrl Pts',(-6.55372575086093,-1.34985996713871,
5.64567850404374));
#148572=CARTESIAN_POINT('Ctrl Pts',(-6.57247683027915,-1.33873894474862,
5.64092505731962));
#148573=CARTESIAN_POINT('Ctrl Pts',(-6.58018586159814,-1.33344492709045,
5.64006663589892));
#148574=CARTESIAN_POINT('Ctrl Pts',(-6.58752317690413,-1.3276894018546,
5.64034657752293));
#148575=CARTESIAN_POINT('Ctrl Pts',(-7.00076789692398,-0.999999999893324,
5.65590389374847));
#148576=CARTESIAN_POINT('Ctrl Pts',(-6.86477623251869,-1.10901473799573,
5.65076120332883));
#148577=CARTESIAN_POINT('Ctrl Pts',(-6.72691991747828,-1.21834403174059,
5.64566500091207));
#148578=CARTESIAN_POINT('Ctrl Pts',(-6.58752317688628,-1.32768940183436,
5.64034657757489));
#148579=CARTESIAN_POINT('',(-6.964793123,-1.32768940200002,5.167265029));
#148580=CARTESIAN_POINT('Ctrl Pts',(-6.9647931225424,-1.32768940189471,
5.1672650290375));
#148581=CARTESIAN_POINT('Ctrl Pts',(-7.00099696010947,-1.21834383456653,
5.3019835847847));
#148582=CARTESIAN_POINT('Ctrl Pts',(-7.03664126779649,-1.10901465449722,
5.43524940021246));
#148583=CARTESIAN_POINT('Ctrl Pts',(-7.07191598528383,-1.00000000019748,
5.56668701235598));
#148584=CARTESIAN_POINT('',(-7.066600514,-1.32768940200002,5.027139175));
#148585=CARTESIAN_POINT('Ctrl Pts',(-6.96479312275204,-1.32768940180384,
5.16726502890744));
#148586=CARTESIAN_POINT('Ctrl Pts',(-6.96328778019254,-1.3322359512407,
5.1616634797066));
#148587=CARTESIAN_POINT('Ctrl Pts',(-6.96242100357657,-1.33650155450293,
5.155669061255));
#148588=CARTESIAN_POINT('Ctrl Pts',(-6.9618674891292,-1.34730670082041,
5.13824666716369));
#148589=CARTESIAN_POINT('Ctrl Pts',(-6.96361169098159,-1.35293307604079,
5.12640402952092));
#148590=CARTESIAN_POINT('Ctrl Pts',(-6.9694817511883,-1.35917045575974,
5.10786676539327));
#148591=CARTESIAN_POINT('Ctrl Pts',(-6.97219721736018,-1.36087898820603,
5.10126736534918));
#148592=CARTESIAN_POINT('Ctrl Pts',(-6.97875598864058,-1.36317274207381,
5.08839864029793));
#148593=CARTESIAN_POINT('Ctrl Pts',(-6.98257621042259,-1.36375173564443,
5.08217148117021));
#148594=CARTESIAN_POINT('Ctrl Pts',(-6.9868716141528,-1.36375173564439,
5.07625936513458));
#148595=CARTESIAN_POINT('Ctrl Pts',(-6.9944268096322,-1.36375173564433,
5.06586053067068));
#148596=CARTESIAN_POINT('Ctrl Pts',(-7.00332913788735,-1.36196031868552,
5.05660475654901));
#148597=CARTESIAN_POINT('Ctrl Pts',(-7.02291772280706,-1.35499086498739,
5.04132450850107));
#148598=CARTESIAN_POINT('Ctrl Pts',(-7.03341709754474,-1.34985996690657,
5.0354792149805));
#148599=CARTESIAN_POINT('Ctrl Pts',(-7.05166659470129,-1.33873894466853,
5.02906407052158));
#148600=CARTESIAN_POINT('Ctrl Pts',(-7.05926764317835,-1.33344492720299,
5.02751807262591));
#148601=CARTESIAN_POINT('Ctrl Pts',(-7.06660051416279,-1.32768940218439,
5.0271391753499));
#148602=CARTESIAN_POINT('Ctrl Pts',(-7.47957617995657,-0.999999999937531,
5.00559089112874));
#148603=CARTESIAN_POINT('Ctrl Pts',(-7.34367099065878,-1.1090147381492,
5.01265910249651));
#148604=CARTESIAN_POINT('Ctrl Pts',(-7.20591282440991,-1.2183440320037,
5.01994076071517));
#148605=CARTESIAN_POINT('Ctrl Pts',(-7.06660051417724,-1.32768940220666,
5.02713917529118));
#148606=CARTESIAN_POINT('',(-7.399944979,-1.32768940200002,4.522143897));
#148607=CARTESIAN_POINT('Ctrl Pts',(-7.39994497873908,-1.3276894021564,
4.52214389722653));
#148608=CARTESIAN_POINT('Ctrl Pts',(-7.44807914856805,-1.21834383484025,
4.65307482860847));
#148609=CARTESIAN_POINT('Ctrl Pts',(-7.49552581838299,-1.10901465478351,
4.78260902385036));
#148610=CARTESIAN_POINT('Ctrl Pts',(-7.5424405069824,-1.00000000049598,
4.9103555054297));
#148611=CARTESIAN_POINT('',(-7.488781739,-1.32768940200002,4.373456206));
#148612=CARTESIAN_POINT('Ctrl Pts',(-7.39994497860661,-1.32768940221744,
4.52214389732625));
#148613=CARTESIAN_POINT('Ctrl Pts',(-7.39794357718913,-1.33223595153308,
4.5166998362934));
#148614=CARTESIAN_POINT('Ctrl Pts',(-7.39654295448025,-1.33650155468582,
4.51080724699966));
#148615=CARTESIAN_POINT('Ctrl Pts',(-7.39442993696486,-1.34730670091578,
4.4935046071502));
#148616=CARTESIAN_POINT('Ctrl Pts',(-7.39510555131524,-1.3529330761409,
4.48155329543664));
#148617=CARTESIAN_POINT('Ctrl Pts',(-7.39929031283406,-1.35917045586763,
4.46256446874344));
#148618=CARTESIAN_POINT('Ctrl Pts',(-7.40140328167635,-1.36087898831677,
4.45574822343215));
#148619=CARTESIAN_POINT('Ctrl Pts',(-7.40678210564818,-1.36317274219025,
4.44234338035806));
#148620=CARTESIAN_POINT('Ctrl Pts',(-7.41002875009816,-1.36375173576373,
4.43579884790071));
#148621=CARTESIAN_POINT('Ctrl Pts',(-7.41377690379883,-1.36375173576648,
4.42952549528285));
#148622=CARTESIAN_POINT('Ctrl Pts',(-7.42036953994479,-1.36375173577133,
4.41849128096622));
#148623=CARTESIAN_POINT('Ctrl Pts',(-7.42840634884571,-1.36196031881741,
4.40847476931493));
#148624=CARTESIAN_POINT('Ctrl Pts',(-7.44654636500287,-1.3549908651285,
4.39150012783265));
#148625=CARTESIAN_POINT('Ctrl Pts',(-7.45647950427152,-1.34985996705218,
4.3847372090463));
#148626=CARTESIAN_POINT('Ctrl Pts',(-7.47408048527612,-1.33873894477316,
4.37671201771834));
#148627=CARTESIAN_POINT('Ctrl Pts',(-7.48151235206001,-1.3334449272496,
4.37449089080898));
#148628=CARTESIAN_POINT('Ctrl Pts',(-7.48878173904294,-1.32768940216483,
4.37345620538491));
#148629=CARTESIAN_POINT('Ctrl Pts',(-7.89816331290478,-0.999999999857505,
4.31497581514083));
#148630=CARTESIAN_POINT('Ctrl Pts',(-7.76343882751087,-1.10901473804168,
4.3341980192771));
#148631=CARTESIAN_POINT('Ctrl Pts',(-7.62688795793261,-1.21834403186849,
4.35379891056257));
#148632=CARTESIAN_POINT('Ctrl Pts',(-7.48878173899302,-1.32768940204296,
4.37345620571205));
#148633=CARTESIAN_POINT('',(-7.77551683,-1.32768940200002,3.840613121));
#148634=CARTESIAN_POINT('Ctrl Pts',(-7.77551682982721,-1.32768940206457,
3.84061312113776));
#148635=CARTESIAN_POINT('Ctrl Pts',(-7.83519378383851,-1.21834383471285,
3.96670224946581));
#148636=CARTESIAN_POINT('Ctrl Pts',(-7.89406080304461,-1.10901465462005,
4.09146189152694));
#148637=CARTESIAN_POINT('Ctrl Pts',(-7.952237733216,-1.00000000029693,4.21448870316095));
#148638=CARTESIAN_POINT('',(-7.85066769791133,-1.32768940203921,3.68456073648917));
#148639=CARTESIAN_POINT('Ctrl Pts',(-7.77551682988423,-1.32768940203625,
3.84061312108627));
#148640=CARTESIAN_POINT('Ctrl Pts',(-7.77303548357002,-1.33223595146919,
3.83537038038259));
#148641=CARTESIAN_POINT('Ctrl Pts',(-7.77111229166754,-1.33650155472793,
3.82962706364747));
#148642=CARTESIAN_POINT('Ctrl Pts',(-7.76745678383559,-1.34730670104337,
3.81258348842368));
#148643=CARTESIAN_POINT('Ctrl Pts',(-7.76705837104186,-1.35293307626466,
3.80061972757349));
#148644=CARTESIAN_POINT('Ctrl Pts',(-7.76952414064379,-1.3591704559852,
3.78133222518374));
#148645=CARTESIAN_POINT('Ctrl Pts',(-7.77101759977719,-1.36087898843209,
3.77435401500558));
#148646=CARTESIAN_POINT('Ctrl Pts',(-7.77517316931866,-1.36317274230107,
3.76052098182607));
#148647=CARTESIAN_POINT('Ctrl Pts',(-7.77782009636727,-1.36375173587229,
3.75371176876822));
#148648=CARTESIAN_POINT('Ctrl Pts',(-7.78099082211098,-1.36375173587283,
3.74712768891714));
#148649=CARTESIAN_POINT('Ctrl Pts',(-7.78656781889864,-1.36375173587379,
3.73554693575616));
#148650=CARTESIAN_POINT('Ctrl Pts',(-7.79367440078957,-1.36196031891597,
3.7248503336419));
#148651=CARTESIAN_POINT('Ctrl Pts',(-7.81021979544659,-1.35499086521966,
3.70631796856791));
#148652=CARTESIAN_POINT('Ctrl Pts',(-7.81950672345208,-1.34985996713973,
3.69869187556753));
#148653=CARTESIAN_POINT('Ctrl Pts',(-7.83631747555383,-1.33873894480565,
3.68912125148975));
#148654=CARTESIAN_POINT('Ctrl Pts',(-7.8435203236244,-1.33344492721708,
3.6862428787659));
#148655=CARTESIAN_POINT('Ctrl Pts',(-7.85066769778106,-1.32768940205954,
3.68456073586607));
#148656=CARTESIAN_POINT('Ctrl Pts',(-8.25315907915067,-1.0000000002333,
3.58961908982468));
#148657=CARTESIAN_POINT('Ctrl Pts',(-8.12070002029395,-1.10901473821362,
3.62084052066842));
#148658=CARTESIAN_POINT('Ctrl Pts',(-7.98645587500192,-1.21834403183509,
3.65260282999209));
#148659=CARTESIAN_POINT('Ctrl Pts',(-7.85066769773845,-1.32768940180501,
3.68456073655596));
#148660=CARTESIAN_POINT('',(-8.088484791,-1.32768940200002,3.128159987));
#148661=CARTESIAN_POINT('Ctrl Pts',(-8.08848479089928,-1.32768940204577,
3.12815998710086));
#148662=CARTESIAN_POINT('Ctrl Pts',(-8.15922404537986,-1.21834383466874,
3.2483921167694));
#148663=CARTESIAN_POINT('Ctrl Pts',(-8.2290374513845,-1.10901465455067,
3.3673727142875));
#148664=CARTESIAN_POINT('Ctrl Pts',(-8.29800821672838,-1.00000000020229,
3.48468931634764));
#148665=CARTESIAN_POINT('',(-8.14934469545831,-1.32768940190648,2.96599935139841));
#148666=CARTESIAN_POINT('Ctrl Pts',(-8.08848479065033,-1.32768940218081,
3.1281599873702));
#148667=CARTESIAN_POINT('Ctrl Pts',(-8.08554347786003,-1.33223595160539,
3.12316077857491));
#148668=CARTESIAN_POINT('Ctrl Pts',(-8.08311320122475,-1.33650155485665,
3.11761297634637));
#148669=CARTESIAN_POINT('Ctrl Pts',(-8.07794463509115,-1.34730670116671,
3.10096569075218));
#148670=CARTESIAN_POINT('Ctrl Pts',(-8.07647540293555,-1.35293307638893,
3.08908580593355));
#148671=CARTESIAN_POINT('Ctrl Pts',(-8.07720232768916,-1.35917045611106,
3.06965491947504));
#148672=CARTESIAN_POINT('Ctrl Pts',(-8.07806425265739,-1.36087898855854,
3.06257092887488));
#148673=CARTESIAN_POINT('Ctrl Pts',(-8.08096310956339,-1.3631727424287,
3.04842108103817));
#148674=CARTESIAN_POINT('Ctrl Pts',(-8.08298900770923,-1.36375173600051,
3.04140201115875));
#148675=CARTESIAN_POINT('Ctrl Pts',(-8.08555677667574,-1.36375173600163,
3.03456021521294));
#148676=CARTESIAN_POINT('Ctrl Pts',(-8.09007323140408,-1.3637517360036,
3.02252616462162));
#148677=CARTESIAN_POINT('Ctrl Pts',(-8.0961923682646,-1.36196031904677,
3.01123559479314));
#148678=CARTESIAN_POINT('Ctrl Pts',(-8.11100992762966,-1.35499086535231,
2.99129471782953));
#148679=CARTESIAN_POINT('Ctrl Pts',(-8.11957587148718,-1.34985996727329,
2.98286685142906));
#148680=CARTESIAN_POINT('Ctrl Pts',(-8.13546104438258,-1.33873894489342,
2.97182785162225));
#148681=CARTESIAN_POINT('Ctrl Pts',(-8.14237688063509,-1.33344492724556,
2.96831540803315));
#148682=CARTESIAN_POINT('Ctrl Pts',(-8.14934469550913,-1.327689402021,2.96599935126671));
#148683=CARTESIAN_POINT('Ctrl Pts',(-8.54170526199855,-0.99999999983659,
2.83536086241028));
#148684=CARTESIAN_POINT('Ctrl Pts',(-8.41257811164622,-1.10901473799347,
2.87833014352137));
#148685=CARTESIAN_POINT('Ctrl Pts',(-8.28172154505887,-1.21834403179278,
2.92199813961197));
#148686=CARTESIAN_POINT('Ctrl Pts',(-8.14934469551528,-1.32768940194035,
2.96599935148564));
#148687=CARTESIAN_POINT('',(-8.336329029,-1.32768940200002,2.390520747));
#148688=CARTESIAN_POINT('Ctrl Pts',(-8.33632902896119,-1.32768940187384,
2.39052074690615));
#148689=CARTESIAN_POINT('Ctrl Pts',(-8.41756103301671,-1.21834383447248,
2.50392783959535));
#148690=CARTESIAN_POINT('Ctrl Pts',(-8.49775872931061,-1.10901465432932,
2.61617143085006));
#148691=CARTESIAN_POINT('Ctrl Pts',(-8.57696801776182,-0.999999999956059,
2.72683325912717));
#148692=CARTESIAN_POINT('',(-8.382407962,-1.32768940200002,2.223557482));
#148693=CARTESIAN_POINT('Ctrl Pts',(-8.33632902867258,-1.32768940204799,
2.39052074728083));
#148694=CARTESIAN_POINT('Ctrl Pts',(-8.33295143111257,-1.33223595148368,
2.3858053210651));
#148695=CARTESIAN_POINT('Ctrl Pts',(-8.33003363689228,-1.33650155474458,
2.38049770096133));
#148696=CARTESIAN_POINT('Ctrl Pts',(-8.32339362671072,-1.34730670105808,
2.36438073912204));
#148697=CARTESIAN_POINT('Ctrl Pts',(-8.32086540459087,-1.35293307627555,
2.3526803801806));
#148698=CARTESIAN_POINT('Ctrl Pts',(-8.31984763173159,-1.35917045598988,
2.33326255572514));
#148699=CARTESIAN_POINT('Ctrl Pts',(-8.3200710828237,-1.3608789884345,2.32612982083004));
#148700=CARTESIAN_POINT('Ctrl Pts',(-8.32168988720682,-1.36317274229893,
2.31177708459179));
#148701=CARTESIAN_POINT('Ctrl Pts',(-8.32307844511106,-1.36375173586787,
2.3046046713151));
#148702=CARTESIAN_POINT('Ctrl Pts',(-8.32502258313608,-1.36375173586619,
2.29756024539374));
#148703=CARTESIAN_POINT('Ctrl Pts',(-8.32844213197043,-1.36375173586324,
2.28516978847247));
#148704=CARTESIAN_POINT('Ctrl Pts',(-8.33352455611133,-1.3619603189015,
2.27337615596146));
#148705=CARTESIAN_POINT('Ctrl Pts',(-8.34649497791398,-1.3549908651978,
2.25218731932978));
#148706=CARTESIAN_POINT('Ctrl Pts',(-8.3542709696827,-1.34985996711426,
2.24302553575725));
#148707=CARTESIAN_POINT('Ctrl Pts',(-8.36910266521966,-1.33873894473671,
2.23060703981489));
#148708=CARTESIAN_POINT('Ctrl Pts',(-8.37567580732036,-1.33344492709784,
2.2264888055179));
#148709=CARTESIAN_POINT('Ctrl Pts',(-8.38240796207933,-1.32768940188415,
2.2235574824097));
#148710=CARTESIAN_POINT('Ctrl Pts',(-8.76147865594041,-1.00000000018313,
2.05827397549611));
#148711=CARTESIAN_POINT('Ctrl Pts',(-8.63672307032885,-1.10901473824795,
2.11264514330979));
#148712=CARTESIAN_POINT('Ctrl Pts',(-8.51030766293713,-1.21834403195478,
2.16786723695558));
#148713=CARTESIAN_POINT('Ctrl Pts',(-8.38240796203887,-1.32768940201087,
2.22355748206797));
#148714=CARTESIAN_POINT('',(-8.517054046,-1.32768940200002,1.633634441));
#148715=CARTESIAN_POINT('Ctrl Pts',(-8.51705404654846,-1.32768940205777,
1.63363444058708));
#148716=CARTESIAN_POINT('Ctrl Pts',(-8.60812476791986,-1.21834383457677,
1.73930340900002));
#148717=CARTESIAN_POINT('Ctrl Pts',(-8.69806104988347,-1.10901465435411,
1.8439062745251));
#148718=CARTESIAN_POINT('Ctrl Pts',(-8.78687111490327,-0.999999999901667,
1.94702234497933));
#148719=CARTESIAN_POINT('',(-8.547981008,-1.32768940200002,1.463212837));
#148720=CARTESIAN_POINT('Ctrl Pts',(-8.51705404632891,-1.32768940220838,
1.6336344409322));
#148721=CARTESIAN_POINT('Ctrl Pts',(-8.5132673585444,-1.33223595152413,
1.62924076322205));
#148722=CARTESIAN_POINT('Ctrl Pts',(-8.50988553919814,-1.33650155467649,
1.62421605920029));
#148723=CARTESIAN_POINT('Ctrl Pts',(-8.501827546491,-1.34730670090064,1.6087591855685));
#148724=CARTESIAN_POINT('Ctrl Pts',(-8.49826069015918,-1.3529330761202,
1.59733255691655));
#148725=CARTESIAN_POINT('Ctrl Pts',(-8.49550641418745,-1.35917045583786,
1.57808413536979));
#148726=CARTESIAN_POINT('Ctrl Pts',(-8.49508959230381,-1.36087898828368,
1.57096008476704));
#148727=CARTESIAN_POINT('Ctrl Pts',(-8.49541531049769,-1.36317274215052,
1.55652001991911));
#148728=CARTESIAN_POINT('Ctrl Pts',(-8.49615534830605,-1.36375173572067,
1.54925201129861));
#148729=CARTESIAN_POINT('Ctrl Pts',(-8.4974602023311,-1.36375173572018,
1.54206167297576));
#148730=CARTESIAN_POINT('Ctrl Pts',(-8.49975531307054,-1.3637517357193,
1.52941457039706));
#148731=CARTESIAN_POINT('Ctrl Pts',(-8.50376010379714,-1.36196031875968,
1.5172128305953));
#148732=CARTESIAN_POINT('Ctrl Pts',(-8.51477895782059,-1.35499086505998,
1.49494663434249));
#148733=CARTESIAN_POINT('Ctrl Pts',(-8.52170238978373,-1.34985996697839,
1.48512469888792));
#148734=CARTESIAN_POINT('Ctrl Pts',(-8.53536119188796,-1.33873894459695,
1.4714266932106));
#148735=CARTESIAN_POINT('Ctrl Pts',(-8.54153871678395,-1.33344492695049,
1.46673582579239));
#148736=CARTESIAN_POINT('Ctrl Pts',(-8.54798100809932,-1.32768940172794,
1.46321283762611));
#148737=CARTESIAN_POINT('Ctrl Pts',(-8.91070977514109,-1.00000000032794,
1.26461507871066));
#148738=CARTESIAN_POINT('Ctrl Pts',(-8.79133021285898,-1.10901473827852,
1.32995036863205));
#148739=CARTESIAN_POINT('Ctrl Pts',(-8.6703737871565,-1.21834403187058,
1.39628194408302));
#148740=CARTESIAN_POINT('Ctrl Pts',(-8.54798100805239,-1.32768940181178,
1.46321283740334));
#148741=CARTESIAN_POINT('',(-8.629204753,-1.32768940200002,0.863595070000001));
#148742=CARTESIAN_POINT('Ctrl Pts',(-8.6292047530183,-1.32768940220178,
0.86359507020837));
#148743=CARTESIAN_POINT('Ctrl Pts',(-8.72938094365667,-1.21834383481036,
0.960675129813629));
#148744=CARTESIAN_POINT('Ctrl Pts',(-8.82833169708263,-1.10901465467741,
1.05679506871452));
#148745=CARTESIAN_POINT('Ctrl Pts',(-8.9260274921021,-1.00000000031437,
1.15153515125643));
#148746=CARTESIAN_POINT('',(-8.644730737,-1.32768940200002,0.691087263000001));
#148747=CARTESIAN_POINT('Ctrl Pts',(-8.62920475309882,-1.32768940213718,
0.863595070052577));
#148748=CARTESIAN_POINT('Ctrl Pts',(-8.62503946318526,-1.33223595143947,
0.859558516080467));
#148749=CARTESIAN_POINT('Ctrl Pts',(-8.62122084706452,-1.33650155457962,
0.85485718399984));
#148750=CARTESIAN_POINT('Ctrl Pts',(-8.6118097500053,-1.34730670079354,
0.840184848108705));
#148751=CARTESIAN_POINT('Ctrl Pts',(-8.60723297769259,-1.35293307601313,
0.829123950240993));
#148752=CARTESIAN_POINT('Ctrl Pts',(-8.60276437442064,-1.35917045573079,
0.810199908575198));
#148753=CARTESIAN_POINT('Ctrl Pts',(-8.60171063556652,-1.3608789881766,
0.803141900931399));
#148754=CARTESIAN_POINT('Ctrl Pts',(-8.60074064508077,-1.36317274204343,
0.788730770385564));
#148755=CARTESIAN_POINT('Ctrl Pts',(-8.60082620444441,-1.36375173561358,
0.781425684153338));
#148756=CARTESIAN_POINT('Ctrl Pts',(-8.60148126855249,-1.36375173561308,
0.77414732580565));
#148757=CARTESIAN_POINT('Ctrl Pts',(-8.60263346231566,-1.3637517356122,
0.76134540460328));
#148758=CARTESIAN_POINT('Ctrl Pts',(-8.60552837540853,-1.36196031865257,
0.748833798745692));
#148759=CARTESIAN_POINT('Ctrl Pts',(-8.61450694432037,-1.35499086495292,
0.72566951719315));
#148760=CARTESIAN_POINT('Ctrl Pts',(-8.6205220730753,-1.34985996687135,
0.715266510306567));
#148761=CARTESIAN_POINT('Ctrl Pts',(-8.63289800898064,-1.33873894459279,
0.700399283329012));
#148762=CARTESIAN_POINT('Ctrl Pts',(-8.63863017872564,-1.33344492707686,
0.695173550994194));
#148763=CARTESIAN_POINT('Ctrl Pts',(-8.64473073689484,-1.32768940200152,
0.691087262840884));
#148764=CARTESIAN_POINT('Ctrl Pts',(-8.98819709909128,-1.00000000022958,
0.460774243805898));
#148765=CARTESIAN_POINT('Ctrl Pts',(-8.87515473393588,-1.10901473830768,
0.53654761461009));
#148766=CARTESIAN_POINT('Ctrl Pts',(-8.76063115969153,-1.21834403202809,
0.613454609141289));
#148767=CARTESIAN_POINT('Ctrl Pts',(-8.64473073681857,-1.32768940209738,
0.69108726259199));
#148768=CARTESIAN_POINT('',(-8.671878177,-1.32768940200002,0.0866025400000026));
#148769=CARTESIAN_POINT('Ctrl Pts',(-8.67187817713732,-1.32768940195935,
0.0866025397794755));
#148770=CARTESIAN_POINT('Ctrl Pts',(-8.78035327729649,-1.21834383460799,
0.174312059059674));
#148771=CARTESIAN_POINT('Ctrl Pts',(-8.88752180893807,-1.10901465451525,
0.261175170144174));
#148772=CARTESIAN_POINT('Ctrl Pts',(-8.99331674489802,-1.00000000019189,
0.346776473370395));
#148773=CARTESIAN_POINT('',(-8.63624826494697,-1.36375173570061,3.85948676359093E-15));
#148774=CARTESIAN_POINT('Ctrl Pts',(-8.67187817702726,-1.32768940206671,
0.0866025400494883));
#148775=CARTESIAN_POINT('Ctrl Pts',(-8.66736782138124,-1.33223595142604,
0.0829556097415469));
#148776=CARTESIAN_POINT('Ctrl Pts',(-8.66314315367645,-1.33650155461798,
0.078615501910959));
#148777=CARTESIAN_POINT('Ctrl Pts',(-8.65245472483424,-1.34730670087631,
0.0648458367127613));
#148778=CARTESIAN_POINT('Ctrl Pts',(-8.64690488602001,-1.35293307609673,
0.0542397254755955));
#148779=CARTESIAN_POINT('Ctrl Pts',(-8.64075793401352,-1.35917045581577,
0.0357924289474454));
#148780=CARTESIAN_POINT('Ctrl Pts',(-8.63907576227445,-1.3608789882621,
0.0288572911901097));
#148781=CARTESIAN_POINT('Ctrl Pts',(-8.63681787290186,-1.36317274212995,
0.0145911248958308));
#148782=CARTESIAN_POINT('Ctrl Pts',(-8.63624826494697,-1.36375173570061,
0.00730777731084098));
#148783=CARTESIAN_POINT('Ctrl Pts',(-8.63624826494697,-1.36375173570061,
4.44089209850063E-15));
#148784=CARTESIAN_POINT('',(-8.50000000044506,-1.50000000044508,3.26139582858007E-15));
#148785=CARTESIAN_POINT('',(-9.,-1.00000000000002,3.32262816848293E-15));
#148786=CARTESIAN_POINT('Origin',(1.11022302462516E-15,-1.50000000000002,
2.22044604925031E-15));
#148787=CARTESIAN_POINT('',(-8.671878177,-1.32768940200002,-0.0866025400000003));
#148788=CARTESIAN_POINT('Ctrl Pts',(-8.63624826494697,-1.36375173570061,
4.44089209850061E-15));
#148789=CARTESIAN_POINT('Ctrl Pts',(-8.63624826494697,-1.36375173570061,
-0.0128536662840206));
#148790=CARTESIAN_POINT('Ctrl Pts',(-8.63800999226789,-1.36196031874185,
-0.0255744021040272));
#148791=CARTESIAN_POINT('Ctrl Pts',(-8.64487598591024,-1.35499086504381,
-0.0494502637821181));
#148792=CARTESIAN_POINT('Ctrl Pts',(-8.64993438117684,-1.34985996696303,
-0.0603505832064033));
#148793=CARTESIAN_POINT('Ctrl Pts',(-8.66092780725787,-1.33873894467796,
-0.0762673294526308));
#148794=CARTESIAN_POINT('Ctrl Pts',(-8.66616846994706,-1.33344492715271,
-0.0819858522681948));
#148795=CARTESIAN_POINT('Ctrl Pts',(-8.67187817702724,-1.32768940206672,
-0.0866025400494692));
#148796=CARTESIAN_POINT('Ctrl Pts',(-8.99331674490455,-1.00000000018596,
-0.34677647335477));
#148797=CARTESIAN_POINT('Ctrl Pts',(-8.88752172769541,-1.10901473823108,
-0.261175104387876));
#148798=CARTESIAN_POINT('Ctrl Pts',(-8.78035308155773,-1.21834403191783,
-0.174311900770753));
#148799=CARTESIAN_POINT('Ctrl Pts',(-8.67187817714367,-1.32768940195315,
-0.0866025397638889));
#148800=CARTESIAN_POINT('',(-8.644730737,-1.32768940200002,-0.691087262999999));
#148801=CARTESIAN_POINT('Ctrl Pts',(-8.64473073694086,-1.32768940194368,
-0.691087262991059));
#148802=CARTESIAN_POINT('Ctrl Pts',(-8.76063136896071,-1.2183438345599,
-0.613454469453119));
#148803=CARTESIAN_POINT('Ctrl Pts',(-8.87515482087759,-1.10901465443496,
-0.536547556821678));
#148804=CARTESIAN_POINT('Ctrl Pts',(-8.9881970992204,-1.00000000007973,
-0.460774244214113));
#148805=CARTESIAN_POINT('',(-8.629204753,-1.32768940200002,-0.863595069999998));
#148806=CARTESIAN_POINT('Ctrl Pts',(-8.64473073689486,-1.3276894020015,
-0.691087262840871));
#148807=CARTESIAN_POINT('Ctrl Pts',(-8.63991163031322,-1.33223595135028,
-0.694315206512241));
#148808=CARTESIAN_POINT('Ctrl Pts',(-8.63531492562229,-1.33650155453274,
-0.698259146043823));
#148809=CARTESIAN_POINT('Ctrl Pts',(-8.62343522198836,-1.34730670078396,
-0.71101527523258));
#148810=CARTESIAN_POINT('Ctrl Pts',(-8.61695700071149,-1.35293307600527,
-0.721081205667742));
#148811=CARTESIAN_POINT('Ctrl Pts',(-8.60918119161373,-1.35917045572572,
-0.738903230273302));
#148812=CARTESIAN_POINT('Ctrl Pts',(-8.60688413084748,-1.36087898817254,
-0.745659660492604));
#148813=CARTESIAN_POINT('Ctrl Pts',(-8.60335652178569,-1.36317274204141,
-0.759665999752388));
#148814=CARTESIAN_POINT('Ctrl Pts',(-8.6021363326606,-1.36375173561258,
-0.766868967457801));
#148815=CARTESIAN_POINT('Ctrl Pts',(-8.60148126855249,-1.36375173561307,
-0.774147325805654));
#148816=CARTESIAN_POINT('Ctrl Pts',(-8.60032907478934,-1.36375173561395,
-0.786949247007962));
#148817=CARTESIAN_POINT('Ctrl Pts',(-8.60094343194575,-1.36196031865609,
-0.799776692904937));
#148818=CARTESIAN_POINT('Ctrl Pts',(-8.60564156937475,-1.35499086495975,
-0.824171900308657));
#148819=CARTESIAN_POINT('Ctrl Pts',(-8.60970250392851,-1.3498599668798,
-0.835481769307742));
#148820=CARTESIAN_POINT('Ctrl Pts',(-8.61922490753858,-1.33873894463695,
-0.852319882468269));
#148821=CARTESIAN_POINT('Ctrl Pts',(-8.62393186837942,-1.33344492716415,
-0.858485153528086));
#148822=CARTESIAN_POINT('Ctrl Pts',(-8.6292047530988,-1.3276894021372,-0.863595070052561));
#148823=CARTESIAN_POINT('Ctrl Pts',(-8.92602749216612,-1.00000000026639,
-1.1515351511352));
#148824=CARTESIAN_POINT('Ctrl Pts',(-8.8283316221154,-1.10901473835186,
-1.0567949958371));
#148825=CARTESIAN_POINT('Ctrl Pts',(-8.72938076294725,-1.2183440320791,
-0.960674954515165));
#148826=CARTESIAN_POINT('Ctrl Pts',(-8.62920475307709,-1.32768940215461,
-0.863595070094572));
#148827=CARTESIAN_POINT('',(-8.547981008,-1.32768940200002,-1.463212838));
#148828=CARTESIAN_POINT('Ctrl Pts',(-8.54798100788837,-1.32768940187191,
-1.46321283800513));
#148829=CARTESIAN_POINT('Ctrl Pts',(-8.67037400794378,-1.21834383453906,
-1.39628182386025));
#148830=CARTESIAN_POINT('Ctrl Pts',(-8.79133030455683,-1.10901465446515,
-1.32995031896542));
#148831=CARTESIAN_POINT('Ctrl Pts',(-8.91070977524376,-1.00000000016074,
-1.26461507917722));
#148832=CARTESIAN_POINT('',(-8.517054046,-1.32768940200002,-1.633634441));
#148833=CARTESIAN_POINT('Ctrl Pts',(-8.54798100783858,-1.32768940196087,
-1.46321283776869));
#148834=CARTESIAN_POINT('Ctrl Pts',(-8.5428919508647,-1.33223595136503,
-1.46599580531845));
#148835=CARTESIAN_POINT('Ctrl Pts',(-8.53796021908521,-1.33650155459768,
-1.4695118223078));
#148836=CARTESIAN_POINT('Ctrl Pts',(-8.52498488898969,-1.34730670089114,
-1.48115171069211));
#148837=CARTESIAN_POINT('Ctrl Pts',(-8.5176304440792,-1.3529330761124,-1.49059641537225));
#148838=CARTESIAN_POINT('Ctrl Pts',(-8.50828838413339,-1.35917045583282,
-1.50764967559236));
#148839=CARTESIAN_POINT('Ctrl Pts',(-8.50539492892273,-1.36087898827965,
-1.51417299947031));
#148840=CARTESIAN_POINT('Ctrl Pts',(-8.50062600240597,-1.36317274214851,
-1.52780674088759));
#148841=CARTESIAN_POINT('Ctrl Pts',(-8.49876505635617,-1.36375173571968,
-1.53487133465274));
#148842=CARTESIAN_POINT('Ctrl Pts',(-8.49746020233109,-1.36375173572018,
-1.54206167297575));
#148843=CARTESIAN_POINT('Ctrl Pts',(-8.49516509159166,-1.36375173572105,
-1.55470877555439));
#148844=CARTESIAN_POINT('Ctrl Pts',(-8.49462713214117,-1.36196031876316,
-1.56753965247642));
#148845=CARTESIAN_POINT('Ctrl Pts',(-8.49711958671714,-1.35499086506676,
-1.59225778973971));
#148846=CARTESIAN_POINT('Ctrl Pts',(-8.50015036430106,-1.34985996698678,
-1.60388614789829));
#148847=CARTESIAN_POINT('Ctrl Pts',(-8.50812507669321,-1.33873894473423,
-1.62151005745983));
#148848=CARTESIAN_POINT('Ctrl Pts',(-8.51226043806651,-1.33344492724917,
-1.62807243767969));
#148849=CARTESIAN_POINT('Ctrl Pts',(-8.51705404632889,-1.3276894022084,
-1.63363444093218));
#148850=CARTESIAN_POINT('Ctrl Pts',(-8.78687111486193,-0.999999999752181,
-1.94702234585691));
#148851=CARTESIAN_POINT('Ctrl Pts',(-8.69806098154262,-1.10901473805156,
-1.84390619609545));
#148852=CARTESIAN_POINT('Ctrl Pts',(-8.60812460334816,-1.2183440319946,
-1.73930321896202));
#148853=CARTESIAN_POINT('Ctrl Pts',(-8.51705404621577,-1.327689402286,-1.63363444110996));
#148854=CARTESIAN_POINT('',(-8.382407962,-1.32768940200002,-2.223557482));
#148855=CARTESIAN_POINT('Ctrl Pts',(-8.38240796213464,-1.3276894017109,
-2.22355748287687));
#148856=CARTESIAN_POINT('Ctrl Pts',(-8.51030789375738,-1.21834383440846,
-2.16786713730407));
#148857=CARTESIAN_POINT('Ctrl Pts',(-8.63672316609019,-1.10901465436549,
-2.11264510242941));
#148858=CARTESIAN_POINT('Ctrl Pts',(-8.76147865582069,-1.00000000009201,
-2.05827397640414));
#148859=CARTESIAN_POINT('',(-8.336329029,-1.32768940200002,-2.390520747));
#148860=CARTESIAN_POINT('Ctrl Pts',(-8.38240796207935,-1.32768940188413,
-2.22355748240969));
#148861=CARTESIAN_POINT('Ctrl Pts',(-8.37708992878106,-1.33223595136664,
-2.22587306701158));
#148862=CARTESIAN_POINT('Ctrl Pts',(-8.37186287728827,-1.33650155467049,
-2.22893285255653));
#148863=CARTESIAN_POINT('Ctrl Pts',(-8.3578963904289,-1.34730670102584,
-2.23936278260429));
#148864=CARTESIAN_POINT('Ctrl Pts',(-8.34972493555017,-1.35293307624908,
-2.24811021831965));
#148865=CARTESIAN_POINT('Ctrl Pts',(-8.33889184152879,-1.35917045597279,
-2.26425741132905));
#148866=CARTESIAN_POINT('Ctrl Pts',(-8.33542528827331,-1.36087898842084,
-2.27049510689713));
#148867=CARTESIAN_POINT('Ctrl Pts',(-8.32945344089287,-1.36317274229213,
-2.28364647960213));
#148868=CARTESIAN_POINT('Ctrl Pts',(-8.32696672116125,-1.36375173586451,
-2.29051581947185));
#148869=CARTESIAN_POINT('Ctrl Pts',(-8.32502258313608,-1.36375173586619,
-2.29756024539374));
#148870=CARTESIAN_POINT('Ctrl Pts',(-8.32160303430179,-1.36375173586915,
-2.30995070231481));
#148871=CARTESIAN_POINT('Ctrl Pts',(-8.31991708957668,-1.36196031891332,
-2.32268170358541));
#148872=CARTESIAN_POINT('Ctrl Pts',(-8.32018379351912,-1.35499086522079,
-2.34752375480153));
#148873=CARTESIAN_POINT('Ctrl Pts',(-8.32216001209316,-1.3498599671427,
-2.3593769774175));
#148874=CARTESIAN_POINT('Ctrl Pts',(-8.32852282561185,-1.3387389448062,
-2.37764478615217));
#148875=CARTESIAN_POINT('Ctrl Pts',(-8.33205329208909,-1.33344492721209,
-2.3845514392093));
#148876=CARTESIAN_POINT('Ctrl Pts',(-8.33632902867257,-1.32768940204801,
-2.39052074728081));
#148877=CARTESIAN_POINT('Ctrl Pts',(-8.57696801758913,-1.00000000005396,
-2.72683325934723));
#148878=CARTESIAN_POINT('Ctrl Pts',(-8.4977586683085,-1.10901473814976,
-2.61617134608161));
#148879=CARTESIAN_POINT('Ctrl Pts',(-8.41756088626376,-1.21834403188794,
-2.50392763516742));
#148880=CARTESIAN_POINT('Ctrl Pts',(-8.33632902879467,-1.32768940197433,
-2.3905207471223));
#148881=CARTESIAN_POINT('',(-8.149344695,-1.32768940200002,-2.965999351));
#148882=CARTESIAN_POINT('Ctrl Pts',(-8.14934469528739,-1.32768940216563,
-2.96599935145307));
#148883=CARTESIAN_POINT('Ctrl Pts',(-8.281721783784,-1.21834383463976,-2.92199806015237));
#148884=CARTESIAN_POINT('Ctrl Pts',(-8.41257821073727,-1.10901465437208,
-2.87833011043717));
#148885=CARTESIAN_POINT('Ctrl Pts',(-8.54170526199449,-0.999999999874979,
-2.83536086230067));
#148886=CARTESIAN_POINT('',(-8.088484791,-1.32768940200002,-3.128159987));
#148887=CARTESIAN_POINT('Ctrl Pts',(-8.14934469528428,-1.32768940220673,
-2.96599935134145));
#148888=CARTESIAN_POINT('Ctrl Pts',(-8.14384050348253,-1.33223595163131,
-2.96782890925026));
#148889=CARTESIAN_POINT('Ctrl Pts',(-8.13836021756285,-1.33650155488223,
-2.97040782769713));
#148890=CARTESIAN_POINT('Ctrl Pts',(-8.12351502401358,-1.3473067011882,
-2.97954382365383));
#148891=CARTESIAN_POINT('Ctrl Pts',(-8.11459235092013,-1.35293307640658,
-2.98752356120022));
#148892=CARTESIAN_POINT('Ctrl Pts',(-8.10235544453277,-1.35917045612245,
-3.00263467930046));
#148893=CARTESIAN_POINT('Ctrl Pts',(-8.09834370388333,-1.36087898856765,
-3.00853652430322));
#148894=CARTESIAN_POINT('Ctrl Pts',(-8.09121701744787,-1.36317274243323,
-3.02109964117803));
#148895=CARTESIAN_POINT('Ctrl Pts',(-8.08812454564211,-1.36375173600275,
-3.02771841926748));
#148896=CARTESIAN_POINT('Ctrl Pts',(-8.08555677667574,-1.36375173600163,
-3.03456021521294));
#148897=CARTESIAN_POINT('Ctrl Pts',(-8.08104032194735,-1.36375173599966,
-3.04659426580439));
#148898=CARTESIAN_POINT('Ctrl Pts',(-8.07821996618797,-1.36196031903889,
-3.05912288888715));
#148899=CARTESIAN_POINT('Ctrl Pts',(-8.0762587721631,-1.35499086533698,
-3.08388884046511));
#148900=CARTESIAN_POINT('Ctrl Pts',(-8.07716452038241,-1.34985996725432,
-3.09587149235794));
#148901=CARTESIAN_POINT('Ctrl Pts',(-8.08186420533724,-1.3387389449198,
-3.11463611845344));
#148902=CARTESIAN_POINT('Ctrl Pts',(-8.08476135158299,-1.33344492733438,
-3.12183143591671));
#148903=CARTESIAN_POINT('Ctrl Pts',(-8.08848479065032,-1.32768940218083,
-3.12815998737017));
#148904=CARTESIAN_POINT('Ctrl Pts',(-8.29800821672471,-1.00000000020416,
-3.48468931635154));
#148905=CARTESIAN_POINT('Ctrl Pts',(-8.22903739841268,-1.10901473827415,
-3.3673726241933));
#148906=CARTESIAN_POINT('Ctrl Pts',(-8.15922391772688,-1.21834403198615,
-3.24839189981149));
#148907=CARTESIAN_POINT('Ctrl Pts',(-8.0884847908968,-1.32768940204711,
-3.12815998710355));
#148908=CARTESIAN_POINT('',(-7.850667698,-1.32768940200002,-3.684560736));
#148909=CARTESIAN_POINT('Ctrl Pts',(-7.85066769785711,-1.32768940157741,
-3.68456073683881));
#148910=CARTESIAN_POINT('Ctrl Pts',(-7.98645612010734,-1.21834383433082,
-3.65260277261617));
#148911=CARTESIAN_POINT('Ctrl Pts',(-8.12070012204856,-1.109014654343,-3.62084049699314));
#148912=CARTESIAN_POINT('Ctrl Pts',(-8.25315907913426,-1.00000000012425,
-3.58961909013581));
#148913=CARTESIAN_POINT('',(-7.77551683,-1.32768940200002,-3.840613121));
#148914=CARTESIAN_POINT('Ctrl Pts',(-7.85066769791922,-1.32768940194829,
-3.68456073583355));
#148915=CARTESIAN_POINT('Ctrl Pts',(-7.84502166401927,-1.3322359514189,
-3.68588953652913));
#148916=CARTESIAN_POINT('Ctrl Pts',(-7.83933226760092,-1.33650155471162,
-3.68796682397788));
#148917=CARTESIAN_POINT('Ctrl Pts',(-7.82372789202241,-1.34730670105384,
-3.69573532823492));
#148918=CARTESIAN_POINT('Ctrl Pts',(-7.81412584082863,-1.35293307627325,
-3.70288311945405));
#148919=CARTESIAN_POINT('Ctrl Pts',(-7.80058364644548,-1.35917045599074,
-3.71683649680358));
#148920=CARTESIAN_POINT('Ctrl Pts',(-7.79605901857717,-1.36087898843653,
-3.72235497305409));
#148921=CARTESIAN_POINT('Ctrl Pts',(-7.78783487297177,-1.36317274230328,
-3.73422868326696));
#148922=CARTESIAN_POINT('Ctrl Pts',(-7.78416154785462,-1.36375173587338,
-3.74054360906622));
#148923=CARTESIAN_POINT('Ctrl Pts',(-7.78099082211098,-1.36375173587283,
-3.74712768891714));
#148924=CARTESIAN_POINT('Ctrl Pts',(-7.7754138253233,-1.36375173587187,
-3.75870844207817));
#148925=CARTESIAN_POINT('Ctrl Pts',(-7.7714817663724,-1.36196031891213,
-3.77093381386658));
#148926=CARTESIAN_POINT('Ctrl Pts',(-7.76730846475425,-1.3549908652122,
-3.7954242649276));
#148927=CARTESIAN_POINT('Ctrl Pts',(-7.76713645006289,-1.3498599671305,
-3.80743986883124));
#148928=CARTESIAN_POINT('Ctrl Pts',(-7.77013516735406,-1.33873894479117,
-3.82655023058136));
#148929=CARTESIAN_POINT('Ctrl Pts',(-7.77237566726015,-1.33344492719833,
-3.83397628000856));
#148930=CARTESIAN_POINT('Ctrl Pts',(-7.77551682988422,-1.32768940203627,
-3.84061312108624));
#148931=CARTESIAN_POINT('Ctrl Pts',(-7.95223773319059,-1.00000000030882,
-4.2144887031835));
#148932=CARTESIAN_POINT('Ctrl Pts',(-7.8940607583389,-1.10901473835463,
-4.0914617970675));
#148933=CARTESIAN_POINT('Ctrl Pts',(-7.83519367612302,-1.21834403204217,
-3.96670202196032));
#148934=CARTESIAN_POINT('Ctrl Pts',(-7.77551682979917,-1.32768940207849,
-3.84061312116309));
#148935=CARTESIAN_POINT('',(-7.488781739,-1.32768940200002,-4.373456205));
#148936=CARTESIAN_POINT('Ctrl Pts',(-7.4887817391053,-1.3276894020377,-4.3734562055302));
#148937=CARTESIAN_POINT('Ctrl Pts',(-7.62688820723029,-1.21834383456909,
-4.3537988749128));
#148938=CARTESIAN_POINT('Ctrl Pts',(-7.76343893103024,-1.1090146543582,
-4.33419800434109));
#148939=CARTESIAN_POINT('Ctrl Pts',(-7.89816331292909,-0.999999999917443,
-4.3149758149713));
#148940=CARTESIAN_POINT('',(-7.399944978,-1.32768940200002,-4.522143898));
#148941=CARTESIAN_POINT('Ctrl Pts',(-7.48878173912938,-1.32768940209639,
-4.37345620537261));
#148942=CARTESIAN_POINT('Ctrl Pts',(-7.48303932181701,-1.33223595148123,
-4.37427355014363));
#148943=CARTESIAN_POINT('Ctrl Pts',(-7.47718662272123,-1.33650155469588,
-4.37583248146923));
#148944=CARTESIAN_POINT('Ctrl Pts',(-7.46094870251595,-1.34730670096865,
-4.38217094653701));
#148945=CARTESIAN_POINT('Ctrl Pts',(-7.45074458329346,-1.35293307618431,
-4.38842924161994));
#148946=CARTESIAN_POINT('Ctrl Pts',(-7.43600613470365,-1.35917045589565,
-4.40111253383243));
#148947=CARTESIAN_POINT('Ctrl Pts',(-7.43100504926067,-1.36087898833917,
-4.40620320980585));
#148948=CARTESIAN_POINT('Ctrl Pts',(-7.42174966047234,-1.3631727422014,
-4.41729191322548));
#148949=CARTESIAN_POINT('Ctrl Pts',(-7.41752505749903,-1.36375173576924,
-4.42325214266577));
#148950=CARTESIAN_POINT('Ctrl Pts',(-7.41377690379883,-1.36375173576648,
-4.42952549528285));
#148951=CARTESIAN_POINT('Ctrl Pts',(-7.40718426765269,-1.36375173576163,
-4.44055970959978));
#148952=CARTESIAN_POINT('Ctrl Pts',(-7.4021721641394,-1.36196031879803,
-4.45238339858914));
#148953=CARTESIAN_POINT('Ctrl Pts',(-7.39582035590394,-1.3549908650908,
-4.47640116642154));
#148954=CARTESIAN_POINT('Ctrl Pts',(-7.39457196326603,-1.34985996700553,
-4.48835297975807));
#148955=CARTESIAN_POINT('Ctrl Pts',(-7.39584556898713,-1.33873894466816,
-4.50765521174129));
#148956=CARTESIAN_POINT('Ctrl Pts',(-7.39741138335892,-1.3334449270826,
-4.51525220292776));
#148957=CARTESIAN_POINT('Ctrl Pts',(-7.39994497873345,-1.32768940192929,
-4.52214389767129));
#148958=CARTESIAN_POINT('Ctrl Pts',(-7.54244050677706,-1.00000000021305,
-4.91035550626367));
#148959=CARTESIAN_POINT('Ctrl Pts',(-7.49552578212922,-1.10901473827983,
-4.78260892651342));
#148960=CARTESIAN_POINT('Ctrl Pts',(-7.4480790614658,-1.21834403198914,
-4.65307459304682));
#148961=CARTESIAN_POINT('Ctrl Pts',(-7.39994497847541,-1.32768940204821,
-4.52214389786548));
#148962=CARTESIAN_POINT('',(-7.066600514,-1.32768940200002,-5.027139175));
#148963=CARTESIAN_POINT('Ctrl Pts',(-7.06660051407375,-1.32768940204712,
-5.02713917571187));
#148964=CARTESIAN_POINT('Ctrl Pts',(-7.20591307568901,-1.21834383453907,
-5.01994074814747));
#148965=CARTESIAN_POINT('Ctrl Pts',(-7.34367109490997,-1.10901465428964,
-5.01265909749143));
#148966=CARTESIAN_POINT('Ctrl Pts',(-7.47957617982504,-0.999999999810883,
-5.00559089155299));
#148967=CARTESIAN_POINT('',(-6.964793122,-1.32768940200002,-5.167265029));
#148968=CARTESIAN_POINT('Ctrl Pts',(-7.06660051416281,-1.32768940218437,
-5.0271391753499));
#148969=CARTESIAN_POINT('Ctrl Pts',(-7.06080794801292,-1.33223595147841,
-5.0274384834299));
#148970=CARTESIAN_POINT('Ctrl Pts',(-7.05483906874339,-1.33650155461116,
-5.02846650704578));
#148971=CARTESIAN_POINT('Ctrl Pts',(-7.0380983421117,-1.34730670081974,
-5.0333238993322));
#148972=CARTESIAN_POINT('Ctrl Pts',(-7.02737431242565,-1.35293307604024,
-5.03864231015989));
#148973=CARTESIAN_POINT('Ctrl Pts',(-7.01155827494507,-1.35917045575939,
-5.04995339881579));
#148974=CARTESIAN_POINT('Ctrl Pts',(-7.00612099772445,-1.36087898820574,
-5.05457528737984));
#148975=CARTESIAN_POINT('Ctrl Pts',(-6.99590888469632,-1.36317274207366,
-5.06478970428212));
#148976=CARTESIAN_POINT('Ctrl Pts',(-6.99116701788302,-1.36375173564436,
-5.07034724909892));
#148977=CARTESIAN_POINT('Ctrl Pts',(-6.9868716141528,-1.36375173564439,
-5.07625936513457));
#148978=CARTESIAN_POINT('Ctrl Pts',(-6.9793164186734,-1.36375173564445,
-5.08665819959847));
#148979=CARTESIAN_POINT('Ctrl Pts',(-6.97326462510242,-1.36196031868577,
-5.09798500839567));
#148980=CARTESIAN_POINT('Ctrl Pts',(-6.96478545126267,-1.35499086498787,
-5.121336716054));
#148981=CARTESIAN_POINT('Ctrl Pts',(-6.96247073199496,-1.34985996690716,
-5.13312850985035));
#148982=CARTESIAN_POINT('Ctrl Pts',(-6.96200897181234,-1.33873894460026,
-5.15246720181947));
#148983=CARTESIAN_POINT('Ctrl Pts',(-6.9628874936231,-1.3334449270472,-5.16017396823524));
#148984=CARTESIAN_POINT('Ctrl Pts',(-6.96479312271032,-1.32768940192986,
-5.16726502875217));
#148985=CARTESIAN_POINT('Ctrl Pts',(-7.07191598493006,-1.0000000000433,
-5.56668701305467));
#148986=CARTESIAN_POINT('Ctrl Pts',(-7.03664124030446,-1.1090147382238,
-5.43524929978372));
#148987=CARTESIAN_POINT('Ctrl Pts',(-7.00099689432893,-1.21834403204728,
-5.30198334200608));
#148988=CARTESIAN_POINT('Ctrl Pts',(-6.96479312204206,-1.32768940221948,
-5.16726502916683));
#148989=CARTESIAN_POINT('',(-6.587523177,-1.32768940200002,-5.640346578));
#148990=CARTESIAN_POINT('Ctrl Pts',(-6.58752317677662,-1.32768940171009,
-5.64034657789402));
#148991=CARTESIAN_POINT('Ctrl Pts',(-6.72692016891382,-1.2183438343021,
-5.64566501082948));
#148992=CARTESIAN_POINT('Ctrl Pts',(-6.86477633685045,-1.10901465415312,
-5.6507612075996));
#148993=CARTESIAN_POINT('Ctrl Pts',(-7.00076789681646,-0.999999999774391,
-5.65590389407081));
#148994=CARTESIAN_POINT('',(-6.473564847,-1.32768940200002,-5.770782381));
#148995=CARTESIAN_POINT('Ctrl Pts',(-6.58752317690415,-1.32768940185457,
-5.64034657752293));
#148996=CARTESIAN_POINT('Ctrl Pts',(-6.58172709993427,-1.33223595135912,
-5.64012543898217));
#148997=CARTESIAN_POINT('Ctrl Pts',(-6.57569009804838,-1.33650155468271,
-5.64061427785487));
#148998=CARTESIAN_POINT('Ctrl Pts',(-6.55858135111833,-1.34730670105206,
-5.64395148859084));
#148999=CARTESIAN_POINT('Ctrl Pts',(-6.54742375455179,-1.35293307627263,
-5.64828719444978));
#149000=CARTESIAN_POINT('Ctrl Pts',(-6.53065746961771,-1.359170455992,-5.65813500931786));
#149001=CARTESIAN_POINT('Ctrl Pts',(-6.52482777837963,-1.36087898843846,
-5.66225089774472));
#149002=CARTESIAN_POINT('Ctrl Pts',(-6.51374116304362,-1.36317274230659,
-5.67150878765279));
#149003=CARTESIAN_POINT('Ctrl Pts',(-6.50852021111509,-1.36375173587738,
-5.67661890176379));
#149004=CARTESIAN_POINT('Ctrl Pts',(-6.50371214142148,-1.36375173587751,
-5.6821221803364));
#149005=CARTESIAN_POINT('Ctrl Pts',(-6.49525521660246,-1.36375173587773,
-5.69180190964827));
#149006=CARTESIAN_POINT('Ctrl Pts',(-6.48821245845978,-1.36196031891918,
-5.70254064144979));
#149007=CARTESIAN_POINT('Ctrl Pts',(-6.47767418834347,-1.35499086522148,
-5.72503827471508));
#149008=CARTESIAN_POINT('Ctrl Pts',(-6.47431177920769,-1.34985996714086,
-5.73657510838083));
#149009=CARTESIAN_POINT('Ctrl Pts',(-6.47211837095175,-1.33873894483526,
-5.7557945565959));
#149010=CARTESIAN_POINT('Ctrl Pts',(-6.47230252687583,-1.33344492728374,
-5.76354904792197));
#149011=CARTESIAN_POINT('Ctrl Pts',(-6.47356484669523,-1.32768940216811,
-5.77078238118694));
#149012=CARTESIAN_POINT('Ctrl Pts',(-6.54445255389812,-0.999999999960802,
-6.17819882898586));
#149013=CARTESIAN_POINT('Ctrl Pts',(-6.52110180080846,-1.10901473814172,
-6.04412824156698));
#149014=CARTESIAN_POINT('Ctrl Pts',(-6.49754681684949,-1.21834403196543,
-5.90820363880618));
#149015=CARTESIAN_POINT('Ctrl Pts',(-6.47356484676908,-1.32768940213768,
-5.77078238114983));
#149016=CARTESIAN_POINT('',(-6.055406976,-1.32768940200002,-6.208141225));
#149017=CARTESIAN_POINT('Ctrl Pts',(-6.05540697605073,-1.32768940208598,
-6.20814122513386));
#149018=CARTESIAN_POINT('Ctrl Pts',(-6.19376605621082,-1.21834383468118,
-6.22593369766438));
#149019=CARTESIAN_POINT('Ctrl Pts',(-6.33061043617275,-1.10901465453519,
-6.24336671027083));
#149020=CARTESIAN_POINT('Ctrl Pts',(-6.46559354722401,-1.00000000015905,
-6.26067888325481));
#149021=CARTESIAN_POINT('',(-5.930215234,-1.32768940200002,-6.327836787));
#149022=CARTESIAN_POINT('Ctrl Pts',(-6.05540697612598,-1.3276894021538,
-6.20814122496572));
#149023=CARTESIAN_POINT('Ctrl Pts',(-6.04965405520632,-1.33223595161668,
-6.20740142034681));
#149024=CARTESIAN_POINT('Ctrl Pts',(-6.04359753738464,-1.33650155490257,
-6.20734713862694));
#149025=CARTESIAN_POINT('Ctrl Pts',(-6.02625852002746,-1.34730670124085,
-6.20913729847659));
#149026=CARTESIAN_POINT('Ctrl Pts',(-6.01475719098768,-1.35293307646214,
-6.21245539081279));
#149027=CARTESIAN_POINT('Ctrl Pts',(-5.99717565086843,-1.35917045618278,
-6.22076064307862));
#149028=CARTESIAN_POINT('Ctrl Pts',(-5.99100048285914,-1.36087898862972,
-6.22433739265494));
#149029=CARTESIAN_POINT('Ctrl Pts',(-5.97912862812349,-1.3631727424988,
-6.23256421648309));
#149030=CARTESIAN_POINT('Ctrl Pts',(-5.97347062711499,-1.36375173607006,
-6.23718575625433));
#149031=CARTESIAN_POINT('Ctrl Pts',(-5.96818860320827,-1.36375173607065,
-6.24223588820087));
#149032=CARTESIAN_POINT('Ctrl Pts',(-5.95889803923611,-1.36375173607169,
-6.25111857687207));
#149033=CARTESIAN_POINT('Ctrl Pts',(-5.95092102066962,-1.36196031911391,
-6.2611827697239));
#149034=CARTESIAN_POINT('Ctrl Pts',(-5.93840850223206,-1.35499086541765,
-6.28264519088179));
#149035=CARTESIAN_POINT('Ctrl Pts',(-5.93402547536983,-1.34985996733774,
-6.29383417661586));
#149036=CARTESIAN_POINT('Ctrl Pts',(-5.93011807903562,-1.33873894492255,
-6.31277963757132));
#149037=CARTESIAN_POINT('Ctrl Pts',(-5.92960638637303,-1.33344492723105,
-6.32051941938347));
#149038=CARTESIAN_POINT('Ctrl Pts',(-5.93021523353628,-1.32768940195741,
-6.32783678700507));
#149039=CARTESIAN_POINT('Ctrl Pts',(-5.96429703904196,-0.999999999791271,
-6.73996742082874));
#149040=CARTESIAN_POINT('Ctrl Pts',(-5.95305828402978,-1.10901473792973,
-6.60434341685274));
#149041=CARTESIAN_POINT('Ctrl Pts',(-5.94178231297559,-1.21834403171087,
-6.46685455414235));
#149042=CARTESIAN_POINT('Ctrl Pts',(-5.93021523383119,-1.32768940184066,
-6.3278367868887));
#149043=CARTESIAN_POINT('',(-5.474536198,-1.32768940200002,-6.725951571));
#149044=CARTESIAN_POINT('Ctrl Pts',(-5.47453619793898,-1.32768940194877,
-6.72595157108985));
#149045=CARTESIAN_POINT('Ctrl Pts',(-5.61074338033991,-1.21834383447162,
-6.75607482866063));
#149046=CARTESIAN_POINT('Ctrl Pts',(-5.74547418201546,-1.10901465425249,
-6.78570429670652));
#149047=CARTESIAN_POINT('Ctrl Pts',(-5.87836203967683,-0.999999999803766,
-6.81504656873443));
#149048=CARTESIAN_POINT('',(-5.339119014,-1.32768940200002,-6.833943172));
#149049=CARTESIAN_POINT('Ctrl Pts',(-5.47453619794346,-1.3276894019521,
-6.72595157108191));
#149050=CARTESIAN_POINT('Ctrl Pts',(-5.46887275217696,-1.33223595140147,
-6.72469905685192));
#149051=CARTESIAN_POINT('Ctrl Pts',(-5.46284548190358,-1.33650155467468,
-6.72410209158784));
#149052=CARTESIAN_POINT('Ctrl Pts',(-5.44541579765377,-1.34730670099757,
-6.72433078725383));
#149053=CARTESIAN_POINT('Ctrl Pts',(-5.43366333807953,-1.35293307621405,
-6.72660455074311));
#149054=CARTESIAN_POINT('Ctrl Pts',(-5.41540809900002,-1.35917045592673,
-6.73330037140443));
#149055=CARTESIAN_POINT('Ctrl Pts',(-5.40893717304231,-1.36087898837075,
-6.73630918424744));
#149056=CARTESIAN_POINT('Ctrl Pts',(-5.39637566410319,-1.36317274223397,
-6.74343870445049));
#149057=CARTESIAN_POINT('Ctrl Pts',(-5.39032616891343,-1.36375173580231,
-6.74753445996235));
#149058=CARTESIAN_POINT('Ctrl Pts',(-5.38461271854601,-1.36375173580003,
-6.75209078459071));
#149059=CARTESIAN_POINT('Ctrl Pts',(-5.37456331758125,-1.36375173579604,
-6.76010491443722));
#149060=CARTESIAN_POINT('Ctrl Pts',(-5.36571626485716,-1.36196031883327,
-6.76941353737757));
#149061=CARTESIAN_POINT('Ctrl Pts',(-5.35133024154627,-1.35499086512763,
-6.78966794363456));
#149062=CARTESIAN_POINT('Ctrl Pts',(-5.34596188651656,-1.34985996704314,
-6.80041899430357));
#149063=CARTESIAN_POINT('Ctrl Pts',(-5.340371962258,-1.33873894475413,-6.81893792987469));
#149064=CARTESIAN_POINT('Ctrl Pts',(-5.33916854083174,-1.33344492722887,
-6.82660068560841));
#149065=CARTESIAN_POINT('Ctrl Pts',(-5.33911901311749,-1.32768940214345,
-6.83394317210648));
#149066=CARTESIAN_POINT('Ctrl Pts',(-5.33612051055408,-1.00000000012717,
-7.2474697580987));
#149067=CARTESIAN_POINT('Ctrl Pts',(-5.33708424139336,-1.10901473818033,
-7.11138430241067));
#149068=CARTESIAN_POINT('Ctrl Pts',(-5.33817807065952,-1.21834403187569,
-6.97343815934645));
#149069=CARTESIAN_POINT('Ctrl Pts',(-5.33911901369835,-1.32768940192049,
-6.83394317193562));
#149070=CARTESIAN_POINT('',(-4.84958767583258,-1.32768940194837,-7.18960850739357));
#149071=CARTESIAN_POINT('Ctrl Pts',(-4.84958767551919,-1.32768940181776,
-7.18960850804234));
#149072=CARTESIAN_POINT('Ctrl Pts',(-4.9825462995355,-1.21834383449911,
-7.2318200159394));
#149073=CARTESIAN_POINT('Ctrl Pts',(-5.11407874926016,-1.10901465444024,
-7.27340738041884));
#149074=CARTESIAN_POINT('Ctrl Pts',(-5.24380141818337,-1.00000000015115,
-7.31454350482226));
#149075=CARTESIAN_POINT('',(-4.705035349,-1.32768940200002,-7.285026664));
#149076=CARTESIAN_POINT('Ctrl Pts',(-4.84958767607711,-1.32768940218148,
-7.18960850722729));
#149077=CARTESIAN_POINT('Ctrl Pts',(-4.84405930425442,-1.33223595156484,
-7.18785336792303));
#149078=CARTESIAN_POINT('Ctrl Pts',(-4.83810980963134,-1.33650155477901,
-7.18671852554355));
#149079=CARTESIAN_POINT('Ctrl Pts',(-4.82072979213365,-1.34730670106102,
-7.1853839156919));
#149080=CARTESIAN_POINT('Ctrl Pts',(-4.80882082591909,-1.35293307628648,
-7.18659504331653));
#149081=CARTESIAN_POINT('Ctrl Pts',(-4.79003886832667,-1.35917045601382,
-7.19162752154787));
#149082=CARTESIAN_POINT('Ctrl Pts',(-4.78332428450955,-1.36087898846318,
-7.19404417246096));
#149083=CARTESIAN_POINT('Ctrl Pts',(-4.77017425924561,-1.36317274233714,
-7.20001898632597));
#149084=CARTESIAN_POINT('Ctrl Pts',(-4.76378197684949,-1.36375173591085,
-7.20355598095978));
#149085=CARTESIAN_POINT('Ctrl Pts',(-4.75768310136027,-1.36375173591383,
-7.20758181342033));
#149086=CARTESIAN_POINT('Ctrl Pts',(-4.74695577526566,-1.36375173591907,
-7.2146628593743));
#149087=CARTESIAN_POINT('Ctrl Pts',(-4.73730991964321,-1.36196031896553,
-7.22314096483993));
#149088=CARTESIAN_POINT('Ctrl Pts',(-4.72116621924342,-1.35499086527729,
-7.24202427961917));
#149089=CARTESIAN_POINT('Ctrl Pts',(-4.71485575887476,-1.3498599672013,
-7.25225083408193));
#149090=CARTESIAN_POINT('Ctrl Pts',(-4.70762831330155,-1.33873894475924,
-7.2701941411816));
#149091=CARTESIAN_POINT('Ctrl Pts',(-4.70574285233601,-1.33344492702836,
-7.27771817531576));
#149092=CARTESIAN_POINT('Ctrl Pts',(-4.70503534864306,-1.32768940170969,
-7.28502666373681));
#149093=CARTESIAN_POINT('Ctrl Pts',(-4.66498067879555,-0.999999999952127,
-7.69661972994159));
#149094=CARTESIAN_POINT('Ctrl Pts',(-4.67813913625211,-1.10901473800108,
-7.56116850237982));
#149095=CARTESIAN_POINT('Ctrl Pts',(-4.6915939591275,-1.21834403169194,
-7.42387573995099));
#149096=CARTESIAN_POINT('Ctrl Pts',(-4.70503534858687,-1.32768940173078,
-7.28502666374798));
#149097=CARTESIAN_POINT('',(-4.185593123,-1.32768940200002,-7.595378945));
#149098=CARTESIAN_POINT('Ctrl Pts',(-4.18559312299155,-1.32768940217896,
-7.59537894538274));
#149099=CARTESIAN_POINT('Ctrl Pts',(-4.31423268431485,-1.21834383483831,
-7.64933884133742));
#149100=CARTESIAN_POINT('Ctrl Pts',(-4.44150776048922,-1.10901465475701,
-7.70254926521416));
#149101=CARTESIAN_POINT('Ctrl Pts',(-4.56702079035568,-1.00000000044527,
-7.75514803807409));
#149102=CARTESIAN_POINT('',(-4.033069504,-1.32768940200002,-7.677455405));
#149103=CARTESIAN_POINT('Ctrl Pts',(-4.18559312312532,-1.32768940225632,
-7.5953789452207));
#149104=CARTESIAN_POINT('Ctrl Pts',(-4.18024433645438,-1.33223595154869,
-7.5931353122223));
#149105=CARTESIAN_POINT('Ctrl Pts',(-4.17442051933056,-1.33650155468029,
-7.59147172983892));
#149106=CARTESIAN_POINT('Ctrl Pts',(-4.1572301022881,-1.3473067008919,-7.58858455999571));
#149107=CARTESIAN_POINT('Ctrl Pts',(-4.14526051342689,-1.35293307611646,
-7.58872330047545));
#149108=CARTESIAN_POINT('Ctrl Pts',(-4.12610305860312,-1.35917045584226,
-7.59205191773052));
#149109=CARTESIAN_POINT('Ctrl Pts',(-4.11919887880873,-1.36087898829105,
-7.59385694926454));
#149110=CARTESIAN_POINT('Ctrl Pts',(-4.10556621349489,-1.36317274216386,
-7.59862895110864));
#149111=CARTESIAN_POINT('Ctrl Pts',(-4.09888261079392,-1.36375173573699,
-7.60157870706549));
#149112=CARTESIAN_POINT('Ctrl Pts',(-4.09244741474498,-1.36375173573942,
-7.60504163372406));
#149113=CARTESIAN_POINT('Ctrl Pts',(-4.0811285336459,-1.36375173574368,
-7.61113258337114));
#149114=CARTESIAN_POINT('Ctrl Pts',(-4.07076153788779,-1.36196031878918,
-7.61871191064466));
#149115=CARTESIAN_POINT('Ctrl Pts',(-4.0529901399933,-1.35499086509917,
-7.63607209660278));
#149116=CARTESIAN_POINT('Ctrl Pts',(-4.04578838240849,-1.34985996702232,
-7.64569181665736));
#149117=CARTESIAN_POINT('Ctrl Pts',(-4.03698160687458,-1.33873894472513,
-7.66291502582497));
#149118=CARTESIAN_POINT('Ctrl Pts',(-4.03442928704494,-1.33344492717922,
-7.67023975875926));
#149119=CARTESIAN_POINT('Ctrl Pts',(-4.03306950367077,-1.32768940206933,
-7.67745540499324));
#149120=CARTESIAN_POINT('Ctrl Pts',(-3.95628116425374,-0.99999999991297,
-8.08380104597694));
#149121=CARTESIAN_POINT('Ctrl Pts',(-3.98152840407528,-1.10901473807425,
-7.95007462013823));
#149122=CARTESIAN_POINT('Ctrl Pts',(-4.00723589014992,-1.21834403187787,
-7.81454063889854));
#149123=CARTESIAN_POINT('Ctrl Pts',(-4.03306950377905,-1.32768940202923,
-7.67745540498166));
#149124=CARTESIAN_POINT('',(-3.48789863553934,-1.3276894017749,-7.93999585849295));
#149125=CARTESIAN_POINT('Ctrl Pts',(-3.48789863503968,-1.32768940145685,
-7.93999585890387));
#149126=CARTESIAN_POINT('Ctrl Pts',(-3.61118340371515,-1.21834383408035,
-8.00526968952849));
#149127=CARTESIAN_POINT('Ctrl Pts',(-3.7331763624119,-1.10901465396194,
-8.06967475372052));
#149128=CARTESIAN_POINT('Ctrl Pts',(-3.85346919624949,-0.999999999613144,
-8.13331268060684));
#149129=CARTESIAN_POINT('',(-3.328631754,-1.32768940200002,-8.00806979));
#149130=CARTESIAN_POINT('Ctrl Pts',(-3.48789863549781,-1.32768940169677,
-7.93999585844058));
#149131=CARTESIAN_POINT('Ctrl Pts',(-3.48277249902713,-1.3322359511742,
-7.93728179597329));
#149132=CARTESIAN_POINT('Ctrl Pts',(-3.47712124905877,-1.3365015544728,
-7.93510286764403));
#149133=CARTESIAN_POINT('Ctrl Pts',(-3.46025883926027,-1.34730670081656,
-7.93068638354844));
#149134=CARTESIAN_POINT('Ctrl Pts',(-3.44832499984238,-1.35293307603251,
-7.92975161983458));
#149135=CARTESIAN_POINT('Ctrl Pts',(-3.42894629234947,-1.35917045574423,
-7.93134957605619));
#149136=CARTESIAN_POINT('Ctrl Pts',(-3.42190810497447,-1.36087898818788,
-7.93252845516265));
#149137=CARTESIAN_POINT('Ctrl Pts',(-3.40790256181816,-1.36317274205036,
-7.93605922364059));
#149138=CARTESIAN_POINT('Ctrl Pts',(-3.40098145125301,-1.36375173561834,
-7.93839799122359));
#149139=CARTESIAN_POINT('Ctrl Pts',(-3.39426174706129,-1.36375173561571,
-7.94127013063417));
#149140=CARTESIAN_POINT('Ctrl Pts',(-3.38244244393535,-1.36375173561109,
-7.94632194323558));
#149141=CARTESIAN_POINT('Ctrl Pts',(-3.37143777699998,-1.36196031864774,
-7.95294146803597));
#149142=CARTESIAN_POINT('Ctrl Pts',(-3.35218176646764,-1.35499086494101,
-7.96863875117293));
#149143=CARTESIAN_POINT('Ctrl Pts',(-3.34414669599052,-1.34985996685599,
-7.97757418449405));
#149144=CARTESIAN_POINT('Ctrl Pts',(-3.33383149747034,-1.33873894463069,
-7.9939386246935));
#149145=CARTESIAN_POINT('Ctrl Pts',(-3.33063286857535,-1.33344492718698,
-8.00100508209111));
#149146=CARTESIAN_POINT('Ctrl Pts',(-3.32863175374708,-1.32768940219364,
-8.0080697900861));
#149147=CARTESIAN_POINT('Ctrl Pts',(-3.21572799953932,-1.00000000015765,
-8.40589634900059));
#149148=CARTESIAN_POINT('Ctrl Pts',(-3.25286074564109,-1.10901473828873,
-8.27497141166348));
#149149=CARTESIAN_POINT('Ctrl Pts',(-3.29061391319593,-1.21834403206224,
-8.14228745177371));
#149150=CARTESIAN_POINT('Ctrl Pts',(-3.32863175377033,-1.32768940218507,
-8.00806979008571));
#149151=CARTESIAN_POINT('',(-2.76212164,-1.32768940200002,-8.220684592));
#149152=CARTESIAN_POINT('Ctrl Pts',(-2.76212164018735,-1.3276894021635,
-8.22068459194698));
#149153=CARTESIAN_POINT('Ctrl Pts',(-2.87905899951265,-1.21834383472095,
-8.29674681085365));
#149154=CARTESIAN_POINT('Ctrl Pts',(-2.99478762493088,-1.10901465453746,
-8.37182796377343));
#149155=CARTESIAN_POINT('Ctrl Pts',(-3.10889173535242,-1.00000000012429,
-8.44599266964046));
#149156=CARTESIAN_POINT('',(-2.59739382,-1.32768940200002,-8.274207905));
#149157=CARTESIAN_POINT('Ctrl Pts',(-2.76212164024878,-1.32768940219308,
-8.22068459189514));
#149158=CARTESIAN_POINT('Ctrl Pts',(-2.7572594268428,-1.33223595159149,
-8.21752195217761));
#149159=CARTESIAN_POINT('Ctrl Pts',(-2.75182624485655,-1.33650155481903,
-8.21484522147966));
#149160=CARTESIAN_POINT('Ctrl Pts',(-2.73542760884484,-1.34730670110943,
-8.20893498211433));
#149161=CARTESIAN_POINT('Ctrl Pts',(-2.72362560313124,-1.35293307633198,
-8.20693424036015));
#149162=CARTESIAN_POINT('Ctrl Pts',(-2.7041816689267,-1.3591704560546,-8.20678866972344));
#149163=CARTESIAN_POINT('Ctrl Pts',(-2.69706614131622,-1.36087898850225,
-8.20733190475376));
#149164=CARTESIAN_POINT('Ctrl Pts',(-2.68280048471138,-1.36317274237276,
-8.20959301218038));
#149165=CARTESIAN_POINT('Ctrl Pts',(-2.67569759099158,-1.36375173594474,
-8.21130196100191));
#149166=CARTESIAN_POINT('Ctrl Pts',(-2.66874748175985,-1.36375173594603,
-8.21356018838122));
#149167=CARTESIAN_POINT('Ctrl Pts',(-2.65652291868143,-1.36375173594831,
-8.21753218970138));
#149168=CARTESIAN_POINT('Ctrl Pts',(-2.64496918366811,-1.36196031899179,
-8.2231386154978));
#149169=CARTESIAN_POINT('Ctrl Pts',(-2.62438359855294,-1.35499086529792,
-8.23704661050358));
#149170=CARTESIAN_POINT('Ctrl Pts',(-2.61557990883475,-1.34985996721919,
-8.24522581422892));
#149171=CARTESIAN_POINT('Ctrl Pts',(-2.60383933905131,-1.33873894490893,
-8.26059972886249));
#149172=CARTESIAN_POINT('Ctrl Pts',(-2.60002015447877,-1.33344492734899,
-8.26735101603765));
#149173=CARTESIAN_POINT('Ctrl Pts',(-2.59739381999828,-1.32768940222356,
-8.27420790518698));
#149174=CARTESIAN_POINT('Ctrl Pts',(-2.44928368525819,-0.999999999982717,
-8.66031231708415));
#149175=CARTESIAN_POINT('Ctrl Pts',(-2.49800296686794,-1.10901473814177,
-8.53324299868092));
#149176=CARTESIAN_POINT('Ctrl Pts',(-2.54749784986341,-1.21834403194323,
-8.40447735317844));
#149177=CARTESIAN_POINT('Ctrl Pts',(-2.59739382035255,-1.32768940209275,
-8.27420790521288));
#149178=CARTESIAN_POINT('',(-2.01410566465369,-1.3276894019719,-8.43518520740466));
#149179=CARTESIAN_POINT('Ctrl Pts',(-2.01410566413619,-1.32768940192452,
-8.43518520800257));
#149180=CARTESIAN_POINT('Ctrl Pts',(-2.12375410335395,-1.21834383447808,
-8.52142340685227));
#149181=CARTESIAN_POINT('Ctrl Pts',(-2.23228661674758,-1.10901465429013,
-8.606576139125));
#149182=CARTESIAN_POINT('Ctrl Pts',(-2.33928330464295,-0.999999999872264,
-8.69067049328867));
#149183=CARTESIAN_POINT('',(-1.845243197,-1.32768940200002,-8.473726964));
#149184=CARTESIAN_POINT('Ctrl Pts',(-2.01410566493824,-1.32768940228522,
-8.43518520744022));
#149185=CARTESIAN_POINT('Ctrl Pts',(-2.00954652218688,-1.33223595171976,
-8.43159945409989));
#149186=CARTESIAN_POINT('Ctrl Pts',(-2.00437515284886,-1.33650155497982,
-8.42844647242926));
#149187=CARTESIAN_POINT('Ctrl Pts',(-1.98857232265248,-1.34730670129488,
-8.42109006353586));
#149188=CARTESIAN_POINT('Ctrl Pts',(-1.97699717345128,-1.35293307651467,
-8.41803945254678));
#149189=CARTESIAN_POINT('Ctrl Pts',(-1.9576445636601,-1.3591704562329,-8.41615152711445));
#149190=CARTESIAN_POINT('Ctrl Pts',(-1.95050898585903,-1.36087898867897,
-8.41605474426427));
#149191=CARTESIAN_POINT('Ctrl Pts',(-1.9360980744867,-1.3631727425463,-8.41702798554097));
#149192=CARTESIAN_POINT('Ctrl Pts',(-1.92887058593776,-1.36375173611669,
-8.41809335615413));
#149193=CARTESIAN_POINT('Ctrl Pts',(-1.92174602986137,-1.36375173611641,
-8.41971948958691));
#149194=CARTESIAN_POINT('Ctrl Pts',(-1.90921463182691,-1.36375173611594,
-8.422579699414));
#149195=CARTESIAN_POINT('Ctrl Pts',(-1.89720485262118,-1.36196031915664,
-8.42712788656892));
#149196=CARTESIAN_POINT('Ctrl Pts',(-1.87545543596194,-1.3549908654575,
-8.43913461445685));
#149197=CARTESIAN_POINT('Ctrl Pts',(-1.8659540091429,-1.34985996737619,
-8.44649173445249));
#149198=CARTESIAN_POINT('Ctrl Pts',(-1.85288259622497,-1.3387389449445,
-8.46075134181751));
#149199=CARTESIAN_POINT('Ctrl Pts',(-1.8484736057682,-1.33344492723397,
-8.46713310140139));
#149200=CARTESIAN_POINT('Ctrl Pts',(-1.84524319731389,-1.32768940193907,
-8.47372696410058));
#149201=CARTESIAN_POINT('Ctrl Pts',(-1.66311917770952,-0.999999999928504,
-8.84500054279377));
#149202=CARTESIAN_POINT('Ctrl Pts',(-1.7230327356253,-1.10901473804792,
-8.72280993090161));
#149203=CARTESIAN_POINT('Ctrl Pts',(-1.78387083017168,-1.21834403180964,
-8.59899934519942));
#149204=CARTESIAN_POINT('Ctrl Pts',(-1.84524319736451,-1.32768940192018,
-8.47372696410889));
#149205=CARTESIAN_POINT('',(-1.249873295,-1.32768940200002,-8.581770672));
#149206=CARTESIAN_POINT('Ctrl Pts',(-1.24987329474725,-1.32768940183712,
-8.58177067208186));
#149207=CARTESIAN_POINT('Ctrl Pts',(-1.35134998891948,-1.21834383452832,
-8.67749051148482));
#149208=CARTESIAN_POINT('Ctrl Pts',(-1.45181255013311,-1.10901465447807,
-8.7720292232633));
#149209=CARTESIAN_POINT('Ctrl Pts',(-1.55084034091679,-1.00000000019697,
-8.86537614731828));
#149210=CARTESIAN_POINT('',(-1.078235761,-1.32768940200002,-8.605020555));
#149211=CARTESIAN_POINT('Ctrl Pts',(-1.24987329478272,-1.32768940185216,
-8.5817706720615));
#149212=CARTESIAN_POINT('Ctrl Pts',(-1.24565393021003,-1.33223595135743,
-8.57779067543879));
#149213=CARTESIAN_POINT('Ctrl Pts',(-1.24078601032253,-1.33650155468153,
-8.5741868287156));
#149214=CARTESIAN_POINT('Ctrl Pts',(-1.22570622100734,-1.34730670104963,
-8.56544347974055));
#149215=CARTESIAN_POINT('Ctrl Pts',(-1.21445112461428,-1.3529330762685,
-8.56136756123979));
#149216=CARTESIAN_POINT('Ctrl Pts',(-1.1953456550714,-1.3591704559851,-8.55775248147335));
#149217=CARTESIAN_POINT('Ctrl Pts',(-1.18824747855661,-1.36087898843055,
-8.55701645997984));
#149218=CARTESIAN_POINT('Ctrl Pts',(-1.17380734060151,-1.36317274229665,
-8.55669399913736));
#149219=CARTESIAN_POINT('Ctrl Pts',(-1.1665134487113,-1.36375173586643,
-8.55710721380306));
#149220=CARTESIAN_POINT('Ctrl Pts',(-1.1592718085262,-1.36375173586556,
-8.55808816061781));
#149221=CARTESIAN_POINT('Ctrl Pts',(-1.14653447098409,-1.36375173586404,
-8.55981355022169));
#149222=CARTESIAN_POINT('Ctrl Pts',(-1.1341653432657,-1.36196031890374,
-8.5632668794042));
#149223=CARTESIAN_POINT('Ctrl Pts',(-1.11142720857434,-1.35499086520275,
-8.5732756690572));
#149224=CARTESIAN_POINT('Ctrl Pts',(-1.10130454455473,-1.34985996712054,
-8.57975147011711));
#149225=CARTESIAN_POINT('Ctrl Pts',(-1.08700753210465,-1.33873894480506,
-8.59278195993714));
#149226=CARTESIAN_POINT('Ctrl Pts',(-1.0820442345278,-1.33344492724318,
-8.59874280941312));
#149227=CARTESIAN_POINT('Ctrl Pts',(-1.07823576149093,-1.32768940211611,
-8.60502055540426));
#149228=CARTESIAN_POINT('Ctrl Pts',(-0.863564212198985,-0.999999999788605,
-8.95847402492269));
#149229=CARTESIAN_POINT('Ctrl Pts',(-0.934189657823289,-1.10901473803966,
-8.84214592630361));
#149230=CARTESIAN_POINT('Ctrl Pts',(-1.00588113150084,-1.2183440319341,
-8.72428725023411));
#149231=CARTESIAN_POINT('Ctrl Pts',(-1.07823576132974,-1.32768940217741,
-8.60502055536268));
#149232=CARTESIAN_POINT('',(-0.475577681,-1.32768940200002,-8.659260764));
#149233=CARTESIAN_POINT('Ctrl Pts',(-0.475577680456156,-1.32768940202431,
-8.65926076450709));
#149234=CARTESIAN_POINT('Ctrl Pts',(-0.568065599076002,-1.21834383457737,
-8.76369156484591));
#149235=CARTESIAN_POINT('Ctrl Pts',(-0.659649342801167,-1.10901465438963,
-8.8668550862539));
#149236=CARTESIAN_POINT('Ctrl Pts',(-0.749910923085495,-0.999999999972134,
-8.96870300589438));
#149237=CARTESIAN_POINT('',(-0.302547006,-1.32768940200002,-8.667031581));
#149238=CARTESIAN_POINT('Ctrl Pts',(-0.475577681121855,-1.32768940229424,
-8.6592607642002));
#149239=CARTESIAN_POINT('Ctrl Pts',(-0.471732066689365,-1.33223595165812,
-8.65491856908753));
#149240=CARTESIAN_POINT('Ctrl Pts',(-0.467206790057779,-1.33650155485448,
-8.65089287353958));
#149241=CARTESIAN_POINT('Ctrl Pts',(-0.452971455449954,-1.34730670111979,
-8.64083298092142));
#149242=CARTESIAN_POINT('Ctrl Pts',(-0.442127031285838,-1.35293307634352,
-8.63576457180455));
#149243=CARTESIAN_POINT('Ctrl Pts',(-0.423422528000185,-1.35917045606808,
-8.6304514441951));
#149244=CARTESIAN_POINT('Ctrl Pts',(-0.416418903115635,-1.36087898851643,
-8.62908211006861));
#149245=CARTESIAN_POINT('Ctrl Pts',(-0.402065802077877,-1.36317274238836,
-8.62746654336825));
#149246=CARTESIAN_POINT('Ctrl Pts',(-0.394764232974746,-1.36375173596106,
-8.62722427512314));
#149247=CARTESIAN_POINT('Ctrl Pts',(-0.387463814108887,-1.36375173596304,
-8.62755213731119));
#149248=CARTESIAN_POINT('Ctrl Pts',(-0.374623090611251,-1.36375173596654,
-8.62812881486618));
#149249=CARTESIAN_POINT('Ctrl Pts',(-0.361994203322079,-1.36196031901124,
-8.63045948189725));
#149250=CARTESIAN_POINT('Ctrl Pts',(-0.338450424685215,-1.35499086531967,
-8.6383897484205));
#149251=CARTESIAN_POINT('Ctrl Pts',(-0.327788025201018,-1.34985996724206,
-8.64393209119935));
#149252=CARTESIAN_POINT('Ctrl Pts',(-0.312380524047814,-1.33873894481487,
-8.65562854990331));
#149253=CARTESIAN_POINT('Ctrl Pts',(-0.306902880703472,-1.33344492710504,
-8.66112049633992));
#149254=CARTESIAN_POINT('Ctrl Pts',(-0.302547006590512,-1.32768940181038,
-8.6670315812505));
#149255=CARTESIAN_POINT('Ctrl Pts',(-0.0570563368422518,-1.00000000016179,
-8.99981914104468));
#149256=CARTESIAN_POINT('Ctrl Pts',(-0.137825035508058,-1.10901473824052,
-8.89029016145374));
#149257=CARTESIAN_POINT('Ctrl Pts',(-0.21979267061258,-1.21834403196143,
-8.77933232408725));
#149258=CARTESIAN_POINT('Ctrl Pts',(-0.302547006027247,-1.32768940203058,
-8.66703158104983));
#149259=CARTESIAN_POINT('',(0.302547007,-1.32768940200002,-8.667031581));
#149260=CARTESIAN_POINT('Ctrl Pts',(0.302547007479098,-1.32768940183626,
-8.66703158119359));
#149261=CARTESIAN_POINT('Ctrl Pts',(0.219792522734841,-1.21834383445799,
-8.77933252688754));
#149262=CARTESIAN_POINT('Ctrl Pts',(0.137824974935765,-1.10901465433772,
-8.89029024572902));
#149263=CARTESIAN_POINT('Ctrl Pts',(0.0570563383027792,-0.999999999986948,
-8.99981914121027));
#149264=CARTESIAN_POINT('',(0.475577681,-1.32768940200002,-8.659260764));
#149265=CARTESIAN_POINT('Ctrl Pts',(0.302547006808484,-1.32768940209839,
-8.66703158095471));
#149266=CARTESIAN_POINT('Ctrl Pts',(0.305987908599573,-1.33223595155284,
-8.66236214793029));
#149267=CARTESIAN_POINT('Ctrl Pts',(0.310134107298286,-1.33650155483069,
-8.65794701589455));
#149268=CARTESIAN_POINT('Ctrl Pts',(0.323410372907643,-1.34730670115791,
-8.64665157582217));
#149269=CARTESIAN_POINT('Ctrl Pts',(0.333756811921418,-1.35293307637481,
-8.64063148394741));
#149270=CARTESIAN_POINT('Ctrl Pts',(0.351909751292211,-1.35917045608827,
-8.63366308668712));
#149271=CARTESIAN_POINT('Ctrl Pts',(0.358762435478143,-1.36087898853258,
-8.63167146500543));
#149272=CARTESIAN_POINT('Ctrl Pts',(0.372912936869227,-1.3631727423964,
-8.62877580004926));
#149273=CARTESIAN_POINT('Ctrl Pts',(0.380163395243691,-1.36375173596503,
-8.6278799994992));
#149274=CARTESIAN_POINT('Ctrl Pts',(0.38746381410889,-1.36375173596304,
-8.62755213731119));
#149275=CARTESIAN_POINT('Ctrl Pts',(0.400304537606769,-1.36375173595955,
-8.62697545975618));
#149276=CARTESIAN_POINT('Ctrl Pts',(0.413091504089368,-1.36196031899726,
-8.6281646994827));
#149277=CARTESIAN_POINT('Ctrl Pts',(0.437251366001841,-1.35499086529249,
-8.63395259304714));
#149278=CARTESIAN_POINT('Ctrl Pts',(0.448367653573957,-1.34985996720843,
-8.63851685386684));
#149279=CARTESIAN_POINT('Ctrl Pts',(0.46476159091214,-1.33873894491584,
-8.64878510818524));
#149280=CARTESIAN_POINT('Ctrl Pts',(0.470709476999128,-1.33344492738548,
-8.65376393332434));
#149281=CARTESIAN_POINT('Ctrl Pts',(0.475577681121842,-1.32768940229425,
-8.65926076420018));
#149282=CARTESIAN_POINT('Ctrl Pts',(0.749910923381227,-1.00000000008659,
-8.9687030057548));
#149283=CARTESIAN_POINT('Ctrl Pts',(0.659649273775833,-1.10901473822727,
-8.86685500789799));
#149284=CARTESIAN_POINT('Ctrl Pts',(0.56806543247335,-1.21834403201054,
-8.76369137626223));
#149285=CARTESIAN_POINT('Ctrl Pts',(0.475577680748767,-1.32768940214297,
-8.65926076437218));
#149286=CARTESIAN_POINT('',(1.07823576159075,-1.32768940191118,-8.60502055527693));
#149287=CARTESIAN_POINT('Ctrl Pts',(1.07823576225904,-1.32768940182398,
-8.60502055560242));
#149288=CARTESIAN_POINT('Ctrl Pts',(1.00588100192119,-1.21834383435451,
-8.72428746560445));
#149289=CARTESIAN_POINT('Ctrl Pts',(0.934189604625298,-1.10901465414413,
-8.84214601570619));
#149290=CARTESIAN_POINT('Ctrl Pts',(0.86356421329429,-0.999999999704432,
-8.95847402490167));
#149291=CARTESIAN_POINT('',(1.249873295,-1.32768940200002,-8.581770672));
#149292=CARTESIAN_POINT('Ctrl Pts',(1.07823576149091,-1.32768940211609,
-8.60502055540428));
#149293=CARTESIAN_POINT('Ctrl Pts',(1.08124424645351,-1.33223595151502,
-8.60006148014485));
#149294=CARTESIAN_POINT('Ctrl Pts',(1.08497798435395,-1.33650155474298,
-8.59529245980226));
#149295=CARTESIAN_POINT('Ctrl Pts',(1.09718828812373,-1.34730670103304,
-8.58285241662335));
#149296=CARTESIAN_POINT('Ctrl Pts',(1.10695343853787,-1.35293307625488,
-8.5759291122228));
#149297=CARTESIAN_POINT('Ctrl Pts',(1.12440865719429,-1.35917045597632,
-8.56736155073659));
#149298=CARTESIAN_POINT('Ctrl Pts',(1.13105522689639,-1.36087898842353,
-8.56476367686195));
#149299=CARTESIAN_POINT('Ctrl Pts',(1.14488919712257,-1.36317274229315,
-8.56061122783272));
#149300=CARTESIAN_POINT('Ctrl Pts',(1.15203016834082,-1.3637517358647,-8.5590691074326));
#149301=CARTESIAN_POINT('Ctrl Pts',(1.15927180852621,-1.36375173586557,
-8.55808816061781));
#149302=CARTESIAN_POINT('Ctrl Pts',(1.17200914606822,-1.36375173586709,
-8.55636277101395));
#149303=CARTESIAN_POINT('Ctrl Pts',(1.18485123861068,-1.36196031890982,
-8.55640100836933));
#149304=CARTESIAN_POINT('Ctrl Pts',(1.20943266280315,-1.35499086521458,
-8.55999992824462));
#149305=CARTESIAN_POINT('Ctrl Pts',(1.22091333665683,-1.34985996713517,
-8.56354935835334));
#149306=CARTESIAN_POINT('Ctrl Pts',(1.23816171620794,-1.3387389447467,-8.57230673456117));
#149307=CARTESIAN_POINT('Ctrl Pts',(1.24453195642251,-1.33344492708842,
-8.57673235212774));
#149308=CARTESIAN_POINT('Ctrl Pts',(1.2498732947827,-1.32768940185218,-8.58177067206148));
#149309=CARTESIAN_POINT('Ctrl Pts',(1.55084034118531,-1.00000000030594,
-8.86537614716069));
#149310=CARTESIAN_POINT('Ctrl Pts',(1.4518124743483,-1.10901473831009,-8.77202915141814));
#149311=CARTESIAN_POINT('Ctrl Pts',(1.35134980606936,-1.21834403195577,
-8.6774903386024));
#149312=CARTESIAN_POINT('Ctrl Pts',(1.24987329501287,-1.32768940194995,
-8.58177067192916));
#149313=CARTESIAN_POINT('',(1.845243197,-1.32768940200002,-8.473726964));
#149314=CARTESIAN_POINT('Ctrl Pts',(1.84524319784117,-1.32768940174229,
-8.47372696418715));
#149315=CARTESIAN_POINT('Ctrl Pts',(1.78387071989928,-1.21834383431894,
-8.59899957133592));
#149316=CARTESIAN_POINT('Ctrl Pts',(1.72303269008614,-1.1090146541547,-8.72281002482354));
#149317=CARTESIAN_POINT('Ctrl Pts',(1.66311917818115,-0.999999999760971,
-8.84500054287555));
#149318=CARTESIAN_POINT('',(2.014105665,-1.32768940200002,-8.435185207));
#149319=CARTESIAN_POINT('Ctrl Pts',(1.84524319731388,-1.32768940193905,
-8.4737269641006));
#149320=CARTESIAN_POINT('Ctrl Pts',(1.8477950429561,-1.33223595150089,-8.46851817393293));
#149321=CARTESIAN_POINT('Ctrl Pts',(1.85108625832112,-1.33650155487643,
-8.46343366240974));
#149322=CARTESIAN_POINT('Ctrl Pts',(1.86213229025263,-1.34730670128967,
-8.44994917584067));
#149323=CARTESIAN_POINT('Ctrl Pts',(1.87123752882059,-1.35293307651039,
-8.44217840129405));
#149324=CARTESIAN_POINT('Ctrl Pts',(1.88785448760806,-1.35917045623014,
-8.43208065655475));
#149325=CARTESIAN_POINT('Ctrl Pts',(1.89424142855602,-1.36087898867676,
-8.42889744704194));
#149326=CARTESIAN_POINT('Ctrl Pts',(1.9076474846242,-1.3631727425452,-8.42352164702133));
#149327=CARTESIAN_POINT('Ctrl Pts',(1.9146214737849,-1.36375173611614,-8.42134562301971));
#149328=CARTESIAN_POINT('Ctrl Pts',(1.92174602986137,-1.36375173611641,
-8.41971948958691));
#149329=CARTESIAN_POINT('Ctrl Pts',(1.9342774278958,-1.36375173611689,-8.41685927975983));
#149330=CARTESIAN_POINT('Ctrl Pts',(1.94707124951949,-1.36196031915855,
-8.41574620688258));
#149331=CARTESIAN_POINT('Ctrl Pts',(1.9718763208155,-1.35499086546122,-8.41712717668837));
#149332=CARTESIAN_POINT('Ctrl Pts',(1.98362894531339,-1.34985996738079,
-8.41963319816523));
#149333=CARTESIAN_POINT('Ctrl Pts',(2.00159289302696,-1.33873894504213,
-8.42680918689579));
#149334=CARTESIAN_POINT('Ctrl Pts',(2.00833419776163,-1.33344492744846,
-8.43064596424567));
#149335=CARTESIAN_POINT('Ctrl Pts',(2.01410566493822,-1.32768940228524,
-8.4351852074402));
#149336=CARTESIAN_POINT('Ctrl Pts',(2.33928330581808,-0.999999999832171,
-8.69067049301388));
#149337=CARTESIAN_POINT('Ctrl Pts',(2.23228653562601,-1.10901473810327,
-8.60657607417562));
#149338=CARTESIAN_POINT('Ctrl Pts',(2.12375390641409,-1.21834403201796,
-8.52142325077419));
#149339=CARTESIAN_POINT('Ctrl Pts',(2.01410566492906,-1.32768940228112,
-8.43518520744662));
#149340=CARTESIAN_POINT('',(2.59739382,-1.32768940200002,-8.274207905));
#149341=CARTESIAN_POINT('Ctrl Pts',(2.59739382005673,-1.32768940220199,
-8.27420790519125));
#149342=CARTESIAN_POINT('Ctrl Pts',(2.54749775952752,-1.21834383473538,
-8.40447758822955));
#149343=CARTESIAN_POINT('Ctrl Pts',(2.49800292915253,-1.10901465452695,
-8.53324309624464));
#149344=CARTESIAN_POINT('Ctrl Pts',(2.44928368495601,-1.00000000008883,
-8.66031231705933));
#149345=CARTESIAN_POINT('',(2.762121641,-1.32768940200002,-8.220684592));
#149346=CARTESIAN_POINT('Ctrl Pts',(2.59739381999827,-1.32768940222355,
-8.274207905187));
#149347=CARTESIAN_POINT('Ctrl Pts',(2.59946848029277,-1.33223595162173,
-8.26879133857389));
#149348=CARTESIAN_POINT('Ctrl Pts',(2.60229067402789,-1.33650155484869,
-8.26343227370456));
#149349=CARTESIAN_POINT('Ctrl Pts',(2.61208349771735,-1.34730670113423,
-8.24901191321329));
#149350=CARTESIAN_POINT('Ctrl Pts',(2.62045551441409,-1.35293307635233,
-8.24045623422956));
#149351=CARTESIAN_POINT('Ctrl Pts',(2.63610042335358,-1.35917045606773,
-8.22890960734339));
#149352=CARTESIAN_POINT('Ctrl Pts',(2.64217631165495,-1.36087898851275,
-8.22516669152493));
#149353=CARTESIAN_POINT('Ctrl Pts',(2.65504651588519,-1.36317274237799,
-8.21861082329637));
#149354=CARTESIAN_POINT('Ctrl Pts',(2.66179737252854,-1.36375173594733,
-8.21581841576039));
#149355=CARTESIAN_POINT('Ctrl Pts',(2.66874748175985,-1.36375173594603,
-8.21356018838122));
#149356=CARTESIAN_POINT('Ctrl Pts',(2.68097204483843,-1.36375173594376,
-8.209588187061));
#149357=CARTESIAN_POINT('Ctrl Pts',(2.69361458721409,-1.3619603189827,-8.20733276576193));
#149358=CARTESIAN_POINT('Ctrl Pts',(2.71844358976387,-1.35499086528025,
-8.20648466674613));
#149359=CARTESIAN_POINT('Ctrl Pts',(2.73037353968325,-1.34985996719732,
-8.20792710258216));
#149360=CARTESIAN_POINT('Ctrl Pts',(2.74890842063212,-1.33873894477132,
-8.2134639270796));
#149361=CARTESIAN_POINT('Ctrl Pts',(2.7559665130382,-1.33344492707015,-8.21668097286978));
#149362=CARTESIAN_POINT('Ctrl Pts',(2.76212164068402,-1.32768940178609,
-8.22068459217825));
#149363=CARTESIAN_POINT('Ctrl Pts',(3.10889173601996,-1.00000000022005,
-8.44599266929271));
#149364=CARTESIAN_POINT('Ctrl Pts',(2.99478753806051,-1.10901473827084,
-8.37182790653101));
#149365=CARTESIAN_POINT('Ctrl Pts',(2.87905878935271,-1.21834403196375,
-8.29674667337776));
#149366=CARTESIAN_POINT('Ctrl Pts',(2.76212164114016,-1.32768940200595,
-8.22068459179305));
#149367=CARTESIAN_POINT('',(3.328631754,-1.32768940200002,-8.00806979));
#149368=CARTESIAN_POINT('Ctrl Pts',(3.32863175341881,-1.32768940231455,
-8.00806979009162));
#149369=CARTESIAN_POINT('Ctrl Pts',(3.29061384423879,-1.21834383487424,
-8.14228769397692));
#149370=CARTESIAN_POINT('Ctrl Pts',(3.25286071676859,-1.10901465469334,
-8.27497151221575));
#149371=CARTESIAN_POINT('Ctrl Pts',(3.21572799918201,-1.00000000028271,
-8.40589634900338));
#149372=CARTESIAN_POINT('',(3.487898636,-1.32768940200002,-7.939995858));
#149373=CARTESIAN_POINT('Ctrl Pts',(3.32863175374707,-1.32768940219362,
-8.00806979008612));
#149374=CARTESIAN_POINT('Ctrl Pts',(3.3302125247748,-1.33223595146223,-8.00248905800613));
#149375=CARTESIAN_POINT('Ctrl Pts',(3.3325429742706,-1.33650155457232,-7.99689858780651));
#149376=CARTESIAN_POINT('Ctrl Pts',(3.34100374369261,-1.34730670076621,
-7.9816584576379));
#149377=CARTESIAN_POINT('Ctrl Pts',(3.3485751319546,-1.35293307599116,-7.97238675950792));
#149378=CARTESIAN_POINT('Ctrl Pts',(3.36312202742944,-1.35917045571755,
-7.95948421711507));
#149379=CARTESIAN_POINT('Ctrl Pts',(3.3688379436014,-1.36087898816654,-7.95521173074453));
#149380=CARTESIAN_POINT('Ctrl Pts',(3.38106867267251,-1.36317274203974,
-7.94752857829612));
#149381=CARTESIAN_POINT('Ctrl Pts',(3.38754204286877,-1.36375173561308,
-7.94414227004508));
#149382=CARTESIAN_POINT('Ctrl Pts',(3.39426174706129,-1.36375173561571,
-7.94127013063417));
#149383=CARTESIAN_POINT('Ctrl Pts',(3.40608105018694,-1.36375173562033,
-7.93621831803287));
#149384=CARTESIAN_POINT('Ctrl Pts',(3.4184705229962,-1.3619603186662,-7.9328387076302));
#149385=CARTESIAN_POINT('Ctrl Pts',(3.44312354827156,-1.35499086497692,
-7.9297683681713));
#149386=CARTESIAN_POINT('Ctrl Pts',(3.45513477067234,-1.34985996690042,
-7.93013560471274));
#149387=CARTESIAN_POINT('Ctrl Pts',(3.47409135267749,-1.33873894453579,
-7.9339886856354));
#149388=CARTESIAN_POINT('Ctrl Pts',(3.48140940496856,-1.33344492690381,
-7.93656009797619));
#149389=CARTESIAN_POINT('Ctrl Pts',(3.48789863549779,-1.32768940169679,
-7.93999585844057));
#149390=CARTESIAN_POINT('Ctrl Pts',(3.8534691968536,-1.00000000021841,-8.13331267965086));
#149391=CARTESIAN_POINT('Ctrl Pts',(3.73317627069964,-1.10901473822962,
-8.06967470393504));
#149392=CARTESIAN_POINT('Ctrl Pts',(3.61118318198707,-1.21834403188242,
-8.00526957087236));
#149393=CARTESIAN_POINT('Ctrl Pts',(3.48789863585382,-1.32768940188326,
-7.93999585808051));
#149394=CARTESIAN_POINT('',(4.033069504,-1.32768940200002,-7.677455405));
#149395=CARTESIAN_POINT('Ctrl Pts',(4.03306950415229,-1.327689401891,-7.67745540494174));
#149396=CARTESIAN_POINT('Ctrl Pts',(4.00723584390748,-1.2183438344254,-7.81454088623289));
#149397=CARTESIAN_POINT('Ctrl Pts',(3.98152838506235,-1.1090146542176,-7.9500747228005));
#149398=CARTESIAN_POINT('Ctrl Pts',(3.95628116463242,-0.999999999779801,
-8.08380104593988));
#149399=CARTESIAN_POINT('',(4.185593123,-1.32768940200002,-7.595378945));
#149400=CARTESIAN_POINT('Ctrl Pts',(4.03306950367076,-1.32768940206931,
-7.67745540499327));
#149401=CARTESIAN_POINT('Ctrl Pts',(4.03414365800827,-1.33223595145271,
-7.67175543994931));
#149402=CARTESIAN_POINT('Ctrl Pts',(4.03596359994506,-1.3365015546661,-7.66597857532337));
#149403=CARTESIAN_POINT('Ctrl Pts',(4.04302419413378,-1.34730670093839,
-7.65004137978483));
#149404=CARTESIAN_POINT('Ctrl Pts',(4.04973399360729,-1.35293307615463,
-7.64012831277831));
#149405=CARTESIAN_POINT('Ctrl Pts',(4.06306575258348,-1.3591704558669,-7.6259737385784));
#149406=CARTESIAN_POINT('Ctrl Pts',(4.0683756754347,-1.36087898831075,-7.62120608120941));
#149407=CARTESIAN_POINT('Ctrl Pts',(4.07986845471533,-1.36317274217366,
-7.61245750477902));
#149408=CARTESIAN_POINT('Ctrl Pts',(4.08601221869675,-1.36375173574184,
-7.60850456038225));
#149409=CARTESIAN_POINT('Ctrl Pts',(4.09244741474498,-1.36375173573942,
-7.60504163372406));
#149410=CARTESIAN_POINT('Ctrl Pts',(4.10376629584433,-1.36375173573516,
-7.59895068407685));
#149411=CARTESIAN_POINT('Ctrl Pts',(4.11580294633933,-1.36196031877213,
-7.59447409521846));
#149412=CARTESIAN_POINT('Ctrl Pts',(4.1400815026765,-1.35499086506602,-7.58920623590949));
#149413=CARTESIAN_POINT('Ctrl Pts',(4.15207729025624,-1.3498599669813,-7.5884953163971));
#149414=CARTESIAN_POINT('Ctrl Pts',(4.17130294590846,-1.33873894473932,
-7.59063363102621));
#149415=CARTESIAN_POINT('Ctrl Pts',(4.17882203729309,-1.33344492727405,
-7.59253870638845));
#149416=CARTESIAN_POINT('Ctrl Pts',(4.1855931231253,-1.32768940225633,-7.59537894522069));
#149417=CARTESIAN_POINT('Ctrl Pts',(4.5670207909907,-1.00000000006023,-7.75514803814697));
#149418=CARTESIAN_POINT('Ctrl Pts',(4.44150766456477,-1.10901473824446,
-7.7025492248208));
#149419=CARTESIAN_POINT('Ctrl Pts',(4.31423245247801,-1.21834403207158,
-7.64933874389548));
#149420=CARTESIAN_POINT('Ctrl Pts',(4.18559312311082,-1.32768940224795,
-7.59537894523824));
#149421=CARTESIAN_POINT('',(4.705035349,-1.32768940200002,-7.285026664));
#149422=CARTESIAN_POINT('Ctrl Pts',(4.70503534876328,-1.32768940166455,
-7.2850266637129));
#149423=CARTESIAN_POINT('Ctrl Pts',(4.6915939350508,-1.21834383431014,-7.42387599047203));
#149424=CARTESIAN_POINT('Ctrl Pts',(4.67813912632766,-1.10901465421366,
-7.56116860636961));
#149425=CARTESIAN_POINT('Ctrl Pts',(4.66498067897969,-0.999999999886531,
-7.69661972990669));
#149426=CARTESIAN_POINT('',(4.849587676,-1.32768940200002,-7.189608507));
#149427=CARTESIAN_POINT('Ctrl Pts',(4.70503534864306,-1.32768940170967,
-7.28502666373683));
#149428=CARTESIAN_POINT('Ctrl Pts',(4.70559423778768,-1.33223595129556,
-7.27925335840597));
#149429=CARTESIAN_POINT('Ctrl Pts',(4.70688901904333,-1.33650155469243,
-7.27333661116776));
#149430=CARTESIAN_POINT('Ctrl Pts',(4.71249259024252,-1.34730670111821,
-7.25683066707283));
#149431=CARTESIAN_POINT('Ctrl Pts',(4.71828677756059,-1.35293307633343,
-7.24635604537204));
#149432=CARTESIAN_POINT('Ctrl Pts',(4.73029606054557,-1.35917045604412,
-7.23106340366536));
#149433=CARTESIAN_POINT('Ctrl Pts',(4.7351572376969,-1.36087898848742,-7.22583896166848));
#149434=CARTESIAN_POINT('Ctrl Pts',(4.74581953408189,-1.3631727423492,-7.21609539964254));
#149435=CARTESIAN_POINT('Ctrl Pts',(4.75158422587189,-1.36375173591681,
-7.21160764588035));
#149436=CARTESIAN_POINT('Ctrl Pts',(4.75768310136027,-1.36375173591383,
-7.20758181342034));
#149437=CARTESIAN_POINT('Ctrl Pts',(4.76841042745519,-1.36375173590859,
-7.20050076746617));
#149438=CARTESIAN_POINT('Ctrl Pts',(4.77999734360255,-1.36196031894456,
-7.19496324300642));
#149439=CARTESIAN_POINT('Ctrl Pts',(4.80370595434181,-1.35499086523651,
-7.18754027753896));
#149440=CARTESIAN_POINT('Ctrl Pts',(4.81558972407363,-1.34985996715085,
-7.18575692587117));
#149441=CARTESIAN_POINT('Ctrl Pts',(4.83492966004747,-1.33873894484204,
-7.18616325779104));
#149442=CARTESIAN_POINT('Ctrl Pts',(4.84258925152042,-1.33344492729325,
-7.18738665775673));
#149443=CARTESIAN_POINT('Ctrl Pts',(4.84958767607709,-1.32768940218149,
-7.18960850722728));
#149444=CARTESIAN_POINT('Ctrl Pts',(5.24380141911386,-1.00000000018046,
-7.31454350411914));
#149445=CARTESIAN_POINT('Ctrl Pts',(5.11407865044419,-1.10901473830268,
-7.27340734808659));
#149446=CARTESIAN_POINT('Ctrl Pts',(4.98254606029434,-1.21834403206745,
-7.23181993899048));
#149447=CARTESIAN_POINT('Ctrl Pts',(4.8495876760775,-1.32768940218176,-7.18960850722668));
#149448=CARTESIAN_POINT('',(5.339119013,-1.32768940200002,-6.833943172));
#149449=CARTESIAN_POINT('Ctrl Pts',(5.33911901336203,-1.3276894020463,-6.83394317203872));
#149450=CARTESIAN_POINT('Ctrl Pts',(5.33817806862294,-1.21834383468527,
-6.9734384111691));
#149451=CARTESIAN_POINT('Ctrl Pts',(5.33708424031203,-1.10901465458379,
-7.11138440702185));
#149452=CARTESIAN_POINT('Ctrl Pts',(5.33612051020986,-1.00000000025242,
-7.2474697581966));
#149453=CARTESIAN_POINT('',(5.474536199,-1.32768940200002,-6.725951571));
#149454=CARTESIAN_POINT('Ctrl Pts',(5.33911901311747,-1.32768940214016,
-6.83394317211068));
#149455=CARTESIAN_POINT('Ctrl Pts',(5.33915813729677,-1.33223595149941,
-6.82814301021648));
#149456=CARTESIAN_POINT('Ctrl Pts',(5.33991733300375,-1.33650155469162,
-6.82213401903261));
#149457=CARTESIAN_POINT('Ctrl Pts',(5.34401876437183,-1.34730670095398,
-6.80519222304139));
#149458=CARTESIAN_POINT('Ctrl Pts',(5.34885068813799,-1.35293307617826,
-6.79424038213927));
#149459=CARTESIAN_POINT('Ctrl Pts',(5.3594408034379,-1.35917045590364,-6.77793280028018));
#149460=CARTESIAN_POINT('Ctrl Pts',(5.3638140955464,-1.36087898835228,-6.77229363778862));
#149461=CARTESIAN_POINT('Ctrl Pts',(5.37356006248997,-1.36317274222478,
-6.76163353959512));
#149462=CARTESIAN_POINT('Ctrl Pts',(5.37889926817801,-1.36375173579776,
-6.75664710921954));
#149463=CARTESIAN_POINT('Ctrl Pts',(5.38461271854601,-1.36375173580003,
-6.75209078459071));
#149464=CARTESIAN_POINT('Ctrl Pts',(5.39466211951056,-1.36375173580403,
-6.74407665474437));
#149465=CARTESIAN_POINT('Ctrl Pts',(5.40570601027228,-1.36196031884925,
-6.73752277956918));
#149466=CARTESIAN_POINT('Ctrl Pts',(5.42865378761812,-1.35499086515872,
-6.7280044732854));
#149467=CARTESIAN_POINT('Ctrl Pts',(5.44032985837541,-1.3498599670816,-6.72516304795477));
#149468=CARTESIAN_POINT('Ctrl Pts',(5.4596283610753,-1.33873894460838,-6.72383412557344));
#149469=CARTESIAN_POINT('Ctrl Pts',(5.46736678229439,-1.33344492683944,
-6.72436600006062));
#149470=CARTESIAN_POINT('Ctrl Pts',(5.47453619853397,-1.32768940147805,
-6.72595157121251));
#149471=CARTESIAN_POINT('Ctrl Pts',(5.87836203986568,-0.99999999994125,
-6.81504656838998));
#149472=CARTESIAN_POINT('Ctrl Pts',(5.74547408034092,-1.10901473795678,
-6.78570427387046));
#149473=CARTESIAN_POINT('Ctrl Pts',(5.61074313513168,-1.21834403161385,
-6.75607477404509));
#149474=CARTESIAN_POINT('Ctrl Pts',(5.47453619872126,-1.32768940161921,
-6.72595157087805));
#149475=CARTESIAN_POINT('',(5.93021523354241,-1.32768940189191,-6.32783678686984));
#149476=CARTESIAN_POINT('Ctrl Pts',(5.93021523412515,-1.32768940176286,
-6.32783678671984));
#149477=CARTESIAN_POINT('Ctrl Pts',(5.94178233414468,-1.21834383430549,
-6.46685480485237));
#149478=CARTESIAN_POINT('Ctrl Pts',(5.95305829295893,-1.10901465410688,
-6.60434352087773));
#149479=CARTESIAN_POINT('Ctrl Pts',(5.96429703934163,-0.999999999678913,
-6.73996742071358));
#149480=CARTESIAN_POINT('',(6.055406976,-1.32768940200002,-6.208141225));
#149481=CARTESIAN_POINT('Ctrl Pts',(5.93021523353202,-1.32768940199765,
-6.32783678695391));
#149482=CARTESIAN_POINT('Ctrl Pts',(5.92973427764573,-1.33223595152411,
-6.32205646756782));
#149483=CARTESIAN_POINT('Ctrl Pts',(5.92995177522348,-1.33650155486745,
-6.31600361284212));
#149484=CARTESIAN_POINT('Ctrl Pts',(5.93251804458815,-1.34730670125214,
-6.29876236986104));
#149485=CARTESIAN_POINT('Ctrl Pts',(5.93634880100404,-1.3529330764714,-6.28742148754437));
#149486=CARTESIAN_POINT('Ctrl Pts',(5.94543448325041,-1.35917045618876,
-6.27023026460103));
#149487=CARTESIAN_POINT('Ctrl Pts',(5.94928467914374,-1.3608789886345,-6.26422178483839));
#149488=CARTESIAN_POINT('Ctrl Pts',(5.95803584785762,-1.36317274250118,
-6.25273097932687));
#149489=CARTESIAN_POINT('Ctrl Pts',(5.9629065793017,-1.36375173607124,-6.24728602014728));
#149490=CARTESIAN_POINT('Ctrl Pts',(5.96818860320827,-1.36375173607065,
-6.24223588820087));
#149491=CARTESIAN_POINT('Ctrl Pts',(5.97747916718049,-1.36375173606962,
-6.23335319952962));
#149492=CARTESIAN_POINT('Ctrl Pts',(5.98789111364513,-1.36196031910978,
-6.22583574159617));
#149493=CARTESIAN_POINT('Ctrl Pts',(6.00989329559082,-1.3549908654096,-6.21429873031895));
#149494=CARTESIAN_POINT('Ctrl Pts',(6.02126765851761,-1.34985996732779,
-6.21042210882142));
#149495=CARTESIAN_POINT('Ctrl Pts',(6.0403693472299,-1.33873894496681,-6.20736863188564));
#149496=CARTESIAN_POINT('Ctrl Pts',(6.04812429250932,-1.33344492734667,
-6.20720469845112));
#149497=CARTESIAN_POINT('Ctrl Pts',(6.05540697612596,-1.32768940215382,
-6.20814122496572));
#149498=CARTESIAN_POINT('Ctrl Pts',(6.46559354791635,-0.999999999885752,
-6.26067888293268));
#149499=CARTESIAN_POINT('Ctrl Pts',(6.33061033303081,-1.10901473812568,
-6.24336669663294));
#149500=CARTESIAN_POINT('Ctrl Pts',(6.19376580688884,-1.21834403200888,
-6.22593366519494));
#149501=CARTESIAN_POINT('Ctrl Pts',(6.05540697622248,-1.32768940224085,
-6.20814122474999));
#149502=CARTESIAN_POINT('',(6.473564847,-1.32768940200002,-5.770782381));
#149503=CARTESIAN_POINT('Ctrl Pts',(6.47356484705234,-1.32768940202094,
-5.77078238100751));
#149504=CARTESIAN_POINT('Ctrl Pts',(6.49754686040969,-1.21834383453442,
-5.90820388664413));
#149505=CARTESIAN_POINT('Ctrl Pts',(6.52110181902666,-1.10901465430654,
-6.04412834439049));
#149506=CARTESIAN_POINT('Ctrl Pts',(6.54445255418411,-0.999999999849283,
-6.17819882884537));
#149507=CARTESIAN_POINT('',(6.587523177,-1.32768940200002,-5.640346578));
#149508=CARTESIAN_POINT('Ctrl Pts',(6.47356484669524,-1.32768940216809,
-5.77078238118696));
#149509=CARTESIAN_POINT('Ctrl Pts',(6.47256768322408,-1.33223595155632,
-5.76506844435757));
#149510=CARTESIAN_POINT('Ctrl Pts',(6.47224173153327,-1.33650155477443,
-5.75902046047074));
#149511=CARTESIAN_POINT('Ctrl Pts',(6.47325217673578,-1.34730670105451,
-5.74161858722322));
#149512=CARTESIAN_POINT('Ctrl Pts',(6.47605092279891,-1.35293307627464,
-5.7299799736068));
#149513=CARTESIAN_POINT('Ctrl Pts',(6.48355901941539,-1.3591704559933,-5.71204352319526));
#149514=CARTESIAN_POINT('Ctrl Pts',(6.48685511957833,-1.3608789884395,-5.70571410290666));
#149515=CARTESIAN_POINT('Ctrl Pts',(6.49454103079465,-1.36317274230711,
-5.69348510728424));
#149516=CARTESIAN_POINT('Ctrl Pts',(6.49890407172791,-1.36375173587764,
-5.68762545890897));
#149517=CARTESIAN_POINT('Ctrl Pts',(6.50371214142148,-1.36375173587751,
-5.6821221803364));
#149518=CARTESIAN_POINT('Ctrl Pts',(6.51216906624052,-1.36375173587729,
-5.67244245102451));
#149519=CARTESIAN_POINT('Ctrl Pts',(6.52186523753564,-1.36196031891828,
-5.6640219364811));
#149520=CARTESIAN_POINT('Ctrl Pts',(6.54274467544732,-1.35499086521973,
-5.65055910943509));
#149521=CARTESIAN_POINT('Ctrl Pts',(6.55372575086094,-1.3498599671387,-5.64567850404373));
#149522=CARTESIAN_POINT('Ctrl Pts',(6.57247683027915,-1.33873894474861,
-5.64092505731962));
#149523=CARTESIAN_POINT('Ctrl Pts',(6.58018586159814,-1.33344492709045,
-5.64006663589892));
#149524=CARTESIAN_POINT('Ctrl Pts',(6.58752317690413,-1.3276894018546,-5.64034657752293));
#149525=CARTESIAN_POINT('Ctrl Pts',(7.00076789692398,-0.999999999893325,
-5.65590389374846));
#149526=CARTESIAN_POINT('Ctrl Pts',(6.86477623251869,-1.10901473799573,
-5.65076120332882));
#149527=CARTESIAN_POINT('Ctrl Pts',(6.72691991747828,-1.21834403174059,
-5.64566500091207));
#149528=CARTESIAN_POINT('Ctrl Pts',(6.58752317688628,-1.32768940183436,
-5.64034657757489));
#149529=CARTESIAN_POINT('',(6.964793123,-1.32768940200002,-5.167265029));
#149530=CARTESIAN_POINT('Ctrl Pts',(6.9647931225424,-1.32768940189471,-5.1672650290375));
#149531=CARTESIAN_POINT('Ctrl Pts',(7.00099696010947,-1.21834383456653,
-5.3019835847847));
#149532=CARTESIAN_POINT('Ctrl Pts',(7.03664126779649,-1.10901465449722,
-5.43524940021246));
#149533=CARTESIAN_POINT('Ctrl Pts',(7.07191598528383,-1.00000000019748,
-5.56668701235598));
#149534=CARTESIAN_POINT('',(7.066600514,-1.32768940200002,-5.027139175));
#149535=CARTESIAN_POINT('Ctrl Pts',(6.96479312275204,-1.32768940180384,
-5.16726502890744));
#149536=CARTESIAN_POINT('Ctrl Pts',(6.96328778019254,-1.3322359512407,-5.1616634797066));
#149537=CARTESIAN_POINT('Ctrl Pts',(6.96242100357658,-1.33650155450292,
-5.155669061255));
#149538=CARTESIAN_POINT('Ctrl Pts',(6.9618674891292,-1.34730670082041,-5.13824666716368));
#149539=CARTESIAN_POINT('Ctrl Pts',(6.96361169098159,-1.35293307604079,
-5.12640402952091));
#149540=CARTESIAN_POINT('Ctrl Pts',(6.96948175118831,-1.35917045575974,
-5.10786676539326));
#149541=CARTESIAN_POINT('Ctrl Pts',(6.97219721736018,-1.36087898820603,
-5.10126736534917));
#149542=CARTESIAN_POINT('Ctrl Pts',(6.97875598864058,-1.3631727420738,-5.08839864029793));
#149543=CARTESIAN_POINT('Ctrl Pts',(6.98257621042259,-1.36375173564443,
-5.08217148117021));
#149544=CARTESIAN_POINT('Ctrl Pts',(6.9868716141528,-1.36375173564439,-5.07625936513457));
#149545=CARTESIAN_POINT('Ctrl Pts',(6.9944268096322,-1.36375173564433,-5.06586053067067));
#149546=CARTESIAN_POINT('Ctrl Pts',(7.00332913788735,-1.36196031868552,
-5.05660475654901));
#149547=CARTESIAN_POINT('Ctrl Pts',(7.02291772280707,-1.35499086498739,
-5.04132450850107));
#149548=CARTESIAN_POINT('Ctrl Pts',(7.03341709754474,-1.34985996690657,
-5.0354792149805));
#149549=CARTESIAN_POINT('Ctrl Pts',(7.05166659470129,-1.33873894466852,
-5.02906407052158));
#149550=CARTESIAN_POINT('Ctrl Pts',(7.05926764317834,-1.33344492720299,
-5.02751807262591));
#149551=CARTESIAN_POINT('Ctrl Pts',(7.06660051416279,-1.32768940218439,
-5.0271391753499));
#149552=CARTESIAN_POINT('Ctrl Pts',(7.47957617995657,-0.999999999937531,
-5.00559089112874));
#149553=CARTESIAN_POINT('Ctrl Pts',(7.34367099065878,-1.1090147381492,-5.0126591024965));
#149554=CARTESIAN_POINT('Ctrl Pts',(7.20591282440991,-1.2183440320037,-5.01994076071516));
#149555=CARTESIAN_POINT('Ctrl Pts',(7.06660051417724,-1.32768940220666,
-5.02713917529117));
#149556=CARTESIAN_POINT('',(7.399944979,-1.32768940200002,-4.522143897));
#149557=CARTESIAN_POINT('Ctrl Pts',(7.39994497873908,-1.32768940215641,
-4.52214389722653));
#149558=CARTESIAN_POINT('Ctrl Pts',(7.44807914856806,-1.21834383484025,
-4.65307482860847));
#149559=CARTESIAN_POINT('Ctrl Pts',(7.495525818383,-1.1090146547835,-4.78260902385036));
#149560=CARTESIAN_POINT('Ctrl Pts',(7.5424405069824,-1.00000000049598,-4.9103555054297));
#149561=CARTESIAN_POINT('',(7.488781739,-1.32768940200002,-4.373456206));
#149562=CARTESIAN_POINT('Ctrl Pts',(7.39994497860661,-1.32768940221744,
-4.52214389732625));
#149563=CARTESIAN_POINT('Ctrl Pts',(7.39794357718913,-1.33223595153308,
-4.5166998362934));
#149564=CARTESIAN_POINT('Ctrl Pts',(7.39654295448025,-1.33650155468582,
-4.51080724699965));
#149565=CARTESIAN_POINT('Ctrl Pts',(7.39442993696486,-1.34730670091578,
-4.49350460715019));
#149566=CARTESIAN_POINT('Ctrl Pts',(7.39510555131524,-1.35293307614091,
-4.48155329543663));
#149567=CARTESIAN_POINT('Ctrl Pts',(7.39929031283406,-1.35917045586763,
-4.46256446874343));
#149568=CARTESIAN_POINT('Ctrl Pts',(7.40140328167635,-1.36087898831677,
-4.45574822343214));
#149569=CARTESIAN_POINT('Ctrl Pts',(7.40678210564818,-1.36317274219025,
-4.44234338035808));
#149570=CARTESIAN_POINT('Ctrl Pts',(7.41002875009816,-1.36375173576373,
-4.43579884790072));
#149571=CARTESIAN_POINT('Ctrl Pts',(7.41377690379883,-1.36375173576648,
-4.42952549528285));
#149572=CARTESIAN_POINT('Ctrl Pts',(7.42036953994479,-1.36375173577133,
-4.41849128096622));
#149573=CARTESIAN_POINT('Ctrl Pts',(7.42840634884571,-1.36196031881741,
-4.40847476931493));
#149574=CARTESIAN_POINT('Ctrl Pts',(7.44654636500287,-1.3549908651285,-4.39150012783264));
#149575=CARTESIAN_POINT('Ctrl Pts',(7.45647950427152,-1.34985996705217,
-4.3847372090463));
#149576=CARTESIAN_POINT('Ctrl Pts',(7.47408048527613,-1.33873894477316,
-4.37671201771834));
#149577=CARTESIAN_POINT('Ctrl Pts',(7.48151235206002,-1.3334449272496,-4.37449089080897));
#149578=CARTESIAN_POINT('Ctrl Pts',(7.48878173904294,-1.32768940216483,
-4.37345620538491));
#149579=CARTESIAN_POINT('Ctrl Pts',(7.89816331290478,-0.999999999857504,
-4.31497581514083));
#149580=CARTESIAN_POINT('Ctrl Pts',(7.76343882751087,-1.10901473804168,
-4.3341980192771));
#149581=CARTESIAN_POINT('Ctrl Pts',(7.62688795793262,-1.21834403186849,
-4.35379891056257));
#149582=CARTESIAN_POINT('Ctrl Pts',(7.48878173899302,-1.32768940204296,
-4.37345620571204));
#149583=CARTESIAN_POINT('',(7.77551683,-1.32768940200002,-3.840613121));
#149584=CARTESIAN_POINT('Ctrl Pts',(7.77551682982721,-1.32768940206457,
-3.84061312113776));
#149585=CARTESIAN_POINT('Ctrl Pts',(7.83519378383851,-1.21834383471285,
-3.96670224946581));
#149586=CARTESIAN_POINT('Ctrl Pts',(7.89406080304461,-1.10901465462005,
-4.09146189152694));
#149587=CARTESIAN_POINT('Ctrl Pts',(7.952237733216,-1.00000000029693,-4.21448870316095));
#149588=CARTESIAN_POINT('',(7.85066769791133,-1.32768940203921,-3.68456073648916));
#149589=CARTESIAN_POINT('Ctrl Pts',(7.77551682988423,-1.32768940203625,
-3.84061312108626));
#149590=CARTESIAN_POINT('Ctrl Pts',(7.77303548357002,-1.33223595146919,
-3.83537038038258));
#149591=CARTESIAN_POINT('Ctrl Pts',(7.77111229166754,-1.33650155472793,
-3.82962706364747));
#149592=CARTESIAN_POINT('Ctrl Pts',(7.76745678383559,-1.34730670104337,
-3.81258348842368));
#149593=CARTESIAN_POINT('Ctrl Pts',(7.76705837104186,-1.35293307626466,
-3.80061972757348));
#149594=CARTESIAN_POINT('Ctrl Pts',(7.76952414064379,-1.3591704559852,-3.78133222518373));
#149595=CARTESIAN_POINT('Ctrl Pts',(7.77101759977719,-1.36087898843209,
-3.77435401500558));
#149596=CARTESIAN_POINT('Ctrl Pts',(7.77517316931867,-1.36317274230107,
-3.76052098182607));
#149597=CARTESIAN_POINT('Ctrl Pts',(7.77782009636727,-1.36375173587229,
-3.75371176876821));
#149598=CARTESIAN_POINT('Ctrl Pts',(7.78099082211098,-1.36375173587283,
-3.74712768891714));
#149599=CARTESIAN_POINT('Ctrl Pts',(7.78656781889864,-1.36375173587379,
-3.73554693575616));
#149600=CARTESIAN_POINT('Ctrl Pts',(7.79367440078957,-1.36196031891597,
-3.7248503336419));
#149601=CARTESIAN_POINT('Ctrl Pts',(7.8102197954466,-1.35499086521966,-3.70631796856791));
#149602=CARTESIAN_POINT('Ctrl Pts',(7.81950672345209,-1.34985996713973,
-3.69869187556752));
#149603=CARTESIAN_POINT('Ctrl Pts',(7.83631747555383,-1.33873894480565,
-3.68912125148975));
#149604=CARTESIAN_POINT('Ctrl Pts',(7.8435203236244,-1.33344492721707,-3.6862428787659));
#149605=CARTESIAN_POINT('Ctrl Pts',(7.85066769778106,-1.32768940205954,
-3.68456073586607));
#149606=CARTESIAN_POINT('Ctrl Pts',(8.25315907915067,-1.0000000002333,-3.58961908982468));
#149607=CARTESIAN_POINT('Ctrl Pts',(8.12070002029395,-1.10901473821362,
-3.62084052066841));
#149608=CARTESIAN_POINT('Ctrl Pts',(7.98645587500192,-1.21834403183509,
-3.65260282999209));
#149609=CARTESIAN_POINT('Ctrl Pts',(7.85066769773846,-1.327689401805,-3.68456073655596));
#149610=CARTESIAN_POINT('',(8.088484791,-1.32768940200002,-3.128159987));
#149611=CARTESIAN_POINT('Ctrl Pts',(8.08848479089928,-1.32768940204577,
-3.12815998710087));
#149612=CARTESIAN_POINT('Ctrl Pts',(8.15922404537986,-1.21834383466874,
-3.2483921167694));
#149613=CARTESIAN_POINT('Ctrl Pts',(8.2290374513845,-1.10901465455067,-3.3673727142875));
#149614=CARTESIAN_POINT('Ctrl Pts',(8.29800821672838,-1.00000000020229,
-3.48468931634764));
#149615=CARTESIAN_POINT('',(8.14934469545831,-1.32768940190648,-2.96599935139841));
#149616=CARTESIAN_POINT('Ctrl Pts',(8.08848479065033,-1.32768940218081,
-3.12815998737019));
#149617=CARTESIAN_POINT('Ctrl Pts',(8.08554347786003,-1.33223595160539,
-3.1231607785749));
#149618=CARTESIAN_POINT('Ctrl Pts',(8.08311320122475,-1.33650155485665,
-3.11761297634637));
#149619=CARTESIAN_POINT('Ctrl Pts',(8.07794463509115,-1.3473067011667,-3.10096569075218));
#149620=CARTESIAN_POINT('Ctrl Pts',(8.07647540293555,-1.35293307638893,
-3.08908580593355));
#149621=CARTESIAN_POINT('Ctrl Pts',(8.07720232768916,-1.35917045611106,
-3.06965491947504));
#149622=CARTESIAN_POINT('Ctrl Pts',(8.07806425265739,-1.36087898855854,
-3.06257092887487));
#149623=CARTESIAN_POINT('Ctrl Pts',(8.08096310956339,-1.3631727424287,-3.04842108103817));
#149624=CARTESIAN_POINT('Ctrl Pts',(8.08298900770923,-1.36375173600051,
-3.04140201115875));
#149625=CARTESIAN_POINT('Ctrl Pts',(8.08555677667574,-1.36375173600163,
-3.03456021521294));
#149626=CARTESIAN_POINT('Ctrl Pts',(8.09007323140408,-1.3637517360036,-3.02252616462162));
#149627=CARTESIAN_POINT('Ctrl Pts',(8.09619236826459,-1.36196031904678,
-3.01123559479314));
#149628=CARTESIAN_POINT('Ctrl Pts',(8.11100992762966,-1.35499086535231,
-2.99129471782952));
#149629=CARTESIAN_POINT('Ctrl Pts',(8.11957587148718,-1.34985996727328,
-2.98286685142905));
#149630=CARTESIAN_POINT('Ctrl Pts',(8.13546104438257,-1.33873894489342,
-2.97182785162225));
#149631=CARTESIAN_POINT('Ctrl Pts',(8.14237688063509,-1.33344492724556,
-2.96831540803315));
#149632=CARTESIAN_POINT('Ctrl Pts',(8.14934469550913,-1.327689402021,-2.96599935126671));
#149633=CARTESIAN_POINT('Ctrl Pts',(8.54170526199855,-0.99999999983659,
-2.83536086241028));
#149634=CARTESIAN_POINT('Ctrl Pts',(8.41257811164622,-1.10901473799347,
-2.87833014352137));
#149635=CARTESIAN_POINT('Ctrl Pts',(8.28172154505887,-1.21834403179278,
-2.92199813961197));
#149636=CARTESIAN_POINT('Ctrl Pts',(8.14934469551528,-1.32768940194035,
-2.96599935148564));
#149637=CARTESIAN_POINT('',(8.336329029,-1.32768940200002,-2.390520747));
#149638=CARTESIAN_POINT('Ctrl Pts',(8.33632902896119,-1.32768940187385,
-2.39052074690614));
#149639=CARTESIAN_POINT('Ctrl Pts',(8.41756103301672,-1.21834383447248,
-2.50392783959535));
#149640=CARTESIAN_POINT('Ctrl Pts',(8.49775872931061,-1.10901465432932,
-2.61617143085006));
#149641=CARTESIAN_POINT('Ctrl Pts',(8.57696801776182,-0.999999999956055,
-2.72683325912718));
#149642=CARTESIAN_POINT('',(8.382407962,-1.32768940200002,-2.223557482));
#149643=CARTESIAN_POINT('Ctrl Pts',(8.33632902867258,-1.32768940204799,
-2.39052074728083));
#149644=CARTESIAN_POINT('Ctrl Pts',(8.33295143111257,-1.33223595148368,
-2.3858053210651));
#149645=CARTESIAN_POINT('Ctrl Pts',(8.33003363689228,-1.33650155474458,
-2.38049770096133));
#149646=CARTESIAN_POINT('Ctrl Pts',(8.32339362671072,-1.34730670105808,
-2.36438073912203));
#149647=CARTESIAN_POINT('Ctrl Pts',(8.32086540459087,-1.35293307627555,
-2.3526803801806));
#149648=CARTESIAN_POINT('Ctrl Pts',(8.31984763173159,-1.35917045598987,
-2.33326255572515));
#149649=CARTESIAN_POINT('Ctrl Pts',(8.3200710828237,-1.3608789884345,-2.32612982083004));
#149650=CARTESIAN_POINT('Ctrl Pts',(8.32168988720682,-1.36317274229893,
-2.31177708459178));
#149651=CARTESIAN_POINT('Ctrl Pts',(8.32307844511106,-1.36375173586787,
-2.30460467131509));
#149652=CARTESIAN_POINT('Ctrl Pts',(8.32502258313608,-1.36375173586619,
-2.29756024539374));
#149653=CARTESIAN_POINT('Ctrl Pts',(8.32844213197043,-1.36375173586324,
-2.28516978847247));
#149654=CARTESIAN_POINT('Ctrl Pts',(8.33352455611133,-1.3619603189015,-2.27337615596146));
#149655=CARTESIAN_POINT('Ctrl Pts',(8.34649497791398,-1.3549908651978,-2.25218731932978));
#149656=CARTESIAN_POINT('Ctrl Pts',(8.3542709696827,-1.34985996711426,-2.24302553575725));
#149657=CARTESIAN_POINT('Ctrl Pts',(8.36910266521966,-1.33873894473671,
-2.23060703981489));
#149658=CARTESIAN_POINT('Ctrl Pts',(8.37567580732036,-1.33344492709784,
-2.2264888055179));
#149659=CARTESIAN_POINT('Ctrl Pts',(8.38240796207933,-1.32768940188415,
-2.2235574824097));
#149660=CARTESIAN_POINT('Ctrl Pts',(8.76147865594041,-1.00000000018314,
-2.05827397549611));
#149661=CARTESIAN_POINT('Ctrl Pts',(8.63672307032885,-1.10901473824796,
-2.11264514330979));
#149662=CARTESIAN_POINT('Ctrl Pts',(8.51030766293714,-1.21834403195478,
-2.16786723695558));
#149663=CARTESIAN_POINT('Ctrl Pts',(8.38240796203887,-1.32768940201087,
-2.22355748206797));
#149664=CARTESIAN_POINT('',(8.517054046,-1.32768940200002,-1.633634441));
#149665=CARTESIAN_POINT('Ctrl Pts',(8.51705404654846,-1.32768940205777,
-1.63363444058707));
#149666=CARTESIAN_POINT('Ctrl Pts',(8.60812476791986,-1.21834383457677,
-1.73930340900002));
#149667=CARTESIAN_POINT('Ctrl Pts',(8.69806104988347,-1.10901465435411,
-1.8439062745251));
#149668=CARTESIAN_POINT('Ctrl Pts',(8.78687111490328,-0.999999999901665,
-1.94702234497933));
#149669=CARTESIAN_POINT('',(8.547981008,-1.32768940200002,-1.463212837));
#149670=CARTESIAN_POINT('Ctrl Pts',(8.51705404632891,-1.32768940220838,
-1.6336344409322));
#149671=CARTESIAN_POINT('Ctrl Pts',(8.5132673585444,-1.33223595152413,-1.62924076322205));
#149672=CARTESIAN_POINT('Ctrl Pts',(8.50988553919814,-1.33650155467649,
-1.62421605920029));
#149673=CARTESIAN_POINT('Ctrl Pts',(8.50182754649101,-1.34730670090065,
-1.6087591855685));
#149674=CARTESIAN_POINT('Ctrl Pts',(8.49826069015919,-1.3529330761202,-1.59733255691655));
#149675=CARTESIAN_POINT('Ctrl Pts',(8.49550641418745,-1.35917045583786,
-1.57808413536979));
#149676=CARTESIAN_POINT('Ctrl Pts',(8.49508959230381,-1.36087898828368,
-1.57096008476704));
#149677=CARTESIAN_POINT('Ctrl Pts',(8.49541531049769,-1.36317274215052,
-1.55652001991912));
#149678=CARTESIAN_POINT('Ctrl Pts',(8.49615534830605,-1.36375173572067,
-1.54925201129861));
#149679=CARTESIAN_POINT('Ctrl Pts',(8.4974602023311,-1.36375173572018,-1.54206167297575));
#149680=CARTESIAN_POINT('Ctrl Pts',(8.49975531307054,-1.3637517357193,-1.52941457039706));
#149681=CARTESIAN_POINT('Ctrl Pts',(8.50376010379714,-1.36196031875968,
-1.51721283059529));
#149682=CARTESIAN_POINT('Ctrl Pts',(8.51477895782059,-1.35499086505998,
-1.49494663434248));
#149683=CARTESIAN_POINT('Ctrl Pts',(8.52170238978374,-1.34985996697839,
-1.48512469888792));
#149684=CARTESIAN_POINT('Ctrl Pts',(8.53536119188796,-1.33873894459695,
-1.4714266932106));
#149685=CARTESIAN_POINT('Ctrl Pts',(8.54153871678395,-1.33344492695049,
-1.46673582579239));
#149686=CARTESIAN_POINT('Ctrl Pts',(8.54798100809932,-1.32768940172794,
-1.46321283762611));
#149687=CARTESIAN_POINT('Ctrl Pts',(8.9107097751411,-1.00000000032794,-1.26461507871065));
#149688=CARTESIAN_POINT('Ctrl Pts',(8.79133021285898,-1.10901473827851,
-1.32995036863204));
#149689=CARTESIAN_POINT('Ctrl Pts',(8.6703737871565,-1.21834403187058,-1.39628194408301));
#149690=CARTESIAN_POINT('Ctrl Pts',(8.54798100805239,-1.32768940181178,
-1.46321283740333));
#149691=CARTESIAN_POINT('',(8.629204753,-1.32768940200002,-0.863595069999998));
#149692=CARTESIAN_POINT('Ctrl Pts',(8.6292047530183,-1.32768940220178,-0.863595070208368));
#149693=CARTESIAN_POINT('Ctrl Pts',(8.72938094365667,-1.21834383481036,
-0.960675129813628));
#149694=CARTESIAN_POINT('Ctrl Pts',(8.82833169708264,-1.10901465467741,
-1.05679506871452));
#149695=CARTESIAN_POINT('Ctrl Pts',(8.92602749210211,-1.00000000031437,
-1.15153515125643));
#149696=CARTESIAN_POINT('',(8.644730737,-1.32768940200002,-0.691087262999999));
#149697=CARTESIAN_POINT('Ctrl Pts',(8.62920475309882,-1.32768940213718,
-0.86359507005258));
#149698=CARTESIAN_POINT('Ctrl Pts',(8.62503946318526,-1.33223595143947,
-0.85955851608047));
#149699=CARTESIAN_POINT('Ctrl Pts',(8.62122084706452,-1.33650155457962,
-0.854857183999841));
#149700=CARTESIAN_POINT('Ctrl Pts',(8.6118097500053,-1.34730670079354,-0.840184848108705));
#149701=CARTESIAN_POINT('Ctrl Pts',(8.60723297769259,-1.35293307601313,
-0.829123950240993));
#149702=CARTESIAN_POINT('Ctrl Pts',(8.60276437442064,-1.3591704557308,-0.810199908575189));
#149703=CARTESIAN_POINT('Ctrl Pts',(8.60171063556652,-1.3608789881766,-0.803141900931394));
#149704=CARTESIAN_POINT('Ctrl Pts',(8.60074064508077,-1.36317274204343,
-0.788730770385562));
#149705=CARTESIAN_POINT('Ctrl Pts',(8.60082620444441,-1.36375173561358,
-0.781425684153338));
#149706=CARTESIAN_POINT('Ctrl Pts',(8.6014812685525,-1.36375173561308,-0.77414732580565));
#149707=CARTESIAN_POINT('Ctrl Pts',(8.60263346231566,-1.3637517356122,-0.761345404603284));
#149708=CARTESIAN_POINT('Ctrl Pts',(8.60552837540853,-1.36196031865258,
-0.748833798745698));
#149709=CARTESIAN_POINT('Ctrl Pts',(8.61450694432037,-1.35499086495292,
-0.72566951719315));
#149710=CARTESIAN_POINT('Ctrl Pts',(8.6205220730753,-1.34985996687135,-0.715266510306567));
#149711=CARTESIAN_POINT('Ctrl Pts',(8.63289800898064,-1.33873894459279,
-0.700399283329013));
#149712=CARTESIAN_POINT('Ctrl Pts',(8.63863017872564,-1.33344492707686,
-0.695173550994194));
#149713=CARTESIAN_POINT('Ctrl Pts',(8.64473073689484,-1.32768940200152,
-0.691087262840885));
#149714=CARTESIAN_POINT('Ctrl Pts',(8.98819709909128,-1.00000000022959,
-0.460774243805896));
#149715=CARTESIAN_POINT('Ctrl Pts',(8.87515473393588,-1.10901473830769,
-0.536547614610087));
#149716=CARTESIAN_POINT('Ctrl Pts',(8.76063115969153,-1.21834403202809,
-0.613454609141287));
#149717=CARTESIAN_POINT('Ctrl Pts',(8.64473073681857,-1.32768940209739,
-0.691087262591988));
#149718=CARTESIAN_POINT('Ctrl Pts',(8.67187817713732,-1.32768940195935,
-0.0866025397794751));
#149719=CARTESIAN_POINT('Ctrl Pts',(8.78035327729649,-1.21834383460799,
-0.174312059059673));
#149720=CARTESIAN_POINT('Ctrl Pts',(8.88752180893808,-1.10901465451525,
-0.261175170144172));
#149721=CARTESIAN_POINT('Ctrl Pts',(8.99331674489802,-1.00000000019189,
-0.346776473370393));
#149722=CARTESIAN_POINT('Origin',(1.11022302462516E-15,2.49999999999998,
2.22044604925031E-15));
#149723=CARTESIAN_POINT('',(-9.,1.75940739586291,2.77153710886662E-15));
#149724=CARTESIAN_POINT('',(-9.,2.49999999999998,3.32262816848293E-15));
#149725=CARTESIAN_POINT('',(-8.999583324,1.69247211199998,0.0866025400000026));
#149726=CARTESIAN_POINT('Ctrl Pts',(-9.,1.75940739586291,2.22044604925031E-15));
#149727=CARTESIAN_POINT('Ctrl Pts',(-9.,1.75940739586291,0.00982275238874841));
#149728=CARTESIAN_POINT('Ctrl Pts',(-8.99998359035555,1.75748289664218,
0.0195489494290313));
#149729=CARTESIAN_POINT('Ctrl Pts',(-8.99992093207107,1.74964163101758,
0.0390855278294033));
#149730=CARTESIAN_POINT('Ctrl Pts',(-8.999873350116,1.74349822247422,0.0484604739130678));
#149731=CARTESIAN_POINT('Ctrl Pts',(-8.9997556224668,1.7263063716269,0.0671302358527082));
#149732=CARTESIAN_POINT('Ctrl Pts',(-8.99968442188485,1.71456563907317,
0.0756568956210235));
#149733=CARTESIAN_POINT('Ctrl Pts',(-8.99960986283583,1.69868853660841,
0.0838135890526348));
#149734=CARTESIAN_POINT('Ctrl Pts',(-8.99959624897225,1.69560796569572,
0.0852593676028396));
#149735=CARTESIAN_POINT('Ctrl Pts',(-8.9995833236904,1.69247211204886,0.0866025401111445));
#149736=CARTESIAN_POINT('Ctrl Pts',(-8.99331674508598,1.00000000014682,
0.346776473475385));
#149737=CARTESIAN_POINT('Ctrl Pts',(-8.99381097525863,1.04120750313464,
0.333959085827753));
#149738=CARTESIAN_POINT('Ctrl Pts',(-8.99429823665098,1.08227801725674,
0.320609565855717));
#149739=CARTESIAN_POINT('Ctrl Pts',(-8.99697437540542,1.31475831842863,
0.242147345620229));
#149740=CARTESIAN_POINT('Ctrl Pts',(-8.99880589307605,1.50385659888367,
0.167391759544172));
#149741=CARTESIAN_POINT('Ctrl Pts',(-8.99958332369329,1.69247211191984,
0.0866025398099413));
#149742=CARTESIAN_POINT('',(-8.971116639,1.69247211199998,0.720462526000001));
#149743=CARTESIAN_POINT('Ctrl Pts',(-8.9711166389309,1.69247211219709,0.7204625255328));
#149744=CARTESIAN_POINT('Ctrl Pts',(-8.97758422784487,1.50385659904378,
0.639928851033998));
#149745=CARTESIAN_POINT('Ctrl Pts',(-8.98246112239683,1.31475831847271,
0.565310032927709));
#149746=CARTESIAN_POINT('Ctrl Pts',(-8.98682905618331,1.08227801719273,
0.486923791245082));
#149747=CARTESIAN_POINT('Ctrl Pts',(-8.98754039810537,1.0412075030817,0.473584334742427));
#149748=CARTESIAN_POINT('Ctrl Pts',(-8.98819709932765,1.000000000105,0.460774243678978));
#149749=CARTESIAN_POINT('',(-8.955590655,1.69247211199998,0.892970333000003));
#149750=CARTESIAN_POINT('Ctrl Pts',(-8.97111663891427,1.69247211210811,
0.720462525739921));
#149751=CARTESIAN_POINT('Ctrl Pts',(-8.97094631389628,1.6974393326074,0.722583393305224));
#149752=CARTESIAN_POINT('Ctrl Pts',(-8.97075555028734,1.70224131070956,
0.724949445788221));
#149753=CARTESIAN_POINT('Ctrl Pts',(-8.96991022372285,1.72064855663712,
0.735372056421202));
#149754=CARTESIAN_POINT('Ctrl Pts',(-8.96910800608783,1.73230722803945,
0.745137489624774));
#149755=CARTESIAN_POINT('Ctrl Pts',(-8.96754183055015,1.7468654653495,0.763706039604066));
#149756=CARTESIAN_POINT('Ctrl Pts',(-8.96684856957967,1.75155833642529,
0.771819838253853));
#149757=CARTESIAN_POINT('Ctrl Pts',(-8.96534621752964,1.75781013611547,
0.789074245141224));
#149758=CARTESIAN_POINT('Ctrl Pts',(-8.96457104154341,1.75940739573185,
0.797838434983111));
#149759=CARTESIAN_POINT('Ctrl Pts',(-8.96376864597118,1.75940739573272,
0.806753779975071));
#149760=CARTESIAN_POINT('Ctrl Pts',(-8.96288814123577,1.75940739573368,
0.816536988849674));
#149761=CARTESIAN_POINT('Ctrl Pts',(-8.96199994807101,1.7574828965141,0.826222560130248));
#149762=CARTESIAN_POINT('Ctrl Pts',(-8.96018629664472,1.74964163089218,
0.845674873362572));
#149763=CARTESIAN_POINT('Ctrl Pts',(-8.95929854255293,1.74349822235063,
0.855007813454931));
#149764=CARTESIAN_POINT('Ctrl Pts',(-8.95750774428347,1.72630637150765,
0.873591863395142));
#149765=CARTESIAN_POINT('Ctrl Pts',(-8.95667250644544,1.71456563895655,
0.882077814966626));
#149766=CARTESIAN_POINT('Ctrl Pts',(-8.95586708718875,1.69868853652541,
0.890194988511478));
#149767=CARTESIAN_POINT('Ctrl Pts',(-8.95572392954188,1.69560796564499,
0.891633726431578));
#149768=CARTESIAN_POINT('Ctrl Pts',(-8.95559065523919,1.69247211203143,
0.892970333097604));
#149769=CARTESIAN_POINT('Ctrl Pts',(-8.92602749238919,1.00000000013511,
1.1515351514879));
#149770=CARTESIAN_POINT('Ctrl Pts',(-8.92766867470473,1.04120750303497,
1.13881366534867));
#149771=CARTESIAN_POINT('Ctrl Pts',(-8.92935061626786,1.0822780170697,1.12556156441892));
#149772=CARTESIAN_POINT('Ctrl Pts',(-8.93904928087935,1.31475831830307,
1.04765509721038));
#149773=CARTESIAN_POINT('Ctrl Pts',(-8.94757446448273,1.50385659890226,
0.973364631047322));
#149774=CARTESIAN_POINT('Ctrl Pts',(-8.95559065522704,1.69247211208388,
0.892970333219481));
#149775=CARTESIAN_POINT('',(-8.870419798,1.69247211199998,1.521726851));
#149776=CARTESIAN_POINT('Ctrl Pts',(-8.87041979790224,1.69247211200266,
1.52172685097689));
#149777=CARTESIAN_POINT('Ctrl Pts',(-8.88408033312625,1.50385659891321,
1.44209713160695));
#149778=CARTESIAN_POINT('Ctrl Pts',(-8.89562637401809,1.31475831840579,
1.36821586841046));
#149779=CARTESIAN_POINT('Ctrl Pts',(-8.90700321231731,1.08227801720866,
1.2905367252853));
#149780=CARTESIAN_POINT('Ctrl Pts',(-8.90890743024755,1.04120750311532,
1.27731473371655));
#149781=CARTESIAN_POINT('Ctrl Pts',(-8.91070977549335,1.00000000015644,
1.26461507856234));
#149782=CARTESIAN_POINT('',(-8.83949283668534,1.69247211210181,1.69214845452143));
#149783=CARTESIAN_POINT('Ctrl Pts',(-8.87041979787082,1.69247211192305,
1.52172685116002));
#149784=CARTESIAN_POINT('Ctrl Pts',(-8.87006004542175,1.69743933254887,
1.52382391295804));
#149785=CARTESIAN_POINT('Ctrl Pts',(-8.86965795845286,1.70224131077037,
1.52616334054193));
#149786=CARTESIAN_POINT('Ctrl Pts',(-8.86788175929939,1.72064855680533,
1.53646821838201));
#149787=CARTESIAN_POINT('Ctrl Pts',(-8.86620740447287,1.73230722820551,
1.54612242858823));
#149788=CARTESIAN_POINT('Ctrl Pts',(-8.86298306190944,1.74686546551234,
1.56447583615115));
#149789=CARTESIAN_POINT('Ctrl Pts',(-8.86156527650011,1.7515583365868,1.57249482759808));
#149790=CARTESIAN_POINT('Ctrl Pts',(-8.85852229936856,1.75781013627524,
1.5895451035149));
#149791=CARTESIAN_POINT('Ctrl Pts',(-8.85696462809229,1.75940739589114,
1.59820452506459));
#149792=CARTESIAN_POINT('Ctrl Pts',(-8.8553662973649,1.75940739589201,1.60701205331319));
#149793=CARTESIAN_POINT('Ctrl Pts',(-8.85361237719985,1.75940739589296,
1.61667695002995));
#149794=CARTESIAN_POINT('Ctrl Pts',(-8.85185955172326,1.75748289667319,
1.62624391302741));
#149795=CARTESIAN_POINT('Ctrl Pts',(-8.84830950960882,1.74964163105064,
1.6454553425064));
#149796=CARTESIAN_POINT('Ctrl Pts',(-8.84658873105369,1.74349822250871,
1.65467113326302));
#149797=CARTESIAN_POINT('Ctrl Pts',(-8.84313928061765,1.72630637166508,
1.6730198433628));
#149798=CARTESIAN_POINT('Ctrl Pts',(-8.8415467303671,1.71456563911397,1.68139676284533));
#149799=CARTESIAN_POINT('Ctrl Pts',(-8.84001693566233,1.69868853665975,
1.68940906182158));
#149800=CARTESIAN_POINT('Ctrl Pts',(-8.83974538685126,1.69560796575533,
1.69082917526325));
#149801=CARTESIAN_POINT('Ctrl Pts',(-8.83949283657224,1.69247211211698,
1.69214845453584));
#149802=CARTESIAN_POINT('Ctrl Pts',(-8.78687111482176,0.999999999979337,
1.94702234489257));
#149803=CARTESIAN_POINT('Ctrl Pts',(-8.78964603545235,1.04120750300605,
1.93449918613234));
#149804=CARTESIAN_POINT('Ctrl Pts',(-8.79250911518946,1.08227801716676,
1.92145120230824));
#149805=CARTESIAN_POINT('Ctrl Pts',(-8.80915221770156,1.31475831840232,
1.84472774523967));
#149806=CARTESIAN_POINT('Ctrl Pts',(-8.82430242745039,1.5038565988819,1.77150054228567));
#149807=CARTESIAN_POINT('Ctrl Pts',(-8.8394928366488,1.69247211194256,1.6921484541359));
#149808=CARTESIAN_POINT('',(-8.698303553,1.69247211199998,2.310739126));
#149809=CARTESIAN_POINT('Ctrl Pts',(-8.69830355259779,1.69247211209572,
2.31073912566189));
#149810=CARTESIAN_POINT('Ctrl Pts',(-8.71904704750919,1.5038565991313,2.23265449314007));
#149811=CARTESIAN_POINT('Ctrl Pts',(-8.7371692727865,1.31475831874758,2.16010563338117));
#149812=CARTESIAN_POINT('Ctrl Pts',(-8.75546341597935,1.08227801752857,
2.08375901557486));
#149813=CARTESIAN_POINT('Ctrl Pts',(-8.75854517828406,1.04120750328463,
2.07076094459201));
#149814=CARTESIAN_POINT('Ctrl Pts',(-8.76147865613757,1.00000000017415,
2.05827397545756));
#149815=CARTESIAN_POINT('',(-8.652224619,1.69247211199998,2.477702391));
#149816=CARTESIAN_POINT('Ctrl Pts',(-8.69830355250322,1.69247211193793,
2.31073912601786));
#149817=CARTESIAN_POINT('Ctrl Pts',(-8.69775726913674,1.69743933262653,
2.31279549771896));
#149818=CARTESIAN_POINT('Ctrl Pts',(-8.69714709617372,1.70224131090743,
2.31508946468109));
#149819=CARTESIAN_POINT('Ctrl Pts',(-8.69445432534047,1.72064855700242,
2.3251936408784));
#149820=CARTESIAN_POINT('Ctrl Pts',(-8.69192131424338,1.73230722840749,
2.33465889806517));
#149821=CARTESIAN_POINT('Ctrl Pts',(-8.6870647651655,1.74686546571993,2.35264939236907));
#149822=CARTESIAN_POINT('Ctrl Pts',(-8.68493387049238,1.75155833679612,
2.36050901241014));
#149823=CARTESIAN_POINT('Ctrl Pts',(-8.6803747685432,1.75781013648825,2.37721787856242));
#149824=CARTESIAN_POINT('Ctrl Pts',(-8.67804714343072,1.75940739610623,
2.38570281125057));
#149825=CARTESIAN_POINT('Ctrl Pts',(-8.67566574636791,1.75940739610916,
2.3943316097188));
#149826=CARTESIAN_POINT('Ctrl Pts',(-8.6730525323078,1.75940739611239,2.40380037821234));
#149827=CARTESIAN_POINT('Ctrl Pts',(-8.67044918724009,1.75748289689478,
2.41317170536637));
#149828=CARTESIAN_POINT('Ctrl Pts',(-8.6651913372909,1.74964163127651,2.43198757195745));
#149829=CARTESIAN_POINT('Ctrl Pts',(-8.66265138897058,1.7434982227376,2.44101201324904));
#149830=CARTESIAN_POINT('Ctrl Pts',(-8.65757105931702,1.72630637190226,
2.45897765048096));
#149831=CARTESIAN_POINT('Ctrl Pts',(-8.65523401893332,1.71456563935741,
2.46717809184323));
#149832=CARTESIAN_POINT('Ctrl Pts',(-8.65299216577076,1.6986885367743,2.47502100598598));
#149833=CARTESIAN_POINT('Ctrl Pts',(-8.65259441213127,1.69560796572895,
2.47641106107899));
#149834=CARTESIAN_POINT('Ctrl Pts',(-8.65222461924908,1.6924721119451,2.47770239093806));
#149835=CARTESIAN_POINT('Ctrl Pts',(-8.57696801773418,1.00000000004553,
2.72683325906904));
#149836=CARTESIAN_POINT('Ctrl Pts',(-8.58085433463339,1.0412075029207,2.71460925687145));
#149837=CARTESIAN_POINT('Ctrl Pts',(-8.58487550069146,1.08227801693089,
2.70187044492656));
#149838=CARTESIAN_POINT('Ctrl Pts',(-8.60832904062519,1.31475831807767,
2.62694773016632));
#149839=CARTESIAN_POINT('Ctrl Pts',(-8.62998229595736,1.50385659861581,
2.55537337269809));
#149840=CARTESIAN_POINT('Ctrl Pts',(-8.65222461938352,1.69247211173591,
2.47770239046857));
#149841=CARTESIAN_POINT('',(-8.456153681,1.69247211199998,3.081146689));
#149842=CARTESIAN_POINT('Ctrl Pts',(-8.45615368104301,1.69247211178115,
3.0811466895594));
#149843=CARTESIAN_POINT('Ctrl Pts',(-8.48381312126247,1.50385659874206,
3.00523583532452));
#149844=CARTESIAN_POINT('Ctrl Pts',(-8.50836562146029,1.31475831828408,
2.93460349966487));
#149845=CARTESIAN_POINT('Ctrl Pts',(-8.53342977587719,1.08227801706105,
2.86020410525441));
#149846=CARTESIAN_POINT('Ctrl Pts',(-8.53766427000695,1.04120750289092,
2.84753460775047));
#149847=CARTESIAN_POINT('Ctrl Pts',(-8.54170526181922,0.999999999854698,
2.83536086243177));
#149848=CARTESIAN_POINT('',(-8.395293776,1.69247211199998,3.243307326));
#149849=CARTESIAN_POINT('Ctrl Pts',(-8.45615368110477,1.6924721118584,3.08114668938989));
#149850=CARTESIAN_POINT('Ctrl Pts',(-8.45542526516038,1.69743933268664,
3.08314581432305));
#149851=CARTESIAN_POINT('Ctrl Pts',(-8.45461191894058,1.70224131109879,
3.08537585102182));
#149852=CARTESIAN_POINT('Ctrl Pts',(-8.45102425701389,1.7206485572912,3.09519797272739));
#149853=CARTESIAN_POINT('Ctrl Pts',(-8.44765298396237,1.7323072286751,3.10439806820338));
#149854=CARTESIAN_POINT('Ctrl Pts',(-8.44120333044821,1.74686546595974,
3.12188080035488));
#149855=CARTESIAN_POINT('Ctrl Pts',(-8.43837648322229,1.75155833702593,
3.12951776794704));
#149856=CARTESIAN_POINT('Ctrl Pts',(-8.432337963664,1.75781013670153,3.14575069436043));
#149857=CARTESIAN_POINT('Ctrl Pts',(-8.42925912538441,1.75940739631255,
3.15399282249319));
#149858=CARTESIAN_POINT('Ctrl Pts',(-8.42611383559583,1.75940739631059,
3.16237341716321));
#149859=CARTESIAN_POINT('Ctrl Pts',(-8.42266236770178,1.75940739630844,
3.17156982047769));
#149860=CARTESIAN_POINT('Ctrl Pts',(-8.41922946364508,1.75748289708497,
3.18067005937171));
#149861=CARTESIAN_POINT('Ctrl Pts',(-8.41230613897276,1.74964163145378,
3.19893886878414));
#149862=CARTESIAN_POINT('Ctrl Pts',(-8.40896747105482,1.74349822290597,
3.20769930111942));
#149863=CARTESIAN_POINT('Ctrl Pts',(-8.4022971660049,1.72630637204837,3.22513721674514));
#149864=CARTESIAN_POINT('Ctrl Pts',(-8.39923445196042,1.71456563948876,
3.23309515485905));
#149865=CARTESIAN_POINT('Ctrl Pts',(-8.39629859042414,1.69868853682826,
3.24070553759573));
#149866=CARTESIAN_POINT('Ctrl Pts',(-8.39577783443639,1.69560796571781,
3.24205434239871));
#149867=CARTESIAN_POINT('Ctrl Pts',(-8.39529377630737,1.69247211186687,
3.24330732578562));
#149868=CARTESIAN_POINT('Ctrl Pts',(-8.29800821684455,0.999999999902031,
3.48468931659343));
#149869=CARTESIAN_POINT('Ctrl Pts',(-8.30297463971393,1.04120750304222,
3.47286289132727));
#149870=CARTESIAN_POINT('Ctrl Pts',(-8.30812151607148,1.08227801731563,
3.4605358165655));
#149871=CARTESIAN_POINT('Ctrl Pts',(-8.33819665933031,1.3147583184983,3.38801707773433));
#149872=CARTESIAN_POINT('Ctrl Pts',(-8.36617862092732,1.50385659881755,
3.31867184053366));
#149873=CARTESIAN_POINT('Ctrl Pts',(-8.39529377643312,1.6924721117174,3.24330732546012));
#149874=CARTESIAN_POINT('',(-8.145919833,1.69247211199998,3.82674667));
#149875=CARTESIAN_POINT('Ctrl Pts',(-8.14591983253155,1.69247211163032,
3.82674667073341));
#149876=CARTESIAN_POINT('Ctrl Pts',(-8.18027252047733,1.50385659864394,
3.75362078440848));
#149877=CARTESIAN_POINT('Ctrl Pts',(-8.21105761327326,1.3147583182386,3.68547366293637));
#149878=CARTESIAN_POINT('Ctrl Pts',(-8.24268997705341,1.08227801715203,
3.61362051213516));
#149879=CARTESIAN_POINT('Ctrl Pts',(-8.24804310934497,1.04120750306483,
3.6013815954542));
#149880=CARTESIAN_POINT('Ctrl Pts',(-8.2531590794202,1.00000000011213,3.58961908978988));
#149881=CARTESIAN_POINT('',(-8.070768965,1.69247211199998,3.982799055));
#149882=CARTESIAN_POINT('Ctrl Pts',(-8.14591983282591,1.69247211192685,
3.82674667010681));
#149883=CARTESIAN_POINT('Ctrl Pts',(-8.14501514910682,1.69743933265066,
3.8286724524188));
#149884=CARTESIAN_POINT('Ctrl Pts',(-8.14400517824978,1.70224131096443,
3.8308206038134));
#149885=CARTESIAN_POINT('Ctrl Pts',(-8.1395515110169,1.72064855707352,3.84028158896135));
#149886=CARTESIAN_POINT('Ctrl Pts',(-8.13536911951964,1.73230722846371,
3.84914244897217));
#149887=CARTESIAN_POINT('Ctrl Pts',(-8.12737829038704,1.74686546575702,
3.86597665830253));
#149888=CARTESIAN_POINT('Ctrl Pts',(-8.12387825071991,1.75155833682648,
3.87332948507808));
#149889=CARTESIAN_POINT('Ctrl Pts',(-8.11640893216073,1.75781013650711,
3.88895577378552));
#149890=CARTESIAN_POINT('Ctrl Pts',(-8.11260366970907,1.75940739611999,
3.89688873659974));
#149891=CARTESIAN_POINT('Ctrl Pts',(-8.10871981121782,1.75940739611904,
3.90495365185858));
#149892=CARTESIAN_POINT('Ctrl Pts',(-8.10445787868249,1.75940739611799,
3.9138036459595));
#149893=CARTESIAN_POINT('Ctrl Pts',(-8.10022305536408,1.75748289689589,
3.92255952681936));
#149894=CARTESIAN_POINT('Ctrl Pts',(-8.09168999851364,1.74964163126793,
3.94013418933557));
#149895=CARTESIAN_POINT('Ctrl Pts',(-8.08757949199218,1.7434982227223,3.94856007886009));
#149896=CARTESIAN_POINT('Ctrl Pts',(-8.07937291692608,1.72630637186984,
3.96532987302821));
#149897=CARTESIAN_POINT('Ctrl Pts',(-8.0756091883959,1.71456563931326,3.97298123525238));
#149898=CARTESIAN_POINT('Ctrl Pts',(-8.07200295636026,1.69868853680513,
3.98029781215842));
#149899=CARTESIAN_POINT('Ctrl Pts',(-8.07136339088196,1.69560796585033,
3.98159450680377));
#149900=CARTESIAN_POINT('Ctrl Pts',(-8.07076896488867,1.69247211216003,
3.98279905536168));
#149901=CARTESIAN_POINT('Ctrl Pts',(-7.95223773338532,1.0000000000746,4.2144887034755));
#149902=CARTESIAN_POINT('Ctrl Pts',(-7.95824427546704,1.04120750308548,
4.20315507466545));
#149903=CARTESIAN_POINT('Ctrl Pts',(-7.96447542245755,1.08227801723047,
4.19133898755649));
#149904=CARTESIAN_POINT('Ctrl Pts',(-8.00093002168167,1.31475831851661,
4.12180810286586));
#149905=CARTESIAN_POINT('Ctrl Pts',(-8.03501539531451,1.50385659906093,
4.05525031280323));
#149906=CARTESIAN_POINT('Ctrl Pts',(-8.07076896486063,1.69247211218716,
3.9827990554185));
#149907=CARTESIAN_POINT('',(-7.770099827,1.69247211199998,4.541535938));
#149908=CARTESIAN_POINT('Ctrl Pts',(-7.77009982692731,1.69247211184426,
4.54153593837858));
#149909=CARTESIAN_POINT('Ctrl Pts',(-7.81086917503205,1.50385659862522,
4.47178378647429));
#149910=CARTESIAN_POINT('Ctrl Pts',(-7.84763899702609,1.31475831798858,
4.40667055962397));
#149911=CARTESIAN_POINT('Ctrl Pts',(-7.88558488501719,1.08227801676248,
4.33794217166716));
#149912=CARTESIAN_POINT('Ctrl Pts',(-7.89201355519076,1.04120750277453,
4.32623237637253));
#149913=CARTESIAN_POINT('Ctrl Pts',(-7.89816331274033,0.999999999921736,
4.31497581514458));
#149914=CARTESIAN_POINT('',(-7.681263067,1.69247211199998,4.69022363));
#149915=CARTESIAN_POINT('Ctrl Pts',(-7.77009982710407,1.69247211199432,
4.54153593807615));
#149916=CARTESIAN_POINT('Ctrl Pts',(-7.76902615958796,1.69743933266121,
4.54337287251751));
#149917=CARTESIAN_POINT('Ctrl Pts',(-7.7678276957807,1.70224131092097,4.54542184297812));
#149918=CARTESIAN_POINT('Ctrl Pts',(-7.76254388154537,1.72064855696673,
4.55444551730453));
#149919=CARTESIAN_POINT('Ctrl Pts',(-7.75758404575988,1.73230722834443,
4.56289579941125));
#149920=CARTESIAN_POINT('Ctrl Pts',(-7.74811637846733,1.74686546562209,
4.57894594675684));
#149921=CARTESIAN_POINT('Ctrl Pts',(-7.74397132662034,1.75155833668633,
4.58595543207489));
#149922=CARTESIAN_POINT('Ctrl Pts',(-7.73513134762144,1.7578101363574,4.60084926938084));
#149923=CARTESIAN_POINT('Ctrl Pts',(-7.73063029873371,1.75940739596569,
4.60840919532058));
#149924=CARTESIAN_POINT('Ctrl Pts',(-7.72603914208534,1.75940739596087,
4.61609349720791));
#149925=CARTESIAN_POINT('Ctrl Pts',(-7.72100105948176,1.75940739595559,
4.62452582714662));
#149926=CARTESIAN_POINT('Ctrl Pts',(-7.71599841320754,1.75748289672923,
4.63286685276749));
#149927=CARTESIAN_POINT('Ctrl Pts',(-7.70592432733087,1.7496416310923,4.6496058675405));
#149928=CARTESIAN_POINT('Ctrl Pts',(-7.70107507758455,1.74349822254042,
4.65762937394832));
#149929=CARTESIAN_POINT('Ctrl Pts',(-7.69139830701293,1.7263063716716,4.67359602614167));
#149930=CARTESIAN_POINT('Ctrl Pts',(-7.68696386732324,1.71456563910337,
4.68087920820852));
#149931=CARTESIAN_POINT('Ctrl Pts',(-7.68271630004147,1.6986885366654,4.68784307054307));
#149932=CARTESIAN_POINT('Ctrl Pts',(-7.68196307447331,1.69560796579605,
4.68907721483747));
#149933=CARTESIAN_POINT('Ctrl Pts',(-7.68126306658054,1.692472112194,4.69022363027454));
#149934=CARTESIAN_POINT('Ctrl Pts',(-7.54244050719113,0.999999999972252,
4.91035550601812));
#149935=CARTESIAN_POINT('Ctrl Pts',(-7.54943880738768,1.0412075031992,4.89960592529647));
#149936=CARTESIAN_POINT('Ctrl Pts',(-7.55670405553103,1.08227801755879,
4.88839596193518));
#149937=CARTESIAN_POINT('Ctrl Pts',(-7.59924459970585,1.31475831885198,
4.82241275323143));
#149938=CARTESIAN_POINT('Ctrl Pts',(-7.63915894989652,1.50385659919618,
4.75917829468802));
#149939=CARTESIAN_POINT('Ctrl Pts',(-7.6812630666695,1.69247211212086,4.69022363012885));
#149940=CARTESIAN_POINT('',(-7.331719547,1.69247211199998,5.219759428));
#149941=CARTESIAN_POINT('Ctrl Pts',(-7.33171954715669,1.69247211218445,
5.2197594275829));
#149942=CARTESIAN_POINT('Ctrl Pts',(-7.37857730449581,1.5038565990772,5.15394261357347));
#149943=CARTESIAN_POINT('Ctrl Pts',(-7.42103580661076,1.31475831855127,
5.09238753490903));
#149944=CARTESIAN_POINT('Ctrl Pts',(-7.46498970082048,1.08227801722486,
5.0273372703834));
#149945=CARTESIAN_POINT('Ctrl Pts',(-7.47244214905171,1.04120750302034,
5.01625087677696));
#149946=CARTESIAN_POINT('Ctrl Pts',(-7.47957617988741,0.999999999949514,
5.00559089111974));
#149947=CARTESIAN_POINT('',(-7.229912155,1.69247211199998,5.359885281));
#149948=CARTESIAN_POINT('Ctrl Pts',(-7.33171954712374,1.69247211216016,
5.21975942762917));
#149949=CARTESIAN_POINT('Ctrl Pts',(-7.33048554037461,1.69743933266442,
5.22149272425506));
#149950=CARTESIAN_POINT('Ctrl Pts',(-7.32910823297432,1.7022413107712,5.22342601663964));
#149951=CARTESIAN_POINT('Ctrl Pts',(-7.32303681394078,1.72064855669881,
5.23193972678211));
#149952=CARTESIAN_POINT('Ctrl Pts',(-7.31733946754655,1.73230722809749,
5.23991139428892));
#149953=CARTESIAN_POINT('Ctrl Pts',(-7.30647119017968,1.74686546540271,
5.25504825331498));
#149954=CARTESIAN_POINT('Ctrl Pts',(-7.30171449967183,1.75155833647675,
5.26165796092615));
#149955=CARTESIAN_POINT('Ctrl Pts',(-7.29157503454324,1.75781013616407,
5.27569943042096));
#149956=CARTESIAN_POINT('Ctrl Pts',(-7.2864144390166,1.75940739577924,5.2828254514138));
#149957=CARTESIAN_POINT('Ctrl Pts',(-7.28115294950206,1.7594073957793,5.29006727045672));
#149958=CARTESIAN_POINT('Ctrl Pts',(-7.27537928051152,1.75940739577936,
5.29801404407048));
#149959=CARTESIAN_POINT('Ctrl Pts',(-7.26964908964959,1.75748289655881,
5.30587305741947));
#149960=CARTESIAN_POINT('Ctrl Pts',(-7.25811508536945,1.74964163093469,
5.32164165174141));
#149961=CARTESIAN_POINT('Ctrl Pts',(-7.25256613571054,1.74349822239162,
5.32919817447285));
#149962=CARTESIAN_POINT('Ctrl Pts',(-7.24149708131024,1.72630637154491,
5.344233130587));
#149963=CARTESIAN_POINT('Ctrl Pts',(-7.23642763396645,1.71456563899138,
5.35108949259295));
#149964=CARTESIAN_POINT('Ctrl Pts',(-7.23157293031562,1.69868853650539,
5.3576445714967));
#149965=CARTESIAN_POINT('Ctrl Pts',(-7.23071210915307,1.69560796557039,
5.3588062288934));
#149966=CARTESIAN_POINT('Ctrl Pts',(-7.2299121553839,1.69247211190049,5.3598852809955));
#149967=CARTESIAN_POINT('Ctrl Pts',(-7.07191598531854,0.999999999848428,
5.56668701263113));
#149968=CARTESIAN_POINT('Ctrl Pts',(-7.0798496973723,1.04120750290071,5.55660802939234));
#149969=CARTESIAN_POINT('Ctrl Pts',(-7.08809055109799,1.08227801708678,
5.54609444591211));
#149970=CARTESIAN_POINT('Ctrl Pts',(-7.13637452878035,1.31475831838269,
5.48419017118036));
#149971=CARTESIAN_POINT('Ctrl Pts',(-7.18179648874699,1.50385659889642,
5.42478817067091));
#149972=CARTESIAN_POINT('Ctrl Pts',(-7.22991215525667,1.69247211199201,
5.35988528116712));
#149973=CARTESIAN_POINT('',(-6.834308572,1.69247211199998,5.855956484));
#149974=CARTESIAN_POINT('Ctrl Pts',(-6.83430857185789,1.69247211190127,
5.85595648418171));
#149975=CARTESIAN_POINT('Ctrl Pts',(-6.88687746734898,1.50385659885685,
5.79460492632121));
#149976=CARTESIAN_POINT('Ctrl Pts',(-6.93468279871554,1.31475831839393,
5.73710360111202));
#149977=CARTESIAN_POINT('Ctrl Pts',(-6.98429080820646,1.08227801718584,
5.67625520655512));
#149978=CARTESIAN_POINT('Ctrl Pts',(-6.99270703172362,1.04120750303555,
5.66588147583171));
#149979=CARTESIAN_POINT('Ctrl Pts',(-7.0007678967871,1.00000000001932,5.65590389374812));
#149980=CARTESIAN_POINT('',(-6.720350242,1.69247211199998,5.986392288));
#149981=CARTESIAN_POINT('Ctrl Pts',(-6.83430857189648,1.69247211192666,
5.85595648413667));
#149982=CARTESIAN_POINT('Ctrl Pts',(-6.83292416134052,1.69743933264486,
5.85757218755852));
#149983=CARTESIAN_POINT('Ctrl Pts',(-6.83137909952495,1.70224131095344,
5.85937423625886));
#149984=CARTESIAN_POINT('Ctrl Pts',(-6.8245689590756,1.72064855706262,5.86730943498249));
#149985=CARTESIAN_POINT('Ctrl Pts',(-6.81817997375611,1.73230722845714,
5.87473830470638));
#149986=CARTESIAN_POINT('Ctrl Pts',(-6.80599859129646,1.74686546575595,
5.88884000231499));
#149987=CARTESIAN_POINT('Ctrl Pts',(-6.80066856020434,1.75155833682738,
5.89499671473559));
#149988=CARTESIAN_POINT('Ctrl Pts',(-6.78931124596147,1.75781013651137,
5.90807276275261));
#149989=CARTESIAN_POINT('Ctrl Pts',(-6.78353265387896,1.75940739612577,
5.91470750426196));
#149990=CARTESIAN_POINT('Ctrl Pts',(-6.77764319392101,1.75940739612599,
5.92144853358502));
#149991=CARTESIAN_POINT('Ctrl Pts',(-6.77118042472805,1.75940739612624,
5.92884576812757));
#149992=CARTESIAN_POINT('Ctrl Pts',(-6.76476882540304,1.75748289690549,
5.93615949305174));
#149993=CARTESIAN_POINT('Ctrl Pts',(-6.75186776773317,1.74964163128042,
5.95083070747797));
#149994=CARTESIAN_POINT('Ctrl Pts',(-6.74566379503781,1.7434982227368,5.95785940585847));
#149995=CARTESIAN_POINT('Ctrl Pts',(-6.73329157831984,1.72630637188949,
5.97184161327271));
#149996=CARTESIAN_POINT('Ctrl Pts',(-6.72762793952884,1.71456563933646,
5.97821595182398));
#149997=CARTESIAN_POINT('Ctrl Pts',(-6.72220518672269,1.69868853678518,
5.98430946965148));
#149998=CARTESIAN_POINT('Ctrl Pts',(-6.72124370078741,1.69560796578166,
5.98538928716463));
#149999=CARTESIAN_POINT('Ctrl Pts',(-6.72035024189579,1.69247211204104,
5.98639228803552));
#150000=CARTESIAN_POINT('Ctrl Pts',(-6.54445255413051,0.999999999900246,
6.17819882868257));
#150001=CARTESIAN_POINT('Ctrl Pts',(-6.553257800479,1.04120750293032,6.16887159293748));
#150002=CARTESIAN_POINT('Ctrl Pts',(-6.56240790930224,1.08227801709433,
6.15913903849141));
#150003=CARTESIAN_POINT('Ctrl Pts',(-6.6160465662733,1.31475831833009,6.1018121145769));
#150004=CARTESIAN_POINT('Ctrl Pts',(-6.66661042504181,1.5038565988065,6.04672084217141));
#150005=CARTESIAN_POINT('Ctrl Pts',(-6.72035024216997,1.69247211186447,
5.98639228772773));
#150006=CARTESIAN_POINT('',(-6.281871763,1.69247211199998,6.445004822));
#150007=CARTESIAN_POINT('Ctrl Pts',(-6.28187176315731,1.69247211214928,
6.44500482166204));
#150008=CARTESIAN_POINT('Ctrl Pts',(-6.33972854297823,1.50385659908023,
6.38861248658687));
#150009=CARTESIAN_POINT('Ctrl Pts',(-6.39249580318892,1.31475831859254,
6.33562788166308));
#150010=CARTESIAN_POINT('Ctrl Pts',(-6.44735851345535,1.08227801735199,
6.27947127252895));
#150011=CARTESIAN_POINT('Ctrl Pts',(-6.45667074978434,1.04120750319416,
6.26989372785291));
#150012=CARTESIAN_POINT('Ctrl Pts',(-6.46559354773797,1.00000000017037,
6.26067888295264));
#150013=CARTESIAN_POINT('',(-6.15668002,1.69247211199998,6.564700384));
#150014=CARTESIAN_POINT('Ctrl Pts',(-6.28187176296278,1.69247211203293,
6.44500482185164));
#150015=CARTESIAN_POINT('Ctrl Pts',(-6.28034809508384,1.6974393328171,6.44648992333557));
#150016=CARTESIAN_POINT('Ctrl Pts',(-6.27864771881356,1.70224131118792,
6.44814621926317));
#150017=CARTESIAN_POINT('Ctrl Pts',(-6.27115368823422,1.7206485573528,6.4554390169499));
#150018=CARTESIAN_POINT('Ctrl Pts',(-6.26412450434296,1.73230722874671,
6.46226527600062));
#150019=CARTESIAN_POINT('Ctrl Pts',(-6.25072809411952,1.74686546604397,
6.47521827361669));
#150020=CARTESIAN_POINT('Ctrl Pts',(-6.24486763671978,1.75155833711437,
6.4808724206194));
#150021=CARTESIAN_POINT('Ctrl Pts',(-6.23238391577944,1.7578101367976,6.49287776651093));
#150022=CARTESIAN_POINT('Ctrl Pts',(-6.22603385296701,1.75940739641221,
6.4989678095005));
#150023=CARTESIAN_POINT('Ctrl Pts',(-6.21956384103444,1.75940739641324,
6.50515377430057));
#150024=CARTESIAN_POINT('Ctrl Pts',(-6.21246400605726,1.75940739641437,
6.51194191158887));
#150025=CARTESIAN_POINT('Ctrl Pts',(-6.20542262069756,1.75748289719422,
6.51865146227563));
#150026=CARTESIAN_POINT('Ctrl Pts',(-6.19125838137018,1.74964163157005,
6.53210717281416));
#150027=CARTESIAN_POINT('Ctrl Pts',(-6.18444933637955,1.74349822302714,
6.53855145589715));
#150028=CARTESIAN_POINT('Ctrl Pts',(-6.17087357116009,1.72630637218225,
6.55136833809903));
#150029=CARTESIAN_POINT('Ctrl Pts',(-6.16466134121213,1.71456563963167,
6.55720933076995));
#150030=CARTESIAN_POINT('Ctrl Pts',(-6.15871420003383,1.69868853693743,
6.56279222612325));
#150031=CARTESIAN_POINT('Ctrl Pts',(-6.15765979061543,1.69560796578235,
6.56378150971813));
#150032=CARTESIAN_POINT('Ctrl Pts',(-6.15668002018172,1.69247211188529,
6.56470038380239));
#150033=CARTESIAN_POINT('Ctrl Pts',(-5.96429703930701,0.999999999993485,
6.73996742031544));
#150034=CARTESIAN_POINT('Ctrl Pts',(-5.97390292527018,1.0412075029378,6.73146702949199));
#150035=CARTESIAN_POINT('Ctrl Pts',(-5.98388861787978,1.08227801701665,
6.72259386489691));
#150036=CARTESIAN_POINT('Ctrl Pts',(-6.04245008719923,1.31475831813608,
6.67030585448667));
#150037=CARTESIAN_POINT('Ctrl Pts',(-6.09774873431316,1.50385659858127,
6.61996887270678));
#150038=CARTESIAN_POINT('Ctrl Pts',(-6.15668002065362,1.69247211160818,
6.56470038335982));
#150039=CARTESIAN_POINT('',(-5.678857015,1.69247211199998,6.982161771));
#150040=CARTESIAN_POINT('Ctrl Pts',(-5.67885701527804,1.69247211202244,
6.98216177125877));
#150041=CARTESIAN_POINT('Ctrl Pts',(-5.74153585071579,1.50385659882619,
6.93118269686947));
#150042=CARTESIAN_POINT('Ctrl Pts',(-5.79884018886956,1.31475831821191,
6.88314141309412));
#150043=CARTESIAN_POINT('Ctrl Pts',(-5.85851587764468,1.08227801691581,
6.83212872938778));
#150044=CARTESIAN_POINT('Ctrl Pts',(-5.86864915011615,1.04120750283384,
6.82342448353686));
#150045=CARTESIAN_POINT('Ctrl Pts',(-5.87836203982082,0.999999999886375,
6.81504656835106));
#150046=CARTESIAN_POINT('',(-5.54343983025804,1.69247211212479,7.09015337246985));
#150047=CARTESIAN_POINT('Ctrl Pts',(-5.678857014964,1.69247211184902,6.98216177151419));
#150048=CARTESIAN_POINT('Ctrl Pts',(-5.67720635746448,1.69743933258059,
6.98350431387102));
#150049=CARTESIAN_POINT('Ctrl Pts',(-5.67536435720179,1.70224131090145,
6.98500152147185));
#150050=CARTESIAN_POINT('Ctrl Pts',(-5.66724677406058,1.72064855700654,
6.99159320075996));
#150051=CARTESIAN_POINT('Ctrl Pts',(-5.65963398645598,1.73230722838665,
6.99776188810862));
#150052=CARTESIAN_POINT('Ctrl Pts',(-5.64513040849174,1.74686546566723,
7.00946189580316));
#150053=CARTESIAN_POINT('Ctrl Pts',(-5.63878670974102,1.75155833673249,
7.01456795351953));
#150054=CARTESIAN_POINT('Ctrl Pts',(-5.62527709368239,1.75781013640549,
7.02540593729718));
#150055=CARTESIAN_POINT('Ctrl Pts',(-5.61840668711161,1.75940739601474,
7.03090224832023));
#150056=CARTESIAN_POINT('Ctrl Pts',(-5.61140821593638,1.75940739601077,
7.03648334284404));
#150057=CARTESIAN_POINT('Ctrl Pts',(-5.60372847887256,1.75940739600641,
7.04260772878464));
#150058=CARTESIAN_POINT('Ctrl Pts',(-5.5961140005745,1.75748289678097,7.04865908387313));
#150059=CARTESIAN_POINT('Ctrl Pts',(-5.58080062171541,1.74964163114594,
7.06079095305035));
#150060=CARTESIAN_POINT('Ctrl Pts',(-5.57344132685396,1.7434982225954,7.06659893525709));
#150061=CARTESIAN_POINT('Ctrl Pts',(-5.55877131720445,1.7263063717301,7.0781472982493));
#150062=CARTESIAN_POINT('Ctrl Pts',(-5.55206051331798,1.71456563916442,
7.08340791680299));
#150063=CARTESIAN_POINT('Ctrl Pts',(-5.54563686680511,1.69868853671578,
7.08843523935246));
#150064=CARTESIAN_POINT('Ctrl Pts',(-5.54449802352356,1.69560796583262,
7.08932602377848));
#150065=CARTESIAN_POINT('Ctrl Pts',(-5.54343983019798,1.69247211221631,
7.09015337273988));
#150066=CARTESIAN_POINT('Ctrl Pts',(-5.33612051021732,1.00000000003863,
7.24746975850456));
#150067=CARTESIAN_POINT('Ctrl Pts',(-5.34644969490053,1.04120750312078,
7.23986465271198));
#150068=CARTESIAN_POINT('Ctrl Pts',(-5.35719057242631,1.08227801733654,
7.23192231942854));
#150069=CARTESIAN_POINT('Ctrl Pts',(-5.42020335165464,1.3147583185972,7.18509421478981));
#150070=CARTESIAN_POINT('Ctrl Pts',(-5.47979155494116,1.50385659904842,
7.13991680741592));
#150071=CARTESIAN_POINT('Ctrl Pts',(-5.54343983044598,1.69247211208145,
7.09015337254597));
#150072=CARTESIAN_POINT('',(-5.030119452,1.69247211199998,7.463102458));
#150073=CARTESIAN_POINT('Ctrl Pts',(-5.03011945219446,1.69247211210034,
7.46310245786931));
#150074=CARTESIAN_POINT('Ctrl Pts',(-5.09711568993067,1.50385659918751,
7.41794709780784));
#150075=CARTESIAN_POINT('Ctrl Pts',(-5.15849572502523,1.31475831885526,
7.3752359354521));
#150076=CARTESIAN_POINT('Ctrl Pts',(-5.22250391870522,1.08227801764803,
7.3297779013181));
#150077=CARTESIAN_POINT('Ctrl Pts',(-5.23337664023476,1.04120750336251,
7.32201703570376));
#150078=CARTESIAN_POINT('Ctrl Pts',(-5.24380141927541,1.00000000021015,
7.31454350422535));
#150079=CARTESIAN_POINT('',(-4.885567124,1.69247211199998,7.558520614));
#150080=CARTESIAN_POINT('Ctrl Pts',(-5.03011945218954,1.69247211209782,
7.46310245787263));
#150081=CARTESIAN_POINT('Ctrl Pts',(-5.02835509520953,1.69743933274048,
7.46429163173374));
#150082=CARTESIAN_POINT('Ctrl Pts',(-5.0263863016777,1.70224131097822,7.46561769636424));
#150083=CARTESIAN_POINT('Ctrl Pts',(-5.01771052400477,1.72064855704174,
7.47145518492245));
#150084=CARTESIAN_POINT('Ctrl Pts',(-5.00957542636928,1.73230722845448,
7.4769166339361));
#150085=CARTESIAN_POINT('Ctrl Pts',(-4.99408145493217,1.74686546577658,
7.4872694501465));
#150086=CARTESIAN_POINT('Ctrl Pts',(-4.98730559056024,1.75155833685606,
7.49178630760795));
#150087=CARTESIAN_POINT('Ctrl Pts',(-4.97287885086278,1.75781013655407,
7.50136966821127));
#150088=CARTESIAN_POINT('Ctrl Pts',(-4.96554341700394,1.7594073961748,7.50622799421013));
#150089=CARTESIAN_POINT('Ctrl Pts',(-4.95807283415526,1.75940739618001,
7.51115928277464));
#150090=CARTESIAN_POINT('Ctrl Pts',(-4.94987502773368,1.75940739618573,
7.51657060741686));
#150091=CARTESIAN_POINT('Ctrl Pts',(-4.94174876379914,1.75748289697065,
7.52191504495915));
#150092=CARTESIAN_POINT('Ctrl Pts',(-4.92540953973939,1.74964163135777,
7.53262539410137));
#150093=CARTESIAN_POINT('Ctrl Pts',(-4.91755924773008,1.74349822282263,
7.53775031297301));
#150094=CARTESIAN_POINT('Ctrl Pts',(-4.90191310796274,1.72630637199696,
7.54793717612114));
#150095=CARTESIAN_POINT('Ctrl Pts',(-4.89475776159462,1.71456563945895,
7.55257506514706));
#150096=CARTESIAN_POINT('Ctrl Pts',(-4.88790932897337,1.69868853680129,
7.55700633800827));
#150097=CARTESIAN_POINT('Ctrl Pts',(-4.88669522094921,1.69560796567097,
7.55779145133232));
#150098=CARTESIAN_POINT('Ctrl Pts',(-4.88556712453283,1.69247211179938,
7.55852061396171));
#150099=CARTESIAN_POINT('Ctrl Pts',(-4.66498067898464,0.999999999967121,
7.69661972977099));
#150100=CARTESIAN_POINT('Ctrl Pts',(-4.67594999777918,1.04120750284047,
7.68997114090538));
#150101=CARTESIAN_POINT('Ctrl Pts',(-4.6873595808967,1.08227801684883,7.68302358599243));
#150102=CARTESIAN_POINT('Ctrl Pts',(-4.75431632809316,1.31475831803052,
7.6420324195285));
#150103=CARTESIAN_POINT('Ctrl Pts',(-4.81771431840041,1.50385659860426,
7.60237832843866));
#150104=CARTESIAN_POINT('Ctrl Pts',(-4.88556712461049,1.69247211175979,
7.55852061391151));
#150105=CARTESIAN_POINT('',(-4.340882323,1.69247211199998,7.883954633));
#150106=CARTESIAN_POINT('Ctrl Pts',(-4.34088232282825,1.69247211188109,
7.88395463326351));
#150107=CARTESIAN_POINT('Ctrl Pts',(-4.41165654866182,1.50385659901075,
7.84498655187241));
#150108=CARTESIAN_POINT('Ctrl Pts',(-4.47661808484275,1.31475831872082,
7.80794939604147));
#150109=CARTESIAN_POINT('Ctrl Pts',(-4.54444342707815,1.08227801765357,
7.76841201286517));
#150110=CARTESIAN_POINT('Ctrl Pts',(-4.55596805683155,1.04120750346539,
7.76165701347468));
#150111=CARTESIAN_POINT('Ctrl Pts',(-4.56702079094976,1.00000000041108,
7.75514803824096));
#150112=CARTESIAN_POINT('',(-4.188358703,1.69247211199998,7.966031093));
#150113=CARTESIAN_POINT('Ctrl Pts',(-4.34088232285577,1.69247211189453,
7.88395463324836));
#150114=CARTESIAN_POINT('Ctrl Pts',(-4.33901847194055,1.69743933251756,
7.88498086410162));
#150115=CARTESIAN_POINT('Ctrl Pts',(-4.33693873668265,1.70224131073674,
7.88612510909012));
#150116=CARTESIAN_POINT('Ctrl Pts',(-4.32777461670888,1.72064855678309,
7.89116140691491));
#150117=CARTESIAN_POINT('Ctrl Pts',(-4.3191827080702,1.73230722819562,7.89587164520933));
#150118=CARTESIAN_POINT('Ctrl Pts',(-4.30282309151686,1.74686546551824,
7.90479391513174));
#150119=CARTESIAN_POINT('Ctrl Pts',(-4.29566961680086,1.7515583365982,7.9086852052531));
#150120=CARTESIAN_POINT('Ctrl Pts',(-4.28044190909274,1.75781013629619,
7.91693678308731));
#150121=CARTESIAN_POINT('Ctrl Pts',(-4.27270050854822,1.75940739591639,
7.92111800767207));
#150122=CARTESIAN_POINT('Ctrl Pts',(-4.26481796277002,1.75940739592062,
7.92535978643457));
#150123=CARTESIAN_POINT('Ctrl Pts',(-4.25616809090657,1.75940739592527,
7.93001448097122));
#150124=CARTESIAN_POINT('Ctrl Pts',(-4.24759546923469,1.75748289670936,
7.93460897069478));
#150125=CARTESIAN_POINT('Ctrl Pts',(-4.23036195379282,1.74964163109505,
7.94381156636528));
#150126=CARTESIAN_POINT('Ctrl Pts',(-4.22208387056523,1.74349822255881,
7.94821215906904));
#150127=CARTESIAN_POINT('Ctrl Pts',(-4.20558757418278,1.72630637172989,
7.95695550374437));
#150128=CARTESIAN_POINT('Ctrl Pts',(-4.19804529596738,1.71456563918893,
7.96093332168898));
#150129=CARTESIAN_POINT('Ctrl Pts',(-4.19082721695447,1.69868853668133,
7.96473286674421));
#150130=CARTESIAN_POINT('Ctrl Pts',(-4.18954761961682,1.69560796571051,
7.96540598759677));
#150131=CARTESIAN_POINT('Ctrl Pts',(-4.18835870300193,1.69247211200357,
7.96603109302167));
#150132=CARTESIAN_POINT('Ctrl Pts',(-3.95628116469446,1.00000000003948,
8.08380104566434));
#150133=CARTESIAN_POINT('Ctrl Pts',(-3.96780229915045,1.04120750292555,
8.07816250421748));
#150134=CARTESIAN_POINT('Ctrl Pts',(-3.97978872466481,1.08227801694657,
8.07226566526221));
#150135=CARTESIAN_POINT('Ctrl Pts',(-4.05015034350906,1.31475831811704,
8.03744147373218));
#150136=CARTESIAN_POINT('Ctrl Pts',(-4.11684767745441,1.50385659866781,
8.00362997039905));
#150137=CARTESIAN_POINT('Ctrl Pts',(-4.18835870342248,1.69247211180005,
7.96603109280055));
#150138=CARTESIAN_POINT('',(-3.61669496163465,1.69247211178013,8.24132984144472));
#150139=CARTESIAN_POINT('Ctrl Pts',(-3.61669496156912,1.69247211175992,
8.24132984141277));
#150140=CARTESIAN_POINT('Ctrl Pts',(-3.69067734322808,1.5038565985687,8.20886278668499));
#150141=CARTESIAN_POINT('Ctrl Pts',(-3.75869734856277,1.3147583179601,8.17779783869765));
#150142=CARTESIAN_POINT('Ctrl Pts',(-3.82979374964924,1.08227801680555,
8.14449943819061));
#150143=CARTESIAN_POINT('Ctrl Pts',(-3.84187749804066,1.04120750286064,
8.13880469232044));
#150144=CARTESIAN_POINT('Ctrl Pts',(-3.85346919708018,1.00000000005117,
8.13331267978517));
#150145=CARTESIAN_POINT('',(-3.45742808,1.69247211199998,8.309403774));
#150146=CARTESIAN_POINT('Ctrl Pts',(-3.61669496113721,1.69247211155784,
8.24132984160231));
#150147=CARTESIAN_POINT('Ctrl Pts',(-3.61474662287773,1.69743933229287,
8.24218486685928));
#150148=CARTESIAN_POINT('Ctrl Pts',(-3.61257269064703,1.702241310617,8.24313807944231));
#150149=CARTESIAN_POINT('Ctrl Pts',(-3.60299401241552,1.72064855672633,
8.24733263725374));
#150150=CARTESIAN_POINT('Ctrl Pts',(-3.59401446977586,1.73230722810795,
8.25125374075691));
#150151=CARTESIAN_POINT('Ctrl Pts',(-3.57692092613147,1.74686546539135,
8.25867362751413));
#150152=CARTESIAN_POINT('Ctrl Pts',(-3.56944743664773,1.75155833645782,
8.26190801991309));
#150153=CARTESIAN_POINT('Ctrl Pts',(-3.55354136548706,1.75781013613199,
8.2687613781201));
#150154=CARTESIAN_POINT('Ctrl Pts',(-3.54545632746744,1.75940739574123,
8.2722318365261));
#150155=CARTESIAN_POINT('Ctrl Pts',(-3.53722528439024,1.75940739573665,
8.27574995317466));
#150156=CARTESIAN_POINT('Ctrl Pts',(-3.52819299076565,1.75940739573161,
8.27961054074264));
#150157=CARTESIAN_POINT('Ctrl Pts',(-3.51924303306519,1.75748289650574,
8.28341809051765));
#150158=CARTESIAN_POINT('Ctrl Pts',(-3.50125398036883,1.74964163087026,
8.29103883882883));
#150159=CARTESIAN_POINT('Ctrl Pts',(-3.49261475617683,1.74349822231932,
8.29467967438141));
#150160=CARTESIAN_POINT('Ctrl Pts',(-3.47540112164682,1.72630637145233,
8.3019091043172));
#150161=CARTESIAN_POINT('Ctrl Pts',(-3.46753263756868,1.71456563888475,
8.30519482413073));
#150162=CARTESIAN_POINT('Ctrl Pts',(-3.46000302790207,1.69868853650819,
8.30833204968783));
#150163=CARTESIAN_POINT('Ctrl Pts',(-3.45866824382614,1.69560796570203,
8.30888775850462));
#150164=CARTESIAN_POINT('Ctrl Pts',(-3.45742807947873,1.69247211216521,
8.30940377375128));
#150165=CARTESIAN_POINT('Ctrl Pts',(-3.21572799916628,1.00000000027708,
8.40589634931207));
#150166=CARTESIAN_POINT('Ctrl Pts',(-3.22770818794205,1.04120750338201,
8.40131325348498));
#150167=CARTESIAN_POINT('Ctrl Pts',(-3.24017494826639,1.08227801762046,
8.39651460834608));
#150168=CARTESIAN_POINT('Ctrl Pts',(-3.31337492842116,1.31475831887219,
8.36813777565844));
#150169=CARTESIAN_POINT('Ctrl Pts',(-3.3828345982506,1.50385659929336,8.34044109045195));
#150170=CARTESIAN_POINT('Ctrl Pts',(-3.45742807919782,1.69247211229553,
8.30940377386816));
#150171=CARTESIAN_POINT('',(-2.8633881,1.69247211199998,8.532350707));
#150172=CARTESIAN_POINT('Ctrl Pts',(-2.86338810042523,1.69247211217985,
8.53235070694725));
#150173=CARTESIAN_POINT('Ctrl Pts',(-2.93998297503229,1.50385659913088,
8.50664608461793));
#150174=CARTESIAN_POINT('Ctrl Pts',(-3.01051379221962,1.31475831866339,
8.48180346126633));
#150175=CARTESIAN_POINT('Ctrl Pts',(-3.08430882573711,1.08227801739708,
8.45501214257094));
#150176=CARTESIAN_POINT('Ctrl Pts',(-3.09685440167008,1.04120750319233,
8.45042350089905));
#150177=CARTESIAN_POINT('Ctrl Pts',(-3.10889173621482,1.00000000012129,
8.44599266945545));
#150178=CARTESIAN_POINT('',(-2.698660279,1.69247211199998,8.585874021));
#150179=CARTESIAN_POINT('Ctrl Pts',(-2.86338809984566,1.69247211191797,
8.53235070714175));
#150180=CARTESIAN_POINT('Ctrl Pts',(-2.86137096114923,1.6974393326637,8.53302764262381));
#150181=CARTESIAN_POINT('Ctrl Pts',(-2.85912033521171,1.70224131099841,
8.53378214807124));
#150182=CARTESIAN_POINT('Ctrl Pts',(-2.84920422065495,1.72064855713849,
8.53710119373168));
#150183=CARTESIAN_POINT('Ctrl Pts',(-2.83990934200021,1.73230722853934,
8.54020159203125));
#150184=CARTESIAN_POINT('Ctrl Pts',(-2.82221949840695,1.746865465846,8.54605935507156));
#150185=CARTESIAN_POINT('Ctrl Pts',(-2.81448616629377,1.75155833692005,
8.54861080832648));
#150186=CARTESIAN_POINT('Ctrl Pts',(-2.79802979800297,1.75781013660889,
8.55401076770457));
#150187=CARTESIAN_POINT('Ctrl Pts',(-2.78966621847436,1.75940739622565,
8.55674251784626));
#150188=CARTESIAN_POINT('Ctrl Pts',(-2.78115294960864,1.7594073962279,8.55950864658032));
#150189=CARTESIAN_POINT('Ctrl Pts',(-2.77181095693984,1.75940739623038,
8.56254404400076));
#150190=CARTESIAN_POINT('Ctrl Pts',(-2.76255572300507,1.75748289701186,
8.56553399767844));
#150191=CARTESIAN_POINT('Ctrl Pts',(-2.74395597033505,1.74964163139145,
8.57151154084736));
#150192=CARTESIAN_POINT('Ctrl Pts',(-2.73502516313974,1.74349822285107,
8.57436330538032));
#150193=CARTESIAN_POINT('Ctrl Pts',(-2.71723278454767,1.7263063720123,8.58002061345238));
#150194=CARTESIAN_POINT('Ctrl Pts',(-2.70910144702474,1.71456563946539,
8.58258778044829));
#150195=CARTESIAN_POINT('Ctrl Pts',(-2.7013209304805,1.69868853681972,8.58503742749617));
#150196=CARTESIAN_POINT('Ctrl Pts',(-2.69994170637387,1.69560796571128,
8.58547125010984));
#150197=CARTESIAN_POINT('Ctrl Pts',(-2.69866027920764,1.69247211186234,
8.58587402058911));
#150198=CARTESIAN_POINT('Ctrl Pts',(-2.44928368492693,1.00000000003541,
8.66031231715986));
#150199=CARTESIAN_POINT('Ctrl Pts',(-2.46162647047221,1.04120750294047,
8.65682156738601));
#150200=CARTESIAN_POINT('Ctrl Pts',(-2.47447319045865,1.08227801698034,
8.65315975197741));
#150201=CARTESIAN_POINT('Ctrl Pts',(-2.54992216866384,1.31475831816348,
8.63145875170902));
#150202=CARTESIAN_POINT('Ctrl Pts',(-2.62158492606628,1.50385659870848,
8.61009988199061));
#150203=CARTESIAN_POINT('Ctrl Pts',(-2.69866027926731,1.69247211183557,
8.58587402057035));
#150204=CARTESIAN_POINT('',(-2.08702692,1.69247211199998,8.754674102));
#150205=CARTESIAN_POINT('Ctrl Pts',(-2.08702692043405,1.69247211217429,
8.75467410206591));
#150206=CARTESIAN_POINT('Ctrl Pts',(-2.1656175912421,1.50385659900165,8.73593887060451));
#150207=CARTESIAN_POINT('Ctrl Pts',(-2.2380913477429,1.31475831841118,8.71751859004947));
#150208=CARTESIAN_POINT('Ctrl Pts',(-2.31399085943843,1.08227801716552,
8.69745006113723));
#150209=CARTESIAN_POINT('Ctrl Pts',(-2.32689725319462,1.04120750310917,
8.69400446875687));
#150210=CARTESIAN_POINT('Ctrl Pts',(-2.33928330559696,1.00000000018754,
8.69067049289958));
#150211=CARTESIAN_POINT('',(-1.918164453,1.69247211199998,8.793215858));
#150212=CARTESIAN_POINT('Ctrl Pts',(-2.08702692043181,1.69247211217334,
8.75467410206645));
#150213=CARTESIAN_POINT('Ctrl Pts',(-2.08495722210436,1.69743933294414,
8.75516749748885));
#150214=CARTESIAN_POINT('Ctrl Pts',(-2.08264802316623,1.70224131130219,
8.75571722096838));
#150215=CARTESIAN_POINT('Ctrl Pts',(-2.0724743109975,1.72064855744848,8.7581340314743));
#150216=CARTESIAN_POINT('Ctrl Pts',(-2.06293893323256,1.73230722883563,
8.76038876198234));
#150217=CARTESIAN_POINT('Ctrl Pts',(-2.044795217923,1.74686546612392,8.76463723803522));
#150218=CARTESIAN_POINT('Ctrl Pts',(-2.03686430742723,1.75155833719122,
8.76648520934269));
#150219=CARTESIAN_POINT('Ctrl Pts',(-2.01999013901601,1.75781013686931,
8.77038829258981));
#150220=CARTESIAN_POINT('Ctrl Pts',(-2.01141535660801,1.75940739648177,
8.77235934001888));
#150221=CARTESIAN_POINT('Ctrl Pts',(-2.00268840579558,1.75940739648129,
8.77435120959334));
#150222=CARTESIAN_POINT('Ctrl Pts',(-1.99311193031393,1.75940739648077,
8.7765369776299));
#150223=CARTESIAN_POINT('Ctrl Pts',(-1.98362593784728,1.75748289725882,
8.7786852618597));
#150224=CARTESIAN_POINT('Ctrl Pts',(-1.96456523947057,1.74964163163066,
8.78297147222287));
#150225=CARTESIAN_POINT('Ctrl Pts',(-1.95541475487495,1.743498223085,8.7850112050058));
#150226=CARTESIAN_POINT('Ctrl Pts',(-1.93718688597779,1.72630637223327,
8.78905084189893));
#150227=CARTESIAN_POINT('Ctrl Pts',(-1.92885816375222,1.71456563967816,
8.79087878675951));
#150228=CARTESIAN_POINT('Ctrl Pts',(-1.92088938462464,1.69868853704812,
8.79262113211973));
#150229=CARTESIAN_POINT('Ctrl Pts',(-1.91947682532086,1.69560796596479,
8.79292957559287));
#150230=CARTESIAN_POINT('Ctrl Pts',(-1.91816445274598,1.69247211214182,
8.79321585838888));
#150231=CARTESIAN_POINT('Ctrl Pts',(-1.66311917827957,0.999999999892244,
8.84500054261382));
#150232=CARTESIAN_POINT('Ctrl Pts',(-1.67572518383153,1.04120750292225,
8.84263024433131));
#150233=CARTESIAN_POINT('Ctrl Pts',(-1.6888484293412,1.0822780170862,8.84013474140826));
#150234=CARTESIAN_POINT('Ctrl Pts',(-1.76593893483276,1.31475831833986,
8.82528429724149));
#150235=CARTESIAN_POINT('Ctrl Pts',(-1.83922779333879,1.50385659883379,
8.81043521210152));
#150236=CARTESIAN_POINT('Ctrl Pts',(-1.91816445327559,1.6924721119096,8.79321585827335));
#150237=CARTESIAN_POINT('',(-1.293862227,1.69247211199998,8.906510009));
#150238=CARTESIAN_POINT('Ctrl Pts',(-1.29386222704835,1.69247211203085,
8.9065100088316));
#150239=CARTESIAN_POINT('Ctrl Pts',(-1.37381592810969,1.50385659888228,
8.89489501332681));
#150240=CARTESIAN_POINT('Ctrl Pts',(-1.44764910778166,1.31475831831576,
8.88304538485746));
#150241=CARTESIAN_POINT('Ctrl Pts',(-1.52504199941119,1.08227801709192,
8.86986122572234));
#150242=CARTESIAN_POINT('Ctrl Pts',(-1.53820529634083,1.04120750303301,
8.86758642450121));
#150243=CARTESIAN_POINT('Ctrl Pts',(-1.55084034142984,1.0000000001088,8.86537614742848));
#150244=CARTESIAN_POINT('',(-1.12222469370069,1.69247211186443,8.92975989245309));
#150245=CARTESIAN_POINT('Ctrl Pts',(-1.29386222678592,1.69247211191724,
8.90651000886973));
#150246=CARTESIAN_POINT('Ctrl Pts',(-1.29175663284455,1.69743933264429,
8.90681589169734));
#150247=CARTESIAN_POINT('Ctrl Pts',(-1.28940745324758,1.70224131096107,
8.90715640715207));
#150248=CARTESIAN_POINT('Ctrl Pts',(-1.27905805625228,1.72064855707096,
8.90865152375763));
#150249=CARTESIAN_POINT('Ctrl Pts',(-1.26935895263151,1.73230722845912,
8.9100424327097));
#150250=CARTESIAN_POINT('Ctrl Pts',(-1.25090744812926,1.74686546574981,
8.91264741554435));
#150251=CARTESIAN_POINT('Ctrl Pts',(-1.24284281427572,1.75155833681844,
8.91377702612638));
#150252=CARTESIAN_POINT('Ctrl Pts',(-1.22568670661819,1.75781013649756,
8.9161518079123));
#150253=CARTESIAN_POINT('Ctrl Pts',(-1.21696976043267,1.75940739610974,
8.91734628291441));
#150254=CARTESIAN_POINT('Ctrl Pts',(-1.20809939194526,1.75940739610823,
8.91854785596744));
#150255=CARTESIAN_POINT('Ctrl Pts',(-1.19836553780408,1.75940739610657,
8.91986639609967));
#150256=CARTESIAN_POINT('Ctrl Pts',(-1.18872516244254,1.75748289688385,
8.92115571415885));
#150257=CARTESIAN_POINT('Ctrl Pts',(-1.1693569839014,1.74964163125455,8.92371608166787));
#150258=CARTESIAN_POINT('Ctrl Pts',(-1.1600604962301,1.743498222708,8.92492735997031));
#150259=CARTESIAN_POINT('Ctrl Pts',(-1.14154389711404,1.72630637185313,
8.92731680090106));
#150260=CARTESIAN_POINT('Ctrl Pts',(-1.13308484816047,1.71456563929489,
8.92839080608825));
#150261=CARTESIAN_POINT('Ctrl Pts',(-1.12499196639287,1.69868853672591,
8.92941182141991));
#150262=CARTESIAN_POINT('Ctrl Pts',(-1.12355744500622,1.69560796570946,
8.92959240234686));
#150263=CARTESIAN_POINT('Ctrl Pts',(-1.12222469348958,1.69247211195553,
8.92975989247876));
#150264=CARTESIAN_POINT('Ctrl Pts',(-0.863564213439779,0.999999999851497,
8.95847402459069));
#150265=CARTESIAN_POINT('Ctrl Pts',(-0.87633194283773,1.04120750294903,
8.95724326205628));
#150266=CARTESIAN_POINT('Ctrl Pts',(-0.889626053196569,1.08227801718005,
8.95593416395052));
#150267=CARTESIAN_POINT('Ctrl Pts',(-0.967737398493407,1.31475831834263,
8.94805384294514));
#150268=CARTESIAN_POINT('Ctrl Pts',(-1.04206227925682,1.503856598683,8.93983409849227));
#150269=CARTESIAN_POINT('Ctrl Pts',(-1.12222469430304,1.69247211160434,
8.92975989237653));
#150270=CARTESIAN_POINT('',(-0.490280117,1.69247211199998,8.986635934));
#150271=CARTESIAN_POINT('Ctrl Pts',(-0.490280116634963,1.69247211184778,
8.98663593383155));
#150272=CARTESIAN_POINT('Ctrl Pts',(-0.570953107639294,1.50385659894552,
8.98223469139443));
#150273=CARTESIAN_POINT('Ctrl Pts',(-0.645551249023955,1.31475831862389,
8.97705112125193));
#150274=CARTESIAN_POINT('Ctrl Pts',(-0.723814398508996,1.08227801747435,
8.97085748298641));
#150275=CARTESIAN_POINT('Ctrl Pts',(-0.737128615539831,1.04120750323641,
8.96977178828106));
#150276=CARTESIAN_POINT('Ctrl Pts',(-0.749910923411969,1.00000000013195,
8.96870300583911));
#150277=CARTESIAN_POINT('',(-0.317249442999998,1.69247211199998,8.99440675));
#150278=CARTESIAN_POINT('Ctrl Pts',(-0.490280117042471,1.6924721120226,
8.98663593380932));
#150279=CARTESIAN_POINT('Ctrl Pts',(-0.488155580485669,1.69743933273219,
8.98675184125671));
#150280=CARTESIAN_POINT('Ctrl Pts',(-0.485785334434531,1.70224131103289,
8.98688040706055));
#150281=CARTESIAN_POINT('Ctrl Pts',(-0.475343579860209,1.72064855714573,
8.98744179197277));
#150282=CARTESIAN_POINT('Ctrl Pts',(-0.465558841857883,1.73230722855105,
8.98795768059026));
#150283=CARTESIAN_POINT('Ctrl Pts',(-0.446948108818774,1.74686546586347,
8.98889819642085));
#150284=CARTESIAN_POINT('Ctrl Pts',(-0.438814683296168,1.75155833693935,
8.98930035131872));
#150285=CARTESIAN_POINT('Ctrl Pts',(-0.421514767281583,1.75781013663146,
8.99012771129987));
#150286=CARTESIAN_POINT('Ctrl Pts',(-0.412725841042246,1.75940739624973,
8.99053599666622));
#150287=CARTESIAN_POINT('Ctrl Pts',(-0.4037834738688,1.7594073962532,8.99093759883976));
#150288=CARTESIAN_POINT('Ctrl Pts',(-0.393970612336493,1.75940739625701,
8.99137829496011));
#150289=CARTESIAN_POINT('Ctrl Pts',(-0.384253472711392,1.75748289703985,
8.99179826602012));
#150290=CARTESIAN_POINT('Ctrl Pts',(-0.364733755191153,1.74964163142237,
8.9926121761055));
#150291=CARTESIAN_POINT('Ctrl Pts',(-0.355366114298903,1.74349822288404,
8.99298524742859));
#150292=CARTESIAN_POINT('Ctrl Pts',(-0.33670986974061,1.72630637205049,
8.99370525402672));
#150293=CARTESIAN_POINT('Ctrl Pts',(-0.328188601351913,1.71456563950727,
8.99401667228356));
#150294=CARTESIAN_POINT('Ctrl Pts',(-0.320036776042561,1.69868853696225,
8.99430813697986));
#150295=CARTESIAN_POINT('Ctrl Pts',(-0.318591842470321,1.69560796595495,
8.99435940143549));
#150296=CARTESIAN_POINT('Ctrl Pts',(-0.31724944252187,1.69247211221038,
8.99440675037657));
#150297=CARTESIAN_POINT('Ctrl Pts',(-0.0570563382849726,0.999999999911669,
8.99981914119731));
#150298=CARTESIAN_POINT('Ctrl Pts',(-0.0698829932121865,1.04120750284218,
8.99973782378958));
#150299=CARTESIAN_POINT('Ctrl Pts',(-0.0832409319874672,1.08227801690732,
8.99962567059222));
#150300=CARTESIAN_POINT('Ctrl Pts',(-0.161744210525077,1.31475831815756,
8.99877892044582));
#150301=CARTESIAN_POINT('Ctrl Pts',(-0.236506693492214,1.50385659874335,
8.9972546972045));
#150302=CARTESIAN_POINT('Ctrl Pts',(-0.317249443220438,1.69247211191093,
8.99440675035193));
#150303=CARTESIAN_POINT('',(0.317249442,1.69247211199998,8.99440675));
#150304=CARTESIAN_POINT('Ctrl Pts',(0.3172494417691,1.69247211210491,8.99440675040312));
#150305=CARTESIAN_POINT('Ctrl Pts',(0.236506691980429,1.50385659883905,
8.99725469724477));
#150306=CARTESIAN_POINT('Ctrl Pts',(0.161744208956719,1.3147583181561,8.99877892047435));
#150307=CARTESIAN_POINT('Ctrl Pts',(0.0832409304009244,1.08227801689511,
8.99962567060685));
#150308=CARTESIAN_POINT('Ctrl Pts',(0.0698829916511325,1.0412075029195,
8.99973782380167));
#150309=CARTESIAN_POINT('Ctrl Pts',(0.0570563367470327,1.00000000007913,
8.99981914120706));
#150310=CARTESIAN_POINT('',(0.490280117,1.69247211199998,8.986635934));
#150311=CARTESIAN_POINT('Ctrl Pts',(0.317249442367011,1.69247211184862,
8.99440675038203));
#150312=CARTESIAN_POINT('Ctrl Pts',(0.319375816065644,1.69743933266916,
8.99433174922977));
#150313=CARTESIAN_POINT('Ctrl Pts',(0.321748044801427,1.70224131107395,
8.99424733024544));
#150314=CARTESIAN_POINT('Ctrl Pts',(0.33219808615543,1.72064855725431,8.99387046351945));
#150315=CARTESIAN_POINT('Ctrl Pts',(0.34198967757272,1.73230722863321,8.99350717816731));
#150316=CARTESIAN_POINT('Ctrl Pts',(0.360609796449283,1.74686546591159,
8.99277565450731));
#150317=CARTESIAN_POINT('Ctrl Pts',(0.368746528075233,1.75155833697567,
8.99244711580377));
#150318=CARTESIAN_POINT('Ctrl Pts',(0.386050963682271,1.75781013664747,
8.99172039255882));
#150319=CARTESIAN_POINT('Ctrl Pts',(0.394841106701611,1.75940739625667,
8.99133920101302));
#150320=CARTESIAN_POINT('Ctrl Pts',(0.403783473868802,1.7594073962532,8.99093759883976));
#150321=CARTESIAN_POINT('Ctrl Pts',(0.413596335402248,1.75940739624939,
8.99049690271936));
#150322=CARTESIAN_POINT('Ctrl Pts',(0.423312002595504,1.75748289702423,
8.99004414541729));
#150323=CARTESIAN_POINT('Ctrl Pts',(0.44282609781397,1.74964163138951,8.98910504494812));
#150324=CARTESIAN_POINT('Ctrl Pts',(0.452189469197952,1.74349822283924,
8.98863690553838));
#150325=CARTESIAN_POINT('Ctrl Pts',(0.470835150104622,1.72630637197519,
8.98768168072916));
#150326=CARTESIAN_POINT('Ctrl Pts',(0.479350029693807,1.71456563941102,
8.98722800469669));
#150327=CARTESIAN_POINT('Ctrl Pts',(0.487495164855629,1.69868853682224,
8.98678757205289));
#150328=CARTESIAN_POINT('Ctrl Pts',(0.488938876868529,1.69560796579137,
8.98670910728539));
#150329=CARTESIAN_POINT('Ctrl Pts',(0.490280117042474,1.6924721120226,8.98663593380932));
#150330=CARTESIAN_POINT('Ctrl Pts',(0.749910923055971,1.00000000002074,
8.96870300586887));
#150331=CARTESIAN_POINT('Ctrl Pts',(0.737128615170063,1.04120750317642,
8.96977178831147));
#150332=CARTESIAN_POINT('Ctrl Pts',(0.723814398124095,1.08227801746521,
8.97085748301749));
#150333=CARTESIAN_POINT('Ctrl Pts',(0.645551248646327,1.31475831860558,
8.97705112127892));
#150334=CARTESIAN_POINT('Ctrl Pts',(0.570953107291636,1.503856598869,8.98223469141624));
#150335=CARTESIAN_POINT('Ctrl Pts',(0.490280116319866,1.69247211171261,
8.98663593384874));
#150336=CARTESIAN_POINT('',(1.122224693,1.69247211199998,8.929759892));
#150337=CARTESIAN_POINT('Ctrl Pts',(1.12222469326036,1.69247211191644,8.92975989250757));
#150338=CARTESIAN_POINT('Ctrl Pts',(1.04206227819181,1.50385659894457,8.9398340986166));
#150339=CARTESIAN_POINT('Ctrl Pts',(0.967737397408283,1.31475831855362,
8.94805384306261));
#150340=CARTESIAN_POINT('Ctrl Pts',(0.889626052114518,1.08227801739532,
8.95593416405797));
#150341=CARTESIAN_POINT('Ctrl Pts',(0.876331941773366,1.04120750322035,
8.95724326216039));
#150342=CARTESIAN_POINT('Ctrl Pts',(0.863564212391513,1.00000000017931,
8.95847402469174));
#150343=CARTESIAN_POINT('',(1.293862227,1.69247211199998,8.906510009));
#150344=CARTESIAN_POINT('Ctrl Pts',(1.12222469343999,1.69247211183887,8.92975989248499));
#150345=CARTESIAN_POINT('Ctrl Pts',(1.12433578390216,1.69743933257241,8.92949458660048));
#150346=CARTESIAN_POINT('Ctrl Pts',(1.12669089544509,1.70224131089559,8.9291978625228));
#150347=CARTESIAN_POINT('Ctrl Pts',(1.13706508588633,1.72064855702352,8.92788577847361));
#150348=CARTESIAN_POINT('Ctrl Pts',(1.14678469459136,1.73230722842326,8.92664624411455));
#150349=CARTESIAN_POINT('Ctrl Pts',(1.16526428107704,1.74686546572888,8.92424857076722));
#150350=CARTESIAN_POINT('Ctrl Pts',(1.17333880663464,1.75155833680264,8.92319198366484));
#150351=CARTESIAN_POINT('Ctrl Pts',(1.19050843670975,1.75781013649061,8.92091702834642));
#150352=CARTESIAN_POINT('Ctrl Pts',(1.19922902345515,1.75940739610672,8.91974942902085));
#150353=CARTESIAN_POINT('Ctrl Pts',(1.20809939194526,1.75940739610823,8.91854785596745));
#150354=CARTESIAN_POINT('Ctrl Pts',(1.21783324608598,1.75940739610989,8.91722931583528));
#150355=CARTESIAN_POINT('Ctrl Pts',(1.2274692160072,1.75748289689063,8.91590747550959));
#150356=CARTESIAN_POINT('Ctrl Pts',(1.24682057289392,1.74964163126884,8.91322292557665));
#150357=CARTESIAN_POINT('Ctrl Pts',(1.25610428640085,1.74349822272749,8.91191734462038));
#150358=CARTESIAN_POINT('Ctrl Pts',(1.27458927957878,1.72630637188588,8.90929457931835));
#150359=CARTESIAN_POINT('Ctrl Pts',(1.2830292135571,1.71456563933674,8.90807946173197));
#150360=CARTESIAN_POINT('Ctrl Pts',(1.29110207873021,1.69868853674836,8.90691067785349));
#150361=CARTESIAN_POINT('Ctrl Pts',(1.29253294526349,1.69560796570205,8.906703115614));
#150362=CARTESIAN_POINT('Ctrl Pts',(1.29386222678592,1.69247211191724,8.90651000886973));
#150363=CARTESIAN_POINT('Ctrl Pts',(1.5508403410948,1.00000000000293,8.86537614748709));
#150364=CARTESIAN_POINT('Ctrl Pts',(1.53820529599185,1.04120750297962,8.86758642456177));
#150365=CARTESIAN_POINT('Ctrl Pts',(1.52504199904688,1.08227801709064,8.869861225785));
#150366=CARTESIAN_POINT('Ctrl Pts',(1.44764910742439,1.31475831830606,8.88304538491551));
#150367=CARTESIAN_POINT('Ctrl Pts',(1.37381592778245,1.50385659881392,8.89489501337705));
#150368=CARTESIAN_POINT('Ctrl Pts',(1.29386222675378,1.69247211190334,8.9065100088744));
#150369=CARTESIAN_POINT('',(1.918164453,1.69247211199998,8.793215858));
#150370=CARTESIAN_POINT('Ctrl Pts',(1.91816445274452,1.69247211214243,8.7932158583892));
#150371=CARTESIAN_POINT('Ctrl Pts',(1.8392277928231,1.50385659907754,8.81043521220902));
#150372=CARTESIAN_POINT('Ctrl Pts',(1.76593893433233,1.31475831859373,8.82528429734154));
#150373=CARTESIAN_POINT('Ctrl Pts',(1.68884842884387,1.08227801731721,8.84013474150329));
#150374=CARTESIAN_POINT('Ctrl Pts',(1.67572518332552,1.04120750311924,8.84263024442721));
#150375=CARTESIAN_POINT('Ctrl Pts',(1.66311917776566,1.00000000005502,8.84500054271045));
#150376=CARTESIAN_POINT('',(2.08702692,1.69247211199998,8.754674102));
#150377=CARTESIAN_POINT('Ctrl Pts',(1.91816445274599,1.69247211214183,8.79321585838888));
#150378=CARTESIAN_POINT('Ctrl Pts',(1.92024326275655,1.69743933291712,8.79276238385459));
#150379=CARTESIAN_POINT('Ctrl Pts',(1.92256229518959,1.70224131127949,8.79225574372561));
#150380=CARTESIAN_POINT('Ctrl Pts',(1.93277710790527,1.72064855743365,8.79001900647378));
#150381=CARTESIAN_POINT('Ctrl Pts',(1.94234647731936,1.73230722882441,8.78791320310791));
#150382=CARTESIAN_POINT('Ctrl Pts',(1.96053674463815,1.74686546611737,8.78386868472646));
#150383=CARTESIAN_POINT('Ctrl Pts',(1.96848405279004,1.75155833718626,8.7820925562423));
#150384=CARTESIAN_POINT('Ctrl Pts',(1.9853806375546,1.75781013686712,8.77828768545105));
#150385=CARTESIAN_POINT('Ctrl Pts',(1.99396145498231,1.75940739648082,8.77634307916798));
#150386=CARTESIAN_POINT('Ctrl Pts',(2.00268840579558,1.75940739648129,8.77435120959334));
#150387=CARTESIAN_POINT('Ctrl Pts',(2.01226488127708,1.75940739648181,8.77216544155681));
#150388=CARTESIAN_POINT('Ctrl Pts',(2.0217435707649,1.75748289726097,8.7699851608862));
#150389=CARTESIAN_POINT('Ctrl Pts',(2.04077638358101,1.74964163163515,8.76557677590213));
#150390=CARTESIAN_POINT('Ctrl Pts',(2.04990569221387,1.7434982230911,8.76344426516706));
#150391=CARTESIAN_POINT('Ctrl Pts',(2.06808116737671,1.72630637224354,8.75917507633169));
#150392=CARTESIAN_POINT('Ctrl Pts',(2.07637820236166,1.71456563969128,8.75720830060181));
#150393=CARTESIAN_POINT('Ctrl Pts',(2.08431379958806,1.69868853706913,8.75532057584465));
#150394=CARTESIAN_POINT('Ctrl Pts',(2.08572030015038,1.69560796599098,8.7549855872994));
#150395=CARTESIAN_POINT('Ctrl Pts',(2.08702692043182,1.69247211217333,8.75467410206645));
#150396=CARTESIAN_POINT('Ctrl Pts',(2.33928330456152,0.999999999853761,
8.69067049317829));
#150397=CARTESIAN_POINT('Ctrl Pts',(2.32689725212173,1.04120750291753,8.69400446904408));
#150398=CARTESIAN_POINT('Ctrl Pts',(2.31399085832436,1.08227801711502,8.6974500614337));
#150399=CARTESIAN_POINT('Ctrl Pts',(2.23809134664659,1.31475831833215,8.71751859033044));
#150400=CARTESIAN_POINT('Ctrl Pts',(2.1656175902253,1.50385659875802,8.73593887085572));
#150401=CARTESIAN_POINT('Ctrl Pts',(2.08702691950425,1.69247211176485,8.75467410228757));
#150402=CARTESIAN_POINT('',(2.698660279,1.69247211199998,8.585874021));
#150403=CARTESIAN_POINT('Ctrl Pts',(2.69866027953189,1.69247211171677,8.58587402048719));
#150404=CARTESIAN_POINT('Ctrl Pts',(2.62158492637212,1.50385659866213,8.61009988189709));
#150405=CARTESIAN_POINT('Ctrl Pts',(2.54992216900827,1.3147583181889,8.63145875160704));
#150406=CARTESIAN_POINT('Ctrl Pts',(2.47447319081348,1.0822780170125,8.65315975187598));
#150407=CARTESIAN_POINT('Ctrl Pts',(2.46162647080814,1.04120750290523,8.65682156729051));
#150408=CARTESIAN_POINT('Ctrl Pts',(2.44928368524565,0.999999999932307,
8.66031231706972));
#150409=CARTESIAN_POINT('',(2.8633881,1.69247211199998,8.532350707));
#150410=CARTESIAN_POINT('Ctrl Pts',(2.69866027920764,1.69247211186232,8.58587402058911));
#150411=CARTESIAN_POINT('Ctrl Pts',(2.70069007140366,1.69743933265977,8.585236028515));
#150412=CARTESIAN_POINT('Ctrl Pts',(2.70295435323217,1.70224131104288,8.58452355150266));
#150413=CARTESIAN_POINT('Ctrl Pts',(2.7129275445438,1.7206485572087,8.58138016994169));
#150414=CARTESIAN_POINT('Ctrl Pts',(2.72226962772913,1.73230722859253,8.57842505226086));
#150415=CARTESIAN_POINT('Ctrl Pts',(2.74002411854311,1.74686546587729,8.57276625293123));
#150416=CARTESIAN_POINT('Ctrl Pts',(2.7477802222385,1.75155833694366,8.57028488340791));
#150417=CARTESIAN_POINT('Ctrl Pts',(2.76426772033127,1.7578101366193,8.56498073172689));
#150418=CARTESIAN_POINT('Ctrl Pts',(2.77263968074679,1.75940739623017,8.56227477531312));
#150419=CARTESIAN_POINT('Ctrl Pts',(2.78115294960864,1.75940739622791,8.55950864658032));
#150420=CARTESIAN_POINT('Ctrl Pts',(2.79049494227812,1.75940739622543,8.55647324915966));
#150421=CARTESIAN_POINT('Ctrl Pts',(2.79974003449488,1.7574828970017,8.5534520824834));
#150422=CARTESIAN_POINT('Ctrl Pts',(2.81830106221836,1.7496416313701,8.54735535617396));
#150423=CARTESIAN_POINT('Ctrl Pts',(2.82720246215092,1.74349822282198,8.54441308538322));
#150424=CARTESIAN_POINT('Ctrl Pts',(2.84492208106079,1.72630637196337,8.53853184601318));
#150425=CARTESIAN_POINT('Ctrl Pts',(2.85300941420689,1.71456563940287,8.53582924746147));
#150426=CARTESIAN_POINT('Ctrl Pts',(2.86074385070299,1.69868853678567,8.53323778068015));
#150427=CARTESIAN_POINT('Ctrl Pts',(2.86211466095963,1.69560796572133,8.53277806296399));
#150428=CARTESIAN_POINT('Ctrl Pts',(2.86338809984566,1.69247211191798,8.53235070714175));
#150429=CARTESIAN_POINT('Ctrl Pts',(3.1088917354371,1.00000000015544,8.44599266974173));
#150430=CARTESIAN_POINT('Ctrl Pts',(3.09685440089955,1.04120750319919,8.45042350118141));
#150431=CARTESIAN_POINT('Ctrl Pts',(3.08430882497446,1.08227801737684,8.45501214284914));
#150432=CARTESIAN_POINT('Ctrl Pts',(3.01051379149163,1.31475831853189,8.4818034615245));
#150433=CARTESIAN_POINT('Ctrl Pts',(2.93998297433824,1.50385659891702,8.5066460848574));
#150434=CARTESIAN_POINT('Ctrl Pts',(2.86338809976884,1.69247211188328,8.53235070716753));
#150435=CARTESIAN_POINT('',(3.45742808,1.69247211199998,8.309403774));
#150436=CARTESIAN_POINT('Ctrl Pts',(3.45742807951293,1.69247211214934,8.30940377373705));
#150437=CARTESIAN_POINT('Ctrl Pts',(3.38283459860251,1.50385659921542,8.34044109030884));
#150438=CARTESIAN_POINT('Ctrl Pts',(3.31337492880746,1.31475831886194,8.36813777550527));
#150439=CARTESIAN_POINT('Ctrl Pts',(3.24017494866242,1.08227801761983,8.39651460819329));
#150440=CARTESIAN_POINT('Ctrl Pts',(3.22770818832162,1.04120750332116,8.40131325333918));
#150441=CARTESIAN_POINT('Ctrl Pts',(3.21572799953086,1.00000000015557,8.4058963491726));
#150442=CARTESIAN_POINT('',(3.616694961,1.69247211199998,8.241329842));
#150443=CARTESIAN_POINT('Ctrl Pts',(3.45742807947874,1.69247211216523,8.30940377375128));
#150444=CARTESIAN_POINT('Ctrl Pts',(3.45939251105716,1.69743933261944,8.30858640091872));
#150445=CARTESIAN_POINT('Ctrl Pts',(3.46158381147327,1.70224131067939,8.30767382352641));
#150446=CARTESIAN_POINT('Ctrl Pts',(3.47123508293627,1.72064855658321,8.30364910638722));
#150447=CARTESIAN_POINT('Ctrl Pts',(3.48027466293952,1.73230722799961,8.29986846725986));
#150448=CARTESIAN_POINT('Ctrl Pts',(3.49745042854423,1.74686546532776,8.29264094830292));
#150449=CARTESIAN_POINT('Ctrl Pts',(3.5049528802026,1.75155833640984,8.28947431626728));
#150450=CARTESIAN_POINT('Ctrl Pts',(3.52089854399714,1.75781013611086,8.28271358960318));
#150451=CARTESIAN_POINT('Ctrl Pts',(3.52899424130546,1.75940739573206,8.27926806982646));
#150452=CARTESIAN_POINT('Ctrl Pts',(3.53722528439024,1.75940739573665,8.27574995317466));
#150453=CARTESIAN_POINT('Ctrl Pts',(3.54625757801351,1.75940739574168,8.27188936560725));
#150454=CARTESIAN_POINT('Ctrl Pts',(3.55519463691193,1.75748289652636,8.26805163758463));
#150455=CARTESIAN_POINT('Ctrl Pts',(3.57313443705392,1.74964163091365,8.26031565721045));
#150456=CARTESIAN_POINT('Ctrl Pts',(3.58173625944175,1.74349822237847,8.25658731580187));
#150457=CARTESIAN_POINT('Ctrl Pts',(3.59885735413302,1.72630637155177,8.24914137818544));
#150458=CARTESIAN_POINT('Ctrl Pts',(3.60666987098365,1.71456563901184,8.24572471654921));
#150459=CARTESIAN_POINT('Ctrl Pts',(3.61414087354956,1.6986885365718,8.24245037274111));
#150460=CARTESIAN_POINT('Ctrl Pts',(3.61546495648722,1.69560796567022,8.24186962725645));
#150461=CARTESIAN_POINT('Ctrl Pts',(3.61669496095015,1.69247211203475,8.2413298416844));
#150462=CARTESIAN_POINT('Ctrl Pts',(3.85346919584842,0.999999999908194,
8.13331268036877));
#150463=CARTESIAN_POINT('Ctrl Pts',(3.84187749678661,1.04120750281033,8.13880469291244));
#150464=CARTESIAN_POINT('Ctrl Pts',(3.82979374837064,1.08227801684729,8.1444994387919));
#150465=CARTESIAN_POINT('Ctrl Pts',(3.75869734727944,1.31475831804487,8.17779783928727));
#150466=CARTESIAN_POINT('Ctrl Pts',(3.69067734197139,1.50385659860643,8.20886278724963));
#150467=CARTESIAN_POINT('Ctrl Pts',(3.61669496034055,1.69247211174959,8.24132984195192));
#150468=CARTESIAN_POINT('',(4.188358703,1.69247211199998,7.966031093));
#150469=CARTESIAN_POINT('Ctrl Pts',(4.18835870309452,1.69247211195877,7.96603109297299));
#150470=CARTESIAN_POINT('Ctrl Pts',(4.11684767709352,1.50385659876227,8.00362997058505));
#150471=CARTESIAN_POINT('Ctrl Pts',(4.05015034311738,1.31475831814771,8.03744147392976));
#150472=CARTESIAN_POINT('Ctrl Pts',(3.97978872423844,1.08227801688172,8.07226566547244));
#150473=CARTESIAN_POINT('Ctrl Pts',(3.96780229871458,1.04120750283049,8.07816250443158));
#150474=CARTESIAN_POINT('Ctrl Pts',(3.95628116424985,0.999999999913974,
8.08380104588194));
#150475=CARTESIAN_POINT('',(4.340882323,1.69247211199998,7.883954633));
#150476=CARTESIAN_POINT('Ctrl Pts',(4.18835870300193,1.69247211200357,7.96603109302167));
#150477=CARTESIAN_POINT('Ctrl Pts',(4.19024195767693,1.69743933264773,7.96504092037285));
#150478=CARTESIAN_POINT('Ctrl Pts',(4.19234263382752,1.7022413108861,7.96393559005549));
#150479=CARTESIAN_POINT('Ctrl Pts',(4.20159427933326,1.72064855691514,7.95906194189284));
#150480=CARTESIAN_POINT('Ctrl Pts',(4.21025857475967,1.7323072282956,7.95448622080495));
#150481=CARTESIAN_POINT('Ctrl Pts',(4.22671732596282,1.74686546557696,7.94574817396074));
#150482=CARTESIAN_POINT('Ctrl Pts',(4.23390572024393,1.7515583366425,7.94192177527461));
#150483=CARTESIAN_POINT('Ctrl Pts',(4.24918116460586,1.75781013631569,7.93375890702995));
#150484=CARTESIAN_POINT('Ctrl Pts',(4.25693541699853,1.75940739592486,7.92960156519345));
#150485=CARTESIAN_POINT('Ctrl Pts',(4.26481796277002,1.75940739592063,7.92535978643457));
#150486=CARTESIAN_POINT('Ctrl Pts',(4.27346783463467,1.75940739591598,7.92070509189727));
#150487=CARTESIAN_POINT('Ctrl Pts',(4.28202490427402,1.75748289669031,7.91608170165456));
#150488=CARTESIAN_POINT('Ctrl Pts',(4.29919903612614,1.74964163105498,7.90676875277056));
#150489=CARTESIAN_POINT('Ctrl Pts',(4.30743202416367,1.7434982225042,7.90228435915017));
#150490=CARTESIAN_POINT('Ctrl Pts',(4.32381674566998,1.72630637163806,7.8933336735851));
#150491=CARTESIAN_POINT('Ctrl Pts',(4.33129154444121,1.71456563907157,7.88923045780917));
#150492=CARTESIAN_POINT('Ctrl Pts',(4.33843896105432,1.69868853654903,7.88529960002584));
#150493=CARTESIAN_POINT('Ctrl Pts',(4.33970565601871,1.69560796558959,7.88460250256148));
#150494=CARTESIAN_POINT('Ctrl Pts',(4.34088232285577,1.69247211189454,7.88395463324836));
#150495=CARTESIAN_POINT('Ctrl Pts',(4.56702079088812,0.999999999926177,
7.75514803827727));
#150496=CARTESIAN_POINT('Ctrl Pts',(4.55596805673791,1.04120750310877,7.7616570135297));
#150497=CARTESIAN_POINT('Ctrl Pts',(4.54444342694939,1.08227801742429,7.76841201294058));
#150498=CARTESIAN_POINT('Ctrl Pts',(4.47661808467104,1.31475831862242,7.80794939613996));
#150499=CARTESIAN_POINT('Ctrl Pts',(4.41165654848376,1.50385659891625,7.84498655197261));
#150500=CARTESIAN_POINT('Ctrl Pts',(4.34088232264359,1.69247211179079,7.88395463336519));
#150501=CARTESIAN_POINT('',(4.885567124,1.69247211199998,7.558520614));
#150502=CARTESIAN_POINT('Ctrl Pts',(4.88556712448749,1.69247211182252,7.55852061399102));
#150503=CARTESIAN_POINT('Ctrl Pts',(4.81771431823801,1.50385659859261,7.60237832854207));
#150504=CARTESIAN_POINT('Ctrl Pts',(4.75431632789338,1.31475831794536,7.64203241965308));
#150505=CARTESIAN_POINT('Ctrl Pts',(4.68735958066341,1.08227801668198,7.68302358613477));
#150506=CARTESIAN_POINT('Ctrl Pts',(4.67594999754258,1.0412075026676,7.68997114104926));
#150507=CARTESIAN_POINT('Ctrl Pts',(4.66498067874495,0.999999999788169,
7.69661972991627));
#150508=CARTESIAN_POINT('',(5.030119452,1.69247211199998,7.463102458));
#150509=CARTESIAN_POINT('Ctrl Pts',(4.88556712453282,1.69247211179936,7.55852061396171));
#150510=CARTESIAN_POINT('Ctrl Pts',(4.8873540394334,1.69743933262184,7.55736561377867));
#150511=CARTESIAN_POINT('Ctrl Pts',(4.88934717789494,1.7022413110283,7.55607642999802));
#150512=CARTESIAN_POINT('Ctrl Pts',(4.89812470861776,1.72064855720425,7.55039309055106));
#150513=CARTESIAN_POINT('Ctrl Pts',(4.90634395966117,1.7323072285775,7.54505912851645));
#150514=CARTESIAN_POINT('Ctrl Pts',(4.9219531802878,1.7468654658488,7.53488090739657));
#150515=CARTESIAN_POINT('Ctrl Pts',(4.92876964047146,1.75155833691055,7.5304255499714));
#150516=CARTESIAN_POINT('Ctrl Pts',(4.94325187651329,1.75781013657807,7.52092626275953));
#150517=CARTESIAN_POINT('Ctrl Pts',(4.95060225131441,1.75940739618523,7.51609057133398));
#150518=CARTESIAN_POINT('Ctrl Pts',(4.95807283415526,1.75940739618001,7.51115928277464));
#150519=CARTESIAN_POINT('Ctrl Pts',(4.96627064057822,1.75940739617429,7.50574795813151));
#150520=CARTESIAN_POINT('Ctrl Pts',(4.97437882446554,1.75748289694724,7.50037613048852));
#150521=CARTESIAN_POINT('Ctrl Pts',(4.99064901201179,1.74964163130848,7.48956119548553));
#150522=CARTESIAN_POINT('Ctrl Pts',(4.99844687851582,1.7434982227554,7.48435685535609));
#150523=CARTESIAN_POINT('Ctrl Pts',(5.01396330668295,1.72630637188402,7.47397348750486));
#150524=CARTESIAN_POINT('Ctrl Pts',(5.02104020468542,1.71456563931462,7.46921675427246));
#150525=CARTESIAN_POINT('Ctrl Pts',(5.02780648852956,1.69868853677723,7.46466103147771));
#150526=CARTESIAN_POINT('Ctrl Pts',(5.02900559682142,1.69560796580551,7.4638531946588));
#150527=CARTESIAN_POINT('Ctrl Pts',(5.03011945218954,1.69247211209781,7.46310245787263));
#150528=CARTESIAN_POINT('Ctrl Pts',(5.24380141833698,1.00000000010371,7.31454350489811));
#150529=CARTESIAN_POINT('Ctrl Pts',(5.23337663930275,1.04120750322152,7.32201703636989));
#150530=CARTESIAN_POINT('Ctrl Pts',(5.2225039177803,1.08227801747271,7.3297779019771));
#150531=CARTESIAN_POINT('Ctrl Pts',(5.15849572412172,1.314758318566,7.37523593608385));
#150532=CARTESIAN_POINT('Ctrl Pts',(5.09711568904592,1.50385659881995,7.41794709841542));
#150533=CARTESIAN_POINT('Ctrl Pts',(5.03011945133157,1.69247211165461,7.4631024584509));
#150534=CARTESIAN_POINT('',(5.54343983057962,1.69247211214185,7.09015337246368));
#150535=CARTESIAN_POINT('Ctrl Pts',(5.54343983074268,1.69247211204734,7.090153372314));
#150536=CARTESIAN_POINT('Ctrl Pts',(5.47979155526345,1.50385659906037,7.13991680716823));
#150537=CARTESIAN_POINT('Ctrl Pts',(5.42020335200143,1.31475831865458,7.185094214528));
#150538=CARTESIAN_POINT('Ctrl Pts',(5.35719057279498,1.08227801744158,7.23192231915544));
#150539=CARTESIAN_POINT('Ctrl Pts',(5.34644969527096,1.0412075032267,7.23986465243843));
#150540=CARTESIAN_POINT('Ctrl Pts',(5.33612051058942,1.00000000014546,7.24746975823059));
#150541=CARTESIAN_POINT('',(5.678857015,1.69247211099998,6.982161771));
#150542=CARTESIAN_POINT('Ctrl Pts',(5.54343983023426,1.69247211232382,7.09015337271151));
#150543=CARTESIAN_POINT('Ctrl Pts',(5.54511601804186,1.69743933283044,7.08884284446661));
#150544=CARTESIAN_POINT('Ctrl Pts',(5.54698557106645,1.70224131093972,7.08738018708892));
#150545=CARTESIAN_POINT('Ctrl Pts',(5.55521831528553,1.72064855688244,7.08093291540946));
#150546=CARTESIAN_POINT('Ctrl Pts',(5.56292634537749,1.73230722829274,7.07488365835215));
#150547=CARTESIAN_POINT('Ctrl Pts',(5.5775603591791,1.74686546561221,7.06334721200285));
#150548=CARTESIAN_POINT('Ctrl Pts',(5.5839500031433,1.75155833669097,7.05829876775497));
#150549=CARTESIAN_POINT('Ctrl Pts',(5.59752242843278,1.7578101363872,7.04753954424594));
#150550=CARTESIAN_POINT('Ctrl Pts',(5.60440974475557,1.7594073960068,7.04206443737231));
#150551=CARTESIAN_POINT('Ctrl Pts',(5.61140821593639,1.75940739601077,7.03648334284404));
#150552=CARTESIAN_POINT('Ctrl Pts',(5.61908795299923,1.75940739601513,7.03035895690422));
#150553=CARTESIAN_POINT('Ctrl Pts',(5.62668196880537,1.75748289679882,7.02428194266244));
#150554=CARTESIAN_POINT('Ctrl Pts',(5.64191721405738,1.7496416311835,7.01205209704974));
#150555=CARTESIAN_POINT('Ctrl Pts',(5.64921717518739,1.7434982226466,7.00616971270523));
#150556=CARTESIAN_POINT('Ctrl Pts',(5.66374038085026,1.72630637181616,6.99443726335541));
#150557=CARTESIAN_POINT('Ctrl Pts',(5.67036239905917,1.71456563927441,6.98906531109188));
#150558=CARTESIAN_POINT('Ctrl Pts',(5.67669307213169,1.69868853641841,6.98392140317849));
#150559=CARTESIAN_POINT('Ctrl Pts',(5.67781493935397,1.69560796508514,6.98300933113573));
#150560=CARTESIAN_POINT('Ctrl Pts',(5.67885701524478,1.69247211100408,6.98216177128582));
#150561=CARTESIAN_POINT('Ctrl Pts',(5.87836203940153,1.00000000015303,6.81504656871273));
#150562=CARTESIAN_POINT('Ctrl Pts',(5.86864914972266,1.04120750297626,6.82342448387522));
#150563=CARTESIAN_POINT('Ctrl Pts',(5.85851587727959,1.08227801693488,6.83212872970076));
#150564=CARTESIAN_POINT('Ctrl Pts',(5.79884018861094,1.31475831779691,6.88314141331103));
#150565=CARTESIAN_POINT('Ctrl Pts',(5.74153585055806,1.50385659810718,6.93118269699841));
#150566=CARTESIAN_POINT('Ctrl Pts',(5.6788570152349,1.69247211099862,6.98216177129386));
#150567=CARTESIAN_POINT('',(6.15668002,1.69247211199998,6.564700384));
#150568=CARTESIAN_POINT('Ctrl Pts',(6.15668002040536,1.69247211175397,6.56470038359266));
#150569=CARTESIAN_POINT('Ctrl Pts',(6.09774873405703,1.50385659870572,6.6199688729428));
#150570=CARTESIAN_POINT('Ctrl Pts',(6.04245008693597,1.31475831823908,6.67030585472521));
#150571=CARTESIAN_POINT('Ctrl Pts',(5.9838886175974,1.08227801704481,6.7225938651483));
#150572=CARTESIAN_POINT('Ctrl Pts',(5.97390292497523,1.04120750291262,6.73146702975377));
#150573=CARTESIAN_POINT('Ctrl Pts',(5.96429703900053,0.999999999914594,
6.73996742058666));
#150574=CARTESIAN_POINT('',(6.281871763,1.69247211199998,6.445004822));
#150575=CARTESIAN_POINT('Ctrl Pts',(6.15668002018172,1.69247211188528,6.56470038380239));
#150576=CARTESIAN_POINT('Ctrl Pts',(6.15823198538401,1.69743933273646,6.56324487896678));
#150577=CARTESIAN_POINT('Ctrl Pts',(6.15996290064518,1.70224131117035,6.56162052427874));
#150578=CARTESIAN_POINT('Ctrl Pts',(6.16758457340532,1.72064855738561,6.55446122979652));
#150579=CARTESIAN_POINT('Ctrl Pts',(6.17471932200875,1.73230722877144,6.54774538278063));
#150580=CARTESIAN_POINT('Ctrl Pts',(6.18826030448659,1.74686546605821,6.53494359589355));
#150581=CARTESIAN_POINT('Ctrl Pts',(6.19417168656544,1.75155833712512,6.52934271193098));
#150582=CARTESIAN_POINT('Ctrl Pts',(6.20672502389222,1.75781013680233,6.51741017907484));
#150583=CARTESIAN_POINT('Ctrl Pts',(6.21309382910321,1.75940739641427,6.51133973909936));
#150584=CARTESIAN_POINT('Ctrl Pts',(6.21956384103445,1.75940739641324,6.50515377430057));
#150585=CARTESIAN_POINT('Ctrl Pts',(6.22666367601188,1.75940739641211,6.49836563701203));
#150586=CARTESIAN_POINT('Ctrl Pts',(6.23368238118684,1.75748289718959,6.4916323647118));
#150587=CARTESIAN_POINT('Ctrl Pts',(6.24776001891509,1.74964163156032,6.47808607599983));
#150588=CARTESIAN_POINT('Ctrl Pts',(6.25450329968281,1.74349822301388,6.47157300893045));
#150589=CARTESIAN_POINT('Ctrl Pts',(6.26791635054222,1.72630637215997,6.45858594084604));
#150590=CARTESIAN_POINT('Ctrl Pts',(6.27403017236558,1.71456563960318,6.45264202134429));
#150591=CARTESIAN_POINT('Ctrl Pts',(6.27987426357281,1.69868853696114,6.44695134421518));
#150592=CARTESIAN_POINT('Ctrl Pts',(6.28090985690551,1.69560796586702,6.44594238057608));
#150593=CARTESIAN_POINT('Ctrl Pts',(6.28187176296278,1.69247211203292,6.44500482185164));
#150594=CARTESIAN_POINT('Ctrl Pts',(6.4655935474153,1.00000000002598,6.26067888328588));
#150595=CARTESIAN_POINT('Ctrl Pts',(6.45667074945246,1.04120750309549,6.2698937281947));
#150596=CARTESIAN_POINT('Ctrl Pts',(6.44735851311335,1.0822780172987,6.27947127288013));
#150597=CARTESIAN_POINT('Ctrl Pts',(6.39249580284863,1.31475831852555,6.3356278820062));
#150598=CARTESIAN_POINT('Ctrl Pts',(6.3397285426547,1.5038565989558,6.38861248690754));
#150599=CARTESIAN_POINT('Ctrl Pts',(6.28187176285276,1.69247211196711,6.44500482195888));
#150600=CARTESIAN_POINT('',(6.720350242,1.69247211199998,5.986392288));
#150601=CARTESIAN_POINT('Ctrl Pts',(6.72035024195089,1.69247211200555,5.98639228797367));
#150602=CARTESIAN_POINT('Ctrl Pts',(6.66661042481084,1.50385659891639,6.04672084242626));
#150603=CARTESIAN_POINT('Ctrl Pts',(6.61604656603123,1.31475831840883,6.10181211483949));
#150604=CARTESIAN_POINT('Ctrl Pts',(6.56240790905556,1.0822780171616,6.15913903875424));
#150605=CARTESIAN_POINT('Ctrl Pts',(6.55325780023637,1.04120750301805,6.16887159319523));
#150606=CARTESIAN_POINT('Ctrl Pts',(6.54445255389156,1.0000000000086,6.17819882893568));
#150607=CARTESIAN_POINT('',(6.834308572,1.69247211199998,5.855956484));
#150608=CARTESIAN_POINT('Ctrl Pts',(6.72035024189579,1.69247211204104,5.98639228803552));
#150609=CARTESIAN_POINT('Ctrl Pts',(6.72176548885911,1.69743933272173,5.98480352558652));
#150610=CARTESIAN_POINT('Ctrl Pts',(6.72334382988621,1.70224131099489,5.98303055207738));
#150611=CARTESIAN_POINT('Ctrl Pts',(6.73029306576593,1.72064855706964,5.97521687739583));
#150612=CARTESIAN_POINT('Ctrl Pts',(6.73679708808436,1.73230722846244,5.96788851247167));
#150613=CARTESIAN_POINT('Ctrl Pts',(6.7491360152204,1.74686546575904,5.95392445750275));
#150614=CARTESIAN_POINT('Ctrl Pts',(6.75452154044654,1.75155833682971,5.94781622884727));
#150615=CARTESIAN_POINT('Ctrl Pts',(6.76595471773228,1.75781013651241,5.93480646037549));
#150616=CARTESIAN_POINT('Ctrl Pts',(6.77175373396333,1.75940739612622,5.92818956290777));
#150617=CARTESIAN_POINT('Ctrl Pts',(6.77764319392101,1.75940739612599,5.92144853358502));
#150618=CARTESIAN_POINT('Ctrl Pts',(6.78410596311401,1.75940739612575,5.91405129904243));
#150619=CARTESIAN_POINT('Ctrl Pts',(6.79049284716903,1.75748289690448,5.90671598103713));
#150620=CARTESIAN_POINT('Ctrl Pts',(6.80329953250676,1.74964163127831,5.89196231598693));
#150621=CARTESIAN_POINT('Ctrl Pts',(6.80943183997698,1.74349822273394,5.8848710055844));
#150622=CARTESIAN_POINT('Ctrl Pts',(6.82162674202862,1.72630637188466,5.87073388301059));
#150623=CARTESIAN_POINT('Ctrl Pts',(6.82718314256654,1.71456563933029,5.86426585321872));
#150624=CARTESIAN_POINT('Ctrl Pts',(6.8324935987988,1.69868853674338,5.85807422480592));
#150625=CARTESIAN_POINT('Ctrl Pts',(6.83343458031894,1.69560796570414,5.85697649310469));
#150626=CARTESIAN_POINT('Ctrl Pts',(6.83430857189648,1.69247211192667,5.85595648413667));
#150627=CARTESIAN_POINT('Ctrl Pts',(7.00076789655382,0.999999999903773,
5.65590389403687));
#150628=CARTESIAN_POINT('Ctrl Pts',(6.99270703148499,1.04120750294805,5.66588147612623));
#150629=CARTESIAN_POINT('Ctrl Pts',(6.98429080796197,1.08227801712618,5.67625520685598));
#150630=CARTESIAN_POINT('Ctrl Pts',(6.93468279847114,1.31475831832256,5.73710360140728));
#150631=CARTESIAN_POINT('Ctrl Pts',(6.8868774671133,1.50385659874697,5.79460492660105));
#150632=CARTESIAN_POINT('Ctrl Pts',(6.83430857163229,1.69247211175275,5.855956484445));
#150633=CARTESIAN_POINT('',(7.229912155,1.69247211199998,5.359885281));
#150634=CARTESIAN_POINT('Ctrl Pts',(7.22991215493042,1.69247211222666,5.35988528160719));
#150635=CARTESIAN_POINT('Ctrl Pts',(7.18179648839481,1.50385659905977,5.42478817113771));
#150636=CARTESIAN_POINT('Ctrl Pts',(7.13637452840358,1.31475831847509,5.48419017167095));
#150637=CARTESIAN_POINT('Ctrl Pts',(7.08809055071595,1.08227801718246,5.54609444640032));
#150638=CARTESIAN_POINT('Ctrl Pts',(7.07984969700402,1.04120750307276,5.55660802986153));
#150639=CARTESIAN_POINT('Ctrl Pts',(7.07191598496283,1.00000000009741,5.56668701308303));
#150640=CARTESIAN_POINT('',(7.331719547,1.69247211199998,5.219759428));
#150641=CARTESIAN_POINT('Ctrl Pts',(7.2299121553839,1.69247211190049,5.3598852809955));
#150642=CARTESIAN_POINT('Ctrl Pts',(7.23117928939508,1.69743933249793,5.35817605269869));
#150643=CARTESIAN_POINT('Ctrl Pts',(7.23259234834446,1.70224131069262,5.35626873528853));
#150644=CARTESIAN_POINT('Ctrl Pts',(7.238813196219,1.72064855670081,5.34786359149694));
#150645=CARTESIAN_POINT('Ctrl Pts',(7.244634125688,1.732307228099,5.33998171234978));
#150646=CARTESIAN_POINT('Ctrl Pts',(7.25567165169417,1.74686546540359,5.32496781965828));
#150647=CARTESIAN_POINT('Ctrl Pts',(7.2604879589843,1.75155833647739,5.31840142617491));
#150648=CARTESIAN_POINT('Ctrl Pts',(7.2707089230063,1.75781013616434,5.30441916909239));
#150649=CARTESIAN_POINT('Ctrl Pts',(7.27589145998758,1.75940739577936,5.29730908949957));
#150650=CARTESIAN_POINT('Ctrl Pts',(7.28115294950206,1.7594073957793,5.29006727045673));
#150651=CARTESIAN_POINT('Ctrl Pts',(7.28692661849263,1.75940739577923,5.28212049684292));
#150652=CARTESIAN_POINT('Ctrl Pts',(7.29263025799211,1.75748289655852,5.27424219279993));
#150653=CARTESIAN_POINT('Ctrl Pts',(7.30406287903832,1.7496416309341,5.25839993924684));
#150654=CARTESIAN_POINT('Ctrl Pts',(7.30953483947673,1.74349822239083,5.25078748057241));
#150655=CARTESIAN_POINT('Ctrl Pts',(7.32041340653934,1.72630637154356,5.23561412730614));
#150656=CARTESIAN_POINT('Ctrl Pts',(7.32536764892156,1.71456563898964,5.22867406399609));
#150657=CARTESIAN_POINT('Ctrl Pts',(7.33010171347168,1.69868853658724,5.22203133570847));
#150658=CARTESIAN_POINT('Ctrl Pts',(7.33094050691844,1.69560796573972,5.22085367428564));
#150659=CARTESIAN_POINT('Ctrl Pts',(7.33171954712375,1.69247211216014,5.21975942762917));
#150660=CARTESIAN_POINT('Ctrl Pts',(7.47957617958273,1.00000000003768,5.00559089157501));
#150661=CARTESIAN_POINT('Ctrl Pts',(7.47244214875601,1.0412075030462,5.01625087721741));
#150662=CARTESIAN_POINT('Ctrl Pts',(7.4649897005347,1.08227801718884,5.0273372708077));
#150663=CARTESIAN_POINT('Ctrl Pts',(7.42103580633787,1.3147583184205,5.09238753530659));
#150664=CARTESIAN_POINT('Ctrl Pts',(7.37857730422629,1.50385659891382,5.15394261395913));
#150665=CARTESIAN_POINT('Ctrl Pts',(7.33171954689145,1.69247211198855,5.21975942795546));
#150666=CARTESIAN_POINT('',(7.681263067,1.69247211199998,4.69022363));
#150667=CARTESIAN_POINT('Ctrl Pts',(7.68126306643363,1.69247211231474,4.69022363051514));
#150668=CARTESIAN_POINT('Ctrl Pts',(7.63915894961858,1.50385659926452,4.75917829513542));
#150669=CARTESIAN_POINT('Ctrl Pts',(7.59924459938714,1.31475831879601,4.8224127537344));
#150670=CARTESIAN_POINT('Ctrl Pts',(7.55670405519824,1.08227801749227,4.88839596244951));
#150671=CARTESIAN_POINT('Ctrl Pts',(7.54943880707296,1.0412075032506,4.89960592578131));
#150672=CARTESIAN_POINT('Ctrl Pts',(7.54244050689292,1.00000000014238,4.91035550647617));
#150673=CARTESIAN_POINT('',(7.770099827,1.69247211199998,4.541535938));
#150674=CARTESIAN_POINT('Ctrl Pts',(7.68126306658055,1.69247211219402,4.69022363027453));
#150675=CARTESIAN_POINT('Ctrl Pts',(7.68237188542729,1.69743933272178,4.68840769783156));
#150676=CARTESIAN_POINT('Ctrl Pts',(7.68360828518667,1.70224131085111,4.68638139311887));
#150677=CARTESIAN_POINT('Ctrl Pts',(7.68905065845815,1.72064855681647,4.67745245349188));
#150678=CARTESIAN_POINT('Ctrl Pts',(7.69414162837983,1.73230722823068,4.66908052037508));
#150679=CARTESIAN_POINT('Ctrl Pts',(7.70378888559199,1.74686546555535,4.65313767299271));
#150680=CARTESIAN_POINT('Ctrl Pts',(7.7079971968728,1.75155833663596,4.64616598342078));
#150681=CARTESIAN_POINT('Ctrl Pts',(7.71692365444042,1.7578101363352,4.63132381464051));
#150682=CARTESIAN_POINT('Ctrl Pts',(7.72144798543253,1.75940739595606,4.6237777991027));
#150683=CARTESIAN_POINT('Ctrl Pts',(7.72603914208535,1.75940739596088,4.61609349720791));
#150684=CARTESIAN_POINT('Ctrl Pts',(7.73107722468816,1.75940739596616,4.60766116727051));
#150685=CARTESIAN_POINT('Ctrl Pts',(7.73605169728343,1.75748289675087,4.59930330866005));
#150686=CARTESIAN_POINT('Ctrl Pts',(7.74601820529917,1.74964163113786,4.58250001911516));
#150687=CARTESIAN_POINT('Ctrl Pts',(7.75078576169848,1.74349822260255,4.57442770321188));
#150688=CARTESIAN_POINT('Ctrl Pts',(7.76026040594584,1.72630637177601,4.55834028617848));
#150689=CARTESIAN_POINT('Ctrl Pts',(7.76457260152491,1.71456563923682,4.550984066663));
#150690=CARTESIAN_POINT('Ctrl Pts',(7.76869215858641,1.69868853671208,4.54394372171134));
#150691=CARTESIAN_POINT('Ctrl Pts',(7.76942201057286,1.69560796572158,4.54269561228855));
#150692=CARTESIAN_POINT('Ctrl Pts',(7.77009982710408,1.69247211199432,4.54153593807615));
#150693=CARTESIAN_POINT('Ctrl Pts',(7.89816331283004,0.999999999979972,
4.31497581498039));
#150694=CARTESIAN_POINT('Ctrl Pts',(7.8920135552809,1.04120750283238,4.3262323762081));
#150695=CARTESIAN_POINT('Ctrl Pts',(7.88558488510779,1.08227801681994,4.33794217150246));
#150696=CARTESIAN_POINT('Ctrl Pts',(7.84763899711798,1.31475831805313,4.40667055946035));
#150697=CARTESIAN_POINT('Ctrl Pts',(7.81086917512474,1.50385659869719,4.47178378631242));
#150698=CARTESIAN_POINT('Ctrl Pts',(7.77009982702068,1.69247211192352,4.54153593821884));
#150699=CARTESIAN_POINT('',(8.070768965,1.69247211199998,3.982799055));
#150700=CARTESIAN_POINT('Ctrl Pts',(8.07076896483245,1.69247211221444,3.98279905547562));
#150701=CARTESIAN_POINT('Ctrl Pts',(8.03501539529516,1.50385659911875,4.05525031284117));
#150702=CARTESIAN_POINT('Ctrl Pts',(8.00093002167116,1.31475831860448,4.12180810288602));
#150703=CARTESIAN_POINT('Ctrl Pts',(7.96447542245618,1.08227801735784,4.19133898755909));
#150704=CARTESIAN_POINT('Ctrl Pts',(7.95824427546741,1.04120750322134,4.20315507466474));
#150705=CARTESIAN_POINT('Ctrl Pts',(7.95223773338732,1.00000000021904,4.21448870347175));
#150706=CARTESIAN_POINT('',(8.14591983279771,1.69247211207413,3.82674667047894));
#150707=CARTESIAN_POINT('Ctrl Pts',(8.07076896488867,1.69247211216004,3.98279905536167));
#150708=CARTESIAN_POINT('Ctrl Pts',(8.07171054104207,1.69743933278747,3.98089103954382));
#150709=CARTESIAN_POINT('Ctrl Pts',(8.07276032688418,1.70224131101044,3.97876206207974));
#150710=CARTESIAN_POINT('Ctrl Pts',(8.07738040680553,1.72064855704371,3.96938121711269));
#150711=CARTESIAN_POINT('Ctrl Pts',(8.08170042767807,1.73230722844115,3.9605866359141));
#150712=CARTESIAN_POINT('Ctrl Pts',(8.08987974204302,1.74686546574377,3.94384319628412));
#150713=CARTESIAN_POINT('Ctrl Pts',(8.09344617446283,1.7515583368165,3.93652234257196));
#150714=CARTESIAN_POINT('Ctrl Pts',(8.10100625498024,1.75781013650272,3.92093976251732));
#150715=CARTESIAN_POINT('Ctrl Pts',(8.10483595272583,1.75940739611808,3.91301856711897));
#150716=CARTESIAN_POINT('Ctrl Pts',(8.10871981121782,1.75940739611904,3.90495365185858));
#150717=CARTESIAN_POINT('Ctrl Pts',(8.11298174375302,1.75940739612009,3.89610365775794));
#150718=CARTESIAN_POINT('Ctrl Pts',(8.11718699791387,1.75748289690017,3.88733353714228));
#150719=CARTESIAN_POINT('Ctrl Pts',(8.1256071484364,1.74964163127696,3.86970450180578));
#150720=CARTESIAN_POINT('Ctrl Pts',(8.12963191523693,1.74349822273463,3.86123732220919));
#150721=CARTESIAN_POINT('Ctrl Pts',(8.13762635240813,1.72630637189053,3.84436536781836));
#150722=CARTESIAN_POINT('Ctrl Pts',(8.14126178192232,1.71456563933969,3.83665222004586));
#150723=CARTESIAN_POINT('Ctrl Pts',(8.14473366319477,1.69868853683267,3.8292709432193));
#150724=CARTESIAN_POINT('Ctrl Pts',(8.14534869733938,1.69560796587296,3.82796243490335));
#150725=CARTESIAN_POINT('Ctrl Pts',(8.14591983278025,1.69247211217755,3.826746670204));
#150726=CARTESIAN_POINT('Ctrl Pts',(8.25315907928445,1.00000000000618,3.589619090102));
#150727=CARTESIAN_POINT('Ctrl Pts',(8.24804310921235,1.04120750292175,3.60138159575791));
#150728=CARTESIAN_POINT('Ctrl Pts',(8.2426899769243,1.08227801697206,3.61362051242964));
#150729=CARTESIAN_POINT('Ctrl Pts',(8.21105761312824,1.31475831812731,3.68547366326025));
#150730=CARTESIAN_POINT('Ctrl Pts',(8.18027252030632,1.50385659863499,3.75362078478248));
#150731=CARTESIAN_POINT('Ctrl Pts',(8.14591983233074,1.6924721117247,3.82674667116087));
#150732=CARTESIAN_POINT('',(8.395293776,1.69247211199998,3.243307326));
#150733=CARTESIAN_POINT('Ctrl Pts',(8.39529377643544,1.69247211171466,3.24330732545414));
#150734=CARTESIAN_POINT('Ctrl Pts',(8.36617862092618,1.50385659880013,3.31867184053676));
#150735=CARTESIAN_POINT('Ctrl Pts',(8.33819665932569,1.31475831846641,3.38801707774585));
#150736=CARTESIAN_POINT('Ctrl Pts',(8.30812151607705,1.08227801737161,3.460535816552));
#150737=CARTESIAN_POINT('Ctrl Pts',(8.30297463973184,1.04120750320158,3.47286289128436));
#150738=CARTESIAN_POINT('Ctrl Pts',(8.29800821687382,1.0000000001655,3.48468931652372));
#150739=CARTESIAN_POINT('',(8.456153681,1.69247211199998,3.081146689));
#150740=CARTESIAN_POINT('Ctrl Pts',(8.39529377630737,1.69247211186685,3.24330732578563));
#150741=CARTESIAN_POINT('Ctrl Pts',(8.39606052875182,1.69743933266438,3.24132258879396));
#150742=CARTESIAN_POINT('Ctrl Pts',(8.39691524842106,1.70224131104791,3.23910807982609));
#150743=CARTESIAN_POINT('Ctrl Pts',(8.40067583683032,1.72064855723031,3.22935085853306));
#150744=CARTESIAN_POINT('Ctrl Pts',(8.40419012638923,1.73230722862897,3.22020443804662));
#150745=CARTESIAN_POINT('Ctrl Pts',(8.41083564288388,1.74686546593259,3.20279521449446));
#150746=CARTESIAN_POINT('Ctrl Pts',(8.41373148162846,1.75155833700544,3.19518413985007));
#150747=CARTESIAN_POINT('Ctrl Pts',(8.4198643157783,1.75781013669251,3.17898661028975));
#150748=CARTESIAN_POINT('Ctrl Pts',(8.42296854580602,1.75940739630863,3.17075401183653));
#150749=CARTESIAN_POINT('Ctrl Pts',(8.42611383559583,1.75940739631059,3.16237341716321));
#150750=CARTESIAN_POINT('Ctrl Pts',(8.42956530348966,1.75940739631274,3.15317701384933));
#150751=CARTESIAN_POINT('Ctrl Pts',(8.43296748098366,1.75748289709378,3.14406524308343));
#150752=CARTESIAN_POINT('Ctrl Pts',(8.43977347991322,1.74964163147232,3.12575240058617));
#150753=CARTESIAN_POINT('Ctrl Pts',(8.44302305205915,1.74349822293125,3.11695853005104));
#150754=CARTESIAN_POINT('Ctrl Pts',(8.44947291564613,1.72630637209084,3.09943788136672));
#150755=CARTESIAN_POINT('Ctrl Pts',(8.45240230875442,1.71456563954306,3.0914299070713));
#150756=CARTESIAN_POINT('Ctrl Pts',(8.45519856073018,1.69868853687056,3.08376712797649));
#150757=CARTESIAN_POINT('Ctrl Pts',(8.45569382517283,1.69560796573518,3.08240875602405));
#150758=CARTESIAN_POINT('Ctrl Pts',(8.45615368110477,1.69247211185842,3.0811466893899));
#150759=CARTESIAN_POINT('Ctrl Pts',(8.54170526185697,0.999999999891995,
2.83536086231805));
#150760=CARTESIAN_POINT('Ctrl Pts',(8.53766427004687,1.04120750290419,2.84753460763075));
#150761=CARTESIAN_POINT('Ctrl Pts',(8.53342977591951,1.08227801705046,2.8602041051281));
#150762=CARTESIAN_POINT('Ctrl Pts',(8.50836562150266,1.31475831827597,2.93460349954225));
#150763=CARTESIAN_POINT('Ctrl Pts',(8.48381312130125,1.50385659875946,3.00523583521544));
#150764=CARTESIAN_POINT('Ctrl Pts',(8.45615368107749,1.6924721118243,3.08114668946476));
#150765=CARTESIAN_POINT('',(8.652224619,1.69247211199998,2.477702391));
#150766=CARTESIAN_POINT('Ctrl Pts',(8.65222461931465,1.69247211184308,2.47770239070909));
#150767=CARTESIAN_POINT('Ctrl Pts',(8.6299822958743,1.50385659864939,2.55537337297999));
#150768=CARTESIAN_POINT('Ctrl Pts',(8.6083290405278,1.31475831803842,2.62694773048628));
#150769=CARTESIAN_POINT('Ctrl Pts',(8.58487550058799,1.08227801688607,2.70187044525523));
#150770=CARTESIAN_POINT('Ctrl Pts',(8.58085433453559,1.04120750294561,2.7146092571805));
#150771=CARTESIAN_POINT('Ctrl Pts',(8.57696801764159,1.00000000014065,2.72683325936026));
#150772=CARTESIAN_POINT('',(8.69830355250517,1.69247211177544,2.31073912599594));
#150773=CARTESIAN_POINT('Ctrl Pts',(8.65222461924908,1.6924721119451,2.47770239093806));
#150774=CARTESIAN_POINT('Ctrl Pts',(8.65281037451573,1.69743933267269,2.47565691277349));
#150775=CARTESIAN_POINT('Ctrl Pts',(8.65346314627405,1.70224131098984,2.47337470231207));
#150776=CARTESIAN_POINT('Ctrl Pts',(8.65633396507629,1.72064855709382,2.46331966420916));
#150777=CARTESIAN_POINT('Ctrl Pts',(8.65901422832519,1.73230722847671,2.45389504603908));
#150778=CARTESIAN_POINT('Ctrl Pts',(8.66407244115264,1.74686546576066,2.43596020740361));
#150779=CARTESIAN_POINT('Ctrl Pts',(8.66627437062938,1.75155833682684,2.42812019172599));
#150780=CARTESIAN_POINT('Ctrl Pts',(8.67093058043353,1.75781013650178,2.41143812564637));
#150781=CARTESIAN_POINT('Ctrl Pts',(8.6732843493065,1.7594073961121,2.40296040818192));
#150782=CARTESIAN_POINT('Ctrl Pts',(8.67566574636791,1.75940739610916,2.3943316097188));
#150783=CARTESIAN_POINT('Ctrl Pts',(8.67827896042827,1.75940739610594,2.38486284122433));
#150784=CARTESIAN_POINT('Ctrl Pts',(8.68085066892037,1.75748289688156,2.37548278293022));
#150785=CARTESIAN_POINT('Ctrl Pts',(8.6859877183523,1.74964163124872,2.35663357751048));
#150786=CARTESIAN_POINT('Ctrl Pts',(8.68843593219854,1.74349822269971,2.34758381910881));
#150787=CARTESIAN_POINT('Ctrl Pts',(8.69328929169141,1.72630637183858,2.32955554208354));
#150788=CARTESIAN_POINT('Ctrl Pts',(8.69548906264279,1.71456563927602,2.3213172167611));
#150789=CARTESIAN_POINT('Ctrl Pts',(8.69758717149787,1.69868853665797,2.31343463170188));
#150790=CARTESIAN_POINT('Ctrl Pts',(8.69795867862005,1.69560796559486,2.31203733302424));
#150791=CARTESIAN_POINT('Ctrl Pts',(8.69830355251919,1.69247211179278,2.31073912595777));
#150792=CARTESIAN_POINT('Ctrl Pts',(8.76147865593336,0.999999999896204,
2.05827397632682));
#150793=CARTESIAN_POINT('Ctrl Pts',(8.75854517807591,1.0412075030467,2.07076094547247));
#150794=CARTESIAN_POINT('Ctrl Pts',(8.75546341576689,1.08227801733033,2.08375901646764));
#150795=CARTESIAN_POINT('Ctrl Pts',(8.73716927257158,1.31475831846967,2.16010563424933));
#150796=CARTESIAN_POINT('Ctrl Pts',(8.71904704729885,1.5038565987368,2.23265449395954));
#150797=CARTESIAN_POINT('Ctrl Pts',(8.69830355239435,1.6924721115845,2.3107391264277));
#150798=CARTESIAN_POINT('',(8.839492837,1.69247211199998,1.692148455));
#150799=CARTESIAN_POINT('Ctrl Pts',(8.83949283651609,1.69247211196709,1.69214845482919));
#150800=CARTESIAN_POINT('Ctrl Pts',(8.82430242730659,1.50385659886908,1.77150054300318));
#150801=CARTESIAN_POINT('Ctrl Pts',(8.80915221754667,1.31475831835278,1.84472774598003));
#150802=CARTESIAN_POINT('Ctrl Pts',(8.79250911503047,1.08227801717924,1.92145120303552));
#150803=CARTESIAN_POINT('Ctrl Pts',(8.78964603529871,1.04120750311893,1.93449918683023));
#150804=CARTESIAN_POINT('Ctrl Pts',(8.78687111467305,1.00000000019332,1.94702234556373));
#150805=CARTESIAN_POINT('',(8.870419798,1.69247211199998,1.521726851));
#150806=CARTESIAN_POINT('Ctrl Pts',(8.83949283655333,1.6924721118822,1.69214845463461));
#150807=CARTESIAN_POINT('Ctrl Pts',(8.83989287848787,1.69743933253477,1.6900587042909));
#150808=CARTESIAN_POINT('Ctrl Pts',(8.84033844660459,1.70224131078139,1.68772716736003));
#150809=CARTESIAN_POINT('Ctrl Pts',(8.84229638166108,1.72064855683246,1.67745526970955));
#150810=CARTESIAN_POINT('Ctrl Pts',(8.84412103869952,1.73230722822604,1.6678283353348));
#150811=CARTESIAN_POINT('Ctrl Pts',(8.84755122211043,1.74686546552434,1.64951228238133));
#150812=CARTESIAN_POINT('Ctrl Pts',(8.84904151368015,1.75155833659586,1.64150644886353));
#150813=CARTESIAN_POINT('Ctrl Pts',(8.85218361007993,1.75781013627923,1.62447416044409));
#150814=CARTESIAN_POINT('Ctrl Pts',(8.85376796663779,1.75940739589287,1.61581958156026));
#150815=CARTESIAN_POINT('Ctrl Pts',(8.8553662973649,1.75940739589201,1.60701205331319));
#150816=CARTESIAN_POINT('Ctrl Pts',(8.85712021753,1.75940739589105,1.59734715659617));
#150817=CARTESIAN_POINT('Ctrl Pts',(8.85884075113717,1.7574828966693,1.5877743334884));
#150818=CARTESIAN_POINT('Ctrl Pts',(8.86226749057167,1.74964163104244,1.56854052787078));
#150819=CARTESIAN_POINT('Ctrl Pts',(8.86389463454005,1.74349822249752,1.55930774494077));
#150820=CARTESIAN_POINT('Ctrl Pts',(8.86711241354167,1.7263063716463,1.54091699267151));
#150821=CARTESIAN_POINT('Ctrl Pts',(8.8685648510738,1.71456563908997,1.5325146464782));
#150822=CARTESIAN_POINT('Ctrl Pts',(8.86994792407433,1.69868853657767,1.5244757214109));
#150823=CARTESIAN_POINT('Ctrl Pts',(8.87019268272299,1.6956079656182,1.52305074624817));
#150824=CARTESIAN_POINT('Ctrl Pts',(8.87041979787082,1.69247211192306,1.52172685116002));
#150825=CARTESIAN_POINT('Ctrl Pts',(8.91070977542002,0.999999999993989,
1.26461507907905));
#150826=CARTESIAN_POINT('Ctrl Pts',(8.90890743017016,1.04120750304135,1.27731473425656));
#150827=CARTESIAN_POINT('Ctrl Pts',(8.9070032122354,1.08227801722256,1.2905367258509));
#150828=CARTESIAN_POINT('Ctrl Pts',(8.89562637393289,1.31475831840746,1.36821586896249));
#150829=CARTESIAN_POINT('Ctrl Pts',(8.88408033304455,1.50385659881792,1.44209713210709));
#150830=CARTESIAN_POINT('Ctrl Pts',(8.87041979782602,1.69247211180957,1.52172685142119));
#150831=CARTESIAN_POINT('',(8.955590655,1.69247211199998,0.892970333000003));
#150832=CARTESIAN_POINT('Ctrl Pts',(8.95559065523521,1.69247211204864,0.892970333137615));
#150833=CARTESIAN_POINT('Ctrl Pts',(8.94757446449693,1.50385659895089,0.973364630912383));
#150834=CARTESIAN_POINT('Ctrl Pts',(8.93904928090067,1.3147583184345,1.04765509702603));
#150835=CARTESIAN_POINT('Ctrl Pts',(8.92935061629266,1.0822780171992,1.12556156422249));
#150836=CARTESIAN_POINT('Ctrl Pts',(8.92766867472662,1.04120750307671,1.13881366517733));
#150837=CARTESIAN_POINT('Ctrl Pts',(8.92602749240836,1.00000000008849,1.15153515133937));
#150838=CARTESIAN_POINT('',(8.971116639,1.69247211199998,0.720462526000001));
#150839=CARTESIAN_POINT('Ctrl Pts',(8.95559065523919,1.69247211203143,0.892970333097603));
#150840=CARTESIAN_POINT('Ctrl Pts',(8.9558017629423,1.69743933257032,0.890853136027186));
#150841=CARTESIAN_POINT('Ctrl Pts',(8.95603653996893,1.7022413107097,0.888491044806472));
#150842=CARTESIAN_POINT('Ctrl Pts',(8.95706582714207,1.72064855666455,0.878084990907337));
#150843=CARTESIAN_POINT('Ctrl Pts',(8.95802018690319,1.73230722806018,0.868333250744331));
#150844=CARTESIAN_POINT('Ctrl Pts',(8.95979472307499,1.7468654653616,0.849783453564592));
#150845=CARTESIAN_POINT('Ctrl Pts',(8.96056137778506,1.75155833643442,0.841676260471873));
#150846=CARTESIAN_POINT('Ctrl Pts',(8.96216406246514,1.7578101361195,0.824430883686815));
#150847=CARTESIAN_POINT('Ctrl Pts',(8.96296625039909,1.7594073957336,0.815669124965459));
#150848=CARTESIAN_POINT('Ctrl Pts',(8.96376864597118,1.75940739573273,0.806753779975069));
#150849=CARTESIAN_POINT('Ctrl Pts',(8.96464915070661,1.75940739573177,0.796970571100184));
#150850=CARTESIAN_POINT('Ctrl Pts',(8.96550465670329,1.75748289651019,0.787282057921248));
#150851=CARTESIAN_POINT('Ctrl Pts',(8.9671934960484,1.74964163088392,0.767818511397058));
#150852=CARTESIAN_POINT('Ctrl Pts',(8.96798646933209,1.74349822233937,0.758477040876455));
#150853=CARTESIAN_POINT('Ctrl Pts',(8.96954276017722,1.72630637148872,0.739871884883412));
#150854=CARTESIAN_POINT('Ctrl Pts',(8.97023617011667,1.71456563893236,0.731373168568872));
#150855=CARTESIAN_POINT('Ctrl Pts',(8.97089307157979,1.69868853652994,0.723242628198454));
#150856=CARTESIAN_POINT('Ctrl Pts',(8.97100911110934,1.69560796568501,0.721801449619328));
#150857=CARTESIAN_POINT('Ctrl Pts',(8.97111663891427,1.6924721121081,0.720462525739917));
#150858=CARTESIAN_POINT('Ctrl Pts',(8.98819709930371,0.999999999959406,
0.460774244146091));
#150859=CARTESIAN_POINT('Ctrl Pts',(8.98754039807928,1.04120750304597,0.473584335238513));
#150860=CARTESIAN_POINT('Ctrl Pts',(8.98682905615476,1.08227801726612,0.486923791773002));
#150861=CARTESIAN_POINT('Ctrl Pts',(8.98246112236426,1.31475831853779,0.565310033439549));
#150862=CARTESIAN_POINT('Ctrl Pts',(8.9775842278123,1.50385659899527,0.639928851482268));
#150863=CARTESIAN_POINT('Ctrl Pts',(8.97111663890039,1.69247211203383,0.72046252591272));
#150864=CARTESIAN_POINT('',(8.999583324,1.69247211199998,0.0866025400000026));
#150865=CARTESIAN_POINT('Ctrl Pts',(8.99958332369346,1.69247211191239,0.0866025397925534));
#150866=CARTESIAN_POINT('Ctrl Pts',(8.99880589307639,1.50385659887802,0.16739175952592));
#150867=CARTESIAN_POINT('Ctrl Pts',(8.99697437540593,1.31475831842477,0.242147345601195));
#150868=CARTESIAN_POINT('Ctrl Pts',(8.99429823665167,1.08227801725348,0.320609565836492));
#150869=CARTESIAN_POINT('Ctrl Pts',(8.99381097525934,1.04120750313013,0.333959085808914));
#150870=CARTESIAN_POINT('Ctrl Pts',(8.9933167450867,1.00000000014106,0.3467764734569));
#150871=CARTESIAN_POINT('',(8.999583324,1.69247211199998,-0.0866025400000003));
#150872=CARTESIAN_POINT('Ctrl Pts',(8.9995833236904,1.69247211204886,-0.0866025401111396));
#150873=CARTESIAN_POINT('Ctrl Pts',(8.99959624897225,1.69560796569572,-0.0852593676028344));
#150874=CARTESIAN_POINT('Ctrl Pts',(8.99960986283583,1.69868853660841,-0.0838135890526297));
#150875=CARTESIAN_POINT('Ctrl Pts',(8.99968442188485,1.71456563907318,-0.0756568956210146));
#150876=CARTESIAN_POINT('Ctrl Pts',(8.99975562246681,1.72630637162691,-0.0671302358526971));
#150877=CARTESIAN_POINT('Ctrl Pts',(8.999873350116,1.74349822247422,-0.0484604739130545));
#150878=CARTESIAN_POINT('Ctrl Pts',(8.99992093207107,1.74964163101758,-0.03908552782939));
#150879=CARTESIAN_POINT('Ctrl Pts',(8.99998359035555,1.75748289664218,-0.0195489494290202));
#150880=CARTESIAN_POINT('Ctrl Pts',(9.,1.7594073958629,-0.00982275238873509));
#150881=CARTESIAN_POINT('Ctrl Pts',(9.,1.7594073958629,2.22044604925031E-15));
#150882=CARTESIAN_POINT('Ctrl Pts',(9.,1.7594073958629,0.00895138061714817));
#150883=CARTESIAN_POINT('Ctrl Pts',(8.99998643943525,1.75781013624804,0.0177497746457833));
#150884=CARTESIAN_POINT('Ctrl Pts',(8.999936070349,1.75155833656183,0.0350693901608712));
#150885=CARTESIAN_POINT('Ctrl Pts',(8.99989922515123,1.7468654654886,0.0432126684760403));
#150886=CARTESIAN_POINT('Ctrl Pts',(8.99979462373951,1.73230722818546,0.0618468578232667));
#150887=CARTESIAN_POINT('Ctrl Pts',(8.99971824519885,1.72064855678819,0.071644888497604));
#150888=CARTESIAN_POINT('Ctrl Pts',(8.99962589311285,1.70224131079953,0.0821013152925228));
#150889=CARTESIAN_POINT('Ctrl Pts',(8.99960379745391,1.69743933262498,0.0844749426937048));
#150890=CARTESIAN_POINT('Ctrl Pts',(8.9995833236904,1.69247211204887,0.0866025401111421));
#150891=CARTESIAN_POINT('Ctrl Pts',(8.99331674508599,1.00000000014682,-0.346776473475384));
#150892=CARTESIAN_POINT('Ctrl Pts',(8.99381097525864,1.04120750313464,-0.333959085827752));
#150893=CARTESIAN_POINT('Ctrl Pts',(8.99429823665098,1.08227801725674,-0.320609565855717));
#150894=CARTESIAN_POINT('Ctrl Pts',(8.99697437540542,1.31475831842863,-0.242147345620229));
#150895=CARTESIAN_POINT('Ctrl Pts',(8.99880589307606,1.50385659888367,-0.16739175954417));
#150896=CARTESIAN_POINT('Ctrl Pts',(8.9995833236933,1.69247211191984,-0.0866025398099395));
#150897=CARTESIAN_POINT('',(8.971116639,1.69247211199998,-0.720462525999999));
#150898=CARTESIAN_POINT('Ctrl Pts',(8.9711166389309,1.69247211219709,-0.720462525532798));
#150899=CARTESIAN_POINT('Ctrl Pts',(8.97758422784487,1.50385659904378,-0.639928851033996));
#150900=CARTESIAN_POINT('Ctrl Pts',(8.98246112239683,1.31475831847271,-0.565310032927709));
#150901=CARTESIAN_POINT('Ctrl Pts',(8.98682905618331,1.08227801719273,-0.486923791245081));
#150902=CARTESIAN_POINT('Ctrl Pts',(8.98754039810538,1.0412075030817,-0.473584334742424));
#150903=CARTESIAN_POINT('Ctrl Pts',(8.98819709932766,1.000000000105,-0.460774243678976));
#150904=CARTESIAN_POINT('',(8.955590655,1.69247211199998,-0.892970333000001));
#150905=CARTESIAN_POINT('Ctrl Pts',(8.97111663891427,1.69247211210811,-0.720462525739922));
#150906=CARTESIAN_POINT('Ctrl Pts',(8.97094631389629,1.69743933260741,-0.72258339330523));
#150907=CARTESIAN_POINT('Ctrl Pts',(8.97075555028735,1.70224131070957,-0.724949445788228));
#150908=CARTESIAN_POINT('Ctrl Pts',(8.96991022372286,1.72064855663687,-0.735372056421064));
#150909=CARTESIAN_POINT('Ctrl Pts',(8.96910800608785,1.7323072280393,-0.745137489624583));
#150910=CARTESIAN_POINT('Ctrl Pts',(8.96754183055015,1.74686546534951,-0.763706039604086));
#150911=CARTESIAN_POINT('Ctrl Pts',(8.96684856957967,1.7515583364253,-0.771819838253878));
#150912=CARTESIAN_POINT('Ctrl Pts',(8.96534621752964,1.75781013611549,-0.789074245141246));
#150913=CARTESIAN_POINT('Ctrl Pts',(8.96457104154341,1.75940739573185,-0.797838434983122));
#150914=CARTESIAN_POINT('Ctrl Pts',(8.96376864597118,1.75940739573272,-0.806753779975073));
#150915=CARTESIAN_POINT('Ctrl Pts',(8.96288814123577,1.75940739573368,-0.816536988849692));
#150916=CARTESIAN_POINT('Ctrl Pts',(8.96199994807101,1.7574828965141,-0.826222560130256));
#150917=CARTESIAN_POINT('Ctrl Pts',(8.96018629664472,1.74964163089217,-0.845674873362596));
#150918=CARTESIAN_POINT('Ctrl Pts',(8.95929854255293,1.74349822235062,-0.855007813454951));
#150919=CARTESIAN_POINT('Ctrl Pts',(8.95750774428347,1.72630637150763,-0.873591863395173));
#150920=CARTESIAN_POINT('Ctrl Pts',(8.95667250644543,1.71456563895651,-0.882077814966651));
#150921=CARTESIAN_POINT('Ctrl Pts',(8.95586708718875,1.69868853652541,-0.890194988511481));
#150922=CARTESIAN_POINT('Ctrl Pts',(8.95572392954189,1.69560796564499,-0.891633726431581));
#150923=CARTESIAN_POINT('Ctrl Pts',(8.95559065523919,1.69247211203143,-0.892970333097606));
#150924=CARTESIAN_POINT('Ctrl Pts',(8.9260274923892,1.0000000001351,-1.1515351514879));
#150925=CARTESIAN_POINT('Ctrl Pts',(8.92766867470473,1.04120750303497,-1.13881366534867));
#150926=CARTESIAN_POINT('Ctrl Pts',(8.92935061626786,1.0822780170697,-1.12556156441892));
#150927=CARTESIAN_POINT('Ctrl Pts',(8.93904928087935,1.31475831830307,-1.04765509721038));
#150928=CARTESIAN_POINT('Ctrl Pts',(8.94757446448273,1.50385659890226,-0.97336463104732));
#150929=CARTESIAN_POINT('Ctrl Pts',(8.95559065522704,1.69247211208388,-0.892970333219478));
#150930=CARTESIAN_POINT('',(8.870419798,1.69247211199998,-1.521726851));
#150931=CARTESIAN_POINT('Ctrl Pts',(8.87041979790224,1.69247211200266,-1.52172685097689));
#150932=CARTESIAN_POINT('Ctrl Pts',(8.88408033312625,1.50385659891321,-1.44209713160694));
#150933=CARTESIAN_POINT('Ctrl Pts',(8.89562637401809,1.31475831840579,-1.36821586841045));
#150934=CARTESIAN_POINT('Ctrl Pts',(8.90700321231731,1.08227801720866,-1.29053672528529));
#150935=CARTESIAN_POINT('Ctrl Pts',(8.90890743024755,1.04120750311532,-1.27731473371655));
#150936=CARTESIAN_POINT('Ctrl Pts',(8.91070977549335,1.00000000015644,-1.26461507856234));
#150937=CARTESIAN_POINT('',(8.83949283668534,1.69247211210181,-1.69214845452143));
#150938=CARTESIAN_POINT('Ctrl Pts',(8.87041979787082,1.69247211192305,-1.52172685116002));
#150939=CARTESIAN_POINT('Ctrl Pts',(8.87006004542175,1.69743933254887,-1.52382391295804));
#150940=CARTESIAN_POINT('Ctrl Pts',(8.86965795845286,1.70224131077038,-1.52616334054193));
#150941=CARTESIAN_POINT('Ctrl Pts',(8.86788175929939,1.72064855680533,-1.53646821838201));
#150942=CARTESIAN_POINT('Ctrl Pts',(8.86620740447288,1.73230722820551,-1.54612242858823));
#150943=CARTESIAN_POINT('Ctrl Pts',(8.86298306190944,1.74686546551235,-1.56447583615116));
#150944=CARTESIAN_POINT('Ctrl Pts',(8.86156527650011,1.7515583365868,-1.57249482759809));
#150945=CARTESIAN_POINT('Ctrl Pts',(8.85852229936856,1.75781013627524,-1.58954510351491));
#150946=CARTESIAN_POINT('Ctrl Pts',(8.85696462809229,1.75940739589114,-1.59820452506459));
#150947=CARTESIAN_POINT('Ctrl Pts',(8.8553662973649,1.759407395892,-1.60701205331319));
#150948=CARTESIAN_POINT('Ctrl Pts',(8.85361237719985,1.75940739589295,-1.61667695002996));
#150949=CARTESIAN_POINT('Ctrl Pts',(8.85185955172326,1.75748289667319,-1.62624391302741));
#150950=CARTESIAN_POINT('Ctrl Pts',(8.84830950960882,1.74964163105063,-1.64545534250641));
#150951=CARTESIAN_POINT('Ctrl Pts',(8.84658873105369,1.74349822250869,-1.65467113326303));
#150952=CARTESIAN_POINT('Ctrl Pts',(8.84313928061765,1.72630637166506,-1.67301984336281));
#150953=CARTESIAN_POINT('Ctrl Pts',(8.84154673036709,1.71456563911395,-1.68139676284534));
#150954=CARTESIAN_POINT('Ctrl Pts',(8.84001693566233,1.69868853665975,-1.68940906182158));
#150955=CARTESIAN_POINT('Ctrl Pts',(8.83974538685126,1.69560796575533,-1.69082917526325));
#150956=CARTESIAN_POINT('Ctrl Pts',(8.83949283657224,1.69247211211698,-1.69214845453584));
#150957=CARTESIAN_POINT('Ctrl Pts',(8.78687111482176,0.999999999979339,
-1.94702234489257));
#150958=CARTESIAN_POINT('Ctrl Pts',(8.78964603545235,1.04120750300605,-1.93449918613234));
#150959=CARTESIAN_POINT('Ctrl Pts',(8.79250911518946,1.08227801716676,-1.92145120230824));
#150960=CARTESIAN_POINT('Ctrl Pts',(8.80915221770156,1.31475831840232,-1.84472774523967));
#150961=CARTESIAN_POINT('Ctrl Pts',(8.8243024274504,1.5038565988819,-1.77150054228567));
#150962=CARTESIAN_POINT('Ctrl Pts',(8.8394928366488,1.69247211194256,-1.69214845413589));
#150963=CARTESIAN_POINT('',(8.698303553,1.69247211199998,-2.310739126));
#150964=CARTESIAN_POINT('Ctrl Pts',(8.69830355259779,1.69247211209572,-2.31073912566189));
#150965=CARTESIAN_POINT('Ctrl Pts',(8.71904704750919,1.5038565991313,-2.23265449314007));
#150966=CARTESIAN_POINT('Ctrl Pts',(8.7371692727865,1.31475831874759,-2.16010563338116));
#150967=CARTESIAN_POINT('Ctrl Pts',(8.75546341597935,1.08227801752857,-2.08375901557486));
#150968=CARTESIAN_POINT('Ctrl Pts',(8.75854517828406,1.04120750328463,-2.07076094459201));
#150969=CARTESIAN_POINT('Ctrl Pts',(8.76147865613757,1.00000000017415,-2.05827397545756));
#150970=CARTESIAN_POINT('',(8.652224619,1.69247211199998,-2.477702391));
#150971=CARTESIAN_POINT('Ctrl Pts',(8.69830355250322,1.69247211193793,-2.31073912601786));
#150972=CARTESIAN_POINT('Ctrl Pts',(8.69775726913674,1.69743933262652,-2.31279549771895));
#150973=CARTESIAN_POINT('Ctrl Pts',(8.69714709617372,1.70224131090741,-2.31508946468108));
#150974=CARTESIAN_POINT('Ctrl Pts',(8.69445432534046,1.7206485570025,-2.32519364087844));
#150975=CARTESIAN_POINT('Ctrl Pts',(8.69192131424337,1.73230722840754,-2.33465889806523));
#150976=CARTESIAN_POINT('Ctrl Pts',(8.6870647651655,1.74686546571993,-2.35264939236908));
#150977=CARTESIAN_POINT('Ctrl Pts',(8.68493387049238,1.75155833679612,-2.36050901241015));
#150978=CARTESIAN_POINT('Ctrl Pts',(8.6803747685432,1.75781013648825,-2.37721787856243));
#150979=CARTESIAN_POINT('Ctrl Pts',(8.67804714343072,1.75940739610622,-2.38570281125058));
#150980=CARTESIAN_POINT('Ctrl Pts',(8.6756657463679,1.75940739610916,-2.3943316097188));
#150981=CARTESIAN_POINT('Ctrl Pts',(8.6730525323078,1.75940739611239,-2.40380037821235));
#150982=CARTESIAN_POINT('Ctrl Pts',(8.67044918724008,1.75748289689477,-2.41317170536637));
#150983=CARTESIAN_POINT('Ctrl Pts',(8.6651913372909,1.74964163127651,-2.43198757195745));
#150984=CARTESIAN_POINT('Ctrl Pts',(8.66265138897059,1.74349822273761,-2.44101201324904));
#150985=CARTESIAN_POINT('Ctrl Pts',(8.65757105931702,1.72630637190226,-2.45897765048096));
#150986=CARTESIAN_POINT('Ctrl Pts',(8.65523401893332,1.7145656393574,-2.46717809184323));
#150987=CARTESIAN_POINT('Ctrl Pts',(8.65299216577075,1.6986885367743,-2.47502100598598));
#150988=CARTESIAN_POINT('Ctrl Pts',(8.65259441213127,1.69560796572895,-2.47641106107899));
#150989=CARTESIAN_POINT('Ctrl Pts',(8.65222461924908,1.6924721119451,-2.47770239093806));
#150990=CARTESIAN_POINT('Ctrl Pts',(8.57696801773418,1.00000000004553,-2.72683325906904));
#150991=CARTESIAN_POINT('Ctrl Pts',(8.58085433463339,1.0412075029207,-2.71460925687145));
#150992=CARTESIAN_POINT('Ctrl Pts',(8.58487550069146,1.08227801693089,-2.70187044492656));
#150993=CARTESIAN_POINT('Ctrl Pts',(8.60832904062519,1.31475831807767,-2.62694773016633));
#150994=CARTESIAN_POINT('Ctrl Pts',(8.62998229595736,1.50385659861581,-2.55537337269809));
#150995=CARTESIAN_POINT('Ctrl Pts',(8.65222461938352,1.69247211173591,-2.47770239046857));
#150996=CARTESIAN_POINT('',(8.456153681,1.69247211199998,-3.081146689));
#150997=CARTESIAN_POINT('Ctrl Pts',(8.45615368104301,1.69247211178115,-3.0811466895594));
#150998=CARTESIAN_POINT('Ctrl Pts',(8.48381312126247,1.50385659874205,-3.00523583532452));
#150999=CARTESIAN_POINT('Ctrl Pts',(8.50836562146028,1.31475831828407,-2.93460349966487));
#151000=CARTESIAN_POINT('Ctrl Pts',(8.53342977587719,1.08227801706105,-2.86020410525441));
#151001=CARTESIAN_POINT('Ctrl Pts',(8.53766427000695,1.04120750289092,-2.84753460775047));
#151002=CARTESIAN_POINT('Ctrl Pts',(8.54170526181922,0.999999999854697,
-2.83536086243177));
#151003=CARTESIAN_POINT('',(8.395293776,1.69247211199998,-3.243307326));
#151004=CARTESIAN_POINT('Ctrl Pts',(8.45615368110477,1.6924721118584,-3.08114668938989));
#151005=CARTESIAN_POINT('Ctrl Pts',(8.45542526516039,1.69743933268663,-3.08314581432304));
#151006=CARTESIAN_POINT('Ctrl Pts',(8.45461191894058,1.70224131109879,-3.08537585102182));
#151007=CARTESIAN_POINT('Ctrl Pts',(8.45102425701386,1.72064855729134,-3.09519797272746));
#151008=CARTESIAN_POINT('Ctrl Pts',(8.44765298396233,1.73230722867518,-3.10439806820348));
#151009=CARTESIAN_POINT('Ctrl Pts',(8.44120333044822,1.74686546595974,-3.12188080035487));
#151010=CARTESIAN_POINT('Ctrl Pts',(8.43837648322229,1.75155833702592,-3.12951776794703));
#151011=CARTESIAN_POINT('Ctrl Pts',(8.432337963664,1.75781013670153,-3.14575069436043));
#151012=CARTESIAN_POINT('Ctrl Pts',(8.42925912538441,1.75940739631255,-3.15399282249319));
#151013=CARTESIAN_POINT('Ctrl Pts',(8.42611383559583,1.75940739631059,-3.16237341716321));
#151014=CARTESIAN_POINT('Ctrl Pts',(8.42266236770178,1.75940739630844,-3.17156982047768));
#151015=CARTESIAN_POINT('Ctrl Pts',(8.41922946364508,1.75748289708497,-3.18067005937171));
#151016=CARTESIAN_POINT('Ctrl Pts',(8.41230613897276,1.74964163145378,-3.19893886878413));
#151017=CARTESIAN_POINT('Ctrl Pts',(8.40896747105483,1.74349822290598,-3.20769930111941));
#151018=CARTESIAN_POINT('Ctrl Pts',(8.4022971660049,1.72630637204838,-3.22513721674513));
#151019=CARTESIAN_POINT('Ctrl Pts',(8.39923445196042,1.71456563948878,-3.23309515485904));
#151020=CARTESIAN_POINT('Ctrl Pts',(8.39629859042414,1.69868853682826,-3.24070553759573));
#151021=CARTESIAN_POINT('Ctrl Pts',(8.39577783443639,1.69560796571781,-3.24205434239871));
#151022=CARTESIAN_POINT('Ctrl Pts',(8.39529377630737,1.69247211186687,-3.24330732578562));
#151023=CARTESIAN_POINT('Ctrl Pts',(8.29800821684455,0.999999999902031,
-3.48468931659343));
#151024=CARTESIAN_POINT('Ctrl Pts',(8.30297463971393,1.04120750304222,-3.47286289132727));
#151025=CARTESIAN_POINT('Ctrl Pts',(8.30812151607148,1.08227801731563,-3.4605358165655));
#151026=CARTESIAN_POINT('Ctrl Pts',(8.33819665933032,1.3147583184983,-3.38801707773433));
#151027=CARTESIAN_POINT('Ctrl Pts',(8.36617862092732,1.50385659881755,-3.31867184053366));
#151028=CARTESIAN_POINT('Ctrl Pts',(8.39529377643312,1.69247211171741,-3.24330732546012));
#151029=CARTESIAN_POINT('',(8.145919833,1.69247211199998,-3.82674667));
#151030=CARTESIAN_POINT('Ctrl Pts',(8.14591983253155,1.69247211163032,-3.8267466707334));
#151031=CARTESIAN_POINT('Ctrl Pts',(8.18027252047733,1.50385659864394,-3.75362078440848));
#151032=CARTESIAN_POINT('Ctrl Pts',(8.21105761327326,1.3147583182386,-3.68547366293637));
#151033=CARTESIAN_POINT('Ctrl Pts',(8.24268997705341,1.08227801715203,-3.61362051213516));
#151034=CARTESIAN_POINT('Ctrl Pts',(8.24804310934497,1.04120750306483,-3.6013815954542));
#151035=CARTESIAN_POINT('Ctrl Pts',(8.2531590794202,1.00000000011213,-3.58961908978988));
#151036=CARTESIAN_POINT('',(8.070768965,1.69247211199998,-3.982799055));
#151037=CARTESIAN_POINT('Ctrl Pts',(8.14591983282591,1.69247211192685,-3.82674667010681));
#151038=CARTESIAN_POINT('Ctrl Pts',(8.14501514910682,1.69743933265066,-3.8286724524188));
#151039=CARTESIAN_POINT('Ctrl Pts',(8.14400517824978,1.70224131096443,-3.8308206038134));
#151040=CARTESIAN_POINT('Ctrl Pts',(8.13955151101689,1.72064855707355,-3.84028158896136));
#151041=CARTESIAN_POINT('Ctrl Pts',(8.13536911951963,1.73230722846373,-3.84914244897219));
#151042=CARTESIAN_POINT('Ctrl Pts',(8.12737829038705,1.746865465757,-3.86597665830251));
#151043=CARTESIAN_POINT('Ctrl Pts',(8.12387825071992,1.75155833682648,-3.87332948507807));
#151044=CARTESIAN_POINT('Ctrl Pts',(8.11640893216073,1.75781013650711,-3.88895577378551));
#151045=CARTESIAN_POINT('Ctrl Pts',(8.11260366970907,1.75940739611999,-3.89688873659974));
#151046=CARTESIAN_POINT('Ctrl Pts',(8.10871981121782,1.75940739611904,-3.90495365185858));
#151047=CARTESIAN_POINT('Ctrl Pts',(8.1044578786825,1.75940739611799,-3.91380364595949));
#151048=CARTESIAN_POINT('Ctrl Pts',(8.10022305536408,1.75748289689589,-3.92255952681935));
#151049=CARTESIAN_POINT('Ctrl Pts',(8.09168999851365,1.74964163126794,-3.94013418933555));
#151050=CARTESIAN_POINT('Ctrl Pts',(8.08757949199219,1.74349822272231,-3.94856007886008));
#151051=CARTESIAN_POINT('Ctrl Pts',(8.07937291692609,1.72630637186985,-3.96532987302819));
#151052=CARTESIAN_POINT('Ctrl Pts',(8.07560918839591,1.71456563931328,-3.97298123525237));
#151053=CARTESIAN_POINT('Ctrl Pts',(8.07200295636026,1.69868853680513,-3.98029781215841));
#151054=CARTESIAN_POINT('Ctrl Pts',(8.07136339088196,1.69560796585033,-3.98159450680377));
#151055=CARTESIAN_POINT('Ctrl Pts',(8.07076896488867,1.69247211216003,-3.98279905536167));
#151056=CARTESIAN_POINT('Ctrl Pts',(7.95223773338533,1.0000000000746,-4.2144887034755));
#151057=CARTESIAN_POINT('Ctrl Pts',(7.95824427546704,1.04120750308548,-4.20315507466545));
#151058=CARTESIAN_POINT('Ctrl Pts',(7.96447542245755,1.08227801723046,-4.19133898755649));
#151059=CARTESIAN_POINT('Ctrl Pts',(8.00093002168167,1.31475831851661,-4.12180810286586));
#151060=CARTESIAN_POINT('Ctrl Pts',(8.03501539531451,1.50385659906093,-4.05525031280324));
#151061=CARTESIAN_POINT('Ctrl Pts',(8.07076896486063,1.69247211218716,-3.9827990554185));
#151062=CARTESIAN_POINT('',(7.770099827,1.69247211199998,-4.541535938));
#151063=CARTESIAN_POINT('Ctrl Pts',(7.77009982692731,1.69247211184427,-4.54153593837858));
#151064=CARTESIAN_POINT('Ctrl Pts',(7.81086917503205,1.50385659862522,-4.47178378647428));
#151065=CARTESIAN_POINT('Ctrl Pts',(7.84763899702609,1.31475831798857,-4.40667055962398));
#151066=CARTESIAN_POINT('Ctrl Pts',(7.88558488501719,1.08227801676247,-4.33794217166716));
#151067=CARTESIAN_POINT('Ctrl Pts',(7.89201355519076,1.04120750277453,-4.32623237637253));
#151068=CARTESIAN_POINT('Ctrl Pts',(7.89816331274033,0.999999999921735,
-4.31497581514458));
#151069=CARTESIAN_POINT('',(7.681263067,1.69247211199998,-4.69022363));
#151070=CARTESIAN_POINT('Ctrl Pts',(7.77009982710407,1.69247211199432,-4.54153593807615));
#151071=CARTESIAN_POINT('Ctrl Pts',(7.76902615958796,1.69743933266121,-4.54337287251751));
#151072=CARTESIAN_POINT('Ctrl Pts',(7.7678276957807,1.70224131092096,-4.54542184297812));
#151073=CARTESIAN_POINT('Ctrl Pts',(7.76254388154541,1.72064855696661,-4.55444551730448));
#151074=CARTESIAN_POINT('Ctrl Pts',(7.75758404575993,1.73230722834436,-4.56289579941117));
#151075=CARTESIAN_POINT('Ctrl Pts',(7.74811637846731,1.74686546562212,-4.57894594675687));
#151076=CARTESIAN_POINT('Ctrl Pts',(7.74397132662032,1.75155833668634,-4.58595543207492));
#151077=CARTESIAN_POINT('Ctrl Pts',(7.73513134762145,1.75781013635739,-4.60084926938084));
#151078=CARTESIAN_POINT('Ctrl Pts',(7.73063029873371,1.75940739596569,-4.60840919532057));
#151079=CARTESIAN_POINT('Ctrl Pts',(7.72603914208534,1.75940739596087,-4.61609349720791));
#151080=CARTESIAN_POINT('Ctrl Pts',(7.72100105948174,1.75940739595559,-4.62452582714664));
#151081=CARTESIAN_POINT('Ctrl Pts',(7.71599841320752,1.75748289672922,-4.63286685276752));
#151082=CARTESIAN_POINT('Ctrl Pts',(7.70592432733086,1.74964163109228,-4.64960586754053));
#151083=CARTESIAN_POINT('Ctrl Pts',(7.70107507758454,1.74349822254039,-4.65762937394834));
#151084=CARTESIAN_POINT('Ctrl Pts',(7.69139830701292,1.72630637167157,-4.6735960261417));
#151085=CARTESIAN_POINT('Ctrl Pts',(7.68696386732323,1.71456563910334,-4.68087920820853));
#151086=CARTESIAN_POINT('Ctrl Pts',(7.68271630004147,1.6986885366654,-4.68784307054307));
#151087=CARTESIAN_POINT('Ctrl Pts',(7.68196307447331,1.69560796579604,-4.68907721483747));
#151088=CARTESIAN_POINT('Ctrl Pts',(7.68126306658054,1.692472112194,-4.69022363027454));
#151089=CARTESIAN_POINT('Ctrl Pts',(7.54244050719113,0.999999999972247,
-4.91035550601811));
#151090=CARTESIAN_POINT('Ctrl Pts',(7.54943880738768,1.0412075031992,-4.89960592529646));
#151091=CARTESIAN_POINT('Ctrl Pts',(7.55670405553103,1.08227801755879,-4.88839596193518));
#151092=CARTESIAN_POINT('Ctrl Pts',(7.59924459970586,1.31475831885198,-4.82241275323143));
#151093=CARTESIAN_POINT('Ctrl Pts',(7.63915894989652,1.50385659919618,-4.75917829468802));
#151094=CARTESIAN_POINT('Ctrl Pts',(7.6812630666695,1.69247211212086,-4.69022363012885));
#151095=CARTESIAN_POINT('',(7.331719547,1.69247211199998,-5.219759428));
#151096=CARTESIAN_POINT('Ctrl Pts',(7.33171954715669,1.69247211218445,-5.2197594275829));
#151097=CARTESIAN_POINT('Ctrl Pts',(7.37857730449581,1.5038565990772,-5.15394261357347));
#151098=CARTESIAN_POINT('Ctrl Pts',(7.42103580661076,1.31475831855127,-5.09238753490902));
#151099=CARTESIAN_POINT('Ctrl Pts',(7.46498970082048,1.08227801722486,-5.02733727038339));
#151100=CARTESIAN_POINT('Ctrl Pts',(7.47244214905171,1.04120750302035,-5.01625087677695));
#151101=CARTESIAN_POINT('Ctrl Pts',(7.47957617988741,0.999999999949517,
-5.00559089111973));
#151102=CARTESIAN_POINT('',(7.229912155,1.69247211199998,-5.359885281));
#151103=CARTESIAN_POINT('Ctrl Pts',(7.33171954712374,1.69247211216015,-5.21975942762917));
#151104=CARTESIAN_POINT('Ctrl Pts',(7.33048554037461,1.69743933266443,-5.22149272425506));
#151105=CARTESIAN_POINT('Ctrl Pts',(7.32910823297432,1.70224131077121,-5.22342601663965));
#151106=CARTESIAN_POINT('Ctrl Pts',(7.32303681394073,1.72064855669899,-5.2319397267822));
#151107=CARTESIAN_POINT('Ctrl Pts',(7.31733946754646,1.7323072280976,-5.23991139428903));
#151108=CARTESIAN_POINT('Ctrl Pts',(7.30647119017968,1.74686546540271,-5.25504825331498));
#151109=CARTESIAN_POINT('Ctrl Pts',(7.30171449967183,1.75155833647675,-5.26165796092615));
#151110=CARTESIAN_POINT('Ctrl Pts',(7.29157503454324,1.75781013616406,-5.27569943042096));
#151111=CARTESIAN_POINT('Ctrl Pts',(7.2864144390166,1.75940739577923,-5.2828254514138));
#151112=CARTESIAN_POINT('Ctrl Pts',(7.28115294950206,1.7594073957793,-5.29006727045672));
#151113=CARTESIAN_POINT('Ctrl Pts',(7.27537928051152,1.75940739577936,-5.29801404407049));
#151114=CARTESIAN_POINT('Ctrl Pts',(7.26964908964958,1.7574828965588,-5.30587305741948));
#151115=CARTESIAN_POINT('Ctrl Pts',(7.25811508536945,1.74964163093468,-5.32164165174141));
#151116=CARTESIAN_POINT('Ctrl Pts',(7.25256613571055,1.74349822239163,-5.32919817447285));
#151117=CARTESIAN_POINT('Ctrl Pts',(7.24149708131024,1.7263063715449,-5.34423313058701));
#151118=CARTESIAN_POINT('Ctrl Pts',(7.23642763396644,1.71456563899135,-5.35108949259296));
#151119=CARTESIAN_POINT('Ctrl Pts',(7.23157293031562,1.69868853650539,-5.3576445714967));
#151120=CARTESIAN_POINT('Ctrl Pts',(7.23071210915306,1.69560796557039,-5.3588062288934));
#151121=CARTESIAN_POINT('Ctrl Pts',(7.2299121553839,1.69247211190049,-5.35988528099549));
#151122=CARTESIAN_POINT('Ctrl Pts',(7.07191598531854,0.999999999848429,
-5.56668701263112));
#151123=CARTESIAN_POINT('Ctrl Pts',(7.0798496973723,1.04120750290071,-5.55660802939234));
#151124=CARTESIAN_POINT('Ctrl Pts',(7.08809055109799,1.08227801708678,-5.54609444591211));
#151125=CARTESIAN_POINT('Ctrl Pts',(7.13637452878035,1.31475831838269,-5.48419017118036));
#151126=CARTESIAN_POINT('Ctrl Pts',(7.18179648874699,1.50385659889642,-5.42478817067091));
#151127=CARTESIAN_POINT('Ctrl Pts',(7.22991215525667,1.69247211199201,-5.35988528116711));
#151128=CARTESIAN_POINT('',(6.834308572,1.69247211199998,-5.855956484));
#151129=CARTESIAN_POINT('Ctrl Pts',(6.83430857185789,1.69247211190127,-5.85595648418171));
#151130=CARTESIAN_POINT('Ctrl Pts',(6.88687746734898,1.50385659885685,-5.79460492632121));
#151131=CARTESIAN_POINT('Ctrl Pts',(6.93468279871554,1.31475831839393,-5.73710360111202));
#151132=CARTESIAN_POINT('Ctrl Pts',(6.98429080820646,1.08227801718584,-5.67625520655512));
#151133=CARTESIAN_POINT('Ctrl Pts',(6.99270703172362,1.04120750303555,-5.66588147583171));
#151134=CARTESIAN_POINT('Ctrl Pts',(7.0007678967871,1.00000000001932,-5.65590389374811));
#151135=CARTESIAN_POINT('',(6.720350242,1.69247211199998,-5.986392288));
#151136=CARTESIAN_POINT('Ctrl Pts',(6.83430857189648,1.69247211192666,-5.85595648413667));
#151137=CARTESIAN_POINT('Ctrl Pts',(6.83292416134052,1.69743933264487,-5.85757218755852));
#151138=CARTESIAN_POINT('Ctrl Pts',(6.83137909952495,1.70224131095345,-5.85937423625887));
#151139=CARTESIAN_POINT('Ctrl Pts',(6.82456895907562,1.72064855706258,-5.86730943498248));
#151140=CARTESIAN_POINT('Ctrl Pts',(6.81817997375613,1.73230722845711,-5.87473830470636));
#151141=CARTESIAN_POINT('Ctrl Pts',(6.80599859129646,1.74686546575594,-5.88884000231498));
#151142=CARTESIAN_POINT('Ctrl Pts',(6.80066856020435,1.75155833682737,-5.89499671473559));
#151143=CARTESIAN_POINT('Ctrl Pts',(6.78931124596146,1.75781013651138,-5.90807276275262));
#151144=CARTESIAN_POINT('Ctrl Pts',(6.78353265387896,1.75940739612577,-5.91470750426196));
#151145=CARTESIAN_POINT('Ctrl Pts',(6.77764319392101,1.75940739612599,-5.92144853358502));
#151146=CARTESIAN_POINT('Ctrl Pts',(6.77118042472805,1.75940739612624,-5.92884576812756));
#151147=CARTESIAN_POINT('Ctrl Pts',(6.76476882540303,1.75748289690548,-5.93615949305174));
#151148=CARTESIAN_POINT('Ctrl Pts',(6.75186776773318,1.74964163128043,-5.95083070747795));
#151149=CARTESIAN_POINT('Ctrl Pts',(6.74566379503783,1.74349822273683,-5.95785940585845));
#151150=CARTESIAN_POINT('Ctrl Pts',(6.73329157831985,1.72630637188949,-5.97184161327271));
#151151=CARTESIAN_POINT('Ctrl Pts',(6.72762793952884,1.71456563933645,-5.97821595182398));
#151152=CARTESIAN_POINT('Ctrl Pts',(6.72220518672269,1.69868853678518,-5.98430946965148));
#151153=CARTESIAN_POINT('Ctrl Pts',(6.72124370078741,1.69560796578166,-5.98538928716462));
#151154=CARTESIAN_POINT('Ctrl Pts',(6.72035024189579,1.69247211204104,-5.98639228803552));
#151155=CARTESIAN_POINT('Ctrl Pts',(6.54445255413051,0.999999999900245,
-6.17819882868257));
#151156=CARTESIAN_POINT('Ctrl Pts',(6.553257800479,1.04120750293032,-6.16887159293748));
#151157=CARTESIAN_POINT('Ctrl Pts',(6.56240790930224,1.08227801709433,-6.15913903849141));
#151158=CARTESIAN_POINT('Ctrl Pts',(6.6160465662733,1.31475831833009,-6.10181211457691));
#151159=CARTESIAN_POINT('Ctrl Pts',(6.66661042504181,1.5038565988065,-6.0467208421714));
#151160=CARTESIAN_POINT('Ctrl Pts',(6.72035024216997,1.69247211186447,-5.98639228772773));
#151161=CARTESIAN_POINT('',(6.281871763,1.69247211199998,-6.445004822));
#151162=CARTESIAN_POINT('Ctrl Pts',(6.28187176315731,1.69247211214928,-6.44500482166204));
#151163=CARTESIAN_POINT('Ctrl Pts',(6.33972854297822,1.50385659908022,-6.38861248658687));
#151164=CARTESIAN_POINT('Ctrl Pts',(6.39249580318891,1.31475831859254,-6.33562788166308));
#151165=CARTESIAN_POINT('Ctrl Pts',(6.44735851345534,1.08227801735199,-6.27947127252895));
#151166=CARTESIAN_POINT('Ctrl Pts',(6.45667074978433,1.04120750319416,-6.26989372785291));
#151167=CARTESIAN_POINT('Ctrl Pts',(6.46559354773797,1.00000000017037,-6.26067888295264));
#151168=CARTESIAN_POINT('',(6.15668002,1.69247211199998,-6.564700384));
#151169=CARTESIAN_POINT('Ctrl Pts',(6.28187176296278,1.69247211203293,-6.44500482185164));
#151170=CARTESIAN_POINT('Ctrl Pts',(6.28034809508384,1.69743933281709,-6.44648992333557));
#151171=CARTESIAN_POINT('Ctrl Pts',(6.27864771881356,1.70224131118791,-6.44814621926316));
#151172=CARTESIAN_POINT('Ctrl Pts',(6.27115368823405,1.72064855735323,-6.45543901695008));
#151173=CARTESIAN_POINT('Ctrl Pts',(6.26412450434272,1.73230722874697,-6.46226527600085));
#151174=CARTESIAN_POINT('Ctrl Pts',(6.25072809411953,1.74686546604395,-6.47521827361668));
#151175=CARTESIAN_POINT('Ctrl Pts',(6.24486763671979,1.75155833711437,-6.48087242061939));
#151176=CARTESIAN_POINT('Ctrl Pts',(6.23238391577944,1.7578101367976,-6.49287776651093));
#151177=CARTESIAN_POINT('Ctrl Pts',(6.22603385296701,1.75940739641221,-6.4989678095005));
#151178=CARTESIAN_POINT('Ctrl Pts',(6.21956384103444,1.75940739641324,-6.50515377430056));
#151179=CARTESIAN_POINT('Ctrl Pts',(6.21246400605725,1.75940739641437,-6.51194191158886));
#151180=CARTESIAN_POINT('Ctrl Pts',(6.20542262069756,1.75748289719422,-6.51865146227563));
#151181=CARTESIAN_POINT('Ctrl Pts',(6.19125838137018,1.74964163157005,-6.53210717281417));
#151182=CARTESIAN_POINT('Ctrl Pts',(6.18444933637955,1.74349822302713,-6.53855145589715));
#151183=CARTESIAN_POINT('Ctrl Pts',(6.17087357116009,1.72630637218225,-6.55136833809903));
#151184=CARTESIAN_POINT('Ctrl Pts',(6.16466134121213,1.71456563963166,-6.55720933076995));
#151185=CARTESIAN_POINT('Ctrl Pts',(6.15871420003383,1.69868853693743,-6.56279222612325));
#151186=CARTESIAN_POINT('Ctrl Pts',(6.15765979061543,1.69560796578235,-6.56378150971813));
#151187=CARTESIAN_POINT('Ctrl Pts',(6.15668002018172,1.69247211188529,-6.56470038380239));
#151188=CARTESIAN_POINT('Ctrl Pts',(5.96429703930701,0.999999999993495,
-6.73996742031544));
#151189=CARTESIAN_POINT('Ctrl Pts',(5.97390292527019,1.04120750293781,-6.73146702949198));
#151190=CARTESIAN_POINT('Ctrl Pts',(5.98388861787979,1.08227801701666,-6.7225938648969));
#151191=CARTESIAN_POINT('Ctrl Pts',(6.04245008719923,1.31475831813608,-6.67030585448667));
#151192=CARTESIAN_POINT('Ctrl Pts',(6.09774873431317,1.50385659858127,-6.61996887270678));
#151193=CARTESIAN_POINT('Ctrl Pts',(6.15668002065362,1.69247211160818,-6.56470038335982));
#151194=CARTESIAN_POINT('',(5.678857015,1.69247211199998,-6.982161771));
#151195=CARTESIAN_POINT('Ctrl Pts',(5.67885701527804,1.69247211202244,-6.98216177125877));
#151196=CARTESIAN_POINT('Ctrl Pts',(5.74153585071579,1.50385659882619,-6.93118269686947));
#151197=CARTESIAN_POINT('Ctrl Pts',(5.79884018886956,1.31475831821191,-6.88314141309411));
#151198=CARTESIAN_POINT('Ctrl Pts',(5.85851587764468,1.08227801691581,-6.83212872938778));
#151199=CARTESIAN_POINT('Ctrl Pts',(5.86864915011615,1.04120750283384,-6.82342448353686));
#151200=CARTESIAN_POINT('Ctrl Pts',(5.87836203982082,0.999999999886374,
-6.81504656835106));
#151201=CARTESIAN_POINT('',(5.54343983025803,1.69247211212479,-7.09015337246984));
#151202=CARTESIAN_POINT('Ctrl Pts',(5.678857014964,1.69247211184902,-6.98216177151419));
#151203=CARTESIAN_POINT('Ctrl Pts',(5.67720635746447,1.6974393325806,-6.98350431387102));
#151204=CARTESIAN_POINT('Ctrl Pts',(5.67536435720178,1.70224131090145,-6.98500152147185));
#151205=CARTESIAN_POINT('Ctrl Pts',(5.66724677406077,1.72064855700609,-6.9915932007598));
#151206=CARTESIAN_POINT('Ctrl Pts',(5.65963398645625,1.73230722838638,-6.9977618881084));
#151207=CARTESIAN_POINT('Ctrl Pts',(5.64513040849172,1.74686546566725,-7.00946189580317));
#151208=CARTESIAN_POINT('Ctrl Pts',(5.63878670974101,1.7515583367325,-7.01456795351954));
#151209=CARTESIAN_POINT('Ctrl Pts',(5.6252770936824,1.75781013640549,-7.02540593729717));
#151210=CARTESIAN_POINT('Ctrl Pts',(5.61840668711161,1.75940739601474,-7.03090224832022));
#151211=CARTESIAN_POINT('Ctrl Pts',(5.61140821593638,1.75940739601077,-7.03648334284404));
#151212=CARTESIAN_POINT('Ctrl Pts',(5.60372847887254,1.75940739600641,-7.04260772878465));
#151213=CARTESIAN_POINT('Ctrl Pts',(5.59611400057448,1.75748289678096,-7.04865908387314));
#151214=CARTESIAN_POINT('Ctrl Pts',(5.58080062171539,1.74964163114593,-7.06079095305036));
#151215=CARTESIAN_POINT('Ctrl Pts',(5.57344132685394,1.74349822259538,-7.0665989352571));
#151216=CARTESIAN_POINT('Ctrl Pts',(5.55877131720443,1.72630637173008,-7.0781472982493));
#151217=CARTESIAN_POINT('Ctrl Pts',(5.55206051331797,1.71456563916439,-7.08340791680299));
#151218=CARTESIAN_POINT('Ctrl Pts',(5.54563686680511,1.69868853671578,-7.08843523935245));
#151219=CARTESIAN_POINT('Ctrl Pts',(5.54449802352356,1.69560796583262,-7.08932602377848));
#151220=CARTESIAN_POINT('Ctrl Pts',(5.54343983019798,1.69247211221631,-7.09015337273987));
#151221=CARTESIAN_POINT('Ctrl Pts',(5.33612051021732,1.00000000003863,-7.24746975850455));
#151222=CARTESIAN_POINT('Ctrl Pts',(5.34644969490054,1.04120750312078,-7.23986465271198));
#151223=CARTESIAN_POINT('Ctrl Pts',(5.35719057242632,1.08227801733654,-7.23192231942854));
#151224=CARTESIAN_POINT('Ctrl Pts',(5.42020335165464,1.3147583185972,-7.1850942147898));
#151225=CARTESIAN_POINT('Ctrl Pts',(5.47979155494116,1.50385659904842,-7.13991680741592));
#151226=CARTESIAN_POINT('Ctrl Pts',(5.54343983044598,1.69247211208145,-7.09015337254597));
#151227=CARTESIAN_POINT('',(5.030119452,1.69247211199998,-7.463102458));
#151228=CARTESIAN_POINT('Ctrl Pts',(5.03011945219447,1.69247211210035,-7.4631024578693));
#151229=CARTESIAN_POINT('Ctrl Pts',(5.09711568993067,1.50385659918751,-7.41794709780783));
#151230=CARTESIAN_POINT('Ctrl Pts',(5.15849572502523,1.31475831885526,-7.37523593545209));
#151231=CARTESIAN_POINT('Ctrl Pts',(5.22250391870522,1.08227801764803,-7.3297779013181));
#151232=CARTESIAN_POINT('Ctrl Pts',(5.23337664023476,1.0412075033625,-7.32201703570375));
#151233=CARTESIAN_POINT('Ctrl Pts',(5.24380141927541,1.00000000021015,-7.31454350422534));
#151234=CARTESIAN_POINT('',(4.885567124,1.69247211199998,-7.558520614));
#151235=CARTESIAN_POINT('Ctrl Pts',(5.03011945218954,1.69247211209782,-7.46310245787263));
#151236=CARTESIAN_POINT('Ctrl Pts',(5.02835509520953,1.69743933274049,-7.46429163173374));
#151237=CARTESIAN_POINT('Ctrl Pts',(5.0263863016777,1.70224131097822,-7.46561769636424));
#151238=CARTESIAN_POINT('Ctrl Pts',(5.01771052400475,1.72064855704178,-7.47145518492247));
#151239=CARTESIAN_POINT('Ctrl Pts',(5.00957542636926,1.7323072284545,-7.47691663393612));
#151240=CARTESIAN_POINT('Ctrl Pts',(4.99408145493216,1.74686546577659,-7.48726945014651));
#151241=CARTESIAN_POINT('Ctrl Pts',(4.98730559056023,1.75155833685605,-7.49178630760795));
#151242=CARTESIAN_POINT('Ctrl Pts',(4.97287885086278,1.75781013655407,-7.50136966821126));
#151243=CARTESIAN_POINT('Ctrl Pts',(4.96554341700395,1.7594073961748,-7.50622799421012));
#151244=CARTESIAN_POINT('Ctrl Pts',(4.95807283415526,1.75940739618001,-7.51115928277464));
#151245=CARTESIAN_POINT('Ctrl Pts',(4.94987502773369,1.75940739618573,-7.51657060741685));
#151246=CARTESIAN_POINT('Ctrl Pts',(4.94174876379916,1.75748289697065,-7.52191504495913));
#151247=CARTESIAN_POINT('Ctrl Pts',(4.92540953973939,1.74964163135777,-7.53262539410137));
#151248=CARTESIAN_POINT('Ctrl Pts',(4.91755924773006,1.7434982228226,-7.53775031297301));
#151249=CARTESIAN_POINT('Ctrl Pts',(4.90191310796274,1.72630637199696,-7.54793717612113));
#151250=CARTESIAN_POINT('Ctrl Pts',(4.89475776159462,1.71456563945896,-7.55257506514705));
#151251=CARTESIAN_POINT('Ctrl Pts',(4.88790932897337,1.69868853680129,-7.55700633800827));
#151252=CARTESIAN_POINT('Ctrl Pts',(4.88669522094921,1.69560796567097,-7.55779145133232));
#151253=CARTESIAN_POINT('Ctrl Pts',(4.88556712453283,1.69247211179938,-7.5585206139617));
#151254=CARTESIAN_POINT('Ctrl Pts',(4.66498067898464,0.999999999967123,
-7.69661972977099));
#151255=CARTESIAN_POINT('Ctrl Pts',(4.67594999777918,1.04120750284047,-7.68997114090538));
#151256=CARTESIAN_POINT('Ctrl Pts',(4.6873595808967,1.08227801684883,-7.68302358599243));
#151257=CARTESIAN_POINT('Ctrl Pts',(4.75431632809316,1.31475831803052,-7.6420324195285));
#151258=CARTESIAN_POINT('Ctrl Pts',(4.81771431840041,1.50385659860426,-7.60237832843866));
#151259=CARTESIAN_POINT('Ctrl Pts',(4.88556712461049,1.69247211175979,-7.55852061391151));
#151260=CARTESIAN_POINT('',(4.340882323,1.69247211199998,-7.883954633));
#151261=CARTESIAN_POINT('Ctrl Pts',(4.34088232282825,1.69247211188109,-7.88395463326351));
#151262=CARTESIAN_POINT('Ctrl Pts',(4.41165654866182,1.50385659901075,-7.84498655187241));
#151263=CARTESIAN_POINT('Ctrl Pts',(4.47661808484275,1.31475831872082,-7.80794939604147));
#151264=CARTESIAN_POINT('Ctrl Pts',(4.54444342707815,1.08227801765357,-7.76841201286517));
#151265=CARTESIAN_POINT('Ctrl Pts',(4.55596805683155,1.04120750346539,-7.76165701347467));
#151266=CARTESIAN_POINT('Ctrl Pts',(4.56702079094976,1.00000000041109,-7.75514803824096));
#151267=CARTESIAN_POINT('',(4.188358703,1.69247211199998,-7.966031093));
#151268=CARTESIAN_POINT('Ctrl Pts',(4.34088232285577,1.69247211189453,-7.88395463324836));
#151269=CARTESIAN_POINT('Ctrl Pts',(4.33901847194056,1.69743933251756,-7.88498086410161));
#151270=CARTESIAN_POINT('Ctrl Pts',(4.33693873668266,1.70224131073673,-7.88612510909012));
#151271=CARTESIAN_POINT('Ctrl Pts',(4.32777461670889,1.72064855678308,-7.8911614069149));
#151272=CARTESIAN_POINT('Ctrl Pts',(4.31918270807021,1.73230722819561,-7.89587164520932));
#151273=CARTESIAN_POINT('Ctrl Pts',(4.30282309151686,1.74686546551823,-7.90479391513174));
#151274=CARTESIAN_POINT('Ctrl Pts',(4.29566961680087,1.75155833659819,-7.90868520525309));
#151275=CARTESIAN_POINT('Ctrl Pts',(4.28044190909277,1.75781013629617,-7.91693678308729));
#151276=CARTESIAN_POINT('Ctrl Pts',(4.27270050854823,1.75940739591638,-7.92111800767207));
#151277=CARTESIAN_POINT('Ctrl Pts',(4.26481796277002,1.75940739592062,-7.92535978643457));
#151278=CARTESIAN_POINT('Ctrl Pts',(4.25616809090658,1.75940739592527,-7.93001448097121));
#151279=CARTESIAN_POINT('Ctrl Pts',(4.24759546923469,1.75748289670936,-7.93460897069477));
#151280=CARTESIAN_POINT('Ctrl Pts',(4.23036195379284,1.74964163109505,-7.94381156636527));
#151281=CARTESIAN_POINT('Ctrl Pts',(4.22208387056526,1.74349822255884,-7.94821215906903));
#151282=CARTESIAN_POINT('Ctrl Pts',(4.20558757418279,1.7263063717299,-7.95695550374436));
#151283=CARTESIAN_POINT('Ctrl Pts',(4.19804529596739,1.71456563918895,-7.96093332168898));
#151284=CARTESIAN_POINT('Ctrl Pts',(4.19082721695448,1.69868853668133,-7.96473286674421));
#151285=CARTESIAN_POINT('Ctrl Pts',(4.18954761961683,1.69560796571051,-7.96540598759677));
#151286=CARTESIAN_POINT('Ctrl Pts',(4.18835870300193,1.69247211200357,-7.96603109302166));
#151287=CARTESIAN_POINT('Ctrl Pts',(3.95628116469446,1.00000000003948,-8.08380104566434));
#151288=CARTESIAN_POINT('Ctrl Pts',(3.96780229915045,1.04120750292555,-8.07816250421748));
#151289=CARTESIAN_POINT('Ctrl Pts',(3.97978872466482,1.08227801694657,-8.0722656652622));
#151290=CARTESIAN_POINT('Ctrl Pts',(4.05015034350906,1.31475831811704,-8.03744147373217));
#151291=CARTESIAN_POINT('Ctrl Pts',(4.11684767745441,1.50385659866781,-8.00362997039905));
#151292=CARTESIAN_POINT('Ctrl Pts',(4.18835870342248,1.69247211180005,-7.96603109280055));
#151293=CARTESIAN_POINT('',(3.61669496163465,1.69247211178013,-8.24132984144472));
#151294=CARTESIAN_POINT('Ctrl Pts',(3.61669496156912,1.69247211175992,-8.24132984141276));
#151295=CARTESIAN_POINT('Ctrl Pts',(3.69067734322808,1.5038565985687,-8.20886278668498));
#151296=CARTESIAN_POINT('Ctrl Pts',(3.75869734856277,1.3147583179601,-8.17779783869765));
#151297=CARTESIAN_POINT('Ctrl Pts',(3.82979374964924,1.08227801680555,-8.14449943819061));
#151298=CARTESIAN_POINT('Ctrl Pts',(3.84187749804066,1.04120750286063,-8.13880469232044));
#151299=CARTESIAN_POINT('Ctrl Pts',(3.85346919708018,1.00000000005117,-8.13331267978517));
#151300=CARTESIAN_POINT('',(3.45742808,1.69247211199998,-8.309403774));
#151301=CARTESIAN_POINT('Ctrl Pts',(3.61669496113721,1.69247211155784,-8.2413298416023));
#151302=CARTESIAN_POINT('Ctrl Pts',(3.61474662287773,1.69743933229287,-8.24218486685928));
#151303=CARTESIAN_POINT('Ctrl Pts',(3.61257269064702,1.702241310617,-8.24313807944231));
#151304=CARTESIAN_POINT('Ctrl Pts',(3.60299401241548,1.72064855672639,-8.24733263725376));
#151305=CARTESIAN_POINT('Ctrl Pts',(3.59401446977581,1.73230722810798,-8.25125374075692));
#151306=CARTESIAN_POINT('Ctrl Pts',(3.57692092613147,1.74686546539134,-8.25867362751413));
#151307=CARTESIAN_POINT('Ctrl Pts',(3.56944743664772,1.75155833645782,-8.26190801991309));
#151308=CARTESIAN_POINT('Ctrl Pts',(3.55354136548705,1.75781013613199,-8.2687613781201));
#151309=CARTESIAN_POINT('Ctrl Pts',(3.54545632746743,1.75940739574123,-8.2722318365261));
#151310=CARTESIAN_POINT('Ctrl Pts',(3.53722528439024,1.75940739573664,-8.27574995317466));
#151311=CARTESIAN_POINT('Ctrl Pts',(3.52819299076564,1.7594073957316,-8.27961054074264));
#151312=CARTESIAN_POINT('Ctrl Pts',(3.51924303306519,1.75748289650574,-8.28341809051765));
#151313=CARTESIAN_POINT('Ctrl Pts',(3.50125398036881,1.74964163087024,-8.29103883882884));
#151314=CARTESIAN_POINT('Ctrl Pts',(3.4926147561768,1.74349822231929,-8.29467967438142));
#151315=CARTESIAN_POINT('Ctrl Pts',(3.47540112164681,1.72630637145232,-8.30190910431719));
#151316=CARTESIAN_POINT('Ctrl Pts',(3.46753263756868,1.71456563888475,-8.30519482413073));
#151317=CARTESIAN_POINT('Ctrl Pts',(3.46000302790207,1.69868853650819,-8.30833204968783));
#151318=CARTESIAN_POINT('Ctrl Pts',(3.45866824382614,1.69560796570203,-8.30888775850462));
#151319=CARTESIAN_POINT('Ctrl Pts',(3.45742807947873,1.69247211216522,-8.30940377375128));
#151320=CARTESIAN_POINT('Ctrl Pts',(3.21572799916628,1.00000000027708,-8.40589634931207));
#151321=CARTESIAN_POINT('Ctrl Pts',(3.22770818794206,1.04120750338201,-8.40131325348497));
#151322=CARTESIAN_POINT('Ctrl Pts',(3.2401749482664,1.08227801762046,-8.39651460834608));
#151323=CARTESIAN_POINT('Ctrl Pts',(3.31337492842116,1.31475831887219,-8.36813777565844));
#151324=CARTESIAN_POINT('Ctrl Pts',(3.3828345982506,1.50385659929336,-8.34044109045194));
#151325=CARTESIAN_POINT('Ctrl Pts',(3.45742807919782,1.69247211229553,-8.30940377386816));
#151326=CARTESIAN_POINT('',(2.8633881,1.69247211199998,-8.532350707));
#151327=CARTESIAN_POINT('Ctrl Pts',(2.86338810042523,1.69247211217985,-8.53235070694725));
#151328=CARTESIAN_POINT('Ctrl Pts',(2.93998297503229,1.50385659913088,-8.50664608461792));
#151329=CARTESIAN_POINT('Ctrl Pts',(3.01051379221962,1.31475831866339,-8.48180346126633));
#151330=CARTESIAN_POINT('Ctrl Pts',(3.08430882573711,1.08227801739708,-8.45501214257094));
#151331=CARTESIAN_POINT('Ctrl Pts',(3.09685440167008,1.04120750319233,-8.45042350089904));
#151332=CARTESIAN_POINT('Ctrl Pts',(3.10889173621482,1.00000000012129,-8.44599266945545));
#151333=CARTESIAN_POINT('',(2.698660279,1.69247211199998,-8.585874021));
#151334=CARTESIAN_POINT('Ctrl Pts',(2.86338809984566,1.69247211191797,-8.53235070714175));
#151335=CARTESIAN_POINT('Ctrl Pts',(2.86137096114923,1.69743933266371,-8.53302764262381));
#151336=CARTESIAN_POINT('Ctrl Pts',(2.85912033521171,1.70224131099841,-8.53378214807124));
#151337=CARTESIAN_POINT('Ctrl Pts',(2.84920422065504,1.72064855713832,-8.53710119373165));
#151338=CARTESIAN_POINT('Ctrl Pts',(2.83990934200035,1.73230722853923,-8.54020159203121));
#151339=CARTESIAN_POINT('Ctrl Pts',(2.82221949840695,1.746865465846,-8.54605935507156));
#151340=CARTESIAN_POINT('Ctrl Pts',(2.81448616629378,1.75155833692005,-8.54861080832647));
#151341=CARTESIAN_POINT('Ctrl Pts',(2.79802979800296,1.7578101366089,-8.55401076770457));
#151342=CARTESIAN_POINT('Ctrl Pts',(2.78966621847435,1.75940739622565,-8.55674251784626));
#151343=CARTESIAN_POINT('Ctrl Pts',(2.78115294960864,1.7594073962279,-8.55950864658031));
#151344=CARTESIAN_POINT('Ctrl Pts',(2.77181095693985,1.75940739623038,-8.56254404400075));
#151345=CARTESIAN_POINT('Ctrl Pts',(2.76255572300506,1.75748289701185,-8.56553399767843));
#151346=CARTESIAN_POINT('Ctrl Pts',(2.74395597033507,1.74964163139145,-8.57151154084734));
#151347=CARTESIAN_POINT('Ctrl Pts',(2.73502516313977,1.74349822285109,-8.57436330538031));
#151348=CARTESIAN_POINT('Ctrl Pts',(2.71723278454769,1.72630637201231,-8.58002061345237));
#151349=CARTESIAN_POINT('Ctrl Pts',(2.70910144702475,1.71456563946542,-8.58258778044829));
#151350=CARTESIAN_POINT('Ctrl Pts',(2.7013209304805,1.69868853681972,-8.58503742749617));
#151351=CARTESIAN_POINT('Ctrl Pts',(2.69994170637387,1.69560796571128,-8.58547125010984));
#151352=CARTESIAN_POINT('Ctrl Pts',(2.69866027920764,1.69247211186233,-8.5858740205891));
#151353=CARTESIAN_POINT('Ctrl Pts',(2.44928368492693,1.00000000003541,-8.66031231715986));
#151354=CARTESIAN_POINT('Ctrl Pts',(2.46162647047221,1.04120750294047,-8.65682156738601));
#151355=CARTESIAN_POINT('Ctrl Pts',(2.47447319045866,1.08227801698034,-8.65315975197741));
#151356=CARTESIAN_POINT('Ctrl Pts',(2.54992216866385,1.31475831816348,-8.63145875170902));
#151357=CARTESIAN_POINT('Ctrl Pts',(2.62158492606628,1.50385659870848,-8.61009988199061));
#151358=CARTESIAN_POINT('Ctrl Pts',(2.69866027926731,1.69247211183557,-8.58587402057035));
#151359=CARTESIAN_POINT('',(2.08702692,1.69247211199998,-8.754674102));
#151360=CARTESIAN_POINT('Ctrl Pts',(2.08702692043405,1.69247211217429,-8.75467410206591));
#151361=CARTESIAN_POINT('Ctrl Pts',(2.1656175912421,1.50385659900165,-8.7359388706045));
#151362=CARTESIAN_POINT('Ctrl Pts',(2.2380913477429,1.31475831841118,-8.71751859004947));
#151363=CARTESIAN_POINT('Ctrl Pts',(2.31399085943843,1.08227801716552,-8.69745006113722));
#151364=CARTESIAN_POINT('Ctrl Pts',(2.32689725319462,1.04120750310917,-8.69400446875687));
#151365=CARTESIAN_POINT('Ctrl Pts',(2.33928330559697,1.00000000018754,-8.69067049289957));
#151366=CARTESIAN_POINT('',(1.918164453,1.69247211199998,-8.793215858));
#151367=CARTESIAN_POINT('Ctrl Pts',(2.08702692043181,1.69247211217334,-8.75467410206644));
#151368=CARTESIAN_POINT('Ctrl Pts',(2.08495722210436,1.69743933294414,-8.75516749748884));
#151369=CARTESIAN_POINT('Ctrl Pts',(2.08264802316623,1.70224131130219,-8.75571722096838));
#151370=CARTESIAN_POINT('Ctrl Pts',(2.0724743109975,1.72064855744848,-8.7581340314743));
#151371=CARTESIAN_POINT('Ctrl Pts',(2.06293893323256,1.73230722883562,-8.76038876198234));
#151372=CARTESIAN_POINT('Ctrl Pts',(2.04479521792301,1.74686546612392,-8.76463723803522));
#151373=CARTESIAN_POINT('Ctrl Pts',(2.03686430742724,1.75155833719122,-8.76648520934269));
#151374=CARTESIAN_POINT('Ctrl Pts',(2.019990139016,1.75781013686931,-8.77038829258981));
#151375=CARTESIAN_POINT('Ctrl Pts',(2.01141535660801,1.75940739648177,-8.77235934001887));
#151376=CARTESIAN_POINT('Ctrl Pts',(2.00268840579558,1.75940739648129,-8.77435120959333));
#151377=CARTESIAN_POINT('Ctrl Pts',(1.99311193031393,1.75940739648077,-8.77653697762989));
#151378=CARTESIAN_POINT('Ctrl Pts',(1.98362593784728,1.75748289725883,-8.77868526185969));
#151379=CARTESIAN_POINT('Ctrl Pts',(1.96456523947057,1.74964163163066,-8.78297147222287));
#151380=CARTESIAN_POINT('Ctrl Pts',(1.95541475487494,1.74349822308499,-8.7850112050058));
#151381=CARTESIAN_POINT('Ctrl Pts',(1.93718688597779,1.72630637223326,-8.78905084189892));
#151382=CARTESIAN_POINT('Ctrl Pts',(1.92885816375222,1.71456563967815,-8.7908787867595));
#151383=CARTESIAN_POINT('Ctrl Pts',(1.92088938462464,1.69868853704811,-8.79262113211972));
#151384=CARTESIAN_POINT('Ctrl Pts',(1.91947682532086,1.69560796596479,-8.79292957559287));
#151385=CARTESIAN_POINT('Ctrl Pts',(1.91816445274598,1.69247211214181,-8.79321585838888));
#151386=CARTESIAN_POINT('Ctrl Pts',(1.66311917827957,0.999999999892245,
-8.84500054261381));
#151387=CARTESIAN_POINT('Ctrl Pts',(1.67572518383153,1.04120750292225,-8.8426302443313));
#151388=CARTESIAN_POINT('Ctrl Pts',(1.6888484293412,1.0822780170862,-8.84013474140826));
#151389=CARTESIAN_POINT('Ctrl Pts',(1.76593893483276,1.31475831833986,-8.82528429724149));
#151390=CARTESIAN_POINT('Ctrl Pts',(1.83922779333879,1.50385659883379,-8.81043521210152));
#151391=CARTESIAN_POINT('Ctrl Pts',(1.91816445327559,1.6924721119096,-8.79321585827335));
#151392=CARTESIAN_POINT('',(1.293862227,1.69247211199998,-8.906510009));
#151393=CARTESIAN_POINT('Ctrl Pts',(1.29386222704835,1.69247211203084,-8.9065100088316));
#151394=CARTESIAN_POINT('Ctrl Pts',(1.37381592810969,1.50385659888228,-8.8948950133268));
#151395=CARTESIAN_POINT('Ctrl Pts',(1.44764910778165,1.31475831831576,-8.88304538485746));
#151396=CARTESIAN_POINT('Ctrl Pts',(1.52504199941119,1.08227801709192,-8.86986122572233));
#151397=CARTESIAN_POINT('Ctrl Pts',(1.53820529634083,1.04120750303301,-8.86758642450121));
#151398=CARTESIAN_POINT('Ctrl Pts',(1.55084034142984,1.0000000001088,-8.86537614742848));
#151399=CARTESIAN_POINT('',(1.12222469370069,1.69247211186443,-8.92975989245308));
#151400=CARTESIAN_POINT('Ctrl Pts',(1.29386222678592,1.69247211191724,-8.90651000886972));
#151401=CARTESIAN_POINT('Ctrl Pts',(1.29175663284455,1.6974393326443,-8.90681589169734));
#151402=CARTESIAN_POINT('Ctrl Pts',(1.28940745324757,1.70224131096108,-8.90715640715206));
#151403=CARTESIAN_POINT('Ctrl Pts',(1.27905805625247,1.72064855707061,-8.90865152375759));
#151404=CARTESIAN_POINT('Ctrl Pts',(1.26935895263178,1.73230722845891,-8.91004243270966));
#151405=CARTESIAN_POINT('Ctrl Pts',(1.25090744812925,1.74686546574982,-8.91264741554434));
#151406=CARTESIAN_POINT('Ctrl Pts',(1.24284281427571,1.75155833681844,-8.91377702612638));
#151407=CARTESIAN_POINT('Ctrl Pts',(1.22568670661819,1.75781013649756,-8.91615180791229));
#151408=CARTESIAN_POINT('Ctrl Pts',(1.21696976043267,1.75940739610974,-8.9173462829144));
#151409=CARTESIAN_POINT('Ctrl Pts',(1.20809939194526,1.75940739610823,-8.91854785596744));
#151410=CARTESIAN_POINT('Ctrl Pts',(1.19836553780406,1.75940739610657,-8.91986639609967));
#151411=CARTESIAN_POINT('Ctrl Pts',(1.18872516244252,1.75748289688384,-8.92115571415885));
#151412=CARTESIAN_POINT('Ctrl Pts',(1.16935698390139,1.74964163125454,-8.92371608166787));
#151413=CARTESIAN_POINT('Ctrl Pts',(1.1600604962301,1.74349822270799,-8.9249273599703));
#151414=CARTESIAN_POINT('Ctrl Pts',(1.14154389711402,1.72630637185311,-8.92731680090106));
#151415=CARTESIAN_POINT('Ctrl Pts',(1.13308484816045,1.71456563929485,-8.92839080608824));
#151416=CARTESIAN_POINT('Ctrl Pts',(1.12499196639287,1.6986885367259,-8.92941182141989));
#151417=CARTESIAN_POINT('Ctrl Pts',(1.12355744500622,1.69560796570946,-8.92959240234685));
#151418=CARTESIAN_POINT('Ctrl Pts',(1.12222469348958,1.69247211195553,-8.92975989247875));
#151419=CARTESIAN_POINT('Ctrl Pts',(0.863564213439779,0.999999999851495,
-8.95847402459069));
#151420=CARTESIAN_POINT('Ctrl Pts',(0.87633194283773,1.04120750294903,-8.95724326205628));
#151421=CARTESIAN_POINT('Ctrl Pts',(0.889626053196569,1.08227801718005,
-8.95593416395052));
#151422=CARTESIAN_POINT('Ctrl Pts',(0.967737398493407,1.31475831834262,
-8.94805384294514));
#151423=CARTESIAN_POINT('Ctrl Pts',(1.04206227925682,1.50385659868299,-8.93983409849226));
#151424=CARTESIAN_POINT('Ctrl Pts',(1.12222469430304,1.69247211160434,-8.92975989237653));
#151425=CARTESIAN_POINT('',(0.490280117,1.69247211199998,-8.986635934));
#151426=CARTESIAN_POINT('Ctrl Pts',(0.490280116634964,1.69247211184778,
-8.98663593383155));
#151427=CARTESIAN_POINT('Ctrl Pts',(0.570953107639295,1.50385659894552,
-8.98223469139443));
#151428=CARTESIAN_POINT('Ctrl Pts',(0.645551249023958,1.31475831862389,
-8.97705112125193));
#151429=CARTESIAN_POINT('Ctrl Pts',(0.723814398508999,1.08227801747435,
-8.97085748298641));
#151430=CARTESIAN_POINT('Ctrl Pts',(0.737128615539833,1.04120750323641,
-8.96977178828106));
#151431=CARTESIAN_POINT('Ctrl Pts',(0.74991092341197,1.00000000013195,-8.9687030058391));
#151432=CARTESIAN_POINT('',(0.317249443000001,1.69247211199998,-8.99440675));
#151433=CARTESIAN_POINT('Ctrl Pts',(0.490280117042473,1.6924721120226,-8.98663593380931));
#151434=CARTESIAN_POINT('Ctrl Pts',(0.488155580485674,1.69743933273218,
-8.98675184125671));
#151435=CARTESIAN_POINT('Ctrl Pts',(0.485785334434538,1.70224131103288,
-8.98688040706054));
#151436=CARTESIAN_POINT('Ctrl Pts',(0.475343579859998,1.72064855714611,
-8.98744179197277));
#151437=CARTESIAN_POINT('Ctrl Pts',(0.465558841857586,1.73230722855128,
-8.98795768059026));
#151438=CARTESIAN_POINT('Ctrl Pts',(0.446948108818821,1.74686546586344,
-8.98889819642084));
#151439=CARTESIAN_POINT('Ctrl Pts',(0.438814683296199,1.75155833693934,
-8.98930035131872));
#151440=CARTESIAN_POINT('Ctrl Pts',(0.421514767281569,1.75781013663147,
-8.99012771129987));
#151441=CARTESIAN_POINT('Ctrl Pts',(0.41272584104224,1.75940739624973,-8.99053599666621));
#151442=CARTESIAN_POINT('Ctrl Pts',(0.403783473868803,1.7594073962532,-8.99093759883976));
#151443=CARTESIAN_POINT('Ctrl Pts',(0.393970612336502,1.75940739625701,
-8.9913782949601));
#151444=CARTESIAN_POINT('Ctrl Pts',(0.384253472711401,1.75748289703986,
-8.99179826602011));
#151445=CARTESIAN_POINT('Ctrl Pts',(0.364733755191164,1.74964163142237,
-8.99261217610549));
#151446=CARTESIAN_POINT('Ctrl Pts',(0.355366114298915,1.74349822288405,
-8.99298524742859));
#151447=CARTESIAN_POINT('Ctrl Pts',(0.336709869740617,1.7263063720505,-8.99370525402671));
#151448=CARTESIAN_POINT('Ctrl Pts',(0.328188601351915,1.71456563950727,
-8.99401667228355));
#151449=CARTESIAN_POINT('Ctrl Pts',(0.320036776042563,1.69868853696225,
-8.99430813697986));
#151450=CARTESIAN_POINT('Ctrl Pts',(0.318591842470323,1.69560796595495,
-8.99435940143549));
#151451=CARTESIAN_POINT('Ctrl Pts',(0.317249442521872,1.69247211221038,
-8.99440675037657));
#151452=CARTESIAN_POINT('Ctrl Pts',(0.0570563382849732,0.999999999911668,
-8.99981914119731));
#151453=CARTESIAN_POINT('Ctrl Pts',(0.069882993212187,1.04120750284218,
-8.99973782378958));
#151454=CARTESIAN_POINT('Ctrl Pts',(0.0832409319874684,1.08227801690732,
-8.99962567059221));
#151455=CARTESIAN_POINT('Ctrl Pts',(0.161744210525078,1.31475831815755,
-8.99877892044582));
#151456=CARTESIAN_POINT('Ctrl Pts',(0.236506693492214,1.50385659874335,
-8.99725469720449));
#151457=CARTESIAN_POINT('Ctrl Pts',(0.317249443220438,1.69247211191093,
-8.99440675035193));
#151458=CARTESIAN_POINT('',(-0.317249441999998,1.69247211199998,-8.99440675));
#151459=CARTESIAN_POINT('Ctrl Pts',(-0.3172494417691,1.69247211210491,-8.99440675040312));
#151460=CARTESIAN_POINT('Ctrl Pts',(-0.236506691980428,1.50385659883905,
-8.99725469724477));
#151461=CARTESIAN_POINT('Ctrl Pts',(-0.161744208956718,1.3147583181561,
-8.99877892047434));
#151462=CARTESIAN_POINT('Ctrl Pts',(-0.0832409304009231,1.08227801689511,
-8.99962567060685));
#151463=CARTESIAN_POINT('Ctrl Pts',(-0.0698829916511323,1.0412075029195,
-8.99973782380167));
#151464=CARTESIAN_POINT('Ctrl Pts',(-0.0570563367470325,1.00000000007913,
-8.99981914120706));
#151465=CARTESIAN_POINT('',(-0.490280117,1.69247211199998,-8.986635934));
#151466=CARTESIAN_POINT('Ctrl Pts',(-0.317249442367008,1.69247211184862,
-8.99440675038203));
#151467=CARTESIAN_POINT('Ctrl Pts',(-0.319375816065643,1.69743933266917,
-8.99433174922977));
#151468=CARTESIAN_POINT('Ctrl Pts',(-0.32174804480143,1.70224131107396,
-8.99424733024544));
#151469=CARTESIAN_POINT('Ctrl Pts',(-0.332198086155421,1.72064855725429,
-8.99387046351945));
#151470=CARTESIAN_POINT('Ctrl Pts',(-0.341989677572707,1.7323072286332,
-8.9935071781673));
#151471=CARTESIAN_POINT('Ctrl Pts',(-0.360609796449266,1.74686546591158,
-8.99277565450731));
#151472=CARTESIAN_POINT('Ctrl Pts',(-0.368746528075211,1.75155833697566,
-8.99244711580377));
#151473=CARTESIAN_POINT('Ctrl Pts',(-0.386050963682256,1.75781013664746,
-8.99172039255882));
#151474=CARTESIAN_POINT('Ctrl Pts',(-0.394841106701602,1.75940739625667,
-8.99133920101302));
#151475=CARTESIAN_POINT('Ctrl Pts',(-0.4037834738688,1.7594073962532,-8.99093759883976));
#151476=CARTESIAN_POINT('Ctrl Pts',(-0.413596335402218,1.75940739624939,
-8.99049690271936));
#151477=CARTESIAN_POINT('Ctrl Pts',(-0.423312002595473,1.75748289702424,
-8.99004414541729));
#151478=CARTESIAN_POINT('Ctrl Pts',(-0.442826097813949,1.74964163138952,
-8.98910504494811));
#151479=CARTESIAN_POINT('Ctrl Pts',(-0.452189469197941,1.74349822283924,
-8.98863690553838));
#151480=CARTESIAN_POINT('Ctrl Pts',(-0.47083515010459,1.72630637197522,
-8.98768168072916));
#151481=CARTESIAN_POINT('Ctrl Pts',(-0.479350029693784,1.71456563941106,
-8.98722800469669));
#151482=CARTESIAN_POINT('Ctrl Pts',(-0.487495164855626,1.69868853682224,
-8.98678757205289));
#151483=CARTESIAN_POINT('Ctrl Pts',(-0.488938876868527,1.69560796579138,
-8.98670910728539));
#151484=CARTESIAN_POINT('Ctrl Pts',(-0.490280117042473,1.6924721120226,
-8.98663593380931));
#151485=CARTESIAN_POINT('Ctrl Pts',(-0.749910923055967,1.00000000002074,
-8.96870300586887));
#151486=CARTESIAN_POINT('Ctrl Pts',(-0.73712861517006,1.04120750317642,
-8.96977178831146));
#151487=CARTESIAN_POINT('Ctrl Pts',(-0.723814398124092,1.08227801746521,
-8.97085748301749));
#151488=CARTESIAN_POINT('Ctrl Pts',(-0.645551248646323,1.31475831860558,
-8.97705112127892));
#151489=CARTESIAN_POINT('Ctrl Pts',(-0.570953107291633,1.503856598869,-8.98223469141623));
#151490=CARTESIAN_POINT('Ctrl Pts',(-0.490280116319863,1.69247211171261,
-8.98663593384873));
#151491=CARTESIAN_POINT('',(-1.122224693,1.69247211199998,-8.929759892));
#151492=CARTESIAN_POINT('Ctrl Pts',(-1.12222469326036,1.69247211191644,
-8.92975989250756));
#151493=CARTESIAN_POINT('Ctrl Pts',(-1.04206227819181,1.50385659894457,
-8.9398340986166));
#151494=CARTESIAN_POINT('Ctrl Pts',(-0.967737397408281,1.31475831855362,
-8.9480538430626));
#151495=CARTESIAN_POINT('Ctrl Pts',(-0.889626052114516,1.08227801739532,
-8.95593416405797));
#151496=CARTESIAN_POINT('Ctrl Pts',(-0.876331941773366,1.04120750322035,
-8.95724326216039));
#151497=CARTESIAN_POINT('Ctrl Pts',(-0.863564212391512,1.00000000017931,
-8.95847402469174));
#151498=CARTESIAN_POINT('',(-1.293862227,1.69247211199998,-8.906510009));
#151499=CARTESIAN_POINT('Ctrl Pts',(-1.12222469343999,1.69247211183886,
-8.92975989248499));
#151500=CARTESIAN_POINT('Ctrl Pts',(-1.12433578390216,1.69743933257241,
-8.92949458660048));
#151501=CARTESIAN_POINT('Ctrl Pts',(-1.12669089544509,1.70224131089559,
-8.92919786252279));
#151502=CARTESIAN_POINT('Ctrl Pts',(-1.13706508588636,1.72064855702356,
-8.9278857784736));
#151503=CARTESIAN_POINT('Ctrl Pts',(-1.1467846945914,1.73230722842328,-8.92664624411453));
#151504=CARTESIAN_POINT('Ctrl Pts',(-1.16526428107703,1.74686546572887,
-8.92424857076721));
#151505=CARTESIAN_POINT('Ctrl Pts',(-1.17333880663464,1.75155833680263,
-8.92319198366484));
#151506=CARTESIAN_POINT('Ctrl Pts',(-1.19050843670974,1.7578101364906,-8.92091702834642));
#151507=CARTESIAN_POINT('Ctrl Pts',(-1.19922902345514,1.75940739610672,
-8.91974942902085));
#151508=CARTESIAN_POINT('Ctrl Pts',(-1.20809939194526,1.75940739610823,
-8.91854785596744));
#151509=CARTESIAN_POINT('Ctrl Pts',(-1.21783324608597,1.75940739610989,
-8.91722931583528));
#151510=CARTESIAN_POINT('Ctrl Pts',(-1.22746921600719,1.75748289689063,
-8.91590747550959));
#151511=CARTESIAN_POINT('Ctrl Pts',(-1.24682057289392,1.74964163126884,
-8.91322292557665));
#151512=CARTESIAN_POINT('Ctrl Pts',(-1.25610428640085,1.74349822272748,
-8.91191734462038));
#151513=CARTESIAN_POINT('Ctrl Pts',(-1.27458927957878,1.72630637188588,
-8.90929457931835));
#151514=CARTESIAN_POINT('Ctrl Pts',(-1.28302921355709,1.71456563933674,
-8.90807946173197));
#151515=CARTESIAN_POINT('Ctrl Pts',(-1.29110207873021,1.69868853674836,
-8.90691067785349));
#151516=CARTESIAN_POINT('Ctrl Pts',(-1.29253294526348,1.69560796570205,
-8.906703115614));
#151517=CARTESIAN_POINT('Ctrl Pts',(-1.29386222678592,1.69247211191724,
-8.90651000886972));
#151518=CARTESIAN_POINT('Ctrl Pts',(-1.5508403410948,1.00000000000292,-8.86537614748708));
#151519=CARTESIAN_POINT('Ctrl Pts',(-1.53820529599185,1.04120750297962,
-8.86758642456176));
#151520=CARTESIAN_POINT('Ctrl Pts',(-1.52504199904687,1.08227801709064,
-8.869861225785));
#151521=CARTESIAN_POINT('Ctrl Pts',(-1.44764910742439,1.31475831830606,
-8.88304538491551));
#151522=CARTESIAN_POINT('Ctrl Pts',(-1.37381592778245,1.50385659881392,
-8.89489501337705));
#151523=CARTESIAN_POINT('Ctrl Pts',(-1.29386222675377,1.69247211190334,
-8.90651000887439));
#151524=CARTESIAN_POINT('',(-1.918164453,1.69247211199998,-8.793215858));
#151525=CARTESIAN_POINT('Ctrl Pts',(-1.91816445274452,1.69247211214243,
-8.7932158583892));
#151526=CARTESIAN_POINT('Ctrl Pts',(-1.8392277928231,1.50385659907754,-8.81043521220902));
#151527=CARTESIAN_POINT('Ctrl Pts',(-1.76593893433233,1.31475831859373,
-8.82528429734153));
#151528=CARTESIAN_POINT('Ctrl Pts',(-1.68884842884387,1.08227801731721,
-8.84013474150328));
#151529=CARTESIAN_POINT('Ctrl Pts',(-1.67572518332552,1.04120750311924,
-8.84263024442721));
#151530=CARTESIAN_POINT('Ctrl Pts',(-1.66311917776566,1.00000000005502,
-8.84500054271044));
#151531=CARTESIAN_POINT('',(-2.08702692,1.69247211199998,-8.754674102));
#151532=CARTESIAN_POINT('Ctrl Pts',(-1.91816445274599,1.69247211214183,
-8.79321585838888));
#151533=CARTESIAN_POINT('Ctrl Pts',(-1.92024326275654,1.69743933291711,
-8.79276238385459));
#151534=CARTESIAN_POINT('Ctrl Pts',(-1.92256229518958,1.70224131127948,
-8.7922557437256));
#151535=CARTESIAN_POINT('Ctrl Pts',(-1.93277710790523,1.72064855743359,
-8.79001900647378));
#151536=CARTESIAN_POINT('Ctrl Pts',(-1.94234647731931,1.73230722882437,
-8.78791320310792));
#151537=CARTESIAN_POINT('Ctrl Pts',(-1.96053674463813,1.74686546611736,
-8.78386868472646));
#151538=CARTESIAN_POINT('Ctrl Pts',(-1.96848405279003,1.75155833718626,
-8.7820925562423));
#151539=CARTESIAN_POINT('Ctrl Pts',(-1.9853806375546,1.75781013686712,-8.77828768545104));
#151540=CARTESIAN_POINT('Ctrl Pts',(-1.99396145498231,1.75940739648082,
-8.77634307916798));
#151541=CARTESIAN_POINT('Ctrl Pts',(-2.00268840579558,1.75940739648129,
-8.77435120959333));
#151542=CARTESIAN_POINT('Ctrl Pts',(-2.0122648812771,1.75940739648181,-8.7721654415568));
#151543=CARTESIAN_POINT('Ctrl Pts',(-2.02174357076493,1.75748289726095,
-8.76998516088618));
#151544=CARTESIAN_POINT('Ctrl Pts',(-2.04077638358099,1.74964163163514,
-8.76557677590213));
#151545=CARTESIAN_POINT('Ctrl Pts',(-2.04990569221385,1.74349822309111,
-8.76344426516706));
#151546=CARTESIAN_POINT('Ctrl Pts',(-2.06808116737671,1.72630637224354,
-8.75917507633169));
#151547=CARTESIAN_POINT('Ctrl Pts',(-2.07637820236166,1.71456563969127,
-8.75720830060181));
#151548=CARTESIAN_POINT('Ctrl Pts',(-2.08431379958806,1.69868853706913,
-8.75532057584465));
#151549=CARTESIAN_POINT('Ctrl Pts',(-2.08572030015037,1.69560796599098,
-8.7549855872994));
#151550=CARTESIAN_POINT('Ctrl Pts',(-2.08702692043181,1.69247211217333,
-8.75467410206644));
#151551=CARTESIAN_POINT('Ctrl Pts',(-2.33928330456152,0.99999999985376,
-8.69067049317829));
#151552=CARTESIAN_POINT('Ctrl Pts',(-2.32689725212172,1.04120750291753,
-8.69400446904408));
#151553=CARTESIAN_POINT('Ctrl Pts',(-2.31399085832435,1.08227801711502,
-8.6974500614337));
#151554=CARTESIAN_POINT('Ctrl Pts',(-2.23809134664659,1.31475831833215,
-8.71751859033044));
#151555=CARTESIAN_POINT('Ctrl Pts',(-2.1656175902253,1.50385659875801,-8.73593887085572));
#151556=CARTESIAN_POINT('Ctrl Pts',(-2.08702691950424,1.69247211176485,
-8.75467410228756));
#151557=CARTESIAN_POINT('',(-2.698660279,1.69247211199998,-8.585874021));
#151558=CARTESIAN_POINT('Ctrl Pts',(-2.69866027953189,1.69247211171677,
-8.58587402048719));
#151559=CARTESIAN_POINT('Ctrl Pts',(-2.62158492637212,1.50385659866213,
-8.61009988189709));
#151560=CARTESIAN_POINT('Ctrl Pts',(-2.54992216900827,1.3147583181889,-8.63145875160704));
#151561=CARTESIAN_POINT('Ctrl Pts',(-2.47447319081348,1.0822780170125,-8.65315975187598));
#151562=CARTESIAN_POINT('Ctrl Pts',(-2.46162647080814,1.04120750290523,
-8.65682156729051));
#151563=CARTESIAN_POINT('Ctrl Pts',(-2.44928368524565,0.999999999932309,
-8.66031231706972));
#151564=CARTESIAN_POINT('',(-2.8633881,1.69247211199998,-8.532350707));
#151565=CARTESIAN_POINT('Ctrl Pts',(-2.69866027920764,1.69247211186232,
-8.5858740205891));
#151566=CARTESIAN_POINT('Ctrl Pts',(-2.70069007140367,1.69743933265977,
-8.58523602851499));
#151567=CARTESIAN_POINT('Ctrl Pts',(-2.70295435323217,1.70224131104289,
-8.58452355150266));
#151568=CARTESIAN_POINT('Ctrl Pts',(-2.71292754454375,1.72064855720862,
-8.5813801699417));
#151569=CARTESIAN_POINT('Ctrl Pts',(-2.72226962772906,1.73230722859247,
-8.57842505226088));
#151570=CARTESIAN_POINT('Ctrl Pts',(-2.74002411854314,1.74686546587731,
-8.57276625293122));
#151571=CARTESIAN_POINT('Ctrl Pts',(-2.74778022223851,1.75155833694367,
-8.5702848834079));
#151572=CARTESIAN_POINT('Ctrl Pts',(-2.76426772033127,1.7578101366193,-8.56498073172688));
#151573=CARTESIAN_POINT('Ctrl Pts',(-2.77263968074679,1.75940739623016,
-8.56227477531311));
#151574=CARTESIAN_POINT('Ctrl Pts',(-2.78115294960864,1.7594073962279,-8.55950864658031));
#151575=CARTESIAN_POINT('Ctrl Pts',(-2.79049494227812,1.75940739622543,
-8.55647324915965));
#151576=CARTESIAN_POINT('Ctrl Pts',(-2.79974003449488,1.7574828970017,-8.5534520824834));
#151577=CARTESIAN_POINT('Ctrl Pts',(-2.81830106221837,1.74964163137009,
-8.54735535617395));
#151578=CARTESIAN_POINT('Ctrl Pts',(-2.82720246215093,1.74349822282197,
-8.54441308538321));
#151579=CARTESIAN_POINT('Ctrl Pts',(-2.8449220810608,1.72630637196336,-8.53853184601318));
#151580=CARTESIAN_POINT('Ctrl Pts',(-2.8530094142069,1.71456563940285,-8.53582924746147));
#151581=CARTESIAN_POINT('Ctrl Pts',(-2.86074385070298,1.69868853678566,
-8.53323778068014));
#151582=CARTESIAN_POINT('Ctrl Pts',(-2.86211466095963,1.69560796572133,
-8.53277806296399));
#151583=CARTESIAN_POINT('Ctrl Pts',(-2.86338809984565,1.69247211191798,
-8.53235070714175));
#151584=CARTESIAN_POINT('Ctrl Pts',(-3.10889173543709,1.00000000015543,
-8.44599266974172));
#151585=CARTESIAN_POINT('Ctrl Pts',(-3.09685440089955,1.04120750319919,
-8.45042350118141));
#151586=CARTESIAN_POINT('Ctrl Pts',(-3.08430882497445,1.08227801737684,
-8.45501214284914));
#151587=CARTESIAN_POINT('Ctrl Pts',(-3.01051379149162,1.31475831853189,
-8.4818034615245));
#151588=CARTESIAN_POINT('Ctrl Pts',(-2.93998297433824,1.50385659891702,
-8.5066460848574));
#151589=CARTESIAN_POINT('Ctrl Pts',(-2.86338809976883,1.69247211188328,
-8.53235070716753));
#151590=CARTESIAN_POINT('',(-3.45742808,1.69247211199998,-8.309403774));
#151591=CARTESIAN_POINT('Ctrl Pts',(-3.45742807951293,1.69247211214934,
-8.30940377373705));
#151592=CARTESIAN_POINT('Ctrl Pts',(-3.38283459860251,1.50385659921542,
-8.34044109030884));
#151593=CARTESIAN_POINT('Ctrl Pts',(-3.31337492880746,1.31475831886194,
-8.36813777550526));
#151594=CARTESIAN_POINT('Ctrl Pts',(-3.24017494866242,1.08227801761983,
-8.39651460819328));
#151595=CARTESIAN_POINT('Ctrl Pts',(-3.22770818832162,1.04120750332116,
-8.40131325333917));
#151596=CARTESIAN_POINT('Ctrl Pts',(-3.21572799953086,1.00000000015557,
-8.4058963491726));
#151597=CARTESIAN_POINT('',(-3.616694961,1.69247211199998,-8.241329842));
#151598=CARTESIAN_POINT('Ctrl Pts',(-3.45742807947874,1.69247211216523,
-8.30940377375127));
#151599=CARTESIAN_POINT('Ctrl Pts',(-3.45939251105716,1.69743933261943,
-8.30858640091872));
#151600=CARTESIAN_POINT('Ctrl Pts',(-3.46158381147326,1.70224131067939,
-8.30767382352641));
#151601=CARTESIAN_POINT('Ctrl Pts',(-3.47123508293639,1.72064855658343,
-8.30364910638717));
#151602=CARTESIAN_POINT('Ctrl Pts',(-3.48027466293968,1.73230722799974,
-8.29986846725979));
#151603=CARTESIAN_POINT('Ctrl Pts',(-3.49745042854421,1.74686546532774,
-8.29264094830292));
#151604=CARTESIAN_POINT('Ctrl Pts',(-3.50495288020258,1.75155833640983,
-8.28947431626728));
#151605=CARTESIAN_POINT('Ctrl Pts',(-3.52089854399714,1.75781013611086,
-8.28271358960317));
#151606=CARTESIAN_POINT('Ctrl Pts',(-3.52899424130546,1.75940739573205,
-8.27926806982646));
#151607=CARTESIAN_POINT('Ctrl Pts',(-3.53722528439024,1.75940739573664,
-8.27574995317466));
#151608=CARTESIAN_POINT('Ctrl Pts',(-3.54625757801348,1.75940739574168,
-8.27188936560725));
#151609=CARTESIAN_POINT('Ctrl Pts',(-3.5551946369119,1.75748289652637,-8.26805163758463));
#151610=CARTESIAN_POINT('Ctrl Pts',(-3.57313443705391,1.74964163091365,
-8.26031565721045));
#151611=CARTESIAN_POINT('Ctrl Pts',(-3.58173625944174,1.74349822237848,
-8.25658731580187));
#151612=CARTESIAN_POINT('Ctrl Pts',(-3.598857354133,1.72630637155178,-8.24914137818544));
#151613=CARTESIAN_POINT('Ctrl Pts',(-3.60666987098363,1.71456563901188,
-8.24572471654922));
#151614=CARTESIAN_POINT('Ctrl Pts',(-3.61414087354956,1.6986885365718,-8.24245037274111));
#151615=CARTESIAN_POINT('Ctrl Pts',(-3.61546495648722,1.69560796567022,
-8.24186962725644));
#151616=CARTESIAN_POINT('Ctrl Pts',(-3.61669496095015,1.69247211203475,
-8.2413298416844));
#151617=CARTESIAN_POINT('Ctrl Pts',(-3.85346919584841,0.999999999908194,
-8.13331268036876));
#151618=CARTESIAN_POINT('Ctrl Pts',(-3.84187749678661,1.04120750281033,
-8.13880469291244));
#151619=CARTESIAN_POINT('Ctrl Pts',(-3.82979374837063,1.08227801684729,
-8.14449943879189));
#151620=CARTESIAN_POINT('Ctrl Pts',(-3.75869734727944,1.31475831804488,
-8.17779783928727));
#151621=CARTESIAN_POINT('Ctrl Pts',(-3.69067734197139,1.50385659860643,
-8.20886278724963));
#151622=CARTESIAN_POINT('Ctrl Pts',(-3.61669496034055,1.6924721117496,-8.24132984195192));
#151623=CARTESIAN_POINT('',(-4.188358703,1.69247211199998,-7.966031093));
#151624=CARTESIAN_POINT('Ctrl Pts',(-4.18835870309451,1.69247211195876,
-7.96603109297299));
#151625=CARTESIAN_POINT('Ctrl Pts',(-4.11684767709351,1.50385659876227,
-8.00362997058504));
#151626=CARTESIAN_POINT('Ctrl Pts',(-4.05015034311738,1.31475831814771,
-8.03744147392975));
#151627=CARTESIAN_POINT('Ctrl Pts',(-3.97978872423843,1.08227801688172,
-8.07226566547243));
#151628=CARTESIAN_POINT('Ctrl Pts',(-3.96780229871458,1.04120750283049,
-8.07816250443158));
#151629=CARTESIAN_POINT('Ctrl Pts',(-3.95628116424985,0.999999999913972,
-8.08380104588193));
#151630=CARTESIAN_POINT('',(-4.340882323,1.69247211199998,-7.883954633));
#151631=CARTESIAN_POINT('Ctrl Pts',(-4.18835870300193,1.69247211200357,
-7.96603109302167));
#151632=CARTESIAN_POINT('Ctrl Pts',(-4.19024195767692,1.69743933264773,
-7.96504092037284));
#151633=CARTESIAN_POINT('Ctrl Pts',(-4.19234263382752,1.70224131088609,
-7.96393559005548));
#151634=CARTESIAN_POINT('Ctrl Pts',(-4.2015942793333,1.72064855691523,-7.95906194189281));
#151635=CARTESIAN_POINT('Ctrl Pts',(-4.21025857475973,1.73230722829565,
-7.95448622080491));
#151636=CARTESIAN_POINT('Ctrl Pts',(-4.2267173259628,1.74686546557695,-7.94574817396073));
#151637=CARTESIAN_POINT('Ctrl Pts',(-4.23390572024391,1.75155833664249,
-7.94192177527461));
#151638=CARTESIAN_POINT('Ctrl Pts',(-4.24918116460585,1.75781013631568,
-7.93375890702995));
#151639=CARTESIAN_POINT('Ctrl Pts',(-4.25693541699852,1.75940739592486,
-7.92960156519345));
#151640=CARTESIAN_POINT('Ctrl Pts',(-4.26481796277002,1.75940739592062,
-7.92535978643457));
#151641=CARTESIAN_POINT('Ctrl Pts',(-4.27346783463465,1.75940739591597,
-7.92070509189728));
#151642=CARTESIAN_POINT('Ctrl Pts',(-4.28202490427399,1.75748289669032,
-7.91608170165457));
#151643=CARTESIAN_POINT('Ctrl Pts',(-4.29919903612613,1.74964163105498,
-7.90676875277056));
#151644=CARTESIAN_POINT('Ctrl Pts',(-4.30743202416365,1.7434982225042,-7.90228435915018));
#151645=CARTESIAN_POINT('Ctrl Pts',(-4.32381674566996,1.72630637163808,
-7.89333367358511));
#151646=CARTESIAN_POINT('Ctrl Pts',(-4.3312915444412,1.71456563907159,-7.88923045780918));
#151647=CARTESIAN_POINT('Ctrl Pts',(-4.33843896105432,1.69868853654903,
-7.88529960002584));
#151648=CARTESIAN_POINT('Ctrl Pts',(-4.3397056560187,1.69560796558959,-7.88460250256148));
#151649=CARTESIAN_POINT('Ctrl Pts',(-4.34088232285577,1.69247211189454,
-7.88395463324836));
#151650=CARTESIAN_POINT('Ctrl Pts',(-4.56702079088811,0.999999999926176,
-7.75514803827726));
#151651=CARTESIAN_POINT('Ctrl Pts',(-4.55596805673791,1.04120750310877,
-7.7616570135297));
#151652=CARTESIAN_POINT('Ctrl Pts',(-4.54444342694939,1.08227801742429,
-7.76841201294057));
#151653=CARTESIAN_POINT('Ctrl Pts',(-4.47661808467103,1.31475831862242,
-7.80794939613996));
#151654=CARTESIAN_POINT('Ctrl Pts',(-4.41165654848376,1.50385659891625,
-7.84498655197261));
#151655=CARTESIAN_POINT('Ctrl Pts',(-4.34088232264358,1.69247211179079,
-7.88395463336519));
#151656=CARTESIAN_POINT('',(-4.885567124,1.69247211199998,-7.558520614));
#151657=CARTESIAN_POINT('Ctrl Pts',(-4.88556712448748,1.69247211182252,
-7.55852061399101));
#151658=CARTESIAN_POINT('Ctrl Pts',(-4.81771431823801,1.50385659859261,
-7.60237832854206));
#151659=CARTESIAN_POINT('Ctrl Pts',(-4.75431632789337,1.31475831794536,
-7.64203241965308));
#151660=CARTESIAN_POINT('Ctrl Pts',(-4.6873595806634,1.08227801668198,-7.68302358613477));
#151661=CARTESIAN_POINT('Ctrl Pts',(-4.67594999754258,1.0412075026676,-7.68997114104925));
#151662=CARTESIAN_POINT('Ctrl Pts',(-4.66498067874495,0.999999999788168,
-7.69661972991626));
#151663=CARTESIAN_POINT('',(-5.030119452,1.69247211199998,-7.463102458));
#151664=CARTESIAN_POINT('Ctrl Pts',(-4.88556712453282,1.69247211179936,
-7.55852061396171));
#151665=CARTESIAN_POINT('Ctrl Pts',(-4.8873540394334,1.69743933262183,-7.55736561377867));
#151666=CARTESIAN_POINT('Ctrl Pts',(-4.88934717789494,1.7022413110283,-7.55607642999801));
#151667=CARTESIAN_POINT('Ctrl Pts',(-4.89812470861776,1.72064855720425,
-7.55039309055105));
#151668=CARTESIAN_POINT('Ctrl Pts',(-4.90634395966117,1.7323072285775,-7.54505912851645));
#151669=CARTESIAN_POINT('Ctrl Pts',(-4.92195318028781,1.74686546584881,
-7.53488090739656));
#151670=CARTESIAN_POINT('Ctrl Pts',(-4.92876964047148,1.75155833691055,
-7.53042554997138));
#151671=CARTESIAN_POINT('Ctrl Pts',(-4.94325187651329,1.75781013657807,
-7.52092626275953));
#151672=CARTESIAN_POINT('Ctrl Pts',(-4.95060225131441,1.75940739618522,
-7.51609057133398));
#151673=CARTESIAN_POINT('Ctrl Pts',(-4.95807283415526,1.75940739618001,
-7.51115928277463));
#151674=CARTESIAN_POINT('Ctrl Pts',(-4.96627064057824,1.75940739617429,
-7.50574795813149));
#151675=CARTESIAN_POINT('Ctrl Pts',(-4.97437882446556,1.75748289694722,
-7.5003761304885));
#151676=CARTESIAN_POINT('Ctrl Pts',(-4.99064901201181,1.74964163130847,
-7.48956119548551));
#151677=CARTESIAN_POINT('Ctrl Pts',(-4.99844687851583,1.74349822275537,
-7.48435685535607));
#151678=CARTESIAN_POINT('Ctrl Pts',(-5.01396330668297,1.726306371884,-7.47397348750484));
#151679=CARTESIAN_POINT('Ctrl Pts',(-5.02104020468543,1.71456563931459,
-7.46921675427245));
#151680=CARTESIAN_POINT('Ctrl Pts',(-5.02780648852956,1.69868853677723,
-7.46466103147771));
#151681=CARTESIAN_POINT('Ctrl Pts',(-5.02900559682142,1.6956079658055,-7.4638531946588));
#151682=CARTESIAN_POINT('Ctrl Pts',(-5.03011945218954,1.69247211209781,
-7.46310245787262));
#151683=CARTESIAN_POINT('Ctrl Pts',(-5.24380141833698,1.00000000010371,
-7.31454350489811));
#151684=CARTESIAN_POINT('Ctrl Pts',(-5.23337663930275,1.04120750322152,
-7.32201703636988));
#151685=CARTESIAN_POINT('Ctrl Pts',(-5.2225039177803,1.08227801747272,-7.32977790197709));
#151686=CARTESIAN_POINT('Ctrl Pts',(-5.15849572412172,1.31475831856601,
-7.37523593608384));
#151687=CARTESIAN_POINT('Ctrl Pts',(-5.09711568904592,1.50385659881995,
-7.41794709841542));
#151688=CARTESIAN_POINT('Ctrl Pts',(-5.03011945133157,1.69247211165461,
-7.46310245845089));
#151689=CARTESIAN_POINT('',(-5.54343983057961,1.69247211214186,-7.09015337246368));
#151690=CARTESIAN_POINT('Ctrl Pts',(-5.54343983074268,1.69247211204734,
-7.09015337231399));
#151691=CARTESIAN_POINT('Ctrl Pts',(-5.47979155526345,1.50385659906037,
-7.13991680716822));
#151692=CARTESIAN_POINT('Ctrl Pts',(-5.42020335200143,1.31475831865458,
-7.185094214528));
#151693=CARTESIAN_POINT('Ctrl Pts',(-5.35719057279498,1.08227801744158,
-7.23192231915544));
#151694=CARTESIAN_POINT('Ctrl Pts',(-5.34644969527096,1.0412075032267,-7.23986465243842));
#151695=CARTESIAN_POINT('Ctrl Pts',(-5.33612051058942,1.00000000014546,
-7.24746975823059));
#151696=CARTESIAN_POINT('',(-5.678857015,1.69247211099998,-6.982161771));
#151697=CARTESIAN_POINT('Ctrl Pts',(-5.54343983023425,1.69247211232382,
-7.09015337271151));
#151698=CARTESIAN_POINT('Ctrl Pts',(-5.54511601804185,1.69743933283043,
-7.08884284446661));
#151699=CARTESIAN_POINT('Ctrl Pts',(-5.54698557106644,1.7022413109397,-7.08738018708892));
#151700=CARTESIAN_POINT('Ctrl Pts',(-5.55521831528555,1.72064855688249,
-7.08093291540944));
#151701=CARTESIAN_POINT('Ctrl Pts',(-5.56292634537752,1.73230722829277,
-7.07488365835213));
#151702=CARTESIAN_POINT('Ctrl Pts',(-5.57756035917907,1.74686546561218,
-7.06334721200287));
#151703=CARTESIAN_POINT('Ctrl Pts',(-5.58395000314327,1.75155833669096,
-7.05829876775499));
#151704=CARTESIAN_POINT('Ctrl Pts',(-5.59752242843277,1.7578101363872,-7.04753954424595));
#151705=CARTESIAN_POINT('Ctrl Pts',(-5.60440974475557,1.7594073960068,-7.04206443737231));
#151706=CARTESIAN_POINT('Ctrl Pts',(-5.61140821593638,1.75940739601077,
-7.03648334284404));
#151707=CARTESIAN_POINT('Ctrl Pts',(-5.61908795299921,1.75940739601513,
-7.03035895690423));
#151708=CARTESIAN_POINT('Ctrl Pts',(-5.62668196880536,1.75748289679882,
-7.02428194266244));
#151709=CARTESIAN_POINT('Ctrl Pts',(-5.64191721405734,1.74964163118351,
-7.01205209704977));
#151710=CARTESIAN_POINT('Ctrl Pts',(-5.64921717518735,1.74349822264663,
-7.00616971270524));
#151711=CARTESIAN_POINT('Ctrl Pts',(-5.66374038085022,1.72630637181619,
-6.99443726335543));
#151712=CARTESIAN_POINT('Ctrl Pts',(-5.67036239905914,1.71456563927445,
-6.9890653110919));
#151713=CARTESIAN_POINT('Ctrl Pts',(-5.67669307213168,1.69868853641841,
-6.98392140317848));
#151714=CARTESIAN_POINT('Ctrl Pts',(-5.67781493935397,1.69560796508514,
-6.98300933113573));
#151715=CARTESIAN_POINT('Ctrl Pts',(-5.67885701524478,1.69247211100408,
-6.98216177128582));
#151716=CARTESIAN_POINT('Ctrl Pts',(-5.87836203940153,1.00000000015303,
-6.81504656871272));
#151717=CARTESIAN_POINT('Ctrl Pts',(-5.86864914972266,1.04120750297626,
-6.82342448387522));
#151718=CARTESIAN_POINT('Ctrl Pts',(-5.85851587727959,1.08227801693488,
-6.83212872970076));
#151719=CARTESIAN_POINT('Ctrl Pts',(-5.79884018861093,1.3147583177969,-6.88314141331103));
#151720=CARTESIAN_POINT('Ctrl Pts',(-5.74153585055806,1.50385659810718,
-6.9311826969984));
#151721=CARTESIAN_POINT('Ctrl Pts',(-5.6788570152349,1.69247211099862,-6.98216177129385));
#151722=CARTESIAN_POINT('',(-6.15668002,1.69247211199998,-6.564700384));
#151723=CARTESIAN_POINT('Ctrl Pts',(-6.15668002040535,1.69247211175397,
-6.56470038359265));
#151724=CARTESIAN_POINT('Ctrl Pts',(-6.09774873405703,1.50385659870572,
-6.6199688729428));
#151725=CARTESIAN_POINT('Ctrl Pts',(-6.04245008693597,1.31475831823908,
-6.67030585472521));
#151726=CARTESIAN_POINT('Ctrl Pts',(-5.98388861759739,1.0822780170448,-6.7225938651483));
#151727=CARTESIAN_POINT('Ctrl Pts',(-5.97390292497523,1.04120750291261,
-6.73146702975377));
#151728=CARTESIAN_POINT('Ctrl Pts',(-5.96429703900053,0.999999999914591,
-6.73996742058665));
#151729=CARTESIAN_POINT('',(-6.281871763,1.69247211199998,-6.445004822));
#151730=CARTESIAN_POINT('Ctrl Pts',(-6.15668002018172,1.69247211188528,
-6.56470038380239));
#151731=CARTESIAN_POINT('Ctrl Pts',(-6.158231985384,1.69743933273647,-6.56324487896678));
#151732=CARTESIAN_POINT('Ctrl Pts',(-6.15996290064517,1.70224131117035,
-6.56162052427873));
#151733=CARTESIAN_POINT('Ctrl Pts',(-6.16758457340519,1.7206485573853,-6.55446122979663));
#151734=CARTESIAN_POINT('Ctrl Pts',(-6.17471932200857,1.73230722877125,
-6.54774538278079));
#151735=CARTESIAN_POINT('Ctrl Pts',(-6.18826030448658,1.7468654660582,-6.53494359589355));
#151736=CARTESIAN_POINT('Ctrl Pts',(-6.19417168656543,1.75155833712512,
-6.52934271193098));
#151737=CARTESIAN_POINT('Ctrl Pts',(-6.20672502389223,1.75781013680233,
-6.51741017907483));
#151738=CARTESIAN_POINT('Ctrl Pts',(-6.21309382910321,1.75940739641427,
-6.51133973909935));
#151739=CARTESIAN_POINT('Ctrl Pts',(-6.21956384103444,1.75940739641324,
-6.50515377430056));
#151740=CARTESIAN_POINT('Ctrl Pts',(-6.22666367601187,1.75940739641211,
-6.49836563701204));
#151741=CARTESIAN_POINT('Ctrl Pts',(-6.23368238118683,1.7574828971896,-6.49163236471182));
#151742=CARTESIAN_POINT('Ctrl Pts',(-6.24776001891508,1.74964163156032,
-6.47808607599983));
#151743=CARTESIAN_POINT('Ctrl Pts',(-6.25450329968281,1.74349822301387,
-6.47157300893044));
#151744=CARTESIAN_POINT('Ctrl Pts',(-6.2679163505422,1.72630637215997,-6.45858594084605));
#151745=CARTESIAN_POINT('Ctrl Pts',(-6.27403017236557,1.71456563960319,
-6.4526420213443));
#151746=CARTESIAN_POINT('Ctrl Pts',(-6.2798742635728,1.69868853696113,-6.44695134421518));
#151747=CARTESIAN_POINT('Ctrl Pts',(-6.28090985690551,1.69560796586702,
-6.44594238057608));
#151748=CARTESIAN_POINT('Ctrl Pts',(-6.28187176296278,1.69247211203292,
-6.44500482185164));
#151749=CARTESIAN_POINT('Ctrl Pts',(-6.46559354741529,1.00000000002598,
-6.26067888328588));
#151750=CARTESIAN_POINT('Ctrl Pts',(-6.45667074945246,1.04120750309549,
-6.2698937281947));
#151751=CARTESIAN_POINT('Ctrl Pts',(-6.44735851311334,1.0822780172987,-6.27947127288012));
#151752=CARTESIAN_POINT('Ctrl Pts',(-6.39249580284863,1.31475831852555,
-6.3356278820062));
#151753=CARTESIAN_POINT('Ctrl Pts',(-6.33972854265469,1.5038565989558,-6.38861248690754));
#151754=CARTESIAN_POINT('Ctrl Pts',(-6.28187176285275,1.69247211196711,
-6.44500482195888));
#151755=CARTESIAN_POINT('',(-6.720350242,1.69247211199998,-5.986392288));
#151756=CARTESIAN_POINT('Ctrl Pts',(-6.72035024195089,1.69247211200556,
-5.98639228797367));
#151757=CARTESIAN_POINT('Ctrl Pts',(-6.66661042481084,1.50385659891639,
-6.04672084242625));
#151758=CARTESIAN_POINT('Ctrl Pts',(-6.61604656603123,1.31475831840883,
-6.10181211483948));
#151759=CARTESIAN_POINT('Ctrl Pts',(-6.56240790905556,1.0822780171616,-6.15913903875423));
#151760=CARTESIAN_POINT('Ctrl Pts',(-6.55325780023636,1.04120750301805,
-6.16887159319522));
#151761=CARTESIAN_POINT('Ctrl Pts',(-6.54445255389156,1.0000000000086,-6.17819882893568));
#151762=CARTESIAN_POINT('',(-6.834308572,1.69247211199998,-5.855956484));
#151763=CARTESIAN_POINT('Ctrl Pts',(-6.72035024189579,1.69247211204104,
-5.98639228803552));
#151764=CARTESIAN_POINT('Ctrl Pts',(-6.72176548885911,1.69743933272174,
-5.98480352558651));
#151765=CARTESIAN_POINT('Ctrl Pts',(-6.72334382988621,1.70224131099489,
-5.98303055207738));
#151766=CARTESIAN_POINT('Ctrl Pts',(-6.7302930657659,1.72064855706955,-5.97521687739586));
#151767=CARTESIAN_POINT('Ctrl Pts',(-6.73679708808431,1.73230722846238,
-5.96788851247172));
#151768=CARTESIAN_POINT('Ctrl Pts',(-6.74913601522039,1.74686546575903,
-5.95392445750275));
#151769=CARTESIAN_POINT('Ctrl Pts',(-6.75452154044654,1.75155833682971,
-5.94781622884727));
#151770=CARTESIAN_POINT('Ctrl Pts',(-6.76595471773228,1.75781013651241,
-5.93480646037548));
#151771=CARTESIAN_POINT('Ctrl Pts',(-6.77175373396333,1.75940739612622,
-5.92818956290777));
#151772=CARTESIAN_POINT('Ctrl Pts',(-6.77764319392101,1.75940739612599,
-5.92144853358502));
#151773=CARTESIAN_POINT('Ctrl Pts',(-6.78410596311402,1.75940739612575,
-5.91405129904242));
#151774=CARTESIAN_POINT('Ctrl Pts',(-6.79049284716903,1.75748289690447,
-5.90671598103711));
#151775=CARTESIAN_POINT('Ctrl Pts',(-6.80329953250677,1.74964163127831,
-5.89196231598691));
#151776=CARTESIAN_POINT('Ctrl Pts',(-6.80943183997698,1.74349822273392,
-5.88487100558439));
#151777=CARTESIAN_POINT('Ctrl Pts',(-6.82162674202863,1.72630637188464,
-5.87073388301057));
#151778=CARTESIAN_POINT('Ctrl Pts',(-6.82718314256655,1.71456563933025,
-5.86426585321871));
#151779=CARTESIAN_POINT('Ctrl Pts',(-6.83249359879879,1.69868853674338,
-5.85807422480591));
#151780=CARTESIAN_POINT('Ctrl Pts',(-6.83343458031894,1.69560796570414,
-5.85697649310469));
#151781=CARTESIAN_POINT('Ctrl Pts',(-6.83430857189647,1.69247211192666,
-5.85595648413667));
#151782=CARTESIAN_POINT('Ctrl Pts',(-7.00076789655381,0.999999999903773,
-5.65590389403687));
#151783=CARTESIAN_POINT('Ctrl Pts',(-6.99270703148499,1.04120750294805,
-5.66588147612623));
#151784=CARTESIAN_POINT('Ctrl Pts',(-6.98429080796196,1.08227801712618,
-5.67625520685598));
#151785=CARTESIAN_POINT('Ctrl Pts',(-6.93468279847113,1.31475831832256,
-5.73710360140729));
#151786=CARTESIAN_POINT('Ctrl Pts',(-6.88687746711329,1.50385659874697,
-5.79460492660105));
#151787=CARTESIAN_POINT('Ctrl Pts',(-6.83430857163228,1.69247211175275,
-5.855956484445));
#151788=CARTESIAN_POINT('',(-7.229912155,1.69247211199998,-5.359885281));
#151789=CARTESIAN_POINT('Ctrl Pts',(-7.22991215493042,1.69247211222666,
-5.35988528160718));
#151790=CARTESIAN_POINT('Ctrl Pts',(-7.18179648839481,1.50385659905977,
-5.4247881711377));
#151791=CARTESIAN_POINT('Ctrl Pts',(-7.13637452840358,1.31475831847509,
-5.48419017167095));
#151792=CARTESIAN_POINT('Ctrl Pts',(-7.08809055071594,1.08227801718246,
-5.54609444640031));
#151793=CARTESIAN_POINT('Ctrl Pts',(-7.07984969700402,1.04120750307276,
-5.55660802986153));
#151794=CARTESIAN_POINT('Ctrl Pts',(-7.07191598496282,1.00000000009741,
-5.56668701308303));
#151795=CARTESIAN_POINT('',(-7.331719547,1.69247211199998,-5.219759428));
#151796=CARTESIAN_POINT('Ctrl Pts',(-7.2299121553839,1.69247211190049,-5.35988528099549));
#151797=CARTESIAN_POINT('Ctrl Pts',(-7.23117928939508,1.69743933249794,
-5.35817605269869));
#151798=CARTESIAN_POINT('Ctrl Pts',(-7.23259234834446,1.70224131069263,
-5.35626873528853));
#151799=CARTESIAN_POINT('Ctrl Pts',(-7.23881319621897,1.72064855670075,
-5.34786359149697));
#151800=CARTESIAN_POINT('Ctrl Pts',(-7.24463412568797,1.73230722809895,
-5.33998171234982));
#151801=CARTESIAN_POINT('Ctrl Pts',(-7.25567165169415,1.74686546540357,
-5.3249678196583));
#151802=CARTESIAN_POINT('Ctrl Pts',(-7.26048795898428,1.75155833647739,
-5.31840142617492));
#151803=CARTESIAN_POINT('Ctrl Pts',(-7.2707089230063,1.75781013616434,-5.30441916909238));
#151804=CARTESIAN_POINT('Ctrl Pts',(-7.27589145998758,1.75940739577936,
-5.29730908949956));
#151805=CARTESIAN_POINT('Ctrl Pts',(-7.28115294950206,1.7594073957793,-5.29006727045672));
#151806=CARTESIAN_POINT('Ctrl Pts',(-7.28692661849261,1.75940739577923,
-5.28212049684293));
#151807=CARTESIAN_POINT('Ctrl Pts',(-7.29263025799209,1.75748289655853,
-5.27424219279995));
#151808=CARTESIAN_POINT('Ctrl Pts',(-7.30406287903831,1.7496416309341,-5.25839993924684));
#151809=CARTESIAN_POINT('Ctrl Pts',(-7.30953483947672,1.74349822239083,
-5.25078748057242));
#151810=CARTESIAN_POINT('Ctrl Pts',(-7.32041340653932,1.72630637154358,
-5.23561412730616));
#151811=CARTESIAN_POINT('Ctrl Pts',(-7.32536764892154,1.71456563898968,
-5.22867406399611));
#151812=CARTESIAN_POINT('Ctrl Pts',(-7.33010171347168,1.69868853658723,
-5.22203133570847));
#151813=CARTESIAN_POINT('Ctrl Pts',(-7.33094050691843,1.69560796573972,
-5.22085367428564));
#151814=CARTESIAN_POINT('Ctrl Pts',(-7.33171954712374,1.69247211216014,
-5.21975942762917));
#151815=CARTESIAN_POINT('Ctrl Pts',(-7.47957617958272,1.00000000003768,
-5.00559089157501));
#151816=CARTESIAN_POINT('Ctrl Pts',(-7.472442148756,1.0412075030462,-5.01625087721741));
#151817=CARTESIAN_POINT('Ctrl Pts',(-7.46498970053469,1.08227801718884,
-5.0273372708077));
#151818=CARTESIAN_POINT('Ctrl Pts',(-7.42103580633786,1.3147583184205,-5.09238753530659));
#151819=CARTESIAN_POINT('Ctrl Pts',(-7.37857730422628,1.50385659891382,
-5.15394261395913));
#151820=CARTESIAN_POINT('Ctrl Pts',(-7.33171954689144,1.69247211198855,
-5.21975942795546));
#151821=CARTESIAN_POINT('',(-7.681263067,1.69247211199998,-4.69022363));
#151822=CARTESIAN_POINT('Ctrl Pts',(-7.68126306643363,1.69247211231474,
-4.69022363051514));
#151823=CARTESIAN_POINT('Ctrl Pts',(-7.63915894961858,1.50385659926452,
-4.75917829513542));
#151824=CARTESIAN_POINT('Ctrl Pts',(-7.59924459938713,1.31475831879601,
-4.8224127537344));
#151825=CARTESIAN_POINT('Ctrl Pts',(-7.55670405519824,1.08227801749227,
-4.88839596244951));
#151826=CARTESIAN_POINT('Ctrl Pts',(-7.54943880707296,1.0412075032506,-4.89960592578131));
#151827=CARTESIAN_POINT('Ctrl Pts',(-7.54244050689292,1.00000000014238,
-4.91035550647617));
#151828=CARTESIAN_POINT('',(-7.770099827,1.69247211199998,-4.541535938));
#151829=CARTESIAN_POINT('Ctrl Pts',(-7.68126306658055,1.69247211219402,
-4.69022363027453));
#151830=CARTESIAN_POINT('Ctrl Pts',(-7.68237188542729,1.6974393327218,-4.68840769783155));
#151831=CARTESIAN_POINT('Ctrl Pts',(-7.68360828518667,1.70224131085113,
-4.68638139311886));
#151832=CARTESIAN_POINT('Ctrl Pts',(-7.68905065845813,1.72064855681643,
-4.6774524534919));
#151833=CARTESIAN_POINT('Ctrl Pts',(-7.69414162837981,1.73230722823066,
-4.6690805203751));
#151834=CARTESIAN_POINT('Ctrl Pts',(-7.70378888559198,1.74686546555534,
-4.65313767299271));
#151835=CARTESIAN_POINT('Ctrl Pts',(-7.7079971968728,1.75155833663595,-4.64616598342078));
#151836=CARTESIAN_POINT('Ctrl Pts',(-7.71692365444042,1.7578101363352,-4.6313238146405));
#151837=CARTESIAN_POINT('Ctrl Pts',(-7.72144798543252,1.75940739595605,
-4.6237777991027));
#151838=CARTESIAN_POINT('Ctrl Pts',(-7.72603914208534,1.75940739596087,
-4.61609349720791));
#151839=CARTESIAN_POINT('Ctrl Pts',(-7.73107722468816,1.75940739596616,
-4.6076611672705));
#151840=CARTESIAN_POINT('Ctrl Pts',(-7.73605169728343,1.75748289675087,
-4.59930330866004));
#151841=CARTESIAN_POINT('Ctrl Pts',(-7.74601820529917,1.74964163113785,
-4.58250001911516));
#151842=CARTESIAN_POINT('Ctrl Pts',(-7.75078576169847,1.74349822260255,
-4.57442770321189));
#151843=CARTESIAN_POINT('Ctrl Pts',(-7.76026040594584,1.726306371776,-4.55834028617847));
#151844=CARTESIAN_POINT('Ctrl Pts',(-7.76457260152491,1.7145656392368,-4.55098406666299));
#151845=CARTESIAN_POINT('Ctrl Pts',(-7.76869215858641,1.69868853671208,
-4.54394372171134));
#151846=CARTESIAN_POINT('Ctrl Pts',(-7.76942201057285,1.69560796572158,
-4.54269561228854));
#151847=CARTESIAN_POINT('Ctrl Pts',(-7.77009982710407,1.69247211199432,
-4.54153593807615));
#151848=CARTESIAN_POINT('Ctrl Pts',(-7.89816331283003,0.999999999979971,
-4.3149758149804));
#151849=CARTESIAN_POINT('Ctrl Pts',(-7.89201355528089,1.04120750283238,
-4.3262323762081));
#151850=CARTESIAN_POINT('Ctrl Pts',(-7.88558488510778,1.08227801681994,
-4.33794217150246));
#151851=CARTESIAN_POINT('Ctrl Pts',(-7.84763899711798,1.31475831805313,
-4.40667055946035));
#151852=CARTESIAN_POINT('Ctrl Pts',(-7.81086917512473,1.50385659869719,
-4.47178378631242));
#151853=CARTESIAN_POINT('Ctrl Pts',(-7.77009982702067,1.69247211192352,
-4.54153593821884));
#151854=CARTESIAN_POINT('',(-8.070768965,1.69247211199998,-3.982799055));
#151855=CARTESIAN_POINT('Ctrl Pts',(-8.07076896483244,1.69247211221444,
-3.98279905547561));
#151856=CARTESIAN_POINT('Ctrl Pts',(-8.03501539529515,1.50385659911875,
-4.05525031284116));
#151857=CARTESIAN_POINT('Ctrl Pts',(-8.00093002167116,1.31475831860448,
-4.12180810288601));
#151858=CARTESIAN_POINT('Ctrl Pts',(-7.96447542245618,1.08227801735784,
-4.19133898755908));
#151859=CARTESIAN_POINT('Ctrl Pts',(-7.95824427546741,1.04120750322134,
-4.20315507466473));
#151860=CARTESIAN_POINT('Ctrl Pts',(-7.95223773338732,1.00000000021904,
-4.21448870347174));
#151861=CARTESIAN_POINT('',(-8.1459198327977,1.69247211207413,-3.82674667047894));
#151862=CARTESIAN_POINT('Ctrl Pts',(-8.07076896488867,1.69247211216004,
-3.98279905536167));
#151863=CARTESIAN_POINT('Ctrl Pts',(-8.07171054104207,1.69743933278747,
-3.98089103954382));
#151864=CARTESIAN_POINT('Ctrl Pts',(-8.07276032688418,1.70224131101044,
-3.97876206207974));
#151865=CARTESIAN_POINT('Ctrl Pts',(-8.07738040680549,1.72064855704358,
-3.96938121711276));
#151866=CARTESIAN_POINT('Ctrl Pts',(-8.08170042767802,1.73230722844107,
-3.96058663591419));
#151867=CARTESIAN_POINT('Ctrl Pts',(-8.08987974204303,1.74686546574379,
-3.94384319628409));
#151868=CARTESIAN_POINT('Ctrl Pts',(-8.09344617446283,1.75155833681651,
-3.93652234257194));
#151869=CARTESIAN_POINT('Ctrl Pts',(-8.10100625498023,1.75781013650272,
-3.92093976251732));
#151870=CARTESIAN_POINT('Ctrl Pts',(-8.10483595272582,1.75940739611808,
-3.91301856711897));
#151871=CARTESIAN_POINT('Ctrl Pts',(-8.10871981121782,1.75940739611904,
-3.90495365185858));
#151872=CARTESIAN_POINT('Ctrl Pts',(-8.11298174375302,1.75940739612008,
-3.89610365775793));
#151873=CARTESIAN_POINT('Ctrl Pts',(-8.11718699791386,1.75748289690017,
-3.88733353714228));
#151874=CARTESIAN_POINT('Ctrl Pts',(-8.12560714843641,1.74964163127695,
-3.86970450180576));
#151875=CARTESIAN_POINT('Ctrl Pts',(-8.12963191523694,1.74349822273462,
-3.86123732220918));
#151876=CARTESIAN_POINT('Ctrl Pts',(-8.13762635240814,1.72630637189051,
-3.84436536781835));
#151877=CARTESIAN_POINT('Ctrl Pts',(-8.14126178192233,1.71456563933967,
-3.83665222004584));
#151878=CARTESIAN_POINT('Ctrl Pts',(-8.14473366319477,1.69868853683266,
-3.8292709432193));
#151879=CARTESIAN_POINT('Ctrl Pts',(-8.14534869733938,1.69560796587296,
-3.82796243490334));
#151880=CARTESIAN_POINT('Ctrl Pts',(-8.14591983278025,1.69247211217755,
-3.826746670204));
#151881=CARTESIAN_POINT('Ctrl Pts',(-8.25315907928445,1.00000000000618,
-3.589619090102));
#151882=CARTESIAN_POINT('Ctrl Pts',(-8.24804310921235,1.04120750292176,
-3.6013815957579));
#151883=CARTESIAN_POINT('Ctrl Pts',(-8.24268997692429,1.08227801697206,
-3.61362051242964));
#151884=CARTESIAN_POINT('Ctrl Pts',(-8.21105761312823,1.31475831812732,
-3.68547366326024));
#151885=CARTESIAN_POINT('Ctrl Pts',(-8.18027252030632,1.50385659863499,
-3.75362078478248));
#151886=CARTESIAN_POINT('Ctrl Pts',(-8.14591983233074,1.6924721117247,-3.82674667116087));
#151887=CARTESIAN_POINT('',(-8.395293776,1.69247211199998,-3.243307326));
#151888=CARTESIAN_POINT('Ctrl Pts',(-8.39529377643543,1.69247211171466,
-3.24330732545413));
#151889=CARTESIAN_POINT('Ctrl Pts',(-8.36617862092618,1.50385659880013,
-3.31867184053676));
#151890=CARTESIAN_POINT('Ctrl Pts',(-8.33819665932569,1.31475831846641,
-3.38801707774584));
#151891=CARTESIAN_POINT('Ctrl Pts',(-8.30812151607705,1.08227801737161,
-3.460535816552));
#151892=CARTESIAN_POINT('Ctrl Pts',(-8.30297463973183,1.04120750320158,
-3.47286289128436));
#151893=CARTESIAN_POINT('Ctrl Pts',(-8.29800821687382,1.0000000001655,-3.48468931652372));
#151894=CARTESIAN_POINT('',(-8.456153681,1.69247211199998,-3.081146689));
#151895=CARTESIAN_POINT('Ctrl Pts',(-8.39529377630737,1.69247211186686,
-3.24330732578562));
#151896=CARTESIAN_POINT('Ctrl Pts',(-8.39606052875182,1.69743933266437,
-3.24132258879396));
#151897=CARTESIAN_POINT('Ctrl Pts',(-8.39691524842105,1.70224131104791,
-3.23910807982608));
#151898=CARTESIAN_POINT('Ctrl Pts',(-8.4006758368303,1.72064855723026,-3.22935085853309));
#151899=CARTESIAN_POINT('Ctrl Pts',(-8.40419012638921,1.73230722862894,
-3.22020443804666));
#151900=CARTESIAN_POINT('Ctrl Pts',(-8.41083564288389,1.7468654659326,-3.20279521449444));
#151901=CARTESIAN_POINT('Ctrl Pts',(-8.41373148162846,1.75155833700544,
-3.19518413985006));
#151902=CARTESIAN_POINT('Ctrl Pts',(-8.41986431577829,1.75781013669251,
-3.17898661028975));
#151903=CARTESIAN_POINT('Ctrl Pts',(-8.42296854580602,1.75940739630863,
-3.17075401183652));
#151904=CARTESIAN_POINT('Ctrl Pts',(-8.42611383559583,1.75940739631059,
-3.1623734171632));
#151905=CARTESIAN_POINT('Ctrl Pts',(-8.42956530348967,1.75940739631274,
-3.15317701384931));
#151906=CARTESIAN_POINT('Ctrl Pts',(-8.43296748098366,1.75748289709377,
-3.1440652430834));
#151907=CARTESIAN_POINT('Ctrl Pts',(-8.43977347991322,1.74964163147231,
-3.12575240058616));
#151908=CARTESIAN_POINT('Ctrl Pts',(-8.44302305205915,1.74349822293125,
-3.11695853005104));
#151909=CARTESIAN_POINT('Ctrl Pts',(-8.44947291564613,1.72630637209083,
-3.09943788136671));
#151910=CARTESIAN_POINT('Ctrl Pts',(-8.45240230875442,1.71456563954304,
-3.09142990707129));
#151911=CARTESIAN_POINT('Ctrl Pts',(-8.45519856073018,1.69868853687056,
-3.08376712797648));
#151912=CARTESIAN_POINT('Ctrl Pts',(-8.45569382517283,1.69560796573517,
-3.08240875602404));
#151913=CARTESIAN_POINT('Ctrl Pts',(-8.45615368110476,1.69247211185841,
-3.08114668938989));
#151914=CARTESIAN_POINT('Ctrl Pts',(-8.54170526185697,0.999999999891994,
-2.83536086231805));
#151915=CARTESIAN_POINT('Ctrl Pts',(-8.53766427004687,1.04120750290419,
-2.84753460763075));
#151916=CARTESIAN_POINT('Ctrl Pts',(-8.53342977591951,1.08227801705046,
-2.8602041051281));
#151917=CARTESIAN_POINT('Ctrl Pts',(-8.50836562150266,1.31475831827597,
-2.93460349954225));
#151918=CARTESIAN_POINT('Ctrl Pts',(-8.48381312130125,1.50385659875945,
-3.00523583521544));
#151919=CARTESIAN_POINT('Ctrl Pts',(-8.45615368107748,1.69247211182429,
-3.08114668946476));
#151920=CARTESIAN_POINT('',(-8.652224619,1.69247211199998,-2.477702391));
#151921=CARTESIAN_POINT('Ctrl Pts',(-8.65222461931464,1.69247211184308,
-2.47770239070908));
#151922=CARTESIAN_POINT('Ctrl Pts',(-8.6299822958743,1.50385659864939,-2.55537337297999));
#151923=CARTESIAN_POINT('Ctrl Pts',(-8.60832904052779,1.31475831803842,
-2.62694773048628));
#151924=CARTESIAN_POINT('Ctrl Pts',(-8.58487550058799,1.08227801688606,
-2.70187044525523));
#151925=CARTESIAN_POINT('Ctrl Pts',(-8.58085433453559,1.04120750294561,
-2.7146092571805));
#151926=CARTESIAN_POINT('Ctrl Pts',(-8.57696801764159,1.00000000014065,
-2.72683325936026));
#151927=CARTESIAN_POINT('',(-8.69830355250517,1.69247211177544,-2.31073912599594));
#151928=CARTESIAN_POINT('Ctrl Pts',(-8.65222461924908,1.6924721119451,-2.47770239093806));
#151929=CARTESIAN_POINT('Ctrl Pts',(-8.65281037451572,1.69743933267268,
-2.4756569127735));
#151930=CARTESIAN_POINT('Ctrl Pts',(-8.65346314627405,1.70224131098984,
-2.47337470231207));
#151931=CARTESIAN_POINT('Ctrl Pts',(-8.6563339650763,1.7206485570939,-2.46331966420912));
#151932=CARTESIAN_POINT('Ctrl Pts',(-8.65901422832519,1.73230722847676,
-2.45389504603903));
#151933=CARTESIAN_POINT('Ctrl Pts',(-8.66407244115263,1.74686546576065,
-2.43596020740362));
#151934=CARTESIAN_POINT('Ctrl Pts',(-8.66627437062938,1.75155833682684,
-2.428120191726));
#151935=CARTESIAN_POINT('Ctrl Pts',(-8.67093058043352,1.75781013650177,
-2.41143812564638));
#151936=CARTESIAN_POINT('Ctrl Pts',(-8.6732843493065,1.7594073961121,-2.40296040818193));
#151937=CARTESIAN_POINT('Ctrl Pts',(-8.6756657463679,1.75940739610916,-2.3943316097188));
#151938=CARTESIAN_POINT('Ctrl Pts',(-8.67827896042827,1.75940739610594,
-2.38486284122433));
#151939=CARTESIAN_POINT('Ctrl Pts',(-8.68085066892036,1.75748289688156,
-2.37548278293022));
#151940=CARTESIAN_POINT('Ctrl Pts',(-8.68598771835229,1.74964163124873,
-2.35663357751049));
#151941=CARTESIAN_POINT('Ctrl Pts',(-8.68843593219853,1.74349822269972,
-2.34758381910882));
#151942=CARTESIAN_POINT('Ctrl Pts',(-8.6932892916914,1.72630637183859,-2.32955554208355));
#151943=CARTESIAN_POINT('Ctrl Pts',(-8.69548906264279,1.71456563927603,
-2.32131721676111));
#151944=CARTESIAN_POINT('Ctrl Pts',(-8.69758717149787,1.69868853665797,
-2.31343463170189));
#151945=CARTESIAN_POINT('Ctrl Pts',(-8.69795867862004,1.69560796559486,
-2.31203733302424));
#151946=CARTESIAN_POINT('Ctrl Pts',(-8.69830355251919,1.69247211179278,
-2.31073912595777));
#151947=CARTESIAN_POINT('Ctrl Pts',(-8.76147865593336,0.999999999896205,
-2.05827397632681));
#151948=CARTESIAN_POINT('Ctrl Pts',(-8.75854517807591,1.0412075030467,-2.07076094547247));
#151949=CARTESIAN_POINT('Ctrl Pts',(-8.75546341576689,1.08227801733034,
-2.08375901646764));
#151950=CARTESIAN_POINT('Ctrl Pts',(-8.73716927257158,1.31475831846968,
-2.16010563424933));
#151951=CARTESIAN_POINT('Ctrl Pts',(-8.71904704729885,1.5038565987368,-2.23265449395954));
#151952=CARTESIAN_POINT('Ctrl Pts',(-8.69830355239435,1.6924721115845,-2.3107391264277));
#151953=CARTESIAN_POINT('',(-8.839492837,1.69247211199998,-1.692148455));
#151954=CARTESIAN_POINT('Ctrl Pts',(-8.83949283651608,1.69247211196708,
-1.69214845482919));
#151955=CARTESIAN_POINT('Ctrl Pts',(-8.82430242730659,1.50385659886907,
-1.77150054300318));
#151956=CARTESIAN_POINT('Ctrl Pts',(-8.80915221754667,1.31475831835278,
-1.84472774598002));
#151957=CARTESIAN_POINT('Ctrl Pts',(-8.79250911503047,1.08227801717924,
-1.92145120303552));
#151958=CARTESIAN_POINT('Ctrl Pts',(-8.78964603529871,1.04120750311893,
-1.93449918683022));
#151959=CARTESIAN_POINT('Ctrl Pts',(-8.78687111467304,1.00000000019332,
-1.94702234556372));
#151960=CARTESIAN_POINT('',(-8.870419798,1.69247211199998,-1.521726851));
#151961=CARTESIAN_POINT('Ctrl Pts',(-8.83949283655333,1.6924721118822,-1.69214845463461));
#151962=CARTESIAN_POINT('Ctrl Pts',(-8.83989287848787,1.69743933253479,
-1.6900587042909));
#151963=CARTESIAN_POINT('Ctrl Pts',(-8.84033844660458,1.70224131078141,
-1.68772716736002));
#151964=CARTESIAN_POINT('Ctrl Pts',(-8.84229638166105,1.72064855683224,
-1.67745526970967));
#151965=CARTESIAN_POINT('Ctrl Pts',(-8.84412103869949,1.7323072282259,-1.66782833533496));
#151966=CARTESIAN_POINT('Ctrl Pts',(-8.84755122211043,1.74686546552436,
-1.64951228238131));
#151967=CARTESIAN_POINT('Ctrl Pts',(-8.84904151368015,1.75155833659586,
-1.64150644886352));
#151968=CARTESIAN_POINT('Ctrl Pts',(-8.85218361007993,1.75781013627922,
-1.62447416044409));
#151969=CARTESIAN_POINT('Ctrl Pts',(-8.85376796663778,1.75940739589287,
-1.61581958156026));
#151970=CARTESIAN_POINT('Ctrl Pts',(-8.8553662973649,1.759407395892,-1.60701205331319));
#151971=CARTESIAN_POINT('Ctrl Pts',(-8.85712021753,1.75940739589105,-1.59734715659617));
#151972=CARTESIAN_POINT('Ctrl Pts',(-8.85884075113716,1.75748289666931,
-1.58777433348841));
#151973=CARTESIAN_POINT('Ctrl Pts',(-8.86226749057167,1.74964163104244,
-1.56854052787078));
#151974=CARTESIAN_POINT('Ctrl Pts',(-8.86389463454005,1.74349822249752,
-1.55930774494077));
#151975=CARTESIAN_POINT('Ctrl Pts',(-8.86711241354167,1.72630637164629,
-1.54091699267149));
#151976=CARTESIAN_POINT('Ctrl Pts',(-8.8685648510738,1.71456563908994,-1.53251464647819));
#151977=CARTESIAN_POINT('Ctrl Pts',(-8.86994792407433,1.69868853657767,
-1.5244757214109));
#151978=CARTESIAN_POINT('Ctrl Pts',(-8.87019268272298,1.6956079656182,-1.52305074624817));
#151979=CARTESIAN_POINT('Ctrl Pts',(-8.87041979787082,1.69247211192306,
-1.52172685116002));
#151980=CARTESIAN_POINT('Ctrl Pts',(-8.91070977542002,0.999999999993989,
-1.26461507907905));
#151981=CARTESIAN_POINT('Ctrl Pts',(-8.90890743017016,1.04120750304135,
-1.27731473425656));
#151982=CARTESIAN_POINT('Ctrl Pts',(-8.9070032122354,1.08227801722256,-1.2905367258509));
#151983=CARTESIAN_POINT('Ctrl Pts',(-8.89562637393288,1.31475831840746,
-1.36821586896249));
#151984=CARTESIAN_POINT('Ctrl Pts',(-8.88408033304455,1.50385659881792,
-1.44209713210709));
#151985=CARTESIAN_POINT('Ctrl Pts',(-8.87041979782602,1.69247211180957,
-1.52172685142118));
#151986=CARTESIAN_POINT('',(-8.955590655,1.69247211199998,-0.892970333000001));
#151987=CARTESIAN_POINT('Ctrl Pts',(-8.9555906552352,1.69247211204864,-0.892970333137612));
#151988=CARTESIAN_POINT('Ctrl Pts',(-8.94757446449693,1.50385659895089,
-0.97336463091238));
#151989=CARTESIAN_POINT('Ctrl Pts',(-8.93904928090067,1.3147583184345,-1.04765509702603));
#151990=CARTESIAN_POINT('Ctrl Pts',(-8.92935061629266,1.0822780171992,-1.12556156422249));
#151991=CARTESIAN_POINT('Ctrl Pts',(-8.92766867472662,1.04120750307671,
-1.13881366517733));
#151992=CARTESIAN_POINT('Ctrl Pts',(-8.92602749240836,1.00000000008849,
-1.15153515133937));
#151993=CARTESIAN_POINT('',(-8.971116639,1.69247211199998,-0.720462525999999));
#151994=CARTESIAN_POINT('Ctrl Pts',(-8.95559065523919,1.69247211203143,
-0.892970333097604));
#151995=CARTESIAN_POINT('Ctrl Pts',(-8.9558017629423,1.69743933257032,-0.890853136027187));
#151996=CARTESIAN_POINT('Ctrl Pts',(-8.95603653996893,1.7022413107097,-0.888491044806472));
#151997=CARTESIAN_POINT('Ctrl Pts',(-8.95706582714206,1.72064855666438,
-0.878084990907433));
#151998=CARTESIAN_POINT('Ctrl Pts',(-8.95802018690317,1.73230722806008,
-0.868333250744462));
#151999=CARTESIAN_POINT('Ctrl Pts',(-8.95979472307499,1.7468654653616,-0.849783453564588));
#152000=CARTESIAN_POINT('Ctrl Pts',(-8.96056137778506,1.75155833643442,
-0.841676260471871));
#152001=CARTESIAN_POINT('Ctrl Pts',(-8.96216406246514,1.7578101361195,-0.824430883686811));
#152002=CARTESIAN_POINT('Ctrl Pts',(-8.96296625039908,1.7594073957336,-0.815669124965457));
#152003=CARTESIAN_POINT('Ctrl Pts',(-8.96376864597117,1.75940739573272,
-0.806753779975071));
#152004=CARTESIAN_POINT('Ctrl Pts',(-8.96464915070661,1.75940739573176,
-0.796970571100177));
#152005=CARTESIAN_POINT('Ctrl Pts',(-8.96550465670328,1.75748289651018,
-0.787282057921237));
#152006=CARTESIAN_POINT('Ctrl Pts',(-8.9671934960484,1.74964163088392,-0.767818511397056));
#152007=CARTESIAN_POINT('Ctrl Pts',(-8.96798646933209,1.74349822233936,
-0.758477040876453));
#152008=CARTESIAN_POINT('Ctrl Pts',(-8.96954276017722,1.72630637148871,
-0.739871884883414));
#152009=CARTESIAN_POINT('Ctrl Pts',(-8.97023617011667,1.71456563893235,
-0.731373168568874));
#152010=CARTESIAN_POINT('Ctrl Pts',(-8.97089307157978,1.69868853652994,
-0.723242628198457));
#152011=CARTESIAN_POINT('Ctrl Pts',(-8.97100911110934,1.695607965685,-0.72180144961933));
#152012=CARTESIAN_POINT('Ctrl Pts',(-8.97111663891427,1.6924721121081,-0.720462525739919));
#152013=CARTESIAN_POINT('Ctrl Pts',(-8.98819709930371,0.999999999959407,
-0.460774244146092));
#152014=CARTESIAN_POINT('Ctrl Pts',(-8.98754039807928,1.04120750304597,
-0.473584335238514));
#152015=CARTESIAN_POINT('Ctrl Pts',(-8.98682905615476,1.08227801726612,
-0.486923791773003));
#152016=CARTESIAN_POINT('Ctrl Pts',(-8.98246112236426,1.31475831853778,
-0.56531003343955));
#152017=CARTESIAN_POINT('Ctrl Pts',(-8.9775842278123,1.50385659899527,-0.639928851482268));
#152018=CARTESIAN_POINT('Ctrl Pts',(-8.97111663890039,1.69247211203383,
-0.72046252591272));
#152019=CARTESIAN_POINT('',(-8.999583324,1.69247211199998,-0.0866025400000003));
#152020=CARTESIAN_POINT('Ctrl Pts',(-8.99958332369346,1.69247211191239,
-0.0866025397925534));
#152021=CARTESIAN_POINT('Ctrl Pts',(-8.99880589307639,1.50385659887802,
-0.167391759525919));
#152022=CARTESIAN_POINT('Ctrl Pts',(-8.99697437540592,1.31475831842477,
-0.242147345601193));
#152023=CARTESIAN_POINT('Ctrl Pts',(-8.99429823665166,1.08227801725347,
-0.320609565836488));
#152024=CARTESIAN_POINT('Ctrl Pts',(-8.99381097525933,1.04120750313013,
-0.333959085808913));
#152025=CARTESIAN_POINT('Ctrl Pts',(-8.9933167450867,1.00000000014106,-0.346776473456898));
#152026=CARTESIAN_POINT('Ctrl Pts',(-8.9995833236904,1.69247211204887,-0.0866025401111392));
#152027=CARTESIAN_POINT('Ctrl Pts',(-8.99960379745391,1.69743933262498,
-0.0844749426937014));
#152028=CARTESIAN_POINT('Ctrl Pts',(-8.99962589311285,1.70224131079953,
-0.082101315292519));
#152029=CARTESIAN_POINT('Ctrl Pts',(-8.99971824519885,1.72064855678832,
-0.0716448884975285));
#152030=CARTESIAN_POINT('Ctrl Pts',(-8.99979462373951,1.73230722818554,
-0.0618468578231623));
#152031=CARTESIAN_POINT('Ctrl Pts',(-8.99989922515123,1.7468654654886,-0.0432126684760381));
#152032=CARTESIAN_POINT('Ctrl Pts',(-8.999936070349,1.75155833656183,-0.0350693901608667));
#152033=CARTESIAN_POINT('Ctrl Pts',(-8.99998643943524,1.75781013624805,
-0.0177497746457722));
#152034=CARTESIAN_POINT('Ctrl Pts',(-9.,1.75940739586291,-0.00895138061713929));
#152035=CARTESIAN_POINT('Ctrl Pts',(-9.,1.75940739586291,2.22044604925031E-15));
#152036=CARTESIAN_POINT('Origin',(1.11022302462516E-15,2.49999999999998,
2.22044604925031E-15));
#152037=CARTESIAN_POINT('',(-3.5,2.49999999999998,2.64907242895189E-15));
#152038=CARTESIAN_POINT('',(-3.5,2.49999999999998,2.64907242895189E-15));
#152039=CARTESIAN_POINT('Origin',(1.11022302462516E-15,2.49999999999998,
2.22044604925031E-15));
#152040=CARTESIAN_POINT('Origin',(1.11022302462516E-15,2.49999999999998,
2.22044604925031E-15));
#152041=CARTESIAN_POINT('',(-2.5,2.49999999999998,2.52660774903715E-15));
#152042=CARTESIAN_POINT('Origin',(3.5,4.99999999999998,2.22044604925031E-15));
#152043=CARTESIAN_POINT('Origin',(9.,2.49999999999998,2.22044604925031E-15));
#152044=CARTESIAN_POINT('Origin',(2.5,-1.50000000000002,2.22044604925031E-15));
#152045=CARTESIAN_POINT('Origin',(10.516666667,-1.77635683940025E-14,0.0866025400000026));
#152046=CARTESIAN_POINT('Origin',(10.516666667,-1.77635683940025E-14,0.0866025400000026));
#152047=CARTESIAN_POINT('Origin',(10.516666667,-1.77635683940025E-14,2.22044604925031E-15));
#152048=CARTESIAN_POINT('Origin',(10.516666667,-1.77635683940025E-14,-0.0866025400000003));
#152049=CARTESIAN_POINT('Origin',(10.516666667,-1.77635683940025E-14,-0.349999999999999));
#152050=CARTESIAN_POINT('Origin',(10.48209265,-1.77635683940025E-14,-0.856452827999998));
#152051=CARTESIAN_POINT('Origin',(10.48209265,-1.77635683940025E-14,-0.856452827999998));
#152052=CARTESIAN_POINT('Origin',(10.474329659,-1.77635683940025E-14,-0.942706732));
#152053=CARTESIAN_POINT('Origin',(10.466566667,-1.77635683940025E-14,-1.028960636));
#152054=CARTESIAN_POINT('Origin',(10.4429559,-1.77635683940025E-14,-1.291297735));
#152055=CARTESIAN_POINT('Origin',(10.363122987,-1.77635683940025E-14,-1.792612542));
#152056=CARTESIAN_POINT('Origin',(10.363122987,-1.77635683940025E-14,-1.792612542));
#152057=CARTESIAN_POINT('Origin',(10.347659507,-1.77635683940025E-14,-1.877823344));
#152058=CARTESIAN_POINT('Origin',(10.332196026,-1.77635683940025E-14,-1.963034146));
#152059=CARTESIAN_POINT('Origin',(10.285164594,-1.77635683940025E-14,-2.2221987));
#152060=CARTESIAN_POINT('Origin',(10.160715552,-1.77635683940025E-14,-2.714339193));
#152061=CARTESIAN_POINT('Origin',(10.160715552,-1.77635683940025E-14,-2.714339193));
#152062=CARTESIAN_POINT('Origin',(10.137676085,-1.77635683940025E-14,-2.797820826));
#152063=CARTESIAN_POINT('Origin',(10.114636618,-1.77635683940025E-14,-2.881302458));
#152064=CARTESIAN_POINT('Origin',(10.044563189,-1.77635683940025E-14,-3.135207827));
#152065=CARTESIAN_POINT('Origin',(9.876500009,-1.77635683940025E-14,-3.614211582));
#152066=CARTESIAN_POINT('Origin',(9.876500009,-1.77635683940025E-14,-3.614211582));
#152067=CARTESIAN_POINT('Origin',(9.846070056,-1.77635683940025E-14,-3.6952919));
#152068=CARTESIAN_POINT('Origin',(9.815640104,-1.77635683940025E-14,-3.776372218));
#152069=CARTESIAN_POINT('Origin',(9.723088868,-1.77635683940025E-14,-4.022974105));
#152070=CARTESIAN_POINT('Origin',(9.512764695,-1.77635683940025E-14,-4.484984464));
#152071=CARTESIAN_POINT('Origin',(9.512764695,-1.77635683940025E-14,-4.484984464));
#152072=CARTESIAN_POINT('Origin',(9.475189261,-1.77635683940025E-14,-4.563010656));
#152073=CARTESIAN_POINT('Origin',(9.437613827,-1.77635683940025E-14,-4.641036849));
#152074=CARTESIAN_POINT('Origin',(9.323329952,-1.77635683940025E-14,-4.87834976));
#152075=CARTESIAN_POINT('Origin',(9.072438193,-1.77635683940025E-14,-5.319646888));
#152076=CARTESIAN_POINT('Origin',(9.072438193,-1.77635683940025E-14,-5.319646888));
#152077=CARTESIAN_POINT('Origin',(9.028019813,-1.77635683940025E-14,-5.393990734));
#152078=CARTESIAN_POINT('Origin',(8.983601433,-1.77635683940025E-14,-5.46833458));
#152079=CARTESIAN_POINT('Origin',(8.848505066,-1.77635683940025E-14,-5.694447812));
#152080=CARTESIAN_POINT('Origin',(8.559065754,-1.77635683940025E-14,-6.111478643));
#152081=CARTESIAN_POINT('Origin',(8.559065754,-1.77635683940025E-14,-6.111478643));
#152082=CARTESIAN_POINT('Origin',(8.508162058,-1.77635683940025E-14,-6.18154157));
#152083=CARTESIAN_POINT('Origin',(8.457258362,-1.77635683940025E-14,-6.251604497));
#152084=CARTESIAN_POINT('Origin',(8.302437219,-1.77635683940025E-14,-6.464697518));
#152085=CARTESIAN_POINT('Origin',(7.976780749,-1.77635683940025E-14,-6.854104366));
#152086=CARTESIAN_POINT('Origin',(7.976780749,-1.77635683940025E-14,-6.854104366));
#152087=CARTESIAN_POINT('Origin',(7.919801584,-1.77635683940025E-14,-6.919322268));
#152088=CARTESIAN_POINT('Origin',(7.862822419,-1.77635683940025E-14,-6.98454017));
#152089=CARTESIAN_POINT('Origin',(7.68952303,-1.77635683940025E-14,-7.182897281));
#152090=CARTESIAN_POINT('Origin',(7.330271397,-1.77635683940025E-14,-7.54154487));
#152091=CARTESIAN_POINT('Origin',(7.330271397,-1.77635683940025E-14,-7.54154487));
#152092=CARTESIAN_POINT('Origin',(7.267675525,-1.77635683940025E-14,-7.601392651));
#152093=CARTESIAN_POINT('Origin',(7.205079654,-1.77635683940025E-14,-7.661240432));
#152094=CARTESIAN_POINT('Origin',(7.014697323,-1.77635683940025E-14,-7.843264578));
#152095=CARTESIAN_POINT('Origin',(6.624743009,-1.77635683940025E-14,-8.16826529));
#152096=CARTESIAN_POINT('Origin',(6.624743009,-1.77635683940025E-14,-8.16826529));
#152097=CARTESIAN_POINT('Origin',(6.557034416,-1.77635683940025E-14,-8.222261091));
#152098=CARTESIAN_POINT('Origin',(6.489325824,-1.77635683940025E-14,-8.276256891));
#152099=CARTESIAN_POINT('Origin',(6.283393397,-1.77635683940025E-14,-8.440482521));
#152100=CARTESIAN_POINT('Origin',(5.865876086,-1.77635683940025E-14,-8.72921964));
#152101=CARTESIAN_POINT('Origin',(5.865876086,-1.77635683940025E-14,-8.72921964));
#152102=CARTESIAN_POINT('Origin',(5.793599922,-1.77635683940025E-14,-8.776928718));
#152103=CARTESIAN_POINT('Origin',(5.721323758,-1.77635683940025E-14,-8.824637796));
#152104=CARTESIAN_POINT('Origin',(5.501499283,-1.77635683940025E-14,-8.969742662));
#152105=CARTESIAN_POINT('Origin',(5.059780577,-1.77635683940025E-14,-9.219891447));
#152106=CARTESIAN_POINT('Origin',(5.059780577,-1.77635683940025E-14,-9.219891447));
#152107=CARTESIAN_POINT('Origin',(4.983518767,-1.77635683940025E-14,-9.260929677));
#152108=CARTESIAN_POINT('Origin',(4.907256957,-1.77635683940025E-14,-9.301967907));
#152109=CARTESIAN_POINT('Origin',(4.675310331,-1.77635683940025E-14,-9.426783709));
#152110=CARTESIAN_POINT('Origin',(4.212946691,-1.77635683940025E-14,-9.636330108));
#152111=CARTESIAN_POINT('Origin',(4.212946691,-1.77635683940025E-14,-9.636330108));
#152112=CARTESIAN_POINT('Origin',(4.13331325,-1.77635683940025E-14,-9.670367075));
#152113=CARTESIAN_POINT('Origin',(4.053679809,-1.77635683940025E-14,-9.704404041));
#152114=CARTESIAN_POINT('Origin',(3.811478529,-1.77635683940025E-14,-9.807925836));
#152115=CARTESIAN_POINT('Origin',(3.332192635,-1.77635683940025E-14,-9.975182706));
#152116=CARTESIAN_POINT('Origin',(3.332192635,-1.77635683940025E-14,-9.975182706));
#152117=CARTESIAN_POINT('Origin',(3.249828724,-1.77635683940025E-14,-10.001944363));
#152118=CARTESIAN_POINT('Origin',(3.167464814,-1.77635683940025E-14,-10.02870602));
#152119=CARTESIAN_POINT('Origin',(2.916958943,-1.77635683940025E-14,-10.110100311));
#152120=CARTESIAN_POINT('Origin',(2.424609723,-1.77635683940025E-14,-10.233720998));
#152121=CARTESIAN_POINT('Origin',(2.424609723,-1.77635683940025E-14,-10.233720998));
#152122=CARTESIAN_POINT('Origin',(2.340178489,-1.77635683940025E-14,-10.252991876));
#152123=CARTESIAN_POINT('Origin',(2.255747255,-1.77635683940025E-14,-10.272262754));
#152124=CARTESIAN_POINT('Origin',(1.99895372,-1.77635683940025E-14,-10.330874203));
#152125=CARTESIAN_POINT('Origin',(1.497505279,-1.77635683940025E-14,-10.409863386));
#152126=CARTESIAN_POINT('Origin',(1.497505279,-1.77635683940025E-14,-10.409863386));
#152127=CARTESIAN_POINT('Origin',(1.411686512,-1.77635683940025E-14,-10.421488328));
#152128=CARTESIAN_POINT('Origin',(1.325867745,-1.77635683940025E-14,-10.43311327));
#152129=CARTESIAN_POINT('Origin',(1.064854096,-1.77635683940025E-14,-10.468469971));
#152130=CARTESIAN_POINT('Origin',(0.558343803000001,-1.77635683940025E-14,
-10.502191675));
#152131=CARTESIAN_POINT('Origin',(0.558343803000001,-1.77635683940025E-14,
-10.502191675));
#152132=CARTESIAN_POINT('Origin',(0.471828466000001,-1.77635683940025E-14,
-10.506077083));
#152133=CARTESIAN_POINT('Origin',(0.385313129000001,-1.77635683940025E-14,
-10.509962491));
#152134=CARTESIAN_POINT('Origin',(0.122180893,-1.77635683940025E-14,-10.521779774));
#152135=CARTESIAN_POINT('Origin',(-0.385313127999999,-1.77635683940025E-14,
-10.509962491));
#152136=CARTESIAN_POINT('Origin',(-0.385313127999999,-1.77635683940025E-14,
-10.509962491));
#152137=CARTESIAN_POINT('Origin',(-0.471828465999998,-1.77635683940025E-14,
-10.506077083));
#152138=CARTESIAN_POINT('Origin',(-0.558343802999999,-1.77635683940025E-14,
-10.502191675));
#152139=CARTESIAN_POINT('Origin',(-0.821476038999999,-1.77635683940025E-14,
-10.490374393));
#152140=CARTESIAN_POINT('Origin',(-1.325867745,-1.77635683940025E-14,-10.43311327));
#152141=CARTESIAN_POINT('Origin',(-1.325867745,-1.77635683940025E-14,-10.43311327));
#152142=CARTESIAN_POINT('Origin',(-1.411686512,-1.77635683940025E-14,-10.421488328));
#152143=CARTESIAN_POINT('Origin',(-1.497505279,-1.77635683940025E-14,-10.409863386));
#152144=CARTESIAN_POINT('Origin',(-1.758518929,-1.77635683940025E-14,-10.374506685));
#152145=CARTESIAN_POINT('Origin',(-2.255747255,-1.77635683940025E-14,-10.272262755));
#152146=CARTESIAN_POINT('Origin',(-2.255747255,-1.77635683940025E-14,-10.272262755));
#152147=CARTESIAN_POINT('Origin',(-2.340178489,-1.77635683940025E-14,-10.252991876));
#152148=CARTESIAN_POINT('Origin',(-2.424609723,-1.77635683940025E-14,-10.233720998));
#152149=CARTESIAN_POINT('Origin',(-2.681403258,-1.77635683940025E-14,-10.17510955));
#152150=CARTESIAN_POINT('Origin',(-3.167464814,-1.77635683940025E-14,-10.02870602));
#152151=CARTESIAN_POINT('Origin',(-3.167464814,-1.77635683940025E-14,-10.02870602));
#152152=CARTESIAN_POINT('Origin',(-3.249828724,-1.77635683940025E-14,-10.001944363));
#152153=CARTESIAN_POINT('Origin',(-3.332192634,-1.77635683940025E-14,-9.975182706));
#152154=CARTESIAN_POINT('Origin',(-3.582698505,-1.77635683940025E-14,-9.893788415));
#152155=CARTESIAN_POINT('Origin',(-4.053679809,-1.77635683940025E-14,-9.704404041));
#152156=CARTESIAN_POINT('Origin',(-4.053679809,-1.77635683940025E-14,-9.704404041));
#152157=CARTESIAN_POINT('Origin',(-4.13331325,-1.77635683940025E-14,-9.670367075));
#152158=CARTESIAN_POINT('Origin',(-4.212946691,-1.77635683940025E-14,-9.636330109));
#152159=CARTESIAN_POINT('Origin',(-4.45514797,-1.77635683940025E-14,-9.532808314));
#152160=CARTESIAN_POINT('Origin',(-4.907256957,-1.77635683940025E-14,-9.301967907));
#152161=CARTESIAN_POINT('Origin',(-4.907256957,-1.77635683940025E-14,-9.301967907));
#152162=CARTESIAN_POINT('Origin',(-4.983518767,-1.77635683940025E-14,-9.260929677));
#152163=CARTESIAN_POINT('Origin',(-5.059780577,-1.77635683940025E-14,-9.219891447));
#152164=CARTESIAN_POINT('Origin',(-5.291727203,-1.77635683940025E-14,-9.095075645));
#152165=CARTESIAN_POINT('Origin',(-5.721323758,-1.77635683940025E-14,-8.824637796));
#152166=CARTESIAN_POINT('Origin',(-5.721323758,-1.77635683940025E-14,-8.824637796));
#152167=CARTESIAN_POINT('Origin',(-5.793599922,-1.77635683940025E-14,-8.776928718));
#152168=CARTESIAN_POINT('Origin',(-5.865876086,-1.77635683940025E-14,-8.72921964));
#152169=CARTESIAN_POINT('Origin',(-6.08570056,-1.77635683940025E-14,-8.584114775));
#152170=CARTESIAN_POINT('Origin',(-6.489325824,-1.77635683940025E-14,-8.276256891));
#152171=CARTESIAN_POINT('Origin',(-6.489325824,-1.77635683940025E-14,-8.276256891));
#152172=CARTESIAN_POINT('Origin',(-6.557034416,-1.77635683940025E-14,-8.222261091));
#152173=CARTESIAN_POINT('Origin',(-6.624743009,-1.77635683940025E-14,-8.16826529));
#152174=CARTESIAN_POINT('Origin',(-6.830675435,-1.77635683940025E-14,-8.00403966));
#152175=CARTESIAN_POINT('Origin',(-7.205079654,-1.77635683940025E-14,-7.661240432));
#152176=CARTESIAN_POINT('Origin',(-7.205079654,-1.77635683940025E-14,-7.661240432));
#152177=CARTESIAN_POINT('Origin',(-7.267675525,-1.77635683940025E-14,-7.601392651));
#152178=CARTESIAN_POINT('Origin',(-7.330271396,-1.77635683940025E-14,-7.54154487));
#152179=CARTESIAN_POINT('Origin',(-7.520653728,-1.77635683940025E-14,-7.359520724));
#152180=CARTESIAN_POINT('Origin',(-7.862822419,-1.77635683940025E-14,-6.98454017));
#152181=CARTESIAN_POINT('Origin',(-7.862822419,-1.77635683940025E-14,-6.98454017));
#152182=CARTESIAN_POINT('Origin',(-7.919801584,-1.77635683940025E-14,-6.919322268));
#152183=CARTESIAN_POINT('Origin',(-7.976780749,-1.77635683940025E-14,-6.854104366));
#152184=CARTESIAN_POINT('Origin',(-8.150080138,-1.77635683940025E-14,-6.655747255));
#152185=CARTESIAN_POINT('Origin',(-8.457258361,-1.77635683940025E-14,-6.251604497));
#152186=CARTESIAN_POINT('Origin',(-8.457258361,-1.77635683940025E-14,-6.251604497));
#152187=CARTESIAN_POINT('Origin',(-8.508162058,-1.77635683940025E-14,-6.18154157));
#152188=CARTESIAN_POINT('Origin',(-8.559065754,-1.77635683940025E-14,-6.111478643));
#152189=CARTESIAN_POINT('Origin',(-8.713886896,-1.77635683940025E-14,-5.898385622));
#152190=CARTESIAN_POINT('Origin',(-8.983601432,-1.77635683940025E-14,-5.46833458));
#152191=CARTESIAN_POINT('Origin',(-8.983601432,-1.77635683940025E-14,-5.46833458));
#152192=CARTESIAN_POINT('Origin',(-9.028019813,-1.77635683940025E-14,-5.393990734));
#152193=CARTESIAN_POINT('Origin',(-9.072438193,-1.77635683940025E-14,-5.319646888));
#152194=CARTESIAN_POINT('Origin',(-9.20753456,-1.77635683940025E-14,-5.093533656));
#152195=CARTESIAN_POINT('Origin',(-9.437613827,-1.77635683940025E-14,-4.641036849));
#152196=CARTESIAN_POINT('Origin',(-9.437613827,-1.77635683940025E-14,-4.641036849));
#152197=CARTESIAN_POINT('Origin',(-9.475189261,-1.77635683940025E-14,-4.563010656));
#152198=CARTESIAN_POINT('Origin',(-9.512764695,-1.77635683940025E-14,-4.484984463));
#152199=CARTESIAN_POINT('Origin',(-9.627048569,-1.77635683940025E-14,-4.247671553));
#152200=CARTESIAN_POINT('Origin',(-9.815640104,-1.77635683940025E-14,-3.776372218));
#152201=CARTESIAN_POINT('Origin',(-9.815640104,-1.77635683940025E-14,-3.776372218));
#152202=CARTESIAN_POINT('Origin',(-9.846070056,-1.77635683940025E-14,-3.6952919));
#152203=CARTESIAN_POINT('Origin',(-9.876500008,-1.77635683940025E-14,-3.614211582));
#152204=CARTESIAN_POINT('Origin',(-9.969051245,-1.77635683940025E-14,-3.367609695));
#152205=CARTESIAN_POINT('Origin',(-10.114636618,-1.77635683940025E-14,-2.881302458));
#152206=CARTESIAN_POINT('Origin',(-10.114636618,-1.77635683940025E-14,-2.881302458));
#152207=CARTESIAN_POINT('Origin',(-10.137676085,-1.77635683940025E-14,-2.797820826));
#152208=CARTESIAN_POINT('Origin',(-10.160715552,-1.77635683940025E-14,-2.714339193));
#152209=CARTESIAN_POINT('Origin',(-10.230788981,-1.77635683940025E-14,-2.460433825));
#152210=CARTESIAN_POINT('Origin',(-10.332196026,-1.77635683940025E-14,-1.963034146));
#152211=CARTESIAN_POINT('Origin',(-10.332196026,-1.77635683940025E-14,-1.963034146));
#152212=CARTESIAN_POINT('Origin',(-10.347659507,-1.77635683940025E-14,-1.877823344));
#152213=CARTESIAN_POINT('Origin',(-10.363122988,-1.77635683940025E-14,-1.792612542));
#152214=CARTESIAN_POINT('Origin',(-10.41015442,-1.77635683940025E-14,-1.533447988));
#152215=CARTESIAN_POINT('Origin',(-10.466566667,-1.77635683940025E-14,-1.028960636));
#152216=CARTESIAN_POINT('Origin',(-10.466566667,-1.77635683940025E-14,-1.028960636));
#152217=CARTESIAN_POINT('Origin',(-10.474329659,-1.77635683940025E-14,-0.942706732));
#152218=CARTESIAN_POINT('Origin',(-10.482092651,-1.77635683940025E-14,-0.856452827999998));
#152219=CARTESIAN_POINT('Origin',(-10.505703417,-1.77635683940025E-14,-0.594115729));
#152220=CARTESIAN_POINT('Origin',(-10.516666667,-1.77635683940025E-14,-0.0866025400000003));
#152221=CARTESIAN_POINT('Origin',(-10.516666667,-1.77635683940025E-14,-0.0866025400000003));
#152222=CARTESIAN_POINT('Origin',(-10.516666667,-1.77635683940025E-14,2.22044604925031E-15));
#152223=CARTESIAN_POINT('Origin',(-10.516666667,-1.77635683940025E-14,0.0866025400000026));
#152224=CARTESIAN_POINT('Origin',(-10.516666667,-1.77635683940025E-14,0.349999999999999));
#152225=CARTESIAN_POINT('Origin',(-10.48209265,-1.77635683940025E-14,0.856452828000001));
#152226=CARTESIAN_POINT('Origin',(-10.48209265,-1.77635683940025E-14,0.856452828000001));
#152227=CARTESIAN_POINT('Origin',(-10.474329659,-1.77635683940025E-14,0.942706731999998));
#152228=CARTESIAN_POINT('Origin',(-10.466566667,-1.77635683940025E-14,1.028960636));
#152229=CARTESIAN_POINT('Origin',(-10.4429559,-1.77635683940025E-14,1.291297735));
#152230=CARTESIAN_POINT('Origin',(-10.363122987,-1.77635683940025E-14,1.792612542));
#152231=CARTESIAN_POINT('Origin',(-10.363122987,-1.77635683940025E-14,1.792612542));
#152232=CARTESIAN_POINT('Origin',(-10.347659507,-1.77635683940025E-14,1.877823344));
#152233=CARTESIAN_POINT('Origin',(-10.332196026,-1.77635683940025E-14,1.963034146));
#152234=CARTESIAN_POINT('Origin',(-10.285164594,-1.77635683940025E-14,2.2221987));
#152235=CARTESIAN_POINT('Origin',(-10.160715552,-1.77635683940025E-14,2.714339193));
#152236=CARTESIAN_POINT('Origin',(-10.160715552,-1.77635683940025E-14,2.714339193));
#152237=CARTESIAN_POINT('Origin',(-10.137676085,-1.77635683940025E-14,2.797820826));
#152238=CARTESIAN_POINT('Origin',(-10.114636618,-1.77635683940025E-14,2.881302458));
#152239=CARTESIAN_POINT('Origin',(-10.044563189,-1.77635683940025E-14,3.135207827));
#152240=CARTESIAN_POINT('Origin',(-9.876500009,-1.77635683940025E-14,3.614211582));
#152241=CARTESIAN_POINT('Origin',(-9.876500009,-1.77635683940025E-14,3.614211582));
#152242=CARTESIAN_POINT('Origin',(-9.846070056,-1.77635683940025E-14,3.6952919));
#152243=CARTESIAN_POINT('Origin',(-9.815640104,-1.77635683940025E-14,3.776372218));
#152244=CARTESIAN_POINT('Origin',(-9.723088868,-1.77635683940025E-14,4.022974105));
#152245=CARTESIAN_POINT('Origin',(-9.512764695,-1.77635683940025E-14,4.484984464));
#152246=CARTESIAN_POINT('Origin',(-9.512764695,-1.77635683940025E-14,4.484984464));
#152247=CARTESIAN_POINT('Origin',(-9.475189261,-1.77635683940025E-14,4.563010656));
#152248=CARTESIAN_POINT('Origin',(-9.437613827,-1.77635683940025E-14,4.641036849));
#152249=CARTESIAN_POINT('Origin',(-9.323329952,-1.77635683940025E-14,4.87834976));
#152250=CARTESIAN_POINT('Origin',(-9.072438193,-1.77635683940025E-14,5.319646888));
#152251=CARTESIAN_POINT('Origin',(-9.072438193,-1.77635683940025E-14,5.319646888));
#152252=CARTESIAN_POINT('Origin',(-9.028019813,-1.77635683940025E-14,5.393990734));
#152253=CARTESIAN_POINT('Origin',(-8.983601433,-1.77635683940025E-14,5.46833458));
#152254=CARTESIAN_POINT('Origin',(-8.848505066,-1.77635683940025E-14,5.694447812));
#152255=CARTESIAN_POINT('Origin',(-8.559065754,-1.77635683940025E-14,6.111478643));
#152256=CARTESIAN_POINT('Origin',(-8.559065754,-1.77635683940025E-14,6.111478643));
#152257=CARTESIAN_POINT('Origin',(-8.508162058,-1.77635683940025E-14,6.18154157));
#152258=CARTESIAN_POINT('Origin',(-8.457258362,-1.77635683940025E-14,6.251604497));
#152259=CARTESIAN_POINT('Origin',(-8.302437219,-1.77635683940025E-14,6.464697518));
#152260=CARTESIAN_POINT('Origin',(-7.976780749,-1.77635683940025E-14,6.854104366));
#152261=CARTESIAN_POINT('Origin',(-7.976780749,-1.77635683940025E-14,6.854104366));
#152262=CARTESIAN_POINT('Origin',(-7.919801584,-1.77635683940025E-14,6.919322268));
#152263=CARTESIAN_POINT('Origin',(-7.862822419,-1.77635683940025E-14,6.98454017));
#152264=CARTESIAN_POINT('Origin',(-7.68952303,-1.77635683940025E-14,7.182897281));
#152265=CARTESIAN_POINT('Origin',(-7.330271397,-1.77635683940025E-14,7.54154487));
#152266=CARTESIAN_POINT('Origin',(-7.330271397,-1.77635683940025E-14,7.54154487));
#152267=CARTESIAN_POINT('Origin',(-7.267675525,-1.77635683940025E-14,7.601392651));
#152268=CARTESIAN_POINT('Origin',(-7.205079654,-1.77635683940025E-14,7.661240432));
#152269=CARTESIAN_POINT('Origin',(-7.014697323,-1.77635683940025E-14,7.843264578));
#152270=CARTESIAN_POINT('Origin',(-6.624743009,-1.77635683940025E-14,8.16826529));
#152271=CARTESIAN_POINT('Origin',(-6.624743009,-1.77635683940025E-14,8.16826529));
#152272=CARTESIAN_POINT('Origin',(-6.557034416,-1.77635683940025E-14,8.222261091));
#152273=CARTESIAN_POINT('Origin',(-6.489325824,-1.77635683940025E-14,8.276256891));
#152274=CARTESIAN_POINT('Origin',(-6.283393397,-1.77635683940025E-14,8.440482521));
#152275=CARTESIAN_POINT('Origin',(-5.865876086,-1.77635683940025E-14,8.72921964));
#152276=CARTESIAN_POINT('Origin',(-5.865876086,-1.77635683940025E-14,8.72921964));
#152277=CARTESIAN_POINT('Origin',(-5.793599922,-1.77635683940025E-14,8.776928718));
#152278=CARTESIAN_POINT('Origin',(-5.721323758,-1.77635683940025E-14,8.824637796));
#152279=CARTESIAN_POINT('Origin',(-5.501499283,-1.77635683940025E-14,8.969742662));
#152280=CARTESIAN_POINT('Origin',(-5.059780577,-1.77635683940025E-14,9.219891447));
#152281=CARTESIAN_POINT('Origin',(-5.059780577,-1.77635683940025E-14,9.219891447));
#152282=CARTESIAN_POINT('Origin',(-4.983518767,-1.77635683940025E-14,9.260929677));
#152283=CARTESIAN_POINT('Origin',(-4.907256957,-1.77635683940025E-14,9.301967907));
#152284=CARTESIAN_POINT('Origin',(-4.675310331,-1.77635683940025E-14,9.426783709));
#152285=CARTESIAN_POINT('Origin',(-4.212946691,-1.77635683940025E-14,9.636330108));
#152286=CARTESIAN_POINT('Origin',(-4.212946691,-1.77635683940025E-14,9.636330108));
#152287=CARTESIAN_POINT('Origin',(-4.13331325,-1.77635683940025E-14,9.670367075));
#152288=CARTESIAN_POINT('Origin',(-4.053679809,-1.77635683940025E-14,9.704404041));
#152289=CARTESIAN_POINT('Origin',(-3.811478529,-1.77635683940025E-14,9.807925836));
#152290=CARTESIAN_POINT('Origin',(-3.332192635,-1.77635683940025E-14,9.975182706));
#152291=CARTESIAN_POINT('Origin',(-3.332192635,-1.77635683940025E-14,9.975182706));
#152292=CARTESIAN_POINT('Origin',(-3.249828724,-1.77635683940025E-14,10.001944363));
#152293=CARTESIAN_POINT('Origin',(-3.167464814,-1.77635683940025E-14,10.02870602));
#152294=CARTESIAN_POINT('Origin',(-2.916958943,-1.77635683940025E-14,10.110100311));
#152295=CARTESIAN_POINT('Origin',(-2.424609723,-1.77635683940025E-14,10.233720998));
#152296=CARTESIAN_POINT('Origin',(-2.424609723,-1.77635683940025E-14,10.233720998));
#152297=CARTESIAN_POINT('Origin',(-2.340178489,-1.77635683940025E-14,10.252991876));
#152298=CARTESIAN_POINT('Origin',(-2.255747255,-1.77635683940025E-14,10.272262754));
#152299=CARTESIAN_POINT('Origin',(-1.99895372,-1.77635683940025E-14,10.330874203));
#152300=CARTESIAN_POINT('Origin',(-1.497505279,-1.77635683940025E-14,10.409863386));
#152301=CARTESIAN_POINT('Origin',(-1.497505279,-1.77635683940025E-14,10.409863386));
#152302=CARTESIAN_POINT('Origin',(-1.411686512,-1.77635683940025E-14,10.421488328));
#152303=CARTESIAN_POINT('Origin',(-1.325867745,-1.77635683940025E-14,10.43311327));
#152304=CARTESIAN_POINT('Origin',(-1.064854096,-1.77635683940025E-14,10.468469971));
#152305=CARTESIAN_POINT('Origin',(-0.558343802999999,-1.77635683940025E-14,
10.502191675));
#152306=CARTESIAN_POINT('Origin',(-0.558343802999999,-1.77635683940025E-14,
10.502191675));
#152307=CARTESIAN_POINT('Origin',(-0.471828465999998,-1.77635683940025E-14,
10.506077083));
#152308=CARTESIAN_POINT('Origin',(-0.385313128999999,-1.77635683940025E-14,
10.509962491));
#152309=CARTESIAN_POINT('Origin',(-0.122180893,-1.77635683940025E-14,10.521779774));
#152310=CARTESIAN_POINT('Origin',(0.385313128000001,-1.77635683940025E-14,
10.509962491));
#152311=CARTESIAN_POINT('Origin',(0.385313128000001,-1.77635683940025E-14,
10.509962491));
#152312=CARTESIAN_POINT('Origin',(0.471828466000001,-1.77635683940025E-14,
10.506077083));
#152313=CARTESIAN_POINT('Origin',(0.558343803000001,-1.77635683940025E-14,
10.502191675));
#152314=CARTESIAN_POINT('Origin',(0.821476039000001,-1.77635683940025E-14,
10.490374393));
#152315=CARTESIAN_POINT('Origin',(1.325867745,-1.77635683940025E-14,10.43311327));
#152316=CARTESIAN_POINT('Origin',(1.325867745,-1.77635683940025E-14,10.43311327));
#152317=CARTESIAN_POINT('Origin',(1.411686512,-1.77635683940025E-14,10.421488328));
#152318=CARTESIAN_POINT('Origin',(1.497505279,-1.77635683940025E-14,10.409863386));
#152319=CARTESIAN_POINT('Origin',(1.758518929,-1.77635683940025E-14,10.374506685));
#152320=CARTESIAN_POINT('Origin',(2.255747255,-1.77635683940025E-14,10.272262755));
#152321=CARTESIAN_POINT('Origin',(2.255747255,-1.77635683940025E-14,10.272262755));
#152322=CARTESIAN_POINT('Origin',(2.340178489,-1.77635683940025E-14,10.252991876));
#152323=CARTESIAN_POINT('Origin',(2.424609723,-1.77635683940025E-14,10.233720998));
#152324=CARTESIAN_POINT('Origin',(2.681403258,-1.77635683940025E-14,10.17510955));
#152325=CARTESIAN_POINT('Origin',(3.167464814,-1.77635683940025E-14,10.02870602));
#152326=CARTESIAN_POINT('Origin',(3.167464814,-1.77635683940025E-14,10.02870602));
#152327=CARTESIAN_POINT('Origin',(3.249828724,-1.77635683940025E-14,10.001944363));
#152328=CARTESIAN_POINT('Origin',(3.332192634,-1.77635683940025E-14,9.975182706));
#152329=CARTESIAN_POINT('Origin',(3.582698505,-1.77635683940025E-14,9.893788415));
#152330=CARTESIAN_POINT('Origin',(4.053679809,-1.77635683940025E-14,9.704404041));
#152331=CARTESIAN_POINT('Origin',(4.053679809,-1.77635683940025E-14,9.704404041));
#152332=CARTESIAN_POINT('Origin',(4.13331325,-1.77635683940025E-14,9.670367075));
#152333=CARTESIAN_POINT('Origin',(4.212946691,-1.77635683940025E-14,9.636330109));
#152334=CARTESIAN_POINT('Origin',(4.45514797,-1.77635683940025E-14,9.532808314));
#152335=CARTESIAN_POINT('Origin',(4.907256957,-1.77635683940025E-14,9.301967907));
#152336=CARTESIAN_POINT('Origin',(4.907256957,-1.77635683940025E-14,9.301967907));
#152337=CARTESIAN_POINT('Origin',(4.983518767,-1.77635683940025E-14,9.260929677));
#152338=CARTESIAN_POINT('Origin',(5.059780577,-1.77635683940025E-14,9.219891447));
#152339=CARTESIAN_POINT('Origin',(5.291727203,-1.77635683940025E-14,9.095075645));
#152340=CARTESIAN_POINT('Origin',(5.721323758,-1.77635683940025E-14,8.824637796));
#152341=CARTESIAN_POINT('Origin',(5.721323758,-1.77635683940025E-14,8.824637796));
#152342=CARTESIAN_POINT('Origin',(5.793599922,-1.77635683940025E-14,8.776928718));
#152343=CARTESIAN_POINT('Origin',(5.865876086,-1.77635683940025E-14,8.72921964));
#152344=CARTESIAN_POINT('Origin',(6.08570056,-1.77635683940025E-14,8.584114775));
#152345=CARTESIAN_POINT('Origin',(6.489325824,-1.77635683940025E-14,8.276256891));
#152346=CARTESIAN_POINT('Origin',(6.489325824,-1.77635683940025E-14,8.276256891));
#152347=CARTESIAN_POINT('Origin',(6.557034416,-1.77635683940025E-14,8.222261091));
#152348=CARTESIAN_POINT('Origin',(6.624743009,-1.77635683940025E-14,8.16826529));
#152349=CARTESIAN_POINT('Origin',(6.830675435,-1.77635683940025E-14,8.00403966));
#152350=CARTESIAN_POINT('Origin',(7.205079654,-1.77635683940025E-14,7.661240432));
#152351=CARTESIAN_POINT('Origin',(7.205079654,-1.77635683940025E-14,7.661240432));
#152352=CARTESIAN_POINT('Origin',(7.267675525,-1.77635683940025E-14,7.601392651));
#152353=CARTESIAN_POINT('Origin',(7.330271396,-1.77635683940025E-14,7.54154487));
#152354=CARTESIAN_POINT('Origin',(7.520653728,-1.77635683940025E-14,7.359520724));
#152355=CARTESIAN_POINT('Origin',(7.862822419,-1.77635683940025E-14,6.98454017));
#152356=CARTESIAN_POINT('Origin',(7.862822419,-1.77635683940025E-14,6.98454017));
#152357=CARTESIAN_POINT('Origin',(7.919801584,-1.77635683940025E-14,6.919322268));
#152358=CARTESIAN_POINT('Origin',(7.976780749,-1.77635683940025E-14,6.854104366));
#152359=CARTESIAN_POINT('Origin',(8.150080138,-1.77635683940025E-14,6.655747255));
#152360=CARTESIAN_POINT('Origin',(8.457258361,-1.77635683940025E-14,6.251604497));
#152361=CARTESIAN_POINT('Origin',(8.457258361,-1.77635683940025E-14,6.251604497));
#152362=CARTESIAN_POINT('Origin',(8.508162058,-1.77635683940025E-14,6.18154157));
#152363=CARTESIAN_POINT('Origin',(8.559065754,-1.77635683940025E-14,6.111478643));
#152364=CARTESIAN_POINT('Origin',(8.713886896,-1.77635683940025E-14,5.898385622));
#152365=CARTESIAN_POINT('Origin',(8.983601432,-1.77635683940025E-14,5.46833458));
#152366=CARTESIAN_POINT('Origin',(8.983601432,-1.77635683940025E-14,5.46833458));
#152367=CARTESIAN_POINT('Origin',(9.028019813,-1.77635683940025E-14,5.393990734));
#152368=CARTESIAN_POINT('Origin',(9.072438193,-1.77635683940025E-14,5.319646888));
#152369=CARTESIAN_POINT('Origin',(9.20753456,-1.77635683940025E-14,5.093533656));
#152370=CARTESIAN_POINT('Origin',(9.437613827,-1.77635683940025E-14,4.641036849));
#152371=CARTESIAN_POINT('Origin',(9.437613827,-1.77635683940025E-14,4.641036849));
#152372=CARTESIAN_POINT('Origin',(9.475189261,-1.77635683940025E-14,4.563010656));
#152373=CARTESIAN_POINT('Origin',(9.512764695,-1.77635683940025E-14,4.484984463));
#152374=CARTESIAN_POINT('Origin',(9.627048569,-1.77635683940025E-14,4.247671553));
#152375=CARTESIAN_POINT('Origin',(9.815640104,-1.77635683940025E-14,3.776372218));
#152376=CARTESIAN_POINT('Origin',(9.815640104,-1.77635683940025E-14,3.776372218));
#152377=CARTESIAN_POINT('Origin',(9.846070056,-1.77635683940025E-14,3.6952919));
#152378=CARTESIAN_POINT('Origin',(9.876500008,-1.77635683940025E-14,3.614211582));
#152379=CARTESIAN_POINT('Origin',(9.969051245,-1.77635683940025E-14,3.367609695));
#152380=CARTESIAN_POINT('Origin',(10.114636618,-1.77635683940025E-14,2.881302458));
#152381=CARTESIAN_POINT('Origin',(10.114636618,-1.77635683940025E-14,2.881302458));
#152382=CARTESIAN_POINT('Origin',(10.137676085,-1.77635683940025E-14,2.797820826));
#152383=CARTESIAN_POINT('Origin',(10.160715552,-1.77635683940025E-14,2.714339193));
#152384=CARTESIAN_POINT('Origin',(10.230788981,-1.77635683940025E-14,2.460433825));
#152385=CARTESIAN_POINT('Origin',(10.332196026,-1.77635683940025E-14,1.963034146));
#152386=CARTESIAN_POINT('Origin',(10.332196026,-1.77635683940025E-14,1.963034146));
#152387=CARTESIAN_POINT('Origin',(10.347659507,-1.77635683940025E-14,1.877823344));
#152388=CARTESIAN_POINT('Origin',(10.363122988,-1.77635683940025E-14,1.792612542));
#152389=CARTESIAN_POINT('Origin',(10.41015442,-1.77635683940025E-14,1.533447988));
#152390=CARTESIAN_POINT('Origin',(10.466566667,-1.77635683940025E-14,1.028960636));
#152391=CARTESIAN_POINT('Origin',(10.466566667,-1.77635683940025E-14,1.028960636));
#152392=CARTESIAN_POINT('Origin',(10.474329659,-1.77635683940025E-14,0.942706731999998));
#152393=CARTESIAN_POINT('Origin',(10.482092651,-1.77635683940025E-14,0.856452828000001));
#152394=CARTESIAN_POINT('Origin',(10.505703417,-1.77635683940025E-14,0.594115729));
#152395=CARTESIAN_POINT('Origin',(-6.,4.49999999999998,2.22044604925031E-15));
#152396=CARTESIAN_POINT('',(-7.,4.49999999999998,2.34291072916505E-15));
#152397=CARTESIAN_POINT('Origin',(-6.,4.49999999999998,2.22044604925031E-15));
#152398=CARTESIAN_POINT('',(-7.,7.49999999999998,2.34291072916505E-15));
#152399=CARTESIAN_POINT('',(-7.,4.49999999999998,2.34291072916505E-15));
#152400=CARTESIAN_POINT('Origin',(-6.,7.49999999999998,2.22044604925031E-15));
#152401=CARTESIAN_POINT('Origin',(6.,4.49999999999998,2.22044604925031E-15));
#152402=CARTESIAN_POINT('',(5.,4.49999999999998,2.34291072916505E-15));
#152403=CARTESIAN_POINT('Origin',(6.,4.49999999999998,2.22044604925031E-15));
#152404=CARTESIAN_POINT('',(5.,7.49999999999998,2.34291072916505E-15));
#152405=CARTESIAN_POINT('',(5.,4.49999999999998,2.34291072916505E-15));
#152406=CARTESIAN_POINT('Origin',(6.,7.49999999999998,2.22044604925031E-15));
#152407=CARTESIAN_POINT('Origin',(-6.,2.39999999999998,2.22044604925031E-15));
#152408=CARTESIAN_POINT('',(-7.6,2.49999999999998,2.41638953711389E-15));
#152409=CARTESIAN_POINT('Origin',(-6.,2.49999999999998,2.22044604925031E-15));
#152410=CARTESIAN_POINT('',(-7.5,2.39999999999998,2.40414306912242E-15));
#152411=CARTESIAN_POINT('Origin',(-7.6,2.39999999999998,2.41638953711389E-15));
#152412=CARTESIAN_POINT('Origin',(-6.,2.39999999999998,2.22044604925031E-15));
#152413=CARTESIAN_POINT('Origin',(6.,2.39999999999998,2.22044604925031E-15));
#152414=CARTESIAN_POINT('',(4.4,2.49999999999998,2.41638953711389E-15));
#152415=CARTESIAN_POINT('Origin',(6.,2.49999999999998,2.22044604925031E-15));
#152416=CARTESIAN_POINT('',(4.5,2.39999999999998,2.40414306912242E-15));
#152417=CARTESIAN_POINT('Origin',(4.4,2.39999999999998,2.41638953711389E-15));
#152418=CARTESIAN_POINT('Origin',(6.,2.39999999999998,2.22044604925031E-15));
#152419=CARTESIAN_POINT('Origin',(2.22044604925031E-15,5.39999999999998,
2.22044604925031E-15));
#152420=CARTESIAN_POINT('',(1.5,5.39999999999998,2.40414306912242E-15));
#152421=CARTESIAN_POINT('',(-1.5,5.39999999999998,2.40414306912242E-15));
#152422=CARTESIAN_POINT('Origin',(2.22044604925031E-15,5.39999999999998,
2.22044604925031E-15));
#152423=CARTESIAN_POINT('',(1.7,5.19999999999998,2.42863600510536E-15));
#152424=CARTESIAN_POINT('Origin',(1.7,5.39999999999998,2.42863600510536E-15));
#152425=CARTESIAN_POINT('Origin',(2.22044604925031E-15,5.19999999999998,
2.22044604925031E-15));
#152426=CARTESIAN_POINT('Origin',(2.22044604925031E-15,5.39999999999998,
2.22044604925031E-15));
#152427=CARTESIAN_POINT('Origin',(2.22044604925031E-15,7.50005079999998,
2.22044604925031E-15));
#152428=CARTESIAN_POINT('',(-1.5,7.50005079999998,2.40414306912242E-15));
#152429=CARTESIAN_POINT('Origin',(2.22044604925031E-15,7.50005079999998,
2.22044604925031E-15));
#152430=CARTESIAN_POINT('',(-1.7,7.70005079999998,2.42863600510536E-15));
#152431=CARTESIAN_POINT('Origin',(-1.7,7.50005079999998,2.42863600510536E-15));
#152432=CARTESIAN_POINT('Origin',(2.22044604925031E-15,7.70005079999998,
2.22044604925031E-15));
#152433=CARTESIAN_POINT('Origin',(2.22044604925031E-15,7.50005079999998,
2.22044604925031E-15));
#152434=CARTESIAN_POINT('',(-2.8,7.70005079999998,2.56334715301157E-15));
#152435=CARTESIAN_POINT('Origin',(2.22044604925031E-15,7.70005079999998,
2.22044604925031E-15));
#152436=CARTESIAN_POINT('',(-3.,7.50005079999998,2.58784008899452E-15));
#152437=CARTESIAN_POINT('Origin',(-2.8,7.50005079999998,2.56334715301157E-15));
#152438=CARTESIAN_POINT('',(3.,7.50005079999998,2.58784008899452E-15));
#152439=CARTESIAN_POINT('Origin',(2.22044604925031E-15,7.50005079999998,
2.22044604925031E-15));
#152440=CARTESIAN_POINT('Origin',(2.22044604925031E-15,7.50005079999998,
2.22044604925031E-15));
#152441=CARTESIAN_POINT('Origin',(6.266666667,2.69999999999998,2.639865316));
#152442=CARTESIAN_POINT('',(6.4000000003749,2.69999999999998,2.26274169893964));
#152443=CARTESIAN_POINT('',(6.63529411786042,2.69999999999998,2.79515151133333));
#152444=CARTESIAN_POINT('Origin',(6.266666667,2.69999999999998,2.639865316));
#152445=CARTESIAN_POINT('',(6.466666667,2.49999999999998,2.074179891));
#152446=CARTESIAN_POINT('Origin',(6.466666667,2.69999999999998,2.074179891));
#152447=CARTESIAN_POINT('',(6.819607843,2.49999999999998,2.872794609));
#152448=CARTESIAN_POINT('Origin',(6.266666667,2.49999999999998,2.639865316));
#152449=CARTESIAN_POINT('Origin',(6.819607843,2.69999999999998,2.872794609));
#152450=CARTESIAN_POINT('Origin',(6.266666667,2.69999999999998,-2.639865316));
#152451=CARTESIAN_POINT('',(6.63529411787831,2.69999999999998,-2.79515151154086));
#152452=CARTESIAN_POINT('',(6.400000001,2.69999999999998,-2.262741699));
#152453=CARTESIAN_POINT('Origin',(6.266666667,2.69999999999998,-2.639865316));
#152454=CARTESIAN_POINT('',(6.819607843,2.49999999999998,-2.872794609));
#152455=CARTESIAN_POINT('Origin',(6.819607843,2.69999999999998,-2.87279461));
#152456=CARTESIAN_POINT('',(6.466666667,2.49999999999998,-2.07417989));
#152457=CARTESIAN_POINT('Origin',(6.266666667,2.49999999999998,-2.639865316));
#152458=CARTESIAN_POINT('Origin',(6.466666668,2.69999999999998,-2.074179889));
#152459=CARTESIAN_POINT('Origin',(2.22044604925031E-15,2.89999999999998,
2.22044604925031E-15));
#152460=CARTESIAN_POINT('',(-3.9,2.49999999999998,2.69805830091778E-15));
#152461=CARTESIAN_POINT('Origin',(2.22044604925031E-15,2.49999999999998,
2.22044604925031E-15));
#152462=CARTESIAN_POINT('',(-3.5,2.89999999999998,2.64907242895189E-15));
#152463=CARTESIAN_POINT('Origin',(-3.9,2.89999999999998,2.69805830091778E-15));
#152464=CARTESIAN_POINT('',(3.5,2.89999999999998,2.64907242895189E-15));
#152465=CARTESIAN_POINT('Origin',(2.22044604925031E-15,2.89999999999998,
2.22044604925031E-15));
#152466=CARTESIAN_POINT('Origin',(2.22044604925031E-15,2.89999999999998,
2.22044604925031E-15));
#152467=CARTESIAN_POINT('Origin',(-6.,-0.900000000000018,2.22044604925031E-15));
#152468=CARTESIAN_POINT('',(-4.9,-1.30000000000002,2.35515719715652E-15));
#152469=CARTESIAN_POINT('Origin',(-6.,-1.30000000000002,2.22044604925031E-15));
#152470=CARTESIAN_POINT('',(-4.5,-0.900000000000018,2.40414306912242E-15));
#152471=CARTESIAN_POINT('Origin',(-4.9,-0.900000000000018,2.35515719715652E-15));
#152472=CARTESIAN_POINT('',(-7.5,-0.900000000000018,2.40414306912242E-15));
#152473=CARTESIAN_POINT('Origin',(-6.,-0.900000000000018,2.22044604925031E-15));
#152474=CARTESIAN_POINT('Origin',(-6.,-0.900000000000018,2.22044604925031E-15));
#152475=CARTESIAN_POINT('Origin',(6.,-0.900000000000018,2.22044604925031E-15));
#152476=CARTESIAN_POINT('',(7.1,-1.30000000000002,2.35515719715652E-15));
#152477=CARTESIAN_POINT('Origin',(6.,-1.30000000000002,2.22044604925031E-15));
#152478=CARTESIAN_POINT('',(7.5,-0.900000000000018,2.40414306912242E-15));
#152479=CARTESIAN_POINT('Origin',(7.1,-0.900000000000018,2.35515719715652E-15));
#152480=CARTESIAN_POINT('',(4.5,-0.900000000000018,2.40414306912242E-15));
#152481=CARTESIAN_POINT('Origin',(6.,-0.900000000000018,2.22044604925031E-15));
#152482=CARTESIAN_POINT('Origin',(6.,-0.900000000000018,2.22044604925031E-15));
#152483=CARTESIAN_POINT('Origin',(-6.266666667,4.99999999999998,2.639865316));
#152484=CARTESIAN_POINT('',(-6.6352941178783,2.69999999999998,2.79515151154086));
#152485=CARTESIAN_POINT('',(-6.40000000011872,2.69999999999998,2.2627416986642));
#152486=CARTESIAN_POINT('Origin',(-6.266666667,2.69999999999998,2.639865316));
#152487=CARTESIAN_POINT('',(-6.4,4.99999999999998,2.262741699));
#152488=CARTESIAN_POINT('',(-6.4,4.99999999999998,2.262741699));
#152489=CARTESIAN_POINT('',(-6.63529411796584,4.99999999999998,2.79515151131895));
#152490=CARTESIAN_POINT('Origin',(-6.266666667,4.99999999999998,2.639865316));
#152491=CARTESIAN_POINT('',(-6.635294118,4.99999999999998,2.795151512));
#152492=CARTESIAN_POINT('Origin',(-6.266666667,4.99999999999998,-2.639865316));
#152493=CARTESIAN_POINT('',(-6.40000000060197,2.70000000049998,-2.26274169880154));
#152494=CARTESIAN_POINT('',(-6.63529411786042,2.69999999999998,-2.79515151133332));
#152495=CARTESIAN_POINT('Origin',(-6.266666667,2.69999999999998,-2.639865316));
#152496=CARTESIAN_POINT('',(-6.63529411796585,4.99999999999998,-2.79515151131894));
#152497=CARTESIAN_POINT('',(-6.635294118,4.99999999999998,-2.795151512));
#152498=CARTESIAN_POINT('',(-6.4,4.99999999999998,-2.262741699));
#152499=CARTESIAN_POINT('Origin',(-6.266666667,4.99999999999998,-2.639865316));
#152500=CARTESIAN_POINT('',(-6.4,4.99999999999998,-2.262741699));
#152501=CARTESIAN_POINT('Origin',(2.22044604925031E-15,5.19999999999998,
2.22044604925031E-15));
#152502=CARTESIAN_POINT('',(3.5,5.19999999999998,2.64907242895189E-15));
#152503=CARTESIAN_POINT('Origin',(2.22044604925031E-15,5.19999999999998,
2.22044604925031E-15));
#152504=CARTESIAN_POINT('',(3.5,5.19999999999998,2.64907242895189E-15));
#152505=CARTESIAN_POINT('Origin',(-6.,-1.30000000000002,2.22044604925031E-15));
#152506=CARTESIAN_POINT('',(-7.5,-1.30000000000002,2.40414306912242E-15));
#152507=CARTESIAN_POINT('Origin',(6.,-1.30000000000002,2.22044604925031E-15));
#152508=CARTESIAN_POINT('',(4.5,-1.30000000000002,2.40414306912242E-15));
#152509=CARTESIAN_POINT('Origin',(2.22044604925031E-15,7.70005079999998,
2.22044604925031E-15));
#152510=CARTESIAN_POINT('',(3.,7.49999999999998,2.58784008899452E-15));
#152511=CARTESIAN_POINT('Origin',(2.22044604925031E-15,7.49999999999998,
2.22044604925031E-15));
#152512=CARTESIAN_POINT('',(3.,7.70005079999998,2.58784008899452E-15));
#152513=CARTESIAN_POINT('Origin',(-1.016576292,2.49999999999998,-8.632506096));
#152514=CARTESIAN_POINT('',(2.65852674,2.49999999999998,-8.20399973));
#152515=CARTESIAN_POINT('',(2.60381795543899,2.49999999999998,-9.3958837827716));
#152516=CARTESIAN_POINT('Origin',(-1.016576292,2.49999999999998,-8.632506096));
#152517=CARTESIAN_POINT('',(2.60381795543899,7.49999999999998,-9.3958837827716));
#152518=CARTESIAN_POINT('',(2.603817955,2.49999999999998,-9.395883783));
#152519=CARTESIAN_POINT('',(2.65852674,7.49999999999998,-8.20399973));
#152520=CARTESIAN_POINT('Origin',(-1.016576292,7.49999999999998,-8.632506096));
#152521=CARTESIAN_POINT('',(2.65852674,2.49999999999998,-8.20399973));
#152522=CARTESIAN_POINT('Origin',(0.456946844000001,2.49999999999998,-8.680137582));
#152523=CARTESIAN_POINT('',(4.006768937,2.49999999999998,-7.636699463));
#152524=CARTESIAN_POINT('',(4.154276471,2.49999999999998,-8.820685177));
#152525=CARTESIAN_POINT('Origin',(0.456946844000001,2.49999999999998,-8.680137582));
#152526=CARTESIAN_POINT('',(4.154276471,7.49999999999998,-8.820685177));
#152527=CARTESIAN_POINT('',(4.154276471,2.49999999999998,-8.820685177));
#152528=CARTESIAN_POINT('',(4.006768937,7.49999999999998,-7.636699463));
#152529=CARTESIAN_POINT('Origin',(0.456946844000001,7.49999999999998,-8.680137582));
#152530=CARTESIAN_POINT('',(4.006768937,2.49999999999998,-7.636699463));
#152531=CARTESIAN_POINT('Origin',(-0.280826403999999,2.49999999999998,8.687619086));
#152532=CARTESIAN_POINT('',(3.391264282,2.49999999999998,9.141215815));
#152533=CARTESIAN_POINT('',(3.34469714851111,2.49999999999998,7.94898590903151));
#152534=CARTESIAN_POINT('Origin',(-0.280826403999999,2.49999999999998,8.687619086));
#152535=CARTESIAN_POINT('',(3.34469714851111,7.49999999999998,7.94898590903151));
#152536=CARTESIAN_POINT('',(3.344697148,2.49999999999998,7.948985909));
#152537=CARTESIAN_POINT('',(3.391264282,7.49999999999998,9.141215815));
#152538=CARTESIAN_POINT('Origin',(-0.280826403999999,7.49999999999998,8.687619086));
#152539=CARTESIAN_POINT('',(3.391264282,7.49999999999998,9.141215815));
#152540=CARTESIAN_POINT('Origin',(-1.745001724,2.49999999999998,8.515195702));
#152541=CARTESIAN_POINT('',(1.797611062,2.49999999999998,9.582854192));
#152542=CARTESIAN_POINT('',(1.953201586,2.49999999999998,8.399903545));
#152543=CARTESIAN_POINT('Origin',(-1.745001724,2.49999999999998,8.515195702));
#152544=CARTESIAN_POINT('',(1.953201586,7.49999999999998,8.399903545));
#152545=CARTESIAN_POINT('',(1.953201586,2.49999999999998,8.399903545));
#152546=CARTESIAN_POINT('',(1.797611062,7.49999999999998,9.582854192));
#152547=CARTESIAN_POINT('Origin',(-1.745001724,7.49999999999998,8.515195702));
#152548=CARTESIAN_POINT('',(1.797611062,7.49999999999998,9.582854192));
#152549=CARTESIAN_POINT('Origin',(2.22044604925031E-15,2.29994919999998,
2.22044604925031E-15));
#152550=CARTESIAN_POINT('',(-1.5,2.29994919999998,2.40414306912242E-15));
#152551=CARTESIAN_POINT('Origin',(2.22044604925031E-15,2.49999999999998,
2.22044604925031E-15));
#152552=CARTESIAN_POINT('',(8.603650246,2.49999999999998,-0.592096652999998));
#152553=CARTESIAN_POINT('',(9.689187855,2.49999999999998,-1.087262023));
#152554=CARTESIAN_POINT('Origin',(7.630970629,2.49999999999998,-4.161955804));
#152555=CARTESIAN_POINT('',(8.622868801,2.49999999999998,-0.139676895));
#152556=CARTESIAN_POINT('Origin',(2.22044604925031E-15,2.49999999999998,
2.22044604925031E-15));
#152557=CARTESIAN_POINT('',(9.746488706,2.49999999999998,0.261644615999999));
#152558=CARTESIAN_POINT('Origin',(7.956438479,2.49999999999998,3.499810792));
#152559=CARTESIAN_POINT('',(9.733565882,2.49999999999998,0.565857946999999));
#152560=CARTESIAN_POINT('Origin',(2.22044604925031E-15,2.49999999999998,
2.22044604925031E-15));
#152561=CARTESIAN_POINT('',(8.579959389,2.49999999999998,0.870444068000003));
#152562=CARTESIAN_POINT('Origin',(8.224580008,2.49999999999998,-2.812449563));
#152563=CARTESIAN_POINT('',(8.522442193,2.49999999999998,1.31960413));
#152564=CARTESIAN_POINT('Origin',(2.22044604925031E-15,2.49999999999998,
2.22044604925031E-15));
#152565=CARTESIAN_POINT('',(9.562076184,2.49999999999998,1.905045682));
#152566=CARTESIAN_POINT('Origin',(7.25052146,2.49999999999998,4.794113829));
#152567=CARTESIAN_POINT('',(9.497926941,2.49999999999998,2.202699214));
#152568=CARTESIAN_POINT('Origin',(2.22044604925031E-15,2.49999999999998,
2.22044604925031E-15));
#152569=CARTESIAN_POINT('',(8.309438723,2.49999999999998,2.307943698));
#152570=CARTESIAN_POINT('Origin',(8.581583195,2.49999999999998,-1.382034268));
#152571=CARTESIAN_POINT('',(8.17684044,2.49999999999998,2.740922548));
#152572=CARTESIAN_POINT('Origin',(2.22044604925031E-15,2.49999999999998,
2.22044604925031E-15));
#152573=CARTESIAN_POINT('',(9.10258013994849,2.49999999999998,3.49364205338694));
#152574=CARTESIAN_POINT('Origin',(6.33602014,2.49999999999998,5.950498941));
#152575=CARTESIAN_POINT('',(8.989049934,2.49999999999998,3.776172836));
#152576=CARTESIAN_POINT('Origin',(2.22044604925031E-15,2.49999999999998,
2.22044604925031E-15));
#152577=CARTESIAN_POINT('',(7.799870633,2.49999999999998,3.679047989));
#152578=CARTESIAN_POINT('Origin',(8.691709858,2.49999999999998,0.088139637000002));
#152579=CARTESIAN_POINT('',(7.596005875,2.49999999999998,4.083389615));
#152580=CARTESIAN_POINT('Origin',(2.22044604925031E-15,2.49999999999998,
2.22044604925031E-15));
#152581=CARTESIAN_POINT('',(8.381219438,2.49999999999998,4.981732704));
#152582=CARTESIAN_POINT('Origin',(5.239243055,2.49999999999998,6.935699032));
#152583=CARTESIAN_POINT('',(8.221574327,2.49999999999998,5.24101284));
#152584=CARTESIAN_POINT('Origin',(2.22044604925031E-15,2.49999999999998,
2.22044604925031E-15));
#152585=CARTESIAN_POINT('',(7.065914466,2.49999999999998,4.944312769));
#152586=CARTESIAN_POINT('Origin',(8.551791853,2.49999999999998,1.555777924));
#152587=CARTESIAN_POINT('',(6.796648051,2.49999999999998,5.308384996));
#152588=CARTESIAN_POINT('Origin',(2.22044604925031E-15,2.49999999999998,
2.22044604925031E-15));
#152589=CARTESIAN_POINT('',(7.418746313,2.49999999999998,6.326507974));
#152590=CARTESIAN_POINT('Origin',(3.991742488,2.49999999999998,7.721371689));
#152591=CARTESIAN_POINT('',(7.217578995,2.49999999999998,6.555078448));
#152592=CARTESIAN_POINT('Origin',(2.22044604925031E-15,2.49999999999998,
2.22044604925031E-15));
#152593=CARTESIAN_POINT('',(6.128684805,2.49999999999998,6.067338672));
#152594=CARTESIAN_POINT('Origin',(8.165854367,2.49999999999998,2.978659314));
#152595=CARTESIAN_POINT('',(5.801763037,2.49999999999998,6.380667807));
#152596=CARTESIAN_POINT('Origin',(2.22044604925031E-15,2.49999999999998,
2.22044604925031E-15));
#152597=CARTESIAN_POINT('',(6.242849363,2.49999999999998,7.489281129));
#152598=CARTESIAN_POINT('Origin',(2.629406756,2.49999999999998,8.284914542));
#152599=CARTESIAN_POINT('',(6.005947057,2.49999999999998,7.680566382));
#152600=CARTESIAN_POINT('Origin',(2.22044604925031E-15,2.49999999999998,
2.22044604925031E-15));
#152601=CARTESIAN_POINT('',(5.015144041,2.49999999999998,7.015818288));
#152602=CARTESIAN_POINT('Origin',(7.545000119,2.49999999999998,4.315850098));
#152603=CARTESIAN_POINT('',(4.639971864,2.49999999999998,7.269390422));
#152604=CARTESIAN_POINT('Origin',(2.22044604925031E-15,2.49999999999998,
2.22044604925031E-15));
#152605=CARTESIAN_POINT('',(4.887357004,2.49999999999998,8.436601301));
#152606=CARTESIAN_POINT('Origin',(1.19142778,2.49999999999998,8.610115487));
#152607=CARTESIAN_POINT('',(4.621534957,2.49999999999998,8.585098406));
#152608=CARTESIAN_POINT('Origin',(2.22044604925031E-15,2.49999999999998,
2.22044604925031E-15));
#152609=CARTESIAN_POINT('',(3.757326714,2.49999999999998,7.762465586));
#152610=CARTESIAN_POINT('Origin',(6.707089953,2.49999999999998,5.528881732));
#152611=CARTESIAN_POINT('Origin',(2.22044604925031E-15,2.49999999999998,
2.22044604925031E-15));
#152612=CARTESIAN_POINT('',(3.104169711,2.49999999999998,9.24265278));
#152613=CARTESIAN_POINT('Origin',(2.22044604925031E-15,2.49999999999998,
2.22044604925031E-15));
#152614=CARTESIAN_POINT('',(2.391417938,2.49999999999998,8.285800881));
#152615=CARTESIAN_POINT('Origin',(5.676229022,2.49999999999998,6.582857506));
#152616=CARTESIAN_POINT('Origin',(2.22044604925031E-15,2.49999999999998,
2.22044604925031E-15));
#152617=CARTESIAN_POINT('',(1.497503154,2.49999999999998,9.634312861));
#152618=CARTESIAN_POINT('Origin',(2.22044604925031E-15,2.49999999999998,
2.22044604925031E-15));
#152619=CARTESIAN_POINT('',(0.956712422000002,2.49999999999998,8.570768772));
#152620=CARTESIAN_POINT('Origin',(4.482073316,2.49999999999998,7.447456454));
#152621=CARTESIAN_POINT('',(0.505515969000001,2.49999999999998,8.60917125));
#152622=CARTESIAN_POINT('Origin',(2.22044604925031E-15,2.49999999999998,
2.22044604925031E-15));
#152623=CARTESIAN_POINT('',(0.152243842000002,2.49999999999998,9.748811303));
#152624=CARTESIAN_POINT('Origin',(-3.158976522,2.49999999999998,8.09780564));
#152625=CARTESIAN_POINT('',(-0.152243841999998,2.49999999999998,9.748811303));
#152626=CARTESIAN_POINT('Origin',(2.22044604925031E-15,2.49999999999998,
2.22044604925031E-15));
#152627=CARTESIAN_POINT('',(-0.505515968999999,2.49999999999998,8.60917125));
#152628=CARTESIAN_POINT('Origin',(3.158976522,2.49999999999998,8.09780564));
#152629=CARTESIAN_POINT('',(-0.956712421999999,2.49999999999998,8.570768772));
#152630=CARTESIAN_POINT('Origin',(2.22044604925031E-15,2.49999999999998,
2.22044604925031E-15));
#152631=CARTESIAN_POINT('',(-1.497503154,2.49999999999998,9.634312861));
#152632=CARTESIAN_POINT('Origin',(-4.482073316,2.49999999999998,7.447456454));
#152633=CARTESIAN_POINT('',(-1.797611062,2.49999999999998,9.582854192));
#152634=CARTESIAN_POINT('Origin',(2.22044604925031E-15,2.49999999999998,
2.22044604925031E-15));
#152635=CARTESIAN_POINT('',(-1.953201585,2.49999999999998,8.399903545));
#152636=CARTESIAN_POINT('Origin',(1.745001724,2.49999999999998,8.515195702));
#152637=CARTESIAN_POINT('',(-2.391417938,2.49999999999998,8.285800881));
#152638=CARTESIAN_POINT('Origin',(2.22044604925031E-15,2.49999999999998,
2.22044604925031E-15));
#152639=CARTESIAN_POINT('',(-3.104169711,2.49999999999998,9.24265278));
#152640=CARTESIAN_POINT('Origin',(-5.676229022,2.49999999999998,6.582857506));
#152641=CARTESIAN_POINT('',(-3.391264282,2.49999999999998,9.141215815));
#152642=CARTESIAN_POINT('Origin',(2.22044604925031E-15,2.49999999999998,
2.22044604925031E-15));
#152643=CARTESIAN_POINT('',(-3.344697148,2.49999999999998,7.948985909));
#152644=CARTESIAN_POINT('Origin',(0.280826404000001,2.49999999999998,8.687619086));
#152645=CARTESIAN_POINT('',(-3.757326714,2.49999999999998,7.762465586));
#152646=CARTESIAN_POINT('Origin',(2.22044604925031E-15,2.49999999999998,
2.22044604925031E-15));
#152647=CARTESIAN_POINT('',(-4.621534957,2.49999999999998,8.585098406));
#152648=CARTESIAN_POINT('Origin',(-6.707089953,2.49999999999998,5.528881732));
#152649=CARTESIAN_POINT('',(-4.887357004,2.49999999999998,8.436601301));
#152650=CARTESIAN_POINT('Origin',(2.22044604925031E-15,2.49999999999998,
2.22044604925031E-15));
#152651=CARTESIAN_POINT('',(-4.639971864,2.49999999999998,7.269390422));
#152652=CARTESIAN_POINT('Origin',(-1.19142778,2.49999999999998,8.610115487));
#152653=CARTESIAN_POINT('',(-5.015144041,2.49999999999998,7.015818288));
#152654=CARTESIAN_POINT('Origin',(2.22044604925031E-15,2.49999999999998,
2.22044604925031E-15));
#152655=CARTESIAN_POINT('',(-6.005947057,2.49999999999998,7.680566382));
#152656=CARTESIAN_POINT('Origin',(-7.545000119,2.49999999999998,4.315850098));
#152657=CARTESIAN_POINT('',(-6.242849363,2.49999999999998,7.489281129));
#152658=CARTESIAN_POINT('Origin',(2.22044604925031E-15,2.49999999999998,
2.22044604925031E-15));
#152659=CARTESIAN_POINT('',(-5.801763037,2.49999999999998,6.380667807));
#152660=CARTESIAN_POINT('Origin',(-2.629406756,2.49999999999998,8.284914542));
#152661=CARTESIAN_POINT('',(-6.128684805,2.49999999999998,6.067338672));
#152662=CARTESIAN_POINT('Origin',(2.22044604925031E-15,2.49999999999998,
2.22044604925031E-15));
#152663=CARTESIAN_POINT('',(-7.217578995,2.49999999999998,6.555078448));
#152664=CARTESIAN_POINT('Origin',(-8.165854367,2.49999999999998,2.978659314));
#152665=CARTESIAN_POINT('',(-7.418746313,2.49999999999998,6.326507974));
#152666=CARTESIAN_POINT('Origin',(2.22044604925031E-15,2.49999999999998,
2.22044604925031E-15));
#152667=CARTESIAN_POINT('',(-6.796648051,2.49999999999998,5.308384996));
#152668=CARTESIAN_POINT('Origin',(-3.991742488,2.49999999999998,7.721371689));
#152669=CARTESIAN_POINT('',(-7.065914466,2.49999999999998,4.944312768));
#152670=CARTESIAN_POINT('Origin',(2.22044604925031E-15,2.49999999999998,
2.22044604925031E-15));
#152671=CARTESIAN_POINT('',(-8.221574327,2.49999999999998,5.24101284));
#152672=CARTESIAN_POINT('Origin',(-8.551791853,2.49999999999998,1.555777924));
#152673=CARTESIAN_POINT('',(-8.381219438,2.49999999999998,4.981732704));
#152674=CARTESIAN_POINT('Origin',(2.22044604925031E-15,2.49999999999998,
2.22044604925031E-15));
#152675=CARTESIAN_POINT('',(-7.596005875,2.49999999999998,4.083389615));
#152676=CARTESIAN_POINT('Origin',(-5.239243055,2.49999999999998,6.935699032));
#152677=CARTESIAN_POINT('',(-7.799870633,2.49999999999998,3.67904799));
#152678=CARTESIAN_POINT('Origin',(2.22044604925031E-15,2.49999999999998,
2.22044604925031E-15));
#152679=CARTESIAN_POINT('',(-8.989049934,2.49999999999998,3.776172836));
#152680=CARTESIAN_POINT('Origin',(-8.691709858,2.49999999999998,0.088139637000002));
#152681=CARTESIAN_POINT('',(-9.10258013994848,2.49999999999998,3.49364205338694));
#152682=CARTESIAN_POINT('Origin',(2.22044604925031E-15,2.49999999999998,
2.22044604925031E-15));
#152683=CARTESIAN_POINT('',(-8.17684044,2.49999999999998,2.740922548));
#152684=CARTESIAN_POINT('Origin',(-6.33602014,2.49999999999998,5.950498941));
#152685=CARTESIAN_POINT('',(-8.309438723,2.49999999999998,2.307943698));
#152686=CARTESIAN_POINT('Origin',(2.22044604925031E-15,2.49999999999998,
2.22044604925031E-15));
#152687=CARTESIAN_POINT('',(-9.497926941,2.49999999999998,2.202699214));
#152688=CARTESIAN_POINT('Origin',(-8.581583195,2.49999999999998,-1.382034268));
#152689=CARTESIAN_POINT('',(-9.562076184,2.49999999999998,1.905045682));
#152690=CARTESIAN_POINT('Origin',(2.22044604925031E-15,2.49999999999998,
2.22044604925031E-15));
#152691=CARTESIAN_POINT('',(-8.522442193,2.49999999999998,1.31960413));
#152692=CARTESIAN_POINT('Origin',(-7.25052146,2.49999999999998,4.794113829));
#152693=CARTESIAN_POINT('',(-8.579959389,2.49999999999998,0.870444068000003));
#152694=CARTESIAN_POINT('Origin',(2.22044604925031E-15,2.49999999999998,
2.22044604925031E-15));
#152695=CARTESIAN_POINT('',(-9.733565882,2.49999999999998,0.565857946999999));
#152696=CARTESIAN_POINT('Origin',(-8.224580008,2.49999999999998,-2.812449563));
#152697=CARTESIAN_POINT('',(-9.746488706,2.49999999999998,0.261644615999999));
#152698=CARTESIAN_POINT('Origin',(2.22044604925031E-15,2.49999999999998,
2.22044604925031E-15));
#152699=CARTESIAN_POINT('',(-8.622868801,2.49999999999998,-0.139676895));
#152700=CARTESIAN_POINT('Origin',(-7.956438479,2.49999999999998,3.499810792));
#152701=CARTESIAN_POINT('',(-8.603650246,2.49999999999998,-0.592096651999998));
#152702=CARTESIAN_POINT('Origin',(2.22044604925031E-15,2.49999999999998,
2.22044604925031E-15));
#152703=CARTESIAN_POINT('',(-9.689187855,2.49999999999998,-1.087262023));
#152704=CARTESIAN_POINT('Origin',(-7.630970629,2.49999999999998,-4.161955804));
#152705=CARTESIAN_POINT('',(-9.650512493,2.49999999999998,-1.389283491));
#152706=CARTESIAN_POINT('Origin',(2.22044604925031E-15,2.49999999999998,
2.22044604925031E-15));
#152707=CARTESIAN_POINT('',(-8.475231174,2.49999999999998,-1.594939671));
#152708=CARTESIAN_POINT('Origin',(-8.43346325,2.49999999999998,2.10482457));
#152709=CARTESIAN_POINT('',(-8.37982974917112,2.49999999999998,-2.03760383055369));
#152710=CARTESIAN_POINT('Origin',(2.22044604925031E-15,2.49999999999998,
2.22044604925031E-15));
#152711=CARTESIAN_POINT('',(-9.366069535,2.49999999999998,-2.709103444));
#152712=CARTESIAN_POINT('Origin',(-6.817832118,2.49999999999998,-5.391730155));
#152713=CARTESIAN_POINT('',(-9.276908607,2.49999999999998,-3.00024444));
#152714=CARTESIAN_POINT('Origin',(2.22044604925031E-15,2.49999999999998,
2.22044604925031E-15));
#152715=CARTESIAN_POINT('',(-8.083776576,2.49999999999998,-3.004318937));
#152716=CARTESIAN_POINT('Origin',(-8.667872637,2.49999999999998,0.649286377));
#152717=CARTESIAN_POINT('',(-7.914936808,2.49999999999998,-3.424492856));
#152718=CARTESIAN_POINT('Origin',(2.22044604925031E-15,2.49999999999998,
2.22044604925031E-15));
#152719=CARTESIAN_POINT('',(-8.773506446,2.49999999999998,-4.253008892));
#152720=CARTESIAN_POINT('Origin',(-5.808556991,2.49999999999998,-6.466394246));
#152721=CARTESIAN_POINT('',(-8.63642495,2.49999999999998,-4.524893819));
#152722=CARTESIAN_POINT('Origin',(2.22044604925031E-15,2.49999999999998,
2.22044604925031E-15));
#152723=CARTESIAN_POINT('',(-7.459766444,2.49999999999998,-4.327269417));
#152724=CARTESIAN_POINT('Origin',(-8.65292311,2.49999999999998,-0.824930601999998));
#152725=CARTESIAN_POINT('',(-7.222345546,2.49999999999998,-4.712865457));
#152726=CARTESIAN_POINT('Origin',(2.22044604925031E-15,2.49999999999998,
2.22044604925031E-15));
#152727=CARTESIAN_POINT('',(-7.928545552,2.49999999999998,-5.674563017));
#152728=CARTESIAN_POINT('Origin',(-4.632180254,2.49999999999998,-7.355031947));
#152729=CARTESIAN_POINT('',(-7.747487072,2.49999999999998,-5.919370243));
#152730=CARTESIAN_POINT('Origin',(2.22044604925031E-15,2.49999999999998,
2.22044604925031E-15));
#152731=CARTESIAN_POINT('',(-6.621152413,2.49999999999998,-5.525732234));
#152732=CARTESIAN_POINT('Origin',(-8.38904474,2.49999999999998,-2.275415831));
#152733=CARTESIAN_POINT('',(-6.321980552,2.49999999999998,-5.8656575));
#152734=CARTESIAN_POINT('Origin',(2.22044604925031E-15,2.49999999999998,
2.22044604925031E-15));
#152735=CARTESIAN_POINT('',(-6.855494836,2.49999999999998,-6.932870296));
#152736=CARTESIAN_POINT('Origin',(-3.322544125,2.49999999999998,-8.032078771));
#152737=CARTESIAN_POINT('',(-6.635668096,2.49999999999998,-7.143557161));
#152738=CARTESIAN_POINT('Origin',(2.22044604925031E-15,2.49999999999998,
2.22044604925031E-15));
#152739=CARTESIAN_POINT('',(-5.592059883,2.49999999999998,-6.565229795));
#152740=CARTESIAN_POINT('Origin',(-7.883828827,2.49999999999998,-3.660441488));
#152741=CARTESIAN_POINT('',(-5.239743688,2.49999999999998,-6.849705256));
#152742=CARTESIAN_POINT('Origin',(2.22044604925031E-15,2.49999999999998,
2.22044604925031E-15));
#152743=CARTESIAN_POINT('',(-5.585224017,2.49999999999998,-7.991731519));
#152744=CARTESIAN_POINT('Origin',(-1.917324452,2.49999999999998,-8.478057313));
#152745=CARTESIAN_POINT('',(-5.3329530316541,2.49999999999998,-8.16223694556031));
#152746=CARTESIAN_POINT('Origin',(2.22044604925031E-15,2.49999999999998,
2.22044604925031E-15));
#152747=CARTESIAN_POINT('',(-4.402093971,2.49999999999998,-7.415857649));
#152748=CARTESIAN_POINT('Origin',(-7.151809512,2.49999999999998,-4.940162908));
#152749=CARTESIAN_POINT('',(-4.006768937,2.49999999999998,-7.636699463));
#152750=CARTESIAN_POINT('Origin',(2.22044604925031E-15,2.49999999999998,
2.22044604925031E-15));
#152751=CARTESIAN_POINT('',(-4.154276471,2.49999999999998,-8.820685177));
#152752=CARTESIAN_POINT('Origin',(-0.456946843999999,2.49999999999998,-8.680137582));
#152753=CARTESIAN_POINT('',(-3.876818617,2.49999999999998,-8.946104035));
#152754=CARTESIAN_POINT('Origin',(2.22044604925031E-15,2.49999999999998,
2.22044604925031E-15));
#152755=CARTESIAN_POINT('',(-3.085487831,2.49999999999998,-8.05314478));
#152756=CARTESIAN_POINT('Origin',(-6.214045658,2.49999999999998,-6.077764837));
#152757=CARTESIAN_POINT('',(-2.65852674,2.49999999999998,-8.20399973));
#152758=CARTESIAN_POINT('Origin',(2.22044604925031E-15,2.49999999999998,
2.22044604925031E-15));
#152759=CARTESIAN_POINT('',(-2.60381795543899,2.49999999999998,-9.3958837827716));
#152760=CARTESIAN_POINT('Origin',(1.016576292,2.49999999999998,-8.632506096));
#152761=CARTESIAN_POINT('',(-2.30915519,2.49999999999998,-9.472607999));
#152762=CARTESIAN_POINT('Origin',(2.22044604925031E-15,2.49999999999998,
2.22044604925031E-15));
#152763=CARTESIAN_POINT('',(-1.680117823,2.49999999999998,-8.458757598));
#152764=CARTESIAN_POINT('Origin',(-5.097515025,2.49999999999998,-7.040520536));
#152765=CARTESIAN_POINT('',(-1.233803569,2.49999999999998,-8.535285862));
#152766=CARTESIAN_POINT('Origin',(2.22044604925031E-15,2.49999999999998,
2.22044604925031E-15));
#152767=CARTESIAN_POINT('',(-0.978452337999998,2.49999999999998,-9.700779918));
#152768=CARTESIAN_POINT('Origin',(2.460854379,2.49999999999998,-8.336533127));
#152769=CARTESIAN_POINT('',(-0.675061571999999,2.49999999999998,-9.726602278));
#152770=CARTESIAN_POINT('Origin',(2.22044604925031E-15,2.49999999999998,
2.22044604925031E-15));
#152771=CARTESIAN_POINT('',(-0.226413884999999,2.49999999999998,-8.621027361));
#152772=CARTESIAN_POINT('Origin',(-3.834338166,2.49999999999998,-7.800733278));
#152773=CARTESIAN_POINT('',(0.226413885000002,2.49999999999998,-8.621027361));
#152774=CARTESIAN_POINT('Origin',(2.22044604925031E-15,2.49999999999998,
2.22044604925031E-15));
#152775=CARTESIAN_POINT('',(0.675061572000001,2.49999999999998,-9.726602278));
#152776=CARTESIAN_POINT('Origin',(3.834338166,2.49999999999998,-7.800733278));
#152777=CARTESIAN_POINT('',(0.978452338000002,2.49999999999998,-9.700779918));
#152778=CARTESIAN_POINT('Origin',(2.22044604925031E-15,2.49999999999998,
2.22044604925031E-15));
#152779=CARTESIAN_POINT('',(1.233803568,2.49999999999998,-8.535285863));
#152780=CARTESIAN_POINT('Origin',(-2.460854379,2.49999999999998,-8.336533127));
#152781=CARTESIAN_POINT('',(1.680117823,2.49999999999998,-8.458757598));
#152782=CARTESIAN_POINT('Origin',(2.22044604925031E-15,2.49999999999998,
2.22044604925031E-15));
#152783=CARTESIAN_POINT('',(2.30915519,2.49999999999998,-9.472607999));
#152784=CARTESIAN_POINT('Origin',(5.097515025,2.49999999999998,-7.040520536));
#152785=CARTESIAN_POINT('Origin',(2.22044604925031E-15,2.49999999999998,
2.22044604925031E-15));
#152786=CARTESIAN_POINT('',(3.08548783,2.49999999999998,-8.05314478));
#152787=CARTESIAN_POINT('Origin',(2.22044604925031E-15,2.49999999999998,
2.22044604925031E-15));
#152788=CARTESIAN_POINT('',(3.876818617,2.49999999999998,-8.946104035));
#152789=CARTESIAN_POINT('Origin',(6.214045658,2.49999999999998,-6.077764837));
#152790=CARTESIAN_POINT('Origin',(2.22044604925031E-15,2.49999999999998,
2.22044604925031E-15));
#152791=CARTESIAN_POINT('',(4.402093972,2.49999999999998,-7.415857648));
#152792=CARTESIAN_POINT('Origin',(2.22044604925031E-15,2.49999999999998,
2.22044604925031E-15));
#152793=CARTESIAN_POINT('',(5.33295303165411,2.49999999999998,-8.16223694556031));
#152794=CARTESIAN_POINT('Origin',(7.151809512,2.49999999999998,-4.940162908));
#152795=CARTESIAN_POINT('',(5.585224017,2.49999999999998,-7.991731519));
#152796=CARTESIAN_POINT('Origin',(2.22044604925031E-15,2.49999999999998,
2.22044604925031E-15));
#152797=CARTESIAN_POINT('',(5.239743687,2.49999999999998,-6.849705256));
#152798=CARTESIAN_POINT('Origin',(1.917324452,2.49999999999998,-8.478057313));
#152799=CARTESIAN_POINT('',(5.592059883,2.49999999999998,-6.565229795));
#152800=CARTESIAN_POINT('Origin',(2.22044604925031E-15,2.49999999999998,
2.22044604925031E-15));
#152801=CARTESIAN_POINT('',(6.635668096,2.49999999999998,-7.143557161));
#152802=CARTESIAN_POINT('Origin',(7.883828827,2.49999999999998,-3.660441488));
#152803=CARTESIAN_POINT('',(6.855494836,2.49999999999998,-6.932870296));
#152804=CARTESIAN_POINT('Origin',(2.22044604925031E-15,2.49999999999998,
2.22044604925031E-15));
#152805=CARTESIAN_POINT('',(6.321980552,2.49999999999998,-5.8656575));
#152806=CARTESIAN_POINT('Origin',(3.322544125,2.49999999999998,-8.032078771));
#152807=CARTESIAN_POINT('',(6.621152413,2.49999999999998,-5.525732234));
#152808=CARTESIAN_POINT('Origin',(2.22044604925031E-15,2.49999999999998,
2.22044604925031E-15));
#152809=CARTESIAN_POINT('',(7.747487072,2.49999999999998,-5.919370243));
#152810=CARTESIAN_POINT('Origin',(8.38904474,2.49999999999998,-2.275415831));
#152811=CARTESIAN_POINT('',(7.928545552,2.49999999999998,-5.674563017));
#152812=CARTESIAN_POINT('Origin',(2.22044604925031E-15,2.49999999999998,
2.22044604925031E-15));
#152813=CARTESIAN_POINT('',(7.222345546,2.49999999999998,-4.712865457));
#152814=CARTESIAN_POINT('Origin',(4.632180254,2.49999999999998,-7.355031947));
#152815=CARTESIAN_POINT('',(7.459766444,2.49999999999998,-4.327269416));
#152816=CARTESIAN_POINT('Origin',(2.22044604925031E-15,2.49999999999998,
2.22044604925031E-15));
#152817=CARTESIAN_POINT('',(8.63642495,2.49999999999998,-4.524893819));
#152818=CARTESIAN_POINT('Origin',(8.65292311,2.49999999999998,-0.824930601999998));
#152819=CARTESIAN_POINT('',(8.773506446,2.49999999999998,-4.253008892));
#152820=CARTESIAN_POINT('Origin',(2.22044604925031E-15,2.49999999999998,
2.22044604925031E-15));
#152821=CARTESIAN_POINT('',(7.914936808,2.49999999999998,-3.424492856));
#152822=CARTESIAN_POINT('Origin',(5.808556991,2.49999999999998,-6.466394246));
#152823=CARTESIAN_POINT('',(8.083776576,2.49999999999998,-3.004318937));
#152824=CARTESIAN_POINT('Origin',(2.22044604925031E-15,2.49999999999998,
2.22044604925031E-15));
#152825=CARTESIAN_POINT('',(9.276908607,2.49999999999998,-3.00024444));
#152826=CARTESIAN_POINT('Origin',(8.667872637,2.49999999999998,0.649286377));
#152827=CARTESIAN_POINT('',(9.366069535,2.49999999999998,-2.709103444));
#152828=CARTESIAN_POINT('Origin',(2.22044604925031E-15,2.49999999999998,
2.22044604925031E-15));
#152829=CARTESIAN_POINT('',(8.37982974945342,2.49999999999998,-2.03760383017956));
#152830=CARTESIAN_POINT('Origin',(6.817832118,2.49999999999998,-5.391730155));
#152831=CARTESIAN_POINT('',(8.475231174,2.49999999999998,-1.594939671));
#152832=CARTESIAN_POINT('Origin',(2.22044604925031E-15,2.49999999999998,
2.22044604925031E-15));
#152833=CARTESIAN_POINT('',(9.650512493,2.49999999999998,-1.389283491));
#152834=CARTESIAN_POINT('Origin',(8.43346325,2.49999999999998,2.10482457));
#152835=CARTESIAN_POINT('Origin',(2.22044604925031E-15,2.49999999999998,
2.22044604925031E-15));
#152836=CARTESIAN_POINT('',(-4.394532211,2.49999999999998,-1.93082538));
#152837=CARTESIAN_POINT('',(4.394532211,2.49999999999998,-1.93082538));
#152838=CARTESIAN_POINT('Origin',(2.22044604925031E-15,2.49999999999998,
2.22044604925031E-15));
#152839=CARTESIAN_POINT('',(5.143848737,2.49999999999998,-1.606493127));
#152840=CARTESIAN_POINT('Origin',(4.943848737,2.49999999999998,-2.172178552));
#152841=CARTESIAN_POINT('',(5.143848737,2.49999999999998,-1.606493127));
#152842=CARTESIAN_POINT('',(-6.819607843,2.49999999999998,-2.872794609));
#152843=CARTESIAN_POINT('Origin',(2.22044604925031E-15,2.49999999999998,
2.22044604925031E-15));
#152844=CARTESIAN_POINT('',(-6.466666667,2.49999999999998,-2.074179891));
#152845=CARTESIAN_POINT('Origin',(-6.266666667,2.49999999999998,-2.639865316));
#152846=CARTESIAN_POINT('',(-5.143848737,2.49999999999998,-1.606493127));
#152847=CARTESIAN_POINT('',(-6.466666667,2.49999999999998,-2.074179891));
#152848=CARTESIAN_POINT('Origin',(-4.943848737,2.49999999999998,-2.172178552));
#152849=CARTESIAN_POINT('',(-5.143848737,2.49999999999998,1.606493127));
#152850=CARTESIAN_POINT('',(-6.466666667,2.49999999999998,2.074179891));
#152851=CARTESIAN_POINT('',(-5.143848737,2.49999999999998,1.606493127));
#152852=CARTESIAN_POINT('',(-6.819607843,2.49999999999998,2.872794609));
#152853=CARTESIAN_POINT('Origin',(-6.266666667,2.49999999999998,2.639865316));
#152854=CARTESIAN_POINT('Origin',(2.22044604925031E-15,2.49999999999998,
2.22044604925031E-15));
#152855=CARTESIAN_POINT('',(5.143848737,2.49999999999998,1.606493127));
#152856=CARTESIAN_POINT('',(6.466666667,2.49999999999998,2.074179891));
#152857=CARTESIAN_POINT('',(4.394532211,2.49999999999998,1.93082538));
#152858=CARTESIAN_POINT('Origin',(4.943848737,2.49999999999998,2.172178552));
#152859=CARTESIAN_POINT('',(-4.394532211,2.49999999999998,1.93082538));
#152860=CARTESIAN_POINT('Origin',(2.22044604925031E-15,2.49999999999998,
2.22044604925031E-15));
#152861=CARTESIAN_POINT('Origin',(-4.943848737,2.49999999999998,2.172178552));
#152862=CARTESIAN_POINT('Origin',(2.22044604925031E-15,17.5,2.22044604925031E-15));
#152863=CARTESIAN_POINT('',(9.689187855,7.49999999999998,-1.087262023));
#152864=CARTESIAN_POINT('',(9.689187855,2.49999999999998,-1.087262023));
#152865=CARTESIAN_POINT('',(9.650512493,7.49999999999998,-1.389283491));
#152866=CARTESIAN_POINT('',(9.650512493,7.49999999999998,-1.389283491));
#152867=CARTESIAN_POINT('Origin',(2.22044604925031E-15,7.49999999999998,
2.22044604925031E-15));
#152868=CARTESIAN_POINT('Origin',(2.22044604925031E-15,17.5,2.22044604925031E-15));
#152869=CARTESIAN_POINT('',(9.746488706,7.49999999999998,0.261644615999999));
#152870=CARTESIAN_POINT('',(9.746488706,7.49999999999998,0.261644615999999));
#152871=CARTESIAN_POINT('',(9.733565882,7.49999999999998,0.565857946999999));
#152872=CARTESIAN_POINT('Origin',(2.22044604925031E-15,7.49999999999998,
2.22044604925031E-15));
#152873=CARTESIAN_POINT('',(9.733565882,2.49999999999998,0.565857946999999));
#152874=CARTESIAN_POINT('Origin',(2.22044604925031E-15,17.5,2.22044604925031E-15));
#152875=CARTESIAN_POINT('',(9.366069535,7.49999999999998,-2.709103444));
#152876=CARTESIAN_POINT('',(9.366069535,2.49999999999998,-2.709103444));
#152877=CARTESIAN_POINT('',(9.276908607,7.49999999999998,-3.00024444));
#152878=CARTESIAN_POINT('',(9.276908607,7.49999999999998,-3.00024444));
#152879=CARTESIAN_POINT('Origin',(2.22044604925031E-15,7.49999999999998,
2.22044604925031E-15));
#152880=CARTESIAN_POINT('Origin',(2.22044604925031E-15,17.5,2.22044604925031E-15));
#152881=CARTESIAN_POINT('',(8.773506446,7.49999999999998,-4.253008892));
#152882=CARTESIAN_POINT('',(8.773506446,2.49999999999998,-4.253008892));
#152883=CARTESIAN_POINT('',(8.63642495,7.49999999999998,-4.524893819));
#152884=CARTESIAN_POINT('',(8.63642495,7.49999999999998,-4.524893819));
#152885=CARTESIAN_POINT('Origin',(2.22044604925031E-15,7.49999999999998,
2.22044604925031E-15));
#152886=CARTESIAN_POINT('Origin',(2.22044604925031E-15,17.5,2.22044604925031E-15));
#152887=CARTESIAN_POINT('',(7.928545552,7.49999999999998,-5.674563017));
#152888=CARTESIAN_POINT('',(7.928545552,2.49999999999998,-5.674563017));
#152889=CARTESIAN_POINT('',(7.747487072,7.49999999999998,-5.919370243));
#152890=CARTESIAN_POINT('',(7.747487072,7.49999999999998,-5.919370243));
#152891=CARTESIAN_POINT('Origin',(2.22044604925031E-15,7.49999999999998,
2.22044604925031E-15));
#152892=CARTESIAN_POINT('Origin',(2.22044604925031E-15,17.5,2.22044604925031E-15));
#152893=CARTESIAN_POINT('',(2.30915519,7.49999999999998,-9.472607999));
#152894=CARTESIAN_POINT('',(2.30915519,7.49999999999998,-9.472607999));
#152895=CARTESIAN_POINT('Origin',(2.22044604925031E-15,7.49999999999998,
2.22044604925031E-15));
#152896=CARTESIAN_POINT('Origin',(2.22044604925031E-15,17.5,2.22044604925031E-15));
#152897=CARTESIAN_POINT('',(3.876818617,7.49999999999998,-8.946104035));
#152898=CARTESIAN_POINT('',(3.876818617,7.49999999999998,-8.946104035));
#152899=CARTESIAN_POINT('Origin',(2.22044604925031E-15,7.49999999999998,
2.22044604925031E-15));
#152900=CARTESIAN_POINT('Origin',(2.22044604925031E-15,17.5,2.22044604925031E-15));
#152901=CARTESIAN_POINT('',(5.33295303165411,7.49999999999998,-8.16223694556031));
#152902=CARTESIAN_POINT('',(5.332953031,7.49999999999998,-8.162236945));
#152903=CARTESIAN_POINT('',(5.585224017,7.49999999999998,-7.991731519));
#152904=CARTESIAN_POINT('Origin',(2.22044604925031E-15,7.49999999999998,
2.22044604925031E-15));
#152905=CARTESIAN_POINT('',(5.585224017,2.49999999999998,-7.991731519));
#152906=CARTESIAN_POINT('Origin',(2.22044604925031E-15,17.5,2.22044604925031E-15));
#152907=CARTESIAN_POINT('',(6.855494836,7.49999999999998,-6.932870296));
#152908=CARTESIAN_POINT('',(6.855494836,2.49999999999998,-6.932870296));
#152909=CARTESIAN_POINT('',(6.635668096,7.49999999999998,-7.143557161));
#152910=CARTESIAN_POINT('',(6.635668096,7.49999999999998,-7.143557161));
#152911=CARTESIAN_POINT('Origin',(2.22044604925031E-15,7.49999999999998,
2.22044604925031E-15));
#152912=CARTESIAN_POINT('Origin',(2.22044604925031E-15,17.5,2.22044604925031E-15));
#152913=CARTESIAN_POINT('',(6.005947057,7.49999999999998,7.680566382));
#152914=CARTESIAN_POINT('',(6.005947057,2.49999999999998,7.680566382));
#152915=CARTESIAN_POINT('',(6.242849363,7.49999999999998,7.489281129));
#152916=CARTESIAN_POINT('',(6.242849363,7.49999999999998,7.489281129));
#152917=CARTESIAN_POINT('Origin',(2.22044604925031E-15,7.49999999999998,
2.22044604925031E-15));
#152918=CARTESIAN_POINT('Origin',(2.22044604925031E-15,17.5,2.22044604925031E-15));
#152919=CARTESIAN_POINT('',(4.887357004,7.49999999999998,8.436601301));
#152920=CARTESIAN_POINT('',(4.887357004,7.49999999999998,8.436601301));
#152921=CARTESIAN_POINT('',(4.621534957,7.49999999999998,8.585098406));
#152922=CARTESIAN_POINT('Origin',(2.22044604925031E-15,7.49999999999998,
2.22044604925031E-15));
#152923=CARTESIAN_POINT('',(4.621534957,2.49999999999998,8.585098406));
#152924=CARTESIAN_POINT('Origin',(2.22044604925031E-15,17.5,2.22044604925031E-15));
#152925=CARTESIAN_POINT('',(7.217578995,7.49999999999998,6.555078448));
#152926=CARTESIAN_POINT('',(7.217578995,2.49999999999998,6.555078448));
#152927=CARTESIAN_POINT('',(7.418746313,7.49999999999998,6.326507974));
#152928=CARTESIAN_POINT('',(7.418746313,7.49999999999998,6.326507974));
#152929=CARTESIAN_POINT('Origin',(2.22044604925031E-15,7.49999999999998,
2.22044604925031E-15));
#152930=CARTESIAN_POINT('Origin',(2.22044604925031E-15,17.5,2.22044604925031E-15));
#152931=CARTESIAN_POINT('',(3.104169711,7.49999999999998,9.24265278));
#152932=CARTESIAN_POINT('Origin',(2.22044604925031E-15,7.49999999999998,
2.22044604925031E-15));
#152933=CARTESIAN_POINT('',(3.104169711,2.49999999999998,9.24265278));
#152934=CARTESIAN_POINT('Origin',(2.22044604925031E-15,17.5,2.22044604925031E-15));
#152935=CARTESIAN_POINT('',(1.497503154,7.49999999999998,9.634312861));
#152936=CARTESIAN_POINT('Origin',(2.22044604925031E-15,7.49999999999998,
2.22044604925031E-15));
#152937=CARTESIAN_POINT('',(1.497503154,2.49999999999998,9.634312861));
#152938=CARTESIAN_POINT('Origin',(2.22044604925031E-15,17.5,2.22044604925031E-15));
#152939=CARTESIAN_POINT('',(0.152243842000002,7.49999999999998,9.748811303));
#152940=CARTESIAN_POINT('',(0.152243842000002,7.49999999999998,9.748811303));
#152941=CARTESIAN_POINT('',(-0.152243841999998,7.49999999999998,9.748811303));
#152942=CARTESIAN_POINT('Origin',(2.22044604925031E-15,7.49999999999998,
2.22044604925031E-15));
#152943=CARTESIAN_POINT('',(-0.152243841999998,2.49999999999998,9.748811303));
#152944=CARTESIAN_POINT('Origin',(2.22044604925031E-15,17.5,2.22044604925031E-15));
#152945=CARTESIAN_POINT('',(8.989049934,7.49999999999998,3.776172836));
#152946=CARTESIAN_POINT('',(8.989049934,2.49999999999998,3.776172836));
#152947=CARTESIAN_POINT('',(9.10258013994849,7.49999999999998,3.49364205338695));
#152948=CARTESIAN_POINT('',(9.10258014,7.49999999999998,3.493642054));
#152949=CARTESIAN_POINT('Origin',(2.22044604925031E-15,7.49999999999998,
2.22044604925031E-15));
#152950=CARTESIAN_POINT('Origin',(2.22044604925031E-15,17.5,2.22044604925031E-15));
#152951=CARTESIAN_POINT('',(8.381219438,7.49999999999998,4.981732704));
#152952=CARTESIAN_POINT('',(8.381219438,7.49999999999998,4.981732704));
#152953=CARTESIAN_POINT('',(8.221574327,7.49999999999998,5.24101284));
#152954=CARTESIAN_POINT('Origin',(2.22044604925031E-15,7.49999999999998,
2.22044604925031E-15));
#152955=CARTESIAN_POINT('',(8.221574327,2.49999999999998,5.24101284));
#152956=CARTESIAN_POINT('Origin',(2.22044604925031E-15,17.5,2.22044604925031E-15));
#152957=CARTESIAN_POINT('',(9.497926941,7.49999999999998,2.202699214));
#152958=CARTESIAN_POINT('',(9.497926941,2.49999999999998,2.202699214));
#152959=CARTESIAN_POINT('',(9.562076184,7.49999999999998,1.905045682));
#152960=CARTESIAN_POINT('',(9.562076184,7.49999999999998,1.905045682));
#152961=CARTESIAN_POINT('Origin',(2.22044604925031E-15,7.49999999999998,
2.22044604925031E-15));
#152962=CARTESIAN_POINT('Origin',(2.22044604925031E-15,17.5,2.22044604925031E-15));
#152963=CARTESIAN_POINT('',(-7.418746313,7.49999999999998,6.326507974));
#152964=CARTESIAN_POINT('',(-7.418746313,2.49999999999998,6.326507974));
#152965=CARTESIAN_POINT('',(-7.217578995,7.49999999999998,6.555078448));
#152966=CARTESIAN_POINT('',(-7.217578995,7.49999999999998,6.555078448));
#152967=CARTESIAN_POINT('Origin',(2.22044604925031E-15,7.49999999999998,
2.22044604925031E-15));
#152968=CARTESIAN_POINT('Origin',(2.22044604925031E-15,17.5,2.22044604925031E-15));
#152969=CARTESIAN_POINT('',(-8.221574327,7.49999999999998,5.24101284));
#152970=CARTESIAN_POINT('',(-8.221574327,7.49999999999998,5.24101284));
#152971=CARTESIAN_POINT('',(-8.381219438,7.49999999999998,4.981732704));
#152972=CARTESIAN_POINT('Origin',(2.22044604925031E-15,7.49999999999998,
2.22044604925031E-15));
#152973=CARTESIAN_POINT('',(-8.381219438,2.49999999999998,4.981732704));
#152974=CARTESIAN_POINT('Origin',(2.22044604925031E-15,17.5,2.22044604925031E-15));
#152975=CARTESIAN_POINT('',(-6.242849363,7.49999999999998,7.489281129));
#152976=CARTESIAN_POINT('',(-6.242849363,2.49999999999998,7.489281129));
#152977=CARTESIAN_POINT('',(-6.005947057,7.49999999999998,7.680566382));
#152978=CARTESIAN_POINT('',(-6.005947057,7.49999999999998,7.680566382));
#152979=CARTESIAN_POINT('Origin',(2.22044604925031E-15,7.49999999999998,
2.22044604925031E-15));
#152980=CARTESIAN_POINT('Origin',(2.22044604925031E-15,17.5,2.22044604925031E-15));
#152981=CARTESIAN_POINT('',(-8.989049934,7.49999999999998,3.776172836));
#152982=CARTESIAN_POINT('',(-8.989049934,7.49999999999998,3.776172836));
#152983=CARTESIAN_POINT('',(-9.10258013994848,7.49999999999998,3.49364205338695));
#152984=CARTESIAN_POINT('Origin',(2.22044604925031E-15,7.49999999999998,
2.22044604925031E-15));
#152985=CARTESIAN_POINT('',(-9.10258014,2.49999999999998,3.493642054));
#152986=CARTESIAN_POINT('Origin',(2.22044604925031E-15,17.5,2.22044604925031E-15));
#152987=CARTESIAN_POINT('',(-9.497926941,7.49999999999998,2.202699214));
#152988=CARTESIAN_POINT('',(-9.497926941,7.49999999999998,2.202699214));
#152989=CARTESIAN_POINT('',(-9.562076184,7.49999999999998,1.905045682));
#152990=CARTESIAN_POINT('Origin',(2.22044604925031E-15,7.49999999999998,
2.22044604925031E-15));
#152991=CARTESIAN_POINT('',(-9.562076184,2.49999999999998,1.905045682));
#152992=CARTESIAN_POINT('Origin',(2.22044604925031E-15,17.5,2.22044604925031E-15));
#152993=CARTESIAN_POINT('',(-9.733565882,7.49999999999998,0.565857946999999));
#152994=CARTESIAN_POINT('',(-9.733565882,7.49999999999998,0.565857946999999));
#152995=CARTESIAN_POINT('',(-9.746488706,7.49999999999998,0.261644615999999));
#152996=CARTESIAN_POINT('Origin',(2.22044604925031E-15,7.49999999999998,
2.22044604925031E-15));
#152997=CARTESIAN_POINT('',(-9.746488706,2.49999999999998,0.261644615999999));
#152998=CARTESIAN_POINT('Origin',(2.22044604925031E-15,17.5,2.22044604925031E-15));
#152999=CARTESIAN_POINT('',(-3.391264282,7.49999999999998,9.141215815));
#153000=CARTESIAN_POINT('',(-3.391264282,2.49999999999998,9.141215815));
#153001=CARTESIAN_POINT('',(-3.104169711,7.49999999999998,9.24265278));
#153002=CARTESIAN_POINT('',(-3.104169711,7.49999999999998,9.24265278));
#153003=CARTESIAN_POINT('Origin',(2.22044604925031E-15,7.49999999999998,
2.22044604925031E-15));
#153004=CARTESIAN_POINT('Origin',(2.22044604925031E-15,17.5,2.22044604925031E-15));
#153005=CARTESIAN_POINT('',(-4.621534957,7.49999999999998,8.585098406));
#153006=CARTESIAN_POINT('',(-4.621534957,7.49999999999998,8.585098406));
#153007=CARTESIAN_POINT('',(-4.887357004,7.49999999999998,8.436601301));
#153008=CARTESIAN_POINT('Origin',(2.22044604925031E-15,7.49999999999998,
2.22044604925031E-15));
#153009=CARTESIAN_POINT('',(-4.887357004,2.49999999999998,8.436601301));
#153010=CARTESIAN_POINT('Origin',(2.22044604925031E-15,17.5,2.22044604925031E-15));
#153011=CARTESIAN_POINT('',(-1.797611062,7.49999999999998,9.582854192));
#153012=CARTESIAN_POINT('',(-1.797611062,2.49999999999998,9.582854192));
#153013=CARTESIAN_POINT('',(-1.497503154,7.49999999999998,9.634312861));
#153014=CARTESIAN_POINT('',(-1.497503154,7.49999999999998,9.634312861));
#153015=CARTESIAN_POINT('Origin',(2.22044604925031E-15,7.49999999999998,
2.22044604925031E-15));
#153016=CARTESIAN_POINT('Origin',(2.22044604925031E-15,17.5,2.22044604925031E-15));
#153017=CARTESIAN_POINT('',(-6.635668096,7.49999999999998,-7.143557161));
#153018=CARTESIAN_POINT('',(-6.635668096,2.49999999999998,-7.143557161));
#153019=CARTESIAN_POINT('',(-6.855494836,7.49999999999998,-6.932870296));
#153020=CARTESIAN_POINT('',(-6.855494836,7.49999999999998,-6.932870296));
#153021=CARTESIAN_POINT('Origin',(2.22044604925031E-15,7.49999999999998,
2.22044604925031E-15));
#153022=CARTESIAN_POINT('Origin',(2.22044604925031E-15,17.5,2.22044604925031E-15));
#153023=CARTESIAN_POINT('',(-5.585224017,7.49999999999998,-7.991731519));
#153024=CARTESIAN_POINT('',(-5.585224017,7.49999999999998,-7.991731519));
#153025=CARTESIAN_POINT('',(-5.33295303165411,7.49999999999998,-8.16223694556031));
#153026=CARTESIAN_POINT('Origin',(2.22044604925031E-15,7.49999999999998,
2.22044604925031E-15));
#153027=CARTESIAN_POINT('',(-5.332953031,2.49999999999998,-8.162236945));
#153028=CARTESIAN_POINT('Origin',(2.22044604925031E-15,17.5,2.22044604925031E-15));
#153029=CARTESIAN_POINT('',(-7.747487072,7.49999999999998,-5.919370243));
#153030=CARTESIAN_POINT('',(-7.747487072,2.49999999999998,-5.919370243));
#153031=CARTESIAN_POINT('',(-7.928545552,7.49999999999998,-5.674563017));
#153032=CARTESIAN_POINT('',(-7.928545552,7.49999999999998,-5.674563017));
#153033=CARTESIAN_POINT('Origin',(2.22044604925031E-15,7.49999999999998,
2.22044604925031E-15));
#153034=CARTESIAN_POINT('Origin',(2.22044604925031E-15,17.5,2.22044604925031E-15));
#153035=CARTESIAN_POINT('',(-4.154276471,7.49999999999998,-8.820685177));
#153036=CARTESIAN_POINT('',(-4.154276471,7.49999999999998,-8.820685177));
#153037=CARTESIAN_POINT('',(-3.876818617,7.49999999999998,-8.946104035));
#153038=CARTESIAN_POINT('Origin',(2.22044604925031E-15,7.49999999999998,
2.22044604925031E-15));
#153039=CARTESIAN_POINT('',(-3.876818617,2.49999999999998,-8.946104035));
#153040=CARTESIAN_POINT('Origin',(2.22044604925031E-15,17.5,2.22044604925031E-15));
#153041=CARTESIAN_POINT('',(-2.60381795543899,7.49999999999998,-9.3958837827716));
#153042=CARTESIAN_POINT('',(-2.603817955,7.49999999999998,-9.395883783));
#153043=CARTESIAN_POINT('',(-2.30915519,7.49999999999998,-9.472607999));
#153044=CARTESIAN_POINT('Origin',(2.22044604925031E-15,7.49999999999998,
2.22044604925031E-15));
#153045=CARTESIAN_POINT('',(-2.30915519,2.49999999999998,-9.472607999));
#153046=CARTESIAN_POINT('Origin',(2.22044604925031E-15,17.5,2.22044604925031E-15));
#153047=CARTESIAN_POINT('',(-0.978452337999998,7.49999999999998,-9.700779918));
#153048=CARTESIAN_POINT('',(-0.978452337999998,7.49999999999998,-9.700779918));
#153049=CARTESIAN_POINT('',(-0.675061571999999,7.49999999999998,-9.726602278));
#153050=CARTESIAN_POINT('Origin',(2.22044604925031E-15,7.49999999999998,
2.22044604925031E-15));
#153051=CARTESIAN_POINT('',(-0.675061571999999,2.49999999999998,-9.726602278));
#153052=CARTESIAN_POINT('Origin',(2.22044604925031E-15,17.5,2.22044604925031E-15));
#153053=CARTESIAN_POINT('',(-8.63642495,7.49999999999998,-4.524893819));
#153054=CARTESIAN_POINT('',(-8.63642495,2.49999999999998,-4.524893819));
#153055=CARTESIAN_POINT('',(-8.773506446,7.49999999999998,-4.253008892));
#153056=CARTESIAN_POINT('',(-8.773506446,7.49999999999998,-4.253008892));
#153057=CARTESIAN_POINT('Origin',(2.22044604925031E-15,7.49999999999998,
2.22044604925031E-15));
#153058=CARTESIAN_POINT('Origin',(2.22044604925031E-15,17.5,2.22044604925031E-15));
#153059=CARTESIAN_POINT('',(-9.276908607,7.49999999999998,-3.00024444));
#153060=CARTESIAN_POINT('',(-9.276908607,2.49999999999998,-3.00024444));
#153061=CARTESIAN_POINT('',(-9.366069535,7.49999999999998,-2.709103444));
#153062=CARTESIAN_POINT('',(-9.366069535,7.49999999999998,-2.709103444));
#153063=CARTESIAN_POINT('Origin',(2.22044604925031E-15,7.49999999999998,
2.22044604925031E-15));
#153064=CARTESIAN_POINT('Origin',(2.22044604925031E-15,17.5,2.22044604925031E-15));
#153065=CARTESIAN_POINT('',(-9.650512493,7.49999999999998,-1.389283491));
#153066=CARTESIAN_POINT('',(-9.650512493,2.49999999999998,-1.389283491));
#153067=CARTESIAN_POINT('',(-9.689187855,7.49999999999998,-1.087262023));
#153068=CARTESIAN_POINT('',(-9.689187855,7.49999999999998,-1.087262023));
#153069=CARTESIAN_POINT('Origin',(2.22044604925031E-15,7.49999999999998,
2.22044604925031E-15));
#153070=CARTESIAN_POINT('Origin',(2.22044604925031E-15,7.49999999999998,
2.22044604925031E-15));
#153071=CARTESIAN_POINT('',(8.603650246,7.49999999999998,-0.592096652999998));
#153072=CARTESIAN_POINT('Origin',(7.630970629,7.49999999999998,-4.161955804));
#153073=CARTESIAN_POINT('',(8.475231174,7.49999999999998,-1.594939671));
#153074=CARTESIAN_POINT('Origin',(8.43346325,7.49999999999998,2.10482457));
#153075=CARTESIAN_POINT('',(8.37982974945342,7.49999999999998,-2.03760383017956));
#153076=CARTESIAN_POINT('Origin',(2.22044604925031E-15,7.49999999999998,
2.22044604925031E-15));
#153077=CARTESIAN_POINT('Origin',(6.817832118,7.49999999999998,-5.391730155));
#153078=CARTESIAN_POINT('',(8.083776576,7.49999999999998,-3.004318937));
#153079=CARTESIAN_POINT('Origin',(8.667872637,7.49999999999998,0.649286377));
#153080=CARTESIAN_POINT('',(7.914936808,7.49999999999998,-3.424492856));
#153081=CARTESIAN_POINT('Origin',(2.22044604925031E-15,7.49999999999998,
2.22044604925031E-15));
#153082=CARTESIAN_POINT('Origin',(5.808556991,7.49999999999998,-6.466394246));
#153083=CARTESIAN_POINT('',(7.459766444,7.49999999999998,-4.327269416));
#153084=CARTESIAN_POINT('Origin',(8.65292311,7.49999999999998,-0.824930601999998));
#153085=CARTESIAN_POINT('',(7.222345546,7.49999999999998,-4.712865457));
#153086=CARTESIAN_POINT('Origin',(2.22044604925031E-15,7.49999999999998,
2.22044604925031E-15));
#153087=CARTESIAN_POINT('Origin',(4.632180254,7.49999999999998,-7.355031947));
#153088=CARTESIAN_POINT('',(6.621152413,7.49999999999998,-5.525732234));
#153089=CARTESIAN_POINT('Origin',(8.38904474,7.49999999999998,-2.275415831));
#153090=CARTESIAN_POINT('',(6.321980552,7.49999999999998,-5.8656575));
#153091=CARTESIAN_POINT('Origin',(2.22044604925031E-15,7.49999999999998,
2.22044604925031E-15));
#153092=CARTESIAN_POINT('Origin',(3.322544125,7.49999999999998,-8.032078771));
#153093=CARTESIAN_POINT('',(5.592059883,7.49999999999998,-6.565229795));
#153094=CARTESIAN_POINT('Origin',(7.883828827,7.49999999999998,-3.660441488));
#153095=CARTESIAN_POINT('',(5.239743687,7.49999999999998,-6.849705256));
#153096=CARTESIAN_POINT('Origin',(2.22044604925031E-15,7.49999999999998,
2.22044604925031E-15));
#153097=CARTESIAN_POINT('Origin',(1.917324452,7.49999999999998,-8.478057313));
#153098=CARTESIAN_POINT('',(4.402093972,7.49999999999998,-7.415857648));
#153099=CARTESIAN_POINT('Origin',(7.151809512,7.49999999999998,-4.940162908));
#153100=CARTESIAN_POINT('Origin',(2.22044604925031E-15,7.49999999999998,
2.22044604925031E-15));
#153101=CARTESIAN_POINT('',(3.08548783,7.49999999999998,-8.05314478));
#153102=CARTESIAN_POINT('Origin',(6.214045658,7.49999999999998,-6.077764837));
#153103=CARTESIAN_POINT('Origin',(2.22044604925031E-15,7.49999999999998,
2.22044604925031E-15));
#153104=CARTESIAN_POINT('',(1.680117823,7.49999999999998,-8.458757598));
#153105=CARTESIAN_POINT('Origin',(5.097515025,7.49999999999998,-7.040520536));
#153106=CARTESIAN_POINT('',(1.233803568,7.49999999999998,-8.535285863));
#153107=CARTESIAN_POINT('Origin',(2.22044604925031E-15,7.49999999999998,
2.22044604925031E-15));
#153108=CARTESIAN_POINT('',(0.978452338000002,7.49999999999998,-9.700779918));
#153109=CARTESIAN_POINT('Origin',(-2.460854379,7.49999999999998,-8.336533127));
#153110=CARTESIAN_POINT('',(0.675061572000001,7.49999999999998,-9.726602278));
#153111=CARTESIAN_POINT('Origin',(2.22044604925031E-15,7.49999999999998,
2.22044604925031E-15));
#153112=CARTESIAN_POINT('',(0.226413885000002,7.49999999999998,-8.621027361));
#153113=CARTESIAN_POINT('Origin',(3.834338166,7.49999999999998,-7.800733278));
#153114=CARTESIAN_POINT('',(-0.226413884999999,7.49999999999998,-8.621027361));
#153115=CARTESIAN_POINT('Origin',(2.22044604925031E-15,7.49999999999998,
2.22044604925031E-15));
#153116=CARTESIAN_POINT('Origin',(-3.834338166,7.49999999999998,-7.800733278));
#153117=CARTESIAN_POINT('',(-1.233803569,7.49999999999998,-8.535285862));
#153118=CARTESIAN_POINT('Origin',(2.460854379,7.49999999999998,-8.336533127));
#153119=CARTESIAN_POINT('',(-1.680117823,7.49999999999998,-8.458757598));
#153120=CARTESIAN_POINT('Origin',(2.22044604925031E-15,7.49999999999998,
2.22044604925031E-15));
#153121=CARTESIAN_POINT('Origin',(-5.097515025,7.49999999999998,-7.040520536));
#153122=CARTESIAN_POINT('',(-2.65852674,7.49999999999998,-8.20399973));
#153123=CARTESIAN_POINT('Origin',(1.016576292,7.49999999999998,-8.632506096));
#153124=CARTESIAN_POINT('',(-3.085487831,7.49999999999998,-8.05314478));
#153125=CARTESIAN_POINT('Origin',(2.22044604925031E-15,7.49999999999998,
2.22044604925031E-15));
#153126=CARTESIAN_POINT('Origin',(-6.214045658,7.49999999999998,-6.077764837));
#153127=CARTESIAN_POINT('',(-4.006768937,7.49999999999998,-7.636699463));
#153128=CARTESIAN_POINT('Origin',(-0.456946843999999,7.49999999999998,-8.680137582));
#153129=CARTESIAN_POINT('',(-4.402093971,7.49999999999998,-7.415857649));
#153130=CARTESIAN_POINT('Origin',(2.22044604925031E-15,7.49999999999998,
2.22044604925031E-15));
#153131=CARTESIAN_POINT('Origin',(-7.151809512,7.49999999999998,-4.940162908));
#153132=CARTESIAN_POINT('',(-5.239743688,7.49999999999998,-6.849705256));
#153133=CARTESIAN_POINT('Origin',(-1.917324452,7.49999999999998,-8.478057313));
#153134=CARTESIAN_POINT('',(-5.592059883,7.49999999999998,-6.565229795));
#153135=CARTESIAN_POINT('Origin',(2.22044604925031E-15,7.49999999999998,
2.22044604925031E-15));
#153136=CARTESIAN_POINT('Origin',(-7.883828827,7.49999999999998,-3.660441488));
#153137=CARTESIAN_POINT('',(-6.321980552,7.49999999999998,-5.8656575));
#153138=CARTESIAN_POINT('Origin',(-3.322544125,7.49999999999998,-8.032078771));
#153139=CARTESIAN_POINT('',(-6.621152413,7.49999999999998,-5.525732234));
#153140=CARTESIAN_POINT('Origin',(2.22044604925031E-15,7.49999999999998,
2.22044604925031E-15));
#153141=CARTESIAN_POINT('Origin',(-8.38904474,7.49999999999998,-2.275415831));
#153142=CARTESIAN_POINT('',(-7.222345546,7.49999999999998,-4.712865457));
#153143=CARTESIAN_POINT('Origin',(-4.632180254,7.49999999999998,-7.355031947));
#153144=CARTESIAN_POINT('',(-7.459766444,7.49999999999998,-4.327269417));
#153145=CARTESIAN_POINT('Origin',(2.22044604925031E-15,7.49999999999998,
2.22044604925031E-15));
#153146=CARTESIAN_POINT('Origin',(-8.65292311,7.49999999999998,-0.824930601999998));
#153147=CARTESIAN_POINT('',(-7.914936808,7.49999999999998,-3.424492856));
#153148=CARTESIAN_POINT('Origin',(-5.808556991,7.49999999999998,-6.466394246));
#153149=CARTESIAN_POINT('',(-8.083776576,7.49999999999998,-3.004318937));
#153150=CARTESIAN_POINT('Origin',(2.22044604925031E-15,7.49999999999998,
2.22044604925031E-15));
#153151=CARTESIAN_POINT('Origin',(-8.667872637,7.49999999999998,0.649286377));
#153152=CARTESIAN_POINT('',(-8.37982974917112,7.49999999999998,-2.03760383055369));
#153153=CARTESIAN_POINT('Origin',(-6.817832118,7.49999999999998,-5.391730155));
#153154=CARTESIAN_POINT('',(-8.475231174,7.49999999999998,-1.594939671));
#153155=CARTESIAN_POINT('Origin',(2.22044604925031E-15,7.49999999999998,
2.22044604925031E-15));
#153156=CARTESIAN_POINT('Origin',(-8.43346325,7.49999999999998,2.10482457));
#153157=CARTESIAN_POINT('',(-8.603650246,7.49999999999998,-0.592096651999998));
#153158=CARTESIAN_POINT('Origin',(-7.630970629,7.49999999999998,-4.161955804));
#153159=CARTESIAN_POINT('',(-8.622868801,7.49999999999998,-0.139676895));
#153160=CARTESIAN_POINT('Origin',(2.22044604925031E-15,7.49999999999998,
2.22044604925031E-15));
#153161=CARTESIAN_POINT('Origin',(-7.956438479,7.49999999999998,3.499810792));
#153162=CARTESIAN_POINT('',(-8.579959389,7.49999999999998,0.870444068000003));
#153163=CARTESIAN_POINT('Origin',(-8.224580008,7.49999999999998,-2.812449563));
#153164=CARTESIAN_POINT('',(-8.522442193,7.49999999999998,1.31960413));
#153165=CARTESIAN_POINT('Origin',(2.22044604925031E-15,7.49999999999998,
2.22044604925031E-15));
#153166=CARTESIAN_POINT('Origin',(-7.25052146,7.49999999999998,4.794113829));
#153167=CARTESIAN_POINT('',(-8.309438723,7.49999999999998,2.307943698));
#153168=CARTESIAN_POINT('Origin',(-8.581583195,7.49999999999998,-1.382034268));
#153169=CARTESIAN_POINT('',(-8.17684044,7.49999999999998,2.740922548));
#153170=CARTESIAN_POINT('Origin',(2.22044604925031E-15,7.49999999999998,
2.22044604925031E-15));
#153171=CARTESIAN_POINT('Origin',(-6.33602014,7.49999999999998,5.950498941));
#153172=CARTESIAN_POINT('',(-7.799870633,7.49999999999998,3.67904799));
#153173=CARTESIAN_POINT('Origin',(-8.691709858,7.49999999999998,0.088139637000002));
#153174=CARTESIAN_POINT('',(-7.596005875,7.49999999999998,4.083389615));
#153175=CARTESIAN_POINT('Origin',(2.22044604925031E-15,7.49999999999998,
2.22044604925031E-15));
#153176=CARTESIAN_POINT('Origin',(-5.239243055,7.49999999999998,6.935699032));
#153177=CARTESIAN_POINT('',(-7.065914466,7.49999999999998,4.944312768));
#153178=CARTESIAN_POINT('Origin',(-8.551791853,7.49999999999998,1.555777924));
#153179=CARTESIAN_POINT('',(-6.796648051,7.49999999999998,5.308384996));
#153180=CARTESIAN_POINT('Origin',(2.22044604925031E-15,7.49999999999998,
2.22044604925031E-15));
#153181=CARTESIAN_POINT('Origin',(-3.991742488,7.49999999999998,7.721371689));
#153182=CARTESIAN_POINT('',(-6.128684805,7.49999999999998,6.067338672));
#153183=CARTESIAN_POINT('Origin',(-8.165854367,7.49999999999998,2.978659314));
#153184=CARTESIAN_POINT('',(-5.801763037,7.49999999999998,6.380667807));
#153185=CARTESIAN_POINT('Origin',(2.22044604925031E-15,7.49999999999998,
2.22044604925031E-15));
#153186=CARTESIAN_POINT('Origin',(-2.629406756,7.49999999999998,8.284914542));
#153187=CARTESIAN_POINT('',(-5.015144041,7.49999999999998,7.015818288));
#153188=CARTESIAN_POINT('Origin',(-7.545000119,7.49999999999998,4.315850098));
#153189=CARTESIAN_POINT('',(-4.639971864,7.49999999999998,7.269390422));
#153190=CARTESIAN_POINT('Origin',(2.22044604925031E-15,7.49999999999998,
2.22044604925031E-15));
#153191=CARTESIAN_POINT('Origin',(-1.19142778,7.49999999999998,8.610115487));
#153192=CARTESIAN_POINT('',(-3.757326714,7.49999999999998,7.762465586));
#153193=CARTESIAN_POINT('Origin',(-6.707089953,7.49999999999998,5.528881732));
#153194=CARTESIAN_POINT('',(-3.344697148,7.49999999999998,7.948985909));
#153195=CARTESIAN_POINT('Origin',(2.22044604925031E-15,7.49999999999998,
2.22044604925031E-15));
#153196=CARTESIAN_POINT('Origin',(0.280826404000001,7.49999999999998,8.687619086));
#153197=CARTESIAN_POINT('',(-2.391417938,7.49999999999998,8.285800881));
#153198=CARTESIAN_POINT('Origin',(-5.676229022,7.49999999999998,6.582857506));
#153199=CARTESIAN_POINT('',(-1.953201585,7.49999999999998,8.399903545));
#153200=CARTESIAN_POINT('Origin',(2.22044604925031E-15,7.49999999999998,
2.22044604925031E-15));
#153201=CARTESIAN_POINT('Origin',(1.745001724,7.49999999999998,8.515195702));
#153202=CARTESIAN_POINT('',(-0.956712421999999,7.49999999999998,8.570768772));
#153203=CARTESIAN_POINT('Origin',(-4.482073316,7.49999999999998,7.447456454));
#153204=CARTESIAN_POINT('',(-0.505515968999999,7.49999999999998,8.60917125));
#153205=CARTESIAN_POINT('Origin',(2.22044604925031E-15,7.49999999999998,
2.22044604925031E-15));
#153206=CARTESIAN_POINT('Origin',(3.158976522,7.49999999999998,8.09780564));
#153207=CARTESIAN_POINT('',(0.505515969000001,7.49999999999998,8.60917125));
#153208=CARTESIAN_POINT('Origin',(-3.158976522,7.49999999999998,8.09780564));
#153209=CARTESIAN_POINT('',(0.956712422000002,7.49999999999998,8.570768772));
#153210=CARTESIAN_POINT('Origin',(2.22044604925031E-15,7.49999999999998,
2.22044604925031E-15));
#153211=CARTESIAN_POINT('Origin',(4.482073316,7.49999999999998,7.447456454));
#153212=CARTESIAN_POINT('',(2.391417938,7.49999999999998,8.285800881));
#153213=CARTESIAN_POINT('Origin',(2.22044604925031E-15,7.49999999999998,
2.22044604925031E-15));
#153214=CARTESIAN_POINT('Origin',(5.676229022,7.49999999999998,6.582857506));
#153215=CARTESIAN_POINT('',(3.757326714,7.49999999999998,7.762465586));
#153216=CARTESIAN_POINT('Origin',(2.22044604925031E-15,7.49999999999998,
2.22044604925031E-15));
#153217=CARTESIAN_POINT('Origin',(6.707089953,7.49999999999998,5.528881732));
#153218=CARTESIAN_POINT('',(4.639971864,7.49999999999998,7.269390422));
#153219=CARTESIAN_POINT('Origin',(1.19142778,7.49999999999998,8.610115487));
#153220=CARTESIAN_POINT('',(5.015144041,7.49999999999998,7.015818288));
#153221=CARTESIAN_POINT('Origin',(2.22044604925031E-15,7.49999999999998,
2.22044604925031E-15));
#153222=CARTESIAN_POINT('Origin',(7.545000119,7.49999999999998,4.315850098));
#153223=CARTESIAN_POINT('',(5.801763037,7.49999999999998,6.380667807));
#153224=CARTESIAN_POINT('Origin',(2.629406756,7.49999999999998,8.284914542));
#153225=CARTESIAN_POINT('',(6.128684805,7.49999999999998,6.067338672));
#153226=CARTESIAN_POINT('Origin',(2.22044604925031E-15,7.49999999999998,
2.22044604925031E-15));
#153227=CARTESIAN_POINT('Origin',(8.165854367,7.49999999999998,2.978659314));
#153228=CARTESIAN_POINT('',(6.796648051,7.49999999999998,5.308384996));
#153229=CARTESIAN_POINT('Origin',(3.991742488,7.49999999999998,7.721371689));
#153230=CARTESIAN_POINT('',(7.065914466,7.49999999999998,4.944312769));
#153231=CARTESIAN_POINT('Origin',(2.22044604925031E-15,7.49999999999998,
2.22044604925031E-15));
#153232=CARTESIAN_POINT('Origin',(8.551791853,7.49999999999998,1.555777924));
#153233=CARTESIAN_POINT('',(7.596005875,7.49999999999998,4.083389615));
#153234=CARTESIAN_POINT('Origin',(5.239243055,7.49999999999998,6.935699032));
#153235=CARTESIAN_POINT('',(7.799870633,7.49999999999998,3.679047989));
#153236=CARTESIAN_POINT('Origin',(2.22044604925031E-15,7.49999999999998,
2.22044604925031E-15));
#153237=CARTESIAN_POINT('Origin',(8.691709858,7.49999999999998,0.088139637000002));
#153238=CARTESIAN_POINT('',(8.17684044,7.49999999999998,2.740922548));
#153239=CARTESIAN_POINT('Origin',(6.33602014,7.49999999999998,5.950498941));
#153240=CARTESIAN_POINT('',(8.309438723,7.49999999999998,2.307943698));
#153241=CARTESIAN_POINT('Origin',(2.22044604925031E-15,7.49999999999998,
2.22044604925031E-15));
#153242=CARTESIAN_POINT('Origin',(8.581583195,7.49999999999998,-1.382034268));
#153243=CARTESIAN_POINT('',(8.522442193,7.49999999999998,1.31960413));
#153244=CARTESIAN_POINT('Origin',(7.25052146,7.49999999999998,4.794113829));
#153245=CARTESIAN_POINT('',(8.579959389,7.49999999999998,0.870444068000003));
#153246=CARTESIAN_POINT('Origin',(2.22044604925031E-15,7.49999999999998,
2.22044604925031E-15));
#153247=CARTESIAN_POINT('Origin',(8.224580008,7.49999999999998,-2.812449563));
#153248=CARTESIAN_POINT('',(8.622868801,7.49999999999998,-0.139676895));
#153249=CARTESIAN_POINT('Origin',(7.956438479,7.49999999999998,3.499810792));
#153250=CARTESIAN_POINT('Origin',(2.22044604925031E-15,7.49999999999998,
2.22044604925031E-15));
#153251=CARTESIAN_POINT('Origin',(2.22044604925031E-15,17.5,2.22044604925031E-15));
#153252=CARTESIAN_POINT('',(0.978452338000002,2.49999999999998,-9.700779918));
#153253=CARTESIAN_POINT('',(0.675061572000001,7.49999999999998,-9.726602278));
#153254=CARTESIAN_POINT('Origin',(-3.834338166,2.49999999999998,-7.800733278));
#153255=CARTESIAN_POINT('',(-0.226413884999999,2.49999999999998,-8.621027361));
#153256=CARTESIAN_POINT('Origin',(3.834338166,2.49999999999998,-7.800733278));
#153257=CARTESIAN_POINT('',(0.226413885000002,2.49999999999998,-8.621027361));
#153258=CARTESIAN_POINT('Origin',(2.22044604925031E-15,2.49999999999998,
2.22044604925031E-15));
#153259=CARTESIAN_POINT('Origin',(-2.460854379,2.49999999999998,-8.336533127));
#153260=CARTESIAN_POINT('',(1.233803568,2.49999999999998,-8.535285863));
#153261=CARTESIAN_POINT('Origin',(5.097515025,2.49999999999998,-7.040520536));
#153262=CARTESIAN_POINT('',(1.680117823,2.49999999999998,-8.458757598));
#153263=CARTESIAN_POINT('Origin',(2.22044604925031E-15,2.49999999999998,
2.22044604925031E-15));
#153264=CARTESIAN_POINT('Origin',(-7.956438479,2.49999999999998,3.499810792));
#153265=CARTESIAN_POINT('',(-8.622868801,2.49999999999998,-0.139676895));
#153266=CARTESIAN_POINT('Origin',(-7.630970629,2.49999999999998,-4.161955804));
#153267=CARTESIAN_POINT('',(-8.603650246,2.49999999999998,-0.592096651999998));
#153268=CARTESIAN_POINT('Origin',(2.22044604925031E-15,2.49999999999998,
2.22044604925031E-15));
#153269=CARTESIAN_POINT('Origin',(-8.43346325,2.49999999999998,2.10482457));
#153270=CARTESIAN_POINT('',(-8.475231174,2.49999999999998,-1.594939671));
#153271=CARTESIAN_POINT('Origin',(-6.817832118,2.49999999999998,-5.391730155));
#153272=CARTESIAN_POINT('',(-8.379829749,2.49999999999998,-2.03760383));
#153273=CARTESIAN_POINT('Origin',(2.22044604925031E-15,2.49999999999998,
2.22044604925031E-15));
#153274=CARTESIAN_POINT('Origin',(-8.667872637,2.49999999999998,0.649286377));
#153275=CARTESIAN_POINT('',(-8.083776576,2.49999999999998,-3.004318937));
#153276=CARTESIAN_POINT('Origin',(-5.808556991,2.49999999999998,-6.466394246));
#153277=CARTESIAN_POINT('',(-7.914936808,2.49999999999998,-3.424492856));
#153278=CARTESIAN_POINT('Origin',(2.22044604925031E-15,2.49999999999998,
2.22044604925031E-15));
#153279=CARTESIAN_POINT('Origin',(-8.65292311,2.49999999999998,-0.824930601999998));
#153280=CARTESIAN_POINT('',(-7.459766444,2.49999999999998,-4.327269417));
#153281=CARTESIAN_POINT('Origin',(-4.632180254,2.49999999999998,-7.355031947));
#153282=CARTESIAN_POINT('',(-7.222345546,2.49999999999998,-4.712865457));
#153283=CARTESIAN_POINT('Origin',(2.22044604925031E-15,2.49999999999998,
2.22044604925031E-15));
#153284=CARTESIAN_POINT('Origin',(-5.097515025,2.49999999999998,-7.040520536));
#153285=CARTESIAN_POINT('',(-1.680117823,2.49999999999998,-8.458757598));
#153286=CARTESIAN_POINT('Origin',(2.460854379,2.49999999999998,-8.336533127));
#153287=CARTESIAN_POINT('',(-1.233803569,2.49999999999998,-8.535285862));
#153288=CARTESIAN_POINT('Origin',(2.22044604925031E-15,2.49999999999998,
2.22044604925031E-15));
#153289=CARTESIAN_POINT('Origin',(-6.214045658,2.49999999999998,-6.077764837));
#153290=CARTESIAN_POINT('',(-3.085487831,2.49999999999998,-8.05314478));
#153291=CARTESIAN_POINT('Origin',(1.016576292,2.49999999999998,-8.632506096));
#153292=CARTESIAN_POINT('',(-2.65852674,2.49999999999998,-8.20399973));
#153293=CARTESIAN_POINT('Origin',(2.22044604925031E-15,2.49999999999998,
2.22044604925031E-15));
#153294=CARTESIAN_POINT('Origin',(-7.151809512,2.49999999999998,-4.940162908));
#153295=CARTESIAN_POINT('',(-4.402093971,2.49999999999998,-7.415857649));
#153296=CARTESIAN_POINT('Origin',(-0.456946843999999,2.49999999999998,-8.680137582));
#153297=CARTESIAN_POINT('',(-4.006768937,2.49999999999998,-7.636699463));
#153298=CARTESIAN_POINT('Origin',(2.22044604925031E-15,2.49999999999998,
2.22044604925031E-15));
#153299=CARTESIAN_POINT('Origin',(-8.38904474,2.49999999999998,-2.275415831));
#153300=CARTESIAN_POINT('',(-6.621152413,2.49999999999998,-5.525732234));
#153301=CARTESIAN_POINT('Origin',(-3.322544125,2.49999999999998,-8.032078771));
#153302=CARTESIAN_POINT('',(-6.321980552,2.49999999999998,-5.8656575));
#153303=CARTESIAN_POINT('Origin',(2.22044604925031E-15,2.49999999999998,
2.22044604925031E-15));
#153304=CARTESIAN_POINT('Origin',(-7.883828827,2.49999999999998,-3.660441488));
#153305=CARTESIAN_POINT('',(-5.592059883,2.49999999999998,-6.565229795));
#153306=CARTESIAN_POINT('Origin',(-1.917324452,2.49999999999998,-8.478057313));
#153307=CARTESIAN_POINT('',(-5.239743688,2.49999999999998,-6.849705256));
#153308=CARTESIAN_POINT('Origin',(2.22044604925031E-15,2.49999999999998,
2.22044604925031E-15));
#153309=CARTESIAN_POINT('Origin',(3.158976522,2.49999999999998,8.09780564));
#153310=CARTESIAN_POINT('',(-0.505515968999999,2.49999999999998,8.60917125));
#153311=CARTESIAN_POINT('Origin',(-4.482073316,2.49999999999998,7.447456454));
#153312=CARTESIAN_POINT('',(-0.956712421999999,2.49999999999998,8.570768772));
#153313=CARTESIAN_POINT('Origin',(2.22044604925031E-15,2.49999999999998,
2.22044604925031E-15));
#153314=CARTESIAN_POINT('Origin',(1.745001724,2.49999999999998,8.515195702));
#153315=CARTESIAN_POINT('',(-1.953201585,2.49999999999998,8.399903545));
#153316=CARTESIAN_POINT('Origin',(-5.676229022,2.49999999999998,6.582857506));
#153317=CARTESIAN_POINT('',(-2.391417938,2.49999999999998,8.285800881));
#153318=CARTESIAN_POINT('Origin',(2.22044604925031E-15,2.49999999999998,
2.22044604925031E-15));
#153319=CARTESIAN_POINT('Origin',(-1.19142778,2.49999999999998,8.610115487));
#153320=CARTESIAN_POINT('',(-4.639971864,2.49999999999998,7.269390422));
#153321=CARTESIAN_POINT('Origin',(-7.545000119,2.49999999999998,4.315850098));
#153322=CARTESIAN_POINT('',(-5.015144041,2.49999999999998,7.015818288));
#153323=CARTESIAN_POINT('Origin',(2.22044604925031E-15,2.49999999999998,
2.22044604925031E-15));
#153324=CARTESIAN_POINT('Origin',(0.280826404000001,2.49999999999998,8.687619086));
#153325=CARTESIAN_POINT('',(-3.344697148,2.49999999999998,7.948985909));
#153326=CARTESIAN_POINT('Origin',(-6.707089953,2.49999999999998,5.528881732));
#153327=CARTESIAN_POINT('',(-3.757326714,2.49999999999998,7.762465586));
#153328=CARTESIAN_POINT('Origin',(2.22044604925031E-15,2.49999999999998,
2.22044604925031E-15));
#153329=CARTESIAN_POINT('Origin',(-7.25052146,2.49999999999998,4.794113829));
#153330=CARTESIAN_POINT('',(-8.522442193,2.49999999999998,1.31960413));
#153331=CARTESIAN_POINT('Origin',(-8.224580008,2.49999999999998,-2.812449563));
#153332=CARTESIAN_POINT('',(-8.579959389,2.49999999999998,0.870444068000003));
#153333=CARTESIAN_POINT('Origin',(2.22044604925031E-15,2.49999999999998,
2.22044604925031E-15));
#153334=CARTESIAN_POINT('Origin',(-6.33602014,2.49999999999998,5.950498941));
#153335=CARTESIAN_POINT('',(-8.17684044,2.49999999999998,2.740922548));
#153336=CARTESIAN_POINT('Origin',(-8.581583195,2.49999999999998,-1.382034268));
#153337=CARTESIAN_POINT('',(-8.309438723,2.49999999999998,2.307943698));
#153338=CARTESIAN_POINT('Origin',(2.22044604925031E-15,2.49999999999998,
2.22044604925031E-15));
#153339=CARTESIAN_POINT('Origin',(-5.239243055,2.49999999999998,6.935699032));
#153340=CARTESIAN_POINT('',(-7.596005875,2.49999999999998,4.083389615));
#153341=CARTESIAN_POINT('Origin',(-8.691709858,2.49999999999998,0.088139637000002));
#153342=CARTESIAN_POINT('',(-7.799870633,2.49999999999998,3.67904799));
#153343=CARTESIAN_POINT('Origin',(2.22044604925031E-15,2.49999999999998,
2.22044604925031E-15));
#153344=CARTESIAN_POINT('Origin',(-2.629406756,2.49999999999998,8.284914542));
#153345=CARTESIAN_POINT('',(-5.801763037,2.49999999999998,6.380667807));
#153346=CARTESIAN_POINT('Origin',(-8.165854367,2.49999999999998,2.978659314));
#153347=CARTESIAN_POINT('',(-6.128684805,2.49999999999998,6.067338672));
#153348=CARTESIAN_POINT('Origin',(2.22044604925031E-15,2.49999999999998,
2.22044604925031E-15));
#153349=CARTESIAN_POINT('Origin',(-3.991742488,2.49999999999998,7.721371689));
#153350=CARTESIAN_POINT('',(-6.796648051,2.49999999999998,5.308384996));
#153351=CARTESIAN_POINT('Origin',(-8.551791853,2.49999999999998,1.555777924));
#153352=CARTESIAN_POINT('',(-7.065914466,2.49999999999998,4.944312768));
#153353=CARTESIAN_POINT('Origin',(2.22044604925031E-15,2.49999999999998,
2.22044604925031E-15));
#153354=CARTESIAN_POINT('Origin',(8.224580008,2.49999999999998,-2.812449563));
#153355=CARTESIAN_POINT('',(8.579959389,2.49999999999998,0.870444068000003));
#153356=CARTESIAN_POINT('Origin',(7.25052146,2.49999999999998,4.794113829));
#153357=CARTESIAN_POINT('',(8.522442193,2.49999999999998,1.31960413));
#153358=CARTESIAN_POINT('Origin',(2.22044604925031E-15,2.49999999999998,
2.22044604925031E-15));
#153359=CARTESIAN_POINT('Origin',(8.581583195,2.49999999999998,-1.382034268));
#153360=CARTESIAN_POINT('',(8.309438723,2.49999999999998,2.307943698));
#153361=CARTESIAN_POINT('Origin',(6.33602014,2.49999999999998,5.950498941));
#153362=CARTESIAN_POINT('',(8.17684044,2.49999999999998,2.740922548));
#153363=CARTESIAN_POINT('Origin',(2.22044604925031E-15,2.49999999999998,
2.22044604925031E-15));
#153364=CARTESIAN_POINT('Origin',(8.551791853,2.49999999999998,1.555777924));
#153365=CARTESIAN_POINT('',(7.065914466,2.49999999999998,4.944312769));
#153366=CARTESIAN_POINT('Origin',(3.991742488,2.49999999999998,7.721371689));
#153367=CARTESIAN_POINT('',(6.796648051,2.49999999999998,5.308384996));
#153368=CARTESIAN_POINT('Origin',(2.22044604925031E-15,2.49999999999998,
2.22044604925031E-15));
#153369=CARTESIAN_POINT('Origin',(8.691709858,2.49999999999998,0.088139637000002));
#153370=CARTESIAN_POINT('',(7.799870633,2.49999999999998,3.679047989));
#153371=CARTESIAN_POINT('Origin',(5.239243055,2.49999999999998,6.935699032));
#153372=CARTESIAN_POINT('',(7.596005875,2.49999999999998,4.083389615));
#153373=CARTESIAN_POINT('Origin',(2.22044604925031E-15,2.49999999999998,
2.22044604925031E-15));
#153374=CARTESIAN_POINT('Origin',(4.482073316,2.49999999999998,7.447456454));
#153375=CARTESIAN_POINT('',(0.956712422000002,2.49999999999998,8.570768772));
#153376=CARTESIAN_POINT('Origin',(-3.158976522,2.49999999999998,8.09780564));
#153377=CARTESIAN_POINT('',(0.505515969000001,2.49999999999998,8.60917125));
#153378=CARTESIAN_POINT('Origin',(2.22044604925031E-15,2.49999999999998,
2.22044604925031E-15));
#153379=CARTESIAN_POINT('Origin',(5.676229022,2.49999999999998,6.582857506));
#153380=CARTESIAN_POINT('',(2.391417938,2.49999999999998,8.285800881));
#153381=CARTESIAN_POINT('Origin',(2.22044604925031E-15,2.49999999999998,
2.22044604925031E-15));
#153382=CARTESIAN_POINT('Origin',(6.707089953,2.49999999999998,5.528881732));
#153383=CARTESIAN_POINT('',(3.757326714,2.49999999999998,7.762465586));
#153384=CARTESIAN_POINT('Origin',(2.22044604925031E-15,2.49999999999998,
2.22044604925031E-15));
#153385=CARTESIAN_POINT('Origin',(8.165854367,2.49999999999998,2.978659314));
#153386=CARTESIAN_POINT('',(6.128684805,2.49999999999998,6.067338672));
#153387=CARTESIAN_POINT('Origin',(2.629406756,2.49999999999998,8.284914542));
#153388=CARTESIAN_POINT('',(5.801763037,2.49999999999998,6.380667807));
#153389=CARTESIAN_POINT('Origin',(2.22044604925031E-15,2.49999999999998,
2.22044604925031E-15));
#153390=CARTESIAN_POINT('Origin',(7.545000119,2.49999999999998,4.315850098));
#153391=CARTESIAN_POINT('',(5.015144041,2.49999999999998,7.015818288));
#153392=CARTESIAN_POINT('Origin',(1.19142778,2.49999999999998,8.610115487));
#153393=CARTESIAN_POINT('',(4.639971864,2.49999999999998,7.269390422));
#153394=CARTESIAN_POINT('Origin',(2.22044604925031E-15,2.49999999999998,
2.22044604925031E-15));
#153395=CARTESIAN_POINT('Origin',(1.917324452,2.49999999999998,-8.478057313));
#153396=CARTESIAN_POINT('',(5.239743687,2.49999999999998,-6.849705256));
#153397=CARTESIAN_POINT('Origin',(7.883828827,2.49999999999998,-3.660441488));
#153398=CARTESIAN_POINT('',(5.592059883,2.49999999999998,-6.565229795));
#153399=CARTESIAN_POINT('Origin',(2.22044604925031E-15,2.49999999999998,
2.22044604925031E-15));
#153400=CARTESIAN_POINT('Origin',(3.322544125,2.49999999999998,-8.032078771));
#153401=CARTESIAN_POINT('',(6.321980552,2.49999999999998,-5.8656575));
#153402=CARTESIAN_POINT('Origin',(8.38904474,2.49999999999998,-2.275415831));
#153403=CARTESIAN_POINT('',(6.621152413,2.49999999999998,-5.525732234));
#153404=CARTESIAN_POINT('Origin',(2.22044604925031E-15,2.49999999999998,
2.22044604925031E-15));
#153405=CARTESIAN_POINT('Origin',(7.151809512,2.49999999999998,-4.940162908));
#153406=CARTESIAN_POINT('',(4.402093972,2.49999999999998,-7.415857648));
#153407=CARTESIAN_POINT('Origin',(2.22044604925031E-15,2.49999999999998,
2.22044604925031E-15));
#153408=CARTESIAN_POINT('Origin',(6.214045658,2.49999999999998,-6.077764837));
#153409=CARTESIAN_POINT('',(3.085487831,2.49999999999998,-8.05314478));
#153410=CARTESIAN_POINT('Origin',(2.22044604925031E-15,2.49999999999998,
2.22044604925031E-15));
#153411=CARTESIAN_POINT('Origin',(4.632180254,2.49999999999998,-7.355031947));
#153412=CARTESIAN_POINT('',(7.222345546,2.49999999999998,-4.712865457));
#153413=CARTESIAN_POINT('Origin',(8.65292311,2.49999999999998,-0.824930601999998));
#153414=CARTESIAN_POINT('',(7.459766444,2.49999999999998,-4.327269416));
#153415=CARTESIAN_POINT('Origin',(2.22044604925031E-15,2.49999999999998,
2.22044604925031E-15));
#153416=CARTESIAN_POINT('Origin',(5.808556991,2.49999999999998,-6.466394246));
#153417=CARTESIAN_POINT('',(7.914936808,2.49999999999998,-3.424492856));
#153418=CARTESIAN_POINT('Origin',(8.667872637,2.49999999999998,0.649286377));
#153419=CARTESIAN_POINT('',(8.083776576,2.49999999999998,-3.004318937));
#153420=CARTESIAN_POINT('Origin',(2.22044604925031E-15,2.49999999999998,
2.22044604925031E-15));
#153421=CARTESIAN_POINT('Origin',(6.817832118,2.49999999999998,-5.391730155));
#153422=CARTESIAN_POINT('',(8.37982975,2.49999999999998,-2.03760383));
#153423=CARTESIAN_POINT('Origin',(8.43346325,2.49999999999998,2.10482457));
#153424=CARTESIAN_POINT('',(8.475231174,2.49999999999998,-1.594939671));
#153425=CARTESIAN_POINT('Origin',(2.22044604925031E-15,2.49999999999998,
2.22044604925031E-15));
#153426=CARTESIAN_POINT('Origin',(7.630970629,2.49999999999998,-4.161955804));
#153427=CARTESIAN_POINT('',(8.603650246,2.49999999999998,-0.592096652999998));
#153428=CARTESIAN_POINT('Origin',(7.956438479,2.49999999999998,3.499810792));
#153429=CARTESIAN_POINT('',(8.622868801,2.49999999999998,-0.139676895));
#153430=CARTESIAN_POINT('Origin',(2.22044604925031E-15,2.49999999999998,
2.22044604925031E-15));
#153431=CARTESIAN_POINT('Origin',(2.22044604925031E-15,7.70005079999998,
2.22044604925031E-15));
#153432=CARTESIAN_POINT('Origin',(2.22044604925031E-15,-1.30000000000002,
2.22044604925031E-15));
#153433=CARTESIAN_POINT('Origin',(2.22044604925031E-15,-1.30000000000002,
2.22044604925031E-15));
#153434=CARTESIAN_POINT('Origin',(2.22044604925031E-15,5.19999999999998,
2.22044604925031E-15));
#153435=CARTESIAN_POINT('Origin',(-5.077182071,4.99999999999998,-1.795054936));
#153436=CARTESIAN_POINT('',(-5.077182071,4.99999999999998,-1.795054936));
#153437=CARTESIAN_POINT('',(-5.07718207126124,2.69999999999998,-1.7950549352611));
#153438=CARTESIAN_POINT('',(-5.077182071,4.99999999999998,-1.795054936));
#153439=CARTESIAN_POINT('',(-5.077182071,2.69999999999998,-1.795054936));
#153440=CARTESIAN_POINT('',(-6.4,4.99999999999998,-2.262741699));
#153441=CARTESIAN_POINT('Origin',(-4.943848737,4.99999999999998,-2.172178552));
#153442=CARTESIAN_POINT('',(-4.57763771968452,4.99999999999998,-2.0112764371543));
#153443=CARTESIAN_POINT('',(-4.57763772,2.69999999999998,-2.011276437));
#153444=CARTESIAN_POINT('',(-4.57763772,4.99999999999998,-2.011276437));
#153445=CARTESIAN_POINT('Origin',(-4.943848737,2.69999999999998,-2.172178552));
#153446=CARTESIAN_POINT('Origin',(-4.943848737,4.99999999999998,-2.172178552));
#153447=CARTESIAN_POINT('Origin',(2.22044604925031E-15,4.99999999999998,
2.22044604925031E-15));
#153448=CARTESIAN_POINT('',(4.57763772,4.99999999999998,-2.011276437));
#153449=CARTESIAN_POINT('',(4.57763772,2.69999999999998,-2.011276437));
#153450=CARTESIAN_POINT('',(4.57763772,4.99999999999998,-2.011276437));
#153451=CARTESIAN_POINT('Origin',(2.22044604925031E-15,2.69999999999998,
2.22044604925031E-15));
#153452=CARTESIAN_POINT('Origin',(2.22044604925031E-15,4.99999999999998,
2.22044604925031E-15));
#153453=CARTESIAN_POINT('Origin',(4.943848737,4.99999999999998,-2.172178552));
#153454=CARTESIAN_POINT('',(5.07718207041197,4.99999999999998,-1.79505493577758));
#153455=CARTESIAN_POINT('',(5.07718207057322,2.69999999999998,-1.79505493573434));
#153456=CARTESIAN_POINT('',(5.077182071,4.99999999999998,-1.795054936));
#153457=CARTESIAN_POINT('Origin',(4.943848737,2.69999999999998,-2.172178552));
#153458=CARTESIAN_POINT('Origin',(4.943848737,4.99999999999998,-2.172178552));
#153459=CARTESIAN_POINT('Origin',(6.4,4.99999999999998,-2.2627417));
#153460=CARTESIAN_POINT('',(6.4,4.99999999999998,-2.2627417));
#153461=CARTESIAN_POINT('',(6.4,4.99999999999998,-2.2627417));
#153462=CARTESIAN_POINT('',(6.4,2.69999999999998,-2.2627417));
#153463=CARTESIAN_POINT('',(5.07718207,4.99999999999998,-1.795054936));
#153464=CARTESIAN_POINT('Origin',(6.266666667,4.99999999999998,-2.639865316));
#153465=CARTESIAN_POINT('',(6.63529411796585,4.99999999999998,-2.79515151131894));
#153466=CARTESIAN_POINT('',(6.635294118,4.99999999999998,-2.795151512));
#153467=CARTESIAN_POINT('Origin',(6.266666667,4.99999999999998,-2.639865316));
#153468=CARTESIAN_POINT('Origin',(2.22044604925031E-15,4.99999999999998,
2.22044604925031E-15));
#153469=CARTESIAN_POINT('Origin',(2.22044604925031E-15,2.69999999999998,
2.22044604925031E-15));
#153470=CARTESIAN_POINT('Origin',(2.22044604925031E-15,4.99999999999998,
2.22044604925031E-15));
#153471=CARTESIAN_POINT('Origin',(-6.266666667,4.99999999999998,-2.639865316));
#153472=CARTESIAN_POINT('Origin',(-4.943848737,4.99999999999998,2.172178552));
#153473=CARTESIAN_POINT('',(-5.077182071,4.99999999999998,1.795054936));
#153474=CARTESIAN_POINT('',(-5.077182071,2.69999999999998,1.795054935));
#153475=CARTESIAN_POINT('',(-5.077182071,4.99999999999998,1.795054936));
#153476=CARTESIAN_POINT('',(-4.57763772,2.69999999999998,2.011276437));
#153477=CARTESIAN_POINT('Origin',(-4.943848737,2.69999999999998,2.172178552));
#153478=CARTESIAN_POINT('',(-4.57763772,4.99999999999998,2.011276437));
#153479=CARTESIAN_POINT('',(-4.57763772,4.99999999999998,2.011276437));
#153480=CARTESIAN_POINT('Origin',(-4.943848737,4.99999999999998,2.172178552));
#153481=CARTESIAN_POINT('Origin',(-5.077182071,4.99999999999998,1.795054936));
#153482=CARTESIAN_POINT('',(-6.4,2.69999999999998,2.262741699));
#153483=CARTESIAN_POINT('',(-5.077182071,4.99999999999998,1.795054936));
#153484=CARTESIAN_POINT('Origin',(2.22044604925031E-15,4.99999999999998,
2.22044604925031E-15));
#153485=CARTESIAN_POINT('',(6.63529411796585,4.99999999999998,2.79515151131895));
#153486=CARTESIAN_POINT('',(6.635294118,4.99999999999998,2.795151512));
#153487=CARTESIAN_POINT('Origin',(2.22044604925031E-15,2.69999999999998,
2.22044604925031E-15));
#153488=CARTESIAN_POINT('Origin',(2.22044604925031E-15,4.99999999999998,
2.22044604925031E-15));
#153489=CARTESIAN_POINT('Origin',(6.266666667,4.99999999999998,2.639865316));
#153490=CARTESIAN_POINT('',(6.40000000007864,4.99999999999998,2.26274169944424));
#153491=CARTESIAN_POINT('',(6.4,4.99999999999998,2.262741699));
#153492=CARTESIAN_POINT('Origin',(6.266666667,4.99999999999998,2.639865316));
#153493=CARTESIAN_POINT('Origin',(6.4,4.99999999999998,2.2627417));
#153494=CARTESIAN_POINT('',(5.07718207037154,4.99999999999998,1.79505493622526));
#153495=CARTESIAN_POINT('',(5.077182071,2.69999999999998,1.795054935));
#153496=CARTESIAN_POINT('',(5.077182071,4.99999999999998,1.795054937));
#153497=CARTESIAN_POINT('',(5.07718207,2.69999999999998,1.795054936));
#153498=CARTESIAN_POINT('',(6.4,4.99999999999998,2.2627417));
#153499=CARTESIAN_POINT('Origin',(4.943848737,4.99999999999998,2.172178552));
#153500=CARTESIAN_POINT('',(4.57763771968453,4.99999999999998,2.0112764371543));
#153501=CARTESIAN_POINT('',(4.57763772,2.69999999999998,2.011276437));
#153502=CARTESIAN_POINT('',(4.57763772,4.99999999999998,2.011276437));
#153503=CARTESIAN_POINT('Origin',(4.943848737,2.69999999999998,2.172178552));
#153504=CARTESIAN_POINT('Origin',(4.943848737,4.99999999999998,2.172178552));
#153505=CARTESIAN_POINT('Origin',(2.22044604925031E-15,4.99999999999998,
2.22044604925031E-15));
#153506=CARTESIAN_POINT('Origin',(2.22044604925031E-15,2.69999999999998,
2.22044604925031E-15));
#153507=CARTESIAN_POINT('Origin',(2.22044604925031E-15,4.99999999999998,
2.22044604925031E-15));
#153508=CARTESIAN_POINT('Origin',(-4.943848737,4.99999999999998,2.172178552));
#153509=CARTESIAN_POINT('Origin',(-6.266666667,2.69999999999998,-2.639865316));
#153510=CARTESIAN_POINT('Origin',(-6.819607843,2.69999999999998,-2.872794609));
#153511=CARTESIAN_POINT('Origin',(-6.466666668,2.69999999999998,-2.074179889));
#153512=CARTESIAN_POINT('Origin',(-0.0666666669999971,2.69999999999998,
0.188561808000001));
#153513=CARTESIAN_POINT('Origin',(-5.143848737,2.69999999999998,-1.606493127));
#153514=CARTESIAN_POINT('Origin',(2.22044604925031E-15,2.69999999999998,
2.22044604925031E-15));
#153515=CARTESIAN_POINT('Origin',(-4.943848737,2.69999999999998,-2.172178552));
#153516=CARTESIAN_POINT('Origin',(-4.394532211,2.69999999999998,-1.93082538));
#153517=CARTESIAN_POINT('Origin',(2.22044604925031E-15,2.69999999999998,
2.22044604925031E-15));
#153518=CARTESIAN_POINT('Origin',(4.394532211,2.69999999999998,-1.93082538));
#153519=CARTESIAN_POINT('Origin',(0.0666666670000016,2.69999999999998,0.188561808000001));
#153520=CARTESIAN_POINT('Origin',(5.143848738,2.69999999999998,-1.606493127));
#153521=CARTESIAN_POINT('Origin',(4.943848737,2.69999999999998,-2.172178552));
#153522=CARTESIAN_POINT('Origin',(4.943848737,2.69999999999998,2.172178552));
#153523=CARTESIAN_POINT('Origin',(5.143848738,2.69999999999998,1.606493125));
#153524=CARTESIAN_POINT('Origin',(4.394532211,2.69999999999998,1.93082538));
#153525=CARTESIAN_POINT('Origin',(2.22044604925031E-15,2.69999999999998,
2.22044604925031E-15));
#153526=CARTESIAN_POINT('Origin',(-4.394532211,2.69999999999998,1.93082538));
#153527=CARTESIAN_POINT('Origin',(0.0666666670000016,2.69999999999998,-0.188561808000001));
#153528=CARTESIAN_POINT('Origin',(-4.943848737,2.69999999999998,2.172178552));
#153529=CARTESIAN_POINT('Origin',(-5.143848738,2.69999999999998,1.606493125));
#153530=CARTESIAN_POINT('Origin',(-0.0666666669999971,2.69999999999998,
-0.188561808000001));
#153531=CARTESIAN_POINT('Origin',(-6.466666667,2.69999999999998,2.074179891));
#153532=CARTESIAN_POINT('Origin',(2.22044604925031E-15,2.69999999999998,
2.22044604925031E-15));
#153533=CARTESIAN_POINT('Origin',(-6.819607843,2.69999999999998,2.87279461));
#153534=CARTESIAN_POINT('Origin',(-6.266666667,2.69999999999998,2.639865316));
#153535=CARTESIAN_POINT('Origin',(6.,4.49999999999998,2.22044604925031E-15));
#153536=CARTESIAN_POINT('Origin',(-6.,4.49999999999998,2.22044604925031E-15));
#153537=CARTESIAN_POINT('',(0.,0.,0.));
#153538=CARTESIAN_POINT('Origin',(-5.66257110645729E-14,15.2,-1.77635683940025E-14));
#153539=CARTESIAN_POINT('',(0.710930733999944,15.2,-11.478004072));
#153540=CARTESIAN_POINT('',(1.09337742899994,15.2,-11.447904865));
#153541=CARTESIAN_POINT('Origin',(-5.66257110645729E-14,15.2,-1.77635683940025E-14));
#153542=CARTESIAN_POINT('',(1.09337742899994,12.2,-11.447904865));
#153543=CARTESIAN_POINT('',(1.09337742899994,15.2,-11.447904865));
#153544=CARTESIAN_POINT('',(0.710930733999944,12.2,-11.478004072));
#153545=CARTESIAN_POINT('Origin',(-5.66257110645729E-14,12.2,-1.77635683940025E-14));
#153546=CARTESIAN_POINT('',(0.710930733999944,15.2,-11.478004072));
#153547=CARTESIAN_POINT('Ctrl Pts',(0.292001928999944,15.2,-10.370890023));
#153548=CARTESIAN_POINT('Ctrl Pts',(0.292001928999944,11.6,-10.370890023));
#153549=CARTESIAN_POINT('Ctrl Pts',(0.292021795999944,15.2,-10.371063246));
#153550=CARTESIAN_POINT('Ctrl Pts',(0.292021795999944,11.6,-10.371063246));
#153551=CARTESIAN_POINT('Ctrl Pts',(0.292062308999944,15.2,-10.371415731));
#153552=CARTESIAN_POINT('Ctrl Pts',(0.292062308999944,11.6,-10.371415731));
#153553=CARTESIAN_POINT('Ctrl Pts',(0.292123960999945,15.2,-10.371949799));
#153554=CARTESIAN_POINT('Ctrl Pts',(0.292123960999945,11.6,-10.371949799));
#153555=CARTESIAN_POINT('Ctrl Pts',(0.292207546999944,15.2,-10.372669176));
#153556=CARTESIAN_POINT('Ctrl Pts',(0.292207546999944,11.6,-10.372669176));
#153557=CARTESIAN_POINT('Ctrl Pts',(0.292314179999943,15.2,-10.373578975));
#153558=CARTESIAN_POINT('Ctrl Pts',(0.292314179999943,11.6,-10.373578975));
#153559=CARTESIAN_POINT('Ctrl Pts',(0.292423468999944,15.2,-10.374503411));
#153560=CARTESIAN_POINT('Ctrl Pts',(0.292423468999944,11.6,-10.374503411));
#153561=CARTESIAN_POINT('Ctrl Pts',(0.292534811999945,15.2,-10.375437184));
#153562=CARTESIAN_POINT('Ctrl Pts',(0.292534811999945,11.6,-10.375437184));
#153563=CARTESIAN_POINT('Ctrl Pts',(0.292648222999944,15.2,-10.376380266));
#153564=CARTESIAN_POINT('Ctrl Pts',(0.292648222999944,11.6,-10.376380266));
#153565=CARTESIAN_POINT('Ctrl Pts',(0.292763716999945,15.2,-10.377332627));
#153566=CARTESIAN_POINT('Ctrl Pts',(0.292763716999945,11.6,-10.377332627));
#153567=CARTESIAN_POINT('Ctrl Pts',(0.292881308999944,15.2,-10.378294239));
#153568=CARTESIAN_POINT('Ctrl Pts',(0.292881308999944,11.6,-10.378294239));
#153569=CARTESIAN_POINT('Ctrl Pts',(0.293001014999945,15.2,-10.379265074));
#153570=CARTESIAN_POINT('Ctrl Pts',(0.293001014999945,11.6,-10.379265074));
#153571=CARTESIAN_POINT('Ctrl Pts',(0.293122845999945,15.2,-10.380245102));
#153572=CARTESIAN_POINT('Ctrl Pts',(0.293122845999945,11.6,-10.380245102));
#153573=CARTESIAN_POINT('Ctrl Pts',(0.293246819999944,15.2,-10.381234297));
#153574=CARTESIAN_POINT('Ctrl Pts',(0.293246819999944,11.6,-10.381234297));
#153575=CARTESIAN_POINT('Ctrl Pts',(0.293372948999944,15.2,-10.382232628));
#153576=CARTESIAN_POINT('Ctrl Pts',(0.293372948999944,11.6,-10.382232628));
#153577=CARTESIAN_POINT('Ctrl Pts',(0.293501248999943,15.2,-10.383240069));
#153578=CARTESIAN_POINT('Ctrl Pts',(0.293501248999943,11.6,-10.383240069));
#153579=CARTESIAN_POINT('Ctrl Pts',(0.293631731999945,15.2,-10.384256592));
#153580=CARTESIAN_POINT('Ctrl Pts',(0.293631731999945,11.6,-10.384256592));
#153581=CARTESIAN_POINT('Ctrl Pts',(0.293764412999945,15.2,-10.385282168));
#153582=CARTESIAN_POINT('Ctrl Pts',(0.293764412999945,11.6,-10.385282168));
#153583=CARTESIAN_POINT('Ctrl Pts',(0.293899306999944,15.2,-10.38631677));
#153584=CARTESIAN_POINT('Ctrl Pts',(0.293899306999944,11.6,-10.38631677));
#153585=CARTESIAN_POINT('Ctrl Pts',(0.294036426999943,15.2,-10.387360371));
#153586=CARTESIAN_POINT('Ctrl Pts',(0.294036426999943,11.6,-10.387360371));
#153587=CARTESIAN_POINT('Ctrl Pts',(0.294175786999944,15.2,-10.388412945));
#153588=CARTESIAN_POINT('Ctrl Pts',(0.294175786999944,11.6,-10.388412945));
#153589=CARTESIAN_POINT('Ctrl Pts',(0.294317400999944,15.2,-10.389474461));
#153590=CARTESIAN_POINT('Ctrl Pts',(0.294317400999944,11.6,-10.389474461));
#153591=CARTESIAN_POINT('Ctrl Pts',(0.294461281999944,15.2,-10.390544895));
#153592=CARTESIAN_POINT('Ctrl Pts',(0.294461281999944,11.6,-10.390544895));
#153593=CARTESIAN_POINT('Ctrl Pts',(0.294607443999944,15.2,-10.391624218));
#153594=CARTESIAN_POINT('Ctrl Pts',(0.294607443999944,11.6,-10.391624218));
#153595=CARTESIAN_POINT('Ctrl Pts',(0.294755900999943,15.2,-10.392712404));
#153596=CARTESIAN_POINT('Ctrl Pts',(0.294755900999943,11.6,-10.392712404));
#153597=CARTESIAN_POINT('Ctrl Pts',(0.294906665999944,15.2,-10.393809427));
#153598=CARTESIAN_POINT('Ctrl Pts',(0.294906665999944,11.6,-10.393809427));
#153599=CARTESIAN_POINT('Ctrl Pts',(0.295059751999943,15.2,-10.394915259));
#153600=CARTESIAN_POINT('Ctrl Pts',(0.295059751999943,11.6,-10.394915259));
#153601=CARTESIAN_POINT('Ctrl Pts',(0.295215172999944,15.2,-10.396029875));
#153602=CARTESIAN_POINT('Ctrl Pts',(0.295215172999944,11.6,-10.396029875));
#153603=CARTESIAN_POINT('Ctrl Pts',(0.295372941999944,15.2,-10.397153247));
#153604=CARTESIAN_POINT('Ctrl Pts',(0.295372941999944,11.6,-10.397153247));
#153605=CARTESIAN_POINT('Ctrl Pts',(0.295533071999945,15.2,-10.39828535));
#153606=CARTESIAN_POINT('Ctrl Pts',(0.295533071999945,11.6,-10.39828535));
#153607=CARTESIAN_POINT('Ctrl Pts',(0.295695575999944,15.2,-10.399426157));
#153608=CARTESIAN_POINT('Ctrl Pts',(0.295695575999944,11.6,-10.399426157));
#153609=CARTESIAN_POINT('Ctrl Pts',(0.295860466999944,15.2,-10.400575642));
#153610=CARTESIAN_POINT('Ctrl Pts',(0.295860466999944,11.6,-10.400575642));
#153611=CARTESIAN_POINT('Ctrl Pts',(0.296027758999945,15.2,-10.401733778));
#153612=CARTESIAN_POINT('Ctrl Pts',(0.296027758999945,11.6,-10.401733778));
#153613=CARTESIAN_POINT('Ctrl Pts',(0.296197462999944,15.2,-10.402900542));
#153614=CARTESIAN_POINT('Ctrl Pts',(0.296197462999944,11.6,-10.402900542));
#153615=CARTESIAN_POINT('Ctrl Pts',(0.296369592999944,15.2,-10.404075906));
#153616=CARTESIAN_POINT('Ctrl Pts',(0.296369592999944,11.6,-10.404075906));
#153617=CARTESIAN_POINT('Ctrl Pts',(0.296544161999943,15.2,-10.405259845));
#153618=CARTESIAN_POINT('Ctrl Pts',(0.296544161999943,11.6,-10.405259845));
#153619=CARTESIAN_POINT('Ctrl Pts',(0.296721181999944,15.2,-10.406452335));
#153620=CARTESIAN_POINT('Ctrl Pts',(0.296721181999944,11.6,-10.406452335));
#153621=CARTESIAN_POINT('Ctrl Pts',(0.296900663999944,15.2,-10.407653347));
#153622=CARTESIAN_POINT('Ctrl Pts',(0.296900663999944,11.6,-10.407653347));
#153623=CARTESIAN_POINT('Ctrl Pts',(0.297082623999945,15.2,-10.408862859));
#153624=CARTESIAN_POINT('Ctrl Pts',(0.297082623999945,11.6,-10.408862859));
#153625=CARTESIAN_POINT('Ctrl Pts',(0.297267072999944,15.2,-10.410080845));
#153626=CARTESIAN_POINT('Ctrl Pts',(0.297267072999944,11.6,-10.410080845));
#153627=CARTESIAN_POINT('Ctrl Pts',(0.297454020999943,15.2,-10.411307279));
#153628=CARTESIAN_POINT('Ctrl Pts',(0.297454020999943,11.6,-10.411307279));
#153629=CARTESIAN_POINT('Ctrl Pts',(0.297643483999943,15.2,-10.412542137));
#153630=CARTESIAN_POINT('Ctrl Pts',(0.297643483999943,11.6,-10.412542137));
#153631=CARTESIAN_POINT('Ctrl Pts',(0.297835472999944,15.2,-10.413785393));
#153632=CARTESIAN_POINT('Ctrl Pts',(0.297835472999944,11.6,-10.413785393));
#153633=CARTESIAN_POINT('Ctrl Pts',(0.298029997999943,15.2,-10.415037024));
#153634=CARTESIAN_POINT('Ctrl Pts',(0.298029997999943,11.6,-10.415037024));
#153635=CARTESIAN_POINT('Ctrl Pts',(0.298227073999945,15.2,-10.416297005));
#153636=CARTESIAN_POINT('Ctrl Pts',(0.298227073999945,11.6,-10.416297005));
#153637=CARTESIAN_POINT('Ctrl Pts',(0.298426710999945,15.2,-10.41756531));
#153638=CARTESIAN_POINT('Ctrl Pts',(0.298426710999945,11.6,-10.41756531));
#153639=CARTESIAN_POINT('Ctrl Pts',(0.298628921999944,15.2,-10.418841915));
#153640=CARTESIAN_POINT('Ctrl Pts',(0.298628921999944,11.6,-10.418841915));
#153641=CARTESIAN_POINT('Ctrl Pts',(0.298833718999945,15.2,-10.420126796));
#153642=CARTESIAN_POINT('Ctrl Pts',(0.298833718999945,11.6,-10.420126796));
#153643=CARTESIAN_POINT('Ctrl Pts',(0.299041113999945,15.2,-10.421419931));
#153644=CARTESIAN_POINT('Ctrl Pts',(0.299041113999945,11.6,-10.421419931));
#153645=CARTESIAN_POINT('Ctrl Pts',(0.299251117999945,15.2,-10.422721292));
#153646=CARTESIAN_POINT('Ctrl Pts',(0.299251117999945,11.6,-10.422721292));
#153647=CARTESIAN_POINT('Ctrl Pts',(0.299463742999944,15.2,-10.424030856));
#153648=CARTESIAN_POINT('Ctrl Pts',(0.299463742999944,11.6,-10.424030856));
#153649=CARTESIAN_POINT('Ctrl Pts',(0.299679000999945,15.2,-10.425348601));
#153650=CARTESIAN_POINT('Ctrl Pts',(0.299679000999945,11.6,-10.425348601));
#153651=CARTESIAN_POINT('Ctrl Pts',(0.299896902999944,15.2,-10.426674502));
#153652=CARTESIAN_POINT('Ctrl Pts',(0.299896902999944,11.6,-10.426674502));
#153653=CARTESIAN_POINT('Ctrl Pts',(0.300117460999945,15.2,-10.428008535));
#153654=CARTESIAN_POINT('Ctrl Pts',(0.300117460999945,11.6,-10.428008535));
#153655=CARTESIAN_POINT('Ctrl Pts',(0.300340685999944,15.2,-10.429350676));
#153656=CARTESIAN_POINT('Ctrl Pts',(0.300340685999944,11.6,-10.429350676));
#153657=CARTESIAN_POINT('Ctrl Pts',(0.300566589999944,15.2,-10.430700902));
#153658=CARTESIAN_POINT('Ctrl Pts',(0.300566589999944,11.6,-10.430700902));
#153659=CARTESIAN_POINT('Ctrl Pts',(0.300795183999943,15.2,-10.43205919));
#153660=CARTESIAN_POINT('Ctrl Pts',(0.300795183999943,11.6,-10.43205919));
#153661=CARTESIAN_POINT('Ctrl Pts',(0.301026478999944,15.2,-10.433425516));
#153662=CARTESIAN_POINT('Ctrl Pts',(0.301026478999944,11.6,-10.433425516));
#153663=CARTESIAN_POINT('Ctrl Pts',(0.301260486999944,15.2,-10.434799858));
#153664=CARTESIAN_POINT('Ctrl Pts',(0.301260486999944,11.6,-10.434799858));
#153665=CARTESIAN_POINT('Ctrl Pts',(0.301497219999945,15.2,-10.43618219));
#153666=CARTESIAN_POINT('Ctrl Pts',(0.301497219999945,11.6,-10.43618219));
#153667=CARTESIAN_POINT('Ctrl Pts',(0.301736685999944,15.2,-10.437572491));
#153668=CARTESIAN_POINT('Ctrl Pts',(0.301736685999944,11.6,-10.437572491));
#153669=CARTESIAN_POINT('Ctrl Pts',(0.301978897999945,15.2,-10.438970738));
#153670=CARTESIAN_POINT('Ctrl Pts',(0.301978897999945,11.6,-10.438970738));
#153671=CARTESIAN_POINT('Ctrl Pts',(0.302223867999943,15.2,-10.440376907));
#153672=CARTESIAN_POINT('Ctrl Pts',(0.302223867999943,11.6,-10.440376907));
#153673=CARTESIAN_POINT('Ctrl Pts',(0.302471604999944,15.2,-10.441790977));
#153674=CARTESIAN_POINT('Ctrl Pts',(0.302471604999944,11.6,-10.441790977));
#153675=CARTESIAN_POINT('Ctrl Pts',(0.302722120999944,15.2,-10.443212923));
#153676=CARTESIAN_POINT('Ctrl Pts',(0.302722120999944,11.6,-10.443212923));
#153677=CARTESIAN_POINT('Ctrl Pts',(0.302975424999945,15.2,-10.444642725));
#153678=CARTESIAN_POINT('Ctrl Pts',(0.302975424999945,11.6,-10.444642725));
#153679=CARTESIAN_POINT('Ctrl Pts',(0.303231531999945,15.2,-10.446080357));
#153680=CARTESIAN_POINT('Ctrl Pts',(0.303231531999945,11.6,-10.446080357));
#153681=CARTESIAN_POINT('Ctrl Pts',(0.303490447999945,15.2,-10.447525799));
#153682=CARTESIAN_POINT('Ctrl Pts',(0.303490447999945,11.6,-10.447525799));
#153683=CARTESIAN_POINT('Ctrl Pts',(0.303752185999944,15.2,-10.448979029));
#153684=CARTESIAN_POINT('Ctrl Pts',(0.303752185999944,11.6,-10.448979029));
#153685=CARTESIAN_POINT('Ctrl Pts',(0.304016755999944,15.2,-10.450440023));
#153686=CARTESIAN_POINT('Ctrl Pts',(0.304016755999944,11.6,-10.450440023));
#153687=CARTESIAN_POINT('Ctrl Pts',(0.304284168999944,15.2,-10.451908761));
#153688=CARTESIAN_POINT('Ctrl Pts',(0.304284168999944,11.6,-10.451908761));
#153689=CARTESIAN_POINT('Ctrl Pts',(0.304554434999943,15.2,-10.453385218));
#153690=CARTESIAN_POINT('Ctrl Pts',(0.304554434999943,11.6,-10.453385218));
#153691=CARTESIAN_POINT('Ctrl Pts',(0.304827565999943,15.2,-10.454869375));
#153692=CARTESIAN_POINT('Ctrl Pts',(0.304827565999943,11.6,-10.454869375));
#153693=CARTESIAN_POINT('Ctrl Pts',(0.305103568999944,15.2,-10.456361208));
#153694=CARTESIAN_POINT('Ctrl Pts',(0.305103568999944,11.6,-10.456361208));
#153695=CARTESIAN_POINT('Ctrl Pts',(0.305382456999944,15.2,-10.457860694));
#153696=CARTESIAN_POINT('Ctrl Pts',(0.305382456999944,11.6,-10.457860694));
#153697=CARTESIAN_POINT('Ctrl Pts',(0.305664239999944,15.2,-10.459367814));
#153698=CARTESIAN_POINT('Ctrl Pts',(0.305664239999944,11.6,-10.459367814));
#153699=CARTESIAN_POINT('Ctrl Pts',(0.305948927999945,15.2,-10.460882546));
#153700=CARTESIAN_POINT('Ctrl Pts',(0.305948927999945,11.6,-10.460882546));
#153701=CARTESIAN_POINT('Ctrl Pts',(0.306236529999945,15.2,-10.462404866));
#153702=CARTESIAN_POINT('Ctrl Pts',(0.306236529999945,11.6,-10.462404866));
#153703=CARTESIAN_POINT('Ctrl Pts',(0.306527057999944,15.2,-10.463934755));
#153704=CARTESIAN_POINT('Ctrl Pts',(0.306527057999944,11.6,-10.463934755));
#153705=CARTESIAN_POINT('Ctrl Pts',(0.306820520999944,15.2,-10.46547219));
#153706=CARTESIAN_POINT('Ctrl Pts',(0.306820520999944,11.6,-10.46547219));
#153707=CARTESIAN_POINT('Ctrl Pts',(0.307116928999944,15.2,-10.46701715));
#153708=CARTESIAN_POINT('Ctrl Pts',(0.307116928999944,11.6,-10.46701715));
#153709=CARTESIAN_POINT('Ctrl Pts',(0.307416291999945,15.2,-10.468569615));
#153710=CARTESIAN_POINT('Ctrl Pts',(0.307416291999945,11.6,-10.468569615));
#153711=CARTESIAN_POINT('Ctrl Pts',(0.307718619999945,15.2,-10.470129561));
#153712=CARTESIAN_POINT('Ctrl Pts',(0.307718619999945,11.6,-10.470129561));
#153713=CARTESIAN_POINT('Ctrl Pts',(0.308023921999944,15.2,-10.47169697));
#153714=CARTESIAN_POINT('Ctrl Pts',(0.308023921999944,11.6,-10.47169697));
#153715=CARTESIAN_POINT('Ctrl Pts',(0.308332209999945,15.2,-10.473271818));
#153716=CARTESIAN_POINT('Ctrl Pts',(0.308332209999945,11.6,-10.473271818));
#153717=CARTESIAN_POINT('Ctrl Pts',(0.308643490999945,15.2,-10.474854086));
#153718=CARTESIAN_POINT('Ctrl Pts',(0.308643490999945,11.6,-10.474854086));
#153719=CARTESIAN_POINT('Ctrl Pts',(0.308957776999945,15.2,-10.476443753));
#153720=CARTESIAN_POINT('Ctrl Pts',(0.308957776999945,11.6,-10.476443753));
#153721=CARTESIAN_POINT('Ctrl Pts',(0.309275075999944,15.2,-10.478040796));
#153722=CARTESIAN_POINT('Ctrl Pts',(0.309275075999944,11.6,-10.478040796));
#153723=CARTESIAN_POINT('Ctrl Pts',(0.309595398999944,15.2,-10.479645198));
#153724=CARTESIAN_POINT('Ctrl Pts',(0.309595398999944,11.6,-10.479645198));
#153725=CARTESIAN_POINT('Ctrl Pts',(0.309918754999944,15.2,-10.481256934));
#153726=CARTESIAN_POINT('Ctrl Pts',(0.309918754999944,11.6,-10.481256934));
#153727=CARTESIAN_POINT('Ctrl Pts',(0.310245152999944,15.2,-10.482875987));
#153728=CARTESIAN_POINT('Ctrl Pts',(0.310245152999944,11.6,-10.482875987));
#153729=CARTESIAN_POINT('Ctrl Pts',(0.310574601999944,15.2,-10.484502335));
#153730=CARTESIAN_POINT('Ctrl Pts',(0.310574601999944,11.6,-10.484502335));
#153731=CARTESIAN_POINT('Ctrl Pts',(0.310907112999944,15.2,-10.486135957));
#153732=CARTESIAN_POINT('Ctrl Pts',(0.310907112999944,11.6,-10.486135957));
#153733=CARTESIAN_POINT('Ctrl Pts',(0.311242694999944,15.2,-10.487776833));
#153734=CARTESIAN_POINT('Ctrl Pts',(0.311242694999944,11.6,-10.487776833));
#153735=CARTESIAN_POINT('Ctrl Pts',(0.311581355999945,15.2,-10.489424943));
#153736=CARTESIAN_POINT('Ctrl Pts',(0.311581355999945,11.6,-10.489424943));
#153737=CARTESIAN_POINT('Ctrl Pts',(0.311923106999944,15.2,-10.491080266));
#153738=CARTESIAN_POINT('Ctrl Pts',(0.311923106999944,11.6,-10.491080266));
#153739=CARTESIAN_POINT('Ctrl Pts',(0.312267955999944,15.2,-10.492742782));
#153740=CARTESIAN_POINT('Ctrl Pts',(0.312267955999944,11.6,-10.492742782));
#153741=CARTESIAN_POINT('Ctrl Pts',(0.312615911999944,15.2,-10.494412473));
#153742=CARTESIAN_POINT('Ctrl Pts',(0.312615911999944,11.6,-10.494412473));
#153743=CARTESIAN_POINT('Ctrl Pts',(0.312966985999944,15.2,-10.496089316));
#153744=CARTESIAN_POINT('Ctrl Pts',(0.312966985999944,11.6,-10.496089316));
#153745=CARTESIAN_POINT('Ctrl Pts',(0.313321185999945,15.2,-10.497773293));
#153746=CARTESIAN_POINT('Ctrl Pts',(0.313321185999945,11.6,-10.497773293));
#153747=CARTESIAN_POINT('Ctrl Pts',(0.313678518999945,15.2,-10.499464382));
#153748=CARTESIAN_POINT('Ctrl Pts',(0.313678518999945,11.6,-10.499464382));
#153749=CARTESIAN_POINT('Ctrl Pts',(0.314038995999945,15.2,-10.501162565));
#153750=CARTESIAN_POINT('Ctrl Pts',(0.314038995999945,11.6,-10.501162565));
#153751=CARTESIAN_POINT('Ctrl Pts',(0.314402626999944,15.2,-10.502867822));
#153752=CARTESIAN_POINT('Ctrl Pts',(0.314402626999944,11.6,-10.502867822));
#153753=CARTESIAN_POINT('Ctrl Pts',(0.314769418999944,15.2,-10.504580133));
#153754=CARTESIAN_POINT('Ctrl Pts',(0.314769418999944,11.6,-10.504580133));
#153755=CARTESIAN_POINT('Ctrl Pts',(0.315139380999945,15.2,-10.506299478));
#153756=CARTESIAN_POINT('Ctrl Pts',(0.315139380999945,11.6,-10.506299478));
#153757=CARTESIAN_POINT('Ctrl Pts',(0.315512523999945,15.2,-10.508025838));
#153758=CARTESIAN_POINT('Ctrl Pts',(0.315512523999945,11.6,-10.508025838));
#153759=CARTESIAN_POINT('Ctrl Pts',(0.315888853999944,15.2,-10.509759194));
#153760=CARTESIAN_POINT('Ctrl Pts',(0.315888853999944,11.6,-10.509759194));
#153761=CARTESIAN_POINT('Ctrl Pts',(0.316268379999943,15.2,-10.511499525));
#153762=CARTESIAN_POINT('Ctrl Pts',(0.316268379999943,11.6,-10.511499525));
#153763=CARTESIAN_POINT('Ctrl Pts',(0.316651111999944,15.2,-10.513246812));
#153764=CARTESIAN_POINT('Ctrl Pts',(0.316651111999944,11.6,-10.513246812));
#153765=CARTESIAN_POINT('Ctrl Pts',(0.317037058999944,15.2,-10.515001037));
#153766=CARTESIAN_POINT('Ctrl Pts',(0.317037058999944,11.6,-10.515001037));
#153767=CARTESIAN_POINT('Ctrl Pts',(0.317426227999944,15.2,-10.516762179));
#153768=CARTESIAN_POINT('Ctrl Pts',(0.317426227999944,11.6,-10.516762179));
#153769=CARTESIAN_POINT('Ctrl Pts',(0.317818627999945,15.2,-10.518530222));
#153770=CARTESIAN_POINT('Ctrl Pts',(0.317818627999945,11.6,-10.518530222));
#153771=CARTESIAN_POINT('Ctrl Pts',(0.318214267999943,15.2,-10.520305143));
#153772=CARTESIAN_POINT('Ctrl Pts',(0.318214267999943,11.6,-10.520305143));
#153773=CARTESIAN_POINT('Ctrl Pts',(0.318613155999945,15.2,-10.522086924));
#153774=CARTESIAN_POINT('Ctrl Pts',(0.318613155999945,11.6,-10.522086924));
#153775=CARTESIAN_POINT('Ctrl Pts',(0.319015301999944,15.2,-10.523875548));
#153776=CARTESIAN_POINT('Ctrl Pts',(0.319015301999944,11.6,-10.523875548));
#153777=CARTESIAN_POINT('Ctrl Pts',(0.319420711999945,15.2,-10.525670994));
#153778=CARTESIAN_POINT('Ctrl Pts',(0.319420711999945,11.6,-10.525670994));
#153779=CARTESIAN_POINT('Ctrl Pts',(0.319829394999944,15.2,-10.527473244));
#153780=CARTESIAN_POINT('Ctrl Pts',(0.319829394999944,11.6,-10.527473244));
#153781=CARTESIAN_POINT('Ctrl Pts',(0.320241359999944,15.2,-10.529282279));
#153782=CARTESIAN_POINT('Ctrl Pts',(0.320241359999944,11.6,-10.529282279));
#153783=CARTESIAN_POINT('Ctrl Pts',(0.320656615999945,15.2,-10.53109808));
#153784=CARTESIAN_POINT('Ctrl Pts',(0.320656615999945,11.6,-10.53109808));
#153785=CARTESIAN_POINT('Ctrl Pts',(0.321075168999944,15.2,-10.532920629));
#153786=CARTESIAN_POINT('Ctrl Pts',(0.321075168999944,11.6,-10.532920629));
#153787=CARTESIAN_POINT('Ctrl Pts',(0.321497027999945,15.2,-10.534749907));
#153788=CARTESIAN_POINT('Ctrl Pts',(0.321497027999945,11.6,-10.534749907));
#153789=CARTESIAN_POINT('Ctrl Pts',(0.321922202999945,15.2,-10.536585896));
#153790=CARTESIAN_POINT('Ctrl Pts',(0.321922202999945,11.6,-10.536585896));
#153791=CARTESIAN_POINT('Ctrl Pts',(0.322350699999945,15.2,-10.538428576));
#153792=CARTESIAN_POINT('Ctrl Pts',(0.322350699999945,11.6,-10.538428576));
#153793=CARTESIAN_POINT('Ctrl Pts',(0.322782527999944,15.2,-10.54027793));
#153794=CARTESIAN_POINT('Ctrl Pts',(0.322782527999944,11.6,-10.54027793));
#153795=CARTESIAN_POINT('Ctrl Pts',(0.323217693999943,15.2,-10.54213394));
#153796=CARTESIAN_POINT('Ctrl Pts',(0.323217693999943,11.6,-10.54213394));
#153797=CARTESIAN_POINT('Ctrl Pts',(0.323656205999944,15.2,-10.543996587));
#153798=CARTESIAN_POINT('Ctrl Pts',(0.323656205999944,11.6,-10.543996587));
#153799=CARTESIAN_POINT('Ctrl Pts',(0.324098074999943,15.2,-10.545865852));
#153800=CARTESIAN_POINT('Ctrl Pts',(0.324098074999943,11.6,-10.545865852));
#153801=CARTESIAN_POINT('Ctrl Pts',(0.324543303999943,15.2,-10.547741717));
#153802=CARTESIAN_POINT('Ctrl Pts',(0.324543303999943,11.6,-10.547741717));
#153803=CARTESIAN_POINT('Ctrl Pts',(0.324991904999944,15.2,-10.549624165));
#153804=CARTESIAN_POINT('Ctrl Pts',(0.324991904999944,11.6,-10.549624165));
#153805=CARTESIAN_POINT('Ctrl Pts',(0.325443882999944,15.2,-10.551513176));
#153806=CARTESIAN_POINT('Ctrl Pts',(0.325443882999944,11.6,-10.551513176));
#153807=CARTESIAN_POINT('Ctrl Pts',(0.325899247999945,15.2,-10.553408734));
#153808=CARTESIAN_POINT('Ctrl Pts',(0.325899247999945,11.6,-10.553408734));
#153809=CARTESIAN_POINT('Ctrl Pts',(0.326358006999945,15.2,-10.555310821));
#153810=CARTESIAN_POINT('Ctrl Pts',(0.326358006999945,11.6,-10.555310821));
#153811=CARTESIAN_POINT('Ctrl Pts',(0.326820166999945,15.2,-10.557219417));
#153812=CARTESIAN_POINT('Ctrl Pts',(0.326820166999945,11.6,-10.557219417));
#153813=CARTESIAN_POINT('Ctrl Pts',(0.327285734999944,15.2,-10.559134506));
#153814=CARTESIAN_POINT('Ctrl Pts',(0.327285734999944,11.6,-10.559134506));
#153815=CARTESIAN_POINT('Ctrl Pts',(0.327754721999945,15.2,-10.56105607));
#153816=CARTESIAN_POINT('Ctrl Pts',(0.327754721999945,11.6,-10.56105607));
#153817=CARTESIAN_POINT('Ctrl Pts',(0.328227131999944,15.2,-10.562984091));
#153818=CARTESIAN_POINT('Ctrl Pts',(0.328227131999944,11.6,-10.562984091));
#153819=CARTESIAN_POINT('Ctrl Pts',(0.328702974999944,15.2,-10.56491855));
#153820=CARTESIAN_POINT('Ctrl Pts',(0.328702974999944,11.6,-10.56491855));
#153821=CARTESIAN_POINT('Ctrl Pts',(0.329182255999945,15.2,-10.566859432));
#153822=CARTESIAN_POINT('Ctrl Pts',(0.329182255999945,11.6,-10.566859432));
#153823=CARTESIAN_POINT('Ctrl Pts',(0.329664984999944,15.2,-10.568806718));
#153824=CARTESIAN_POINT('Ctrl Pts',(0.329664984999944,11.6,-10.568806718));
#153825=CARTESIAN_POINT('Ctrl Pts',(0.330151167999944,15.2,-10.57076039));
#153826=CARTESIAN_POINT('Ctrl Pts',(0.330151167999944,11.6,-10.57076039));
#153827=CARTESIAN_POINT('Ctrl Pts',(0.330640813999944,15.2,-10.572720431));
#153828=CARTESIAN_POINT('Ctrl Pts',(0.330640813999944,11.6,-10.572720431));
#153829=CARTESIAN_POINT('Ctrl Pts',(0.331133927999945,15.2,-10.574686823));
#153830=CARTESIAN_POINT('Ctrl Pts',(0.331133927999945,11.6,-10.574686823));
#153831=CARTESIAN_POINT('Ctrl Pts',(0.331630518999945,15.2,-10.57665955));
#153832=CARTESIAN_POINT('Ctrl Pts',(0.331630518999945,11.6,-10.57665955));
#153833=CARTESIAN_POINT('Ctrl Pts',(0.332130593999944,15.2,-10.578638595));
#153834=CARTESIAN_POINT('Ctrl Pts',(0.332130593999944,11.6,-10.578638595));
#153835=CARTESIAN_POINT('Ctrl Pts',(0.332634160999945,15.2,-10.580623937));
#153836=CARTESIAN_POINT('Ctrl Pts',(0.332634160999945,11.6,-10.580623937));
#153837=CARTESIAN_POINT('Ctrl Pts',(0.333141224999943,15.2,-10.582615564));
#153838=CARTESIAN_POINT('Ctrl Pts',(0.333141224999943,11.6,-10.582615564));
#153839=CARTESIAN_POINT('Ctrl Pts',(0.333651795999945,15.2,-10.584613455));
#153840=CARTESIAN_POINT('Ctrl Pts',(0.333651795999945,11.6,-10.584613455));
#153841=CARTESIAN_POINT('Ctrl Pts',(0.334165878999944,15.2,-10.586617594));
#153842=CARTESIAN_POINT('Ctrl Pts',(0.334165878999944,11.6,-10.586617594));
#153843=CARTESIAN_POINT('Ctrl Pts',(0.334683482999945,15.2,-10.588627965));
#153844=CARTESIAN_POINT('Ctrl Pts',(0.334683482999945,11.6,-10.588627965));
#153845=CARTESIAN_POINT('Ctrl Pts',(0.335204611999943,15.2,-10.59064455));
#153846=CARTESIAN_POINT('Ctrl Pts',(0.335204611999943,11.6,-10.59064455));
#153847=CARTESIAN_POINT('Ctrl Pts',(0.335729277999944,15.2,-10.592667332));
#153848=CARTESIAN_POINT('Ctrl Pts',(0.335729277999944,11.6,-10.592667332));
#153849=CARTESIAN_POINT('Ctrl Pts',(0.336257482999944,15.2,-10.594696293));
#153850=CARTESIAN_POINT('Ctrl Pts',(0.336257482999944,11.6,-10.594696293));
#153851=CARTESIAN_POINT('Ctrl Pts',(0.336789236999945,15.2,-10.59673142));
#153852=CARTESIAN_POINT('Ctrl Pts',(0.336789236999945,11.6,-10.59673142));
#153853=CARTESIAN_POINT('Ctrl Pts',(0.337324545999945,15.2,-10.598772692));
#153854=CARTESIAN_POINT('Ctrl Pts',(0.337324545999945,11.6,-10.598772692));
#153855=CARTESIAN_POINT('Ctrl Pts',(0.337863417999945,15.2,-10.600820093));
#153856=CARTESIAN_POINT('Ctrl Pts',(0.337863417999945,11.6,-10.600820093));
#153857=CARTESIAN_POINT('Ctrl Pts',(0.338405857999945,15.2,-10.602873609));
#153858=CARTESIAN_POINT('Ctrl Pts',(0.338405857999945,11.6,-10.602873609));
#153859=CARTESIAN_POINT('Ctrl Pts',(0.338951873999944,15.2,-10.60493322));
#153860=CARTESIAN_POINT('Ctrl Pts',(0.338951873999944,11.6,-10.60493322));
#153861=CARTESIAN_POINT('Ctrl Pts',(0.339501472999943,15.2,-10.606998913));
#153862=CARTESIAN_POINT('Ctrl Pts',(0.339501472999943,11.6,-10.606998913));
#153863=CARTESIAN_POINT('Ctrl Pts',(0.340054661999943,15.2,-10.609070667));
#153864=CARTESIAN_POINT('Ctrl Pts',(0.340054661999943,11.6,-10.609070667));
#153865=CARTESIAN_POINT('Ctrl Pts',(0.340611446999944,15.2,-10.611148469));
#153866=CARTESIAN_POINT('Ctrl Pts',(0.340611446999944,11.6,-10.611148469));
#153867=CARTESIAN_POINT('Ctrl Pts',(0.341171834999944,15.2,-10.613232302));
#153868=CARTESIAN_POINT('Ctrl Pts',(0.341171834999944,11.6,-10.613232302));
#153869=CARTESIAN_POINT('Ctrl Pts',(0.341735832999944,15.2,-10.615322148));
#153870=CARTESIAN_POINT('Ctrl Pts',(0.341735832999944,11.6,-10.615322148));
#153871=CARTESIAN_POINT('Ctrl Pts',(0.342303446999944,15.2,-10.617417992));
#153872=CARTESIAN_POINT('Ctrl Pts',(0.342303446999944,11.6,-10.617417992));
#153873=CARTESIAN_POINT('Ctrl Pts',(0.342874684999943,15.2,-10.619519817));
#153874=CARTESIAN_POINT('Ctrl Pts',(0.342874684999943,11.6,-10.619519817));
#153875=CARTESIAN_POINT('Ctrl Pts',(0.343449551999945,15.2,-10.621627608));
#153876=CARTESIAN_POINT('Ctrl Pts',(0.343449551999945,11.6,-10.621627608));
#153877=CARTESIAN_POINT('Ctrl Pts',(0.344028054999944,15.2,-10.623741347));
#153878=CARTESIAN_POINT('Ctrl Pts',(0.344028054999944,11.6,-10.623741347));
#153879=CARTESIAN_POINT('Ctrl Pts',(0.344610201999943,15.2,-10.625861018));
#153880=CARTESIAN_POINT('Ctrl Pts',(0.344610201999943,11.6,-10.625861018));
#153881=CARTESIAN_POINT('Ctrl Pts',(0.345195997999944,15.2,-10.627986606));
#153882=CARTESIAN_POINT('Ctrl Pts',(0.345195997999944,11.6,-10.627986606));
#153883=CARTESIAN_POINT('Ctrl Pts',(0.345785448999945,15.2,-10.630118095));
#153884=CARTESIAN_POINT('Ctrl Pts',(0.345785448999945,11.6,-10.630118095));
#153885=CARTESIAN_POINT('Ctrl Pts',(0.346378563999944,15.2,-10.632255468));
#153886=CARTESIAN_POINT('Ctrl Pts',(0.346378563999944,11.6,-10.632255468));
#153887=CARTESIAN_POINT('Ctrl Pts',(0.346975346999944,15.2,-10.634398708));
#153888=CARTESIAN_POINT('Ctrl Pts',(0.346975346999944,11.6,-10.634398708));
#153889=CARTESIAN_POINT('Ctrl Pts',(0.347575804999943,15.2,-10.636547803));
#153890=CARTESIAN_POINT('Ctrl Pts',(0.347575804999943,11.6,-10.636547803));
#153891=CARTESIAN_POINT('Ctrl Pts',(0.348179944999943,15.2,-10.638702732));
#153892=CARTESIAN_POINT('Ctrl Pts',(0.348179944999943,11.6,-10.638702732));
#153893=CARTESIAN_POINT('Ctrl Pts',(0.348787772999944,15.2,-10.640863483));
#153894=CARTESIAN_POINT('Ctrl Pts',(0.348787772999944,11.6,-10.640863483));
#153895=CARTESIAN_POINT('Ctrl Pts',(0.349399294999945,15.2,-10.643030038));
#153896=CARTESIAN_POINT('Ctrl Pts',(0.349399294999945,11.6,-10.643030038));
#153897=CARTESIAN_POINT('Ctrl Pts',(0.350014516999944,15.2,-10.645202383));
#153898=CARTESIAN_POINT('Ctrl Pts',(0.350014516999944,11.6,-10.645202383));
#153899=CARTESIAN_POINT('Ctrl Pts',(0.350633445999945,15.2,-10.647380501));
#153900=CARTESIAN_POINT('Ctrl Pts',(0.350633445999945,11.6,-10.647380501));
#153901=CARTESIAN_POINT('Ctrl Pts',(0.351256087999945,15.2,-10.649564376));
#153902=CARTESIAN_POINT('Ctrl Pts',(0.351256087999945,11.6,-10.649564376));
#153903=CARTESIAN_POINT('Ctrl Pts',(0.351882449999945,15.2,-10.651753993));
#153904=CARTESIAN_POINT('Ctrl Pts',(0.351882449999945,11.6,-10.651753993));
#153905=CARTESIAN_POINT('Ctrl Pts',(0.352512535999944,15.2,-10.653949337));
#153906=CARTESIAN_POINT('Ctrl Pts',(0.352512535999944,11.6,-10.653949337));
#153907=CARTESIAN_POINT('Ctrl Pts',(0.353146353999945,15.2,-10.656150391));
#153908=CARTESIAN_POINT('Ctrl Pts',(0.353146353999945,11.6,-10.656150391));
#153909=CARTESIAN_POINT('Ctrl Pts',(0.353783908999944,15.2,-10.658357141));
#153910=CARTESIAN_POINT('Ctrl Pts',(0.353783908999944,11.6,-10.658357141));
#153911=CARTESIAN_POINT('Ctrl Pts',(0.354425208999943,15.2,-10.660569571));
#153912=CARTESIAN_POINT('Ctrl Pts',(0.354425208999943,11.6,-10.660569571));
#153913=CARTESIAN_POINT('Ctrl Pts',(0.355070257999944,15.2,-10.662787664));
#153914=CARTESIAN_POINT('Ctrl Pts',(0.355070257999944,11.6,-10.662787664));
#153915=CARTESIAN_POINT('Ctrl Pts',(0.355719062999944,15.2,-10.665011407));
#153916=CARTESIAN_POINT('Ctrl Pts',(0.355719062999944,11.6,-10.665011407));
#153917=CARTESIAN_POINT('Ctrl Pts',(0.356371629999943,15.2,-10.667240784));
#153918=CARTESIAN_POINT('Ctrl Pts',(0.356371629999943,11.6,-10.667240784));
#153919=CARTESIAN_POINT('Ctrl Pts',(0.357027963999944,15.2,-10.669475778));
#153920=CARTESIAN_POINT('Ctrl Pts',(0.357027963999944,11.6,-10.669475778));
#153921=CARTESIAN_POINT('Ctrl Pts',(0.357688070999943,15.2,-10.671716375));
#153922=CARTESIAN_POINT('Ctrl Pts',(0.357688070999943,11.6,-10.671716375));
#153923=CARTESIAN_POINT('Ctrl Pts',(0.358351957999944,15.2,-10.673962561));
#153924=CARTESIAN_POINT('Ctrl Pts',(0.358351957999944,11.6,-10.673962561));
#153925=CARTESIAN_POINT('Ctrl Pts',(0.359019631999944,15.2,-10.676214319));
#153926=CARTESIAN_POINT('Ctrl Pts',(0.359019631999944,11.6,-10.676214319));
#153927=CARTESIAN_POINT('Ctrl Pts',(0.359691094999944,15.2,-10.678471635));
#153928=CARTESIAN_POINT('Ctrl Pts',(0.359691094999944,11.6,-10.678471635));
#153929=CARTESIAN_POINT('Ctrl Pts',(0.360366356999944,15.2,-10.680734493));
#153930=CARTESIAN_POINT('Ctrl Pts',(0.360366356999944,11.6,-10.680734493));
#153931=CARTESIAN_POINT('Ctrl Pts',(0.361045420999944,15.2,-10.683002879));
#153932=CARTESIAN_POINT('Ctrl Pts',(0.361045420999944,11.6,-10.683002879));
#153933=CARTESIAN_POINT('Ctrl Pts',(0.361728292999944,15.2,-10.685276775));
#153934=CARTESIAN_POINT('Ctrl Pts',(0.361728292999944,11.6,-10.685276775));
#153935=CARTESIAN_POINT('Ctrl Pts',(0.362414979999944,15.2,-10.687556171));
#153936=CARTESIAN_POINT('Ctrl Pts',(0.362414979999944,11.6,-10.687556171));
#153937=CARTESIAN_POINT('Ctrl Pts',(0.363105486999944,15.2,-10.689841047));
#153938=CARTESIAN_POINT('Ctrl Pts',(0.363105486999944,11.6,-10.689841047));
#153939=CARTESIAN_POINT('Ctrl Pts',(0.363799819999944,15.2,-10.692131392));
#153940=CARTESIAN_POINT('Ctrl Pts',(0.363799819999944,11.6,-10.692131392));
#153941=CARTESIAN_POINT('Ctrl Pts',(0.364497983999945,15.2,-10.69442719));
#153942=CARTESIAN_POINT('Ctrl Pts',(0.364497983999945,11.6,-10.69442719));
#153943=CARTESIAN_POINT('Ctrl Pts',(0.365199985999943,15.2,-10.696728424));
#153944=CARTESIAN_POINT('Ctrl Pts',(0.365199985999943,11.6,-10.696728424));
#153945=CARTESIAN_POINT('Ctrl Pts',(0.365905829999944,15.2,-10.699035082));
#153946=CARTESIAN_POINT('Ctrl Pts',(0.365905829999944,11.6,-10.699035082));
#153947=CARTESIAN_POINT('Ctrl Pts',(0.366615521999943,15.2,-10.701347148));
#153948=CARTESIAN_POINT('Ctrl Pts',(0.366615521999943,11.6,-10.701347148));
#153949=CARTESIAN_POINT('Ctrl Pts',(0.367329068999943,15.2,-10.703664607));
#153950=CARTESIAN_POINT('Ctrl Pts',(0.367329068999943,11.6,-10.703664607));
#153951=CARTESIAN_POINT('Ctrl Pts',(0.368046474999945,15.2,-10.705987445));
#153952=CARTESIAN_POINT('Ctrl Pts',(0.368046474999945,11.6,-10.705987445));
#153953=CARTESIAN_POINT('Ctrl Pts',(0.368767745999945,15.2,-10.708315648));
#153954=CARTESIAN_POINT('Ctrl Pts',(0.368767745999945,11.6,-10.708315648));
#153955=CARTESIAN_POINT('Ctrl Pts',(0.369492886999945,15.2,-10.710649199));
#153956=CARTESIAN_POINT('Ctrl Pts',(0.369492886999945,11.6,-10.710649199));
#153957=CARTESIAN_POINT('Ctrl Pts',(0.370221902999944,15.2,-10.712988086));
#153958=CARTESIAN_POINT('Ctrl Pts',(0.370221902999944,11.6,-10.712988086));
#153959=CARTESIAN_POINT('Ctrl Pts',(0.370954801999943,15.2,-10.715332293));
#153960=CARTESIAN_POINT('Ctrl Pts',(0.370954801999943,11.6,-10.715332293));
#153961=CARTESIAN_POINT('Ctrl Pts',(0.371691585999944,15.2,-10.717681807));
#153962=CARTESIAN_POINT('Ctrl Pts',(0.371691585999944,11.6,-10.717681807));
#153963=CARTESIAN_POINT('Ctrl Pts',(0.372432262999943,15.2,-10.720036612));
#153964=CARTESIAN_POINT('Ctrl Pts',(0.372432262999943,11.6,-10.720036612));
#153965=CARTESIAN_POINT('Ctrl Pts',(0.373176837999944,15.2,-10.722396693));
#153966=CARTESIAN_POINT('Ctrl Pts',(0.373176837999944,11.6,-10.722396693));
#153967=CARTESIAN_POINT('Ctrl Pts',(0.373925314999944,15.2,-10.724762038));
#153968=CARTESIAN_POINT('Ctrl Pts',(0.373925314999944,11.6,-10.724762038));
#153969=CARTESIAN_POINT('Ctrl Pts',(0.374677699999945,15.2,-10.72713263));
#153970=CARTESIAN_POINT('Ctrl Pts',(0.374677699999945,11.6,-10.72713263));
#153971=CARTESIAN_POINT('Ctrl Pts',(0.375433997999943,15.2,-10.729508457));
#153972=CARTESIAN_POINT('Ctrl Pts',(0.375433997999943,11.6,-10.729508457));
#153973=CARTESIAN_POINT('Ctrl Pts',(0.376194214999943,15.2,-10.731889504));
#153974=CARTESIAN_POINT('Ctrl Pts',(0.376194214999943,11.6,-10.731889504));
#153975=CARTESIAN_POINT('Ctrl Pts',(0.376958354999944,15.2,-10.734275757));
#153976=CARTESIAN_POINT('Ctrl Pts',(0.376958354999944,11.6,-10.734275757));
#153977=CARTESIAN_POINT('Ctrl Pts',(0.377726424999943,15.2,-10.7366672));
#153978=CARTESIAN_POINT('Ctrl Pts',(0.377726424999943,11.6,-10.7366672));
#153979=CARTESIAN_POINT('Ctrl Pts',(0.378498428999944,15.2,-10.73906382));
#153980=CARTESIAN_POINT('Ctrl Pts',(0.378498428999944,11.6,-10.73906382));
#153981=CARTESIAN_POINT('Ctrl Pts',(0.379274372999945,15.2,-10.741465604));
#153982=CARTESIAN_POINT('Ctrl Pts',(0.379274372999945,11.6,-10.741465604));
#153983=CARTESIAN_POINT('Ctrl Pts',(0.380054259999945,15.2,-10.743872536));
#153984=CARTESIAN_POINT('Ctrl Pts',(0.380054259999945,11.6,-10.743872536));
#153985=CARTESIAN_POINT('Ctrl Pts',(0.380838096999945,15.2,-10.746284604));
#153986=CARTESIAN_POINT('Ctrl Pts',(0.380838096999945,11.6,-10.746284604));
#153987=CARTESIAN_POINT('Ctrl Pts',(0.381625889999944,15.2,-10.748701792));
#153988=CARTESIAN_POINT('Ctrl Pts',(0.381625889999944,11.6,-10.748701792));
#153989=CARTESIAN_POINT('Ctrl Pts',(0.382417640999944,15.2,-10.751124087));
#153990=CARTESIAN_POINT('Ctrl Pts',(0.382417640999944,11.6,-10.751124087));
#153991=CARTESIAN_POINT('Ctrl Pts',(0.383213356999944,15.2,-10.753551475));
#153992=CARTESIAN_POINT('Ctrl Pts',(0.383213356999944,11.6,-10.753551475));
#153993=CARTESIAN_POINT('Ctrl Pts',(0.384013043999945,15.2,-10.755983942));
#153994=CARTESIAN_POINT('Ctrl Pts',(0.384013043999945,11.6,-10.755983942));
#153995=CARTESIAN_POINT('Ctrl Pts',(0.384816703999944,15.2,-10.758421474));
#153996=CARTESIAN_POINT('Ctrl Pts',(0.384816703999944,11.6,-10.758421474));
#153997=CARTESIAN_POINT('Ctrl Pts',(0.385624345999943,15.2,-10.760864057));
#153998=CARTESIAN_POINT('Ctrl Pts',(0.385624345999943,11.6,-10.760864057));
#153999=CARTESIAN_POINT('Ctrl Pts',(0.386435970999944,15.2,-10.763311678));
#154000=CARTESIAN_POINT('Ctrl Pts',(0.386435970999944,11.6,-10.763311678));
#154001=CARTESIAN_POINT('Ctrl Pts',(0.387251585999945,15.2,-10.765764322));
#154002=CARTESIAN_POINT('Ctrl Pts',(0.387251585999945,11.6,-10.765764322));
#154003=CARTESIAN_POINT('Ctrl Pts',(0.388071194999944,15.2,-10.768221976));
#154004=CARTESIAN_POINT('Ctrl Pts',(0.388071194999944,11.6,-10.768221976));
#154005=CARTESIAN_POINT('Ctrl Pts',(0.388894804999945,15.2,-10.770684626));
#154006=CARTESIAN_POINT('Ctrl Pts',(0.388894804999945,11.6,-10.770684626));
#154007=CARTESIAN_POINT('Ctrl Pts',(0.389722417999945,15.2,-10.773152259));
#154008=CARTESIAN_POINT('Ctrl Pts',(0.389722417999945,11.6,-10.773152259));
#154009=CARTESIAN_POINT('Ctrl Pts',(0.390554040999945,15.2,-10.77562486));
#154010=CARTESIAN_POINT('Ctrl Pts',(0.390554040999945,11.6,-10.77562486));
#154011=CARTESIAN_POINT('Ctrl Pts',(0.391389675999945,15.2,-10.778102417));
#154012=CARTESIAN_POINT('Ctrl Pts',(0.391389675999945,11.6,-10.778102417));
#154013=CARTESIAN_POINT('Ctrl Pts',(0.392229331999945,15.2,-10.780584915));
#154014=CARTESIAN_POINT('Ctrl Pts',(0.392229331999945,11.6,-10.780584915));
#154015=CARTESIAN_POINT('Ctrl Pts',(0.393073008999943,15.2,-10.78307234));
#154016=CARTESIAN_POINT('Ctrl Pts',(0.393073008999943,11.6,-10.78307234));
#154017=CARTESIAN_POINT('Ctrl Pts',(0.393920715999944,15.2,-10.785564681));
#154018=CARTESIAN_POINT('Ctrl Pts',(0.393920715999944,11.6,-10.785564681));
#154019=CARTESIAN_POINT('Ctrl Pts',(0.394772454999943,15.2,-10.788061922));
#154020=CARTESIAN_POINT('Ctrl Pts',(0.394772454999943,11.6,-10.788061922));
#154021=CARTESIAN_POINT('Ctrl Pts',(0.395628231999944,15.2,-10.790564051));
#154022=CARTESIAN_POINT('Ctrl Pts',(0.395628231999944,11.6,-10.790564051));
#154023=CARTESIAN_POINT('Ctrl Pts',(0.396488050999944,15.2,-10.793071054));
#154024=CARTESIAN_POINT('Ctrl Pts',(0.396488050999944,11.6,-10.793071054));
#154025=CARTESIAN_POINT('Ctrl Pts',(0.397351916999943,15.2,-10.795582918));
#154026=CARTESIAN_POINT('Ctrl Pts',(0.397351916999943,11.6,-10.795582918));
#154027=CARTESIAN_POINT('Ctrl Pts',(0.398219834999944,15.2,-10.798099629));
#154028=CARTESIAN_POINT('Ctrl Pts',(0.398219834999944,11.6,-10.798099629));
#154029=CARTESIAN_POINT('Ctrl Pts',(0.399091808999945,15.2,-10.800621174));
#154030=CARTESIAN_POINT('Ctrl Pts',(0.399091808999945,11.6,-10.800621174));
#154031=CARTESIAN_POINT('Ctrl Pts',(0.399967842999944,15.2,-10.80314754));
#154032=CARTESIAN_POINT('Ctrl Pts',(0.399967842999944,11.6,-10.80314754));
#154033=CARTESIAN_POINT('Ctrl Pts',(0.400847942999943,15.2,-10.805678712));
#154034=CARTESIAN_POINT('Ctrl Pts',(0.400847942999943,11.6,-10.805678712));
#154035=CARTESIAN_POINT('Ctrl Pts',(0.401732111999945,15.2,-10.808214679));
#154036=CARTESIAN_POINT('Ctrl Pts',(0.401732111999945,11.6,-10.808214679));
#154037=CARTESIAN_POINT('Ctrl Pts',(0.402620355999943,15.2,-10.810755427));
#154038=CARTESIAN_POINT('Ctrl Pts',(0.402620355999943,11.6,-10.810755427));
#154039=CARTESIAN_POINT('Ctrl Pts',(0.403512678999943,15.2,-10.813300943));
#154040=CARTESIAN_POINT('Ctrl Pts',(0.403512678999943,11.6,-10.813300943));
#154041=CARTESIAN_POINT('Ctrl Pts',(0.404409085999945,15.2,-10.815851213));
#154042=CARTESIAN_POINT('Ctrl Pts',(0.404409085999945,11.6,-10.815851213));
#154043=CARTESIAN_POINT('Ctrl Pts',(0.405309579999944,15.2,-10.818406225));
#154044=CARTESIAN_POINT('Ctrl Pts',(0.405309579999944,11.6,-10.818406225));
#154045=CARTESIAN_POINT('Ctrl Pts',(0.406214165999945,15.2,-10.820965964));
#154046=CARTESIAN_POINT('Ctrl Pts',(0.406214165999945,11.6,-10.820965964));
#154047=CARTESIAN_POINT('Ctrl Pts',(0.407122848999943,15.2,-10.82353042));
#154048=CARTESIAN_POINT('Ctrl Pts',(0.407122848999943,11.6,-10.82353042));
#154049=CARTESIAN_POINT('Ctrl Pts',(0.408035631999945,15.2,-10.826099577));
#154050=CARTESIAN_POINT('Ctrl Pts',(0.408035631999945,11.6,-10.826099577));
#154051=CARTESIAN_POINT('Ctrl Pts',(0.408952521999945,15.2,-10.828673424));
#154052=CARTESIAN_POINT('Ctrl Pts',(0.408952521999945,11.6,-10.828673424));
#154053=CARTESIAN_POINT('Ctrl Pts',(0.409873521999945,15.2,-10.831251946));
#154054=CARTESIAN_POINT('Ctrl Pts',(0.409873521999945,11.6,-10.831251946));
#154055=CARTESIAN_POINT('Ctrl Pts',(0.410798634999944,15.2,-10.833835132));
#154056=CARTESIAN_POINT('Ctrl Pts',(0.410798634999944,11.6,-10.833835132));
#154057=CARTESIAN_POINT('Ctrl Pts',(0.411727865999945,15.2,-10.836422969));
#154058=CARTESIAN_POINT('Ctrl Pts',(0.411727865999945,11.6,-10.836422969));
#154059=CARTESIAN_POINT('Ctrl Pts',(0.412661221999944,15.2,-10.839015443));
#154060=CARTESIAN_POINT('Ctrl Pts',(0.412661221999944,11.6,-10.839015443));
#154061=CARTESIAN_POINT('Ctrl Pts',(0.413598702999943,15.2,-10.841612542));
#154062=CARTESIAN_POINT('Ctrl Pts',(0.413598702999943,11.6,-10.841612542));
#154063=CARTESIAN_POINT('Ctrl Pts',(0.414540315999944,15.2,-10.844214253));
#154064=CARTESIAN_POINT('Ctrl Pts',(0.414540315999944,11.6,-10.844214253));
#154065=CARTESIAN_POINT('Ctrl Pts',(0.415486064999945,15.2,-10.846820562));
#154066=CARTESIAN_POINT('Ctrl Pts',(0.415486064999945,11.6,-10.846820562));
#154067=CARTESIAN_POINT('Ctrl Pts',(0.416435952999944,15.2,-10.849431457));
#154068=CARTESIAN_POINT('Ctrl Pts',(0.416435952999944,11.6,-10.849431457));
#154069=CARTESIAN_POINT('Ctrl Pts',(0.417389984999945,15.2,-10.852046927));
#154070=CARTESIAN_POINT('Ctrl Pts',(0.417389984999945,11.6,-10.852046927));
#154071=CARTESIAN_POINT('Ctrl Pts',(0.418348164999944,15.2,-10.854666958));
#154072=CARTESIAN_POINT('Ctrl Pts',(0.418348164999944,11.6,-10.854666958));
#154073=CARTESIAN_POINT('Ctrl Pts',(0.419310496999945,15.2,-10.857291535));
#154074=CARTESIAN_POINT('Ctrl Pts',(0.419310496999945,11.6,-10.857291535));
#154075=CARTESIAN_POINT('Ctrl Pts',(0.420276985999944,15.2,-10.859920649));
#154076=CARTESIAN_POINT('Ctrl Pts',(0.420276985999944,11.6,-10.859920649));
#154077=CARTESIAN_POINT('Ctrl Pts',(0.421247635999944,15.2,-10.862554285));
#154078=CARTESIAN_POINT('Ctrl Pts',(0.421247635999944,11.6,-10.862554285));
#154079=CARTESIAN_POINT('Ctrl Pts',(0.422222449999945,15.2,-10.865192432));
#154080=CARTESIAN_POINT('Ctrl Pts',(0.422222449999945,11.6,-10.865192432));
#154081=CARTESIAN_POINT('Ctrl Pts',(0.423201432999945,15.2,-10.867835076));
#154082=CARTESIAN_POINT('Ctrl Pts',(0.423201432999945,11.6,-10.867835076));
#154083=CARTESIAN_POINT('Ctrl Pts',(0.424184586999944,15.2,-10.870482205));
#154084=CARTESIAN_POINT('Ctrl Pts',(0.424184586999944,11.6,-10.870482205));
#154085=CARTESIAN_POINT('Ctrl Pts',(0.425171919999944,15.2,-10.873133806));
#154086=CARTESIAN_POINT('Ctrl Pts',(0.425171919999944,11.6,-10.873133806));
#154087=CARTESIAN_POINT('Ctrl Pts',(0.426163432999944,15.2,-10.875789868));
#154088=CARTESIAN_POINT('Ctrl Pts',(0.426163432999944,11.6,-10.875789868));
#154089=CARTESIAN_POINT('Ctrl Pts',(0.427159130999945,15.2,-10.878450378));
#154090=CARTESIAN_POINT('Ctrl Pts',(0.427159130999945,11.6,-10.878450378));
#154091=CARTESIAN_POINT('Ctrl Pts',(0.428159016999944,15.2,-10.881115322));
#154092=CARTESIAN_POINT('Ctrl Pts',(0.428159016999944,11.6,-10.881115322));
#154093=CARTESIAN_POINT('Ctrl Pts',(0.429163096999944,15.2,-10.883784689));
#154094=CARTESIAN_POINT('Ctrl Pts',(0.429163096999944,11.6,-10.883784689));
#154095=CARTESIAN_POINT('Ctrl Pts',(0.430171372999943,15.2,-10.886458467));
#154096=CARTESIAN_POINT('Ctrl Pts',(0.430171372999943,11.6,-10.886458467));
#154097=CARTESIAN_POINT('Ctrl Pts',(0.431183849999943,15.2,-10.889136642));
#154098=CARTESIAN_POINT('Ctrl Pts',(0.431183849999943,11.6,-10.889136642));
#154099=CARTESIAN_POINT('Ctrl Pts',(0.432200529999944,15.2,-10.891819203));
#154100=CARTESIAN_POINT('Ctrl Pts',(0.432200529999944,11.6,-10.891819203));
#154101=CARTESIAN_POINT('Ctrl Pts',(0.433221419999944,15.2,-10.894506138));
#154102=CARTESIAN_POINT('Ctrl Pts',(0.433221419999944,11.6,-10.894506138));
#154103=CARTESIAN_POINT('Ctrl Pts',(0.434246522999944,15.2,-10.897197434));
#154104=CARTESIAN_POINT('Ctrl Pts',(0.434246522999944,11.6,-10.897197434));
#154105=CARTESIAN_POINT('Ctrl Pts',(0.435275840999945,15.2,-10.899893077));
#154106=CARTESIAN_POINT('Ctrl Pts',(0.435275840999945,11.6,-10.899893077));
#154107=CARTESIAN_POINT('Ctrl Pts',(0.436309378999944,15.2,-10.902593058));
#154108=CARTESIAN_POINT('Ctrl Pts',(0.436309378999944,11.6,-10.902593058));
#154109=CARTESIAN_POINT('Ctrl Pts',(0.437347139999943,15.2,-10.905297364));
#154110=CARTESIAN_POINT('Ctrl Pts',(0.437347139999943,11.6,-10.905297364));
#154111=CARTESIAN_POINT('Ctrl Pts',(0.438389128999944,15.2,-10.908005981));
#154112=CARTESIAN_POINT('Ctrl Pts',(0.438389128999944,11.6,-10.908005981));
#154113=CARTESIAN_POINT('Ctrl Pts',(0.439435350999944,15.2,-10.910718898));
#154114=CARTESIAN_POINT('Ctrl Pts',(0.439435350999944,11.6,-10.910718898));
#154115=CARTESIAN_POINT('Ctrl Pts',(0.440485805999945,15.2,-10.913436104));
#154116=CARTESIAN_POINT('Ctrl Pts',(0.440485805999945,11.6,-10.913436104));
#154117=CARTESIAN_POINT('Ctrl Pts',(0.441540500999944,15.2,-10.916157585));
#154118=CARTESIAN_POINT('Ctrl Pts',(0.441540500999944,11.6,-10.916157585));
#154119=CARTESIAN_POINT('Ctrl Pts',(0.442599438999943,15.2,-10.91888333));
#154120=CARTESIAN_POINT('Ctrl Pts',(0.442599438999943,11.6,-10.91888333));
#154121=CARTESIAN_POINT('Ctrl Pts',(0.443662621999945,15.2,-10.921613326));
#154122=CARTESIAN_POINT('Ctrl Pts',(0.443662621999945,11.6,-10.921613326));
#154123=CARTESIAN_POINT('Ctrl Pts',(0.444730055999945,15.2,-10.924347562));
#154124=CARTESIAN_POINT('Ctrl Pts',(0.444730055999945,11.6,-10.924347562));
#154125=CARTESIAN_POINT('Ctrl Pts',(0.445801742999944,15.2,-10.927086026));
#154126=CARTESIAN_POINT('Ctrl Pts',(0.445801742999944,11.6,-10.927086026));
#154127=CARTESIAN_POINT('Ctrl Pts',(0.446877687999944,15.2,-10.929828706));
#154128=CARTESIAN_POINT('Ctrl Pts',(0.446877687999944,11.6,-10.929828706));
#154129=CARTESIAN_POINT('Ctrl Pts',(0.447957893999943,15.2,-10.932575589));
#154130=CARTESIAN_POINT('Ctrl Pts',(0.447957893999943,11.6,-10.932575589));
#154131=CARTESIAN_POINT('Ctrl Pts',(0.449042363999944,15.2,-10.935326664));
#154132=CARTESIAN_POINT('Ctrl Pts',(0.449042363999944,11.6,-10.935326664));
#154133=CARTESIAN_POINT('Ctrl Pts',(0.450131101999943,15.2,-10.93808192));
#154134=CARTESIAN_POINT('Ctrl Pts',(0.450131101999943,11.6,-10.93808192));
#154135=CARTESIAN_POINT('Ctrl Pts',(0.451224112999944,15.2,-10.940841343));
#154136=CARTESIAN_POINT('Ctrl Pts',(0.451224112999944,11.6,-10.940841343));
#154137=CARTESIAN_POINT('Ctrl Pts',(0.452321397999944,15.2,-10.943604921));
#154138=CARTESIAN_POINT('Ctrl Pts',(0.452321397999944,11.6,-10.943604921));
#154139=CARTESIAN_POINT('Ctrl Pts',(0.453422961999944,15.2,-10.946372645));
#154140=CARTESIAN_POINT('Ctrl Pts',(0.453422961999944,11.6,-10.946372645));
#154141=CARTESIAN_POINT('Ctrl Pts',(0.454528808999944,15.2,-10.949144502));
#154142=CARTESIAN_POINT('Ctrl Pts',(0.454528808999944,11.6,-10.949144502));
#154143=CARTESIAN_POINT('Ctrl Pts',(0.455638941999944,15.2,-10.951920478));
#154144=CARTESIAN_POINT('Ctrl Pts',(0.455638941999944,11.6,-10.951920478));
#154145=CARTESIAN_POINT('Ctrl Pts',(0.456753363999944,15.2,-10.954700564));
#154146=CARTESIAN_POINT('Ctrl Pts',(0.456753363999944,11.6,-10.954700564));
#154147=CARTESIAN_POINT('Ctrl Pts',(0.457872078999945,15.2,-10.957484747));
#154148=CARTESIAN_POINT('Ctrl Pts',(0.457872078999945,11.6,-10.957484747));
#154149=CARTESIAN_POINT('Ctrl Pts',(0.458995090999944,15.2,-10.960273016));
#154150=CARTESIAN_POINT('Ctrl Pts',(0.458995090999944,11.6,-10.960273016));
#154151=CARTESIAN_POINT('Ctrl Pts',(0.460122400999945,15.2,-10.963065359));
#154152=CARTESIAN_POINT('Ctrl Pts',(0.460122400999945,11.6,-10.963065359));
#154153=CARTESIAN_POINT('Ctrl Pts',(0.461254015999945,15.2,-10.965861764));
#154154=CARTESIAN_POINT('Ctrl Pts',(0.461254015999945,11.6,-10.965861764));
#154155=CARTESIAN_POINT('Ctrl Pts',(0.462389937999944,15.2,-10.96866222));
#154156=CARTESIAN_POINT('Ctrl Pts',(0.462389937999944,11.6,-10.96866222));
#154157=CARTESIAN_POINT('Ctrl Pts',(0.463530168999944,15.2,-10.971466714));
#154158=CARTESIAN_POINT('Ctrl Pts',(0.463530168999944,11.6,-10.971466714));
#154159=CARTESIAN_POINT('Ctrl Pts',(0.464674712999944,15.2,-10.974275237));
#154160=CARTESIAN_POINT('Ctrl Pts',(0.464674712999944,11.6,-10.974275237));
#154161=CARTESIAN_POINT('Ctrl Pts',(0.465823575999943,15.2,-10.977087774));
#154162=CARTESIAN_POINT('Ctrl Pts',(0.465823575999943,11.6,-10.977087774));
#154163=CARTESIAN_POINT('Ctrl Pts',(0.466976756999945,15.2,-10.979904316));
#154164=CARTESIAN_POINT('Ctrl Pts',(0.466976756999945,11.6,-10.979904316));
#154165=CARTESIAN_POINT('Ctrl Pts',(0.468134261999945,15.2,-10.982724852));
#154166=CARTESIAN_POINT('Ctrl Pts',(0.468134261999945,11.6,-10.982724852));
#154167=CARTESIAN_POINT('Ctrl Pts',(0.469296094999944,15.2,-10.985549368));
#154168=CARTESIAN_POINT('Ctrl Pts',(0.469296094999944,11.6,-10.985549368));
#154169=CARTESIAN_POINT('Ctrl Pts',(0.470462256999945,15.2,-10.988377854));
#154170=CARTESIAN_POINT('Ctrl Pts',(0.470462256999945,11.6,-10.988377854));
#154171=CARTESIAN_POINT('Ctrl Pts',(0.471632752999945,15.2,-10.991210298));
#154172=CARTESIAN_POINT('Ctrl Pts',(0.471632752999945,11.6,-10.991210298));
#154173=CARTESIAN_POINT('Ctrl Pts',(0.472807584999944,15.2,-10.994046689));
#154174=CARTESIAN_POINT('Ctrl Pts',(0.472807584999944,11.6,-10.994046689));
#154175=CARTESIAN_POINT('Ctrl Pts',(0.473986757999943,15.2,-10.996887016));
#154176=CARTESIAN_POINT('Ctrl Pts',(0.473986757999943,11.6,-10.996887016));
#154177=CARTESIAN_POINT('Ctrl Pts',(0.475170271999945,15.2,-10.999731268));
#154178=CARTESIAN_POINT('Ctrl Pts',(0.475170271999945,11.6,-10.999731268));
#154179=CARTESIAN_POINT('Ctrl Pts',(0.476358134999944,15.2,-11.002579431));
#154180=CARTESIAN_POINT('Ctrl Pts',(0.476358134999944,11.6,-11.002579431));
#154181=CARTESIAN_POINT('Ctrl Pts',(0.477550345999944,15.2,-11.005431497));
#154182=CARTESIAN_POINT('Ctrl Pts',(0.477550345999944,11.6,-11.005431497));
#154183=CARTESIAN_POINT('Ctrl Pts',(0.478746909999943,15.2,-11.008287453));
#154184=CARTESIAN_POINT('Ctrl Pts',(0.478746909999943,11.6,-11.008287453));
#154185=CARTESIAN_POINT('Ctrl Pts',(0.479947829999944,15.2,-11.011147287));
#154186=CARTESIAN_POINT('Ctrl Pts',(0.479947829999944,11.6,-11.011147287));
#154187=CARTESIAN_POINT('Ctrl Pts',(0.481153109999944,15.2,-11.014010988));
#154188=CARTESIAN_POINT('Ctrl Pts',(0.481153109999944,11.6,-11.014010988));
#154189=CARTESIAN_POINT('Ctrl Pts',(0.482362750999944,15.2,-11.016878547));
#154190=CARTESIAN_POINT('Ctrl Pts',(0.482362750999944,11.6,-11.016878547));
#154191=CARTESIAN_POINT('Ctrl Pts',(0.483576757999945,15.2,-11.01974995));
#154192=CARTESIAN_POINT('Ctrl Pts',(0.483576757999945,11.6,-11.01974995));
#154193=CARTESIAN_POINT('Ctrl Pts',(0.484795132999943,15.2,-11.022625188));
#154194=CARTESIAN_POINT('Ctrl Pts',(0.484795132999943,11.6,-11.022625188));
#154195=CARTESIAN_POINT('Ctrl Pts',(0.486017879999944,15.2,-11.025504247));
#154196=CARTESIAN_POINT('Ctrl Pts',(0.486017879999944,11.6,-11.025504247));
#154197=CARTESIAN_POINT('Ctrl Pts',(0.487245001999945,15.2,-11.028387119));
#154198=CARTESIAN_POINT('Ctrl Pts',(0.487245001999945,11.6,-11.028387119));
#154199=CARTESIAN_POINT('Ctrl Pts',(0.488476501999945,15.2,-11.031273791));
#154200=CARTESIAN_POINT('Ctrl Pts',(0.488476501999945,11.6,-11.031273791));
#154201=CARTESIAN_POINT('Ctrl Pts',(0.489712381999944,15.2,-11.034164252));
#154202=CARTESIAN_POINT('Ctrl Pts',(0.489712381999944,11.6,-11.034164252));
#154203=CARTESIAN_POINT('Ctrl Pts',(0.490952645999944,15.2,-11.037058491));
#154204=CARTESIAN_POINT('Ctrl Pts',(0.490952645999944,11.6,-11.037058491));
#154205=CARTESIAN_POINT('Ctrl Pts',(0.492197297999944,15.2,-11.039956497));
#154206=CARTESIAN_POINT('Ctrl Pts',(0.492197297999944,11.6,-11.039956497));
#154207=CARTESIAN_POINT('Ctrl Pts',(0.493446337999943,15.2,-11.04285826));
#154208=CARTESIAN_POINT('Ctrl Pts',(0.493446337999943,11.6,-11.04285826));
#154209=CARTESIAN_POINT('Ctrl Pts',(0.494699771999944,15.2,-11.045763768));
#154210=CARTESIAN_POINT('Ctrl Pts',(0.494699771999944,11.6,-11.045763768));
#154211=CARTESIAN_POINT('Ctrl Pts',(0.495957600999944,15.2,-11.04867301));
#154212=CARTESIAN_POINT('Ctrl Pts',(0.495957600999944,11.6,-11.04867301));
#154213=CARTESIAN_POINT('Ctrl Pts',(0.497219829999944,15.2,-11.051585974));
#154214=CARTESIAN_POINT('Ctrl Pts',(0.497219829999944,11.6,-11.051585974));
#154215=CARTESIAN_POINT('Ctrl Pts',(0.498486459999944,15.2,-11.05450265));
#154216=CARTESIAN_POINT('Ctrl Pts',(0.498486459999944,11.6,-11.05450265));
#154217=CARTESIAN_POINT('Ctrl Pts',(0.499757494999944,15.2,-11.057423028));
#154218=CARTESIAN_POINT('Ctrl Pts',(0.499757494999944,11.6,-11.057423028));
#154219=CARTESIAN_POINT('Ctrl Pts',(0.501032935999944,15.2,-11.060347096));
#154220=CARTESIAN_POINT('Ctrl Pts',(0.501032935999944,11.6,-11.060347096));
#154221=CARTESIAN_POINT('Ctrl Pts',(0.502312788999945,15.2,-11.063274844));
#154222=CARTESIAN_POINT('Ctrl Pts',(0.502312788999945,11.6,-11.063274844));
#154223=CARTESIAN_POINT('Ctrl Pts',(0.503597054999945,15.2,-11.066206259));
#154224=CARTESIAN_POINT('Ctrl Pts',(0.503597054999945,11.6,-11.066206259));
#154225=CARTESIAN_POINT('Ctrl Pts',(0.504885736999944,15.2,-11.069141332));
#154226=CARTESIAN_POINT('Ctrl Pts',(0.504885736999944,11.6,-11.069141332));
#154227=CARTESIAN_POINT('Ctrl Pts',(0.506178838999943,15.2,-11.072080052));
#154228=CARTESIAN_POINT('Ctrl Pts',(0.506178838999943,11.6,-11.072080052));
#154229=CARTESIAN_POINT('Ctrl Pts',(0.507476362999945,15.2,-11.075022407));
#154230=CARTESIAN_POINT('Ctrl Pts',(0.507476362999945,11.6,-11.075022407));
#154231=CARTESIAN_POINT('Ctrl Pts',(0.508778309999944,15.2,-11.077968387));
#154232=CARTESIAN_POINT('Ctrl Pts',(0.508778309999944,11.6,-11.077968387));
#154233=CARTESIAN_POINT('Ctrl Pts',(0.510084685999944,15.2,-11.080917982));
#154234=CARTESIAN_POINT('Ctrl Pts',(0.510084685999944,11.6,-11.080917982));
#154235=CARTESIAN_POINT('Ctrl Pts',(0.511395492999944,15.2,-11.08387118));
#154236=CARTESIAN_POINT('Ctrl Pts',(0.511395492999944,11.6,-11.08387118));
#154237=CARTESIAN_POINT('Ctrl Pts',(0.512710730999945,15.2,-11.086827972));
#154238=CARTESIAN_POINT('Ctrl Pts',(0.512710730999945,11.6,-11.086827972));
#154239=CARTESIAN_POINT('Ctrl Pts',(0.514030406999945,15.2,-11.089788344));
#154240=CARTESIAN_POINT('Ctrl Pts',(0.514030406999945,11.6,-11.089788344));
#154241=CARTESIAN_POINT('Ctrl Pts',(0.515354519999944,15.2,-11.092752289));
#154242=CARTESIAN_POINT('Ctrl Pts',(0.515354519999944,11.6,-11.092752289));
#154243=CARTESIAN_POINT('Ctrl Pts',(0.516683075999944,15.2,-11.095719793));
#154244=CARTESIAN_POINT('Ctrl Pts',(0.516683075999944,11.6,-11.095719793));
#154245=CARTESIAN_POINT('Ctrl Pts',(0.518016074999944,15.2,-11.098690848));
#154246=CARTESIAN_POINT('Ctrl Pts',(0.518016074999944,11.6,-11.098690848));
#154247=CARTESIAN_POINT('Ctrl Pts',(0.519353520999944,15.2,-11.101665441));
#154248=CARTESIAN_POINT('Ctrl Pts',(0.519353520999944,11.6,-11.101665441));
#154249=CARTESIAN_POINT('Ctrl Pts',(0.520695416999944,15.2,-11.104643564));
#154250=CARTESIAN_POINT('Ctrl Pts',(0.520695416999944,11.6,-11.104643564));
#154251=CARTESIAN_POINT('Ctrl Pts',(0.522041764999944,15.2,-11.107625205));
#154252=CARTESIAN_POINT('Ctrl Pts',(0.522041764999944,11.6,-11.107625205));
#154253=CARTESIAN_POINT('Ctrl Pts',(0.523392567999944,15.2,-11.110610353));
#154254=CARTESIAN_POINT('Ctrl Pts',(0.523392567999944,11.6,-11.110610353));
#154255=CARTESIAN_POINT('Ctrl Pts',(0.524747828999944,15.2,-11.113598997));
#154256=CARTESIAN_POINT('Ctrl Pts',(0.524747828999944,11.6,-11.113598997));
#154257=CARTESIAN_POINT('Ctrl Pts',(0.526107550999945,15.2,-11.116591128));
#154258=CARTESIAN_POINT('Ctrl Pts',(0.526107550999945,11.6,-11.116591128));
#154259=CARTESIAN_POINT('Ctrl Pts',(0.527471734999944,15.2,-11.119586735));
#154260=CARTESIAN_POINT('Ctrl Pts',(0.527471734999944,11.6,-11.119586735));
#154261=CARTESIAN_POINT('Ctrl Pts',(0.528840383999943,15.2,-11.122585808));
#154262=CARTESIAN_POINT('Ctrl Pts',(0.528840383999943,11.6,-11.122585808));
#154263=CARTESIAN_POINT('Ctrl Pts',(0.530213500999944,15.2,-11.125588334));
#154264=CARTESIAN_POINT('Ctrl Pts',(0.530213500999944,11.6,-11.125588334));
#154265=CARTESIAN_POINT('Ctrl Pts',(0.531591089999944,15.2,-11.128594306));
#154266=CARTESIAN_POINT('Ctrl Pts',(0.531591089999944,11.6,-11.128594306));
#154267=CARTESIAN_POINT('Ctrl Pts',(0.532973150999945,15.2,-11.131603711));
#154268=CARTESIAN_POINT('Ctrl Pts',(0.532973150999945,11.6,-11.131603711));
#154269=CARTESIAN_POINT('Ctrl Pts',(0.534359687999945,15.2,-11.13461654));
#154270=CARTESIAN_POINT('Ctrl Pts',(0.534359687999945,11.6,-11.13461654));
#154271=CARTESIAN_POINT('Ctrl Pts',(0.535750703999944,15.2,-11.137632781));
#154272=CARTESIAN_POINT('Ctrl Pts',(0.535750703999944,11.6,-11.137632781));
#154273=CARTESIAN_POINT('Ctrl Pts',(0.537146200999944,15.2,-11.140652425));
#154274=CARTESIAN_POINT('Ctrl Pts',(0.537146200999944,11.6,-11.140652425));
#154275=CARTESIAN_POINT('Ctrl Pts',(0.538546180999945,15.2,-11.143675461));
#154276=CARTESIAN_POINT('Ctrl Pts',(0.538546180999945,11.6,-11.143675461));
#154277=CARTESIAN_POINT('Ctrl Pts',(0.539950646999944,15.2,-11.146701879));
#154278=CARTESIAN_POINT('Ctrl Pts',(0.539950646999944,11.6,-11.146701879));
#154279=CARTESIAN_POINT('Ctrl Pts',(0.541359600999944,15.2,-11.149731669));
#154280=CARTESIAN_POINT('Ctrl Pts',(0.541359600999944,11.6,-11.149731669));
#154281=CARTESIAN_POINT('Ctrl Pts',(0.542773046999944,15.2,-11.152764819));
#154282=CARTESIAN_POINT('Ctrl Pts',(0.542773046999944,11.6,-11.152764819));
#154283=CARTESIAN_POINT('Ctrl Pts',(0.544190985999945,15.2,-11.155801321));
#154284=CARTESIAN_POINT('Ctrl Pts',(0.544190985999945,11.6,-11.155801321));
#154285=CARTESIAN_POINT('Ctrl Pts',(0.545613420999944,15.2,-11.158841164));
#154286=CARTESIAN_POINT('Ctrl Pts',(0.545613420999944,11.6,-11.158841164));
#154287=CARTESIAN_POINT('Ctrl Pts',(0.547040353999945,15.2,-11.161884336));
#154288=CARTESIAN_POINT('Ctrl Pts',(0.547040353999945,11.6,-11.161884336));
#154289=CARTESIAN_POINT('Ctrl Pts',(0.548471787999943,15.2,-11.164930828));
#154290=CARTESIAN_POINT('Ctrl Pts',(0.548471787999943,11.6,-11.164930828));
#154291=CARTESIAN_POINT('Ctrl Pts',(0.549907724999944,15.2,-11.167980631));
#154292=CARTESIAN_POINT('Ctrl Pts',(0.549907724999944,11.6,-11.167980631));
#154293=CARTESIAN_POINT('Ctrl Pts',(0.551348166999944,15.2,-11.171033733));
#154294=CARTESIAN_POINT('Ctrl Pts',(0.551348166999944,11.6,-11.171033733));
#154295=CARTESIAN_POINT('Ctrl Pts',(0.552793118999944,15.2,-11.174090123));
#154296=CARTESIAN_POINT('Ctrl Pts',(0.552793118999944,11.6,-11.174090123));
#154297=CARTESIAN_POINT('Ctrl Pts',(0.554242579999944,15.2,-11.177149794));
#154298=CARTESIAN_POINT('Ctrl Pts',(0.554242579999944,11.6,-11.177149794));
#154299=CARTESIAN_POINT('Ctrl Pts',(0.555696552999944,15.2,-11.180212734));
#154300=CARTESIAN_POINT('Ctrl Pts',(0.555696552999944,11.6,-11.180212734));
#154301=CARTESIAN_POINT('Ctrl Pts',(0.557155042999944,15.2,-11.183278932));
#154302=CARTESIAN_POINT('Ctrl Pts',(0.557155042999944,11.6,-11.183278932));
#154303=CARTESIAN_POINT('Ctrl Pts',(0.558618047999944,15.2,-11.186348379));
#154304=CARTESIAN_POINT('Ctrl Pts',(0.558618047999944,11.6,-11.186348379));
#154305=CARTESIAN_POINT('Ctrl Pts',(0.560085574999943,15.2,-11.189421065));
#154306=CARTESIAN_POINT('Ctrl Pts',(0.560085574999943,11.6,-11.189421065));
#154307=CARTESIAN_POINT('Ctrl Pts',(0.561557623999944,15.2,-11.192496979));
#154308=CARTESIAN_POINT('Ctrl Pts',(0.561557623999944,11.6,-11.192496979));
#154309=CARTESIAN_POINT('Ctrl Pts',(0.563034195999944,15.2,-11.195576112));
#154310=CARTESIAN_POINT('Ctrl Pts',(0.563034195999944,11.6,-11.195576112));
#154311=CARTESIAN_POINT('Ctrl Pts',(0.564515294999944,15.2,-11.198658453));
#154312=CARTESIAN_POINT('Ctrl Pts',(0.564515294999944,11.6,-11.198658453));
#154313=CARTESIAN_POINT('Ctrl Pts',(0.566000922999944,15.2,-11.201743993));
#154314=CARTESIAN_POINT('Ctrl Pts',(0.566000922999944,11.6,-11.201743993));
#154315=CARTESIAN_POINT('Ctrl Pts',(0.567491082999945,15.2,-11.204832721));
#154316=CARTESIAN_POINT('Ctrl Pts',(0.567491082999945,11.6,-11.204832721));
#154317=CARTESIAN_POINT('Ctrl Pts',(0.568985775999944,15.2,-11.207924627));
#154318=CARTESIAN_POINT('Ctrl Pts',(0.568985775999944,11.6,-11.207924627));
#154319=CARTESIAN_POINT('Ctrl Pts',(0.570485004999944,15.2,-11.211019702));
#154320=CARTESIAN_POINT('Ctrl Pts',(0.570485004999944,11.6,-11.211019702));
#154321=CARTESIAN_POINT('Ctrl Pts',(0.571988771999944,15.2,-11.214117935));
#154322=CARTESIAN_POINT('Ctrl Pts',(0.571988771999944,11.6,-11.214117935));
#154323=CARTESIAN_POINT('Ctrl Pts',(0.573497078999944,15.2,-11.217219316));
#154324=CARTESIAN_POINT('Ctrl Pts',(0.573497078999944,11.6,-11.217219316));
#154325=CARTESIAN_POINT('Ctrl Pts',(0.575009928999944,15.2,-11.220323837));
#154326=CARTESIAN_POINT('Ctrl Pts',(0.575009928999944,11.6,-11.220323837));
#154327=CARTESIAN_POINT('Ctrl Pts',(0.576527321999943,15.2,-11.223431485));
#154328=CARTESIAN_POINT('Ctrl Pts',(0.576527321999943,11.6,-11.223431485));
#154329=CARTESIAN_POINT('Ctrl Pts',(0.578049262999943,15.2,-11.226542253));
#154330=CARTESIAN_POINT('Ctrl Pts',(0.578049262999943,11.6,-11.226542253));
#154331=CARTESIAN_POINT('Ctrl Pts',(0.579575752999945,15.2,-11.229656128));
#154332=CARTESIAN_POINT('Ctrl Pts',(0.579575752999945,11.6,-11.229656128));
#154333=CARTESIAN_POINT('Ctrl Pts',(0.581106792999945,15.2,-11.232773103));
#154334=CARTESIAN_POINT('Ctrl Pts',(0.581106792999945,11.6,-11.232773103));
#154335=CARTESIAN_POINT('Ctrl Pts',(0.582642387999944,15.2,-11.235893168));
#154336=CARTESIAN_POINT('Ctrl Pts',(0.582642387999944,11.6,-11.235893168));
#154337=CARTESIAN_POINT('Ctrl Pts',(0.584182536999944,15.2,-11.23901631));
#154338=CARTESIAN_POINT('Ctrl Pts',(0.584182536999944,11.6,-11.23901631));
#154339=CARTESIAN_POINT('Ctrl Pts',(0.585727243999944,15.2,-11.242142523));
#154340=CARTESIAN_POINT('Ctrl Pts',(0.585727243999944,11.6,-11.242142523));
#154341=CARTESIAN_POINT('Ctrl Pts',(0.587276510999944,15.2,-11.245271795));
#154342=CARTESIAN_POINT('Ctrl Pts',(0.587276510999944,11.6,-11.245271795));
#154343=CARTESIAN_POINT('Ctrl Pts',(0.588830339999945,15.2,-11.248404117));
#154344=CARTESIAN_POINT('Ctrl Pts',(0.588830339999945,11.6,-11.248404117));
#154345=CARTESIAN_POINT('Ctrl Pts',(0.590388730999944,15.2,-11.251539479));
#154346=CARTESIAN_POINT('Ctrl Pts',(0.590388730999944,11.6,-11.251539479));
#154347=CARTESIAN_POINT('Ctrl Pts',(0.591951689999944,15.2,-11.254677871));
#154348=CARTESIAN_POINT('Ctrl Pts',(0.591951689999944,11.6,-11.254677871));
#154349=CARTESIAN_POINT('Ctrl Pts',(0.593519214999944,15.2,-11.257819284));
#154350=CARTESIAN_POINT('Ctrl Pts',(0.593519214999944,11.6,-11.257819284));
#154351=CARTESIAN_POINT('Ctrl Pts',(0.595091311999945,15.2,-11.260963707));
#154352=CARTESIAN_POINT('Ctrl Pts',(0.595091311999945,11.6,-11.260963707));
#154353=CARTESIAN_POINT('Ctrl Pts',(0.596667979999944,15.2,-11.264111132));
#154354=CARTESIAN_POINT('Ctrl Pts',(0.596667979999944,11.6,-11.264111132));
#154355=CARTESIAN_POINT('Ctrl Pts',(0.598249221999944,15.2,-11.267261548));
#154356=CARTESIAN_POINT('Ctrl Pts',(0.598249221999944,11.6,-11.267261548));
#154357=CARTESIAN_POINT('Ctrl Pts',(0.599835039999944,15.2,-11.270414946));
#154358=CARTESIAN_POINT('Ctrl Pts',(0.599835039999944,11.6,-11.270414946));
#154359=CARTESIAN_POINT('Ctrl Pts',(0.601425436999944,15.2,-11.273571316));
#154360=CARTESIAN_POINT('Ctrl Pts',(0.601425436999944,11.6,-11.273571316));
#154361=CARTESIAN_POINT('Ctrl Pts',(0.603020412999945,15.2,-11.276730648));
#154362=CARTESIAN_POINT('Ctrl Pts',(0.603020412999945,11.6,-11.276730648));
#154363=CARTESIAN_POINT('Ctrl Pts',(0.604619971999945,15.2,-11.279892934));
#154364=CARTESIAN_POINT('Ctrl Pts',(0.604619971999945,11.6,-11.279892934));
#154365=CARTESIAN_POINT('Ctrl Pts',(0.606224114999944,15.2,-11.283058161));
#154366=CARTESIAN_POINT('Ctrl Pts',(0.606224114999944,11.6,-11.283058161));
#154367=CARTESIAN_POINT('Ctrl Pts',(0.607832842999944,15.2,-11.286226323));
#154368=CARTESIAN_POINT('Ctrl Pts',(0.607832842999944,11.6,-11.286226323));
#154369=CARTESIAN_POINT('Ctrl Pts',(0.609446159999945,15.2,-11.289397409));
#154370=CARTESIAN_POINT('Ctrl Pts',(0.609446159999945,11.6,-11.289397409));
#154371=CARTESIAN_POINT('Ctrl Pts',(0.611064066999945,15.2,-11.29257141));
#154372=CARTESIAN_POINT('Ctrl Pts',(0.611064066999945,11.6,-11.29257141));
#154373=CARTESIAN_POINT('Ctrl Pts',(0.612686564999944,15.2,-11.295748315));
#154374=CARTESIAN_POINT('Ctrl Pts',(0.612686564999944,11.6,-11.295748315));
#154375=CARTESIAN_POINT('Ctrl Pts',(0.614313656999944,15.2,-11.298928116));
#154376=CARTESIAN_POINT('Ctrl Pts',(0.614313656999944,11.6,-11.298928116));
#154377=CARTESIAN_POINT('Ctrl Pts',(0.615945344999944,15.2,-11.302110802));
#154378=CARTESIAN_POINT('Ctrl Pts',(0.615945344999944,11.6,-11.302110802));
#154379=CARTESIAN_POINT('Ctrl Pts',(0.617581629999945,15.2,-11.305296365));
#154380=CARTESIAN_POINT('Ctrl Pts',(0.617581629999945,11.6,-11.305296365));
#154381=CARTESIAN_POINT('Ctrl Pts',(0.619222514999944,15.2,-11.308484795));
#154382=CARTESIAN_POINT('Ctrl Pts',(0.619222514999944,11.6,-11.308484795));
#154383=CARTESIAN_POINT('Ctrl Pts',(0.620868000999945,15.2,-11.311676082));
#154384=CARTESIAN_POINT('Ctrl Pts',(0.620868000999945,11.6,-11.311676082));
#154385=CARTESIAN_POINT('Ctrl Pts',(0.622518089999944,15.2,-11.314870217));
#154386=CARTESIAN_POINT('Ctrl Pts',(0.622518089999944,11.6,-11.314870217));
#154387=CARTESIAN_POINT('Ctrl Pts',(0.624172783999944,15.2,-11.31806719));
#154388=CARTESIAN_POINT('Ctrl Pts',(0.624172783999944,11.6,-11.31806719));
#154389=CARTESIAN_POINT('Ctrl Pts',(0.625832085999944,15.2,-11.321266994));
#154390=CARTESIAN_POINT('Ctrl Pts',(0.625832085999944,11.6,-11.321266994));
#154391=CARTESIAN_POINT('Ctrl Pts',(0.627495994999945,15.2,-11.324469616));
#154392=CARTESIAN_POINT('Ctrl Pts',(0.627495994999945,11.6,-11.324469616));
#154393=CARTESIAN_POINT('Ctrl Pts',(0.629164515999945,15.2,-11.327675049));
#154394=CARTESIAN_POINT('Ctrl Pts',(0.629164515999945,11.6,-11.327675049));
#154395=CARTESIAN_POINT('Ctrl Pts',(0.630837647999944,15.2,-11.330883282));
#154396=CARTESIAN_POINT('Ctrl Pts',(0.630837647999944,11.6,-11.330883282));
#154397=CARTESIAN_POINT('Ctrl Pts',(0.632515393999945,15.2,-11.334094307));
#154398=CARTESIAN_POINT('Ctrl Pts',(0.632515393999945,11.6,-11.334094307));
#154399=CARTESIAN_POINT('Ctrl Pts',(0.634197756999945,15.2,-11.337308115));
#154400=CARTESIAN_POINT('Ctrl Pts',(0.634197756999945,11.6,-11.337308115));
#154401=CARTESIAN_POINT('Ctrl Pts',(0.635884736999944,15.2,-11.340524695));
#154402=CARTESIAN_POINT('Ctrl Pts',(0.635884736999944,11.6,-11.340524695));
#154403=CARTESIAN_POINT('Ctrl Pts',(0.637576336999944,15.2,-11.343744038));
#154404=CARTESIAN_POINT('Ctrl Pts',(0.637576336999944,11.6,-11.343744038));
#154405=CARTESIAN_POINT('Ctrl Pts',(0.639272556999945,15.2,-11.346966135));
#154406=CARTESIAN_POINT('Ctrl Pts',(0.639272556999945,11.6,-11.346966135));
#154407=CARTESIAN_POINT('Ctrl Pts',(0.640973400999945,15.2,-11.350190979));
#154408=CARTESIAN_POINT('Ctrl Pts',(0.640973400999945,11.6,-11.350190979));
#154409=CARTESIAN_POINT('Ctrl Pts',(0.642678868999944,15.2,-11.353418557));
#154410=CARTESIAN_POINT('Ctrl Pts',(0.642678868999944,11.6,-11.353418557));
#154411=CARTESIAN_POINT('Ctrl Pts',(0.644388963999944,15.2,-11.356648862));
#154412=CARTESIAN_POINT('Ctrl Pts',(0.644388963999944,11.6,-11.356648862));
#154413=CARTESIAN_POINT('Ctrl Pts',(0.646103685999945,15.2,-11.359881884));
#154414=CARTESIAN_POINT('Ctrl Pts',(0.646103685999945,11.6,-11.359881884));
#154415=CARTESIAN_POINT('Ctrl Pts',(0.647823038999944,15.2,-11.363117614));
#154416=CARTESIAN_POINT('Ctrl Pts',(0.647823038999944,11.6,-11.363117614));
#154417=CARTESIAN_POINT('Ctrl Pts',(0.649547021999944,15.2,-11.366356043));
#154418=CARTESIAN_POINT('Ctrl Pts',(0.649547021999944,11.6,-11.366356043));
#154419=CARTESIAN_POINT('Ctrl Pts',(0.651275639999944,15.2,-11.369597161));
#154420=CARTESIAN_POINT('Ctrl Pts',(0.651275639999944,11.6,-11.369597161));
#154421=CARTESIAN_POINT('Ctrl Pts',(0.653008890999944,15.2,-11.37284096));
#154422=CARTESIAN_POINT('Ctrl Pts',(0.653008890999944,11.6,-11.37284096));
#154423=CARTESIAN_POINT('Ctrl Pts',(0.654746778999944,15.2,-11.37608743));
#154424=CARTESIAN_POINT('Ctrl Pts',(0.654746778999944,11.6,-11.37608743));
#154425=CARTESIAN_POINT('Ctrl Pts',(0.656489305999944,15.2,-11.379336561));
#154426=CARTESIAN_POINT('Ctrl Pts',(0.656489305999944,11.6,-11.379336561));
#154427=CARTESIAN_POINT('Ctrl Pts',(0.658236471999943,15.2,-11.382588345));
#154428=CARTESIAN_POINT('Ctrl Pts',(0.658236471999943,11.6,-11.382588345));
#154429=CARTESIAN_POINT('Ctrl Pts',(0.659988278999944,15.2,-11.385842772));
#154430=CARTESIAN_POINT('Ctrl Pts',(0.659988278999944,11.6,-11.385842772));
#154431=CARTESIAN_POINT('Ctrl Pts',(0.661744729999943,15.2,-11.389099835));
#154432=CARTESIAN_POINT('Ctrl Pts',(0.661744729999943,11.6,-11.389099835));
#154433=CARTESIAN_POINT('Ctrl Pts',(0.663505824999944,15.2,-11.392359523));
#154434=CARTESIAN_POINT('Ctrl Pts',(0.663505824999944,11.6,-11.392359523));
#154435=CARTESIAN_POINT('Ctrl Pts',(0.665271565999944,15.2,-11.395621827));
#154436=CARTESIAN_POINT('Ctrl Pts',(0.665271565999944,11.6,-11.395621827));
#154437=CARTESIAN_POINT('Ctrl Pts',(0.667041954999944,15.2,-11.39888674));
#154438=CARTESIAN_POINT('Ctrl Pts',(0.667041954999944,11.6,-11.39888674));
#154439=CARTESIAN_POINT('Ctrl Pts',(0.668816992999944,15.2,-11.402154251));
#154440=CARTESIAN_POINT('Ctrl Pts',(0.668816992999944,11.6,-11.402154251));
#154441=CARTESIAN_POINT('Ctrl Pts',(0.670596681999944,15.2,-11.405424352));
#154442=CARTESIAN_POINT('Ctrl Pts',(0.670596681999944,11.6,-11.405424352));
#154443=CARTESIAN_POINT('Ctrl Pts',(0.672381022999944,15.2,-11.408697032));
#154444=CARTESIAN_POINT('Ctrl Pts',(0.672381022999944,11.6,-11.408697032));
#154445=CARTESIAN_POINT('Ctrl Pts',(0.674170018999944,15.2,-11.411972283));
#154446=CARTESIAN_POINT('Ctrl Pts',(0.674170018999944,11.6,-11.411972283));
#154447=CARTESIAN_POINT('Ctrl Pts',(0.675963669999944,15.2,-11.415250096));
#154448=CARTESIAN_POINT('Ctrl Pts',(0.675963669999944,11.6,-11.415250096));
#154449=CARTESIAN_POINT('Ctrl Pts',(0.677761977999943,15.2,-11.418530461));
#154450=CARTESIAN_POINT('Ctrl Pts',(0.677761977999943,11.6,-11.418530461));
#154451=CARTESIAN_POINT('Ctrl Pts',(0.679564944999944,15.2,-11.421813369));
#154452=CARTESIAN_POINT('Ctrl Pts',(0.679564944999944,11.6,-11.421813369));
#154453=CARTESIAN_POINT('Ctrl Pts',(0.681372572999944,15.2,-11.425098811));
#154454=CARTESIAN_POINT('Ctrl Pts',(0.681372572999944,11.6,-11.425098811));
#154455=CARTESIAN_POINT('Ctrl Pts',(0.683184861999945,15.2,-11.42838678));
#154456=CARTESIAN_POINT('Ctrl Pts',(0.683184861999945,11.6,-11.42838678));
#154457=CARTESIAN_POINT('Ctrl Pts',(0.685001812999944,15.2,-11.431677269));
#154458=CARTESIAN_POINT('Ctrl Pts',(0.685001812999944,11.6,-11.431677269));
#154459=CARTESIAN_POINT('Ctrl Pts',(0.686823428999944,15.2,-11.434970268));
#154460=CARTESIAN_POINT('Ctrl Pts',(0.686823428999944,11.6,-11.434970268));
#154461=CARTESIAN_POINT('Ctrl Pts',(0.688649710999945,15.2,-11.438265769));
#154462=CARTESIAN_POINT('Ctrl Pts',(0.688649710999945,11.6,-11.438265769));
#154463=CARTESIAN_POINT('Ctrl Pts',(0.690480658999945,15.2,-11.441563763));
#154464=CARTESIAN_POINT('Ctrl Pts',(0.690480658999945,11.6,-11.441563763));
#154465=CARTESIAN_POINT('Ctrl Pts',(0.692316276999944,15.2,-11.444864239));
#154466=CARTESIAN_POINT('Ctrl Pts',(0.692316276999944,11.6,-11.444864239));
#154467=CARTESIAN_POINT('Ctrl Pts',(0.694156563999945,15.2,-11.448167187));
#154468=CARTESIAN_POINT('Ctrl Pts',(0.694156563999945,11.6,-11.448167187));
#154469=CARTESIAN_POINT('Ctrl Pts',(0.696001524999944,15.2,-11.451472595));
#154470=CARTESIAN_POINT('Ctrl Pts',(0.696001524999944,11.6,-11.451472595));
#154471=CARTESIAN_POINT('Ctrl Pts',(0.697851158999944,15.2,-11.454780453));
#154472=CARTESIAN_POINT('Ctrl Pts',(0.697851158999944,11.6,-11.454780453));
#154473=CARTESIAN_POINT('Ctrl Pts',(0.699705468999944,15.2,-11.458090751));
#154474=CARTESIAN_POINT('Ctrl Pts',(0.699705468999944,11.6,-11.458090751));
#154475=CARTESIAN_POINT('Ctrl Pts',(0.701564455999945,15.2,-11.461403481));
#154476=CARTESIAN_POINT('Ctrl Pts',(0.701564455999945,11.6,-11.461403481));
#154477=CARTESIAN_POINT('Ctrl Pts',(0.703428120999944,15.2,-11.464718637));
#154478=CARTESIAN_POINT('Ctrl Pts',(0.703428120999944,11.6,-11.464718637));
#154479=CARTESIAN_POINT('Ctrl Pts',(0.705296462999944,15.2,-11.468036216));
#154480=CARTESIAN_POINT('Ctrl Pts',(0.705296462999944,11.6,-11.468036216));
#154481=CARTESIAN_POINT('Ctrl Pts',(0.707169485999944,15.2,-11.471356215));
#154482=CARTESIAN_POINT('Ctrl Pts',(0.707169485999944,11.6,-11.471356215));
#154483=CARTESIAN_POINT('Ctrl Pts',(0.708671644999944,15.2,-11.474014149));
#154484=CARTESIAN_POINT('Ctrl Pts',(0.708671644999944,11.6,-11.474014149));
#154485=CARTESIAN_POINT('Ctrl Pts',(0.709800370999945,15.2,-11.476008688));
#154486=CARTESIAN_POINT('Ctrl Pts',(0.709800370999945,11.6,-11.476008688));
#154487=CARTESIAN_POINT('Ctrl Pts',(0.710553790999944,15.2,-11.477338863));
#154488=CARTESIAN_POINT('Ctrl Pts',(0.710553790999944,11.6,-11.477338863));
#154489=CARTESIAN_POINT('Ctrl Pts',(0.710930733999944,15.2,-11.478004072));
#154490=CARTESIAN_POINT('Ctrl Pts',(0.710930733999944,11.6,-11.478004072));
#154491=CARTESIAN_POINT('',(0.292001928999944,15.2,-10.370890023));
#154492=CARTESIAN_POINT('',(0.292001928999944,12.2,-10.370890023));
#154493=CARTESIAN_POINT('',(0.292001928999944,15.2,-10.370890023));
#154494=CARTESIAN_POINT('Ctrl Pts',(0.292001928999944,15.2,-10.370890023));
#154495=CARTESIAN_POINT('Ctrl Pts',(0.292021795999944,15.2,-10.371063245));
#154496=CARTESIAN_POINT('Ctrl Pts',(0.292062308999944,15.2,-10.371415731));
#154497=CARTESIAN_POINT('Ctrl Pts',(0.292123960999945,15.2,-10.371949799));
#154498=CARTESIAN_POINT('Ctrl Pts',(0.292207546999944,15.2,-10.372669176));
#154499=CARTESIAN_POINT('Ctrl Pts',(0.292314179999943,15.2,-10.373578975));
#154500=CARTESIAN_POINT('Ctrl Pts',(0.292423468999944,15.2,-10.374503411));
#154501=CARTESIAN_POINT('Ctrl Pts',(0.292534811999945,15.2,-10.375437184));
#154502=CARTESIAN_POINT('Ctrl Pts',(0.292648222999944,15.2,-10.376380266));
#154503=CARTESIAN_POINT('Ctrl Pts',(0.292763716999945,15.2,-10.377332627));
#154504=CARTESIAN_POINT('Ctrl Pts',(0.292881308999944,15.2,-10.378294239));
#154505=CARTESIAN_POINT('Ctrl Pts',(0.293001014999945,15.2,-10.379265074));
#154506=CARTESIAN_POINT('Ctrl Pts',(0.293122845999945,15.2,-10.380245102));
#154507=CARTESIAN_POINT('Ctrl Pts',(0.293246819999944,15.2,-10.381234297));
#154508=CARTESIAN_POINT('Ctrl Pts',(0.293372948999944,15.2,-10.382232628));
#154509=CARTESIAN_POINT('Ctrl Pts',(0.293501248999943,15.2,-10.383240069));
#154510=CARTESIAN_POINT('Ctrl Pts',(0.293631731999945,15.2,-10.384256592));
#154511=CARTESIAN_POINT('Ctrl Pts',(0.293764412999945,15.2,-10.385282168));
#154512=CARTESIAN_POINT('Ctrl Pts',(0.293899306999944,15.2,-10.38631677));
#154513=CARTESIAN_POINT('Ctrl Pts',(0.294036426999943,15.2,-10.387360371));
#154514=CARTESIAN_POINT('Ctrl Pts',(0.294175786999944,15.2,-10.388412945));
#154515=CARTESIAN_POINT('Ctrl Pts',(0.294317400999944,15.2,-10.389474461));
#154516=CARTESIAN_POINT('Ctrl Pts',(0.294461281999944,15.2,-10.390544895));
#154517=CARTESIAN_POINT('Ctrl Pts',(0.294607443999944,15.2,-10.391624218));
#154518=CARTESIAN_POINT('Ctrl Pts',(0.294755900999943,15.2,-10.392712404));
#154519=CARTESIAN_POINT('Ctrl Pts',(0.294906665999944,15.2,-10.393809427));
#154520=CARTESIAN_POINT('Ctrl Pts',(0.295059751999943,15.2,-10.394915259));
#154521=CARTESIAN_POINT('Ctrl Pts',(0.295215172999944,15.2,-10.396029875));
#154522=CARTESIAN_POINT('Ctrl Pts',(0.295372941999944,15.2,-10.397153247));
#154523=CARTESIAN_POINT('Ctrl Pts',(0.295533071999945,15.2,-10.39828535));
#154524=CARTESIAN_POINT('Ctrl Pts',(0.295695575999944,15.2,-10.399426157));
#154525=CARTESIAN_POINT('Ctrl Pts',(0.295860466999944,15.2,-10.400575642));
#154526=CARTESIAN_POINT('Ctrl Pts',(0.296027758999945,15.2,-10.401733778));
#154527=CARTESIAN_POINT('Ctrl Pts',(0.296197462999944,15.2,-10.402900542));
#154528=CARTESIAN_POINT('Ctrl Pts',(0.296369592999944,15.2,-10.404075906));
#154529=CARTESIAN_POINT('Ctrl Pts',(0.296544161999943,15.2,-10.405259845));
#154530=CARTESIAN_POINT('Ctrl Pts',(0.296721181999944,15.2,-10.406452335));
#154531=CARTESIAN_POINT('Ctrl Pts',(0.296900663999944,15.2,-10.407653347));
#154532=CARTESIAN_POINT('Ctrl Pts',(0.297082623999945,15.2,-10.408862859));
#154533=CARTESIAN_POINT('Ctrl Pts',(0.297267072999944,15.2,-10.410080845));
#154534=CARTESIAN_POINT('Ctrl Pts',(0.297454020999943,15.2,-10.411307279));
#154535=CARTESIAN_POINT('Ctrl Pts',(0.297643483999943,15.2,-10.412542137));
#154536=CARTESIAN_POINT('Ctrl Pts',(0.297835472999944,15.2,-10.413785393));
#154537=CARTESIAN_POINT('Ctrl Pts',(0.298029997999943,15.2,-10.415037024));
#154538=CARTESIAN_POINT('Ctrl Pts',(0.298227073999945,15.2,-10.416297005));
#154539=CARTESIAN_POINT('Ctrl Pts',(0.298426710999945,15.2,-10.41756531));
#154540=CARTESIAN_POINT('Ctrl Pts',(0.298628921999944,15.2,-10.418841915));
#154541=CARTESIAN_POINT('Ctrl Pts',(0.298874678413339,15.2,-10.420383772284));
#154542=CARTESIAN_POINT('Ctrl Pts',(0.299124331804587,15.2,-10.4219380104286));
#154543=CARTESIAN_POINT('Ctrl Pts',(0.299377904195303,15.2,-10.4235045735714));
#154544=CARTESIAN_POINT('Ctrl Pts',(0.299635420609226,15.2,-10.4250834208572));
#154545=CARTESIAN_POINT('Ctrl Pts',(0.299896902999944,15.2,-10.426674502));
#154546=CARTESIAN_POINT('Ctrl Pts',(0.300117460999945,15.2,-10.428008535));
#154547=CARTESIAN_POINT('Ctrl Pts',(0.300340685999944,15.2,-10.429350676));
#154548=CARTESIAN_POINT('Ctrl Pts',(0.300566589999944,15.2,-10.430700902));
#154549=CARTESIAN_POINT('Ctrl Pts',(0.300795183999943,15.2,-10.43205919));
#154550=CARTESIAN_POINT('Ctrl Pts',(0.301026478999944,15.2,-10.433425516));
#154551=CARTESIAN_POINT('Ctrl Pts',(0.301260486999944,15.2,-10.434799858));
#154552=CARTESIAN_POINT('Ctrl Pts',(0.301497219999945,15.2,-10.43618219));
#154553=CARTESIAN_POINT('Ctrl Pts',(0.301736685999944,15.2,-10.437572491));
#154554=CARTESIAN_POINT('Ctrl Pts',(0.301978897999945,15.2,-10.438970738));
#154555=CARTESIAN_POINT('Ctrl Pts',(0.302223867999943,15.2,-10.440376907));
#154556=CARTESIAN_POINT('Ctrl Pts',(0.302471604999944,15.2,-10.441790977));
#154557=CARTESIAN_POINT('Ctrl Pts',(0.302722120999944,15.2,-10.443212923));
#154558=CARTESIAN_POINT('Ctrl Pts',(0.302975424999945,15.2,-10.444642725));
#154559=CARTESIAN_POINT('Ctrl Pts',(0.303231531999945,15.2,-10.446080357));
#154560=CARTESIAN_POINT('Ctrl Pts',(0.303490447999945,15.2,-10.447525799));
#154561=CARTESIAN_POINT('Ctrl Pts',(0.303752185999944,15.2,-10.448979029));
#154562=CARTESIAN_POINT('Ctrl Pts',(0.304016755999944,15.2,-10.450440023));
#154563=CARTESIAN_POINT('Ctrl Pts',(0.304284168999944,15.2,-10.451908761));
#154564=CARTESIAN_POINT('Ctrl Pts',(0.304554434999943,15.2,-10.453385218));
#154565=CARTESIAN_POINT('Ctrl Pts',(0.304827565999943,15.2,-10.454869375));
#154566=CARTESIAN_POINT('Ctrl Pts',(0.305103568999944,15.2,-10.456361208));
#154567=CARTESIAN_POINT('Ctrl Pts',(0.305382456999944,15.2,-10.457860694));
#154568=CARTESIAN_POINT('Ctrl Pts',(0.305664239999944,15.2,-10.459367814));
#154569=CARTESIAN_POINT('Ctrl Pts',(0.305948927999945,15.2,-10.460882546));
#154570=CARTESIAN_POINT('Ctrl Pts',(0.306236529999945,15.2,-10.462404866));
#154571=CARTESIAN_POINT('Ctrl Pts',(0.306527057999944,15.2,-10.463934755));
#154572=CARTESIAN_POINT('Ctrl Pts',(0.306820520999944,15.2,-10.46547219));
#154573=CARTESIAN_POINT('Ctrl Pts',(0.307116928999944,15.2,-10.46701715));
#154574=CARTESIAN_POINT('Ctrl Pts',(0.307416291999945,15.2,-10.468569615));
#154575=CARTESIAN_POINT('Ctrl Pts',(0.307718619999945,15.2,-10.470129561));
#154576=CARTESIAN_POINT('Ctrl Pts',(0.308023921999944,15.2,-10.47169697));
#154577=CARTESIAN_POINT('Ctrl Pts',(0.308332209999945,15.2,-10.473271818));
#154578=CARTESIAN_POINT('Ctrl Pts',(0.308643490999945,15.2,-10.474854086));
#154579=CARTESIAN_POINT('Ctrl Pts',(0.308957776999945,15.2,-10.476443753));
#154580=CARTESIAN_POINT('Ctrl Pts',(0.309275075999944,15.2,-10.478040796));
#154581=CARTESIAN_POINT('Ctrl Pts',(0.309595398999944,15.2,-10.479645198));
#154582=CARTESIAN_POINT('Ctrl Pts',(0.309918754999944,15.2,-10.481256934));
#154583=CARTESIAN_POINT('Ctrl Pts',(0.310245152999944,15.2,-10.482875987));
#154584=CARTESIAN_POINT('Ctrl Pts',(0.310574601999944,15.2,-10.484502335));
#154585=CARTESIAN_POINT('Ctrl Pts',(0.310907112999944,15.2,-10.486135957));
#154586=CARTESIAN_POINT('Ctrl Pts',(0.311242694999944,15.2,-10.487776833));
#154587=CARTESIAN_POINT('Ctrl Pts',(0.311581355999945,15.2,-10.489424943));
#154588=CARTESIAN_POINT('Ctrl Pts',(0.311923106999944,15.2,-10.491080266));
#154589=CARTESIAN_POINT('Ctrl Pts',(0.312267955999944,15.2,-10.492742782));
#154590=CARTESIAN_POINT('Ctrl Pts',(0.312615911999944,15.2,-10.494412473));
#154591=CARTESIAN_POINT('Ctrl Pts',(0.312966985999944,15.2,-10.496089316));
#154592=CARTESIAN_POINT('Ctrl Pts',(0.313321185999945,15.2,-10.497773293));
#154593=CARTESIAN_POINT('Ctrl Pts',(0.313678518999945,15.2,-10.499464382));
#154594=CARTESIAN_POINT('Ctrl Pts',(0.314038995999945,15.2,-10.501162565));
#154595=CARTESIAN_POINT('Ctrl Pts',(0.314402626999944,15.2,-10.502867822));
#154596=CARTESIAN_POINT('Ctrl Pts',(0.314769418999944,15.2,-10.504580133));
#154597=CARTESIAN_POINT('Ctrl Pts',(0.315139380999945,15.2,-10.506299478));
#154598=CARTESIAN_POINT('Ctrl Pts',(0.315512523999945,15.2,-10.508025838));
#154599=CARTESIAN_POINT('Ctrl Pts',(0.315888853999944,15.2,-10.509759194));
#154600=CARTESIAN_POINT('Ctrl Pts',(0.316268379999943,15.2,-10.511499525));
#154601=CARTESIAN_POINT('Ctrl Pts',(0.316651111999944,15.2,-10.513246812));
#154602=CARTESIAN_POINT('Ctrl Pts',(0.317037058999944,15.2,-10.515001037));
#154603=CARTESIAN_POINT('Ctrl Pts',(0.317426227999944,15.2,-10.516762179));
#154604=CARTESIAN_POINT('Ctrl Pts',(0.317818627999945,15.2,-10.518530222));
#154605=CARTESIAN_POINT('Ctrl Pts',(0.318214267999943,15.2,-10.520305143));
#154606=CARTESIAN_POINT('Ctrl Pts',(0.318613155999945,15.2,-10.522086924));
#154607=CARTESIAN_POINT('Ctrl Pts',(0.319015301999944,15.2,-10.523875548));
#154608=CARTESIAN_POINT('Ctrl Pts',(0.319420711999945,15.2,-10.525670994));
#154609=CARTESIAN_POINT('Ctrl Pts',(0.319829394999944,15.2,-10.527473244));
#154610=CARTESIAN_POINT('Ctrl Pts',(0.320241359999944,15.2,-10.529282279));
#154611=CARTESIAN_POINT('Ctrl Pts',(0.320656615999945,15.2,-10.53109808));
#154612=CARTESIAN_POINT('Ctrl Pts',(0.321075168999944,15.2,-10.532920629));
#154613=CARTESIAN_POINT('Ctrl Pts',(0.321497027999945,15.2,-10.534749907));
#154614=CARTESIAN_POINT('Ctrl Pts',(0.321922202999945,15.2,-10.536585896));
#154615=CARTESIAN_POINT('Ctrl Pts',(0.322350699999945,15.2,-10.538428576));
#154616=CARTESIAN_POINT('Ctrl Pts',(0.322782527999944,15.2,-10.54027793));
#154617=CARTESIAN_POINT('Ctrl Pts',(0.323217693999943,15.2,-10.54213394));
#154618=CARTESIAN_POINT('Ctrl Pts',(0.323656205999944,15.2,-10.543996587));
#154619=CARTESIAN_POINT('Ctrl Pts',(0.324098074999943,15.2,-10.545865852));
#154620=CARTESIAN_POINT('Ctrl Pts',(0.324543303999943,15.2,-10.547741717));
#154621=CARTESIAN_POINT('Ctrl Pts',(0.324991904999944,15.2,-10.549624165));
#154622=CARTESIAN_POINT('Ctrl Pts',(0.325443882999944,15.2,-10.551513176));
#154623=CARTESIAN_POINT('Ctrl Pts',(0.325899247999945,15.2,-10.553408734));
#154624=CARTESIAN_POINT('Ctrl Pts',(0.326358006999945,15.2,-10.555310821));
#154625=CARTESIAN_POINT('Ctrl Pts',(0.326820166999945,15.2,-10.557219417));
#154626=CARTESIAN_POINT('Ctrl Pts',(0.327285734999944,15.2,-10.559134506));
#154627=CARTESIAN_POINT('Ctrl Pts',(0.327754721999945,15.2,-10.56105607));
#154628=CARTESIAN_POINT('Ctrl Pts',(0.328227131999944,15.2,-10.562984091));
#154629=CARTESIAN_POINT('Ctrl Pts',(0.328702974999944,15.2,-10.56491855));
#154630=CARTESIAN_POINT('Ctrl Pts',(0.329182255999945,15.2,-10.566859432));
#154631=CARTESIAN_POINT('Ctrl Pts',(0.329664984999944,15.2,-10.568806718));
#154632=CARTESIAN_POINT('Ctrl Pts',(0.330151167999944,15.2,-10.57076039));
#154633=CARTESIAN_POINT('Ctrl Pts',(0.330640813999944,15.2,-10.572720431));
#154634=CARTESIAN_POINT('Ctrl Pts',(0.331133927999945,15.2,-10.574686823));
#154635=CARTESIAN_POINT('Ctrl Pts',(0.331630518999945,15.2,-10.57665955));
#154636=CARTESIAN_POINT('Ctrl Pts',(0.332130593999944,15.2,-10.578638595));
#154637=CARTESIAN_POINT('Ctrl Pts',(0.332634160999945,15.2,-10.580623937));
#154638=CARTESIAN_POINT('Ctrl Pts',(0.333141224999943,15.2,-10.582615564));
#154639=CARTESIAN_POINT('Ctrl Pts',(0.333651795999945,15.2,-10.584613455));
#154640=CARTESIAN_POINT('Ctrl Pts',(0.334165878999944,15.2,-10.586617594));
#154641=CARTESIAN_POINT('Ctrl Pts',(0.334683482999945,15.2,-10.588627965));
#154642=CARTESIAN_POINT('Ctrl Pts',(0.335204611999943,15.2,-10.59064455));
#154643=CARTESIAN_POINT('Ctrl Pts',(0.335729277999944,15.2,-10.592667332));
#154644=CARTESIAN_POINT('Ctrl Pts',(0.336257482999944,15.2,-10.594696293));
#154645=CARTESIAN_POINT('Ctrl Pts',(0.336789236999945,15.2,-10.59673142));
#154646=CARTESIAN_POINT('Ctrl Pts',(0.337324545999945,15.2,-10.598772692));
#154647=CARTESIAN_POINT('Ctrl Pts',(0.337863417999945,15.2,-10.600820093));
#154648=CARTESIAN_POINT('Ctrl Pts',(0.338405857999945,15.2,-10.602873609));
#154649=CARTESIAN_POINT('Ctrl Pts',(0.338951873999944,15.2,-10.60493322));
#154650=CARTESIAN_POINT('Ctrl Pts',(0.339501472999943,15.2,-10.606998913));
#154651=CARTESIAN_POINT('Ctrl Pts',(0.340054661999943,15.2,-10.609070667));
#154652=CARTESIAN_POINT('Ctrl Pts',(0.340611446999944,15.2,-10.611148469));
#154653=CARTESIAN_POINT('Ctrl Pts',(0.341171834999944,15.2,-10.613232302));
#154654=CARTESIAN_POINT('Ctrl Pts',(0.341735832999944,15.2,-10.615322148));
#154655=CARTESIAN_POINT('Ctrl Pts',(0.342303446999944,15.2,-10.617417992));
#154656=CARTESIAN_POINT('Ctrl Pts',(0.342874684999943,15.2,-10.619519817));
#154657=CARTESIAN_POINT('Ctrl Pts',(0.343449551999945,15.2,-10.621627608));
#154658=CARTESIAN_POINT('Ctrl Pts',(0.344028054999944,15.2,-10.623741347));
#154659=CARTESIAN_POINT('Ctrl Pts',(0.344610201999943,15.2,-10.625861018));
#154660=CARTESIAN_POINT('Ctrl Pts',(0.345195997999944,15.2,-10.627986606));
#154661=CARTESIAN_POINT('Ctrl Pts',(0.345785448999945,15.2,-10.630118095));
#154662=CARTESIAN_POINT('Ctrl Pts',(0.346378563999944,15.2,-10.632255468));
#154663=CARTESIAN_POINT('Ctrl Pts',(0.346975346999944,15.2,-10.634398708));
#154664=CARTESIAN_POINT('Ctrl Pts',(0.347575804999943,15.2,-10.636547803));
#154665=CARTESIAN_POINT('Ctrl Pts',(0.348179944999943,15.2,-10.638702732));
#154666=CARTESIAN_POINT('Ctrl Pts',(0.348787772999944,15.2,-10.640863483));
#154667=CARTESIAN_POINT('Ctrl Pts',(0.349399294999945,15.2,-10.643030038));
#154668=CARTESIAN_POINT('Ctrl Pts',(0.350014516999944,15.2,-10.645202383));
#154669=CARTESIAN_POINT('Ctrl Pts',(0.350633445999945,15.2,-10.647380501));
#154670=CARTESIAN_POINT('Ctrl Pts',(0.351256087999945,15.2,-10.649564376));
#154671=CARTESIAN_POINT('Ctrl Pts',(0.351882449999945,15.2,-10.651753993));
#154672=CARTESIAN_POINT('Ctrl Pts',(0.352512535999944,15.2,-10.653949337));
#154673=CARTESIAN_POINT('Ctrl Pts',(0.353146353999945,15.2,-10.656150391));
#154674=CARTESIAN_POINT('Ctrl Pts',(0.353783908999944,15.2,-10.658357141));
#154675=CARTESIAN_POINT('Ctrl Pts',(0.354425208999943,15.2,-10.660569571));
#154676=CARTESIAN_POINT('Ctrl Pts',(0.355070257999944,15.2,-10.662787664));
#154677=CARTESIAN_POINT('Ctrl Pts',(0.355719062999944,15.2,-10.665011407));
#154678=CARTESIAN_POINT('Ctrl Pts',(0.356371629999943,15.2,-10.667240784));
#154679=CARTESIAN_POINT('Ctrl Pts',(0.357027963999944,15.2,-10.669475778));
#154680=CARTESIAN_POINT('Ctrl Pts',(0.357688070999943,15.2,-10.671716375));
#154681=CARTESIAN_POINT('Ctrl Pts',(0.358351957999944,15.2,-10.673962561));
#154682=CARTESIAN_POINT('Ctrl Pts',(0.359019631999944,15.2,-10.676214319));
#154683=CARTESIAN_POINT('Ctrl Pts',(0.359691094999944,15.2,-10.678471635));
#154684=CARTESIAN_POINT('Ctrl Pts',(0.360366356999944,15.2,-10.680734493));
#154685=CARTESIAN_POINT('Ctrl Pts',(0.361045420999944,15.2,-10.683002879));
#154686=CARTESIAN_POINT('Ctrl Pts',(0.361728292999944,15.2,-10.685276775));
#154687=CARTESIAN_POINT('Ctrl Pts',(0.362414979999944,15.2,-10.687556171));
#154688=CARTESIAN_POINT('Ctrl Pts',(0.363105486999944,15.2,-10.689841047));
#154689=CARTESIAN_POINT('Ctrl Pts',(0.363799819999944,15.2,-10.692131392));
#154690=CARTESIAN_POINT('Ctrl Pts',(0.364497983999945,15.2,-10.69442719));
#154691=CARTESIAN_POINT('Ctrl Pts',(0.365199985999943,15.2,-10.696728424));
#154692=CARTESIAN_POINT('Ctrl Pts',(0.365905829999944,15.2,-10.699035082));
#154693=CARTESIAN_POINT('Ctrl Pts',(0.366615521999943,15.2,-10.701347148));
#154694=CARTESIAN_POINT('Ctrl Pts',(0.367329068999943,15.2,-10.703664607));
#154695=CARTESIAN_POINT('Ctrl Pts',(0.368046474999945,15.2,-10.705987445));
#154696=CARTESIAN_POINT('Ctrl Pts',(0.368767745999945,15.2,-10.708315648));
#154697=CARTESIAN_POINT('Ctrl Pts',(0.369492886999945,15.2,-10.710649199));
#154698=CARTESIAN_POINT('Ctrl Pts',(0.370221902999944,15.2,-10.712988086));
#154699=CARTESIAN_POINT('Ctrl Pts',(0.370954801999943,15.2,-10.715332293));
#154700=CARTESIAN_POINT('Ctrl Pts',(0.371691585999944,15.2,-10.717681807));
#154701=CARTESIAN_POINT('Ctrl Pts',(0.372432262999943,15.2,-10.720036612));
#154702=CARTESIAN_POINT('Ctrl Pts',(0.373176837999944,15.2,-10.722396693));
#154703=CARTESIAN_POINT('Ctrl Pts',(0.373925314999944,15.2,-10.724762038));
#154704=CARTESIAN_POINT('Ctrl Pts',(0.374677699999945,15.2,-10.72713263));
#154705=CARTESIAN_POINT('Ctrl Pts',(0.375433997999943,15.2,-10.729508457));
#154706=CARTESIAN_POINT('Ctrl Pts',(0.376194214999943,15.2,-10.731889504));
#154707=CARTESIAN_POINT('Ctrl Pts',(0.376958354999944,15.2,-10.734275757));
#154708=CARTESIAN_POINT('Ctrl Pts',(0.377726424999943,15.2,-10.7366672));
#154709=CARTESIAN_POINT('Ctrl Pts',(0.378498428999944,15.2,-10.73906382));
#154710=CARTESIAN_POINT('Ctrl Pts',(0.379274372999945,15.2,-10.741465604));
#154711=CARTESIAN_POINT('Ctrl Pts',(0.380054259999945,15.2,-10.743872536));
#154712=CARTESIAN_POINT('Ctrl Pts',(0.380838096999945,15.2,-10.746284604));
#154713=CARTESIAN_POINT('Ctrl Pts',(0.381625889999944,15.2,-10.748701792));
#154714=CARTESIAN_POINT('Ctrl Pts',(0.382417640999944,15.2,-10.751124087));
#154715=CARTESIAN_POINT('Ctrl Pts',(0.383213356999944,15.2,-10.753551475));
#154716=CARTESIAN_POINT('Ctrl Pts',(0.384013043999945,15.2,-10.755983942));
#154717=CARTESIAN_POINT('Ctrl Pts',(0.384816703999944,15.2,-10.758421474));
#154718=CARTESIAN_POINT('Ctrl Pts',(0.385624345999943,15.2,-10.760864057));
#154719=CARTESIAN_POINT('Ctrl Pts',(0.386435970999944,15.2,-10.763311678));
#154720=CARTESIAN_POINT('Ctrl Pts',(0.387251585999945,15.2,-10.765764322));
#154721=CARTESIAN_POINT('Ctrl Pts',(0.388071194999944,15.2,-10.768221976));
#154722=CARTESIAN_POINT('Ctrl Pts',(0.388894804999945,15.2,-10.770684626));
#154723=CARTESIAN_POINT('Ctrl Pts',(0.389722417999945,15.2,-10.773152259));
#154724=CARTESIAN_POINT('Ctrl Pts',(0.390554040999945,15.2,-10.77562486));
#154725=CARTESIAN_POINT('Ctrl Pts',(0.391389675999945,15.2,-10.778102417));
#154726=CARTESIAN_POINT('Ctrl Pts',(0.392229331999945,15.2,-10.780584915));
#154727=CARTESIAN_POINT('Ctrl Pts',(0.393073008999943,15.2,-10.78307234));
#154728=CARTESIAN_POINT('Ctrl Pts',(0.393920715999944,15.2,-10.785564681));
#154729=CARTESIAN_POINT('Ctrl Pts',(0.394772454999943,15.2,-10.788061922));
#154730=CARTESIAN_POINT('Ctrl Pts',(0.395628231999944,15.2,-10.790564051));
#154731=CARTESIAN_POINT('Ctrl Pts',(0.396488050999944,15.2,-10.793071054));
#154732=CARTESIAN_POINT('Ctrl Pts',(0.397351916999943,15.2,-10.795582918));
#154733=CARTESIAN_POINT('Ctrl Pts',(0.398219834999944,15.2,-10.798099629));
#154734=CARTESIAN_POINT('Ctrl Pts',(0.399091808999945,15.2,-10.800621174));
#154735=CARTESIAN_POINT('Ctrl Pts',(0.399967842999944,15.2,-10.80314754));
#154736=CARTESIAN_POINT('Ctrl Pts',(0.400847942999943,15.2,-10.805678712));
#154737=CARTESIAN_POINT('Ctrl Pts',(0.401732111999945,15.2,-10.808214679));
#154738=CARTESIAN_POINT('Ctrl Pts',(0.402620355999943,15.2,-10.810755427));
#154739=CARTESIAN_POINT('Ctrl Pts',(0.403512678999943,15.2,-10.813300943));
#154740=CARTESIAN_POINT('Ctrl Pts',(0.404409085999945,15.2,-10.815851213));
#154741=CARTESIAN_POINT('Ctrl Pts',(0.405309579999944,15.2,-10.818406225));
#154742=CARTESIAN_POINT('Ctrl Pts',(0.406214165999945,15.2,-10.820965964));
#154743=CARTESIAN_POINT('Ctrl Pts',(0.407122848999943,15.2,-10.82353042));
#154744=CARTESIAN_POINT('Ctrl Pts',(0.408035631999945,15.2,-10.826099577));
#154745=CARTESIAN_POINT('Ctrl Pts',(0.408952521999945,15.2,-10.828673424));
#154746=CARTESIAN_POINT('Ctrl Pts',(0.409873521999945,15.2,-10.831251946));
#154747=CARTESIAN_POINT('Ctrl Pts',(0.410798634999944,15.2,-10.833835132));
#154748=CARTESIAN_POINT('Ctrl Pts',(0.411727865999945,15.2,-10.836422969));
#154749=CARTESIAN_POINT('Ctrl Pts',(0.412661221999944,15.2,-10.839015443));
#154750=CARTESIAN_POINT('Ctrl Pts',(0.413598702999943,15.2,-10.841612542));
#154751=CARTESIAN_POINT('Ctrl Pts',(0.414540315999944,15.2,-10.844214253));
#154752=CARTESIAN_POINT('Ctrl Pts',(0.415486064999945,15.2,-10.846820562));
#154753=CARTESIAN_POINT('Ctrl Pts',(0.416435952999944,15.2,-10.849431457));
#154754=CARTESIAN_POINT('Ctrl Pts',(0.417389984999945,15.2,-10.852046927));
#154755=CARTESIAN_POINT('Ctrl Pts',(0.418348164999944,15.2,-10.854666958));
#154756=CARTESIAN_POINT('Ctrl Pts',(0.419310496999945,15.2,-10.857291535));
#154757=CARTESIAN_POINT('Ctrl Pts',(0.420276985999944,15.2,-10.859920649));
#154758=CARTESIAN_POINT('Ctrl Pts',(0.421247635999944,15.2,-10.862554285));
#154759=CARTESIAN_POINT('Ctrl Pts',(0.422222449999945,15.2,-10.865192432));
#154760=CARTESIAN_POINT('Ctrl Pts',(0.423201432999945,15.2,-10.867835076));
#154761=CARTESIAN_POINT('Ctrl Pts',(0.424184586999944,15.2,-10.870482205));
#154762=CARTESIAN_POINT('Ctrl Pts',(0.425171919999944,15.2,-10.873133806));
#154763=CARTESIAN_POINT('Ctrl Pts',(0.426163432999944,15.2,-10.875789868));
#154764=CARTESIAN_POINT('Ctrl Pts',(0.427159130999945,15.2,-10.878450378));
#154765=CARTESIAN_POINT('Ctrl Pts',(0.428159016999944,15.2,-10.881115322));
#154766=CARTESIAN_POINT('Ctrl Pts',(0.429163096999944,15.2,-10.883784689));
#154767=CARTESIAN_POINT('Ctrl Pts',(0.430171372999943,15.2,-10.886458467));
#154768=CARTESIAN_POINT('Ctrl Pts',(0.431183849999943,15.2,-10.889136642));
#154769=CARTESIAN_POINT('Ctrl Pts',(0.432200529999944,15.2,-10.891819203));
#154770=CARTESIAN_POINT('Ctrl Pts',(0.433221419999944,15.2,-10.894506138));
#154771=CARTESIAN_POINT('Ctrl Pts',(0.434246522999944,15.2,-10.897197434));
#154772=CARTESIAN_POINT('Ctrl Pts',(0.435275840999945,15.2,-10.899893077));
#154773=CARTESIAN_POINT('Ctrl Pts',(0.436309378999944,15.2,-10.902593058));
#154774=CARTESIAN_POINT('Ctrl Pts',(0.437347139999943,15.2,-10.905297364));
#154775=CARTESIAN_POINT('Ctrl Pts',(0.438389128999944,15.2,-10.908005981));
#154776=CARTESIAN_POINT('Ctrl Pts',(0.439435350999944,15.2,-10.910718898));
#154777=CARTESIAN_POINT('Ctrl Pts',(0.440485805999945,15.2,-10.913436104));
#154778=CARTESIAN_POINT('Ctrl Pts',(0.441540500999944,15.2,-10.916157585));
#154779=CARTESIAN_POINT('Ctrl Pts',(0.442599438999943,15.2,-10.91888333));
#154780=CARTESIAN_POINT('Ctrl Pts',(0.443662621999945,15.2,-10.921613326));
#154781=CARTESIAN_POINT('Ctrl Pts',(0.444730055999945,15.2,-10.924347562));
#154782=CARTESIAN_POINT('Ctrl Pts',(0.445801742999944,15.2,-10.927086026));
#154783=CARTESIAN_POINT('Ctrl Pts',(0.446877687999944,15.2,-10.929828706));
#154784=CARTESIAN_POINT('Ctrl Pts',(0.447957893999943,15.2,-10.932575589));
#154785=CARTESIAN_POINT('Ctrl Pts',(0.449042363999944,15.2,-10.935326664));
#154786=CARTESIAN_POINT('Ctrl Pts',(0.450131101999943,15.2,-10.93808192));
#154787=CARTESIAN_POINT('Ctrl Pts',(0.451224112999944,15.2,-10.940841343));
#154788=CARTESIAN_POINT('Ctrl Pts',(0.452321397999944,15.2,-10.943604921));
#154789=CARTESIAN_POINT('Ctrl Pts',(0.453422961999944,15.2,-10.946372645));
#154790=CARTESIAN_POINT('Ctrl Pts',(0.454528808999944,15.2,-10.949144502));
#154791=CARTESIAN_POINT('Ctrl Pts',(0.455638941999944,15.2,-10.951920478));
#154792=CARTESIAN_POINT('Ctrl Pts',(0.456753363999944,15.2,-10.954700564));
#154793=CARTESIAN_POINT('Ctrl Pts',(0.457872078999945,15.2,-10.957484747));
#154794=CARTESIAN_POINT('Ctrl Pts',(0.458995090999944,15.2,-10.960273016));
#154795=CARTESIAN_POINT('Ctrl Pts',(0.460122400999945,15.2,-10.963065359));
#154796=CARTESIAN_POINT('Ctrl Pts',(0.461254015999945,15.2,-10.965861764));
#154797=CARTESIAN_POINT('Ctrl Pts',(0.462389937999944,15.2,-10.96866222));
#154798=CARTESIAN_POINT('Ctrl Pts',(0.463530168999944,15.2,-10.971466714));
#154799=CARTESIAN_POINT('Ctrl Pts',(0.464674712999944,15.2,-10.974275237));
#154800=CARTESIAN_POINT('Ctrl Pts',(0.465823575999943,15.2,-10.977087774));
#154801=CARTESIAN_POINT('Ctrl Pts',(0.466976756999945,15.2,-10.979904316));
#154802=CARTESIAN_POINT('Ctrl Pts',(0.468134261999945,15.2,-10.982724852));
#154803=CARTESIAN_POINT('Ctrl Pts',(0.469296094999944,15.2,-10.985549368));
#154804=CARTESIAN_POINT('Ctrl Pts',(0.470462256999945,15.2,-10.988377854));
#154805=CARTESIAN_POINT('Ctrl Pts',(0.471632752999945,15.2,-10.991210298));
#154806=CARTESIAN_POINT('Ctrl Pts',(0.472807584999944,15.2,-10.994046689));
#154807=CARTESIAN_POINT('Ctrl Pts',(0.473986757999943,15.2,-10.996887016));
#154808=CARTESIAN_POINT('Ctrl Pts',(0.475170271999945,15.2,-10.999731268));
#154809=CARTESIAN_POINT('Ctrl Pts',(0.476358134999944,15.2,-11.002579431));
#154810=CARTESIAN_POINT('Ctrl Pts',(0.477550345999944,15.2,-11.005431497));
#154811=CARTESIAN_POINT('Ctrl Pts',(0.478746909999943,15.2,-11.008287453));
#154812=CARTESIAN_POINT('Ctrl Pts',(0.479947829999944,15.2,-11.011147287));
#154813=CARTESIAN_POINT('Ctrl Pts',(0.481153109999944,15.2,-11.014010988));
#154814=CARTESIAN_POINT('Ctrl Pts',(0.482362750999944,15.2,-11.016878547));
#154815=CARTESIAN_POINT('Ctrl Pts',(0.483576757999945,15.2,-11.01974995));
#154816=CARTESIAN_POINT('Ctrl Pts',(0.484795132999943,15.2,-11.022625188));
#154817=CARTESIAN_POINT('Ctrl Pts',(0.486017879999944,15.2,-11.025504247));
#154818=CARTESIAN_POINT('Ctrl Pts',(0.487245001999945,15.2,-11.028387119));
#154819=CARTESIAN_POINT('Ctrl Pts',(0.488476501999945,15.2,-11.031273791));
#154820=CARTESIAN_POINT('Ctrl Pts',(0.489712381999944,15.2,-11.034164252));
#154821=CARTESIAN_POINT('Ctrl Pts',(0.490952645999944,15.2,-11.037058491));
#154822=CARTESIAN_POINT('Ctrl Pts',(0.492197297999944,15.2,-11.039956497));
#154823=CARTESIAN_POINT('Ctrl Pts',(0.493446337999943,15.2,-11.04285826));
#154824=CARTESIAN_POINT('Ctrl Pts',(0.494699771999944,15.2,-11.045763768));
#154825=CARTESIAN_POINT('Ctrl Pts',(0.495957600999944,15.2,-11.04867301));
#154826=CARTESIAN_POINT('Ctrl Pts',(0.497219829999944,15.2,-11.051585974));
#154827=CARTESIAN_POINT('Ctrl Pts',(0.498486459999944,15.2,-11.05450265));
#154828=CARTESIAN_POINT('Ctrl Pts',(0.499757494999944,15.2,-11.057423028));
#154829=CARTESIAN_POINT('Ctrl Pts',(0.501032935999944,15.2,-11.060347096));
#154830=CARTESIAN_POINT('Ctrl Pts',(0.502312788999945,15.2,-11.063274844));
#154831=CARTESIAN_POINT('Ctrl Pts',(0.503597054999945,15.2,-11.066206259));
#154832=CARTESIAN_POINT('Ctrl Pts',(0.504885736999944,15.2,-11.069141332));
#154833=CARTESIAN_POINT('Ctrl Pts',(0.506178838999943,15.2,-11.072080052));
#154834=CARTESIAN_POINT('Ctrl Pts',(0.507476362999945,15.2,-11.075022407));
#154835=CARTESIAN_POINT('Ctrl Pts',(0.508778309999944,15.2,-11.077968387));
#154836=CARTESIAN_POINT('Ctrl Pts',(0.510084685999944,15.2,-11.080917982));
#154837=CARTESIAN_POINT('Ctrl Pts',(0.511395492999944,15.2,-11.08387118));
#154838=CARTESIAN_POINT('Ctrl Pts',(0.512710730999945,15.2,-11.086827972));
#154839=CARTESIAN_POINT('Ctrl Pts',(0.514030406999945,15.2,-11.089788344));
#154840=CARTESIAN_POINT('Ctrl Pts',(0.515354519999944,15.2,-11.092752289));
#154841=CARTESIAN_POINT('Ctrl Pts',(0.516683075999944,15.2,-11.095719793));
#154842=CARTESIAN_POINT('Ctrl Pts',(0.518016074999944,15.2,-11.098690848));
#154843=CARTESIAN_POINT('Ctrl Pts',(0.519353520999944,15.2,-11.101665441));
#154844=CARTESIAN_POINT('Ctrl Pts',(0.520695416999944,15.2,-11.104643564));
#154845=CARTESIAN_POINT('Ctrl Pts',(0.522041764999944,15.2,-11.107625205));
#154846=CARTESIAN_POINT('Ctrl Pts',(0.523392567999944,15.2,-11.110610353));
#154847=CARTESIAN_POINT('Ctrl Pts',(0.524747828999944,15.2,-11.113598997));
#154848=CARTESIAN_POINT('Ctrl Pts',(0.526107550999945,15.2,-11.116591128));
#154849=CARTESIAN_POINT('Ctrl Pts',(0.527471734999944,15.2,-11.119586735));
#154850=CARTESIAN_POINT('Ctrl Pts',(0.528840383999943,15.2,-11.122585808));
#154851=CARTESIAN_POINT('Ctrl Pts',(0.530213500999944,15.2,-11.125588334));
#154852=CARTESIAN_POINT('Ctrl Pts',(0.531591089999944,15.2,-11.128594306));
#154853=CARTESIAN_POINT('Ctrl Pts',(0.532973150999945,15.2,-11.131603711));
#154854=CARTESIAN_POINT('Ctrl Pts',(0.534359687999945,15.2,-11.13461654));
#154855=CARTESIAN_POINT('Ctrl Pts',(0.535750703999944,15.2,-11.137632781));
#154856=CARTESIAN_POINT('Ctrl Pts',(0.537146200999944,15.2,-11.140652425));
#154857=CARTESIAN_POINT('Ctrl Pts',(0.538546180999945,15.2,-11.143675461));
#154858=CARTESIAN_POINT('Ctrl Pts',(0.539950646999944,15.2,-11.146701879));
#154859=CARTESIAN_POINT('Ctrl Pts',(0.541359600999944,15.2,-11.149731669));
#154860=CARTESIAN_POINT('Ctrl Pts',(0.542773046999944,15.2,-11.152764819));
#154861=CARTESIAN_POINT('Ctrl Pts',(0.544190985999945,15.2,-11.155801321));
#154862=CARTESIAN_POINT('Ctrl Pts',(0.545613420999944,15.2,-11.158841164));
#154863=CARTESIAN_POINT('Ctrl Pts',(0.547040353999945,15.2,-11.161884336));
#154864=CARTESIAN_POINT('Ctrl Pts',(0.548471787999943,15.2,-11.164930828));
#154865=CARTESIAN_POINT('Ctrl Pts',(0.549907724999944,15.2,-11.167980631));
#154866=CARTESIAN_POINT('Ctrl Pts',(0.551348166999944,15.2,-11.171033733));
#154867=CARTESIAN_POINT('Ctrl Pts',(0.552793118999944,15.2,-11.174090123));
#154868=CARTESIAN_POINT('Ctrl Pts',(0.554242579999944,15.2,-11.177149794));
#154869=CARTESIAN_POINT('Ctrl Pts',(0.555696552999944,15.2,-11.180212734));
#154870=CARTESIAN_POINT('Ctrl Pts',(0.557155042999944,15.2,-11.183278932));
#154871=CARTESIAN_POINT('Ctrl Pts',(0.558618047999944,15.2,-11.186348379));
#154872=CARTESIAN_POINT('Ctrl Pts',(0.560085574999943,15.2,-11.189421065));
#154873=CARTESIAN_POINT('Ctrl Pts',(0.561557623999944,15.2,-11.192496979));
#154874=CARTESIAN_POINT('Ctrl Pts',(0.563034195999944,15.2,-11.195576112));
#154875=CARTESIAN_POINT('Ctrl Pts',(0.564515294999944,15.2,-11.198658453));
#154876=CARTESIAN_POINT('Ctrl Pts',(0.566000922999944,15.2,-11.201743993));
#154877=CARTESIAN_POINT('Ctrl Pts',(0.567491082999945,15.2,-11.204832721));
#154878=CARTESIAN_POINT('Ctrl Pts',(0.568985775999944,15.2,-11.207924627));
#154879=CARTESIAN_POINT('Ctrl Pts',(0.570485004999944,15.2,-11.211019702));
#154880=CARTESIAN_POINT('Ctrl Pts',(0.571988771999944,15.2,-11.214117935));
#154881=CARTESIAN_POINT('Ctrl Pts',(0.573497078999944,15.2,-11.217219316));
#154882=CARTESIAN_POINT('Ctrl Pts',(0.575009928999944,15.2,-11.220323837));
#154883=CARTESIAN_POINT('Ctrl Pts',(0.576527321999943,15.2,-11.223431485));
#154884=CARTESIAN_POINT('Ctrl Pts',(0.578049262999943,15.2,-11.226542253));
#154885=CARTESIAN_POINT('Ctrl Pts',(0.579575752999945,15.2,-11.229656128));
#154886=CARTESIAN_POINT('Ctrl Pts',(0.581106792999945,15.2,-11.232773103));
#154887=CARTESIAN_POINT('Ctrl Pts',(0.582642387999944,15.2,-11.235893168));
#154888=CARTESIAN_POINT('Ctrl Pts',(0.584182536999944,15.2,-11.23901631));
#154889=CARTESIAN_POINT('Ctrl Pts',(0.585727243999944,15.2,-11.242142523));
#154890=CARTESIAN_POINT('Ctrl Pts',(0.587276510999944,15.2,-11.245271795));
#154891=CARTESIAN_POINT('Ctrl Pts',(0.588830339999945,15.2,-11.248404117));
#154892=CARTESIAN_POINT('Ctrl Pts',(0.590388730999944,15.2,-11.251539479));
#154893=CARTESIAN_POINT('Ctrl Pts',(0.591951689999944,15.2,-11.254677871));
#154894=CARTESIAN_POINT('Ctrl Pts',(0.593519214999944,15.2,-11.257819284));
#154895=CARTESIAN_POINT('Ctrl Pts',(0.595091311999945,15.2,-11.260963707));
#154896=CARTESIAN_POINT('Ctrl Pts',(0.596667979999944,15.2,-11.264111132));
#154897=CARTESIAN_POINT('Ctrl Pts',(0.598249221999944,15.2,-11.267261548));
#154898=CARTESIAN_POINT('Ctrl Pts',(0.599835039999944,15.2,-11.270414946));
#154899=CARTESIAN_POINT('Ctrl Pts',(0.601425436999944,15.2,-11.273571316));
#154900=CARTESIAN_POINT('Ctrl Pts',(0.603020412999945,15.2,-11.276730648));
#154901=CARTESIAN_POINT('Ctrl Pts',(0.604619971999945,15.2,-11.279892934));
#154902=CARTESIAN_POINT('Ctrl Pts',(0.606224114999944,15.2,-11.283058161));
#154903=CARTESIAN_POINT('Ctrl Pts',(0.607832842999944,15.2,-11.286226323));
#154904=CARTESIAN_POINT('Ctrl Pts',(0.609446159999945,15.2,-11.289397409));
#154905=CARTESIAN_POINT('Ctrl Pts',(0.611064066999945,15.2,-11.29257141));
#154906=CARTESIAN_POINT('Ctrl Pts',(0.612686564999944,15.2,-11.295748315));
#154907=CARTESIAN_POINT('Ctrl Pts',(0.614313656999944,15.2,-11.298928116));
#154908=CARTESIAN_POINT('Ctrl Pts',(0.615945344999944,15.2,-11.302110802));
#154909=CARTESIAN_POINT('Ctrl Pts',(0.617581629999945,15.2,-11.305296365));
#154910=CARTESIAN_POINT('Ctrl Pts',(0.619222514999944,15.2,-11.308484795));
#154911=CARTESIAN_POINT('Ctrl Pts',(0.620868000999945,15.2,-11.311676082));
#154912=CARTESIAN_POINT('Ctrl Pts',(0.622518089999944,15.2,-11.314870217));
#154913=CARTESIAN_POINT('Ctrl Pts',(0.624172783999944,15.2,-11.31806719));
#154914=CARTESIAN_POINT('Ctrl Pts',(0.625832085999944,15.2,-11.321266994));
#154915=CARTESIAN_POINT('Ctrl Pts',(0.627495994999945,15.2,-11.324469616));
#154916=CARTESIAN_POINT('Ctrl Pts',(0.629164515999945,15.2,-11.327675049));
#154917=CARTESIAN_POINT('Ctrl Pts',(0.630837647999944,15.2,-11.330883282));
#154918=CARTESIAN_POINT('Ctrl Pts',(0.632515393999945,15.2,-11.334094307));
#154919=CARTESIAN_POINT('Ctrl Pts',(0.634197756999945,15.2,-11.337308115));
#154920=CARTESIAN_POINT('Ctrl Pts',(0.635884736999944,15.2,-11.340524695));
#154921=CARTESIAN_POINT('Ctrl Pts',(0.637576336999944,15.2,-11.343744038));
#154922=CARTESIAN_POINT('Ctrl Pts',(0.639272556999945,15.2,-11.346966135));
#154923=CARTESIAN_POINT('Ctrl Pts',(0.640973400999945,15.2,-11.350190979));
#154924=CARTESIAN_POINT('Ctrl Pts',(0.642678868999944,15.2,-11.353418557));
#154925=CARTESIAN_POINT('Ctrl Pts',(0.644388963999944,15.2,-11.356648862));
#154926=CARTESIAN_POINT('Ctrl Pts',(0.646103685999945,15.2,-11.359881884));
#154927=CARTESIAN_POINT('Ctrl Pts',(0.647823038999944,15.2,-11.363117614));
#154928=CARTESIAN_POINT('Ctrl Pts',(0.649547021999944,15.2,-11.366356043));
#154929=CARTESIAN_POINT('Ctrl Pts',(0.651275639999944,15.2,-11.369597161));
#154930=CARTESIAN_POINT('Ctrl Pts',(0.653008890999944,15.2,-11.37284096));
#154931=CARTESIAN_POINT('Ctrl Pts',(0.654746778999944,15.2,-11.37608743));
#154932=CARTESIAN_POINT('Ctrl Pts',(0.656489305999944,15.2,-11.379336561));
#154933=CARTESIAN_POINT('Ctrl Pts',(0.658236471999943,15.2,-11.382588345));
#154934=CARTESIAN_POINT('Ctrl Pts',(0.659988278999944,15.2,-11.385842772));
#154935=CARTESIAN_POINT('Ctrl Pts',(0.661744729999943,15.2,-11.389099835));
#154936=CARTESIAN_POINT('Ctrl Pts',(0.663505824999944,15.2,-11.392359523));
#154937=CARTESIAN_POINT('Ctrl Pts',(0.665271565999944,15.2,-11.395621827));
#154938=CARTESIAN_POINT('Ctrl Pts',(0.667041954999944,15.2,-11.39888674));
#154939=CARTESIAN_POINT('Ctrl Pts',(0.668816992999944,15.2,-11.402154251));
#154940=CARTESIAN_POINT('Ctrl Pts',(0.670596681999944,15.2,-11.405424352));
#154941=CARTESIAN_POINT('Ctrl Pts',(0.672381022999944,15.2,-11.408697032));
#154942=CARTESIAN_POINT('Ctrl Pts',(0.674170018999944,15.2,-11.411972283));
#154943=CARTESIAN_POINT('Ctrl Pts',(0.675963669999944,15.2,-11.415250096));
#154944=CARTESIAN_POINT('Ctrl Pts',(0.677761977999943,15.2,-11.418530461));
#154945=CARTESIAN_POINT('Ctrl Pts',(0.679564944999944,15.2,-11.421813369));
#154946=CARTESIAN_POINT('Ctrl Pts',(0.681372572999944,15.2,-11.425098811));
#154947=CARTESIAN_POINT('Ctrl Pts',(0.683184861999945,15.2,-11.42838678));
#154948=CARTESIAN_POINT('Ctrl Pts',(0.685001812999944,15.2,-11.431677269));
#154949=CARTESIAN_POINT('Ctrl Pts',(0.686823428999944,15.2,-11.434970268));
#154950=CARTESIAN_POINT('Ctrl Pts',(0.688649710999945,15.2,-11.438265769));
#154951=CARTESIAN_POINT('Ctrl Pts',(0.690480658999945,15.2,-11.441563763));
#154952=CARTESIAN_POINT('Ctrl Pts',(0.692316276999944,15.2,-11.444864239));
#154953=CARTESIAN_POINT('Ctrl Pts',(0.694156563999945,15.2,-11.448167187));
#154954=CARTESIAN_POINT('Ctrl Pts',(0.696001524999944,15.2,-11.451472595));
#154955=CARTESIAN_POINT('Ctrl Pts',(0.697851158999944,15.2,-11.454780453));
#154956=CARTESIAN_POINT('Ctrl Pts',(0.699705468999944,15.2,-11.458090751));
#154957=CARTESIAN_POINT('Ctrl Pts',(0.701564455999945,15.2,-11.461403481));
#154958=CARTESIAN_POINT('Ctrl Pts',(0.703428120999944,15.2,-11.464718637));
#154959=CARTESIAN_POINT('Ctrl Pts',(0.705296462999944,15.2,-11.468036216));
#154960=CARTESIAN_POINT('Ctrl Pts',(0.707169485999944,15.2,-11.471356215));
#154961=CARTESIAN_POINT('Ctrl Pts',(0.708671644999944,15.2,-11.474014149));
#154962=CARTESIAN_POINT('Ctrl Pts',(0.709800370999945,15.2,-11.476008688));
#154963=CARTESIAN_POINT('Ctrl Pts',(0.710553790999944,15.2,-11.477338863));
#154964=CARTESIAN_POINT('Ctrl Pts',(0.710930733999944,15.2,-11.478004072));
#154965=CARTESIAN_POINT('Ctrl Pts',(0.292001928999944,12.2,-10.370890023));
#154966=CARTESIAN_POINT('Ctrl Pts',(0.292021795999944,12.2,-10.371063245));
#154967=CARTESIAN_POINT('Ctrl Pts',(0.292062308999944,12.2,-10.371415731));
#154968=CARTESIAN_POINT('Ctrl Pts',(0.292123960999945,12.2,-10.371949799));
#154969=CARTESIAN_POINT('Ctrl Pts',(0.292207546999944,12.2,-10.372669176));
#154970=CARTESIAN_POINT('Ctrl Pts',(0.292314179999943,12.2,-10.373578975));
#154971=CARTESIAN_POINT('Ctrl Pts',(0.292423468999944,12.2,-10.374503411));
#154972=CARTESIAN_POINT('Ctrl Pts',(0.292534811999945,12.2,-10.375437184));
#154973=CARTESIAN_POINT('Ctrl Pts',(0.292648222999944,12.2,-10.376380266));
#154974=CARTESIAN_POINT('Ctrl Pts',(0.292763716999945,12.2,-10.377332627));
#154975=CARTESIAN_POINT('Ctrl Pts',(0.292881308999944,12.2,-10.378294239));
#154976=CARTESIAN_POINT('Ctrl Pts',(0.293001014999945,12.2,-10.379265074));
#154977=CARTESIAN_POINT('Ctrl Pts',(0.293122845999945,12.2,-10.380245102));
#154978=CARTESIAN_POINT('Ctrl Pts',(0.293246819999944,12.2,-10.381234297));
#154979=CARTESIAN_POINT('Ctrl Pts',(0.293372948999944,12.2,-10.382232628));
#154980=CARTESIAN_POINT('Ctrl Pts',(0.293501248999943,12.2,-10.383240069));
#154981=CARTESIAN_POINT('Ctrl Pts',(0.293631731999945,12.2,-10.384256592));
#154982=CARTESIAN_POINT('Ctrl Pts',(0.293764412999945,12.2,-10.385282168));
#154983=CARTESIAN_POINT('Ctrl Pts',(0.293899306999944,12.2,-10.38631677));
#154984=CARTESIAN_POINT('Ctrl Pts',(0.294036426999943,12.2,-10.387360371));
#154985=CARTESIAN_POINT('Ctrl Pts',(0.294175786999944,12.2,-10.388412945));
#154986=CARTESIAN_POINT('Ctrl Pts',(0.294317400999944,12.2,-10.389474461));
#154987=CARTESIAN_POINT('Ctrl Pts',(0.294461281999944,12.2,-10.390544895));
#154988=CARTESIAN_POINT('Ctrl Pts',(0.294607443999944,12.2,-10.391624218));
#154989=CARTESIAN_POINT('Ctrl Pts',(0.294755900999943,12.2,-10.392712404));
#154990=CARTESIAN_POINT('Ctrl Pts',(0.294906665999944,12.2,-10.393809427));
#154991=CARTESIAN_POINT('Ctrl Pts',(0.295059751999943,12.2,-10.394915259));
#154992=CARTESIAN_POINT('Ctrl Pts',(0.295215172999944,12.2,-10.396029875));
#154993=CARTESIAN_POINT('Ctrl Pts',(0.295372941999944,12.2,-10.397153247));
#154994=CARTESIAN_POINT('Ctrl Pts',(0.295533071999945,12.2,-10.39828535));
#154995=CARTESIAN_POINT('Ctrl Pts',(0.295695575999944,12.2,-10.399426157));
#154996=CARTESIAN_POINT('Ctrl Pts',(0.295860466999944,12.2,-10.400575642));
#154997=CARTESIAN_POINT('Ctrl Pts',(0.296027758999945,12.2,-10.401733778));
#154998=CARTESIAN_POINT('Ctrl Pts',(0.296197462999944,12.2,-10.402900542));
#154999=CARTESIAN_POINT('Ctrl Pts',(0.296369592999944,12.2,-10.404075906));
#155000=CARTESIAN_POINT('Ctrl Pts',(0.296544161999943,12.2,-10.405259845));
#155001=CARTESIAN_POINT('Ctrl Pts',(0.296721181999944,12.2,-10.406452335));
#155002=CARTESIAN_POINT('Ctrl Pts',(0.296900663999944,12.2,-10.407653347));
#155003=CARTESIAN_POINT('Ctrl Pts',(0.297082623999945,12.2,-10.408862859));
#155004=CARTESIAN_POINT('Ctrl Pts',(0.297267072999944,12.2,-10.410080845));
#155005=CARTESIAN_POINT('Ctrl Pts',(0.297454020999943,12.2,-10.411307279));
#155006=CARTESIAN_POINT('Ctrl Pts',(0.297643483999943,12.2,-10.412542137));
#155007=CARTESIAN_POINT('Ctrl Pts',(0.297835472999944,12.2,-10.413785393));
#155008=CARTESIAN_POINT('Ctrl Pts',(0.298029997999943,12.2,-10.415037024));
#155009=CARTESIAN_POINT('Ctrl Pts',(0.298227073999945,12.2,-10.416297005));
#155010=CARTESIAN_POINT('Ctrl Pts',(0.298426710999945,12.2,-10.41756531));
#155011=CARTESIAN_POINT('Ctrl Pts',(0.298628921999944,12.2,-10.418841915));
#155012=CARTESIAN_POINT('Ctrl Pts',(0.298874678413339,12.2,-10.420383772284));
#155013=CARTESIAN_POINT('Ctrl Pts',(0.299124331804587,12.2,-10.4219380104286));
#155014=CARTESIAN_POINT('Ctrl Pts',(0.299377904195303,12.2,-10.4235045735714));
#155015=CARTESIAN_POINT('Ctrl Pts',(0.299635420609226,12.2,-10.4250834208572));
#155016=CARTESIAN_POINT('Ctrl Pts',(0.299896902999944,12.2,-10.426674502));
#155017=CARTESIAN_POINT('Ctrl Pts',(0.300117460999945,12.2,-10.428008535));
#155018=CARTESIAN_POINT('Ctrl Pts',(0.300340685999944,12.2,-10.429350676));
#155019=CARTESIAN_POINT('Ctrl Pts',(0.300566589999944,12.2,-10.430700902));
#155020=CARTESIAN_POINT('Ctrl Pts',(0.300795183999943,12.2,-10.43205919));
#155021=CARTESIAN_POINT('Ctrl Pts',(0.301026478999944,12.2,-10.433425516));
#155022=CARTESIAN_POINT('Ctrl Pts',(0.301260486999944,12.2,-10.434799858));
#155023=CARTESIAN_POINT('Ctrl Pts',(0.301497219999945,12.2,-10.43618219));
#155024=CARTESIAN_POINT('Ctrl Pts',(0.301736685999944,12.2,-10.437572491));
#155025=CARTESIAN_POINT('Ctrl Pts',(0.301978897999945,12.2,-10.438970738));
#155026=CARTESIAN_POINT('Ctrl Pts',(0.302223867999943,12.2,-10.440376907));
#155027=CARTESIAN_POINT('Ctrl Pts',(0.302471604999944,12.2,-10.441790977));
#155028=CARTESIAN_POINT('Ctrl Pts',(0.302722120999944,12.2,-10.443212923));
#155029=CARTESIAN_POINT('Ctrl Pts',(0.302975424999945,12.2,-10.444642725));
#155030=CARTESIAN_POINT('Ctrl Pts',(0.303231531999945,12.2,-10.446080357));
#155031=CARTESIAN_POINT('Ctrl Pts',(0.303490447999945,12.2,-10.447525799));
#155032=CARTESIAN_POINT('Ctrl Pts',(0.303752185999944,12.2,-10.448979029));
#155033=CARTESIAN_POINT('Ctrl Pts',(0.304016755999944,12.2,-10.450440023));
#155034=CARTESIAN_POINT('Ctrl Pts',(0.304284168999944,12.2,-10.451908761));
#155035=CARTESIAN_POINT('Ctrl Pts',(0.304554434999943,12.2,-10.453385218));
#155036=CARTESIAN_POINT('Ctrl Pts',(0.304827565999943,12.2,-10.454869375));
#155037=CARTESIAN_POINT('Ctrl Pts',(0.305103568999944,12.2,-10.456361208));
#155038=CARTESIAN_POINT('Ctrl Pts',(0.305382456999944,12.2,-10.457860694));
#155039=CARTESIAN_POINT('Ctrl Pts',(0.305664239999944,12.2,-10.459367814));
#155040=CARTESIAN_POINT('Ctrl Pts',(0.305948927999945,12.2,-10.460882546));
#155041=CARTESIAN_POINT('Ctrl Pts',(0.306236529999945,12.2,-10.462404866));
#155042=CARTESIAN_POINT('Ctrl Pts',(0.306527057999944,12.2,-10.463934755));
#155043=CARTESIAN_POINT('Ctrl Pts',(0.306820520999944,12.2,-10.46547219));
#155044=CARTESIAN_POINT('Ctrl Pts',(0.307116928999944,12.2,-10.46701715));
#155045=CARTESIAN_POINT('Ctrl Pts',(0.307416291999945,12.2,-10.468569615));
#155046=CARTESIAN_POINT('Ctrl Pts',(0.307718619999945,12.2,-10.470129561));
#155047=CARTESIAN_POINT('Ctrl Pts',(0.308023921999944,12.2,-10.47169697));
#155048=CARTESIAN_POINT('Ctrl Pts',(0.308332209999945,12.2,-10.473271818));
#155049=CARTESIAN_POINT('Ctrl Pts',(0.308643490999945,12.2,-10.474854086));
#155050=CARTESIAN_POINT('Ctrl Pts',(0.308957776999945,12.2,-10.476443753));
#155051=CARTESIAN_POINT('Ctrl Pts',(0.309275075999944,12.2,-10.478040796));
#155052=CARTESIAN_POINT('Ctrl Pts',(0.309595398999944,12.2,-10.479645198));
#155053=CARTESIAN_POINT('Ctrl Pts',(0.309918754999944,12.2,-10.481256934));
#155054=CARTESIAN_POINT('Ctrl Pts',(0.310245152999944,12.2,-10.482875987));
#155055=CARTESIAN_POINT('Ctrl Pts',(0.310574601999944,12.2,-10.484502335));
#155056=CARTESIAN_POINT('Ctrl Pts',(0.310907112999944,12.2,-10.486135957));
#155057=CARTESIAN_POINT('Ctrl Pts',(0.311242694999944,12.2,-10.487776833));
#155058=CARTESIAN_POINT('Ctrl Pts',(0.311581355999945,12.2,-10.489424943));
#155059=CARTESIAN_POINT('Ctrl Pts',(0.311923106999944,12.2,-10.491080266));
#155060=CARTESIAN_POINT('Ctrl Pts',(0.312267955999944,12.2,-10.492742782));
#155061=CARTESIAN_POINT('Ctrl Pts',(0.312615911999944,12.2,-10.494412473));
#155062=CARTESIAN_POINT('Ctrl Pts',(0.312966985999944,12.2,-10.496089316));
#155063=CARTESIAN_POINT('Ctrl Pts',(0.313321185999945,12.2,-10.497773293));
#155064=CARTESIAN_POINT('Ctrl Pts',(0.313678518999945,12.2,-10.499464382));
#155065=CARTESIAN_POINT('Ctrl Pts',(0.314038995999945,12.2,-10.501162565));
#155066=CARTESIAN_POINT('Ctrl Pts',(0.314402626999944,12.2,-10.502867822));
#155067=CARTESIAN_POINT('Ctrl Pts',(0.314769418999944,12.2,-10.504580133));
#155068=CARTESIAN_POINT('Ctrl Pts',(0.315139380999945,12.2,-10.506299478));
#155069=CARTESIAN_POINT('Ctrl Pts',(0.315512523999945,12.2,-10.508025838));
#155070=CARTESIAN_POINT('Ctrl Pts',(0.315888853999944,12.2,-10.509759194));
#155071=CARTESIAN_POINT('Ctrl Pts',(0.316268379999943,12.2,-10.511499525));
#155072=CARTESIAN_POINT('Ctrl Pts',(0.316651111999944,12.2,-10.513246812));
#155073=CARTESIAN_POINT('Ctrl Pts',(0.317037058999944,12.2,-10.515001037));
#155074=CARTESIAN_POINT('Ctrl Pts',(0.317426227999944,12.2,-10.516762179));
#155075=CARTESIAN_POINT('Ctrl Pts',(0.317818627999945,12.2,-10.518530222));
#155076=CARTESIAN_POINT('Ctrl Pts',(0.318214267999943,12.2,-10.520305143));
#155077=CARTESIAN_POINT('Ctrl Pts',(0.318613155999945,12.2,-10.522086924));
#155078=CARTESIAN_POINT('Ctrl Pts',(0.319015301999944,12.2,-10.523875548));
#155079=CARTESIAN_POINT('Ctrl Pts',(0.319420711999945,12.2,-10.525670994));
#155080=CARTESIAN_POINT('Ctrl Pts',(0.319829394999944,12.2,-10.527473244));
#155081=CARTESIAN_POINT('Ctrl Pts',(0.320241359999944,12.2,-10.529282279));
#155082=CARTESIAN_POINT('Ctrl Pts',(0.320656615999945,12.2,-10.53109808));
#155083=CARTESIAN_POINT('Ctrl Pts',(0.321075168999944,12.2,-10.532920629));
#155084=CARTESIAN_POINT('Ctrl Pts',(0.321497027999945,12.2,-10.534749907));
#155085=CARTESIAN_POINT('Ctrl Pts',(0.321922202999945,12.2,-10.536585896));
#155086=CARTESIAN_POINT('Ctrl Pts',(0.322350699999945,12.2,-10.538428576));
#155087=CARTESIAN_POINT('Ctrl Pts',(0.322782527999944,12.2,-10.54027793));
#155088=CARTESIAN_POINT('Ctrl Pts',(0.323217693999943,12.2,-10.54213394));
#155089=CARTESIAN_POINT('Ctrl Pts',(0.323656205999944,12.2,-10.543996587));
#155090=CARTESIAN_POINT('Ctrl Pts',(0.324098074999943,12.2,-10.545865852));
#155091=CARTESIAN_POINT('Ctrl Pts',(0.324543303999943,12.2,-10.547741717));
#155092=CARTESIAN_POINT('Ctrl Pts',(0.324991904999944,12.2,-10.549624165));
#155093=CARTESIAN_POINT('Ctrl Pts',(0.325443882999944,12.2,-10.551513176));
#155094=CARTESIAN_POINT('Ctrl Pts',(0.325899247999945,12.2,-10.553408734));
#155095=CARTESIAN_POINT('Ctrl Pts',(0.326358006999945,12.2,-10.555310821));
#155096=CARTESIAN_POINT('Ctrl Pts',(0.326820166999945,12.2,-10.557219417));
#155097=CARTESIAN_POINT('Ctrl Pts',(0.327285734999944,12.2,-10.559134506));
#155098=CARTESIAN_POINT('Ctrl Pts',(0.327754721999945,12.2,-10.56105607));
#155099=CARTESIAN_POINT('Ctrl Pts',(0.328227131999944,12.2,-10.562984091));
#155100=CARTESIAN_POINT('Ctrl Pts',(0.328702974999944,12.2,-10.56491855));
#155101=CARTESIAN_POINT('Ctrl Pts',(0.329182255999945,12.2,-10.566859432));
#155102=CARTESIAN_POINT('Ctrl Pts',(0.329664984999944,12.2,-10.568806718));
#155103=CARTESIAN_POINT('Ctrl Pts',(0.330151167999944,12.2,-10.57076039));
#155104=CARTESIAN_POINT('Ctrl Pts',(0.330640813999944,12.2,-10.572720431));
#155105=CARTESIAN_POINT('Ctrl Pts',(0.331133927999945,12.2,-10.574686823));
#155106=CARTESIAN_POINT('Ctrl Pts',(0.331630518999945,12.2,-10.57665955));
#155107=CARTESIAN_POINT('Ctrl Pts',(0.332130593999944,12.2,-10.578638595));
#155108=CARTESIAN_POINT('Ctrl Pts',(0.332634160999945,12.2,-10.580623937));
#155109=CARTESIAN_POINT('Ctrl Pts',(0.333141224999943,12.2,-10.582615564));
#155110=CARTESIAN_POINT('Ctrl Pts',(0.333651795999945,12.2,-10.584613455));
#155111=CARTESIAN_POINT('Ctrl Pts',(0.334165878999944,12.2,-10.586617594));
#155112=CARTESIAN_POINT('Ctrl Pts',(0.334683482999945,12.2,-10.588627965));
#155113=CARTESIAN_POINT('Ctrl Pts',(0.335204611999943,12.2,-10.59064455));
#155114=CARTESIAN_POINT('Ctrl Pts',(0.335729277999944,12.2,-10.592667332));
#155115=CARTESIAN_POINT('Ctrl Pts',(0.336257482999944,12.2,-10.594696293));
#155116=CARTESIAN_POINT('Ctrl Pts',(0.336789236999945,12.2,-10.59673142));
#155117=CARTESIAN_POINT('Ctrl Pts',(0.337324545999945,12.2,-10.598772692));
#155118=CARTESIAN_POINT('Ctrl Pts',(0.337863417999945,12.2,-10.600820093));
#155119=CARTESIAN_POINT('Ctrl Pts',(0.338405857999945,12.2,-10.602873609));
#155120=CARTESIAN_POINT('Ctrl Pts',(0.338951873999944,12.2,-10.60493322));
#155121=CARTESIAN_POINT('Ctrl Pts',(0.339501472999943,12.2,-10.606998913));
#155122=CARTESIAN_POINT('Ctrl Pts',(0.340054661999943,12.2,-10.609070667));
#155123=CARTESIAN_POINT('Ctrl Pts',(0.340611446999944,12.2,-10.611148469));
#155124=CARTESIAN_POINT('Ctrl Pts',(0.341171834999944,12.2,-10.613232302));
#155125=CARTESIAN_POINT('Ctrl Pts',(0.341735832999944,12.2,-10.615322148));
#155126=CARTESIAN_POINT('Ctrl Pts',(0.342303446999944,12.2,-10.617417992));
#155127=CARTESIAN_POINT('Ctrl Pts',(0.342874684999943,12.2,-10.619519817));
#155128=CARTESIAN_POINT('Ctrl Pts',(0.343449551999945,12.2,-10.621627608));
#155129=CARTESIAN_POINT('Ctrl Pts',(0.344028054999944,12.2,-10.623741347));
#155130=CARTESIAN_POINT('Ctrl Pts',(0.344610201999943,12.2,-10.625861018));
#155131=CARTESIAN_POINT('Ctrl Pts',(0.345195997999944,12.2,-10.627986606));
#155132=CARTESIAN_POINT('Ctrl Pts',(0.345785448999945,12.2,-10.630118095));
#155133=CARTESIAN_POINT('Ctrl Pts',(0.346378563999944,12.2,-10.632255468));
#155134=CARTESIAN_POINT('Ctrl Pts',(0.346975346999944,12.2,-10.634398708));
#155135=CARTESIAN_POINT('Ctrl Pts',(0.347575804999943,12.2,-10.636547803));
#155136=CARTESIAN_POINT('Ctrl Pts',(0.348179944999943,12.2,-10.638702732));
#155137=CARTESIAN_POINT('Ctrl Pts',(0.348787772999944,12.2,-10.640863483));
#155138=CARTESIAN_POINT('Ctrl Pts',(0.349399294999945,12.2,-10.643030038));
#155139=CARTESIAN_POINT('Ctrl Pts',(0.350014516999944,12.2,-10.645202383));
#155140=CARTESIAN_POINT('Ctrl Pts',(0.350633445999945,12.2,-10.647380501));
#155141=CARTESIAN_POINT('Ctrl Pts',(0.351256087999945,12.2,-10.649564376));
#155142=CARTESIAN_POINT('Ctrl Pts',(0.351882449999945,12.2,-10.651753993));
#155143=CARTESIAN_POINT('Ctrl Pts',(0.352512535999944,12.2,-10.653949337));
#155144=CARTESIAN_POINT('Ctrl Pts',(0.353146353999945,12.2,-10.656150391));
#155145=CARTESIAN_POINT('Ctrl Pts',(0.353783908999944,12.2,-10.658357141));
#155146=CARTESIAN_POINT('Ctrl Pts',(0.354425208999943,12.2,-10.660569571));
#155147=CARTESIAN_POINT('Ctrl Pts',(0.355070257999944,12.2,-10.662787664));
#155148=CARTESIAN_POINT('Ctrl Pts',(0.355719062999944,12.2,-10.665011407));
#155149=CARTESIAN_POINT('Ctrl Pts',(0.356371629999943,12.2,-10.667240784));
#155150=CARTESIAN_POINT('Ctrl Pts',(0.357027963999944,12.2,-10.669475778));
#155151=CARTESIAN_POINT('Ctrl Pts',(0.357688070999943,12.2,-10.671716375));
#155152=CARTESIAN_POINT('Ctrl Pts',(0.358351957999944,12.2,-10.673962561));
#155153=CARTESIAN_POINT('Ctrl Pts',(0.359019631999944,12.2,-10.676214319));
#155154=CARTESIAN_POINT('Ctrl Pts',(0.359691094999944,12.2,-10.678471635));
#155155=CARTESIAN_POINT('Ctrl Pts',(0.360366356999944,12.2,-10.680734493));
#155156=CARTESIAN_POINT('Ctrl Pts',(0.361045420999944,12.2,-10.683002879));
#155157=CARTESIAN_POINT('Ctrl Pts',(0.361728292999944,12.2,-10.685276775));
#155158=CARTESIAN_POINT('Ctrl Pts',(0.362414979999944,12.2,-10.687556171));
#155159=CARTESIAN_POINT('Ctrl Pts',(0.363105486999944,12.2,-10.689841047));
#155160=CARTESIAN_POINT('Ctrl Pts',(0.363799819999944,12.2,-10.692131392));
#155161=CARTESIAN_POINT('Ctrl Pts',(0.364497983999945,12.2,-10.69442719));
#155162=CARTESIAN_POINT('Ctrl Pts',(0.365199985999943,12.2,-10.696728424));
#155163=CARTESIAN_POINT('Ctrl Pts',(0.365905829999944,12.2,-10.699035082));
#155164=CARTESIAN_POINT('Ctrl Pts',(0.366615521999943,12.2,-10.701347148));
#155165=CARTESIAN_POINT('Ctrl Pts',(0.367329068999943,12.2,-10.703664607));
#155166=CARTESIAN_POINT('Ctrl Pts',(0.368046474999945,12.2,-10.705987445));
#155167=CARTESIAN_POINT('Ctrl Pts',(0.368767745999945,12.2,-10.708315648));
#155168=CARTESIAN_POINT('Ctrl Pts',(0.369492886999945,12.2,-10.710649199));
#155169=CARTESIAN_POINT('Ctrl Pts',(0.370221902999944,12.2,-10.712988086));
#155170=CARTESIAN_POINT('Ctrl Pts',(0.370954801999943,12.2,-10.715332293));
#155171=CARTESIAN_POINT('Ctrl Pts',(0.371691585999944,12.2,-10.717681807));
#155172=CARTESIAN_POINT('Ctrl Pts',(0.372432262999943,12.2,-10.720036612));
#155173=CARTESIAN_POINT('Ctrl Pts',(0.373176837999944,12.2,-10.722396693));
#155174=CARTESIAN_POINT('Ctrl Pts',(0.373925314999944,12.2,-10.724762038));
#155175=CARTESIAN_POINT('Ctrl Pts',(0.374677699999945,12.2,-10.72713263));
#155176=CARTESIAN_POINT('Ctrl Pts',(0.375433997999943,12.2,-10.729508457));
#155177=CARTESIAN_POINT('Ctrl Pts',(0.376194214999943,12.2,-10.731889504));
#155178=CARTESIAN_POINT('Ctrl Pts',(0.376958354999944,12.2,-10.734275757));
#155179=CARTESIAN_POINT('Ctrl Pts',(0.377726424999943,12.2,-10.7366672));
#155180=CARTESIAN_POINT('Ctrl Pts',(0.378498428999944,12.2,-10.73906382));
#155181=CARTESIAN_POINT('Ctrl Pts',(0.379274372999945,12.2,-10.741465604));
#155182=CARTESIAN_POINT('Ctrl Pts',(0.380054259999945,12.2,-10.743872536));
#155183=CARTESIAN_POINT('Ctrl Pts',(0.380838096999945,12.2,-10.746284604));
#155184=CARTESIAN_POINT('Ctrl Pts',(0.381625889999944,12.2,-10.748701792));
#155185=CARTESIAN_POINT('Ctrl Pts',(0.382417640999944,12.2,-10.751124087));
#155186=CARTESIAN_POINT('Ctrl Pts',(0.383213356999944,12.2,-10.753551475));
#155187=CARTESIAN_POINT('Ctrl Pts',(0.384013043999945,12.2,-10.755983942));
#155188=CARTESIAN_POINT('Ctrl Pts',(0.384816703999944,12.2,-10.758421474));
#155189=CARTESIAN_POINT('Ctrl Pts',(0.385624345999943,12.2,-10.760864057));
#155190=CARTESIAN_POINT('Ctrl Pts',(0.386435970999944,12.2,-10.763311678));
#155191=CARTESIAN_POINT('Ctrl Pts',(0.387251585999945,12.2,-10.765764322));
#155192=CARTESIAN_POINT('Ctrl Pts',(0.388071194999944,12.2,-10.768221976));
#155193=CARTESIAN_POINT('Ctrl Pts',(0.388894804999945,12.2,-10.770684626));
#155194=CARTESIAN_POINT('Ctrl Pts',(0.389722417999945,12.2,-10.773152259));
#155195=CARTESIAN_POINT('Ctrl Pts',(0.390554040999945,12.2,-10.77562486));
#155196=CARTESIAN_POINT('Ctrl Pts',(0.391389675999945,12.2,-10.778102417));
#155197=CARTESIAN_POINT('Ctrl Pts',(0.392229331999945,12.2,-10.780584915));
#155198=CARTESIAN_POINT('Ctrl Pts',(0.393073008999943,12.2,-10.78307234));
#155199=CARTESIAN_POINT('Ctrl Pts',(0.393920715999944,12.2,-10.785564681));
#155200=CARTESIAN_POINT('Ctrl Pts',(0.394772454999943,12.2,-10.788061922));
#155201=CARTESIAN_POINT('Ctrl Pts',(0.395628231999944,12.2,-10.790564051));
#155202=CARTESIAN_POINT('Ctrl Pts',(0.396488050999944,12.2,-10.793071054));
#155203=CARTESIAN_POINT('Ctrl Pts',(0.397351916999943,12.2,-10.795582918));
#155204=CARTESIAN_POINT('Ctrl Pts',(0.398219834999944,12.2,-10.798099629));
#155205=CARTESIAN_POINT('Ctrl Pts',(0.399091808999945,12.2,-10.800621174));
#155206=CARTESIAN_POINT('Ctrl Pts',(0.399967842999944,12.2,-10.80314754));
#155207=CARTESIAN_POINT('Ctrl Pts',(0.400847942999943,12.2,-10.805678712));
#155208=CARTESIAN_POINT('Ctrl Pts',(0.401732111999945,12.2,-10.808214679));
#155209=CARTESIAN_POINT('Ctrl Pts',(0.402620355999943,12.2,-10.810755427));
#155210=CARTESIAN_POINT('Ctrl Pts',(0.403512678999943,12.2,-10.813300943));
#155211=CARTESIAN_POINT('Ctrl Pts',(0.404409085999945,12.2,-10.815851213));
#155212=CARTESIAN_POINT('Ctrl Pts',(0.405309579999944,12.2,-10.818406225));
#155213=CARTESIAN_POINT('Ctrl Pts',(0.406214165999945,12.2,-10.820965964));
#155214=CARTESIAN_POINT('Ctrl Pts',(0.407122848999943,12.2,-10.82353042));
#155215=CARTESIAN_POINT('Ctrl Pts',(0.408035631999945,12.2,-10.826099577));
#155216=CARTESIAN_POINT('Ctrl Pts',(0.408952521999945,12.2,-10.828673424));
#155217=CARTESIAN_POINT('Ctrl Pts',(0.409873521999945,12.2,-10.831251946));
#155218=CARTESIAN_POINT('Ctrl Pts',(0.410798634999944,12.2,-10.833835132));
#155219=CARTESIAN_POINT('Ctrl Pts',(0.411727865999945,12.2,-10.836422969));
#155220=CARTESIAN_POINT('Ctrl Pts',(0.412661221999944,12.2,-10.839015443));
#155221=CARTESIAN_POINT('Ctrl Pts',(0.413598702999943,12.2,-10.841612542));
#155222=CARTESIAN_POINT('Ctrl Pts',(0.414540315999944,12.2,-10.844214253));
#155223=CARTESIAN_POINT('Ctrl Pts',(0.415486064999945,12.2,-10.846820562));
#155224=CARTESIAN_POINT('Ctrl Pts',(0.416435952999944,12.2,-10.849431457));
#155225=CARTESIAN_POINT('Ctrl Pts',(0.417389984999945,12.2,-10.852046927));
#155226=CARTESIAN_POINT('Ctrl Pts',(0.418348164999944,12.2,-10.854666958));
#155227=CARTESIAN_POINT('Ctrl Pts',(0.419310496999945,12.2,-10.857291535));
#155228=CARTESIAN_POINT('Ctrl Pts',(0.420276985999944,12.2,-10.859920649));
#155229=CARTESIAN_POINT('Ctrl Pts',(0.421247635999944,12.2,-10.862554285));
#155230=CARTESIAN_POINT('Ctrl Pts',(0.422222449999945,12.2,-10.865192432));
#155231=CARTESIAN_POINT('Ctrl Pts',(0.423201432999945,12.2,-10.867835076));
#155232=CARTESIAN_POINT('Ctrl Pts',(0.424184586999944,12.2,-10.870482205));
#155233=CARTESIAN_POINT('Ctrl Pts',(0.425171919999944,12.2,-10.873133806));
#155234=CARTESIAN_POINT('Ctrl Pts',(0.426163432999944,12.2,-10.875789868));
#155235=CARTESIAN_POINT('Ctrl Pts',(0.427159130999945,12.2,-10.878450378));
#155236=CARTESIAN_POINT('Ctrl Pts',(0.428159016999944,12.2,-10.881115322));
#155237=CARTESIAN_POINT('Ctrl Pts',(0.429163096999944,12.2,-10.883784689));
#155238=CARTESIAN_POINT('Ctrl Pts',(0.430171372999943,12.2,-10.886458467));
#155239=CARTESIAN_POINT('Ctrl Pts',(0.431183849999943,12.2,-10.889136642));
#155240=CARTESIAN_POINT('Ctrl Pts',(0.432200529999944,12.2,-10.891819203));
#155241=CARTESIAN_POINT('Ctrl Pts',(0.433221419999944,12.2,-10.894506138));
#155242=CARTESIAN_POINT('Ctrl Pts',(0.434246522999944,12.2,-10.897197434));
#155243=CARTESIAN_POINT('Ctrl Pts',(0.435275840999945,12.2,-10.899893077));
#155244=CARTESIAN_POINT('Ctrl Pts',(0.436309378999944,12.2,-10.902593058));
#155245=CARTESIAN_POINT('Ctrl Pts',(0.437347139999943,12.2,-10.905297364));
#155246=CARTESIAN_POINT('Ctrl Pts',(0.438389128999944,12.2,-10.908005981));
#155247=CARTESIAN_POINT('Ctrl Pts',(0.439435350999944,12.2,-10.910718898));
#155248=CARTESIAN_POINT('Ctrl Pts',(0.440485805999945,12.2,-10.913436104));
#155249=CARTESIAN_POINT('Ctrl Pts',(0.441540500999944,12.2,-10.916157585));
#155250=CARTESIAN_POINT('Ctrl Pts',(0.442599438999943,12.2,-10.91888333));
#155251=CARTESIAN_POINT('Ctrl Pts',(0.443662621999945,12.2,-10.921613326));
#155252=CARTESIAN_POINT('Ctrl Pts',(0.444730055999945,12.2,-10.924347562));
#155253=CARTESIAN_POINT('Ctrl Pts',(0.445801742999944,12.2,-10.927086026));
#155254=CARTESIAN_POINT('Ctrl Pts',(0.446877687999944,12.2,-10.929828706));
#155255=CARTESIAN_POINT('Ctrl Pts',(0.447957893999943,12.2,-10.932575589));
#155256=CARTESIAN_POINT('Ctrl Pts',(0.449042363999944,12.2,-10.935326664));
#155257=CARTESIAN_POINT('Ctrl Pts',(0.450131101999943,12.2,-10.93808192));
#155258=CARTESIAN_POINT('Ctrl Pts',(0.451224112999944,12.2,-10.940841343));
#155259=CARTESIAN_POINT('Ctrl Pts',(0.452321397999944,12.2,-10.943604921));
#155260=CARTESIAN_POINT('Ctrl Pts',(0.453422961999944,12.2,-10.946372645));
#155261=CARTESIAN_POINT('Ctrl Pts',(0.454528808999944,12.2,-10.949144502));
#155262=CARTESIAN_POINT('Ctrl Pts',(0.455638941999944,12.2,-10.951920478));
#155263=CARTESIAN_POINT('Ctrl Pts',(0.456753363999944,12.2,-10.954700564));
#155264=CARTESIAN_POINT('Ctrl Pts',(0.457872078999945,12.2,-10.957484747));
#155265=CARTESIAN_POINT('Ctrl Pts',(0.458995090999944,12.2,-10.960273016));
#155266=CARTESIAN_POINT('Ctrl Pts',(0.460122400999945,12.2,-10.963065359));
#155267=CARTESIAN_POINT('Ctrl Pts',(0.461254015999945,12.2,-10.965861764));
#155268=CARTESIAN_POINT('Ctrl Pts',(0.462389937999944,12.2,-10.96866222));
#155269=CARTESIAN_POINT('Ctrl Pts',(0.463530168999944,12.2,-10.971466714));
#155270=CARTESIAN_POINT('Ctrl Pts',(0.464674712999944,12.2,-10.974275237));
#155271=CARTESIAN_POINT('Ctrl Pts',(0.465823575999943,12.2,-10.977087774));
#155272=CARTESIAN_POINT('Ctrl Pts',(0.466976756999945,12.2,-10.979904316));
#155273=CARTESIAN_POINT('Ctrl Pts',(0.468134261999945,12.2,-10.982724852));
#155274=CARTESIAN_POINT('Ctrl Pts',(0.469296094999944,12.2,-10.985549368));
#155275=CARTESIAN_POINT('Ctrl Pts',(0.470462256999945,12.2,-10.988377854));
#155276=CARTESIAN_POINT('Ctrl Pts',(0.471632752999945,12.2,-10.991210298));
#155277=CARTESIAN_POINT('Ctrl Pts',(0.472807584999944,12.2,-10.994046689));
#155278=CARTESIAN_POINT('Ctrl Pts',(0.473986757999943,12.2,-10.996887016));
#155279=CARTESIAN_POINT('Ctrl Pts',(0.475170271999945,12.2,-10.999731268));
#155280=CARTESIAN_POINT('Ctrl Pts',(0.476358134999944,12.2,-11.002579431));
#155281=CARTESIAN_POINT('Ctrl Pts',(0.477550345999944,12.2,-11.005431497));
#155282=CARTESIAN_POINT('Ctrl Pts',(0.478746909999943,12.2,-11.008287453));
#155283=CARTESIAN_POINT('Ctrl Pts',(0.479947829999944,12.2,-11.011147287));
#155284=CARTESIAN_POINT('Ctrl Pts',(0.481153109999944,12.2,-11.014010988));
#155285=CARTESIAN_POINT('Ctrl Pts',(0.482362750999944,12.2,-11.016878547));
#155286=CARTESIAN_POINT('Ctrl Pts',(0.483576757999945,12.2,-11.01974995));
#155287=CARTESIAN_POINT('Ctrl Pts',(0.484795132999943,12.2,-11.022625188));
#155288=CARTESIAN_POINT('Ctrl Pts',(0.486017879999944,12.2,-11.025504247));
#155289=CARTESIAN_POINT('Ctrl Pts',(0.487245001999945,12.2,-11.028387119));
#155290=CARTESIAN_POINT('Ctrl Pts',(0.488476501999945,12.2,-11.031273791));
#155291=CARTESIAN_POINT('Ctrl Pts',(0.489712381999944,12.2,-11.034164252));
#155292=CARTESIAN_POINT('Ctrl Pts',(0.490952645999944,12.2,-11.037058491));
#155293=CARTESIAN_POINT('Ctrl Pts',(0.492197297999944,12.2,-11.039956497));
#155294=CARTESIAN_POINT('Ctrl Pts',(0.493446337999943,12.2,-11.04285826));
#155295=CARTESIAN_POINT('Ctrl Pts',(0.494699771999944,12.2,-11.045763768));
#155296=CARTESIAN_POINT('Ctrl Pts',(0.495957600999944,12.2,-11.04867301));
#155297=CARTESIAN_POINT('Ctrl Pts',(0.497219829999944,12.2,-11.051585974));
#155298=CARTESIAN_POINT('Ctrl Pts',(0.498486459999944,12.2,-11.05450265));
#155299=CARTESIAN_POINT('Ctrl Pts',(0.499757494999944,12.2,-11.057423028));
#155300=CARTESIAN_POINT('Ctrl Pts',(0.501032935999944,12.2,-11.060347096));
#155301=CARTESIAN_POINT('Ctrl Pts',(0.502312788999945,12.2,-11.063274844));
#155302=CARTESIAN_POINT('Ctrl Pts',(0.503597054999945,12.2,-11.066206259));
#155303=CARTESIAN_POINT('Ctrl Pts',(0.504885736999944,12.2,-11.069141332));
#155304=CARTESIAN_POINT('Ctrl Pts',(0.506178838999943,12.2,-11.072080052));
#155305=CARTESIAN_POINT('Ctrl Pts',(0.507476362999945,12.2,-11.075022407));
#155306=CARTESIAN_POINT('Ctrl Pts',(0.508778309999944,12.2,-11.077968387));
#155307=CARTESIAN_POINT('Ctrl Pts',(0.510084685999944,12.2,-11.080917982));
#155308=CARTESIAN_POINT('Ctrl Pts',(0.511395492999944,12.2,-11.08387118));
#155309=CARTESIAN_POINT('Ctrl Pts',(0.512710730999945,12.2,-11.086827972));
#155310=CARTESIAN_POINT('Ctrl Pts',(0.514030406999945,12.2,-11.089788344));
#155311=CARTESIAN_POINT('Ctrl Pts',(0.515354519999944,12.2,-11.092752289));
#155312=CARTESIAN_POINT('Ctrl Pts',(0.516683075999944,12.2,-11.095719793));
#155313=CARTESIAN_POINT('Ctrl Pts',(0.518016074999944,12.2,-11.098690848));
#155314=CARTESIAN_POINT('Ctrl Pts',(0.519353520999944,12.2,-11.101665441));
#155315=CARTESIAN_POINT('Ctrl Pts',(0.520695416999944,12.2,-11.104643564));
#155316=CARTESIAN_POINT('Ctrl Pts',(0.522041764999944,12.2,-11.107625205));
#155317=CARTESIAN_POINT('Ctrl Pts',(0.523392567999944,12.2,-11.110610353));
#155318=CARTESIAN_POINT('Ctrl Pts',(0.524747828999944,12.2,-11.113598997));
#155319=CARTESIAN_POINT('Ctrl Pts',(0.526107550999945,12.2,-11.116591128));
#155320=CARTESIAN_POINT('Ctrl Pts',(0.527471734999944,12.2,-11.119586735));
#155321=CARTESIAN_POINT('Ctrl Pts',(0.528840383999943,12.2,-11.122585808));
#155322=CARTESIAN_POINT('Ctrl Pts',(0.530213500999944,12.2,-11.125588334));
#155323=CARTESIAN_POINT('Ctrl Pts',(0.531591089999944,12.2,-11.128594306));
#155324=CARTESIAN_POINT('Ctrl Pts',(0.532973150999945,12.2,-11.131603711));
#155325=CARTESIAN_POINT('Ctrl Pts',(0.534359687999945,12.2,-11.13461654));
#155326=CARTESIAN_POINT('Ctrl Pts',(0.535750703999944,12.2,-11.137632781));
#155327=CARTESIAN_POINT('Ctrl Pts',(0.537146200999944,12.2,-11.140652425));
#155328=CARTESIAN_POINT('Ctrl Pts',(0.538546180999945,12.2,-11.143675461));
#155329=CARTESIAN_POINT('Ctrl Pts',(0.539950646999944,12.2,-11.146701879));
#155330=CARTESIAN_POINT('Ctrl Pts',(0.541359600999944,12.2,-11.149731669));
#155331=CARTESIAN_POINT('Ctrl Pts',(0.542773046999944,12.2,-11.152764819));
#155332=CARTESIAN_POINT('Ctrl Pts',(0.544190985999945,12.2,-11.155801321));
#155333=CARTESIAN_POINT('Ctrl Pts',(0.545613420999944,12.2,-11.158841164));
#155334=CARTESIAN_POINT('Ctrl Pts',(0.547040353999945,12.2,-11.161884336));
#155335=CARTESIAN_POINT('Ctrl Pts',(0.548471787999943,12.2,-11.164930828));
#155336=CARTESIAN_POINT('Ctrl Pts',(0.549907724999944,12.2,-11.167980631));
#155337=CARTESIAN_POINT('Ctrl Pts',(0.551348166999944,12.2,-11.171033733));
#155338=CARTESIAN_POINT('Ctrl Pts',(0.552793118999944,12.2,-11.174090123));
#155339=CARTESIAN_POINT('Ctrl Pts',(0.554242579999944,12.2,-11.177149794));
#155340=CARTESIAN_POINT('Ctrl Pts',(0.555696552999944,12.2,-11.180212734));
#155341=CARTESIAN_POINT('Ctrl Pts',(0.557155042999944,12.2,-11.183278932));
#155342=CARTESIAN_POINT('Ctrl Pts',(0.558618047999944,12.2,-11.186348379));
#155343=CARTESIAN_POINT('Ctrl Pts',(0.560085574999943,12.2,-11.189421065));
#155344=CARTESIAN_POINT('Ctrl Pts',(0.561557623999944,12.2,-11.192496979));
#155345=CARTESIAN_POINT('Ctrl Pts',(0.563034195999944,12.2,-11.195576112));
#155346=CARTESIAN_POINT('Ctrl Pts',(0.564515294999944,12.2,-11.198658453));
#155347=CARTESIAN_POINT('Ctrl Pts',(0.566000922999944,12.2,-11.201743993));
#155348=CARTESIAN_POINT('Ctrl Pts',(0.567491082999945,12.2,-11.204832721));
#155349=CARTESIAN_POINT('Ctrl Pts',(0.568985775999944,12.2,-11.207924627));
#155350=CARTESIAN_POINT('Ctrl Pts',(0.570485004999944,12.2,-11.211019702));
#155351=CARTESIAN_POINT('Ctrl Pts',(0.571988771999944,12.2,-11.214117935));
#155352=CARTESIAN_POINT('Ctrl Pts',(0.573497078999944,12.2,-11.217219316));
#155353=CARTESIAN_POINT('Ctrl Pts',(0.575009928999944,12.2,-11.220323837));
#155354=CARTESIAN_POINT('Ctrl Pts',(0.576527321999943,12.2,-11.223431485));
#155355=CARTESIAN_POINT('Ctrl Pts',(0.578049262999943,12.2,-11.226542253));
#155356=CARTESIAN_POINT('Ctrl Pts',(0.579575752999945,12.2,-11.229656128));
#155357=CARTESIAN_POINT('Ctrl Pts',(0.581106792999945,12.2,-11.232773103));
#155358=CARTESIAN_POINT('Ctrl Pts',(0.582642387999944,12.2,-11.235893168));
#155359=CARTESIAN_POINT('Ctrl Pts',(0.584182536999944,12.2,-11.23901631));
#155360=CARTESIAN_POINT('Ctrl Pts',(0.585727243999944,12.2,-11.242142523));
#155361=CARTESIAN_POINT('Ctrl Pts',(0.587276510999944,12.2,-11.245271795));
#155362=CARTESIAN_POINT('Ctrl Pts',(0.588830339999945,12.2,-11.248404117));
#155363=CARTESIAN_POINT('Ctrl Pts',(0.590388730999944,12.2,-11.251539479));
#155364=CARTESIAN_POINT('Ctrl Pts',(0.591951689999944,12.2,-11.254677871));
#155365=CARTESIAN_POINT('Ctrl Pts',(0.593519214999944,12.2,-11.257819284));
#155366=CARTESIAN_POINT('Ctrl Pts',(0.595091311999945,12.2,-11.260963707));
#155367=CARTESIAN_POINT('Ctrl Pts',(0.596667979999944,12.2,-11.264111132));
#155368=CARTESIAN_POINT('Ctrl Pts',(0.598249221999944,12.2,-11.267261548));
#155369=CARTESIAN_POINT('Ctrl Pts',(0.599835039999944,12.2,-11.270414946));
#155370=CARTESIAN_POINT('Ctrl Pts',(0.601425436999944,12.2,-11.273571316));
#155371=CARTESIAN_POINT('Ctrl Pts',(0.603020412999945,12.2,-11.276730648));
#155372=CARTESIAN_POINT('Ctrl Pts',(0.604619971999945,12.2,-11.279892934));
#155373=CARTESIAN_POINT('Ctrl Pts',(0.606224114999944,12.2,-11.283058161));
#155374=CARTESIAN_POINT('Ctrl Pts',(0.607832842999944,12.2,-11.286226323));
#155375=CARTESIAN_POINT('Ctrl Pts',(0.609446159999945,12.2,-11.289397409));
#155376=CARTESIAN_POINT('Ctrl Pts',(0.611064066999945,12.2,-11.29257141));
#155377=CARTESIAN_POINT('Ctrl Pts',(0.612686564999944,12.2,-11.295748315));
#155378=CARTESIAN_POINT('Ctrl Pts',(0.614313656999944,12.2,-11.298928116));
#155379=CARTESIAN_POINT('Ctrl Pts',(0.615945344999944,12.2,-11.302110802));
#155380=CARTESIAN_POINT('Ctrl Pts',(0.617581629999945,12.2,-11.305296365));
#155381=CARTESIAN_POINT('Ctrl Pts',(0.619222514999944,12.2,-11.308484795));
#155382=CARTESIAN_POINT('Ctrl Pts',(0.620868000999945,12.2,-11.311676082));
#155383=CARTESIAN_POINT('Ctrl Pts',(0.622518089999944,12.2,-11.314870217));
#155384=CARTESIAN_POINT('Ctrl Pts',(0.624172783999944,12.2,-11.31806719));
#155385=CARTESIAN_POINT('Ctrl Pts',(0.625832085999944,12.2,-11.321266994));
#155386=CARTESIAN_POINT('Ctrl Pts',(0.627495994999945,12.2,-11.324469616));
#155387=CARTESIAN_POINT('Ctrl Pts',(0.629164515999945,12.2,-11.327675049));
#155388=CARTESIAN_POINT('Ctrl Pts',(0.630837647999944,12.2,-11.330883282));
#155389=CARTESIAN_POINT('Ctrl Pts',(0.632515393999945,12.2,-11.334094307));
#155390=CARTESIAN_POINT('Ctrl Pts',(0.634197756999945,12.2,-11.337308115));
#155391=CARTESIAN_POINT('Ctrl Pts',(0.635884736999944,12.2,-11.340524695));
#155392=CARTESIAN_POINT('Ctrl Pts',(0.637576336999944,12.2,-11.343744038));
#155393=CARTESIAN_POINT('Ctrl Pts',(0.639272556999945,12.2,-11.346966135));
#155394=CARTESIAN_POINT('Ctrl Pts',(0.640973400999945,12.2,-11.350190979));
#155395=CARTESIAN_POINT('Ctrl Pts',(0.642678868999944,12.2,-11.353418557));
#155396=CARTESIAN_POINT('Ctrl Pts',(0.644388963999944,12.2,-11.356648862));
#155397=CARTESIAN_POINT('Ctrl Pts',(0.646103685999945,12.2,-11.359881884));
#155398=CARTESIAN_POINT('Ctrl Pts',(0.647823038999944,12.2,-11.363117614));
#155399=CARTESIAN_POINT('Ctrl Pts',(0.649547021999944,12.2,-11.366356043));
#155400=CARTESIAN_POINT('Ctrl Pts',(0.651275639999944,12.2,-11.369597161));
#155401=CARTESIAN_POINT('Ctrl Pts',(0.653008890999944,12.2,-11.37284096));
#155402=CARTESIAN_POINT('Ctrl Pts',(0.654746778999944,12.2,-11.37608743));
#155403=CARTESIAN_POINT('Ctrl Pts',(0.656489305999944,12.2,-11.379336561));
#155404=CARTESIAN_POINT('Ctrl Pts',(0.658236471999943,12.2,-11.382588345));
#155405=CARTESIAN_POINT('Ctrl Pts',(0.659988278999944,12.2,-11.385842772));
#155406=CARTESIAN_POINT('Ctrl Pts',(0.661744729999943,12.2,-11.389099835));
#155407=CARTESIAN_POINT('Ctrl Pts',(0.663505824999944,12.2,-11.392359523));
#155408=CARTESIAN_POINT('Ctrl Pts',(0.665271565999944,12.2,-11.395621827));
#155409=CARTESIAN_POINT('Ctrl Pts',(0.667041954999944,12.2,-11.39888674));
#155410=CARTESIAN_POINT('Ctrl Pts',(0.668816992999944,12.2,-11.402154251));
#155411=CARTESIAN_POINT('Ctrl Pts',(0.670596681999944,12.2,-11.405424352));
#155412=CARTESIAN_POINT('Ctrl Pts',(0.672381022999944,12.2,-11.408697032));
#155413=CARTESIAN_POINT('Ctrl Pts',(0.674170018999944,12.2,-11.411972283));
#155414=CARTESIAN_POINT('Ctrl Pts',(0.675963669999944,12.2,-11.415250096));
#155415=CARTESIAN_POINT('Ctrl Pts',(0.677761977999943,12.2,-11.418530461));
#155416=CARTESIAN_POINT('Ctrl Pts',(0.679564944999944,12.2,-11.421813369));
#155417=CARTESIAN_POINT('Ctrl Pts',(0.681372572999944,12.2,-11.425098811));
#155418=CARTESIAN_POINT('Ctrl Pts',(0.683184861999945,12.2,-11.42838678));
#155419=CARTESIAN_POINT('Ctrl Pts',(0.685001812999944,12.2,-11.431677269));
#155420=CARTESIAN_POINT('Ctrl Pts',(0.686823428999944,12.2,-11.434970268));
#155421=CARTESIAN_POINT('Ctrl Pts',(0.688649710999945,12.2,-11.438265769));
#155422=CARTESIAN_POINT('Ctrl Pts',(0.690480658999945,12.2,-11.441563763));
#155423=CARTESIAN_POINT('Ctrl Pts',(0.692316276999944,12.2,-11.444864239));
#155424=CARTESIAN_POINT('Ctrl Pts',(0.694156563999945,12.2,-11.448167187));
#155425=CARTESIAN_POINT('Ctrl Pts',(0.696001524999944,12.2,-11.451472595));
#155426=CARTESIAN_POINT('Ctrl Pts',(0.697851158999944,12.2,-11.454780453));
#155427=CARTESIAN_POINT('Ctrl Pts',(0.699705468999944,12.2,-11.458090751));
#155428=CARTESIAN_POINT('Ctrl Pts',(0.701564455999945,12.2,-11.461403481));
#155429=CARTESIAN_POINT('Ctrl Pts',(0.703428120999944,12.2,-11.464718637));
#155430=CARTESIAN_POINT('Ctrl Pts',(0.705296462999944,12.2,-11.468036216));
#155431=CARTESIAN_POINT('Ctrl Pts',(0.707169485999944,12.2,-11.471356215));
#155432=CARTESIAN_POINT('Ctrl Pts',(0.708671644999944,12.2,-11.474014149));
#155433=CARTESIAN_POINT('Ctrl Pts',(0.709800370999945,12.2,-11.476008688));
#155434=CARTESIAN_POINT('Ctrl Pts',(0.710553790999944,12.2,-11.477338863));
#155435=CARTESIAN_POINT('Ctrl Pts',(0.710930733999944,12.2,-11.478004072));
#155436=CARTESIAN_POINT('Ctrl Pts',(1.09337742899994,15.2,-11.447904865));
#155437=CARTESIAN_POINT('Ctrl Pts',(1.09337742899994,11.6,-11.447904865));
#155438=CARTESIAN_POINT('Ctrl Pts',(1.09364566999994,15.2,-11.447188878));
#155439=CARTESIAN_POINT('Ctrl Pts',(1.09364566999994,11.6,-11.447188878));
#155440=CARTESIAN_POINT('Ctrl Pts',(1.09418172899994,15.2,-11.445757219));
#155441=CARTESIAN_POINT('Ctrl Pts',(1.09418172899994,11.6,-11.445757219));
#155442=CARTESIAN_POINT('Ctrl Pts',(1.09498454299994,15.2,-11.443610664));
#155443=CARTESIAN_POINT('Ctrl Pts',(1.09498454299994,11.6,-11.443610664));
#155444=CARTESIAN_POINT('Ctrl Pts',(1.09605241599994,15.2,-11.440750465));
#155445=CARTESIAN_POINT('Ctrl Pts',(1.09605241599994,11.6,-11.440750465));
#155446=CARTESIAN_POINT('Ctrl Pts',(1.09738301599994,15.2,-11.437178335));
#155447=CARTESIAN_POINT('Ctrl Pts',(1.09738301599994,11.6,-11.437178335));
#155448=CARTESIAN_POINT('Ctrl Pts',(1.09870937299994,15.2,-11.433609328));
#155449=CARTESIAN_POINT('Ctrl Pts',(1.09870937299994,11.6,-11.433609328));
#155450=CARTESIAN_POINT('Ctrl Pts',(1.10003148899994,15.2,-11.430043446));
#155451=CARTESIAN_POINT('Ctrl Pts',(1.10003148899994,11.6,-11.430043446));
#155452=CARTESIAN_POINT('Ctrl Pts',(1.10134936299994,15.2,-11.426480691));
#155453=CARTESIAN_POINT('Ctrl Pts',(1.10134936299994,11.6,-11.426480691));
#155454=CARTESIAN_POINT('Ctrl Pts',(1.10266299899994,15.2,-11.422921069));
#155455=CARTESIAN_POINT('Ctrl Pts',(1.10266299899994,11.6,-11.422921069));
#155456=CARTESIAN_POINT('Ctrl Pts',(1.10397239799994,15.2,-11.419364591));
#155457=CARTESIAN_POINT('Ctrl Pts',(1.10397239799994,11.6,-11.419364591));
#155458=CARTESIAN_POINT('Ctrl Pts',(1.10527756399994,15.2,-11.415811262));
#155459=CARTESIAN_POINT('Ctrl Pts',(1.10527756399994,11.6,-11.415811262));
#155460=CARTESIAN_POINT('Ctrl Pts',(1.10657849999994,15.2,-11.412261095));
#155461=CARTESIAN_POINT('Ctrl Pts',(1.10657849999994,11.6,-11.412261095));
#155462=CARTESIAN_POINT('Ctrl Pts',(1.10787520999994,15.2,-11.408714099));
#155463=CARTESIAN_POINT('Ctrl Pts',(1.10787520999994,11.6,-11.408714099));
#155464=CARTESIAN_POINT('Ctrl Pts',(1.10916769599994,15.2,-11.405170286));
#155465=CARTESIAN_POINT('Ctrl Pts',(1.10916769599994,11.6,-11.405170286));
#155466=CARTESIAN_POINT('Ctrl Pts',(1.11045596299994,15.2,-11.401629665));
#155467=CARTESIAN_POINT('Ctrl Pts',(1.11045596299994,11.6,-11.401629665));
#155468=CARTESIAN_POINT('Ctrl Pts',(1.11174001299994,15.2,-11.398092244));
#155469=CARTESIAN_POINT('Ctrl Pts',(1.11174001299994,11.6,-11.398092244));
#155470=CARTESIAN_POINT('Ctrl Pts',(1.11301984899994,15.2,-11.394558034));
#155471=CARTESIAN_POINT('Ctrl Pts',(1.11301984899994,11.6,-11.394558034));
#155472=CARTESIAN_POINT('Ctrl Pts',(1.11429547399994,15.2,-11.39102704));
#155473=CARTESIAN_POINT('Ctrl Pts',(1.11429547399994,11.6,-11.39102704));
#155474=CARTESIAN_POINT('Ctrl Pts',(1.11556688999994,15.2,-11.387499272));
#155475=CARTESIAN_POINT('Ctrl Pts',(1.11556688999994,11.6,-11.387499272));
#155476=CARTESIAN_POINT('Ctrl Pts',(1.11683409999994,15.2,-11.383974735));
#155477=CARTESIAN_POINT('Ctrl Pts',(1.11683409999994,11.6,-11.383974735));
#155478=CARTESIAN_POINT('Ctrl Pts',(1.11809710599994,15.2,-11.38045344));
#155479=CARTESIAN_POINT('Ctrl Pts',(1.11809710599994,11.6,-11.38045344));
#155480=CARTESIAN_POINT('Ctrl Pts',(1.11935591099994,15.2,-11.376935393));
#155481=CARTESIAN_POINT('Ctrl Pts',(1.11935591099994,11.6,-11.376935393));
#155482=CARTESIAN_POINT('Ctrl Pts',(1.12061051899994,15.2,-11.373420606));
#155483=CARTESIAN_POINT('Ctrl Pts',(1.12061051899994,11.6,-11.373420606));
#155484=CARTESIAN_POINT('Ctrl Pts',(1.12186093199994,15.2,-11.369909084));
#155485=CARTESIAN_POINT('Ctrl Pts',(1.12186093199994,11.6,-11.369909084));
#155486=CARTESIAN_POINT('Ctrl Pts',(1.12310715399994,15.2,-11.366400839));
#155487=CARTESIAN_POINT('Ctrl Pts',(1.12310715399994,11.6,-11.366400839));
#155488=CARTESIAN_POINT('Ctrl Pts',(1.12434918699994,15.2,-11.36289588));
#155489=CARTESIAN_POINT('Ctrl Pts',(1.12434918699994,11.6,-11.36289588));
#155490=CARTESIAN_POINT('Ctrl Pts',(1.12558703399994,15.2,-11.359394214));
#155491=CARTESIAN_POINT('Ctrl Pts',(1.12558703399994,11.6,-11.359394214));
#155492=CARTESIAN_POINT('Ctrl Pts',(1.12682069999994,15.2,-11.355895851));
#155493=CARTESIAN_POINT('Ctrl Pts',(1.12682069999994,11.6,-11.355895851));
#155494=CARTESIAN_POINT('Ctrl Pts',(1.12805018499994,15.2,-11.3524008));
#155495=CARTESIAN_POINT('Ctrl Pts',(1.12805018499994,11.6,-11.3524008));
#155496=CARTESIAN_POINT('Ctrl Pts',(1.12927549399994,15.2,-11.348909068));
#155497=CARTESIAN_POINT('Ctrl Pts',(1.12927549399994,11.6,-11.348909068));
#155498=CARTESIAN_POINT('Ctrl Pts',(1.13049662999994,15.2,-11.345420665));
#155499=CARTESIAN_POINT('Ctrl Pts',(1.13049662999994,11.6,-11.345420665));
#155500=CARTESIAN_POINT('Ctrl Pts',(1.13171359399994,15.2,-11.341935598));
#155501=CARTESIAN_POINT('Ctrl Pts',(1.13171359399994,11.6,-11.341935598));
#155502=CARTESIAN_POINT('Ctrl Pts',(1.13292639099994,15.2,-11.338453878));
#155503=CARTESIAN_POINT('Ctrl Pts',(1.13292639099994,11.6,-11.338453878));
#155504=CARTESIAN_POINT('Ctrl Pts',(1.13413502299994,15.2,-11.334975512));
#155505=CARTESIAN_POINT('Ctrl Pts',(1.13413502299994,11.6,-11.334975512));
#155506=CARTESIAN_POINT('Ctrl Pts',(1.13533949399994,15.2,-11.331500509));
#155507=CARTESIAN_POINT('Ctrl Pts',(1.13533949399994,11.6,-11.331500509));
#155508=CARTESIAN_POINT('Ctrl Pts',(1.13653980599994,15.2,-11.32802888));
#155509=CARTESIAN_POINT('Ctrl Pts',(1.13653980599994,11.6,-11.32802888));
#155510=CARTESIAN_POINT('Ctrl Pts',(1.13773596199994,15.2,-11.324560631));
#155511=CARTESIAN_POINT('Ctrl Pts',(1.13773596199994,11.6,-11.324560631));
#155512=CARTESIAN_POINT('Ctrl Pts',(1.13892796699994,15.2,-11.321095772));
#155513=CARTESIAN_POINT('Ctrl Pts',(1.13892796699994,11.6,-11.321095772));
#155514=CARTESIAN_POINT('Ctrl Pts',(1.14011582299994,15.2,-11.317634312));
#155515=CARTESIAN_POINT('Ctrl Pts',(1.14011582299994,11.6,-11.317634312));
#155516=CARTESIAN_POINT('Ctrl Pts',(1.14129953199994,15.2,-11.31417626));
#155517=CARTESIAN_POINT('Ctrl Pts',(1.14129953199994,11.6,-11.31417626));
#155518=CARTESIAN_POINT('Ctrl Pts',(1.14247909799994,15.2,-11.310721625));
#155519=CARTESIAN_POINT('Ctrl Pts',(1.14247909799994,11.6,-11.310721625));
#155520=CARTESIAN_POINT('Ctrl Pts',(1.14365452599994,15.2,-11.307270414));
#155521=CARTESIAN_POINT('Ctrl Pts',(1.14365452599994,11.6,-11.307270414));
#155522=CARTESIAN_POINT('Ctrl Pts',(1.14482581499994,15.2,-11.303822638));
#155523=CARTESIAN_POINT('Ctrl Pts',(1.14482581499994,11.6,-11.303822638));
#155524=CARTESIAN_POINT('Ctrl Pts',(1.14599297199994,15.2,-11.300378306));
#155525=CARTESIAN_POINT('Ctrl Pts',(1.14599297199994,11.6,-11.300378306));
#155526=CARTESIAN_POINT('Ctrl Pts',(1.14715599899994,15.2,-11.296937426));
#155527=CARTESIAN_POINT('Ctrl Pts',(1.14715599899994,11.6,-11.296937426));
#155528=CARTESIAN_POINT('Ctrl Pts',(1.14831489899994,15.2,-11.293500006));
#155529=CARTESIAN_POINT('Ctrl Pts',(1.14831489899994,11.6,-11.293500006));
#155530=CARTESIAN_POINT('Ctrl Pts',(1.14946967399994,15.2,-11.290066057));
#155531=CARTESIAN_POINT('Ctrl Pts',(1.14946967399994,11.6,-11.290066057));
#155532=CARTESIAN_POINT('Ctrl Pts',(1.15062032899994,15.2,-11.286635586));
#155533=CARTESIAN_POINT('Ctrl Pts',(1.15062032899994,11.6,-11.286635586));
#155534=CARTESIAN_POINT('Ctrl Pts',(1.15176686799994,15.2,-11.283208603));
#155535=CARTESIAN_POINT('Ctrl Pts',(1.15176686799994,11.6,-11.283208603));
#155536=CARTESIAN_POINT('Ctrl Pts',(1.15290929199994,15.2,-11.279785118));
#155537=CARTESIAN_POINT('Ctrl Pts',(1.15290929199994,11.6,-11.279785118));
#155538=CARTESIAN_POINT('Ctrl Pts',(1.15404760399994,15.2,-11.276365138));
#155539=CARTESIAN_POINT('Ctrl Pts',(1.15404760399994,11.6,-11.276365138));
#155540=CARTESIAN_POINT('Ctrl Pts',(1.15518180899994,15.2,-11.272948673));
#155541=CARTESIAN_POINT('Ctrl Pts',(1.15518180899994,11.6,-11.272948673));
#155542=CARTESIAN_POINT('Ctrl Pts',(1.15631190999994,15.2,-11.269535732));
#155543=CARTESIAN_POINT('Ctrl Pts',(1.15631190999994,11.6,-11.269535732));
#155544=CARTESIAN_POINT('Ctrl Pts',(1.15743790999994,15.2,-11.266126325));
#155545=CARTESIAN_POINT('Ctrl Pts',(1.15743790999994,11.6,-11.266126325));
#155546=CARTESIAN_POINT('Ctrl Pts',(1.15855981299994,15.2,-11.262720459));
#155547=CARTESIAN_POINT('Ctrl Pts',(1.15855981299994,11.6,-11.262720459));
#155548=CARTESIAN_POINT('Ctrl Pts',(1.15967762099994,15.2,-11.259318144));
#155549=CARTESIAN_POINT('Ctrl Pts',(1.15967762099994,11.6,-11.259318144));
#155550=CARTESIAN_POINT('Ctrl Pts',(1.16079133799994,15.2,-11.25591939));
#155551=CARTESIAN_POINT('Ctrl Pts',(1.16079133799994,11.6,-11.25591939));
#155552=CARTESIAN_POINT('Ctrl Pts',(1.16190096699994,15.2,-11.252524204));
#155553=CARTESIAN_POINT('Ctrl Pts',(1.16190096699994,11.6,-11.252524204));
#155554=CARTESIAN_POINT('Ctrl Pts',(1.16300651299994,15.2,-11.249132598));
#155555=CARTESIAN_POINT('Ctrl Pts',(1.16300651299994,11.6,-11.249132598));
#155556=CARTESIAN_POINT('Ctrl Pts',(1.16410797799994,15.2,-11.245744578));
#155557=CARTESIAN_POINT('Ctrl Pts',(1.16410797799994,11.6,-11.245744578));
#155558=CARTESIAN_POINT('Ctrl Pts',(1.16520536399994,15.2,-11.242360155));
#155559=CARTESIAN_POINT('Ctrl Pts',(1.16520536399994,11.6,-11.242360155));
#155560=CARTESIAN_POINT('Ctrl Pts',(1.16629867699995,15.2,-11.238979338));
#155561=CARTESIAN_POINT('Ctrl Pts',(1.16629867699995,11.6,-11.238979338));
#155562=CARTESIAN_POINT('Ctrl Pts',(1.16738791999994,15.2,-11.235602136));
#155563=CARTESIAN_POINT('Ctrl Pts',(1.16738791999994,11.6,-11.235602136));
#155564=CARTESIAN_POINT('Ctrl Pts',(1.16847309399994,15.2,-11.232228557));
#155565=CARTESIAN_POINT('Ctrl Pts',(1.16847309399994,11.6,-11.232228557));
#155566=CARTESIAN_POINT('Ctrl Pts',(1.16955420599994,15.2,-11.228858612));
#155567=CARTESIAN_POINT('Ctrl Pts',(1.16955420599994,11.6,-11.228858612));
#155568=CARTESIAN_POINT('Ctrl Pts',(1.17063125699994,15.2,-11.22549231));
#155569=CARTESIAN_POINT('Ctrl Pts',(1.17063125699994,11.6,-11.22549231));
#155570=CARTESIAN_POINT('Ctrl Pts',(1.17170425099994,15.2,-11.222129659));
#155571=CARTESIAN_POINT('Ctrl Pts',(1.17170425099994,11.6,-11.222129659));
#155572=CARTESIAN_POINT('Ctrl Pts',(1.17277319199994,15.2,-11.218770669));
#155573=CARTESIAN_POINT('Ctrl Pts',(1.17277319199994,11.6,-11.218770669));
#155574=CARTESIAN_POINT('Ctrl Pts',(1.17383808199994,15.2,-11.215415349));
#155575=CARTESIAN_POINT('Ctrl Pts',(1.17383808199994,11.6,-11.215415349));
#155576=CARTESIAN_POINT('Ctrl Pts',(1.17489892699994,15.2,-11.212063708));
#155577=CARTESIAN_POINT('Ctrl Pts',(1.17489892699994,11.6,-11.212063708));
#155578=CARTESIAN_POINT('Ctrl Pts',(1.17595572899994,15.2,-11.208715756));
#155579=CARTESIAN_POINT('Ctrl Pts',(1.17595572899994,11.6,-11.208715756));
#155580=CARTESIAN_POINT('Ctrl Pts',(1.17700849199994,15.2,-11.205371503));
#155581=CARTESIAN_POINT('Ctrl Pts',(1.17700849199994,11.6,-11.205371503));
#155582=CARTESIAN_POINT('Ctrl Pts',(1.17805721899994,15.2,-11.202030955));
#155583=CARTESIAN_POINT('Ctrl Pts',(1.17805721899994,11.6,-11.202030955));
#155584=CARTESIAN_POINT('Ctrl Pts',(1.17910191399994,15.2,-11.198694125));
#155585=CARTESIAN_POINT('Ctrl Pts',(1.17910191399994,11.6,-11.198694125));
#155586=CARTESIAN_POINT('Ctrl Pts',(1.18014258099994,15.2,-11.195361021));
#155587=CARTESIAN_POINT('Ctrl Pts',(1.18014258099994,11.6,-11.195361021));
#155588=CARTESIAN_POINT('Ctrl Pts',(1.18117922299994,15.2,-11.192031652));
#155589=CARTESIAN_POINT('Ctrl Pts',(1.18117922299994,11.6,-11.192031652));
#155590=CARTESIAN_POINT('Ctrl Pts',(1.18221184299994,15.2,-11.188706028));
#155591=CARTESIAN_POINT('Ctrl Pts',(1.18221184299994,11.6,-11.188706028));
#155592=CARTESIAN_POINT('Ctrl Pts',(1.18324044599994,15.2,-11.185384157));
#155593=CARTESIAN_POINT('Ctrl Pts',(1.18324044599994,11.6,-11.185384157));
#155594=CARTESIAN_POINT('Ctrl Pts',(1.18426503499994,15.2,-11.18206605));
#155595=CARTESIAN_POINT('Ctrl Pts',(1.18426503499994,11.6,-11.18206605));
#155596=CARTESIAN_POINT('Ctrl Pts',(1.18528561399994,15.2,-11.178751715));
#155597=CARTESIAN_POINT('Ctrl Pts',(1.18528561399994,11.6,-11.178751715));
#155598=CARTESIAN_POINT('Ctrl Pts',(1.18630218599994,15.2,-11.175441163));
#155599=CARTESIAN_POINT('Ctrl Pts',(1.18630218599994,11.6,-11.175441163));
#155600=CARTESIAN_POINT('Ctrl Pts',(1.18731475499994,15.2,-11.172134402));
#155601=CARTESIAN_POINT('Ctrl Pts',(1.18731475499994,11.6,-11.172134402));
#155602=CARTESIAN_POINT('Ctrl Pts',(1.18832332499994,15.2,-11.168831442));
#155603=CARTESIAN_POINT('Ctrl Pts',(1.18832332499994,11.6,-11.168831442));
#155604=CARTESIAN_POINT('Ctrl Pts',(1.18932789799994,15.2,-11.165532292));
#155605=CARTESIAN_POINT('Ctrl Pts',(1.18932789799994,11.6,-11.165532292));
#155606=CARTESIAN_POINT('Ctrl Pts',(1.19032848099994,15.2,-11.162236962));
#155607=CARTESIAN_POINT('Ctrl Pts',(1.19032848099994,11.6,-11.162236962));
#155608=CARTESIAN_POINT('Ctrl Pts',(1.19132507499994,15.2,-11.158945462));
#155609=CARTESIAN_POINT('Ctrl Pts',(1.19132507499994,11.6,-11.158945462));
#155610=CARTESIAN_POINT('Ctrl Pts',(1.19231768599994,15.2,-11.155657801));
#155611=CARTESIAN_POINT('Ctrl Pts',(1.19231768599994,11.6,-11.155657801));
#155612=CARTESIAN_POINT('Ctrl Pts',(1.19330631499994,15.2,-11.152373988));
#155613=CARTESIAN_POINT('Ctrl Pts',(1.19330631499994,11.6,-11.152373988));
#155614=CARTESIAN_POINT('Ctrl Pts',(1.19429096799994,15.2,-11.149094033));
#155615=CARTESIAN_POINT('Ctrl Pts',(1.19429096799994,11.6,-11.149094033));
#155616=CARTESIAN_POINT('Ctrl Pts',(1.19527164899994,15.2,-11.145817945));
#155617=CARTESIAN_POINT('Ctrl Pts',(1.19527164899994,11.6,-11.145817945));
#155618=CARTESIAN_POINT('Ctrl Pts',(1.19624835999994,15.2,-11.142545735));
#155619=CARTESIAN_POINT('Ctrl Pts',(1.19624835999994,11.6,-11.142545735));
#155620=CARTESIAN_POINT('Ctrl Pts',(1.19722110599994,15.2,-11.139277411));
#155621=CARTESIAN_POINT('Ctrl Pts',(1.19722110599994,11.6,-11.139277411));
#155622=CARTESIAN_POINT('Ctrl Pts',(1.19818989099994,15.2,-11.136012983));
#155623=CARTESIAN_POINT('Ctrl Pts',(1.19818989099994,11.6,-11.136012983));
#155624=CARTESIAN_POINT('Ctrl Pts',(1.19915471699994,15.2,-11.132752462));
#155625=CARTESIAN_POINT('Ctrl Pts',(1.19915471699994,11.6,-11.132752462));
#155626=CARTESIAN_POINT('Ctrl Pts',(1.20011559099995,15.2,-11.129495855));
#155627=CARTESIAN_POINT('Ctrl Pts',(1.20011559099995,11.6,-11.129495855));
#155628=CARTESIAN_POINT('Ctrl Pts',(1.20107251499994,15.2,-11.126243174));
#155629=CARTESIAN_POINT('Ctrl Pts',(1.20107251499994,11.6,-11.126243174));
#155630=CARTESIAN_POINT('Ctrl Pts',(1.20202549299994,15.2,-11.122994428));
#155631=CARTESIAN_POINT('Ctrl Pts',(1.20202549299994,11.6,-11.122994428));
#155632=CARTESIAN_POINT('Ctrl Pts',(1.20297452899994,15.2,-11.119749625));
#155633=CARTESIAN_POINT('Ctrl Pts',(1.20297452899994,11.6,-11.119749625));
#155634=CARTESIAN_POINT('Ctrl Pts',(1.20391962699994,15.2,-11.116508778));
#155635=CARTESIAN_POINT('Ctrl Pts',(1.20391962699994,11.6,-11.116508778));
#155636=CARTESIAN_POINT('Ctrl Pts',(1.20486078999994,15.2,-11.113271894));
#155637=CARTESIAN_POINT('Ctrl Pts',(1.20486078999994,11.6,-11.113271894));
#155638=CARTESIAN_POINT('Ctrl Pts',(1.20579802499994,15.2,-11.110038983));
#155639=CARTESIAN_POINT('Ctrl Pts',(1.20579802499994,11.6,-11.110038983));
#155640=CARTESIAN_POINT('Ctrl Pts',(1.20673133299994,15.2,-11.106810055));
#155641=CARTESIAN_POINT('Ctrl Pts',(1.20673133299994,11.6,-11.106810055));
#155642=CARTESIAN_POINT('Ctrl Pts',(1.20766071899994,15.2,-11.103585121));
#155643=CARTESIAN_POINT('Ctrl Pts',(1.20766071899994,11.6,-11.103585121));
#155644=CARTESIAN_POINT('Ctrl Pts',(1.20858618699994,15.2,-11.100364189));
#155645=CARTESIAN_POINT('Ctrl Pts',(1.20858618699994,11.6,-11.100364189));
#155646=CARTESIAN_POINT('Ctrl Pts',(1.20950774199994,15.2,-11.09714727));
#155647=CARTESIAN_POINT('Ctrl Pts',(1.20950774199994,11.6,-11.09714727));
#155648=CARTESIAN_POINT('Ctrl Pts',(1.21042538699994,15.2,-11.093934372));
#155649=CARTESIAN_POINT('Ctrl Pts',(1.21042538699994,11.6,-11.093934372));
#155650=CARTESIAN_POINT('Ctrl Pts',(1.21133912499995,15.2,-11.090725508));
#155651=CARTESIAN_POINT('Ctrl Pts',(1.21133912499995,11.6,-11.090725508));
#155652=CARTESIAN_POINT('Ctrl Pts',(1.21224896299994,15.2,-11.087520685));
#155653=CARTESIAN_POINT('Ctrl Pts',(1.21224896299994,11.6,-11.087520685));
#155654=CARTESIAN_POINT('Ctrl Pts',(1.21315490199994,15.2,-11.084319915));
#155655=CARTESIAN_POINT('Ctrl Pts',(1.21315490199994,11.6,-11.084319915));
#155656=CARTESIAN_POINT('Ctrl Pts',(1.21405694699994,15.2,-11.081123205));
#155657=CARTESIAN_POINT('Ctrl Pts',(1.21405694699994,11.6,-11.081123205));
#155658=CARTESIAN_POINT('Ctrl Pts',(1.21495510399994,15.2,-11.077930567));
#155659=CARTESIAN_POINT('Ctrl Pts',(1.21495510399994,11.6,-11.077930567));
#155660=CARTESIAN_POINT('Ctrl Pts',(1.21584937499994,15.2,-11.074742011));
#155661=CARTESIAN_POINT('Ctrl Pts',(1.21584937499994,11.6,-11.074742011));
#155662=CARTESIAN_POINT('Ctrl Pts',(1.21673976599994,15.2,-11.071557546));
#155663=CARTESIAN_POINT('Ctrl Pts',(1.21673976599994,11.6,-11.071557546));
#155664=CARTESIAN_POINT('Ctrl Pts',(1.21762627899994,15.2,-11.068377182));
#155665=CARTESIAN_POINT('Ctrl Pts',(1.21762627899994,11.6,-11.068377182));
#155666=CARTESIAN_POINT('Ctrl Pts',(1.21850891999994,15.2,-11.06520093));
#155667=CARTESIAN_POINT('Ctrl Pts',(1.21850891999994,11.6,-11.06520093));
#155668=CARTESIAN_POINT('Ctrl Pts',(1.21938769199994,15.2,-11.062028798));
#155669=CARTESIAN_POINT('Ctrl Pts',(1.21938769199994,11.6,-11.062028798));
#155670=CARTESIAN_POINT('Ctrl Pts',(1.22026259999994,15.2,-11.058860798));
#155671=CARTESIAN_POINT('Ctrl Pts',(1.22026259999994,11.6,-11.058860798));
#155672=CARTESIAN_POINT('Ctrl Pts',(1.22113364899994,15.2,-11.055696939));
#155673=CARTESIAN_POINT('Ctrl Pts',(1.22113364899994,11.6,-11.055696939));
#155674=CARTESIAN_POINT('Ctrl Pts',(1.22200084099994,15.2,-11.052537231));
#155675=CARTESIAN_POINT('Ctrl Pts',(1.22200084099994,11.6,-11.052537231));
#155676=CARTESIAN_POINT('Ctrl Pts',(1.22286418199994,15.2,-11.049381684));
#155677=CARTESIAN_POINT('Ctrl Pts',(1.22286418199994,11.6,-11.049381684));
#155678=CARTESIAN_POINT('Ctrl Pts',(1.22372367599994,15.2,-11.046230309));
#155679=CARTESIAN_POINT('Ctrl Pts',(1.22372367599994,11.6,-11.046230309));
#155680=CARTESIAN_POINT('Ctrl Pts',(1.22457932699994,15.2,-11.043083114));
#155681=CARTESIAN_POINT('Ctrl Pts',(1.22457932699994,11.6,-11.043083114));
#155682=CARTESIAN_POINT('Ctrl Pts',(1.22543113999994,15.2,-11.03994011));
#155683=CARTESIAN_POINT('Ctrl Pts',(1.22543113999994,11.6,-11.03994011));
#155684=CARTESIAN_POINT('Ctrl Pts',(1.22627911799994,15.2,-11.036801309));
#155685=CARTESIAN_POINT('Ctrl Pts',(1.22627911799994,11.6,-11.036801309));
#155686=CARTESIAN_POINT('Ctrl Pts',(1.22712326699994,15.2,-11.033666719));
#155687=CARTESIAN_POINT('Ctrl Pts',(1.22712326699994,11.6,-11.033666719));
#155688=CARTESIAN_POINT('Ctrl Pts',(1.22796359099994,15.2,-11.030536351));
#155689=CARTESIAN_POINT('Ctrl Pts',(1.22796359099994,11.6,-11.030536351));
#155690=CARTESIAN_POINT('Ctrl Pts',(1.22880009299994,15.2,-11.027410214));
#155691=CARTESIAN_POINT('Ctrl Pts',(1.22880009299994,11.6,-11.027410214));
#155692=CARTESIAN_POINT('Ctrl Pts',(1.22963277899994,15.2,-11.024288319));
#155693=CARTESIAN_POINT('Ctrl Pts',(1.22963277899994,11.6,-11.024288319));
#155694=CARTESIAN_POINT('Ctrl Pts',(1.23046165299994,15.2,-11.021170677));
#155695=CARTESIAN_POINT('Ctrl Pts',(1.23046165299994,11.6,-11.021170677));
#155696=CARTESIAN_POINT('Ctrl Pts',(1.23128671899994,15.2,-11.018057297));
#155697=CARTESIAN_POINT('Ctrl Pts',(1.23128671899994,11.6,-11.018057297));
#155698=CARTESIAN_POINT('Ctrl Pts',(1.23210798199994,15.2,-11.01494819));
#155699=CARTESIAN_POINT('Ctrl Pts',(1.23210798199994,11.6,-11.01494819));
#155700=CARTESIAN_POINT('Ctrl Pts',(1.23292544599995,15.2,-11.011843364));
#155701=CARTESIAN_POINT('Ctrl Pts',(1.23292544599995,11.6,-11.011843364));
#155702=CARTESIAN_POINT('Ctrl Pts',(1.23373911599994,15.2,-11.008742833));
#155703=CARTESIAN_POINT('Ctrl Pts',(1.23373911599994,11.6,-11.008742833));
#155704=CARTESIAN_POINT('Ctrl Pts',(1.23454899599994,15.2,-11.005646604));
#155705=CARTESIAN_POINT('Ctrl Pts',(1.23454899599994,11.6,-11.005646604));
#155706=CARTESIAN_POINT('Ctrl Pts',(1.23535509099994,15.2,-11.002554689));
#155707=CARTESIAN_POINT('Ctrl Pts',(1.23535509099994,11.6,-11.002554689));
#155708=CARTESIAN_POINT('Ctrl Pts',(1.23615740499994,15.2,-10.999467099));
#155709=CARTESIAN_POINT('Ctrl Pts',(1.23615740499994,11.6,-10.999467099));
#155710=CARTESIAN_POINT('Ctrl Pts',(1.23695594399994,15.2,-10.996383842));
#155711=CARTESIAN_POINT('Ctrl Pts',(1.23695594399994,11.6,-10.996383842));
#155712=CARTESIAN_POINT('Ctrl Pts',(1.23775071099994,15.2,-10.99330493));
#155713=CARTESIAN_POINT('Ctrl Pts',(1.23775071099994,11.6,-10.99330493));
#155714=CARTESIAN_POINT('Ctrl Pts',(1.23854171099994,15.2,-10.990230373));
#155715=CARTESIAN_POINT('Ctrl Pts',(1.23854171099994,11.6,-10.990230373));
#155716=CARTESIAN_POINT('Ctrl Pts',(1.23932894799994,15.2,-10.98716018));
#155717=CARTESIAN_POINT('Ctrl Pts',(1.23932894799994,11.6,-10.98716018));
#155718=CARTESIAN_POINT('Ctrl Pts',(1.24011242899994,15.2,-10.984094365));
#155719=CARTESIAN_POINT('Ctrl Pts',(1.24011242899994,11.6,-10.984094365));
#155720=CARTESIAN_POINT('Ctrl Pts',(1.24089215599994,15.2,-10.981032935));
#155721=CARTESIAN_POINT('Ctrl Pts',(1.24089215599994,11.6,-10.981032935));
#155722=CARTESIAN_POINT('Ctrl Pts',(1.24166813499994,15.2,-10.977975901));
#155723=CARTESIAN_POINT('Ctrl Pts',(1.24166813499994,11.6,-10.977975901));
#155724=CARTESIAN_POINT('Ctrl Pts',(1.24244037099994,15.2,-10.974923275));
#155725=CARTESIAN_POINT('Ctrl Pts',(1.24244037099994,11.6,-10.974923275));
#155726=CARTESIAN_POINT('Ctrl Pts',(1.24320886799994,15.2,-10.971875066));
#155727=CARTESIAN_POINT('Ctrl Pts',(1.24320886799994,11.6,-10.971875066));
#155728=CARTESIAN_POINT('Ctrl Pts',(1.24397362999994,15.2,-10.968831284));
#155729=CARTESIAN_POINT('Ctrl Pts',(1.24397362999994,11.6,-10.968831284));
#155730=CARTESIAN_POINT('Ctrl Pts',(1.24473466399994,15.2,-10.965791941));
#155731=CARTESIAN_POINT('Ctrl Pts',(1.24473466399994,11.6,-10.965791941));
#155732=CARTESIAN_POINT('Ctrl Pts',(1.24549197299994,15.2,-10.962757048));
#155733=CARTESIAN_POINT('Ctrl Pts',(1.24549197299994,11.6,-10.962757048));
#155734=CARTESIAN_POINT('Ctrl Pts',(1.24624556199994,15.2,-10.959726614));
#155735=CARTESIAN_POINT('Ctrl Pts',(1.24624556199994,11.6,-10.959726614));
#155736=CARTESIAN_POINT('Ctrl Pts',(1.24699543599994,15.2,-10.95670065));
#155737=CARTESIAN_POINT('Ctrl Pts',(1.24699543599994,11.6,-10.95670065));
#155738=CARTESIAN_POINT('Ctrl Pts',(1.24774159999994,15.2,-10.953679166));
#155739=CARTESIAN_POINT('Ctrl Pts',(1.24774159999994,11.6,-10.953679166));
#155740=CARTESIAN_POINT('Ctrl Pts',(1.24848405899994,15.2,-10.950662174));
#155741=CARTESIAN_POINT('Ctrl Pts',(1.24848405899994,11.6,-10.950662174));
#155742=CARTESIAN_POINT('Ctrl Pts',(1.24922281699994,15.2,-10.947649684));
#155743=CARTESIAN_POINT('Ctrl Pts',(1.24922281699994,11.6,-10.947649684));
#155744=CARTESIAN_POINT('Ctrl Pts',(1.24995787899994,15.2,-10.944641705));
#155745=CARTESIAN_POINT('Ctrl Pts',(1.24995787899994,11.6,-10.944641705));
#155746=CARTESIAN_POINT('Ctrl Pts',(1.25068925199994,15.2,-10.941638251));
#155747=CARTESIAN_POINT('Ctrl Pts',(1.25068925199994,11.6,-10.941638251));
#155748=CARTESIAN_POINT('Ctrl Pts',(1.25141693799994,15.2,-10.93863933));
#155749=CARTESIAN_POINT('Ctrl Pts',(1.25141693799994,11.6,-10.93863933));
#155750=CARTESIAN_POINT('Ctrl Pts',(1.25214094299994,15.2,-10.935644954));
#155751=CARTESIAN_POINT('Ctrl Pts',(1.25214094299994,11.6,-10.935644954));
#155752=CARTESIAN_POINT('Ctrl Pts',(1.25286127299994,15.2,-10.932655133));
#155753=CARTESIAN_POINT('Ctrl Pts',(1.25286127299994,11.6,-10.932655133));
#155754=CARTESIAN_POINT('Ctrl Pts',(1.25357793199994,15.2,-10.929669878));
#155755=CARTESIAN_POINT('Ctrl Pts',(1.25357793199994,11.6,-10.929669878));
#155756=CARTESIAN_POINT('Ctrl Pts',(1.25429092499994,15.2,-10.9266892));
#155757=CARTESIAN_POINT('Ctrl Pts',(1.25429092499994,11.6,-10.9266892));
#155758=CARTESIAN_POINT('Ctrl Pts',(1.25500025699994,15.2,-10.923713108));
#155759=CARTESIAN_POINT('Ctrl Pts',(1.25500025699994,11.6,-10.923713108));
#155760=CARTESIAN_POINT('Ctrl Pts',(1.25570593399994,15.2,-10.920741616));
#155761=CARTESIAN_POINT('Ctrl Pts',(1.25570593399994,11.6,-10.920741616));
#155762=CARTESIAN_POINT('Ctrl Pts',(1.25640795899994,15.2,-10.917774733));
#155763=CARTESIAN_POINT('Ctrl Pts',(1.25640795899994,11.6,-10.917774733));
#155764=CARTESIAN_POINT('Ctrl Pts',(1.25710633899994,15.2,-10.91481247));
#155765=CARTESIAN_POINT('Ctrl Pts',(1.25710633899994,11.6,-10.91481247));
#155766=CARTESIAN_POINT('Ctrl Pts',(1.25780107799994,15.2,-10.911854838));
#155767=CARTESIAN_POINT('Ctrl Pts',(1.25780107799994,11.6,-10.911854838));
#155768=CARTESIAN_POINT('Ctrl Pts',(1.25849218299994,15.2,-10.908901847));
#155769=CARTESIAN_POINT('Ctrl Pts',(1.25849218299994,11.6,-10.908901847));
#155770=CARTESIAN_POINT('Ctrl Pts',(1.25917965599994,15.2,-10.905953509));
#155771=CARTESIAN_POINT('Ctrl Pts',(1.25917965599994,11.6,-10.905953509));
#155772=CARTESIAN_POINT('Ctrl Pts',(1.25986350399994,15.2,-10.903009834));
#155773=CARTESIAN_POINT('Ctrl Pts',(1.25986350399994,11.6,-10.903009834));
#155774=CARTESIAN_POINT('Ctrl Pts',(1.26054373299994,15.2,-10.900070834));
#155775=CARTESIAN_POINT('Ctrl Pts',(1.26054373299994,11.6,-10.900070834));
#155776=CARTESIAN_POINT('Ctrl Pts',(1.26122034599994,15.2,-10.89713652));
#155777=CARTESIAN_POINT('Ctrl Pts',(1.26122034599994,11.6,-10.89713652));
#155778=CARTESIAN_POINT('Ctrl Pts',(1.26189334999994,15.2,-10.894206901));
#155779=CARTESIAN_POINT('Ctrl Pts',(1.26189334999994,11.6,-10.894206901));
#155780=CARTESIAN_POINT('Ctrl Pts',(1.26256274999994,15.2,-10.89128199));
#155781=CARTESIAN_POINT('Ctrl Pts',(1.26256274999994,11.6,-10.89128199));
#155782=CARTESIAN_POINT('Ctrl Pts',(1.26322855099994,15.2,-10.888361798));
#155783=CARTESIAN_POINT('Ctrl Pts',(1.26322855099994,11.6,-10.888361798));
#155784=CARTESIAN_POINT('Ctrl Pts',(1.26389075699994,15.2,-10.885446335));
#155785=CARTESIAN_POINT('Ctrl Pts',(1.26389075699994,11.6,-10.885446335));
#155786=CARTESIAN_POINT('Ctrl Pts',(1.26454937499994,15.2,-10.882535612));
#155787=CARTESIAN_POINT('Ctrl Pts',(1.26454937499994,11.6,-10.882535612));
#155788=CARTESIAN_POINT('Ctrl Pts',(1.26520440999994,15.2,-10.879629641));
#155789=CARTESIAN_POINT('Ctrl Pts',(1.26520440999994,11.6,-10.879629641));
#155790=CARTESIAN_POINT('Ctrl Pts',(1.26585586699994,15.2,-10.876728433));
#155791=CARTESIAN_POINT('Ctrl Pts',(1.26585586699994,11.6,-10.876728433));
#155792=CARTESIAN_POINT('Ctrl Pts',(1.26650375199994,15.2,-10.873831999));
#155793=CARTESIAN_POINT('Ctrl Pts',(1.26650375199994,11.6,-10.873831999));
#155794=CARTESIAN_POINT('Ctrl Pts',(1.26714806899994,15.2,-10.870940349));
#155795=CARTESIAN_POINT('Ctrl Pts',(1.26714806899994,11.6,-10.870940349));
#155796=CARTESIAN_POINT('Ctrl Pts',(1.26778882499994,15.2,-10.868053496));
#155797=CARTESIAN_POINT('Ctrl Pts',(1.26778882499994,11.6,-10.868053496));
#155798=CARTESIAN_POINT('Ctrl Pts',(1.26842602399994,15.2,-10.86517145));
#155799=CARTESIAN_POINT('Ctrl Pts',(1.26842602399994,11.6,-10.86517145));
#155800=CARTESIAN_POINT('Ctrl Pts',(1.26905967299994,15.2,-10.862294222));
#155801=CARTESIAN_POINT('Ctrl Pts',(1.26905967299994,11.6,-10.862294222));
#155802=CARTESIAN_POINT('Ctrl Pts',(1.26968977599994,15.2,-10.859421825));
#155803=CARTESIAN_POINT('Ctrl Pts',(1.26968977599994,11.6,-10.859421825));
#155804=CARTESIAN_POINT('Ctrl Pts',(1.27031633899994,15.2,-10.856554267));
#155805=CARTESIAN_POINT('Ctrl Pts',(1.27031633899994,11.6,-10.856554267));
#155806=CARTESIAN_POINT('Ctrl Pts',(1.27093936699994,15.2,-10.853691563));
#155807=CARTESIAN_POINT('Ctrl Pts',(1.27093936699994,11.6,-10.853691563));
#155808=CARTESIAN_POINT('Ctrl Pts',(1.27155886699994,15.2,-10.850833723));
#155809=CARTESIAN_POINT('Ctrl Pts',(1.27155886699994,11.6,-10.850833723));
#155810=CARTESIAN_POINT('Ctrl Pts',(1.27217484299994,15.2,-10.847980757));
#155811=CARTESIAN_POINT('Ctrl Pts',(1.27217484299994,11.6,-10.847980757));
#155812=CARTESIAN_POINT('Ctrl Pts',(1.27278730099994,15.2,-10.845132677));
#155813=CARTESIAN_POINT('Ctrl Pts',(1.27278730099994,11.6,-10.845132677));
#155814=CARTESIAN_POINT('Ctrl Pts',(1.27339624799994,15.2,-10.842289496));
#155815=CARTESIAN_POINT('Ctrl Pts',(1.27339624799994,11.6,-10.842289496));
#155816=CARTESIAN_POINT('Ctrl Pts',(1.27400168799994,15.2,-10.839451223));
#155817=CARTESIAN_POINT('Ctrl Pts',(1.27400168799994,11.6,-10.839451223));
#155818=CARTESIAN_POINT('Ctrl Pts',(1.27460362599994,15.2,-10.83661787));
#155819=CARTESIAN_POINT('Ctrl Pts',(1.27460362599994,11.6,-10.83661787));
#155820=CARTESIAN_POINT('Ctrl Pts',(1.27520206999994,15.2,-10.833789449));
#155821=CARTESIAN_POINT('Ctrl Pts',(1.27520206999994,11.6,-10.833789449));
#155822=CARTESIAN_POINT('Ctrl Pts',(1.27579702299994,15.2,-10.830965973));
#155823=CARTESIAN_POINT('Ctrl Pts',(1.27579702299994,11.6,-10.830965973));
#155824=CARTESIAN_POINT('Ctrl Pts',(1.27638849299994,15.2,-10.828147449));
#155825=CARTESIAN_POINT('Ctrl Pts',(1.27638849299994,11.6,-10.828147449));
#155826=CARTESIAN_POINT('Ctrl Pts',(1.27697648499994,15.2,-10.825333894));
#155827=CARTESIAN_POINT('Ctrl Pts',(1.27697648499994,11.6,-10.825333894));
#155828=CARTESIAN_POINT('Ctrl Pts',(1.27756100499994,15.2,-10.822525316));
#155829=CARTESIAN_POINT('Ctrl Pts',(1.27756100499994,11.6,-10.822525316));
#155830=CARTESIAN_POINT('Ctrl Pts',(1.27814205599994,15.2,-10.819721726));
#155831=CARTESIAN_POINT('Ctrl Pts',(1.27814205599994,11.6,-10.819721726));
#155832=CARTESIAN_POINT('Ctrl Pts',(1.27871964799994,15.2,-10.816923139));
#155833=CARTESIAN_POINT('Ctrl Pts',(1.27871964799994,11.6,-10.816923139));
#155834=CARTESIAN_POINT('Ctrl Pts',(1.27929378499994,15.2,-10.814129563));
#155835=CARTESIAN_POINT('Ctrl Pts',(1.27929378499994,11.6,-10.814129563));
#155836=CARTESIAN_POINT('Ctrl Pts',(1.27986447099994,15.2,-10.811341012));
#155837=CARTESIAN_POINT('Ctrl Pts',(1.27986447099994,11.6,-10.811341012));
#155838=CARTESIAN_POINT('Ctrl Pts',(1.28043171499994,15.2,-10.808557497));
#155839=CARTESIAN_POINT('Ctrl Pts',(1.28043171499994,11.6,-10.808557497));
#155840=CARTESIAN_POINT('Ctrl Pts',(1.28099552199994,15.2,-10.805779028));
#155841=CARTESIAN_POINT('Ctrl Pts',(1.28099552199994,11.6,-10.805779028));
#155842=CARTESIAN_POINT('Ctrl Pts',(1.28155589699994,15.2,-10.80300562));
#155843=CARTESIAN_POINT('Ctrl Pts',(1.28155589699994,11.6,-10.80300562));
#155844=CARTESIAN_POINT('Ctrl Pts',(1.28211284599994,15.2,-10.800237282));
#155845=CARTESIAN_POINT('Ctrl Pts',(1.28211284599994,11.6,-10.800237282));
#155846=CARTESIAN_POINT('Ctrl Pts',(1.28266637399994,15.2,-10.797474026));
#155847=CARTESIAN_POINT('Ctrl Pts',(1.28266637399994,11.6,-10.797474026));
#155848=CARTESIAN_POINT('Ctrl Pts',(1.28321648999994,15.2,-10.794715865));
#155849=CARTESIAN_POINT('Ctrl Pts',(1.28321648999994,11.6,-10.794715865));
#155850=CARTESIAN_POINT('Ctrl Pts',(1.28376319699994,15.2,-10.791962811));
#155851=CARTESIAN_POINT('Ctrl Pts',(1.28376319699994,11.6,-10.791962811));
#155852=CARTESIAN_POINT('Ctrl Pts',(1.28430650299994,15.2,-10.789214873));
#155853=CARTESIAN_POINT('Ctrl Pts',(1.28430650299994,11.6,-10.789214873));
#155854=CARTESIAN_POINT('Ctrl Pts',(1.28484641299994,15.2,-10.786472067));
#155855=CARTESIAN_POINT('Ctrl Pts',(1.28484641299994,11.6,-10.786472067));
#155856=CARTESIAN_POINT('Ctrl Pts',(1.28538293299994,15.2,-10.7837344));
#155857=CARTESIAN_POINT('Ctrl Pts',(1.28538293299994,11.6,-10.7837344));
#155858=CARTESIAN_POINT('Ctrl Pts',(1.28591606999994,15.2,-10.781001888));
#155859=CARTESIAN_POINT('Ctrl Pts',(1.28591606999994,11.6,-10.781001888));
#155860=CARTESIAN_POINT('Ctrl Pts',(1.28644582999994,15.2,-10.778274541));
#155861=CARTESIAN_POINT('Ctrl Pts',(1.28644582999994,11.6,-10.778274541));
#155862=CARTESIAN_POINT('Ctrl Pts',(1.28697221699994,15.2,-10.775552372));
#155863=CARTESIAN_POINT('Ctrl Pts',(1.28697221699994,11.6,-10.775552372));
#155864=CARTESIAN_POINT('Ctrl Pts',(1.28749524099994,15.2,-10.772835393));
#155865=CARTESIAN_POINT('Ctrl Pts',(1.28749524099994,11.6,-10.772835393));
#155866=CARTESIAN_POINT('Ctrl Pts',(1.28801490399994,15.2,-10.770123614));
#155867=CARTESIAN_POINT('Ctrl Pts',(1.28801490399994,11.6,-10.770123614));
#155868=CARTESIAN_POINT('Ctrl Pts',(1.28853121599994,15.2,-10.767417049));
#155869=CARTESIAN_POINT('Ctrl Pts',(1.28853121599994,11.6,-10.767417049));
#155870=CARTESIAN_POINT('Ctrl Pts',(1.28904418099994,15.2,-10.764715709));
#155871=CARTESIAN_POINT('Ctrl Pts',(1.28904418099994,11.6,-10.764715709));
#155872=CARTESIAN_POINT('Ctrl Pts',(1.28955380499994,15.2,-10.762019607));
#155873=CARTESIAN_POINT('Ctrl Pts',(1.28955380499994,11.6,-10.762019607));
#155874=CARTESIAN_POINT('Ctrl Pts',(1.29006009599994,15.2,-10.759328754));
#155875=CARTESIAN_POINT('Ctrl Pts',(1.29006009599994,11.6,-10.759328754));
#155876=CARTESIAN_POINT('Ctrl Pts',(1.29056305799994,15.2,-10.756643162));
#155877=CARTESIAN_POINT('Ctrl Pts',(1.29056305799994,11.6,-10.756643162));
#155878=CARTESIAN_POINT('Ctrl Pts',(1.29106269899994,15.2,-10.753962844));
#155879=CARTESIAN_POINT('Ctrl Pts',(1.29106269899994,11.6,-10.753962844));
#155880=CARTESIAN_POINT('Ctrl Pts',(1.29155902499994,15.2,-10.751287813));
#155881=CARTESIAN_POINT('Ctrl Pts',(1.29155902499994,11.6,-10.751287813));
#155882=CARTESIAN_POINT('Ctrl Pts',(1.29205204299994,15.2,-10.748618079));
#155883=CARTESIAN_POINT('Ctrl Pts',(1.29205204299994,11.6,-10.748618079));
#155884=CARTESIAN_POINT('Ctrl Pts',(1.29254175999994,15.2,-10.745953656));
#155885=CARTESIAN_POINT('Ctrl Pts',(1.29254175999994,11.6,-10.745953656));
#155886=CARTESIAN_POINT('Ctrl Pts',(1.29302817899994,15.2,-10.743294554));
#155887=CARTESIAN_POINT('Ctrl Pts',(1.29302817899994,11.6,-10.743294554));
#155888=CARTESIAN_POINT('Ctrl Pts',(1.29351130999994,15.2,-10.740640788));
#155889=CARTESIAN_POINT('Ctrl Pts',(1.29351130999994,11.6,-10.740640788));
#155890=CARTESIAN_POINT('Ctrl Pts',(1.29399115799994,15.2,-10.737992369));
#155891=CARTESIAN_POINT('Ctrl Pts',(1.29399115799994,11.6,-10.737992369));
#155892=CARTESIAN_POINT('Ctrl Pts',(1.29446772899994,15.2,-10.73534931));
#155893=CARTESIAN_POINT('Ctrl Pts',(1.29446772899994,11.6,-10.73534931));
#155894=CARTESIAN_POINT('Ctrl Pts',(1.29494102999994,15.2,-10.732711622));
#155895=CARTESIAN_POINT('Ctrl Pts',(1.29494102999994,11.6,-10.732711622));
#155896=CARTESIAN_POINT('Ctrl Pts',(1.29541106899994,15.2,-10.730079319));
#155897=CARTESIAN_POINT('Ctrl Pts',(1.29541106899994,11.6,-10.730079319));
#155898=CARTESIAN_POINT('Ctrl Pts',(1.29587784999994,15.2,-10.727452411));
#155899=CARTESIAN_POINT('Ctrl Pts',(1.29587784999994,11.6,-10.727452411));
#155900=CARTESIAN_POINT('Ctrl Pts',(1.29634138199994,15.2,-10.724830913));
#155901=CARTESIAN_POINT('Ctrl Pts',(1.29634138199994,11.6,-10.724830913));
#155902=CARTESIAN_POINT('Ctrl Pts',(1.29680167099994,15.2,-10.722214836));
#155903=CARTESIAN_POINT('Ctrl Pts',(1.29680167099994,11.6,-10.722214836));
#155904=CARTESIAN_POINT('Ctrl Pts',(1.29725872199994,15.2,-10.719604194));
#155905=CARTESIAN_POINT('Ctrl Pts',(1.29725872199994,11.6,-10.719604194));
#155906=CARTESIAN_POINT('Ctrl Pts',(1.29771254399994,15.2,-10.716998997));
#155907=CARTESIAN_POINT('Ctrl Pts',(1.29771254399994,11.6,-10.716998997));
#155908=CARTESIAN_POINT('Ctrl Pts',(1.29816314199994,15.2,-10.714399259));
#155909=CARTESIAN_POINT('Ctrl Pts',(1.29816314199994,11.6,-10.714399259));
#155910=CARTESIAN_POINT('Ctrl Pts',(1.29861052399994,15.2,-10.711804993));
#155911=CARTESIAN_POINT('Ctrl Pts',(1.29861052399994,11.6,-10.711804993));
#155912=CARTESIAN_POINT('Ctrl Pts',(1.29905469599994,15.2,-10.70921621));
#155913=CARTESIAN_POINT('Ctrl Pts',(1.29905469599994,11.6,-10.70921621));
#155914=CARTESIAN_POINT('Ctrl Pts',(1.29949566599994,15.2,-10.706632926));
#155915=CARTESIAN_POINT('Ctrl Pts',(1.29949566599994,11.6,-10.706632926));
#155916=CARTESIAN_POINT('Ctrl Pts',(1.29993343799994,15.2,-10.70405515));
#155917=CARTESIAN_POINT('Ctrl Pts',(1.29993343799994,11.6,-10.70405515));
#155918=CARTESIAN_POINT('Ctrl Pts',(1.30036802199994,15.2,-10.701482895));
#155919=CARTESIAN_POINT('Ctrl Pts',(1.30036802199994,11.6,-10.701482895));
#155920=CARTESIAN_POINT('Ctrl Pts',(1.30079942299994,15.2,-10.698916176));
#155921=CARTESIAN_POINT('Ctrl Pts',(1.30079942299994,11.6,-10.698916176));
#155922=CARTESIAN_POINT('Ctrl Pts',(1.30122764799994,15.2,-10.696355005));
#155923=CARTESIAN_POINT('Ctrl Pts',(1.30122764799994,11.6,-10.696355005));
#155924=CARTESIAN_POINT('Ctrl Pts',(1.30165270499994,15.2,-10.693799393));
#155925=CARTESIAN_POINT('Ctrl Pts',(1.30165270499994,11.6,-10.693799393));
#155926=CARTESIAN_POINT('Ctrl Pts',(1.30207460099994,15.2,-10.691249355));
#155927=CARTESIAN_POINT('Ctrl Pts',(1.30207460099994,11.6,-10.691249355));
#155928=CARTESIAN_POINT('Ctrl Pts',(1.30249334099994,15.2,-10.688704902));
#155929=CARTESIAN_POINT('Ctrl Pts',(1.30249334099994,11.6,-10.688704902));
#155930=CARTESIAN_POINT('Ctrl Pts',(1.30290893499994,15.2,-10.686166048));
#155931=CARTESIAN_POINT('Ctrl Pts',(1.30290893499994,11.6,-10.686166048));
#155932=CARTESIAN_POINT('Ctrl Pts',(1.30332138799994,15.2,-10.683632806));
#155933=CARTESIAN_POINT('Ctrl Pts',(1.30332138799994,11.6,-10.683632806));
#155934=CARTESIAN_POINT('Ctrl Pts',(1.30373070599994,15.2,-10.681105188));
#155935=CARTESIAN_POINT('Ctrl Pts',(1.30373070599994,11.6,-10.681105188));
#155936=CARTESIAN_POINT('Ctrl Pts',(1.30413689999994,15.2,-10.678583208));
#155937=CARTESIAN_POINT('Ctrl Pts',(1.30413689999994,11.6,-10.678583208));
#155938=CARTESIAN_POINT('Ctrl Pts',(1.30453997299994,15.2,-10.676066879));
#155939=CARTESIAN_POINT('Ctrl Pts',(1.30453997299994,11.6,-10.676066879));
#155940=CARTESIAN_POINT('Ctrl Pts',(1.30493993399994,15.2,-10.673556212));
#155941=CARTESIAN_POINT('Ctrl Pts',(1.30493993399994,11.6,-10.673556212));
#155942=CARTESIAN_POINT('Ctrl Pts',(1.30533679099994,15.2,-10.671051222));
#155943=CARTESIAN_POINT('Ctrl Pts',(1.30533679099994,11.6,-10.671051222));
#155944=CARTESIAN_POINT('Ctrl Pts',(1.30573054999994,15.2,-10.668551921));
#155945=CARTESIAN_POINT('Ctrl Pts',(1.30573054999994,11.6,-10.668551921));
#155946=CARTESIAN_POINT('Ctrl Pts',(1.30612121799994,15.2,-10.666058323));
#155947=CARTESIAN_POINT('Ctrl Pts',(1.30612121799994,11.6,-10.666058323));
#155948=CARTESIAN_POINT('Ctrl Pts',(1.30650880299994,15.2,-10.663570441));
#155949=CARTESIAN_POINT('Ctrl Pts',(1.30650880299994,11.6,-10.663570441));
#155950=CARTESIAN_POINT('Ctrl Pts',(1.30689331299994,15.2,-10.661088288));
#155951=CARTESIAN_POINT('Ctrl Pts',(1.30689331299994,11.6,-10.661088288));
#155952=CARTESIAN_POINT('Ctrl Pts',(1.30727475299994,15.2,-10.658611877));
#155953=CARTESIAN_POINT('Ctrl Pts',(1.30727475299994,11.6,-10.658611877));
#155954=CARTESIAN_POINT('Ctrl Pts',(1.30765313299994,15.2,-10.65614122));
#155955=CARTESIAN_POINT('Ctrl Pts',(1.30765313299994,11.6,-10.65614122));
#155956=CARTESIAN_POINT('Ctrl Pts',(1.30802845799994,15.2,-10.653676332));
#155957=CARTESIAN_POINT('Ctrl Pts',(1.30802845799994,11.6,-10.653676332));
#155958=CARTESIAN_POINT('Ctrl Pts',(1.30840073799994,15.2,-10.651217227));
#155959=CARTESIAN_POINT('Ctrl Pts',(1.30840073799994,11.6,-10.651217227));
#155960=CARTESIAN_POINT('Ctrl Pts',(1.30876997899994,15.2,-10.648763916));
#155961=CARTESIAN_POINT('Ctrl Pts',(1.30876997899994,11.6,-10.648763916));
#155962=CARTESIAN_POINT('Ctrl Pts',(1.30913618799994,15.2,-10.646316414));
#155963=CARTESIAN_POINT('Ctrl Pts',(1.30913618799994,11.6,-10.646316414));
#155964=CARTESIAN_POINT('Ctrl Pts',(1.30949937299994,15.2,-10.643874733));
#155965=CARTESIAN_POINT('Ctrl Pts',(1.30949937299994,11.6,-10.643874733));
#155966=CARTESIAN_POINT('Ctrl Pts',(1.30985954199994,15.2,-10.641438888));
#155967=CARTESIAN_POINT('Ctrl Pts',(1.30985954199994,11.6,-10.641438888));
#155968=CARTESIAN_POINT('Ctrl Pts',(1.31021670199994,15.2,-10.639008891));
#155969=CARTESIAN_POINT('Ctrl Pts',(1.31021670199994,11.6,-10.639008891));
#155970=CARTESIAN_POINT('Ctrl Pts',(1.31057086099994,15.2,-10.636584756));
#155971=CARTESIAN_POINT('Ctrl Pts',(1.31057086099994,11.6,-10.636584756));
#155972=CARTESIAN_POINT('Ctrl Pts',(1.31092202599994,15.2,-10.634166498));
#155973=CARTESIAN_POINT('Ctrl Pts',(1.31092202599994,11.6,-10.634166498));
#155974=CARTESIAN_POINT('Ctrl Pts',(1.31127020599994,15.2,-10.631754128));
#155975=CARTESIAN_POINT('Ctrl Pts',(1.31127020599994,11.6,-10.631754128));
#155976=CARTESIAN_POINT('Ctrl Pts',(1.31161540699994,15.2,-10.629347661));
#155977=CARTESIAN_POINT('Ctrl Pts',(1.31161540699994,11.6,-10.629347661));
#155978=CARTESIAN_POINT('Ctrl Pts',(1.31195763899994,15.2,-10.62694711));
#155979=CARTESIAN_POINT('Ctrl Pts',(1.31195763899994,11.6,-10.62694711));
#155980=CARTESIAN_POINT('Ctrl Pts',(1.31229690599994,15.2,-10.62455249));
#155981=CARTESIAN_POINT('Ctrl Pts',(1.31229690599994,11.6,-10.62455249));
#155982=CARTESIAN_POINT('Ctrl Pts',(1.31263321999994,15.2,-10.622163812));
#155983=CARTESIAN_POINT('Ctrl Pts',(1.31263321999994,11.6,-10.622163812));
#155984=CARTESIAN_POINT('Ctrl Pts',(1.31296658599994,15.2,-10.619781092));
#155985=CARTESIAN_POINT('Ctrl Pts',(1.31296658599994,11.6,-10.619781092));
#155986=CARTESIAN_POINT('Ctrl Pts',(1.31329701299994,15.2,-10.617404343));
#155987=CARTESIAN_POINT('Ctrl Pts',(1.31329701299994,11.6,-10.617404343));
#155988=CARTESIAN_POINT('Ctrl Pts',(1.31362450899994,15.2,-10.615033578));
#155989=CARTESIAN_POINT('Ctrl Pts',(1.31362450899994,11.6,-10.615033578));
#155990=CARTESIAN_POINT('Ctrl Pts',(1.31394908099994,15.2,-10.612668813));
#155991=CARTESIAN_POINT('Ctrl Pts',(1.31394908099994,11.6,-10.612668813));
#155992=CARTESIAN_POINT('Ctrl Pts',(1.31427073799994,15.2,-10.61031006));
#155993=CARTESIAN_POINT('Ctrl Pts',(1.31427073799994,11.6,-10.61031006));
#155994=CARTESIAN_POINT('Ctrl Pts',(1.31458948699994,15.2,-10.607957333));
#155995=CARTESIAN_POINT('Ctrl Pts',(1.31458948699994,11.6,-10.607957333));
#155996=CARTESIAN_POINT('Ctrl Pts',(1.31490533699994,15.2,-10.605610646));
#155997=CARTESIAN_POINT('Ctrl Pts',(1.31490533699994,11.6,-10.605610646));
#155998=CARTESIAN_POINT('Ctrl Pts',(1.31521829599994,15.2,-10.603270013));
#155999=CARTESIAN_POINT('Ctrl Pts',(1.31521829599994,11.6,-10.603270013));
#156000=CARTESIAN_POINT('Ctrl Pts',(1.31552837099994,15.2,-10.600935449));
#156001=CARTESIAN_POINT('Ctrl Pts',(1.31552837099994,11.6,-10.600935449));
#156002=CARTESIAN_POINT('Ctrl Pts',(1.31583557099994,15.2,-10.598606966));
#156003=CARTESIAN_POINT('Ctrl Pts',(1.31583557099994,11.6,-10.598606966));
#156004=CARTESIAN_POINT('Ctrl Pts',(1.31613990399994,15.2,-10.59628458));
#156005=CARTESIAN_POINT('Ctrl Pts',(1.31613990399994,11.6,-10.59628458));
#156006=CARTESIAN_POINT('Ctrl Pts',(1.31644137799994,15.2,-10.593968305));
#156007=CARTESIAN_POINT('Ctrl Pts',(1.31644137799994,11.6,-10.593968305));
#156008=CARTESIAN_POINT('Ctrl Pts',(1.31674000099994,15.2,-10.591658153));
#156009=CARTESIAN_POINT('Ctrl Pts',(1.31674000099994,11.6,-10.591658153));
#156010=CARTESIAN_POINT('Ctrl Pts',(1.31703578199994,15.2,-10.58935414));
#156011=CARTESIAN_POINT('Ctrl Pts',(1.31703578199994,11.6,-10.58935414));
#156012=CARTESIAN_POINT('Ctrl Pts',(1.31732872999994,15.2,-10.58705628));
#156013=CARTESIAN_POINT('Ctrl Pts',(1.31732872999994,11.6,-10.58705628));
#156014=CARTESIAN_POINT('Ctrl Pts',(1.31761885099994,15.2,-10.584764587));
#156015=CARTESIAN_POINT('Ctrl Pts',(1.31761885099994,11.6,-10.584764587));
#156016=CARTESIAN_POINT('Ctrl Pts',(1.31790615399994,15.2,-10.582479074));
#156017=CARTESIAN_POINT('Ctrl Pts',(1.31790615399994,11.6,-10.582479074));
#156018=CARTESIAN_POINT('Ctrl Pts',(1.31819064899994,15.2,-10.580199758));
#156019=CARTESIAN_POINT('Ctrl Pts',(1.31819064899994,11.6,-10.580199758));
#156020=CARTESIAN_POINT('Ctrl Pts',(1.31847234299994,15.2,-10.577926652));
#156021=CARTESIAN_POINT('Ctrl Pts',(1.31847234299994,11.6,-10.577926652));
#156022=CARTESIAN_POINT('Ctrl Pts',(1.31875124399994,15.2,-10.575659769));
#156023=CARTESIAN_POINT('Ctrl Pts',(1.31875124399994,11.6,-10.575659769));
#156024=CARTESIAN_POINT('Ctrl Pts',(1.31902736199994,15.2,-10.573399125));
#156025=CARTESIAN_POINT('Ctrl Pts',(1.31902736199994,11.6,-10.573399125));
#156026=CARTESIAN_POINT('Ctrl Pts',(1.31930070599994,15.2,-10.571144734));
#156027=CARTESIAN_POINT('Ctrl Pts',(1.31930070599994,11.6,-10.571144734));
#156028=CARTESIAN_POINT('Ctrl Pts',(1.31957128199994,15.2,-10.56889661));
#156029=CARTESIAN_POINT('Ctrl Pts',(1.31957128199994,11.6,-10.56889661));
#156030=CARTESIAN_POINT('Ctrl Pts',(1.31983910099994,15.2,-10.566654769));
#156031=CARTESIAN_POINT('Ctrl Pts',(1.31983910099994,11.6,-10.566654769));
#156032=CARTESIAN_POINT('Ctrl Pts',(1.32010416999994,15.2,-10.564419224));
#156033=CARTESIAN_POINT('Ctrl Pts',(1.32010416999994,11.6,-10.564419224));
#156034=CARTESIAN_POINT('Ctrl Pts',(1.32036649799994,15.2,-10.562189991));
#156035=CARTESIAN_POINT('Ctrl Pts',(1.32036649799994,11.6,-10.562189991));
#156036=CARTESIAN_POINT('Ctrl Pts',(1.32062609499994,15.2,-10.559967084));
#156037=CARTESIAN_POINT('Ctrl Pts',(1.32062609499994,11.6,-10.559967084));
#156038=CARTESIAN_POINT('Ctrl Pts',(1.32088296799994,15.2,-10.557750517));
#156039=CARTESIAN_POINT('Ctrl Pts',(1.32088296799994,11.6,-10.557750517));
#156040=CARTESIAN_POINT('Ctrl Pts',(1.32113712699994,15.2,-10.555540305));
#156041=CARTESIAN_POINT('Ctrl Pts',(1.32113712699994,11.6,-10.555540305));
#156042=CARTESIAN_POINT('Ctrl Pts',(1.32138857999994,15.2,-10.553336463));
#156043=CARTESIAN_POINT('Ctrl Pts',(1.32138857999994,11.6,-10.553336463));
#156044=CARTESIAN_POINT('Ctrl Pts',(1.32163733599994,15.2,-10.551139007));
#156045=CARTESIAN_POINT('Ctrl Pts',(1.32163733599994,11.6,-10.551139007));
#156046=CARTESIAN_POINT('Ctrl Pts',(1.32188340499994,15.2,-10.548947949));
#156047=CARTESIAN_POINT('Ctrl Pts',(1.32188340499994,11.6,-10.548947949));
#156048=CARTESIAN_POINT('Ctrl Pts',(1.32212679399994,15.2,-10.546763306));
#156049=CARTESIAN_POINT('Ctrl Pts',(1.32212679399994,11.6,-10.546763306));
#156050=CARTESIAN_POINT('Ctrl Pts',(1.32236751399994,15.2,-10.544585093));
#156051=CARTESIAN_POINT('Ctrl Pts',(1.32236751399994,11.6,-10.544585093));
#156052=CARTESIAN_POINT('Ctrl Pts',(1.32260557299994,15.2,-10.542413324));
#156053=CARTESIAN_POINT('Ctrl Pts',(1.32260557299994,11.6,-10.542413324));
#156054=CARTESIAN_POINT('Ctrl Pts',(1.32284097899994,15.2,-10.540248014));
#156055=CARTESIAN_POINT('Ctrl Pts',(1.32284097899994,11.6,-10.540248014));
#156056=CARTESIAN_POINT('Ctrl Pts',(1.32307374299994,15.2,-10.53808918));
#156057=CARTESIAN_POINT('Ctrl Pts',(1.32307374299994,11.6,-10.53808918));
#156058=CARTESIAN_POINT('Ctrl Pts',(1.32330387399994,15.2,-10.535936834));
#156059=CARTESIAN_POINT('Ctrl Pts',(1.32330387399994,11.6,-10.535936834));
#156060=CARTESIAN_POINT('Ctrl Pts',(1.32353137899994,15.2,-10.533790993));
#156061=CARTESIAN_POINT('Ctrl Pts',(1.32353137899994,11.6,-10.533790993));
#156062=CARTESIAN_POINT('Ctrl Pts',(1.32375626899994,15.2,-10.531651672));
#156063=CARTESIAN_POINT('Ctrl Pts',(1.32375626899994,11.6,-10.531651672));
#156064=CARTESIAN_POINT('Ctrl Pts',(1.32397855299994,15.2,-10.529518885));
#156065=CARTESIAN_POINT('Ctrl Pts',(1.32397855299994,11.6,-10.529518885));
#156066=CARTESIAN_POINT('Ctrl Pts',(1.32419823999994,15.2,-10.52739265));
#156067=CARTESIAN_POINT('Ctrl Pts',(1.32419823999994,11.6,-10.52739265));
#156068=CARTESIAN_POINT('Ctrl Pts',(1.32441533999994,15.2,-10.52527298));
#156069=CARTESIAN_POINT('Ctrl Pts',(1.32441533999994,11.6,-10.52527298));
#156070=CARTESIAN_POINT('Ctrl Pts',(1.32462986099994,15.2,-10.523159891));
#156071=CARTESIAN_POINT('Ctrl Pts',(1.32462986099994,11.6,-10.523159891));
#156072=CARTESIAN_POINT('Ctrl Pts',(1.32484181499994,15.2,-10.521053397));
#156073=CARTESIAN_POINT('Ctrl Pts',(1.32484181499994,11.6,-10.521053397));
#156074=CARTESIAN_POINT('Ctrl Pts',(1.32505120699994,15.2,-10.518953515));
#156075=CARTESIAN_POINT('Ctrl Pts',(1.32505120699994,11.6,-10.518953515));
#156076=CARTESIAN_POINT('Ctrl Pts',(1.32525805199994,15.2,-10.516860261));
#156077=CARTESIAN_POINT('Ctrl Pts',(1.32525805199994,11.6,-10.516860261));
#156078=CARTESIAN_POINT('Ctrl Pts',(1.32546235399994,15.2,-10.514773649));
#156079=CARTESIAN_POINT('Ctrl Pts',(1.32546235399994,11.6,-10.514773649));
#156080=CARTESIAN_POINT('Ctrl Pts',(1.32566412699994,15.2,-10.512693695));
#156081=CARTESIAN_POINT('Ctrl Pts',(1.32566412699994,11.6,-10.512693695));
#156082=CARTESIAN_POINT('Ctrl Pts',(1.32586337699994,15.2,-10.510620415));
#156083=CARTESIAN_POINT('Ctrl Pts',(1.32586337699994,11.6,-10.510620415));
#156084=CARTESIAN_POINT('Ctrl Pts',(1.32606011699994,15.2,-10.508553825));
#156085=CARTESIAN_POINT('Ctrl Pts',(1.32606011699994,11.6,-10.508553825));
#156086=CARTESIAN_POINT('Ctrl Pts',(1.32625435399994,15.2,-10.506493939));
#156087=CARTESIAN_POINT('Ctrl Pts',(1.32625435399994,11.6,-10.506493939));
#156088=CARTESIAN_POINT('Ctrl Pts',(1.32644609999994,15.2,-10.504440774));
#156089=CARTESIAN_POINT('Ctrl Pts',(1.32644609999994,11.6,-10.504440774));
#156090=CARTESIAN_POINT('Ctrl Pts',(1.32663536199994,15.2,-10.502394346));
#156091=CARTESIAN_POINT('Ctrl Pts',(1.32663536199994,11.6,-10.502394346));
#156092=CARTESIAN_POINT('Ctrl Pts',(1.32682215299994,15.2,-10.500354671));
#156093=CARTESIAN_POINT('Ctrl Pts',(1.32682215299994,11.6,-10.500354671));
#156094=CARTESIAN_POINT('Ctrl Pts',(1.32700648099994,15.2,-10.498321763));
#156095=CARTESIAN_POINT('Ctrl Pts',(1.32700648099994,11.6,-10.498321763));
#156096=CARTESIAN_POINT('Ctrl Pts',(1.32718835599994,15.2,-10.49629564));
#156097=CARTESIAN_POINT('Ctrl Pts',(1.32718835599994,11.6,-10.49629564));
#156098=CARTESIAN_POINT('Ctrl Pts',(1.32736778799994,15.2,-10.494276317));
#156099=CARTESIAN_POINT('Ctrl Pts',(1.32736778799994,11.6,-10.494276317));
#156100=CARTESIAN_POINT('Ctrl Pts',(1.32754478699994,15.2,-10.49226381));
#156101=CARTESIAN_POINT('Ctrl Pts',(1.32754478699994,11.6,-10.49226381));
#156102=CARTESIAN_POINT('Ctrl Pts',(1.32771936299994,15.2,-10.490258135));
#156103=CARTESIAN_POINT('Ctrl Pts',(1.32771936299994,11.6,-10.490258135));
#156104=CARTESIAN_POINT('Ctrl Pts',(1.32789152599994,15.2,-10.488259308));
#156105=CARTESIAN_POINT('Ctrl Pts',(1.32789152599994,11.6,-10.488259308));
#156106=CARTESIAN_POINT('Ctrl Pts',(1.32806128599994,15.2,-10.486267346));
#156107=CARTESIAN_POINT('Ctrl Pts',(1.32806128599994,11.6,-10.486267346));
#156108=CARTESIAN_POINT('Ctrl Pts',(1.32822865399994,15.2,-10.484282264));
#156109=CARTESIAN_POINT('Ctrl Pts',(1.32822865399994,11.6,-10.484282264));
#156110=CARTESIAN_POINT('Ctrl Pts',(1.32839363899994,15.2,-10.48230408));
#156111=CARTESIAN_POINT('Ctrl Pts',(1.32839363899994,11.6,-10.48230408));
#156112=CARTESIAN_POINT('Ctrl Pts',(1.32855625199994,15.2,-10.480332808));
#156113=CARTESIAN_POINT('Ctrl Pts',(1.32855625199994,11.6,-10.480332808));
#156114=CARTESIAN_POINT('Ctrl Pts',(1.32871650299994,15.2,-10.478368465));
#156115=CARTESIAN_POINT('Ctrl Pts',(1.32871650299994,11.6,-10.478368465));
#156116=CARTESIAN_POINT('Ctrl Pts',(1.32887440299994,15.2,-10.476411069));
#156117=CARTESIAN_POINT('Ctrl Pts',(1.32887440299994,11.6,-10.476411069));
#156118=CARTESIAN_POINT('Ctrl Pts',(1.32902996199994,15.2,-10.474460635));
#156119=CARTESIAN_POINT('Ctrl Pts',(1.32902996199994,11.6,-10.474460635));
#156120=CARTESIAN_POINT('Ctrl Pts',(1.32918318899994,15.2,-10.47251718));
#156121=CARTESIAN_POINT('Ctrl Pts',(1.32918318899994,11.6,-10.47251718));
#156122=CARTESIAN_POINT('Ctrl Pts',(1.32933409699994,15.2,-10.47058072));
#156123=CARTESIAN_POINT('Ctrl Pts',(1.32933409699994,11.6,-10.47058072));
#156124=CARTESIAN_POINT('Ctrl Pts',(1.32948269399994,15.2,-10.468651272));
#156125=CARTESIAN_POINT('Ctrl Pts',(1.32948269399994,11.6,-10.468651272));
#156126=CARTESIAN_POINT('Ctrl Pts',(1.32962899299994,15.2,-10.466728852));
#156127=CARTESIAN_POINT('Ctrl Pts',(1.32962899299994,11.6,-10.466728852));
#156128=CARTESIAN_POINT('Ctrl Pts',(1.32977300299994,15.2,-10.464813477));
#156129=CARTESIAN_POINT('Ctrl Pts',(1.32977300299994,11.6,-10.464813477));
#156130=CARTESIAN_POINT('Ctrl Pts',(1.32991473499994,15.2,-10.462905165));
#156131=CARTESIAN_POINT('Ctrl Pts',(1.32991473499994,11.6,-10.462905165));
#156132=CARTESIAN_POINT('Ctrl Pts',(1.33005419999994,15.2,-10.461003932));
#156133=CARTESIAN_POINT('Ctrl Pts',(1.33005419999994,11.6,-10.461003932));
#156134=CARTESIAN_POINT('Ctrl Pts',(1.33019140799994,15.2,-10.459109793));
#156135=CARTESIAN_POINT('Ctrl Pts',(1.33019140799994,11.6,-10.459109793));
#156136=CARTESIAN_POINT('Ctrl Pts',(1.33032637099994,15.2,-10.457222766));
#156137=CARTESIAN_POINT('Ctrl Pts',(1.33032637099994,11.6,-10.457222766));
#156138=CARTESIAN_POINT('Ctrl Pts',(1.33045909799994,15.2,-10.45534287));
#156139=CARTESIAN_POINT('Ctrl Pts',(1.33045909799994,11.6,-10.45534287));
#156140=CARTESIAN_POINT('Ctrl Pts',(1.33058960299994,15.2,-10.453470121));
#156141=CARTESIAN_POINT('Ctrl Pts',(1.33058960299994,11.6,-10.453470121));
#156142=CARTESIAN_POINT('Ctrl Pts',(1.33071789299994,15.2,-10.451604534));
#156143=CARTESIAN_POINT('Ctrl Pts',(1.33071789299994,11.6,-10.451604534));
#156144=CARTESIAN_POINT('Ctrl Pts',(1.33084398199994,15.2,-10.449746128));
#156145=CARTESIAN_POINT('Ctrl Pts',(1.33084398199994,11.6,-10.449746128));
#156146=CARTESIAN_POINT('Ctrl Pts',(1.33096787999994,15.2,-10.447894919));
#156147=CARTESIAN_POINT('Ctrl Pts',(1.33096787999994,11.6,-10.447894919));
#156148=CARTESIAN_POINT('Ctrl Pts',(1.33108959799994,15.2,-10.446050926));
#156149=CARTESIAN_POINT('Ctrl Pts',(1.33108959799994,11.6,-10.446050926));
#156150=CARTESIAN_POINT('Ctrl Pts',(1.33120914699994,15.2,-10.444214164));
#156151=CARTESIAN_POINT('Ctrl Pts',(1.33120914699994,11.6,-10.444214164));
#156152=CARTESIAN_POINT('Ctrl Pts',(1.33132653899994,15.2,-10.442384652));
#156153=CARTESIAN_POINT('Ctrl Pts',(1.33132653899994,11.6,-10.442384652));
#156154=CARTESIAN_POINT('Ctrl Pts',(1.33144178299994,15.2,-10.440562407));
#156155=CARTESIAN_POINT('Ctrl Pts',(1.33144178299994,11.6,-10.440562407));
#156156=CARTESIAN_POINT('Ctrl Pts',(1.33155489399994,15.2,-10.438747447));
#156157=CARTESIAN_POINT('Ctrl Pts',(1.33155489399994,11.6,-10.438747447));
#156158=CARTESIAN_POINT('Ctrl Pts',(1.33166587999994,15.2,-10.436939788));
#156159=CARTESIAN_POINT('Ctrl Pts',(1.33166587999994,11.6,-10.436939788));
#156160=CARTESIAN_POINT('Ctrl Pts',(1.33177475499994,15.2,-10.435139448));
#156161=CARTESIAN_POINT('Ctrl Pts',(1.33177475499994,11.6,-10.435139448));
#156162=CARTESIAN_POINT('Ctrl Pts',(1.33188152799994,15.2,-10.433346446));
#156163=CARTESIAN_POINT('Ctrl Pts',(1.33188152799994,11.6,-10.433346446));
#156164=CARTESIAN_POINT('Ctrl Pts',(1.33198621199994,15.2,-10.431560797));
#156165=CARTESIAN_POINT('Ctrl Pts',(1.33198621199994,11.6,-10.431560797));
#156166=CARTESIAN_POINT('Ctrl Pts',(1.33208881899994,15.2,-10.429782521));
#156167=CARTESIAN_POINT('Ctrl Pts',(1.33208881899994,11.6,-10.429782521));
#156168=CARTESIAN_POINT('Ctrl Pts',(1.33218935899994,15.2,-10.428011636));
#156169=CARTESIAN_POINT('Ctrl Pts',(1.33218935899994,11.6,-10.428011636));
#156170=CARTESIAN_POINT('Ctrl Pts',(1.33228784499994,15.2,-10.426248158));
#156171=CARTESIAN_POINT('Ctrl Pts',(1.33228784499994,11.6,-10.426248158));
#156172=CARTESIAN_POINT('Ctrl Pts',(1.33238428799994,15.2,-10.424492106));
#156173=CARTESIAN_POINT('Ctrl Pts',(1.33238428799994,11.6,-10.424492106));
#156174=CARTESIAN_POINT('Ctrl Pts',(1.33247869999994,15.2,-10.422743497));
#156175=CARTESIAN_POINT('Ctrl Pts',(1.33247869999994,11.6,-10.422743497));
#156176=CARTESIAN_POINT('Ctrl Pts',(1.33257109199994,15.2,-10.421002351));
#156177=CARTESIAN_POINT('Ctrl Pts',(1.33257109199994,11.6,-10.421002351));
#156178=CARTESIAN_POINT('Ctrl Pts',(1.33266147799994,15.2,-10.419268684));
#156179=CARTESIAN_POINT('Ctrl Pts',(1.33266147799994,11.6,-10.419268684));
#156180=CARTESIAN_POINT('Ctrl Pts',(1.33274986699994,15.2,-10.417542515));
#156181=CARTESIAN_POINT('Ctrl Pts',(1.33274986699994,11.6,-10.417542515));
#156182=CARTESIAN_POINT('Ctrl Pts',(1.33283627399994,15.2,-10.415823863));
#156183=CARTESIAN_POINT('Ctrl Pts',(1.33283627399994,11.6,-10.415823863));
#156184=CARTESIAN_POINT('Ctrl Pts',(1.33292070899994,15.2,-10.414112744));
#156185=CARTESIAN_POINT('Ctrl Pts',(1.33292070899994,11.6,-10.414112744));
#156186=CARTESIAN_POINT('Ctrl Pts',(1.33300318399994,15.2,-10.412409178));
#156187=CARTESIAN_POINT('Ctrl Pts',(1.33300318399994,11.6,-10.412409178));
#156188=CARTESIAN_POINT('Ctrl Pts',(1.33308371299994,15.2,-10.410713184));
#156189=CARTESIAN_POINT('Ctrl Pts',(1.33308371299994,11.6,-10.410713184));
#156190=CARTESIAN_POINT('Ctrl Pts',(1.33316230599994,15.2,-10.409024778));
#156191=CARTESIAN_POINT('Ctrl Pts',(1.33316230599994,11.6,-10.409024778));
#156192=CARTESIAN_POINT('Ctrl Pts',(1.33323897699994,15.2,-10.40734398));
#156193=CARTESIAN_POINT('Ctrl Pts',(1.33323897699994,11.6,-10.40734398));
#156194=CARTESIAN_POINT('Ctrl Pts',(1.33331373699994,15.2,-10.405670811));
#156195=CARTESIAN_POINT('Ctrl Pts',(1.33331373699994,11.6,-10.405670811));
#156196=CARTESIAN_POINT('Ctrl Pts',(1.33338659999994,15.2,-10.404005285));
#156197=CARTESIAN_POINT('Ctrl Pts',(1.33338659999994,11.6,-10.404005285));
#156198=CARTESIAN_POINT('Ctrl Pts',(1.33345757699994,15.2,-10.402347423));
#156199=CARTESIAN_POINT('Ctrl Pts',(1.33345757699994,11.6,-10.402347423));
#156200=CARTESIAN_POINT('Ctrl Pts',(1.33352668099994,15.2,-10.400697244));
#156201=CARTESIAN_POINT('Ctrl Pts',(1.33352668099994,11.6,-10.400697244));
#156202=CARTESIAN_POINT('Ctrl Pts',(1.33359392399994,15.2,-10.399054766));
#156203=CARTESIAN_POINT('Ctrl Pts',(1.33359392399994,11.6,-10.399054766));
#156204=CARTESIAN_POINT('Ctrl Pts',(1.33365931999994,15.2,-10.397420008));
#156205=CARTESIAN_POINT('Ctrl Pts',(1.33365931999994,11.6,-10.397420008));
#156206=CARTESIAN_POINT('Ctrl Pts',(1.33372287999994,15.2,-10.39579299));
#156207=CARTESIAN_POINT('Ctrl Pts',(1.33372287999994,11.6,-10.39579299));
#156208=CARTESIAN_POINT('Ctrl Pts',(1.33378461799994,15.2,-10.39417373));
#156209=CARTESIAN_POINT('Ctrl Pts',(1.33378461799994,11.6,-10.39417373));
#156210=CARTESIAN_POINT('Ctrl Pts',(1.33384454499994,15.2,-10.392562248));
#156211=CARTESIAN_POINT('Ctrl Pts',(1.33384454499994,11.6,-10.392562248));
#156212=CARTESIAN_POINT('Ctrl Pts',(1.33390267699994,15.2,-10.39095856));
#156213=CARTESIAN_POINT('Ctrl Pts',(1.33390267699994,11.6,-10.39095856));
#156214=CARTESIAN_POINT('Ctrl Pts',(1.33395902399994,15.2,-10.38936269));
#156215=CARTESIAN_POINT('Ctrl Pts',(1.33395902399994,11.6,-10.38936269));
#156216=CARTESIAN_POINT('Ctrl Pts',(1.33401359999994,15.2,-10.387774654));
#156217=CARTESIAN_POINT('Ctrl Pts',(1.33401359999994,11.6,-10.387774654));
#156218=CARTESIAN_POINT('Ctrl Pts',(1.33406641799994,15.2,-10.386194473));
#156219=CARTESIAN_POINT('Ctrl Pts',(1.33406641799994,11.6,-10.386194473));
#156220=CARTESIAN_POINT('Ctrl Pts',(1.33411749199994,15.2,-10.384622165));
#156221=CARTESIAN_POINT('Ctrl Pts',(1.33411749199994,11.6,-10.384622165));
#156222=CARTESIAN_POINT('Ctrl Pts',(1.33416683399994,15.2,-10.383057751));
#156223=CARTESIAN_POINT('Ctrl Pts',(1.33416683399994,11.6,-10.383057751));
#156224=CARTESIAN_POINT('Ctrl Pts',(1.33421445699994,15.2,-10.381501249));
#156225=CARTESIAN_POINT('Ctrl Pts',(1.33421445699994,11.6,-10.381501249));
#156226=CARTESIAN_POINT('Ctrl Pts',(1.33426037499994,15.2,-10.379952679));
#156227=CARTESIAN_POINT('Ctrl Pts',(1.33426037499994,11.6,-10.379952679));
#156228=CARTESIAN_POINT('Ctrl Pts',(1.33430460199994,15.2,-10.378412062));
#156229=CARTESIAN_POINT('Ctrl Pts',(1.33430460199994,11.6,-10.378412062));
#156230=CARTESIAN_POINT('Ctrl Pts',(1.33434714999994,15.2,-10.376879417));
#156231=CARTESIAN_POINT('Ctrl Pts',(1.33434714999994,11.6,-10.376879417));
#156232=CARTESIAN_POINT('Ctrl Pts',(1.33438803299994,15.2,-10.375354763));
#156233=CARTESIAN_POINT('Ctrl Pts',(1.33438803299994,11.6,-10.375354763));
#156234=CARTESIAN_POINT('Ctrl Pts',(1.33442726499994,15.2,-10.373838121));
#156235=CARTESIAN_POINT('Ctrl Pts',(1.33442726499994,11.6,-10.373838121));
#156236=CARTESIAN_POINT('Ctrl Pts',(1.33446485899994,15.2,-10.37232951));
#156237=CARTESIAN_POINT('Ctrl Pts',(1.33446485899994,11.6,-10.37232951));
#156238=CARTESIAN_POINT('Ctrl Pts',(1.33450082899994,15.2,-10.370828951));
#156239=CARTESIAN_POINT('Ctrl Pts',(1.33450082899994,11.6,-10.370828951));
#156240=CARTESIAN_POINT('Ctrl Pts',(1.33453518799994,15.2,-10.369336464));
#156241=CARTESIAN_POINT('Ctrl Pts',(1.33453518799994,11.6,-10.369336464));
#156242=CARTESIAN_POINT('Ctrl Pts',(1.33456795099994,15.2,-10.367852069));
#156243=CARTESIAN_POINT('Ctrl Pts',(1.33456795099994,11.6,-10.367852069));
#156244=CARTESIAN_POINT('Ctrl Pts',(1.33459913199994,15.2,-10.366375787));
#156245=CARTESIAN_POINT('Ctrl Pts',(1.33459913199994,11.6,-10.366375787));
#156246=CARTESIAN_POINT('Ctrl Pts',(1.33462874399994,15.2,-10.364907637));
#156247=CARTESIAN_POINT('Ctrl Pts',(1.33462874399994,11.6,-10.364907637));
#156248=CARTESIAN_POINT('Ctrl Pts',(1.33465680099994,15.2,-10.363447639));
#156249=CARTESIAN_POINT('Ctrl Pts',(1.33465680099994,11.6,-10.363447639));
#156250=CARTESIAN_POINT('Ctrl Pts',(1.33468331799994,15.2,-10.361995816));
#156251=CARTESIAN_POINT('Ctrl Pts',(1.33468331799994,11.6,-10.361995816));
#156252=CARTESIAN_POINT('Ctrl Pts',(1.33470830799994,15.2,-10.360552186));
#156253=CARTESIAN_POINT('Ctrl Pts',(1.33470830799994,11.6,-10.360552186));
#156254=CARTESIAN_POINT('Ctrl Pts',(1.33473178599994,15.2,-10.359116771));
#156255=CARTESIAN_POINT('Ctrl Pts',(1.33473178599994,11.6,-10.359116771));
#156256=CARTESIAN_POINT('Ctrl Pts',(1.33475376599994,15.2,-10.357689593));
#156257=CARTESIAN_POINT('Ctrl Pts',(1.33475376599994,11.6,-10.357689593));
#156258=CARTESIAN_POINT('Ctrl Pts',(1.33477426199994,15.2,-10.356270671));
#156259=CARTESIAN_POINT('Ctrl Pts',(1.33477426199994,11.6,-10.356270671));
#156260=CARTESIAN_POINT('Ctrl Pts',(1.33479328899994,15.2,-10.354860026));
#156261=CARTESIAN_POINT('Ctrl Pts',(1.33479328899994,11.6,-10.354860026));
#156262=CARTESIAN_POINT('Ctrl Pts',(1.33481086199994,15.2,-10.353457679));
#156263=CARTESIAN_POINT('Ctrl Pts',(1.33481086199994,11.6,-10.353457679));
#156264=CARTESIAN_POINT('Ctrl Pts',(1.33482699499994,15.2,-10.352063652));
#156265=CARTESIAN_POINT('Ctrl Pts',(1.33482699499994,11.6,-10.352063652));
#156266=CARTESIAN_POINT('Ctrl Pts',(1.33484170199994,15.2,-10.350677965));
#156267=CARTESIAN_POINT('Ctrl Pts',(1.33484170199994,11.6,-10.350677965));
#156268=CARTESIAN_POINT('Ctrl Pts',(1.33485499899994,15.2,-10.34930064));
#156269=CARTESIAN_POINT('Ctrl Pts',(1.33485499899994,11.6,-10.34930064));
#156270=CARTESIAN_POINT('Ctrl Pts',(1.33486689899994,15.2,-10.347931697));
#156271=CARTESIAN_POINT('Ctrl Pts',(1.33486689899994,11.6,-10.347931697));
#156272=CARTESIAN_POINT('Ctrl Pts',(1.33487741999994,15.2,-10.34657116));
#156273=CARTESIAN_POINT('Ctrl Pts',(1.33487741999994,11.6,-10.34657116));
#156274=CARTESIAN_POINT('Ctrl Pts',(1.33488657299994,15.2,-10.345219049));
#156275=CARTESIAN_POINT('Ctrl Pts',(1.33488657299994,11.6,-10.345219049));
#156276=CARTESIAN_POINT('Ctrl Pts',(1.33489437599994,15.2,-10.343875384));
#156277=CARTESIAN_POINT('Ctrl Pts',(1.33489437599994,11.6,-10.343875384));
#156278=CARTESIAN_POINT('Ctrl Pts',(1.33490084299994,15.2,-10.342540189));
#156279=CARTESIAN_POINT('Ctrl Pts',(1.33490084299994,11.6,-10.342540189));
#156280=CARTESIAN_POINT('Ctrl Pts',(1.33490598899994,15.2,-10.341213485));
#156281=CARTESIAN_POINT('Ctrl Pts',(1.33490598899994,11.6,-10.341213485));
#156282=CARTESIAN_POINT('Ctrl Pts',(1.33490982999994,15.2,-10.339895294));
#156283=CARTESIAN_POINT('Ctrl Pts',(1.33490982999994,11.6,-10.339895294));
#156284=CARTESIAN_POINT('Ctrl Pts',(1.33491238099994,15.2,-10.338585637));
#156285=CARTESIAN_POINT('Ctrl Pts',(1.33491238099994,11.6,-10.338585637));
#156286=CARTESIAN_POINT('Ctrl Pts',(1.33491365599994,15.2,-10.337284537));
#156287=CARTESIAN_POINT('Ctrl Pts',(1.33491365599994,11.6,-10.337284537));
#156288=CARTESIAN_POINT('Ctrl Pts',(1.33491367299994,15.2,-10.335992016));
#156289=CARTESIAN_POINT('Ctrl Pts',(1.33491367299994,11.6,-10.335992016));
#156290=CARTESIAN_POINT('Ctrl Pts',(1.33491244599994,15.2,-10.334708096));
#156291=CARTESIAN_POINT('Ctrl Pts',(1.33491244599994,11.6,-10.334708096));
#156292=CARTESIAN_POINT('Ctrl Pts',(1.33490999099994,15.2,-10.333432799));
#156293=CARTESIAN_POINT('Ctrl Pts',(1.33490999099994,11.6,-10.333432799));
#156294=CARTESIAN_POINT('Ctrl Pts',(1.33490632299994,15.2,-10.332166147));
#156295=CARTESIAN_POINT('Ctrl Pts',(1.33490632299994,11.6,-10.332166147));
#156296=CARTESIAN_POINT('Ctrl Pts',(1.33490145899994,15.2,-10.330908163));
#156297=CARTESIAN_POINT('Ctrl Pts',(1.33490145899994,11.6,-10.330908163));
#156298=CARTESIAN_POINT('Ctrl Pts',(1.33489541499994,15.2,-10.32965887));
#156299=CARTESIAN_POINT('Ctrl Pts',(1.33489541499994,11.6,-10.32965887));
#156300=CARTESIAN_POINT('Ctrl Pts',(1.33488820599994,15.2,-10.32841829));
#156301=CARTESIAN_POINT('Ctrl Pts',(1.33488820599994,11.6,-10.32841829));
#156302=CARTESIAN_POINT('Ctrl Pts',(1.33487984899994,15.2,-10.327186447));
#156303=CARTESIAN_POINT('Ctrl Pts',(1.33487984899994,11.6,-10.327186447));
#156304=CARTESIAN_POINT('Ctrl Pts',(1.33487035799994,15.2,-10.32596336));
#156305=CARTESIAN_POINT('Ctrl Pts',(1.33487035799994,11.6,-10.32596336));
#156306=CARTESIAN_POINT('Ctrl Pts',(1.33485975199994,15.2,-10.324749056));
#156307=CARTESIAN_POINT('Ctrl Pts',(1.33485975199994,11.6,-10.324749056));
#156308=CARTESIAN_POINT('Ctrl Pts',(1.33484804599994,15.2,-10.323543558));
#156309=CARTESIAN_POINT('Ctrl Pts',(1.33484804599994,11.6,-10.323543558));
#156310=CARTESIAN_POINT('Ctrl Pts',(1.33483525599994,15.2,-10.322346886));
#156311=CARTESIAN_POINT('Ctrl Pts',(1.33483525599994,11.6,-10.322346886));
#156312=CARTESIAN_POINT('Ctrl Pts',(1.33482139999994,15.2,-10.321159066));
#156313=CARTESIAN_POINT('Ctrl Pts',(1.33482139999994,11.6,-10.321159066));
#156314=CARTESIAN_POINT('Ctrl Pts',(1.33480649299994,15.2,-10.319980119));
#156315=CARTESIAN_POINT('Ctrl Pts',(1.33480649299994,11.6,-10.319980119));
#156316=CARTESIAN_POINT('Ctrl Pts',(1.33479055199994,15.2,-10.318810071));
#156317=CARTESIAN_POINT('Ctrl Pts',(1.33479055199994,11.6,-10.318810071));
#156318=CARTESIAN_POINT('Ctrl Pts',(1.33477359399994,15.2,-10.317648943));
#156319=CARTESIAN_POINT('Ctrl Pts',(1.33477359399994,11.6,-10.317648943));
#156320=CARTESIAN_POINT('Ctrl Pts',(1.33475563599994,15.2,-10.31649676));
#156321=CARTESIAN_POINT('Ctrl Pts',(1.33475563599994,11.6,-10.31649676));
#156322=CARTESIAN_POINT('Ctrl Pts',(1.33473669499994,15.2,-10.315353546));
#156323=CARTESIAN_POINT('Ctrl Pts',(1.33473669499994,11.6,-10.315353546));
#156324=CARTESIAN_POINT('Ctrl Pts',(1.33471678699994,15.2,-10.314219324));
#156325=CARTESIAN_POINT('Ctrl Pts',(1.33471678699994,11.6,-10.314219324));
#156326=CARTESIAN_POINT('Ctrl Pts',(1.33469592999994,15.2,-10.313094118));
#156327=CARTESIAN_POINT('Ctrl Pts',(1.33469592999994,11.6,-10.313094118));
#156328=CARTESIAN_POINT('Ctrl Pts',(1.33467414199994,15.2,-10.311977952));
#156329=CARTESIAN_POINT('Ctrl Pts',(1.33467414199994,11.6,-10.311977952));
#156330=CARTESIAN_POINT('Ctrl Pts',(1.33465143899994,15.2,-10.310870851));
#156331=CARTESIAN_POINT('Ctrl Pts',(1.33465143899994,11.6,-10.310870851));
#156332=CARTESIAN_POINT('Ctrl Pts',(1.33462783799994,15.2,-10.309772837));
#156333=CARTESIAN_POINT('Ctrl Pts',(1.33462783799994,11.6,-10.309772837));
#156334=CARTESIAN_POINT('Ctrl Pts',(1.33460335699994,15.2,-10.308683938));
#156335=CARTESIAN_POINT('Ctrl Pts',(1.33460335699994,11.6,-10.308683938));
#156336=CARTESIAN_POINT('Ctrl Pts',(1.33457801399994,15.2,-10.307604175));
#156337=CARTESIAN_POINT('Ctrl Pts',(1.33457801399994,11.6,-10.307604175));
#156338=CARTESIAN_POINT('Ctrl Pts',(1.33455182599994,15.2,-10.306533574));
#156339=CARTESIAN_POINT('Ctrl Pts',(1.33455182599994,11.6,-10.306533574));
#156340=CARTESIAN_POINT('Ctrl Pts',(1.33452481199994,15.2,-10.30547216));
#156341=CARTESIAN_POINT('Ctrl Pts',(1.33452481199994,11.6,-10.30547216));
#156342=CARTESIAN_POINT('Ctrl Pts',(1.33449698899994,15.2,-10.304419957));
#156343=CARTESIAN_POINT('Ctrl Pts',(1.33449698899994,11.6,-10.304419957));
#156344=CARTESIAN_POINT('Ctrl Pts',(1.33446837399994,15.2,-10.30337699));
#156345=CARTESIAN_POINT('Ctrl Pts',(1.33446837399994,11.6,-10.30337699));
#156346=CARTESIAN_POINT('Ctrl Pts',(1.33443898699994,15.2,-10.302343284));
#156347=CARTESIAN_POINT('Ctrl Pts',(1.33443898699994,11.6,-10.302343284));
#156348=CARTESIAN_POINT('Ctrl Pts',(1.33440884499994,15.2,-10.301318864));
#156349=CARTESIAN_POINT('Ctrl Pts',(1.33440884499994,11.6,-10.301318864));
#156350=CARTESIAN_POINT('Ctrl Pts',(1.33437796499994,15.2,-10.300303756));
#156351=CARTESIAN_POINT('Ctrl Pts',(1.33437796499994,11.6,-10.300303756));
#156352=CARTESIAN_POINT('Ctrl Pts',(1.33434636799994,15.2,-10.299297985));
#156353=CARTESIAN_POINT('Ctrl Pts',(1.33434636799994,11.6,-10.299297985));
#156354=CARTESIAN_POINT('Ctrl Pts',(1.33431407099994,15.2,-10.298301576));
#156355=CARTESIAN_POINT('Ctrl Pts',(1.33431407099994,11.6,-10.298301576));
#156356=CARTESIAN_POINT('Ctrl Pts',(1.33428109299994,15.2,-10.297314555));
#156357=CARTESIAN_POINT('Ctrl Pts',(1.33428109299994,11.6,-10.297314555));
#156358=CARTESIAN_POINT('Ctrl Pts',(1.33424745199994,15.2,-10.296336946));
#156359=CARTESIAN_POINT('Ctrl Pts',(1.33424745199994,11.6,-10.296336946));
#156360=CARTESIAN_POINT('Ctrl Pts',(1.33421316699994,15.2,-10.295368778));
#156361=CARTESIAN_POINT('Ctrl Pts',(1.33421316699994,11.6,-10.295368778));
#156362=CARTESIAN_POINT('Ctrl Pts',(1.33417825799994,15.2,-10.294410075));
#156363=CARTESIAN_POINT('Ctrl Pts',(1.33417825799994,11.6,-10.294410075));
#156364=CARTESIAN_POINT('Ctrl Pts',(1.33414274299994,15.2,-10.293460862));
#156365=CARTESIAN_POINT('Ctrl Pts',(1.33414274299994,11.6,-10.293460862));
#156366=CARTESIAN_POINT('Ctrl Pts',(1.33410663999994,15.2,-10.292521167));
#156367=CARTESIAN_POINT('Ctrl Pts',(1.33410663999994,11.6,-10.292521167));
#156368=CARTESIAN_POINT('Ctrl Pts',(1.33406996899994,15.2,-10.291591017));
#156369=CARTESIAN_POINT('Ctrl Pts',(1.33406996899994,11.6,-10.291591017));
#156370=CARTESIAN_POINT('Ctrl Pts',(1.33403296599994,15.2,-10.290675738));
#156371=CARTESIAN_POINT('Ctrl Pts',(1.33403296599994,11.6,-10.290675738));
#156372=CARTESIAN_POINT('Ctrl Pts',(1.33400298699994,15.2,-10.289952142));
#156373=CARTESIAN_POINT('Ctrl Pts',(1.33400298699994,11.6,-10.289952142));
#156374=CARTESIAN_POINT('Ctrl Pts',(1.33398033299994,15.2,-10.289415004));
#156375=CARTESIAN_POINT('Ctrl Pts',(1.33398033299994,11.6,-10.289415004));
#156376=CARTESIAN_POINT('Ctrl Pts',(1.33396520799994,15.2,-10.289060521));
#156377=CARTESIAN_POINT('Ctrl Pts',(1.33396520799994,11.6,-10.289060521));
#156378=CARTESIAN_POINT('Ctrl Pts',(1.33395773199994,15.2,-10.288886323));
#156379=CARTESIAN_POINT('Ctrl Pts',(1.33395773199994,11.6,-10.288886323));
#156380=CARTESIAN_POINT('',(1.33395773199994,12.2,-10.288886323));
#156381=CARTESIAN_POINT('',(1.33395773199994,15.2,-10.288886323));
#156382=CARTESIAN_POINT('',(1.33395773199994,12.2,-10.288886323));
#156383=CARTESIAN_POINT('Ctrl Pts',(1.09337742899994,12.2,-11.447904865));
#156384=CARTESIAN_POINT('Ctrl Pts',(1.09364566999994,12.2,-11.447188878));
#156385=CARTESIAN_POINT('Ctrl Pts',(1.09418172899994,12.2,-11.445757219));
#156386=CARTESIAN_POINT('Ctrl Pts',(1.09498454299994,12.2,-11.443610664));
#156387=CARTESIAN_POINT('Ctrl Pts',(1.09605241599994,12.2,-11.440750465));
#156388=CARTESIAN_POINT('Ctrl Pts',(1.09738301599994,12.2,-11.437178335));
#156389=CARTESIAN_POINT('Ctrl Pts',(1.09870937299994,12.2,-11.433609328));
#156390=CARTESIAN_POINT('Ctrl Pts',(1.10003148899994,12.2,-11.430043446));
#156391=CARTESIAN_POINT('Ctrl Pts',(1.10134936299994,12.2,-11.426480691));
#156392=CARTESIAN_POINT('Ctrl Pts',(1.10266299899994,12.2,-11.422921069));
#156393=CARTESIAN_POINT('Ctrl Pts',(1.10397239799994,12.2,-11.419364591));
#156394=CARTESIAN_POINT('Ctrl Pts',(1.10527756399994,12.2,-11.415811262));
#156395=CARTESIAN_POINT('Ctrl Pts',(1.10657849999994,12.2,-11.412261095));
#156396=CARTESIAN_POINT('Ctrl Pts',(1.10787520999994,12.2,-11.408714099));
#156397=CARTESIAN_POINT('Ctrl Pts',(1.10916769599994,12.2,-11.405170286));
#156398=CARTESIAN_POINT('Ctrl Pts',(1.11045596299994,12.2,-11.401629665));
#156399=CARTESIAN_POINT('Ctrl Pts',(1.11174001299994,12.2,-11.398092244));
#156400=CARTESIAN_POINT('Ctrl Pts',(1.11301984899994,12.2,-11.394558034));
#156401=CARTESIAN_POINT('Ctrl Pts',(1.11429547399994,12.2,-11.39102704));
#156402=CARTESIAN_POINT('Ctrl Pts',(1.11556688999994,12.2,-11.387499272));
#156403=CARTESIAN_POINT('Ctrl Pts',(1.11683409999994,12.2,-11.383974735));
#156404=CARTESIAN_POINT('Ctrl Pts',(1.11809710599994,12.2,-11.38045344));
#156405=CARTESIAN_POINT('Ctrl Pts',(1.11935591099994,12.2,-11.376935393));
#156406=CARTESIAN_POINT('Ctrl Pts',(1.12061051899994,12.2,-11.373420606));
#156407=CARTESIAN_POINT('Ctrl Pts',(1.12186093199994,12.2,-11.369909084));
#156408=CARTESIAN_POINT('Ctrl Pts',(1.12310715399994,12.2,-11.366400839));
#156409=CARTESIAN_POINT('Ctrl Pts',(1.12434918699994,12.2,-11.36289588));
#156410=CARTESIAN_POINT('Ctrl Pts',(1.12558703399994,12.2,-11.359394214));
#156411=CARTESIAN_POINT('Ctrl Pts',(1.12682069999994,12.2,-11.355895851));
#156412=CARTESIAN_POINT('Ctrl Pts',(1.12805018499994,12.2,-11.3524008));
#156413=CARTESIAN_POINT('Ctrl Pts',(1.12927549399994,12.2,-11.348909068));
#156414=CARTESIAN_POINT('Ctrl Pts',(1.13049662999994,12.2,-11.345420665));
#156415=CARTESIAN_POINT('Ctrl Pts',(1.13171359399994,12.2,-11.341935598));
#156416=CARTESIAN_POINT('Ctrl Pts',(1.13292639099994,12.2,-11.338453878));
#156417=CARTESIAN_POINT('Ctrl Pts',(1.13413502299994,12.2,-11.334975512));
#156418=CARTESIAN_POINT('Ctrl Pts',(1.13533949399994,12.2,-11.331500509));
#156419=CARTESIAN_POINT('Ctrl Pts',(1.13653980599994,12.2,-11.32802888));
#156420=CARTESIAN_POINT('Ctrl Pts',(1.13773596199994,12.2,-11.324560631));
#156421=CARTESIAN_POINT('Ctrl Pts',(1.13892796699994,12.2,-11.321095772));
#156422=CARTESIAN_POINT('Ctrl Pts',(1.14011582299994,12.2,-11.317634312));
#156423=CARTESIAN_POINT('Ctrl Pts',(1.14129953199994,12.2,-11.31417626));
#156424=CARTESIAN_POINT('Ctrl Pts',(1.14247909799994,12.2,-11.310721625));
#156425=CARTESIAN_POINT('Ctrl Pts',(1.14365452599994,12.2,-11.307270414));
#156426=CARTESIAN_POINT('Ctrl Pts',(1.14482581499994,12.2,-11.303822638));
#156427=CARTESIAN_POINT('Ctrl Pts',(1.14599297199994,12.2,-11.300378306));
#156428=CARTESIAN_POINT('Ctrl Pts',(1.14715599899994,12.2,-11.296937426));
#156429=CARTESIAN_POINT('Ctrl Pts',(1.14831489899994,12.2,-11.293500006));
#156430=CARTESIAN_POINT('Ctrl Pts',(1.14946967399994,12.2,-11.290066057));
#156431=CARTESIAN_POINT('Ctrl Pts',(1.15062032899994,12.2,-11.286635586));
#156432=CARTESIAN_POINT('Ctrl Pts',(1.15176686799994,12.2,-11.283208603));
#156433=CARTESIAN_POINT('Ctrl Pts',(1.15290929199994,12.2,-11.279785118));
#156434=CARTESIAN_POINT('Ctrl Pts',(1.15404760399994,12.2,-11.276365138));
#156435=CARTESIAN_POINT('Ctrl Pts',(1.15518180899994,12.2,-11.272948673));
#156436=CARTESIAN_POINT('Ctrl Pts',(1.15631190999994,12.2,-11.269535732));
#156437=CARTESIAN_POINT('Ctrl Pts',(1.15743790999994,12.2,-11.266126325));
#156438=CARTESIAN_POINT('Ctrl Pts',(1.15855981299994,12.2,-11.262720459));
#156439=CARTESIAN_POINT('Ctrl Pts',(1.15967762099994,12.2,-11.259318144));
#156440=CARTESIAN_POINT('Ctrl Pts',(1.16079133799994,12.2,-11.25591939));
#156441=CARTESIAN_POINT('Ctrl Pts',(1.16190096699994,12.2,-11.252524204));
#156442=CARTESIAN_POINT('Ctrl Pts',(1.16300651299994,12.2,-11.249132598));
#156443=CARTESIAN_POINT('Ctrl Pts',(1.16410797799994,12.2,-11.245744578));
#156444=CARTESIAN_POINT('Ctrl Pts',(1.16520536399994,12.2,-11.242360155));
#156445=CARTESIAN_POINT('Ctrl Pts',(1.16629867699995,12.2,-11.238979338));
#156446=CARTESIAN_POINT('Ctrl Pts',(1.16738791999994,12.2,-11.235602136));
#156447=CARTESIAN_POINT('Ctrl Pts',(1.16847309399994,12.2,-11.232228557));
#156448=CARTESIAN_POINT('Ctrl Pts',(1.16955420599994,12.2,-11.228858612));
#156449=CARTESIAN_POINT('Ctrl Pts',(1.17063125699994,12.2,-11.22549231));
#156450=CARTESIAN_POINT('Ctrl Pts',(1.17170425099994,12.2,-11.222129659));
#156451=CARTESIAN_POINT('Ctrl Pts',(1.17277319199994,12.2,-11.218770669));
#156452=CARTESIAN_POINT('Ctrl Pts',(1.17383808199994,12.2,-11.215415349));
#156453=CARTESIAN_POINT('Ctrl Pts',(1.17489892699994,12.2,-11.212063708));
#156454=CARTESIAN_POINT('Ctrl Pts',(1.17595572899994,12.2,-11.208715756));
#156455=CARTESIAN_POINT('Ctrl Pts',(1.17700849199994,12.2,-11.205371503));
#156456=CARTESIAN_POINT('Ctrl Pts',(1.17805721899994,12.2,-11.202030955));
#156457=CARTESIAN_POINT('Ctrl Pts',(1.17910191399994,12.2,-11.198694125));
#156458=CARTESIAN_POINT('Ctrl Pts',(1.18014258099994,12.2,-11.195361021));
#156459=CARTESIAN_POINT('Ctrl Pts',(1.18117922299994,12.2,-11.192031652));
#156460=CARTESIAN_POINT('Ctrl Pts',(1.18221184299994,12.2,-11.188706028));
#156461=CARTESIAN_POINT('Ctrl Pts',(1.18324044599994,12.2,-11.185384157));
#156462=CARTESIAN_POINT('Ctrl Pts',(1.18426503499994,12.2,-11.18206605));
#156463=CARTESIAN_POINT('Ctrl Pts',(1.18528561399994,12.2,-11.178751715));
#156464=CARTESIAN_POINT('Ctrl Pts',(1.18630218599994,12.2,-11.175441163));
#156465=CARTESIAN_POINT('Ctrl Pts',(1.18731475499994,12.2,-11.172134402));
#156466=CARTESIAN_POINT('Ctrl Pts',(1.18832332499994,12.2,-11.168831442));
#156467=CARTESIAN_POINT('Ctrl Pts',(1.18932789799994,12.2,-11.165532292));
#156468=CARTESIAN_POINT('Ctrl Pts',(1.19032848099994,12.2,-11.162236962));
#156469=CARTESIAN_POINT('Ctrl Pts',(1.19132507499994,12.2,-11.158945462));
#156470=CARTESIAN_POINT('Ctrl Pts',(1.19231768599994,12.2,-11.155657801));
#156471=CARTESIAN_POINT('Ctrl Pts',(1.19330631499994,12.2,-11.152373988));
#156472=CARTESIAN_POINT('Ctrl Pts',(1.19429096799994,12.2,-11.149094033));
#156473=CARTESIAN_POINT('Ctrl Pts',(1.19527164899994,12.2,-11.145817945));
#156474=CARTESIAN_POINT('Ctrl Pts',(1.19624835999994,12.2,-11.142545735));
#156475=CARTESIAN_POINT('Ctrl Pts',(1.19722110599994,12.2,-11.139277411));
#156476=CARTESIAN_POINT('Ctrl Pts',(1.19818989099994,12.2,-11.136012983));
#156477=CARTESIAN_POINT('Ctrl Pts',(1.19915471699994,12.2,-11.132752462));
#156478=CARTESIAN_POINT('Ctrl Pts',(1.20011559099995,12.2,-11.129495855));
#156479=CARTESIAN_POINT('Ctrl Pts',(1.20107251499994,12.2,-11.126243174));
#156480=CARTESIAN_POINT('Ctrl Pts',(1.20202549299994,12.2,-11.122994428));
#156481=CARTESIAN_POINT('Ctrl Pts',(1.20297452899994,12.2,-11.119749625));
#156482=CARTESIAN_POINT('Ctrl Pts',(1.20391962699994,12.2,-11.116508778));
#156483=CARTESIAN_POINT('Ctrl Pts',(1.20486078999994,12.2,-11.113271894));
#156484=CARTESIAN_POINT('Ctrl Pts',(1.20579802499994,12.2,-11.110038983));
#156485=CARTESIAN_POINT('Ctrl Pts',(1.20673133299994,12.2,-11.106810055));
#156486=CARTESIAN_POINT('Ctrl Pts',(1.20766071899994,12.2,-11.103585121));
#156487=CARTESIAN_POINT('Ctrl Pts',(1.20858618699994,12.2,-11.100364189));
#156488=CARTESIAN_POINT('Ctrl Pts',(1.20950774199994,12.2,-11.09714727));
#156489=CARTESIAN_POINT('Ctrl Pts',(1.21042538699994,12.2,-11.093934372));
#156490=CARTESIAN_POINT('Ctrl Pts',(1.21133912499995,12.2,-11.090725508));
#156491=CARTESIAN_POINT('Ctrl Pts',(1.21224896299994,12.2,-11.087520685));
#156492=CARTESIAN_POINT('Ctrl Pts',(1.21315490199994,12.2,-11.084319915));
#156493=CARTESIAN_POINT('Ctrl Pts',(1.21405694699994,12.2,-11.081123205));
#156494=CARTESIAN_POINT('Ctrl Pts',(1.21495510399994,12.2,-11.077930567));
#156495=CARTESIAN_POINT('Ctrl Pts',(1.21584937499994,12.2,-11.074742011));
#156496=CARTESIAN_POINT('Ctrl Pts',(1.21673976599994,12.2,-11.071557546));
#156497=CARTESIAN_POINT('Ctrl Pts',(1.21762627899994,12.2,-11.068377182));
#156498=CARTESIAN_POINT('Ctrl Pts',(1.21850891999994,12.2,-11.06520093));
#156499=CARTESIAN_POINT('Ctrl Pts',(1.21938769199994,12.2,-11.062028798));
#156500=CARTESIAN_POINT('Ctrl Pts',(1.22026259999994,12.2,-11.058860798));
#156501=CARTESIAN_POINT('Ctrl Pts',(1.22113364899994,12.2,-11.055696939));
#156502=CARTESIAN_POINT('Ctrl Pts',(1.22200084099994,12.2,-11.052537231));
#156503=CARTESIAN_POINT('Ctrl Pts',(1.22286418199994,12.2,-11.049381684));
#156504=CARTESIAN_POINT('Ctrl Pts',(1.22372367599994,12.2,-11.046230309));
#156505=CARTESIAN_POINT('Ctrl Pts',(1.22457932699994,12.2,-11.043083114));
#156506=CARTESIAN_POINT('Ctrl Pts',(1.22543113999994,12.2,-11.03994011));
#156507=CARTESIAN_POINT('Ctrl Pts',(1.22627911799994,12.2,-11.036801309));
#156508=CARTESIAN_POINT('Ctrl Pts',(1.22712326699994,12.2,-11.033666719));
#156509=CARTESIAN_POINT('Ctrl Pts',(1.22796359099994,12.2,-11.030536351));
#156510=CARTESIAN_POINT('Ctrl Pts',(1.22880009299994,12.2,-11.027410214));
#156511=CARTESIAN_POINT('Ctrl Pts',(1.22963277899994,12.2,-11.024288319));
#156512=CARTESIAN_POINT('Ctrl Pts',(1.23046165299994,12.2,-11.021170677));
#156513=CARTESIAN_POINT('Ctrl Pts',(1.23128671899994,12.2,-11.018057297));
#156514=CARTESIAN_POINT('Ctrl Pts',(1.23210798199994,12.2,-11.01494819));
#156515=CARTESIAN_POINT('Ctrl Pts',(1.23292544599995,12.2,-11.011843364));
#156516=CARTESIAN_POINT('Ctrl Pts',(1.23373911599994,12.2,-11.008742833));
#156517=CARTESIAN_POINT('Ctrl Pts',(1.23454899599994,12.2,-11.005646604));
#156518=CARTESIAN_POINT('Ctrl Pts',(1.23535509099994,12.2,-11.002554689));
#156519=CARTESIAN_POINT('Ctrl Pts',(1.23615740499994,12.2,-10.999467099));
#156520=CARTESIAN_POINT('Ctrl Pts',(1.23695594399994,12.2,-10.996383842));
#156521=CARTESIAN_POINT('Ctrl Pts',(1.23775071099994,12.2,-10.99330493));
#156522=CARTESIAN_POINT('Ctrl Pts',(1.23854171099994,12.2,-10.990230373));
#156523=CARTESIAN_POINT('Ctrl Pts',(1.23932894799994,12.2,-10.98716018));
#156524=CARTESIAN_POINT('Ctrl Pts',(1.24011242899994,12.2,-10.984094365));
#156525=CARTESIAN_POINT('Ctrl Pts',(1.24089215599994,12.2,-10.981032935));
#156526=CARTESIAN_POINT('Ctrl Pts',(1.24166813499994,12.2,-10.977975901));
#156527=CARTESIAN_POINT('Ctrl Pts',(1.24244037099994,12.2,-10.974923275));
#156528=CARTESIAN_POINT('Ctrl Pts',(1.24320886799994,12.2,-10.971875066));
#156529=CARTESIAN_POINT('Ctrl Pts',(1.24397362999994,12.2,-10.968831284));
#156530=CARTESIAN_POINT('Ctrl Pts',(1.24473466399994,12.2,-10.965791941));
#156531=CARTESIAN_POINT('Ctrl Pts',(1.24549197299994,12.2,-10.962757048));
#156532=CARTESIAN_POINT('Ctrl Pts',(1.24624556199994,12.2,-10.959726614));
#156533=CARTESIAN_POINT('Ctrl Pts',(1.24699543599994,12.2,-10.95670065));
#156534=CARTESIAN_POINT('Ctrl Pts',(1.24774159999994,12.2,-10.953679166));
#156535=CARTESIAN_POINT('Ctrl Pts',(1.24848405899994,12.2,-10.950662174));
#156536=CARTESIAN_POINT('Ctrl Pts',(1.24922281699994,12.2,-10.947649684));
#156537=CARTESIAN_POINT('Ctrl Pts',(1.24995787899994,12.2,-10.944641705));
#156538=CARTESIAN_POINT('Ctrl Pts',(1.25068925199994,12.2,-10.941638251));
#156539=CARTESIAN_POINT('Ctrl Pts',(1.25141693799994,12.2,-10.93863933));
#156540=CARTESIAN_POINT('Ctrl Pts',(1.25214094299994,12.2,-10.935644954));
#156541=CARTESIAN_POINT('Ctrl Pts',(1.25286127299994,12.2,-10.932655133));
#156542=CARTESIAN_POINT('Ctrl Pts',(1.25357793199994,12.2,-10.929669878));
#156543=CARTESIAN_POINT('Ctrl Pts',(1.25429092499994,12.2,-10.9266892));
#156544=CARTESIAN_POINT('Ctrl Pts',(1.25500025699994,12.2,-10.923713108));
#156545=CARTESIAN_POINT('Ctrl Pts',(1.25570593399994,12.2,-10.920741616));
#156546=CARTESIAN_POINT('Ctrl Pts',(1.25640795899994,12.2,-10.917774733));
#156547=CARTESIAN_POINT('Ctrl Pts',(1.25710633899994,12.2,-10.91481247));
#156548=CARTESIAN_POINT('Ctrl Pts',(1.25780107799994,12.2,-10.911854838));
#156549=CARTESIAN_POINT('Ctrl Pts',(1.25849218299994,12.2,-10.908901847));
#156550=CARTESIAN_POINT('Ctrl Pts',(1.25917965599994,12.2,-10.905953509));
#156551=CARTESIAN_POINT('Ctrl Pts',(1.25986350399994,12.2,-10.903009834));
#156552=CARTESIAN_POINT('Ctrl Pts',(1.26054373299994,12.2,-10.900070834));
#156553=CARTESIAN_POINT('Ctrl Pts',(1.26122034599994,12.2,-10.89713652));
#156554=CARTESIAN_POINT('Ctrl Pts',(1.26189334999994,12.2,-10.894206901));
#156555=CARTESIAN_POINT('Ctrl Pts',(1.26256274999994,12.2,-10.89128199));
#156556=CARTESIAN_POINT('Ctrl Pts',(1.26322855099994,12.2,-10.888361798));
#156557=CARTESIAN_POINT('Ctrl Pts',(1.26389075699994,12.2,-10.885446335));
#156558=CARTESIAN_POINT('Ctrl Pts',(1.26454937499994,12.2,-10.882535612));
#156559=CARTESIAN_POINT('Ctrl Pts',(1.26520440999994,12.2,-10.879629641));
#156560=CARTESIAN_POINT('Ctrl Pts',(1.26585586699994,12.2,-10.876728433));
#156561=CARTESIAN_POINT('Ctrl Pts',(1.26650375199994,12.2,-10.873831999));
#156562=CARTESIAN_POINT('Ctrl Pts',(1.26714806899994,12.2,-10.870940349));
#156563=CARTESIAN_POINT('Ctrl Pts',(1.26778882499994,12.2,-10.868053496));
#156564=CARTESIAN_POINT('Ctrl Pts',(1.26842602399994,12.2,-10.86517145));
#156565=CARTESIAN_POINT('Ctrl Pts',(1.26905967299994,12.2,-10.862294222));
#156566=CARTESIAN_POINT('Ctrl Pts',(1.26968977599994,12.2,-10.859421825));
#156567=CARTESIAN_POINT('Ctrl Pts',(1.27031633899994,12.2,-10.856554267));
#156568=CARTESIAN_POINT('Ctrl Pts',(1.27093936699994,12.2,-10.853691563));
#156569=CARTESIAN_POINT('Ctrl Pts',(1.27155886699994,12.2,-10.850833723));
#156570=CARTESIAN_POINT('Ctrl Pts',(1.27217484299994,12.2,-10.847980757));
#156571=CARTESIAN_POINT('Ctrl Pts',(1.27278730099994,12.2,-10.845132677));
#156572=CARTESIAN_POINT('Ctrl Pts',(1.27339624799994,12.2,-10.842289496));
#156573=CARTESIAN_POINT('Ctrl Pts',(1.27400168799994,12.2,-10.839451223));
#156574=CARTESIAN_POINT('Ctrl Pts',(1.27460362599994,12.2,-10.83661787));
#156575=CARTESIAN_POINT('Ctrl Pts',(1.27520206999994,12.2,-10.833789449));
#156576=CARTESIAN_POINT('Ctrl Pts',(1.27579702299994,12.2,-10.830965973));
#156577=CARTESIAN_POINT('Ctrl Pts',(1.27638849299994,12.2,-10.828147449));
#156578=CARTESIAN_POINT('Ctrl Pts',(1.27697648499994,12.2,-10.825333894));
#156579=CARTESIAN_POINT('Ctrl Pts',(1.27756100499994,12.2,-10.822525316));
#156580=CARTESIAN_POINT('Ctrl Pts',(1.27814205599994,12.2,-10.819721726));
#156581=CARTESIAN_POINT('Ctrl Pts',(1.27871964799994,12.2,-10.816923139));
#156582=CARTESIAN_POINT('Ctrl Pts',(1.27929378499994,12.2,-10.814129563));
#156583=CARTESIAN_POINT('Ctrl Pts',(1.27986447099994,12.2,-10.811341012));
#156584=CARTESIAN_POINT('Ctrl Pts',(1.28043171499994,12.2,-10.808557497));
#156585=CARTESIAN_POINT('Ctrl Pts',(1.28099552199994,12.2,-10.805779028));
#156586=CARTESIAN_POINT('Ctrl Pts',(1.28155589699994,12.2,-10.80300562));
#156587=CARTESIAN_POINT('Ctrl Pts',(1.28211284599994,12.2,-10.800237282));
#156588=CARTESIAN_POINT('Ctrl Pts',(1.28266637399994,12.2,-10.797474026));
#156589=CARTESIAN_POINT('Ctrl Pts',(1.28321648999994,12.2,-10.794715865));
#156590=CARTESIAN_POINT('Ctrl Pts',(1.28376319699994,12.2,-10.791962811));
#156591=CARTESIAN_POINT('Ctrl Pts',(1.28430650299994,12.2,-10.789214873));
#156592=CARTESIAN_POINT('Ctrl Pts',(1.28484641299994,12.2,-10.786472067));
#156593=CARTESIAN_POINT('Ctrl Pts',(1.28538293299994,12.2,-10.7837344));
#156594=CARTESIAN_POINT('Ctrl Pts',(1.28591606999994,12.2,-10.781001888));
#156595=CARTESIAN_POINT('Ctrl Pts',(1.28644582999994,12.2,-10.778274541));
#156596=CARTESIAN_POINT('Ctrl Pts',(1.28697221699994,12.2,-10.775552372));
#156597=CARTESIAN_POINT('Ctrl Pts',(1.28749524099994,12.2,-10.772835393));
#156598=CARTESIAN_POINT('Ctrl Pts',(1.28801490399994,12.2,-10.770123614));
#156599=CARTESIAN_POINT('Ctrl Pts',(1.28853121599994,12.2,-10.767417049));
#156600=CARTESIAN_POINT('Ctrl Pts',(1.28904418099994,12.2,-10.764715709));
#156601=CARTESIAN_POINT('Ctrl Pts',(1.28955380499994,12.2,-10.762019607));
#156602=CARTESIAN_POINT('Ctrl Pts',(1.29006009599994,12.2,-10.759328754));
#156603=CARTESIAN_POINT('Ctrl Pts',(1.29056305799994,12.2,-10.756643162));
#156604=CARTESIAN_POINT('Ctrl Pts',(1.29106269899994,12.2,-10.753962844));
#156605=CARTESIAN_POINT('Ctrl Pts',(1.29155902499994,12.2,-10.751287813));
#156606=CARTESIAN_POINT('Ctrl Pts',(1.29205204299994,12.2,-10.748618079));
#156607=CARTESIAN_POINT('Ctrl Pts',(1.29254175999994,12.2,-10.745953656));
#156608=CARTESIAN_POINT('Ctrl Pts',(1.29302817899994,12.2,-10.743294554));
#156609=CARTESIAN_POINT('Ctrl Pts',(1.29351130999994,12.2,-10.740640788));
#156610=CARTESIAN_POINT('Ctrl Pts',(1.29399115799994,12.2,-10.737992369));
#156611=CARTESIAN_POINT('Ctrl Pts',(1.29446772899994,12.2,-10.73534931));
#156612=CARTESIAN_POINT('Ctrl Pts',(1.29494102999994,12.2,-10.732711622));
#156613=CARTESIAN_POINT('Ctrl Pts',(1.29541106899994,12.2,-10.730079319));
#156614=CARTESIAN_POINT('Ctrl Pts',(1.29587784999994,12.2,-10.727452411));
#156615=CARTESIAN_POINT('Ctrl Pts',(1.29634138199994,12.2,-10.724830913));
#156616=CARTESIAN_POINT('Ctrl Pts',(1.29680167099994,12.2,-10.722214836));
#156617=CARTESIAN_POINT('Ctrl Pts',(1.29725872199994,12.2,-10.719604194));
#156618=CARTESIAN_POINT('Ctrl Pts',(1.29771254399994,12.2,-10.716998997));
#156619=CARTESIAN_POINT('Ctrl Pts',(1.29816314199994,12.2,-10.714399259));
#156620=CARTESIAN_POINT('Ctrl Pts',(1.29861052399994,12.2,-10.711804993));
#156621=CARTESIAN_POINT('Ctrl Pts',(1.29905469599994,12.2,-10.70921621));
#156622=CARTESIAN_POINT('Ctrl Pts',(1.29949566599994,12.2,-10.706632926));
#156623=CARTESIAN_POINT('Ctrl Pts',(1.29993343799994,12.2,-10.70405515));
#156624=CARTESIAN_POINT('Ctrl Pts',(1.30036802199994,12.2,-10.701482895));
#156625=CARTESIAN_POINT('Ctrl Pts',(1.30079942299994,12.2,-10.698916176));
#156626=CARTESIAN_POINT('Ctrl Pts',(1.30122764799994,12.2,-10.696355005));
#156627=CARTESIAN_POINT('Ctrl Pts',(1.30165270499994,12.2,-10.693799393));
#156628=CARTESIAN_POINT('Ctrl Pts',(1.30207460099994,12.2,-10.691249355));
#156629=CARTESIAN_POINT('Ctrl Pts',(1.30249334099994,12.2,-10.688704902));
#156630=CARTESIAN_POINT('Ctrl Pts',(1.30290893499994,12.2,-10.686166048));
#156631=CARTESIAN_POINT('Ctrl Pts',(1.30332138799994,12.2,-10.683632806));
#156632=CARTESIAN_POINT('Ctrl Pts',(1.30373070599994,12.2,-10.681105188));
#156633=CARTESIAN_POINT('Ctrl Pts',(1.30413689999994,12.2,-10.678583208));
#156634=CARTESIAN_POINT('Ctrl Pts',(1.30453997299994,12.2,-10.676066879));
#156635=CARTESIAN_POINT('Ctrl Pts',(1.30493993399994,12.2,-10.673556212));
#156636=CARTESIAN_POINT('Ctrl Pts',(1.30533679099994,12.2,-10.671051222));
#156637=CARTESIAN_POINT('Ctrl Pts',(1.30573054999994,12.2,-10.668551921));
#156638=CARTESIAN_POINT('Ctrl Pts',(1.30612121799994,12.2,-10.666058323));
#156639=CARTESIAN_POINT('Ctrl Pts',(1.30650880299994,12.2,-10.663570441));
#156640=CARTESIAN_POINT('Ctrl Pts',(1.30689331299994,12.2,-10.661088288));
#156641=CARTESIAN_POINT('Ctrl Pts',(1.30727475299994,12.2,-10.658611877));
#156642=CARTESIAN_POINT('Ctrl Pts',(1.30765313299994,12.2,-10.65614122));
#156643=CARTESIAN_POINT('Ctrl Pts',(1.30802845799994,12.2,-10.653676332));
#156644=CARTESIAN_POINT('Ctrl Pts',(1.30840073799994,12.2,-10.651217227));
#156645=CARTESIAN_POINT('Ctrl Pts',(1.30876997899994,12.2,-10.648763916));
#156646=CARTESIAN_POINT('Ctrl Pts',(1.30913618799994,12.2,-10.646316414));
#156647=CARTESIAN_POINT('Ctrl Pts',(1.30949937299994,12.2,-10.643874733));
#156648=CARTESIAN_POINT('Ctrl Pts',(1.30985954199994,12.2,-10.641438888));
#156649=CARTESIAN_POINT('Ctrl Pts',(1.31021670199994,12.2,-10.639008891));
#156650=CARTESIAN_POINT('Ctrl Pts',(1.31057086099994,12.2,-10.636584756));
#156651=CARTESIAN_POINT('Ctrl Pts',(1.31092202599994,12.2,-10.634166498));
#156652=CARTESIAN_POINT('Ctrl Pts',(1.31127020599994,12.2,-10.631754128));
#156653=CARTESIAN_POINT('Ctrl Pts',(1.31161540699994,12.2,-10.629347661));
#156654=CARTESIAN_POINT('Ctrl Pts',(1.31195763899994,12.2,-10.62694711));
#156655=CARTESIAN_POINT('Ctrl Pts',(1.31229690599994,12.2,-10.62455249));
#156656=CARTESIAN_POINT('Ctrl Pts',(1.31263321999994,12.2,-10.622163812));
#156657=CARTESIAN_POINT('Ctrl Pts',(1.31296658599994,12.2,-10.619781092));
#156658=CARTESIAN_POINT('Ctrl Pts',(1.31329701299994,12.2,-10.617404343));
#156659=CARTESIAN_POINT('Ctrl Pts',(1.31362450899994,12.2,-10.615033578));
#156660=CARTESIAN_POINT('Ctrl Pts',(1.31394908099994,12.2,-10.612668813));
#156661=CARTESIAN_POINT('Ctrl Pts',(1.31427073799994,12.2,-10.61031006));
#156662=CARTESIAN_POINT('Ctrl Pts',(1.31458948699994,12.2,-10.607957333));
#156663=CARTESIAN_POINT('Ctrl Pts',(1.31490533699994,12.2,-10.605610646));
#156664=CARTESIAN_POINT('Ctrl Pts',(1.31521829599994,12.2,-10.603270013));
#156665=CARTESIAN_POINT('Ctrl Pts',(1.31552837099994,12.2,-10.600935449));
#156666=CARTESIAN_POINT('Ctrl Pts',(1.31583557099994,12.2,-10.598606966));
#156667=CARTESIAN_POINT('Ctrl Pts',(1.31613990399994,12.2,-10.59628458));
#156668=CARTESIAN_POINT('Ctrl Pts',(1.31644137799994,12.2,-10.593968305));
#156669=CARTESIAN_POINT('Ctrl Pts',(1.31674000099994,12.2,-10.591658153));
#156670=CARTESIAN_POINT('Ctrl Pts',(1.31703578199994,12.2,-10.58935414));
#156671=CARTESIAN_POINT('Ctrl Pts',(1.31732872999994,12.2,-10.58705628));
#156672=CARTESIAN_POINT('Ctrl Pts',(1.31761885099994,12.2,-10.584764587));
#156673=CARTESIAN_POINT('Ctrl Pts',(1.31790615399994,12.2,-10.582479074));
#156674=CARTESIAN_POINT('Ctrl Pts',(1.31819064899994,12.2,-10.580199758));
#156675=CARTESIAN_POINT('Ctrl Pts',(1.31847234299994,12.2,-10.577926652));
#156676=CARTESIAN_POINT('Ctrl Pts',(1.31875124399994,12.2,-10.575659769));
#156677=CARTESIAN_POINT('Ctrl Pts',(1.31902736199994,12.2,-10.573399125));
#156678=CARTESIAN_POINT('Ctrl Pts',(1.31930070599994,12.2,-10.571144734));
#156679=CARTESIAN_POINT('Ctrl Pts',(1.31957128199994,12.2,-10.56889661));
#156680=CARTESIAN_POINT('Ctrl Pts',(1.31983910099994,12.2,-10.566654769));
#156681=CARTESIAN_POINT('Ctrl Pts',(1.32010416999994,12.2,-10.564419224));
#156682=CARTESIAN_POINT('Ctrl Pts',(1.32036649799994,12.2,-10.562189991));
#156683=CARTESIAN_POINT('Ctrl Pts',(1.32062609499994,12.2,-10.559967084));
#156684=CARTESIAN_POINT('Ctrl Pts',(1.32088296799994,12.2,-10.557750517));
#156685=CARTESIAN_POINT('Ctrl Pts',(1.32113712699994,12.2,-10.555540305));
#156686=CARTESIAN_POINT('Ctrl Pts',(1.32138857999994,12.2,-10.553336463));
#156687=CARTESIAN_POINT('Ctrl Pts',(1.32163733599994,12.2,-10.551139007));
#156688=CARTESIAN_POINT('Ctrl Pts',(1.32188340499994,12.2,-10.548947949));
#156689=CARTESIAN_POINT('Ctrl Pts',(1.32212679399994,12.2,-10.546763306));
#156690=CARTESIAN_POINT('Ctrl Pts',(1.32236751399994,12.2,-10.544585093));
#156691=CARTESIAN_POINT('Ctrl Pts',(1.32260557299994,12.2,-10.542413324));
#156692=CARTESIAN_POINT('Ctrl Pts',(1.32284097899994,12.2,-10.540248014));
#156693=CARTESIAN_POINT('Ctrl Pts',(1.32307374299994,12.2,-10.53808918));
#156694=CARTESIAN_POINT('Ctrl Pts',(1.32330387399994,12.2,-10.535936834));
#156695=CARTESIAN_POINT('Ctrl Pts',(1.32353137899994,12.2,-10.533790993));
#156696=CARTESIAN_POINT('Ctrl Pts',(1.32375626899994,12.2,-10.531651672));
#156697=CARTESIAN_POINT('Ctrl Pts',(1.32397855299994,12.2,-10.529518885));
#156698=CARTESIAN_POINT('Ctrl Pts',(1.32419823999994,12.2,-10.52739265));
#156699=CARTESIAN_POINT('Ctrl Pts',(1.32441533999994,12.2,-10.52527298));
#156700=CARTESIAN_POINT('Ctrl Pts',(1.32462986099994,12.2,-10.523159891));
#156701=CARTESIAN_POINT('Ctrl Pts',(1.32484181499994,12.2,-10.521053397));
#156702=CARTESIAN_POINT('Ctrl Pts',(1.32505120699994,12.2,-10.518953515));
#156703=CARTESIAN_POINT('Ctrl Pts',(1.32525805199994,12.2,-10.516860261));
#156704=CARTESIAN_POINT('Ctrl Pts',(1.32546235399994,12.2,-10.514773649));
#156705=CARTESIAN_POINT('Ctrl Pts',(1.32566412699994,12.2,-10.512693695));
#156706=CARTESIAN_POINT('Ctrl Pts',(1.32586337699994,12.2,-10.510620415));
#156707=CARTESIAN_POINT('Ctrl Pts',(1.32606011699994,12.2,-10.508553825));
#156708=CARTESIAN_POINT('Ctrl Pts',(1.32625435399994,12.2,-10.506493939));
#156709=CARTESIAN_POINT('Ctrl Pts',(1.32644609999994,12.2,-10.504440774));
#156710=CARTESIAN_POINT('Ctrl Pts',(1.32663536199994,12.2,-10.502394346));
#156711=CARTESIAN_POINT('Ctrl Pts',(1.32682215299994,12.2,-10.500354671));
#156712=CARTESIAN_POINT('Ctrl Pts',(1.32700648099994,12.2,-10.498321763));
#156713=CARTESIAN_POINT('Ctrl Pts',(1.32718835599994,12.2,-10.49629564));
#156714=CARTESIAN_POINT('Ctrl Pts',(1.32736778799994,12.2,-10.494276317));
#156715=CARTESIAN_POINT('Ctrl Pts',(1.32754478699994,12.2,-10.49226381));
#156716=CARTESIAN_POINT('Ctrl Pts',(1.32771936299994,12.2,-10.490258135));
#156717=CARTESIAN_POINT('Ctrl Pts',(1.32789152599994,12.2,-10.488259308));
#156718=CARTESIAN_POINT('Ctrl Pts',(1.32806128599994,12.2,-10.486267346));
#156719=CARTESIAN_POINT('Ctrl Pts',(1.32822865399994,12.2,-10.484282264));
#156720=CARTESIAN_POINT('Ctrl Pts',(1.32839363899994,12.2,-10.48230408));
#156721=CARTESIAN_POINT('Ctrl Pts',(1.32855625199994,12.2,-10.480332808));
#156722=CARTESIAN_POINT('Ctrl Pts',(1.32871650299994,12.2,-10.478368465));
#156723=CARTESIAN_POINT('Ctrl Pts',(1.32887440299994,12.2,-10.476411069));
#156724=CARTESIAN_POINT('Ctrl Pts',(1.32902996199994,12.2,-10.474460635));
#156725=CARTESIAN_POINT('Ctrl Pts',(1.32918318899994,12.2,-10.47251718));
#156726=CARTESIAN_POINT('Ctrl Pts',(1.32933409699994,12.2,-10.47058072));
#156727=CARTESIAN_POINT('Ctrl Pts',(1.32948269399994,12.2,-10.468651272));
#156728=CARTESIAN_POINT('Ctrl Pts',(1.32962899299994,12.2,-10.466728852));
#156729=CARTESIAN_POINT('Ctrl Pts',(1.32977300299994,12.2,-10.464813477));
#156730=CARTESIAN_POINT('Ctrl Pts',(1.32991473499994,12.2,-10.462905165));
#156731=CARTESIAN_POINT('Ctrl Pts',(1.33005419999994,12.2,-10.461003932));
#156732=CARTESIAN_POINT('Ctrl Pts',(1.33019140799994,12.2,-10.459109793));
#156733=CARTESIAN_POINT('Ctrl Pts',(1.33032637099994,12.2,-10.457222766));
#156734=CARTESIAN_POINT('Ctrl Pts',(1.33045909799994,12.2,-10.45534287));
#156735=CARTESIAN_POINT('Ctrl Pts',(1.33058960299994,12.2,-10.453470121));
#156736=CARTESIAN_POINT('Ctrl Pts',(1.33071789299994,12.2,-10.451604534));
#156737=CARTESIAN_POINT('Ctrl Pts',(1.33084398199994,12.2,-10.449746128));
#156738=CARTESIAN_POINT('Ctrl Pts',(1.33096787999994,12.2,-10.447894919));
#156739=CARTESIAN_POINT('Ctrl Pts',(1.33108959799994,12.2,-10.446050926));
#156740=CARTESIAN_POINT('Ctrl Pts',(1.33120914699994,12.2,-10.444214164));
#156741=CARTESIAN_POINT('Ctrl Pts',(1.33132653899994,12.2,-10.442384652));
#156742=CARTESIAN_POINT('Ctrl Pts',(1.33144178299994,12.2,-10.440562407));
#156743=CARTESIAN_POINT('Ctrl Pts',(1.33155489399994,12.2,-10.438747447));
#156744=CARTESIAN_POINT('Ctrl Pts',(1.33166587999994,12.2,-10.436939788));
#156745=CARTESIAN_POINT('Ctrl Pts',(1.33177475499994,12.2,-10.435139448));
#156746=CARTESIAN_POINT('Ctrl Pts',(1.33188152799994,12.2,-10.433346446));
#156747=CARTESIAN_POINT('Ctrl Pts',(1.33198621199994,12.2,-10.431560797));
#156748=CARTESIAN_POINT('Ctrl Pts',(1.33208881899994,12.2,-10.429782521));
#156749=CARTESIAN_POINT('Ctrl Pts',(1.33218935899994,12.2,-10.428011636));
#156750=CARTESIAN_POINT('Ctrl Pts',(1.33228784499994,12.2,-10.426248158));
#156751=CARTESIAN_POINT('Ctrl Pts',(1.33238428799994,12.2,-10.424492106));
#156752=CARTESIAN_POINT('Ctrl Pts',(1.33247869999994,12.2,-10.422743497));
#156753=CARTESIAN_POINT('Ctrl Pts',(1.33257109199994,12.2,-10.421002351));
#156754=CARTESIAN_POINT('Ctrl Pts',(1.33266147799994,12.2,-10.419268684));
#156755=CARTESIAN_POINT('Ctrl Pts',(1.33274986699994,12.2,-10.417542515));
#156756=CARTESIAN_POINT('Ctrl Pts',(1.33283627399994,12.2,-10.415823863));
#156757=CARTESIAN_POINT('Ctrl Pts',(1.33292070899994,12.2,-10.414112744));
#156758=CARTESIAN_POINT('Ctrl Pts',(1.33300318399994,12.2,-10.412409178));
#156759=CARTESIAN_POINT('Ctrl Pts',(1.33308371299994,12.2,-10.410713184));
#156760=CARTESIAN_POINT('Ctrl Pts',(1.33316230599994,12.2,-10.409024778));
#156761=CARTESIAN_POINT('Ctrl Pts',(1.33323897699994,12.2,-10.40734398));
#156762=CARTESIAN_POINT('Ctrl Pts',(1.33331373699994,12.2,-10.405670811));
#156763=CARTESIAN_POINT('Ctrl Pts',(1.33338659999994,12.2,-10.404005285));
#156764=CARTESIAN_POINT('Ctrl Pts',(1.33345757699994,12.2,-10.402347423));
#156765=CARTESIAN_POINT('Ctrl Pts',(1.33352668099994,12.2,-10.400697244));
#156766=CARTESIAN_POINT('Ctrl Pts',(1.33359392399994,12.2,-10.399054766));
#156767=CARTESIAN_POINT('Ctrl Pts',(1.33365931999994,12.2,-10.397420008));
#156768=CARTESIAN_POINT('Ctrl Pts',(1.33372287999994,12.2,-10.39579299));
#156769=CARTESIAN_POINT('Ctrl Pts',(1.33378461799994,12.2,-10.39417373));
#156770=CARTESIAN_POINT('Ctrl Pts',(1.33384454499994,12.2,-10.392562248));
#156771=CARTESIAN_POINT('Ctrl Pts',(1.33390267699994,12.2,-10.39095856));
#156772=CARTESIAN_POINT('Ctrl Pts',(1.33395902399994,12.2,-10.38936269));
#156773=CARTESIAN_POINT('Ctrl Pts',(1.33401359999994,12.2,-10.387774654));
#156774=CARTESIAN_POINT('Ctrl Pts',(1.33406641799994,12.2,-10.386194473));
#156775=CARTESIAN_POINT('Ctrl Pts',(1.33411749199994,12.2,-10.384622165));
#156776=CARTESIAN_POINT('Ctrl Pts',(1.33416683399994,12.2,-10.383057751));
#156777=CARTESIAN_POINT('Ctrl Pts',(1.33421445699994,12.2,-10.381501249));
#156778=CARTESIAN_POINT('Ctrl Pts',(1.33426037499994,12.2,-10.379952679));
#156779=CARTESIAN_POINT('Ctrl Pts',(1.33430460199994,12.2,-10.378412062));
#156780=CARTESIAN_POINT('Ctrl Pts',(1.33434714999994,12.2,-10.376879417));
#156781=CARTESIAN_POINT('Ctrl Pts',(1.33438803299994,12.2,-10.375354763));
#156782=CARTESIAN_POINT('Ctrl Pts',(1.33442726499994,12.2,-10.373838121));
#156783=CARTESIAN_POINT('Ctrl Pts',(1.33446485899994,12.2,-10.37232951));
#156784=CARTESIAN_POINT('Ctrl Pts',(1.33450082899994,12.2,-10.370828951));
#156785=CARTESIAN_POINT('Ctrl Pts',(1.33453518799994,12.2,-10.369336464));
#156786=CARTESIAN_POINT('Ctrl Pts',(1.33456795099994,12.2,-10.367852069));
#156787=CARTESIAN_POINT('Ctrl Pts',(1.33459913199994,12.2,-10.366375787));
#156788=CARTESIAN_POINT('Ctrl Pts',(1.33462874399994,12.2,-10.364907637));
#156789=CARTESIAN_POINT('Ctrl Pts',(1.33465680099994,12.2,-10.363447639));
#156790=CARTESIAN_POINT('Ctrl Pts',(1.33468331799994,12.2,-10.361995816));
#156791=CARTESIAN_POINT('Ctrl Pts',(1.33470830799994,12.2,-10.360552186));
#156792=CARTESIAN_POINT('Ctrl Pts',(1.33473178599994,12.2,-10.359116771));
#156793=CARTESIAN_POINT('Ctrl Pts',(1.33475376599994,12.2,-10.357689593));
#156794=CARTESIAN_POINT('Ctrl Pts',(1.33477426199994,12.2,-10.356270671));
#156795=CARTESIAN_POINT('Ctrl Pts',(1.33479328899994,12.2,-10.354860026));
#156796=CARTESIAN_POINT('Ctrl Pts',(1.33481086199994,12.2,-10.353457679));
#156797=CARTESIAN_POINT('Ctrl Pts',(1.33482699499994,12.2,-10.352063652));
#156798=CARTESIAN_POINT('Ctrl Pts',(1.33484170199994,12.2,-10.350677965));
#156799=CARTESIAN_POINT('Ctrl Pts',(1.33485499899994,12.2,-10.34930064));
#156800=CARTESIAN_POINT('Ctrl Pts',(1.33486689899994,12.2,-10.347931697));
#156801=CARTESIAN_POINT('Ctrl Pts',(1.33487741999994,12.2,-10.34657116));
#156802=CARTESIAN_POINT('Ctrl Pts',(1.33488657299994,12.2,-10.345219049));
#156803=CARTESIAN_POINT('Ctrl Pts',(1.33489437599994,12.2,-10.343875384));
#156804=CARTESIAN_POINT('Ctrl Pts',(1.33490084299994,12.2,-10.342540189));
#156805=CARTESIAN_POINT('Ctrl Pts',(1.33490598899994,12.2,-10.341213485));
#156806=CARTESIAN_POINT('Ctrl Pts',(1.33490982999994,12.2,-10.339895294));
#156807=CARTESIAN_POINT('Ctrl Pts',(1.33491238099994,12.2,-10.338585637));
#156808=CARTESIAN_POINT('Ctrl Pts',(1.33491365599994,12.2,-10.337284537));
#156809=CARTESIAN_POINT('Ctrl Pts',(1.33491367299994,12.2,-10.335992016));
#156810=CARTESIAN_POINT('Ctrl Pts',(1.33491244599994,12.2,-10.334708096));
#156811=CARTESIAN_POINT('Ctrl Pts',(1.33490999099994,12.2,-10.333432799));
#156812=CARTESIAN_POINT('Ctrl Pts',(1.33490632299994,12.2,-10.332166147));
#156813=CARTESIAN_POINT('Ctrl Pts',(1.33490145899994,12.2,-10.330908163));
#156814=CARTESIAN_POINT('Ctrl Pts',(1.33489541499994,12.2,-10.32965887));
#156815=CARTESIAN_POINT('Ctrl Pts',(1.33488820599994,12.2,-10.32841829));
#156816=CARTESIAN_POINT('Ctrl Pts',(1.33487984899994,12.2,-10.327186447));
#156817=CARTESIAN_POINT('Ctrl Pts',(1.33487035799994,12.2,-10.32596336));
#156818=CARTESIAN_POINT('Ctrl Pts',(1.33485975199994,12.2,-10.324749056));
#156819=CARTESIAN_POINT('Ctrl Pts',(1.33484804599994,12.2,-10.323543558));
#156820=CARTESIAN_POINT('Ctrl Pts',(1.33483525599994,12.2,-10.322346886));
#156821=CARTESIAN_POINT('Ctrl Pts',(1.33482139999994,12.2,-10.321159066));
#156822=CARTESIAN_POINT('Ctrl Pts',(1.33480649299994,12.2,-10.319980119));
#156823=CARTESIAN_POINT('Ctrl Pts',(1.33479055199994,12.2,-10.318810071));
#156824=CARTESIAN_POINT('Ctrl Pts',(1.33477359399994,12.2,-10.317648943));
#156825=CARTESIAN_POINT('Ctrl Pts',(1.33475563599994,12.2,-10.31649676));
#156826=CARTESIAN_POINT('Ctrl Pts',(1.33473669499994,12.2,-10.315353546));
#156827=CARTESIAN_POINT('Ctrl Pts',(1.33471678699994,12.2,-10.314219324));
#156828=CARTESIAN_POINT('Ctrl Pts',(1.33469592999994,12.2,-10.313094118));
#156829=CARTESIAN_POINT('Ctrl Pts',(1.33467414199994,12.2,-10.311977952));
#156830=CARTESIAN_POINT('Ctrl Pts',(1.33465143899994,12.2,-10.310870851));
#156831=CARTESIAN_POINT('Ctrl Pts',(1.33462783799994,12.2,-10.309772837));
#156832=CARTESIAN_POINT('Ctrl Pts',(1.33460335699994,12.2,-10.308683938));
#156833=CARTESIAN_POINT('Ctrl Pts',(1.33457801399994,12.2,-10.307604175));
#156834=CARTESIAN_POINT('Ctrl Pts',(1.33455182599994,12.2,-10.306533574));
#156835=CARTESIAN_POINT('Ctrl Pts',(1.33452481199994,12.2,-10.30547216));
#156836=CARTESIAN_POINT('Ctrl Pts',(1.33449698899994,12.2,-10.304419957));
#156837=CARTESIAN_POINT('Ctrl Pts',(1.33446837399994,12.2,-10.30337699));
#156838=CARTESIAN_POINT('Ctrl Pts',(1.33443898699994,12.2,-10.302343284));
#156839=CARTESIAN_POINT('Ctrl Pts',(1.33440884499994,12.2,-10.301318864));
#156840=CARTESIAN_POINT('Ctrl Pts',(1.33437796499994,12.2,-10.300303756));
#156841=CARTESIAN_POINT('Ctrl Pts',(1.33434636799994,12.2,-10.299297985));
#156842=CARTESIAN_POINT('Ctrl Pts',(1.33431407099994,12.2,-10.298301576));
#156843=CARTESIAN_POINT('Ctrl Pts',(1.33428109299994,12.2,-10.297314555));
#156844=CARTESIAN_POINT('Ctrl Pts',(1.33424745199994,12.2,-10.296336946));
#156845=CARTESIAN_POINT('Ctrl Pts',(1.33421316699994,12.2,-10.295368778));
#156846=CARTESIAN_POINT('Ctrl Pts',(1.33417825799994,12.2,-10.294410075));
#156847=CARTESIAN_POINT('Ctrl Pts',(1.33414274299994,12.2,-10.293460862));
#156848=CARTESIAN_POINT('Ctrl Pts',(1.33410663999994,12.2,-10.292521167));
#156849=CARTESIAN_POINT('Ctrl Pts',(1.33406996899994,12.2,-10.291591017));
#156850=CARTESIAN_POINT('Ctrl Pts',(1.33403296599994,12.2,-10.290675738));
#156851=CARTESIAN_POINT('Ctrl Pts',(1.33400298699994,12.2,-10.289952142));
#156852=CARTESIAN_POINT('Ctrl Pts',(1.33398033299994,12.2,-10.289415004));
#156853=CARTESIAN_POINT('Ctrl Pts',(1.33396520799994,12.2,-10.289060521));
#156854=CARTESIAN_POINT('Ctrl Pts',(1.33395773199994,12.2,-10.288886323));
#156855=CARTESIAN_POINT('Ctrl Pts',(1.33395773199994,15.2,-10.288886323));
#156856=CARTESIAN_POINT('Ctrl Pts',(1.33396520799994,15.2,-10.289060521));
#156857=CARTESIAN_POINT('Ctrl Pts',(1.33398033299994,15.2,-10.289415004));
#156858=CARTESIAN_POINT('Ctrl Pts',(1.33400298699994,15.2,-10.289952142));
#156859=CARTESIAN_POINT('Ctrl Pts',(1.33403296599994,15.2,-10.290675738));
#156860=CARTESIAN_POINT('Ctrl Pts',(1.33406996899994,15.2,-10.291591017));
#156861=CARTESIAN_POINT('Ctrl Pts',(1.33410663999994,15.2,-10.292521167));
#156862=CARTESIAN_POINT('Ctrl Pts',(1.33414274299994,15.2,-10.293460862));
#156863=CARTESIAN_POINT('Ctrl Pts',(1.33417825799994,15.2,-10.294410075));
#156864=CARTESIAN_POINT('Ctrl Pts',(1.33421316699994,15.2,-10.295368778));
#156865=CARTESIAN_POINT('Ctrl Pts',(1.33424745199994,15.2,-10.296336946));
#156866=CARTESIAN_POINT('Ctrl Pts',(1.33428109299994,15.2,-10.297314555));
#156867=CARTESIAN_POINT('Ctrl Pts',(1.33431407099994,15.2,-10.298301576));
#156868=CARTESIAN_POINT('Ctrl Pts',(1.33434636799994,15.2,-10.299297985));
#156869=CARTESIAN_POINT('Ctrl Pts',(1.33437796499994,15.2,-10.300303756));
#156870=CARTESIAN_POINT('Ctrl Pts',(1.33440884499994,15.2,-10.301318864));
#156871=CARTESIAN_POINT('Ctrl Pts',(1.33443898699994,15.2,-10.302343284));
#156872=CARTESIAN_POINT('Ctrl Pts',(1.33446837399994,15.2,-10.30337699));
#156873=CARTESIAN_POINT('Ctrl Pts',(1.33449698899994,15.2,-10.304419957));
#156874=CARTESIAN_POINT('Ctrl Pts',(1.33452481199994,15.2,-10.30547216));
#156875=CARTESIAN_POINT('Ctrl Pts',(1.33455182599994,15.2,-10.306533574));
#156876=CARTESIAN_POINT('Ctrl Pts',(1.33457801399994,15.2,-10.307604175));
#156877=CARTESIAN_POINT('Ctrl Pts',(1.33460335699994,15.2,-10.308683938));
#156878=CARTESIAN_POINT('Ctrl Pts',(1.33462783799994,15.2,-10.309772837));
#156879=CARTESIAN_POINT('Ctrl Pts',(1.33465143899994,15.2,-10.310870851));
#156880=CARTESIAN_POINT('Ctrl Pts',(1.33467414199994,15.2,-10.311977952));
#156881=CARTESIAN_POINT('Ctrl Pts',(1.33469592999994,15.2,-10.313094118));
#156882=CARTESIAN_POINT('Ctrl Pts',(1.33471678699994,15.2,-10.314219324));
#156883=CARTESIAN_POINT('Ctrl Pts',(1.33473669499994,15.2,-10.315353546));
#156884=CARTESIAN_POINT('Ctrl Pts',(1.33475563599994,15.2,-10.31649676));
#156885=CARTESIAN_POINT('Ctrl Pts',(1.33477359399994,15.2,-10.317648943));
#156886=CARTESIAN_POINT('Ctrl Pts',(1.33479055199994,15.2,-10.318810071));
#156887=CARTESIAN_POINT('Ctrl Pts',(1.33480649299994,15.2,-10.319980119));
#156888=CARTESIAN_POINT('Ctrl Pts',(1.33482139999994,15.2,-10.321159066));
#156889=CARTESIAN_POINT('Ctrl Pts',(1.33483525599994,15.2,-10.322346886));
#156890=CARTESIAN_POINT('Ctrl Pts',(1.33484804599994,15.2,-10.323543558));
#156891=CARTESIAN_POINT('Ctrl Pts',(1.33485975199994,15.2,-10.324749056));
#156892=CARTESIAN_POINT('Ctrl Pts',(1.33487035799994,15.2,-10.32596336));
#156893=CARTESIAN_POINT('Ctrl Pts',(1.33487984899994,15.2,-10.327186447));
#156894=CARTESIAN_POINT('Ctrl Pts',(1.33488820599994,15.2,-10.32841829));
#156895=CARTESIAN_POINT('Ctrl Pts',(1.33489541499994,15.2,-10.32965887));
#156896=CARTESIAN_POINT('Ctrl Pts',(1.33490145899994,15.2,-10.330908163));
#156897=CARTESIAN_POINT('Ctrl Pts',(1.33490632299994,15.2,-10.332166147));
#156898=CARTESIAN_POINT('Ctrl Pts',(1.33490999099994,15.2,-10.333432799));
#156899=CARTESIAN_POINT('Ctrl Pts',(1.33491244599994,15.2,-10.334708096));
#156900=CARTESIAN_POINT('Ctrl Pts',(1.33491367299994,15.2,-10.335992016));
#156901=CARTESIAN_POINT('Ctrl Pts',(1.33491365599994,15.2,-10.337284537));
#156902=CARTESIAN_POINT('Ctrl Pts',(1.33491238099994,15.2,-10.338585637));
#156903=CARTESIAN_POINT('Ctrl Pts',(1.33490982999994,15.2,-10.339895294));
#156904=CARTESIAN_POINT('Ctrl Pts',(1.33490598899994,15.2,-10.341213485));
#156905=CARTESIAN_POINT('Ctrl Pts',(1.33490084299994,15.2,-10.342540189));
#156906=CARTESIAN_POINT('Ctrl Pts',(1.33489437599994,15.2,-10.343875384));
#156907=CARTESIAN_POINT('Ctrl Pts',(1.33488657299994,15.2,-10.345219049));
#156908=CARTESIAN_POINT('Ctrl Pts',(1.33487741999994,15.2,-10.34657116));
#156909=CARTESIAN_POINT('Ctrl Pts',(1.33486689899994,15.2,-10.347931697));
#156910=CARTESIAN_POINT('Ctrl Pts',(1.33485499899994,15.2,-10.34930064));
#156911=CARTESIAN_POINT('Ctrl Pts',(1.33484170199994,15.2,-10.350677965));
#156912=CARTESIAN_POINT('Ctrl Pts',(1.33482699499994,15.2,-10.352063652));
#156913=CARTESIAN_POINT('Ctrl Pts',(1.33481086199994,15.2,-10.353457679));
#156914=CARTESIAN_POINT('Ctrl Pts',(1.33479328899994,15.2,-10.354860026));
#156915=CARTESIAN_POINT('Ctrl Pts',(1.33477426199994,15.2,-10.356270671));
#156916=CARTESIAN_POINT('Ctrl Pts',(1.33475376599994,15.2,-10.357689593));
#156917=CARTESIAN_POINT('Ctrl Pts',(1.33473178599994,15.2,-10.359116771));
#156918=CARTESIAN_POINT('Ctrl Pts',(1.33470830799994,15.2,-10.360552186));
#156919=CARTESIAN_POINT('Ctrl Pts',(1.33468331799994,15.2,-10.361995816));
#156920=CARTESIAN_POINT('Ctrl Pts',(1.33465680099994,15.2,-10.363447639));
#156921=CARTESIAN_POINT('Ctrl Pts',(1.33462874399994,15.2,-10.364907637));
#156922=CARTESIAN_POINT('Ctrl Pts',(1.33459913199994,15.2,-10.366375787));
#156923=CARTESIAN_POINT('Ctrl Pts',(1.33456795099994,15.2,-10.367852069));
#156924=CARTESIAN_POINT('Ctrl Pts',(1.33453518799994,15.2,-10.369336464));
#156925=CARTESIAN_POINT('Ctrl Pts',(1.33450082899994,15.2,-10.370828951));
#156926=CARTESIAN_POINT('Ctrl Pts',(1.33446485899994,15.2,-10.37232951));
#156927=CARTESIAN_POINT('Ctrl Pts',(1.33442726499994,15.2,-10.373838121));
#156928=CARTESIAN_POINT('Ctrl Pts',(1.33438803299994,15.2,-10.375354763));
#156929=CARTESIAN_POINT('Ctrl Pts',(1.33434714999994,15.2,-10.376879417));
#156930=CARTESIAN_POINT('Ctrl Pts',(1.33430460199994,15.2,-10.378412062));
#156931=CARTESIAN_POINT('Ctrl Pts',(1.33426037499994,15.2,-10.379952679));
#156932=CARTESIAN_POINT('Ctrl Pts',(1.33421445699994,15.2,-10.381501249));
#156933=CARTESIAN_POINT('Ctrl Pts',(1.33416683399994,15.2,-10.383057751));
#156934=CARTESIAN_POINT('Ctrl Pts',(1.33411749199994,15.2,-10.384622165));
#156935=CARTESIAN_POINT('Ctrl Pts',(1.33406641799994,15.2,-10.386194473));
#156936=CARTESIAN_POINT('Ctrl Pts',(1.33401359999994,15.2,-10.387774654));
#156937=CARTESIAN_POINT('Ctrl Pts',(1.33395902399994,15.2,-10.38936269));
#156938=CARTESIAN_POINT('Ctrl Pts',(1.33390267699994,15.2,-10.39095856));
#156939=CARTESIAN_POINT('Ctrl Pts',(1.33384454499994,15.2,-10.392562248));
#156940=CARTESIAN_POINT('Ctrl Pts',(1.33378461799994,15.2,-10.39417373));
#156941=CARTESIAN_POINT('Ctrl Pts',(1.33372287999994,15.2,-10.39579299));
#156942=CARTESIAN_POINT('Ctrl Pts',(1.33365931999994,15.2,-10.397420008));
#156943=CARTESIAN_POINT('Ctrl Pts',(1.33359392399994,15.2,-10.399054766));
#156944=CARTESIAN_POINT('Ctrl Pts',(1.33352668099994,15.2,-10.400697244));
#156945=CARTESIAN_POINT('Ctrl Pts',(1.33345757699994,15.2,-10.402347423));
#156946=CARTESIAN_POINT('Ctrl Pts',(1.33338659999994,15.2,-10.404005285));
#156947=CARTESIAN_POINT('Ctrl Pts',(1.33331373699994,15.2,-10.405670811));
#156948=CARTESIAN_POINT('Ctrl Pts',(1.33323897699994,15.2,-10.40734398));
#156949=CARTESIAN_POINT('Ctrl Pts',(1.33316230599994,15.2,-10.409024778));
#156950=CARTESIAN_POINT('Ctrl Pts',(1.33308371299994,15.2,-10.410713184));
#156951=CARTESIAN_POINT('Ctrl Pts',(1.33300318399994,15.2,-10.412409178));
#156952=CARTESIAN_POINT('Ctrl Pts',(1.33292070899994,15.2,-10.414112744));
#156953=CARTESIAN_POINT('Ctrl Pts',(1.33283627399994,15.2,-10.415823863));
#156954=CARTESIAN_POINT('Ctrl Pts',(1.33274986699994,15.2,-10.417542515));
#156955=CARTESIAN_POINT('Ctrl Pts',(1.33266147799994,15.2,-10.419268684));
#156956=CARTESIAN_POINT('Ctrl Pts',(1.33257109199994,15.2,-10.421002351));
#156957=CARTESIAN_POINT('Ctrl Pts',(1.33247869999994,15.2,-10.422743497));
#156958=CARTESIAN_POINT('Ctrl Pts',(1.33238428799994,15.2,-10.424492106));
#156959=CARTESIAN_POINT('Ctrl Pts',(1.33228784499994,15.2,-10.426248158));
#156960=CARTESIAN_POINT('Ctrl Pts',(1.33218935899994,15.2,-10.428011636));
#156961=CARTESIAN_POINT('Ctrl Pts',(1.33208881899994,15.2,-10.429782521));
#156962=CARTESIAN_POINT('Ctrl Pts',(1.33198621199994,15.2,-10.431560797));
#156963=CARTESIAN_POINT('Ctrl Pts',(1.33188152799994,15.2,-10.433346446));
#156964=CARTESIAN_POINT('Ctrl Pts',(1.33177475499994,15.2,-10.435139448));
#156965=CARTESIAN_POINT('Ctrl Pts',(1.33166587999994,15.2,-10.436939788));
#156966=CARTESIAN_POINT('Ctrl Pts',(1.33155489399994,15.2,-10.438747447));
#156967=CARTESIAN_POINT('Ctrl Pts',(1.33144178299994,15.2,-10.440562407));
#156968=CARTESIAN_POINT('Ctrl Pts',(1.33132653899994,15.2,-10.442384652));
#156969=CARTESIAN_POINT('Ctrl Pts',(1.33120914699994,15.2,-10.444214164));
#156970=CARTESIAN_POINT('Ctrl Pts',(1.33108959799994,15.2,-10.446050926));
#156971=CARTESIAN_POINT('Ctrl Pts',(1.33096787999994,15.2,-10.447894919));
#156972=CARTESIAN_POINT('Ctrl Pts',(1.33084398199994,15.2,-10.449746128));
#156973=CARTESIAN_POINT('Ctrl Pts',(1.33071789299994,15.2,-10.451604534));
#156974=CARTESIAN_POINT('Ctrl Pts',(1.33058960299994,15.2,-10.453470121));
#156975=CARTESIAN_POINT('Ctrl Pts',(1.33045909799994,15.2,-10.45534287));
#156976=CARTESIAN_POINT('Ctrl Pts',(1.33032637099994,15.2,-10.457222766));
#156977=CARTESIAN_POINT('Ctrl Pts',(1.33019140799994,15.2,-10.459109793));
#156978=CARTESIAN_POINT('Ctrl Pts',(1.33005419999994,15.2,-10.461003932));
#156979=CARTESIAN_POINT('Ctrl Pts',(1.32991473499994,15.2,-10.462905165));
#156980=CARTESIAN_POINT('Ctrl Pts',(1.32977300299994,15.2,-10.464813477));
#156981=CARTESIAN_POINT('Ctrl Pts',(1.32962899299994,15.2,-10.466728852));
#156982=CARTESIAN_POINT('Ctrl Pts',(1.32948269399994,15.2,-10.468651272));
#156983=CARTESIAN_POINT('Ctrl Pts',(1.32933409699994,15.2,-10.47058072));
#156984=CARTESIAN_POINT('Ctrl Pts',(1.32918318899994,15.2,-10.47251718));
#156985=CARTESIAN_POINT('Ctrl Pts',(1.32902996199994,15.2,-10.474460635));
#156986=CARTESIAN_POINT('Ctrl Pts',(1.32887440299994,15.2,-10.476411069));
#156987=CARTESIAN_POINT('Ctrl Pts',(1.32871650299994,15.2,-10.478368465));
#156988=CARTESIAN_POINT('Ctrl Pts',(1.32855625199994,15.2,-10.480332808));
#156989=CARTESIAN_POINT('Ctrl Pts',(1.32839363899994,15.2,-10.48230408));
#156990=CARTESIAN_POINT('Ctrl Pts',(1.32822865399994,15.2,-10.484282264));
#156991=CARTESIAN_POINT('Ctrl Pts',(1.32806128599994,15.2,-10.486267346));
#156992=CARTESIAN_POINT('Ctrl Pts',(1.32789152599994,15.2,-10.488259308));
#156993=CARTESIAN_POINT('Ctrl Pts',(1.32771936299994,15.2,-10.490258135));
#156994=CARTESIAN_POINT('Ctrl Pts',(1.32754478699994,15.2,-10.49226381));
#156995=CARTESIAN_POINT('Ctrl Pts',(1.32736778799994,15.2,-10.494276317));
#156996=CARTESIAN_POINT('Ctrl Pts',(1.32718835599994,15.2,-10.49629564));
#156997=CARTESIAN_POINT('Ctrl Pts',(1.32700648099994,15.2,-10.498321763));
#156998=CARTESIAN_POINT('Ctrl Pts',(1.32682215299994,15.2,-10.500354671));
#156999=CARTESIAN_POINT('Ctrl Pts',(1.32663536199994,15.2,-10.502394346));
#157000=CARTESIAN_POINT('Ctrl Pts',(1.32644609999994,15.2,-10.504440774));
#157001=CARTESIAN_POINT('Ctrl Pts',(1.32625435399994,15.2,-10.506493939));
#157002=CARTESIAN_POINT('Ctrl Pts',(1.32606011699994,15.2,-10.508553825));
#157003=CARTESIAN_POINT('Ctrl Pts',(1.32586337699994,15.2,-10.510620415));
#157004=CARTESIAN_POINT('Ctrl Pts',(1.32566412699994,15.2,-10.512693695));
#157005=CARTESIAN_POINT('Ctrl Pts',(1.32546235399994,15.2,-10.514773649));
#157006=CARTESIAN_POINT('Ctrl Pts',(1.32525805199994,15.2,-10.516860261));
#157007=CARTESIAN_POINT('Ctrl Pts',(1.32505120699994,15.2,-10.518953515));
#157008=CARTESIAN_POINT('Ctrl Pts',(1.32484181499994,15.2,-10.521053397));
#157009=CARTESIAN_POINT('Ctrl Pts',(1.32462986099994,15.2,-10.523159891));
#157010=CARTESIAN_POINT('Ctrl Pts',(1.32441533999994,15.2,-10.52527298));
#157011=CARTESIAN_POINT('Ctrl Pts',(1.32419823999994,15.2,-10.52739265));
#157012=CARTESIAN_POINT('Ctrl Pts',(1.32397855299994,15.2,-10.529518885));
#157013=CARTESIAN_POINT('Ctrl Pts',(1.32375626899994,15.2,-10.531651672));
#157014=CARTESIAN_POINT('Ctrl Pts',(1.32353137899994,15.2,-10.533790993));
#157015=CARTESIAN_POINT('Ctrl Pts',(1.32330387399994,15.2,-10.535936834));
#157016=CARTESIAN_POINT('Ctrl Pts',(1.32307374299994,15.2,-10.53808918));
#157017=CARTESIAN_POINT('Ctrl Pts',(1.32284097899994,15.2,-10.540248014));
#157018=CARTESIAN_POINT('Ctrl Pts',(1.32260557299994,15.2,-10.542413324));
#157019=CARTESIAN_POINT('Ctrl Pts',(1.32236751399994,15.2,-10.544585093));
#157020=CARTESIAN_POINT('Ctrl Pts',(1.32212679399994,15.2,-10.546763306));
#157021=CARTESIAN_POINT('Ctrl Pts',(1.32188340499994,15.2,-10.548947949));
#157022=CARTESIAN_POINT('Ctrl Pts',(1.32163733599994,15.2,-10.551139007));
#157023=CARTESIAN_POINT('Ctrl Pts',(1.32138857999994,15.2,-10.553336463));
#157024=CARTESIAN_POINT('Ctrl Pts',(1.32113712699994,15.2,-10.555540305));
#157025=CARTESIAN_POINT('Ctrl Pts',(1.32088296799994,15.2,-10.557750517));
#157026=CARTESIAN_POINT('Ctrl Pts',(1.32062609499994,15.2,-10.559967084));
#157027=CARTESIAN_POINT('Ctrl Pts',(1.32036649799994,15.2,-10.562189991));
#157028=CARTESIAN_POINT('Ctrl Pts',(1.32010416999994,15.2,-10.564419224));
#157029=CARTESIAN_POINT('Ctrl Pts',(1.31983910099994,15.2,-10.566654769));
#157030=CARTESIAN_POINT('Ctrl Pts',(1.31957128199994,15.2,-10.56889661));
#157031=CARTESIAN_POINT('Ctrl Pts',(1.31930070599994,15.2,-10.571144734));
#157032=CARTESIAN_POINT('Ctrl Pts',(1.31902736199994,15.2,-10.573399125));
#157033=CARTESIAN_POINT('Ctrl Pts',(1.31875124399994,15.2,-10.575659769));
#157034=CARTESIAN_POINT('Ctrl Pts',(1.31847234299994,15.2,-10.577926652));
#157035=CARTESIAN_POINT('Ctrl Pts',(1.31819064899994,15.2,-10.580199758));
#157036=CARTESIAN_POINT('Ctrl Pts',(1.31790615399994,15.2,-10.582479074));
#157037=CARTESIAN_POINT('Ctrl Pts',(1.31761885099994,15.2,-10.584764587));
#157038=CARTESIAN_POINT('Ctrl Pts',(1.31732872999994,15.2,-10.58705628));
#157039=CARTESIAN_POINT('Ctrl Pts',(1.31703578199994,15.2,-10.58935414));
#157040=CARTESIAN_POINT('Ctrl Pts',(1.31674000099994,15.2,-10.591658153));
#157041=CARTESIAN_POINT('Ctrl Pts',(1.31644137799994,15.2,-10.593968305));
#157042=CARTESIAN_POINT('Ctrl Pts',(1.31613990399994,15.2,-10.59628458));
#157043=CARTESIAN_POINT('Ctrl Pts',(1.31583557099994,15.2,-10.598606966));
#157044=CARTESIAN_POINT('Ctrl Pts',(1.31552837099994,15.2,-10.600935449));
#157045=CARTESIAN_POINT('Ctrl Pts',(1.31521829599994,15.2,-10.603270013));
#157046=CARTESIAN_POINT('Ctrl Pts',(1.31490533699994,15.2,-10.605610646));
#157047=CARTESIAN_POINT('Ctrl Pts',(1.31458948699994,15.2,-10.607957333));
#157048=CARTESIAN_POINT('Ctrl Pts',(1.31427073799994,15.2,-10.61031006));
#157049=CARTESIAN_POINT('Ctrl Pts',(1.31394908099994,15.2,-10.612668813));
#157050=CARTESIAN_POINT('Ctrl Pts',(1.31362450899994,15.2,-10.615033578));
#157051=CARTESIAN_POINT('Ctrl Pts',(1.31329701299994,15.2,-10.617404343));
#157052=CARTESIAN_POINT('Ctrl Pts',(1.31296658599994,15.2,-10.619781092));
#157053=CARTESIAN_POINT('Ctrl Pts',(1.31263321999994,15.2,-10.622163812));
#157054=CARTESIAN_POINT('Ctrl Pts',(1.31229690599994,15.2,-10.62455249));
#157055=CARTESIAN_POINT('Ctrl Pts',(1.31195763899994,15.2,-10.62694711));
#157056=CARTESIAN_POINT('Ctrl Pts',(1.31161540699994,15.2,-10.629347661));
#157057=CARTESIAN_POINT('Ctrl Pts',(1.31127020599994,15.2,-10.631754128));
#157058=CARTESIAN_POINT('Ctrl Pts',(1.31092202599994,15.2,-10.634166498));
#157059=CARTESIAN_POINT('Ctrl Pts',(1.31057086099994,15.2,-10.636584756));
#157060=CARTESIAN_POINT('Ctrl Pts',(1.31021670199994,15.2,-10.639008891));
#157061=CARTESIAN_POINT('Ctrl Pts',(1.30985954199994,15.2,-10.641438888));
#157062=CARTESIAN_POINT('Ctrl Pts',(1.30949937299994,15.2,-10.643874733));
#157063=CARTESIAN_POINT('Ctrl Pts',(1.30913618799994,15.2,-10.646316414));
#157064=CARTESIAN_POINT('Ctrl Pts',(1.30876997899994,15.2,-10.648763916));
#157065=CARTESIAN_POINT('Ctrl Pts',(1.30840073799994,15.2,-10.651217227));
#157066=CARTESIAN_POINT('Ctrl Pts',(1.30802845799994,15.2,-10.653676332));
#157067=CARTESIAN_POINT('Ctrl Pts',(1.30765313299994,15.2,-10.65614122));
#157068=CARTESIAN_POINT('Ctrl Pts',(1.30727475299994,15.2,-10.658611877));
#157069=CARTESIAN_POINT('Ctrl Pts',(1.30689331299994,15.2,-10.661088288));
#157070=CARTESIAN_POINT('Ctrl Pts',(1.30650880299994,15.2,-10.663570441));
#157071=CARTESIAN_POINT('Ctrl Pts',(1.30612121799994,15.2,-10.666058323));
#157072=CARTESIAN_POINT('Ctrl Pts',(1.30573054999994,15.2,-10.668551921));
#157073=CARTESIAN_POINT('Ctrl Pts',(1.30533679099994,15.2,-10.671051222));
#157074=CARTESIAN_POINT('Ctrl Pts',(1.30493993399994,15.2,-10.673556212));
#157075=CARTESIAN_POINT('Ctrl Pts',(1.30453997299994,15.2,-10.676066879));
#157076=CARTESIAN_POINT('Ctrl Pts',(1.30413689999994,15.2,-10.678583208));
#157077=CARTESIAN_POINT('Ctrl Pts',(1.30373070599994,15.2,-10.681105188));
#157078=CARTESIAN_POINT('Ctrl Pts',(1.30332138799994,15.2,-10.683632806));
#157079=CARTESIAN_POINT('Ctrl Pts',(1.30290893499994,15.2,-10.686166048));
#157080=CARTESIAN_POINT('Ctrl Pts',(1.30249334099994,15.2,-10.688704902));
#157081=CARTESIAN_POINT('Ctrl Pts',(1.30207460099994,15.2,-10.691249355));
#157082=CARTESIAN_POINT('Ctrl Pts',(1.30165270499994,15.2,-10.693799393));
#157083=CARTESIAN_POINT('Ctrl Pts',(1.30122764799994,15.2,-10.696355005));
#157084=CARTESIAN_POINT('Ctrl Pts',(1.30079942299994,15.2,-10.698916176));
#157085=CARTESIAN_POINT('Ctrl Pts',(1.30036802199994,15.2,-10.701482895));
#157086=CARTESIAN_POINT('Ctrl Pts',(1.29993343799994,15.2,-10.70405515));
#157087=CARTESIAN_POINT('Ctrl Pts',(1.29949566599994,15.2,-10.706632926));
#157088=CARTESIAN_POINT('Ctrl Pts',(1.29905469599994,15.2,-10.70921621));
#157089=CARTESIAN_POINT('Ctrl Pts',(1.29861052399994,15.2,-10.711804993));
#157090=CARTESIAN_POINT('Ctrl Pts',(1.29816314199994,15.2,-10.714399259));
#157091=CARTESIAN_POINT('Ctrl Pts',(1.29771254399994,15.2,-10.716998997));
#157092=CARTESIAN_POINT('Ctrl Pts',(1.29725872199994,15.2,-10.719604194));
#157093=CARTESIAN_POINT('Ctrl Pts',(1.29680167099994,15.2,-10.722214836));
#157094=CARTESIAN_POINT('Ctrl Pts',(1.29634138199994,15.2,-10.724830913));
#157095=CARTESIAN_POINT('Ctrl Pts',(1.29587784999994,15.2,-10.727452411));
#157096=CARTESIAN_POINT('Ctrl Pts',(1.29541106899994,15.2,-10.730079319));
#157097=CARTESIAN_POINT('Ctrl Pts',(1.29494102999994,15.2,-10.732711622));
#157098=CARTESIAN_POINT('Ctrl Pts',(1.29446772899994,15.2,-10.73534931));
#157099=CARTESIAN_POINT('Ctrl Pts',(1.29399115799994,15.2,-10.737992369));
#157100=CARTESIAN_POINT('Ctrl Pts',(1.29351130999994,15.2,-10.740640788));
#157101=CARTESIAN_POINT('Ctrl Pts',(1.29302817899994,15.2,-10.743294554));
#157102=CARTESIAN_POINT('Ctrl Pts',(1.29254175999994,15.2,-10.745953656));
#157103=CARTESIAN_POINT('Ctrl Pts',(1.29205204299994,15.2,-10.748618079));
#157104=CARTESIAN_POINT('Ctrl Pts',(1.29155902499994,15.2,-10.751287813));
#157105=CARTESIAN_POINT('Ctrl Pts',(1.29106269899994,15.2,-10.753962844));
#157106=CARTESIAN_POINT('Ctrl Pts',(1.29056305799994,15.2,-10.756643162));
#157107=CARTESIAN_POINT('Ctrl Pts',(1.29006009599994,15.2,-10.759328754));
#157108=CARTESIAN_POINT('Ctrl Pts',(1.28955380499994,15.2,-10.762019607));
#157109=CARTESIAN_POINT('Ctrl Pts',(1.28904418099994,15.2,-10.764715709));
#157110=CARTESIAN_POINT('Ctrl Pts',(1.28853121599994,15.2,-10.767417049));
#157111=CARTESIAN_POINT('Ctrl Pts',(1.28801490399994,15.2,-10.770123614));
#157112=CARTESIAN_POINT('Ctrl Pts',(1.28749524099994,15.2,-10.772835393));
#157113=CARTESIAN_POINT('Ctrl Pts',(1.28697221699994,15.2,-10.775552372));
#157114=CARTESIAN_POINT('Ctrl Pts',(1.28644582999994,15.2,-10.778274541));
#157115=CARTESIAN_POINT('Ctrl Pts',(1.28591606999994,15.2,-10.781001888));
#157116=CARTESIAN_POINT('Ctrl Pts',(1.28538293299994,15.2,-10.7837344));
#157117=CARTESIAN_POINT('Ctrl Pts',(1.28484641299994,15.2,-10.786472067));
#157118=CARTESIAN_POINT('Ctrl Pts',(1.28430650299994,15.2,-10.789214873));
#157119=CARTESIAN_POINT('Ctrl Pts',(1.28376319699994,15.2,-10.791962811));
#157120=CARTESIAN_POINT('Ctrl Pts',(1.28321648999994,15.2,-10.794715865));
#157121=CARTESIAN_POINT('Ctrl Pts',(1.28266637399994,15.2,-10.797474026));
#157122=CARTESIAN_POINT('Ctrl Pts',(1.28211284599994,15.2,-10.800237282));
#157123=CARTESIAN_POINT('Ctrl Pts',(1.28155589699994,15.2,-10.80300562));
#157124=CARTESIAN_POINT('Ctrl Pts',(1.28099552199994,15.2,-10.805779028));
#157125=CARTESIAN_POINT('Ctrl Pts',(1.28043171499994,15.2,-10.808557497));
#157126=CARTESIAN_POINT('Ctrl Pts',(1.27986447099994,15.2,-10.811341012));
#157127=CARTESIAN_POINT('Ctrl Pts',(1.27929378499994,15.2,-10.814129563));
#157128=CARTESIAN_POINT('Ctrl Pts',(1.27871964799994,15.2,-10.816923139));
#157129=CARTESIAN_POINT('Ctrl Pts',(1.27814205599994,15.2,-10.819721726));
#157130=CARTESIAN_POINT('Ctrl Pts',(1.27756100499994,15.2,-10.822525316));
#157131=CARTESIAN_POINT('Ctrl Pts',(1.27697648499994,15.2,-10.825333894));
#157132=CARTESIAN_POINT('Ctrl Pts',(1.27638849299994,15.2,-10.828147449));
#157133=CARTESIAN_POINT('Ctrl Pts',(1.27579702299994,15.2,-10.830965973));
#157134=CARTESIAN_POINT('Ctrl Pts',(1.27520206999994,15.2,-10.833789449));
#157135=CARTESIAN_POINT('Ctrl Pts',(1.27460362599994,15.2,-10.83661787));
#157136=CARTESIAN_POINT('Ctrl Pts',(1.27400168799994,15.2,-10.839451223));
#157137=CARTESIAN_POINT('Ctrl Pts',(1.27339624799994,15.2,-10.842289496));
#157138=CARTESIAN_POINT('Ctrl Pts',(1.27278730099994,15.2,-10.845132677));
#157139=CARTESIAN_POINT('Ctrl Pts',(1.27217484299994,15.2,-10.847980757));
#157140=CARTESIAN_POINT('Ctrl Pts',(1.27155886699994,15.2,-10.850833723));
#157141=CARTESIAN_POINT('Ctrl Pts',(1.27093936699994,15.2,-10.853691563));
#157142=CARTESIAN_POINT('Ctrl Pts',(1.27031633899994,15.2,-10.856554267));
#157143=CARTESIAN_POINT('Ctrl Pts',(1.26968977599994,15.2,-10.859421825));
#157144=CARTESIAN_POINT('Ctrl Pts',(1.26905967299994,15.2,-10.862294222));
#157145=CARTESIAN_POINT('Ctrl Pts',(1.26842602399994,15.2,-10.86517145));
#157146=CARTESIAN_POINT('Ctrl Pts',(1.26778882499994,15.2,-10.868053496));
#157147=CARTESIAN_POINT('Ctrl Pts',(1.26714806899994,15.2,-10.870940349));
#157148=CARTESIAN_POINT('Ctrl Pts',(1.26650375199994,15.2,-10.873831999));
#157149=CARTESIAN_POINT('Ctrl Pts',(1.26585586699994,15.2,-10.876728433));
#157150=CARTESIAN_POINT('Ctrl Pts',(1.26520440999994,15.2,-10.879629641));
#157151=CARTESIAN_POINT('Ctrl Pts',(1.26454937499994,15.2,-10.882535612));
#157152=CARTESIAN_POINT('Ctrl Pts',(1.26389075699994,15.2,-10.885446335));
#157153=CARTESIAN_POINT('Ctrl Pts',(1.26322855099994,15.2,-10.888361798));
#157154=CARTESIAN_POINT('Ctrl Pts',(1.26256274999994,15.2,-10.89128199));
#157155=CARTESIAN_POINT('Ctrl Pts',(1.26189334999994,15.2,-10.894206901));
#157156=CARTESIAN_POINT('Ctrl Pts',(1.26122034599994,15.2,-10.89713652));
#157157=CARTESIAN_POINT('Ctrl Pts',(1.26054373299994,15.2,-10.900070834));
#157158=CARTESIAN_POINT('Ctrl Pts',(1.25986350399994,15.2,-10.903009834));
#157159=CARTESIAN_POINT('Ctrl Pts',(1.25917965599994,15.2,-10.905953509));
#157160=CARTESIAN_POINT('Ctrl Pts',(1.25849218299994,15.2,-10.908901847));
#157161=CARTESIAN_POINT('Ctrl Pts',(1.25780107799994,15.2,-10.911854838));
#157162=CARTESIAN_POINT('Ctrl Pts',(1.25710633899994,15.2,-10.91481247));
#157163=CARTESIAN_POINT('Ctrl Pts',(1.25640795899994,15.2,-10.917774733));
#157164=CARTESIAN_POINT('Ctrl Pts',(1.25570593399994,15.2,-10.920741616));
#157165=CARTESIAN_POINT('Ctrl Pts',(1.25500025699994,15.2,-10.923713108));
#157166=CARTESIAN_POINT('Ctrl Pts',(1.25429092499994,15.2,-10.9266892));
#157167=CARTESIAN_POINT('Ctrl Pts',(1.25357793199994,15.2,-10.929669878));
#157168=CARTESIAN_POINT('Ctrl Pts',(1.25286127299994,15.2,-10.932655133));
#157169=CARTESIAN_POINT('Ctrl Pts',(1.25214094299994,15.2,-10.935644954));
#157170=CARTESIAN_POINT('Ctrl Pts',(1.25141693799994,15.2,-10.93863933));
#157171=CARTESIAN_POINT('Ctrl Pts',(1.25068925199994,15.2,-10.941638251));
#157172=CARTESIAN_POINT('Ctrl Pts',(1.24995787899994,15.2,-10.944641705));
#157173=CARTESIAN_POINT('Ctrl Pts',(1.24922281699994,15.2,-10.947649684));
#157174=CARTESIAN_POINT('Ctrl Pts',(1.24848405899994,15.2,-10.950662174));
#157175=CARTESIAN_POINT('Ctrl Pts',(1.24774159999994,15.2,-10.953679166));
#157176=CARTESIAN_POINT('Ctrl Pts',(1.24699543599994,15.2,-10.95670065));
#157177=CARTESIAN_POINT('Ctrl Pts',(1.24624556199994,15.2,-10.959726614));
#157178=CARTESIAN_POINT('Ctrl Pts',(1.24549197299994,15.2,-10.962757048));
#157179=CARTESIAN_POINT('Ctrl Pts',(1.24473466399994,15.2,-10.965791941));
#157180=CARTESIAN_POINT('Ctrl Pts',(1.24397362999994,15.2,-10.968831284));
#157181=CARTESIAN_POINT('Ctrl Pts',(1.24320886799994,15.2,-10.971875066));
#157182=CARTESIAN_POINT('Ctrl Pts',(1.24244037099994,15.2,-10.974923275));
#157183=CARTESIAN_POINT('Ctrl Pts',(1.24166813499994,15.2,-10.977975901));
#157184=CARTESIAN_POINT('Ctrl Pts',(1.24089215599994,15.2,-10.981032935));
#157185=CARTESIAN_POINT('Ctrl Pts',(1.24011242899994,15.2,-10.984094365));
#157186=CARTESIAN_POINT('Ctrl Pts',(1.23932894799994,15.2,-10.98716018));
#157187=CARTESIAN_POINT('Ctrl Pts',(1.23854171099994,15.2,-10.990230373));
#157188=CARTESIAN_POINT('Ctrl Pts',(1.23775071099994,15.2,-10.99330493));
#157189=CARTESIAN_POINT('Ctrl Pts',(1.23695594399994,15.2,-10.996383842));
#157190=CARTESIAN_POINT('Ctrl Pts',(1.23615740499994,15.2,-10.999467099));
#157191=CARTESIAN_POINT('Ctrl Pts',(1.23535509099994,15.2,-11.002554689));
#157192=CARTESIAN_POINT('Ctrl Pts',(1.23454899599994,15.2,-11.005646604));
#157193=CARTESIAN_POINT('Ctrl Pts',(1.23373911599994,15.2,-11.008742833));
#157194=CARTESIAN_POINT('Ctrl Pts',(1.23292544599995,15.2,-11.011843364));
#157195=CARTESIAN_POINT('Ctrl Pts',(1.23210798199994,15.2,-11.01494819));
#157196=CARTESIAN_POINT('Ctrl Pts',(1.23128671899994,15.2,-11.018057297));
#157197=CARTESIAN_POINT('Ctrl Pts',(1.23046165299994,15.2,-11.021170677));
#157198=CARTESIAN_POINT('Ctrl Pts',(1.22963277899994,15.2,-11.024288319));
#157199=CARTESIAN_POINT('Ctrl Pts',(1.22880009299994,15.2,-11.027410214));
#157200=CARTESIAN_POINT('Ctrl Pts',(1.22796359099994,15.2,-11.030536351));
#157201=CARTESIAN_POINT('Ctrl Pts',(1.22712326699994,15.2,-11.033666719));
#157202=CARTESIAN_POINT('Ctrl Pts',(1.22627911799994,15.2,-11.036801309));
#157203=CARTESIAN_POINT('Ctrl Pts',(1.22543113999994,15.2,-11.03994011));
#157204=CARTESIAN_POINT('Ctrl Pts',(1.22457932699994,15.2,-11.043083114));
#157205=CARTESIAN_POINT('Ctrl Pts',(1.22372367599994,15.2,-11.046230309));
#157206=CARTESIAN_POINT('Ctrl Pts',(1.22286418199994,15.2,-11.049381684));
#157207=CARTESIAN_POINT('Ctrl Pts',(1.22200084099994,15.2,-11.052537231));
#157208=CARTESIAN_POINT('Ctrl Pts',(1.22113364899994,15.2,-11.055696939));
#157209=CARTESIAN_POINT('Ctrl Pts',(1.22026259999994,15.2,-11.058860798));
#157210=CARTESIAN_POINT('Ctrl Pts',(1.21938769199994,15.2,-11.062028798));
#157211=CARTESIAN_POINT('Ctrl Pts',(1.21850891999994,15.2,-11.06520093));
#157212=CARTESIAN_POINT('Ctrl Pts',(1.21762627899994,15.2,-11.068377182));
#157213=CARTESIAN_POINT('Ctrl Pts',(1.21673976599994,15.2,-11.071557546));
#157214=CARTESIAN_POINT('Ctrl Pts',(1.21584937499994,15.2,-11.074742011));
#157215=CARTESIAN_POINT('Ctrl Pts',(1.21495510399994,15.2,-11.077930567));
#157216=CARTESIAN_POINT('Ctrl Pts',(1.21405694699994,15.2,-11.081123205));
#157217=CARTESIAN_POINT('Ctrl Pts',(1.21315490199994,15.2,-11.084319915));
#157218=CARTESIAN_POINT('Ctrl Pts',(1.21224896299994,15.2,-11.087520685));
#157219=CARTESIAN_POINT('Ctrl Pts',(1.21133912499995,15.2,-11.090725508));
#157220=CARTESIAN_POINT('Ctrl Pts',(1.21042538699994,15.2,-11.093934372));
#157221=CARTESIAN_POINT('Ctrl Pts',(1.20950774199994,15.2,-11.09714727));
#157222=CARTESIAN_POINT('Ctrl Pts',(1.20858618699994,15.2,-11.100364189));
#157223=CARTESIAN_POINT('Ctrl Pts',(1.20766071899994,15.2,-11.103585121));
#157224=CARTESIAN_POINT('Ctrl Pts',(1.20673133299994,15.2,-11.106810055));
#157225=CARTESIAN_POINT('Ctrl Pts',(1.20579802499994,15.2,-11.110038983));
#157226=CARTESIAN_POINT('Ctrl Pts',(1.20486078999994,15.2,-11.113271894));
#157227=CARTESIAN_POINT('Ctrl Pts',(1.20391962699994,15.2,-11.116508778));
#157228=CARTESIAN_POINT('Ctrl Pts',(1.20297452899994,15.2,-11.119749625));
#157229=CARTESIAN_POINT('Ctrl Pts',(1.20202549299994,15.2,-11.122994428));
#157230=CARTESIAN_POINT('Ctrl Pts',(1.20107251499994,15.2,-11.126243174));
#157231=CARTESIAN_POINT('Ctrl Pts',(1.20011559099995,15.2,-11.129495855));
#157232=CARTESIAN_POINT('Ctrl Pts',(1.19915471699994,15.2,-11.132752462));
#157233=CARTESIAN_POINT('Ctrl Pts',(1.19818989099994,15.2,-11.136012983));
#157234=CARTESIAN_POINT('Ctrl Pts',(1.19722110599994,15.2,-11.139277411));
#157235=CARTESIAN_POINT('Ctrl Pts',(1.19624835999994,15.2,-11.142545735));
#157236=CARTESIAN_POINT('Ctrl Pts',(1.19527164899994,15.2,-11.145817945));
#157237=CARTESIAN_POINT('Ctrl Pts',(1.19429096799994,15.2,-11.149094033));
#157238=CARTESIAN_POINT('Ctrl Pts',(1.19330631499994,15.2,-11.152373988));
#157239=CARTESIAN_POINT('Ctrl Pts',(1.19231768599994,15.2,-11.155657801));
#157240=CARTESIAN_POINT('Ctrl Pts',(1.19132507499994,15.2,-11.158945462));
#157241=CARTESIAN_POINT('Ctrl Pts',(1.19032848099994,15.2,-11.162236962));
#157242=CARTESIAN_POINT('Ctrl Pts',(1.18932789799994,15.2,-11.165532292));
#157243=CARTESIAN_POINT('Ctrl Pts',(1.18832332499994,15.2,-11.168831442));
#157244=CARTESIAN_POINT('Ctrl Pts',(1.18731475499994,15.2,-11.172134402));
#157245=CARTESIAN_POINT('Ctrl Pts',(1.18630218599994,15.2,-11.175441163));
#157246=CARTESIAN_POINT('Ctrl Pts',(1.18528561399994,15.2,-11.178751715));
#157247=CARTESIAN_POINT('Ctrl Pts',(1.18426503499994,15.2,-11.18206605));
#157248=CARTESIAN_POINT('Ctrl Pts',(1.18324044599994,15.2,-11.185384157));
#157249=CARTESIAN_POINT('Ctrl Pts',(1.18221184299994,15.2,-11.188706028));
#157250=CARTESIAN_POINT('Ctrl Pts',(1.18117922299994,15.2,-11.192031652));
#157251=CARTESIAN_POINT('Ctrl Pts',(1.18014258099994,15.2,-11.195361021));
#157252=CARTESIAN_POINT('Ctrl Pts',(1.17910191399994,15.2,-11.198694125));
#157253=CARTESIAN_POINT('Ctrl Pts',(1.17805721899994,15.2,-11.202030955));
#157254=CARTESIAN_POINT('Ctrl Pts',(1.17700849199994,15.2,-11.205371503));
#157255=CARTESIAN_POINT('Ctrl Pts',(1.17595572899994,15.2,-11.208715756));
#157256=CARTESIAN_POINT('Ctrl Pts',(1.17489892699994,15.2,-11.212063708));
#157257=CARTESIAN_POINT('Ctrl Pts',(1.17383808199994,15.2,-11.215415349));
#157258=CARTESIAN_POINT('Ctrl Pts',(1.17277319199994,15.2,-11.218770669));
#157259=CARTESIAN_POINT('Ctrl Pts',(1.17170425099994,15.2,-11.222129659));
#157260=CARTESIAN_POINT('Ctrl Pts',(1.17063125699994,15.2,-11.22549231));
#157261=CARTESIAN_POINT('Ctrl Pts',(1.16955420599994,15.2,-11.228858612));
#157262=CARTESIAN_POINT('Ctrl Pts',(1.16847309399994,15.2,-11.232228557));
#157263=CARTESIAN_POINT('Ctrl Pts',(1.16738791999994,15.2,-11.235602136));
#157264=CARTESIAN_POINT('Ctrl Pts',(1.16629867699995,15.2,-11.238979338));
#157265=CARTESIAN_POINT('Ctrl Pts',(1.16520536399994,15.2,-11.242360155));
#157266=CARTESIAN_POINT('Ctrl Pts',(1.16410797799994,15.2,-11.245744578));
#157267=CARTESIAN_POINT('Ctrl Pts',(1.16300651299994,15.2,-11.249132598));
#157268=CARTESIAN_POINT('Ctrl Pts',(1.16190096699994,15.2,-11.252524204));
#157269=CARTESIAN_POINT('Ctrl Pts',(1.16079133799994,15.2,-11.25591939));
#157270=CARTESIAN_POINT('Ctrl Pts',(1.15967762099994,15.2,-11.259318144));
#157271=CARTESIAN_POINT('Ctrl Pts',(1.15855981299994,15.2,-11.262720459));
#157272=CARTESIAN_POINT('Ctrl Pts',(1.15743790999994,15.2,-11.266126325));
#157273=CARTESIAN_POINT('Ctrl Pts',(1.15631190999994,15.2,-11.269535732));
#157274=CARTESIAN_POINT('Ctrl Pts',(1.15518180899994,15.2,-11.272948673));
#157275=CARTESIAN_POINT('Ctrl Pts',(1.15404760399994,15.2,-11.276365138));
#157276=CARTESIAN_POINT('Ctrl Pts',(1.15290929199994,15.2,-11.279785118));
#157277=CARTESIAN_POINT('Ctrl Pts',(1.15176686799994,15.2,-11.283208603));
#157278=CARTESIAN_POINT('Ctrl Pts',(1.15062032899994,15.2,-11.286635586));
#157279=CARTESIAN_POINT('Ctrl Pts',(1.14946967399994,15.2,-11.290066057));
#157280=CARTESIAN_POINT('Ctrl Pts',(1.14831489899994,15.2,-11.293500006));
#157281=CARTESIAN_POINT('Ctrl Pts',(1.14715599899994,15.2,-11.296937426));
#157282=CARTESIAN_POINT('Ctrl Pts',(1.14599297199994,15.2,-11.300378306));
#157283=CARTESIAN_POINT('Ctrl Pts',(1.14482581499994,15.2,-11.303822638));
#157284=CARTESIAN_POINT('Ctrl Pts',(1.14365452599994,15.2,-11.307270414));
#157285=CARTESIAN_POINT('Ctrl Pts',(1.14247909799994,15.2,-11.310721625));
#157286=CARTESIAN_POINT('Ctrl Pts',(1.14129953199994,15.2,-11.31417626));
#157287=CARTESIAN_POINT('Ctrl Pts',(1.14011582299994,15.2,-11.317634312));
#157288=CARTESIAN_POINT('Ctrl Pts',(1.13892796699994,15.2,-11.321095772));
#157289=CARTESIAN_POINT('Ctrl Pts',(1.13773596199994,15.2,-11.324560631));
#157290=CARTESIAN_POINT('Ctrl Pts',(1.13653980599994,15.2,-11.32802888));
#157291=CARTESIAN_POINT('Ctrl Pts',(1.13533949399994,15.2,-11.331500509));
#157292=CARTESIAN_POINT('Ctrl Pts',(1.13413502299994,15.2,-11.334975512));
#157293=CARTESIAN_POINT('Ctrl Pts',(1.13292639099994,15.2,-11.338453878));
#157294=CARTESIAN_POINT('Ctrl Pts',(1.13171359399994,15.2,-11.341935598));
#157295=CARTESIAN_POINT('Ctrl Pts',(1.13049662999994,15.2,-11.345420665));
#157296=CARTESIAN_POINT('Ctrl Pts',(1.12927549399994,15.2,-11.348909068));
#157297=CARTESIAN_POINT('Ctrl Pts',(1.12805018499994,15.2,-11.3524008));
#157298=CARTESIAN_POINT('Ctrl Pts',(1.12682069999994,15.2,-11.355895851));
#157299=CARTESIAN_POINT('Ctrl Pts',(1.12558703399994,15.2,-11.359394214));
#157300=CARTESIAN_POINT('Ctrl Pts',(1.12434918699994,15.2,-11.36289588));
#157301=CARTESIAN_POINT('Ctrl Pts',(1.12310715399994,15.2,-11.366400839));
#157302=CARTESIAN_POINT('Ctrl Pts',(1.12186093199994,15.2,-11.369909084));
#157303=CARTESIAN_POINT('Ctrl Pts',(1.12061051899994,15.2,-11.373420606));
#157304=CARTESIAN_POINT('Ctrl Pts',(1.11935591099994,15.2,-11.376935393));
#157305=CARTESIAN_POINT('Ctrl Pts',(1.11809710599994,15.2,-11.38045344));
#157306=CARTESIAN_POINT('Ctrl Pts',(1.11683409999994,15.2,-11.383974735));
#157307=CARTESIAN_POINT('Ctrl Pts',(1.11556688999994,15.2,-11.387499272));
#157308=CARTESIAN_POINT('Ctrl Pts',(1.11429547399994,15.2,-11.39102704));
#157309=CARTESIAN_POINT('Ctrl Pts',(1.11301984899994,15.2,-11.394558034));
#157310=CARTESIAN_POINT('Ctrl Pts',(1.11174001299994,15.2,-11.398092244));
#157311=CARTESIAN_POINT('Ctrl Pts',(1.11045596299994,15.2,-11.401629665));
#157312=CARTESIAN_POINT('Ctrl Pts',(1.10916769599994,15.2,-11.405170286));
#157313=CARTESIAN_POINT('Ctrl Pts',(1.10787520999994,15.2,-11.408714099));
#157314=CARTESIAN_POINT('Ctrl Pts',(1.10657849999994,15.2,-11.412261095));
#157315=CARTESIAN_POINT('Ctrl Pts',(1.10527756399994,15.2,-11.415811262));
#157316=CARTESIAN_POINT('Ctrl Pts',(1.10397239799994,15.2,-11.419364591));
#157317=CARTESIAN_POINT('Ctrl Pts',(1.10266299899994,15.2,-11.422921069));
#157318=CARTESIAN_POINT('Ctrl Pts',(1.10134936299994,15.2,-11.426480691));
#157319=CARTESIAN_POINT('Ctrl Pts',(1.10003148899994,15.2,-11.430043446));
#157320=CARTESIAN_POINT('Ctrl Pts',(1.09870937299994,15.2,-11.433609328));
#157321=CARTESIAN_POINT('Ctrl Pts',(1.09738301599994,15.2,-11.437178335));
#157322=CARTESIAN_POINT('Ctrl Pts',(1.09605241599994,15.2,-11.440750465));
#157323=CARTESIAN_POINT('Ctrl Pts',(1.09498454299994,15.2,-11.443610664));
#157324=CARTESIAN_POINT('Ctrl Pts',(1.09418172899994,15.2,-11.445757219));
#157325=CARTESIAN_POINT('Ctrl Pts',(1.09364566999994,15.2,-11.447188878));
#157326=CARTESIAN_POINT('Ctrl Pts',(1.09337742899994,15.2,-11.447904865));
#157327=CARTESIAN_POINT('Origin',(-5.66257110645729E-14,15.2,-1.77635683940025E-14));
#157328=CARTESIAN_POINT('',(1.76496130699994,15.2,-10.223773109));
#157329=CARTESIAN_POINT('',(1.76496130699994,12.2,-10.223773109));
#157330=CARTESIAN_POINT('',(1.76496130699994,15.2,-10.223773109));
#157331=CARTESIAN_POINT('Origin',(-5.66257110645729E-14,12.2,-1.77635683940025E-14));
#157332=CARTESIAN_POINT('Origin',(-5.66257110645729E-14,15.2,-1.77635683940025E-14));
#157333=CARTESIAN_POINT('Origin',(-5.66257110645729E-14,15.2,-1.77635683940025E-14));
#157334=CARTESIAN_POINT('',(2.33718477799994,15.2,-11.259998548));
#157335=CARTESIAN_POINT('',(2.71145515299994,15.2,-11.175777867));
#157336=CARTESIAN_POINT('Origin',(-5.66257110645729E-14,15.2,-1.77635683940025E-14));
#157337=CARTESIAN_POINT('',(2.71145515299994,12.2,-11.175777867));
#157338=CARTESIAN_POINT('',(2.71145515299994,15.2,-11.175777867));
#157339=CARTESIAN_POINT('',(2.33718477799994,12.2,-11.259998548));
#157340=CARTESIAN_POINT('Origin',(-5.66257110645729E-14,12.2,-1.77635683940025E-14));
#157341=CARTESIAN_POINT('',(2.33718477799994,15.2,-11.259998548));
#157342=CARTESIAN_POINT('Ctrl Pts',(2.71145515299994,15.2,-11.175777867));
#157343=CARTESIAN_POINT('Ctrl Pts',(2.71145515299994,11.6,-11.175777867));
#157344=CARTESIAN_POINT('Ctrl Pts',(2.71161876799995,15.2,-11.175030995));
#157345=CARTESIAN_POINT('Ctrl Pts',(2.71161876799995,11.6,-11.175030995));
#157346=CARTESIAN_POINT('Ctrl Pts',(2.71194562399995,15.2,-11.173537618));
#157347=CARTESIAN_POINT('Ctrl Pts',(2.71194562399995,11.6,-11.173537618));
#157348=CARTESIAN_POINT('Ctrl Pts',(2.71243477999994,15.2,-11.17129866));
#157349=CARTESIAN_POINT('Ctrl Pts',(2.71243477999994,11.6,-11.17129866));
#157350=CARTESIAN_POINT('Ctrl Pts',(2.71308473599994,15.2,-11.168315598));
#157351=CARTESIAN_POINT('Ctrl Pts',(2.71308473599994,11.6,-11.168315598));
#157352=CARTESIAN_POINT('Ctrl Pts',(2.71389342499994,15.2,-11.164590464));
#157353=CARTESIAN_POINT('Ctrl Pts',(2.71389342499994,11.6,-11.164590464));
#157354=CARTESIAN_POINT('Ctrl Pts',(2.71469835899994,15.2,-11.160869024));
#157355=CARTESIAN_POINT('Ctrl Pts',(2.71469835899994,11.6,-11.160869024));
#157356=CARTESIAN_POINT('Ctrl Pts',(2.71549953799994,15.2,-11.15715128));
#157357=CARTESIAN_POINT('Ctrl Pts',(2.71549953799994,11.6,-11.15715128));
#157358=CARTESIAN_POINT('Ctrl Pts',(2.71629696599994,15.2,-11.153437236));
#157359=CARTESIAN_POINT('Ctrl Pts',(2.71629696599994,11.6,-11.153437236));
#157360=CARTESIAN_POINT('Ctrl Pts',(2.71709064399994,15.2,-11.149726897));
#157361=CARTESIAN_POINT('Ctrl Pts',(2.71709064399994,11.6,-11.149726897));
#157362=CARTESIAN_POINT('Ctrl Pts',(2.71788057599994,15.2,-11.146020271));
#157363=CARTESIAN_POINT('Ctrl Pts',(2.71788057599994,11.6,-11.146020271));
#157364=CARTESIAN_POINT('Ctrl Pts',(2.71866676599994,15.2,-11.142317365));
#157365=CARTESIAN_POINT('Ctrl Pts',(2.71866676599994,11.6,-11.142317365));
#157366=CARTESIAN_POINT('Ctrl Pts',(2.71944921799995,15.2,-11.138618191));
#157367=CARTESIAN_POINT('Ctrl Pts',(2.71944921799995,11.6,-11.138618191));
#157368=CARTESIAN_POINT('Ctrl Pts',(2.72022793899994,15.2,-11.134922758));
#157369=CARTESIAN_POINT('Ctrl Pts',(2.72022793899994,11.6,-11.134922758));
#157370=CARTESIAN_POINT('Ctrl Pts',(2.72100293299995,15.2,-11.131231076));
#157371=CARTESIAN_POINT('Ctrl Pts',(2.72100293299995,11.6,-11.131231076));
#157372=CARTESIAN_POINT('Ctrl Pts',(2.72177420399994,15.2,-11.127543154));
#157373=CARTESIAN_POINT('Ctrl Pts',(2.72177420399994,11.6,-11.127543154));
#157374=CARTESIAN_POINT('Ctrl Pts',(2.72254175699994,15.2,-11.123859));
#157375=CARTESIAN_POINT('Ctrl Pts',(2.72254175699994,11.6,-11.123859));
#157376=CARTESIAN_POINT('Ctrl Pts',(2.72330559599995,15.2,-11.120178623));
#157377=CARTESIAN_POINT('Ctrl Pts',(2.72330559599995,11.6,-11.120178623));
#157378=CARTESIAN_POINT('Ctrl Pts',(2.72406572399994,15.2,-11.11650203));
#157379=CARTESIAN_POINT('Ctrl Pts',(2.72406572399994,11.6,-11.11650203));
#157380=CARTESIAN_POINT('Ctrl Pts',(2.72482214499994,15.2,-11.112829226));
#157381=CARTESIAN_POINT('Ctrl Pts',(2.72482214499994,11.6,-11.112829226));
#157382=CARTESIAN_POINT('Ctrl Pts',(2.72557486199994,15.2,-11.109160223));
#157383=CARTESIAN_POINT('Ctrl Pts',(2.72557486199994,11.6,-11.109160223));
#157384=CARTESIAN_POINT('Ctrl Pts',(2.72632387999994,15.2,-11.105495024));
#157385=CARTESIAN_POINT('Ctrl Pts',(2.72632387999994,11.6,-11.105495024));
#157386=CARTESIAN_POINT('Ctrl Pts',(2.72706920299994,15.2,-11.10183364));
#157387=CARTESIAN_POINT('Ctrl Pts',(2.72706920299994,11.6,-11.10183364));
#157388=CARTESIAN_POINT('Ctrl Pts',(2.72781083399994,15.2,-11.098176078));
#157389=CARTESIAN_POINT('Ctrl Pts',(2.72781083399994,11.6,-11.098176078));
#157390=CARTESIAN_POINT('Ctrl Pts',(2.72854877799994,15.2,-11.094522347));
#157391=CARTESIAN_POINT('Ctrl Pts',(2.72854877799994,11.6,-11.094522347));
#157392=CARTESIAN_POINT('Ctrl Pts',(2.72928303999994,15.2,-11.090872455));
#157393=CARTESIAN_POINT('Ctrl Pts',(2.72928303999994,11.6,-11.090872455));
#157394=CARTESIAN_POINT('Ctrl Pts',(2.73001362299994,15.2,-11.087226412));
#157395=CARTESIAN_POINT('Ctrl Pts',(2.73001362299994,11.6,-11.087226412));
#157396=CARTESIAN_POINT('Ctrl Pts',(2.73074053199994,15.2,-11.083584223));
#157397=CARTESIAN_POINT('Ctrl Pts',(2.73074053199994,11.6,-11.083584223));
#157398=CARTESIAN_POINT('Ctrl Pts',(2.73146377099994,15.2,-11.079945899));
#157399=CARTESIAN_POINT('Ctrl Pts',(2.73146377099994,11.6,-11.079945899));
#157400=CARTESIAN_POINT('Ctrl Pts',(2.73218334399994,15.2,-11.076311448));
#157401=CARTESIAN_POINT('Ctrl Pts',(2.73218334399994,11.6,-11.076311448));
#157402=CARTESIAN_POINT('Ctrl Pts',(2.73289925699994,15.2,-11.072680878));
#157403=CARTESIAN_POINT('Ctrl Pts',(2.73289925699994,11.6,-11.072680878));
#157404=CARTESIAN_POINT('Ctrl Pts',(2.73361150999994,15.2,-11.069054196));
#157405=CARTESIAN_POINT('Ctrl Pts',(2.73361150999994,11.6,-11.069054196));
#157406=CARTESIAN_POINT('Ctrl Pts',(2.73432011199994,15.2,-11.06543141));
#157407=CARTESIAN_POINT('Ctrl Pts',(2.73432011199994,11.6,-11.06543141));
#157408=CARTESIAN_POINT('Ctrl Pts',(2.73502506399995,15.2,-11.06181253));
#157409=CARTESIAN_POINT('Ctrl Pts',(2.73502506399995,11.6,-11.06181253));
#157410=CARTESIAN_POINT('Ctrl Pts',(2.73572636999994,15.2,-11.058197563));
#157411=CARTESIAN_POINT('Ctrl Pts',(2.73572636999994,11.6,-11.058197563));
#157412=CARTESIAN_POINT('Ctrl Pts',(2.73642403699994,15.2,-11.054586516));
#157413=CARTESIAN_POINT('Ctrl Pts',(2.73642403699994,11.6,-11.054586516));
#157414=CARTESIAN_POINT('Ctrl Pts',(2.73711806699994,15.2,-11.050979401));
#157415=CARTESIAN_POINT('Ctrl Pts',(2.73711806699994,11.6,-11.050979401));
#157416=CARTESIAN_POINT('Ctrl Pts',(2.73780846499994,15.2,-11.047376223));
#157417=CARTESIAN_POINT('Ctrl Pts',(2.73780846499994,11.6,-11.047376223));
#157418=CARTESIAN_POINT('Ctrl Pts',(2.73849523599994,15.2,-11.043776991));
#157419=CARTESIAN_POINT('Ctrl Pts',(2.73849523599994,11.6,-11.043776991));
#157420=CARTESIAN_POINT('Ctrl Pts',(2.73917838399994,15.2,-11.040181714));
#157421=CARTESIAN_POINT('Ctrl Pts',(2.73917838399994,11.6,-11.040181714));
#157422=CARTESIAN_POINT('Ctrl Pts',(2.73985791299994,15.2,-11.036590401));
#157423=CARTESIAN_POINT('Ctrl Pts',(2.73985791299994,11.6,-11.036590401));
#157424=CARTESIAN_POINT('Ctrl Pts',(2.74053382699994,15.2,-11.033003059));
#157425=CARTESIAN_POINT('Ctrl Pts',(2.74053382699994,11.6,-11.033003059));
#157426=CARTESIAN_POINT('Ctrl Pts',(2.74120613199994,15.2,-11.029419697));
#157427=CARTESIAN_POINT('Ctrl Pts',(2.74120613199994,11.6,-11.029419697));
#157428=CARTESIAN_POINT('Ctrl Pts',(2.74187482999994,15.2,-11.025840322));
#157429=CARTESIAN_POINT('Ctrl Pts',(2.74187482999994,11.6,-11.025840322));
#157430=CARTESIAN_POINT('Ctrl Pts',(2.74253992699995,15.2,-11.022264944));
#157431=CARTESIAN_POINT('Ctrl Pts',(2.74253992699995,11.6,-11.022264944));
#157432=CARTESIAN_POINT('Ctrl Pts',(2.74320142799994,15.2,-11.018693571));
#157433=CARTESIAN_POINT('Ctrl Pts',(2.74320142799994,11.6,-11.018693571));
#157434=CARTESIAN_POINT('Ctrl Pts',(2.74385933599994,15.2,-11.015126211));
#157435=CARTESIAN_POINT('Ctrl Pts',(2.74385933599994,11.6,-11.015126211));
#157436=CARTESIAN_POINT('Ctrl Pts',(2.74451365599994,15.2,-11.011562873));
#157437=CARTESIAN_POINT('Ctrl Pts',(2.74451365599994,11.6,-11.011562873));
#157438=CARTESIAN_POINT('Ctrl Pts',(2.74516439099994,15.2,-11.008003563));
#157439=CARTESIAN_POINT('Ctrl Pts',(2.74516439099994,11.6,-11.008003563));
#157440=CARTESIAN_POINT('Ctrl Pts',(2.74581154899994,15.2,-11.004448293));
#157441=CARTESIAN_POINT('Ctrl Pts',(2.74581154899994,11.6,-11.004448293));
#157442=CARTESIAN_POINT('Ctrl Pts',(2.74645513199994,15.2,-11.00089707));
#157443=CARTESIAN_POINT('Ctrl Pts',(2.74645513199994,11.6,-11.00089707));
#157444=CARTESIAN_POINT('Ctrl Pts',(2.74709514399994,15.2,-10.997349902));
#157445=CARTESIAN_POINT('Ctrl Pts',(2.74709514399994,11.6,-10.997349902));
#157446=CARTESIAN_POINT('Ctrl Pts',(2.74773159199994,15.2,-10.993806797));
#157447=CARTESIAN_POINT('Ctrl Pts',(2.74773159199994,11.6,-10.993806797));
#157448=CARTESIAN_POINT('Ctrl Pts',(2.74836447799994,15.2,-10.990267766));
#157449=CARTESIAN_POINT('Ctrl Pts',(2.74836447799994,11.6,-10.990267766));
#157450=CARTESIAN_POINT('Ctrl Pts',(2.74899380799994,15.2,-10.986732814));
#157451=CARTESIAN_POINT('Ctrl Pts',(2.74899380799994,11.6,-10.986732814));
#157452=CARTESIAN_POINT('Ctrl Pts',(2.74961958599994,15.2,-10.983201952));
#157453=CARTESIAN_POINT('Ctrl Pts',(2.74961958599994,11.6,-10.983201952));
#157454=CARTESIAN_POINT('Ctrl Pts',(2.75024181599994,15.2,-10.979675187));
#157455=CARTESIAN_POINT('Ctrl Pts',(2.75024181599994,11.6,-10.979675187));
#157456=CARTESIAN_POINT('Ctrl Pts',(2.75086050399994,15.2,-10.976152529));
#157457=CARTESIAN_POINT('Ctrl Pts',(2.75086050399994,11.6,-10.976152529));
#157458=CARTESIAN_POINT('Ctrl Pts',(2.75147565299994,15.2,-10.972633984));
#157459=CARTESIAN_POINT('Ctrl Pts',(2.75147565299994,11.6,-10.972633984));
#157460=CARTESIAN_POINT('Ctrl Pts',(2.75208726999994,15.2,-10.969119563));
#157461=CARTESIAN_POINT('Ctrl Pts',(2.75208726999994,11.6,-10.969119563));
#157462=CARTESIAN_POINT('Ctrl Pts',(2.75269535799994,15.2,-10.965609275));
#157463=CARTESIAN_POINT('Ctrl Pts',(2.75269535799994,11.6,-10.965609275));
#157464=CARTESIAN_POINT('Ctrl Pts',(2.75329991999994,15.2,-10.962103125));
#157465=CARTESIAN_POINT('Ctrl Pts',(2.75329991999994,11.6,-10.962103125));
#157466=CARTESIAN_POINT('Ctrl Pts',(2.75390096499994,15.2,-10.958601125));
#157467=CARTESIAN_POINT('Ctrl Pts',(2.75390096499994,11.6,-10.958601125));
#157468=CARTESIAN_POINT('Ctrl Pts',(2.75449849399994,15.2,-10.955103283));
#157469=CARTESIAN_POINT('Ctrl Pts',(2.75449849399994,11.6,-10.955103283));
#157470=CARTESIAN_POINT('Ctrl Pts',(2.75509251299995,15.2,-10.951609607));
#157471=CARTESIAN_POINT('Ctrl Pts',(2.75509251299995,11.6,-10.951609607));
#157472=CARTESIAN_POINT('Ctrl Pts',(2.75568302799994,15.2,-10.948120104));
#157473=CARTESIAN_POINT('Ctrl Pts',(2.75568302799994,11.6,-10.948120104));
#157474=CARTESIAN_POINT('Ctrl Pts',(2.75627004099994,15.2,-10.944634786));
#157475=CARTESIAN_POINT('Ctrl Pts',(2.75627004099994,11.6,-10.944634786));
#157476=CARTESIAN_POINT('Ctrl Pts',(2.75685355899994,15.2,-10.941153659));
#157477=CARTESIAN_POINT('Ctrl Pts',(2.75685355899994,11.6,-10.941153659));
#157478=CARTESIAN_POINT('Ctrl Pts',(2.75743358399994,15.2,-10.937676732));
#157479=CARTESIAN_POINT('Ctrl Pts',(2.75743358399994,11.6,-10.937676732));
#157480=CARTESIAN_POINT('Ctrl Pts',(2.75801012499994,15.2,-10.934204015));
#157481=CARTESIAN_POINT('Ctrl Pts',(2.75801012499994,11.6,-10.934204015));
#157482=CARTESIAN_POINT('Ctrl Pts',(2.75858318399994,15.2,-10.930735515));
#157483=CARTESIAN_POINT('Ctrl Pts',(2.75858318399994,11.6,-10.930735515));
#157484=CARTESIAN_POINT('Ctrl Pts',(2.75915276499994,15.2,-10.927271242));
#157485=CARTESIAN_POINT('Ctrl Pts',(2.75915276499994,11.6,-10.927271242));
#157486=CARTESIAN_POINT('Ctrl Pts',(2.75971887499994,15.2,-10.923811204));
#157487=CARTESIAN_POINT('Ctrl Pts',(2.75971887499994,11.6,-10.923811204));
#157488=CARTESIAN_POINT('Ctrl Pts',(2.76028151899995,15.2,-10.92035541));
#157489=CARTESIAN_POINT('Ctrl Pts',(2.76028151899995,11.6,-10.92035541));
#157490=CARTESIAN_POINT('Ctrl Pts',(2.76084070099994,15.2,-10.916903868));
#157491=CARTESIAN_POINT('Ctrl Pts',(2.76084070099994,11.6,-10.916903868));
#157492=CARTESIAN_POINT('Ctrl Pts',(2.76139642499994,15.2,-10.913456588));
#157493=CARTESIAN_POINT('Ctrl Pts',(2.76139642499994,11.6,-10.913456588));
#157494=CARTESIAN_POINT('Ctrl Pts',(2.76194869599995,15.2,-10.910013578));
#157495=CARTESIAN_POINT('Ctrl Pts',(2.76194869599995,11.6,-10.910013578));
#157496=CARTESIAN_POINT('Ctrl Pts',(2.76249751999994,15.2,-10.906574846));
#157497=CARTESIAN_POINT('Ctrl Pts',(2.76249751999994,11.6,-10.906574846));
#157498=CARTESIAN_POINT('Ctrl Pts',(2.76304290199994,15.2,-10.903140401));
#157499=CARTESIAN_POINT('Ctrl Pts',(2.76304290199994,11.6,-10.903140401));
#157500=CARTESIAN_POINT('Ctrl Pts',(2.76358484599994,15.2,-10.899710254));
#157501=CARTESIAN_POINT('Ctrl Pts',(2.76358484599994,11.6,-10.899710254));
#157502=CARTESIAN_POINT('Ctrl Pts',(2.76412335699994,15.2,-10.896284411));
#157503=CARTESIAN_POINT('Ctrl Pts',(2.76412335699994,11.6,-10.896284411));
#157504=CARTESIAN_POINT('Ctrl Pts',(2.76465844099994,15.2,-10.892862882));
#157505=CARTESIAN_POINT('Ctrl Pts',(2.76465844099994,11.6,-10.892862882));
#157506=CARTESIAN_POINT('Ctrl Pts',(2.76519010299995,15.2,-10.889445675));
#157507=CARTESIAN_POINT('Ctrl Pts',(2.76519010299995,11.6,-10.889445675));
#157508=CARTESIAN_POINT('Ctrl Pts',(2.76571834699994,15.2,-10.8860328));
#157509=CARTESIAN_POINT('Ctrl Pts',(2.76571834699994,11.6,-10.8860328));
#157510=CARTESIAN_POINT('Ctrl Pts',(2.76624317799994,15.2,-10.882624265));
#157511=CARTESIAN_POINT('Ctrl Pts',(2.76624317799994,11.6,-10.882624265));
#157512=CARTESIAN_POINT('Ctrl Pts',(2.76676460199994,15.2,-10.87922008));
#157513=CARTESIAN_POINT('Ctrl Pts',(2.76676460199994,11.6,-10.87922008));
#157514=CARTESIAN_POINT('Ctrl Pts',(2.76728262299994,15.2,-10.875820251));
#157515=CARTESIAN_POINT('Ctrl Pts',(2.76728262299994,11.6,-10.875820251));
#157516=CARTESIAN_POINT('Ctrl Pts',(2.76779724699994,15.2,-10.872424791));
#157517=CARTESIAN_POINT('Ctrl Pts',(2.76779724699994,11.6,-10.872424791));
#157518=CARTESIAN_POINT('Ctrl Pts',(2.76830847799994,15.2,-10.869033706));
#157519=CARTESIAN_POINT('Ctrl Pts',(2.76830847799994,11.6,-10.869033706));
#157520=CARTESIAN_POINT('Ctrl Pts',(2.76881632299995,15.2,-10.865647005));
#157521=CARTESIAN_POINT('Ctrl Pts',(2.76881632299995,11.6,-10.865647005));
#157522=CARTESIAN_POINT('Ctrl Pts',(2.76932078499994,15.2,-10.862264698));
#157523=CARTESIAN_POINT('Ctrl Pts',(2.76932078499994,11.6,-10.862264698));
#157524=CARTESIAN_POINT('Ctrl Pts',(2.76982187099994,15.2,-10.858886794));
#157525=CARTESIAN_POINT('Ctrl Pts',(2.76982187099994,11.6,-10.858886794));
#157526=CARTESIAN_POINT('Ctrl Pts',(2.77031958499995,15.2,-10.8555133));
#157527=CARTESIAN_POINT('Ctrl Pts',(2.77031958499995,11.6,-10.8555133));
#157528=CARTESIAN_POINT('Ctrl Pts',(2.77081393199994,15.2,-10.852144228));
#157529=CARTESIAN_POINT('Ctrl Pts',(2.77081393199994,11.6,-10.852144228));
#157530=CARTESIAN_POINT('Ctrl Pts',(2.77130491799995,15.2,-10.848779584));
#157531=CARTESIAN_POINT('Ctrl Pts',(2.77130491799995,11.6,-10.848779584));
#157532=CARTESIAN_POINT('Ctrl Pts',(2.77179254699994,15.2,-10.845419378));
#157533=CARTESIAN_POINT('Ctrl Pts',(2.77179254699994,11.6,-10.845419378));
#157534=CARTESIAN_POINT('Ctrl Pts',(2.77227682599994,15.2,-10.84206362));
#157535=CARTESIAN_POINT('Ctrl Pts',(2.77227682599994,11.6,-10.84206362));
#157536=CARTESIAN_POINT('Ctrl Pts',(2.77275775999994,15.2,-10.838712319));
#157537=CARTESIAN_POINT('Ctrl Pts',(2.77275775999994,11.6,-10.838712319));
#157538=CARTESIAN_POINT('Ctrl Pts',(2.77323535199994,15.2,-10.835365482));
#157539=CARTESIAN_POINT('Ctrl Pts',(2.77323535199994,11.6,-10.835365482));
#157540=CARTESIAN_POINT('Ctrl Pts',(2.77370960899994,15.2,-10.83202312));
#157541=CARTESIAN_POINT('Ctrl Pts',(2.77370960899994,11.6,-10.83202312));
#157542=CARTESIAN_POINT('Ctrl Pts',(2.77418053799994,15.2,-10.828685241));
#157543=CARTESIAN_POINT('Ctrl Pts',(2.77418053799994,11.6,-10.828685241));
#157544=CARTESIAN_POINT('Ctrl Pts',(2.77464813999994,15.2,-10.825351854));
#157545=CARTESIAN_POINT('Ctrl Pts',(2.77464813999994,11.6,-10.825351854));
#157546=CARTESIAN_POINT('Ctrl Pts',(2.77511242499994,15.2,-10.822022969));
#157547=CARTESIAN_POINT('Ctrl Pts',(2.77511242499994,11.6,-10.822022969));
#157548=CARTESIAN_POINT('Ctrl Pts',(2.77557339499995,15.2,-10.818698595));
#157549=CARTESIAN_POINT('Ctrl Pts',(2.77557339499995,11.6,-10.818698595));
#157550=CARTESIAN_POINT('Ctrl Pts',(2.77603105699994,15.2,-10.815378739));
#157551=CARTESIAN_POINT('Ctrl Pts',(2.77603105699994,11.6,-10.815378739));
#157552=CARTESIAN_POINT('Ctrl Pts',(2.77648541599994,15.2,-10.812063413));
#157553=CARTESIAN_POINT('Ctrl Pts',(2.77648541599994,11.6,-10.812063413));
#157554=CARTESIAN_POINT('Ctrl Pts',(2.77693647799994,15.2,-10.808752624));
#157555=CARTESIAN_POINT('Ctrl Pts',(2.77693647799994,11.6,-10.808752624));
#157556=CARTESIAN_POINT('Ctrl Pts',(2.77738424599994,15.2,-10.805446382));
#157557=CARTESIAN_POINT('Ctrl Pts',(2.77738424599994,11.6,-10.805446382));
#157558=CARTESIAN_POINT('Ctrl Pts',(2.77782872899994,15.2,-10.802144697));
#157559=CARTESIAN_POINT('Ctrl Pts',(2.77782872899994,11.6,-10.802144697));
#157560=CARTESIAN_POINT('Ctrl Pts',(2.77826992999994,15.2,-10.798847577));
#157561=CARTESIAN_POINT('Ctrl Pts',(2.77826992999994,11.6,-10.798847577));
#157562=CARTESIAN_POINT('Ctrl Pts',(2.77870785499994,15.2,-10.795555031));
#157563=CARTESIAN_POINT('Ctrl Pts',(2.77870785499994,11.6,-10.795555031));
#157564=CARTESIAN_POINT('Ctrl Pts',(2.77914250899994,15.2,-10.792267068));
#157565=CARTESIAN_POINT('Ctrl Pts',(2.77914250899994,11.6,-10.792267068));
#157566=CARTESIAN_POINT('Ctrl Pts',(2.77957389999994,15.2,-10.788983698));
#157567=CARTESIAN_POINT('Ctrl Pts',(2.77957389999994,11.6,-10.788983698));
#157568=CARTESIAN_POINT('Ctrl Pts',(2.78000203099994,15.2,-10.785704931));
#157569=CARTESIAN_POINT('Ctrl Pts',(2.78000203099994,11.6,-10.785704931));
#157570=CARTESIAN_POINT('Ctrl Pts',(2.78042690799994,15.2,-10.782430775));
#157571=CARTESIAN_POINT('Ctrl Pts',(2.78042690799994,11.6,-10.782430775));
#157572=CARTESIAN_POINT('Ctrl Pts',(2.78084853699994,15.2,-10.779161239));
#157573=CARTESIAN_POINT('Ctrl Pts',(2.78084853699994,11.6,-10.779161239));
#157574=CARTESIAN_POINT('Ctrl Pts',(2.78126692299994,15.2,-10.775896332));
#157575=CARTESIAN_POINT('Ctrl Pts',(2.78126692299994,11.6,-10.775896332));
#157576=CARTESIAN_POINT('Ctrl Pts',(2.78168207299994,15.2,-10.772636066));
#157577=CARTESIAN_POINT('Ctrl Pts',(2.78168207299994,11.6,-10.772636066));
#157578=CARTESIAN_POINT('Ctrl Pts',(2.78209398999994,15.2,-10.769380447));
#157579=CARTESIAN_POINT('Ctrl Pts',(2.78209398999994,11.6,-10.769380447));
#157580=CARTESIAN_POINT('Ctrl Pts',(2.78250268299994,15.2,-10.766129486));
#157581=CARTESIAN_POINT('Ctrl Pts',(2.78250268299994,11.6,-10.766129486));
#157582=CARTESIAN_POINT('Ctrl Pts',(2.78290815499994,15.2,-10.762883192));
#157583=CARTESIAN_POINT('Ctrl Pts',(2.78290815499994,11.6,-10.762883192));
#157584=CARTESIAN_POINT('Ctrl Pts',(2.78331041399994,15.2,-10.759641574));
#157585=CARTESIAN_POINT('Ctrl Pts',(2.78331041399994,11.6,-10.759641574));
#157586=CARTESIAN_POINT('Ctrl Pts',(2.78370946199994,15.2,-10.756404642));
#157587=CARTESIAN_POINT('Ctrl Pts',(2.78370946199994,11.6,-10.756404642));
#157588=CARTESIAN_POINT('Ctrl Pts',(2.78410530899994,15.2,-10.753172404));
#157589=CARTESIAN_POINT('Ctrl Pts',(2.78410530899994,11.6,-10.753172404));
#157590=CARTESIAN_POINT('Ctrl Pts',(2.78449795899995,15.2,-10.74994487));
#157591=CARTESIAN_POINT('Ctrl Pts',(2.78449795899995,11.6,-10.74994487));
#157592=CARTESIAN_POINT('Ctrl Pts',(2.78488741699995,15.2,-10.746722051));
#157593=CARTESIAN_POINT('Ctrl Pts',(2.78488741699995,11.6,-10.746722051));
#157594=CARTESIAN_POINT('Ctrl Pts',(2.78527368899995,15.2,-10.743503955));
#157595=CARTESIAN_POINT('Ctrl Pts',(2.78527368899995,11.6,-10.743503955));
#157596=CARTESIAN_POINT('Ctrl Pts',(2.78565678099994,15.2,-10.740290592));
#157597=CARTESIAN_POINT('Ctrl Pts',(2.78565678099994,11.6,-10.740290592));
#157598=CARTESIAN_POINT('Ctrl Pts',(2.78603669999994,15.2,-10.737081969));
#157599=CARTESIAN_POINT('Ctrl Pts',(2.78603669999994,11.6,-10.737081969));
#157600=CARTESIAN_POINT('Ctrl Pts',(2.78641344899994,15.2,-10.733878099));
#157601=CARTESIAN_POINT('Ctrl Pts',(2.78641344899994,11.6,-10.733878099));
#157602=CARTESIAN_POINT('Ctrl Pts',(2.78678703799994,15.2,-10.73067899));
#157603=CARTESIAN_POINT('Ctrl Pts',(2.78678703799994,11.6,-10.73067899));
#157604=CARTESIAN_POINT('Ctrl Pts',(2.78715746899994,15.2,-10.72748465));
#157605=CARTESIAN_POINT('Ctrl Pts',(2.78715746899994,11.6,-10.72748465));
#157606=CARTESIAN_POINT('Ctrl Pts',(2.78752474999994,15.2,-10.724295091));
#157607=CARTESIAN_POINT('Ctrl Pts',(2.78752474999994,11.6,-10.724295091));
#157608=CARTESIAN_POINT('Ctrl Pts',(2.78788888599995,15.2,-10.721110321));
#157609=CARTESIAN_POINT('Ctrl Pts',(2.78788888599995,11.6,-10.721110321));
#157610=CARTESIAN_POINT('Ctrl Pts',(2.78824988299994,15.2,-10.71793035));
#157611=CARTESIAN_POINT('Ctrl Pts',(2.78824988299994,11.6,-10.71793035));
#157612=CARTESIAN_POINT('Ctrl Pts',(2.78860774899994,15.2,-10.714755187));
#157613=CARTESIAN_POINT('Ctrl Pts',(2.78860774899994,11.6,-10.714755187));
#157614=CARTESIAN_POINT('Ctrl Pts',(2.78896248599994,15.2,-10.711584842));
#157615=CARTESIAN_POINT('Ctrl Pts',(2.78896248599994,11.6,-10.711584842));
#157616=CARTESIAN_POINT('Ctrl Pts',(2.78931410399994,15.2,-10.708419325));
#157617=CARTESIAN_POINT('Ctrl Pts',(2.78931410399994,11.6,-10.708419325));
#157618=CARTESIAN_POINT('Ctrl Pts',(2.78966260699994,15.2,-10.705258645));
#157619=CARTESIAN_POINT('Ctrl Pts',(2.78966260699994,11.6,-10.705258645));
#157620=CARTESIAN_POINT('Ctrl Pts',(2.79000799999995,15.2,-10.702102811));
#157621=CARTESIAN_POINT('Ctrl Pts',(2.79000799999995,11.6,-10.702102811));
#157622=CARTESIAN_POINT('Ctrl Pts',(2.79035029199994,15.2,-10.698951833));
#157623=CARTESIAN_POINT('Ctrl Pts',(2.79035029199994,11.6,-10.698951833));
#157624=CARTESIAN_POINT('Ctrl Pts',(2.79068948599994,15.2,-10.695805722));
#157625=CARTESIAN_POINT('Ctrl Pts',(2.79068948599994,11.6,-10.695805722));
#157626=CARTESIAN_POINT('Ctrl Pts',(2.79102558999994,15.2,-10.692664486));
#157627=CARTESIAN_POINT('Ctrl Pts',(2.79102558999994,11.6,-10.692664486));
#157628=CARTESIAN_POINT('Ctrl Pts',(2.79135860899994,15.2,-10.689528135));
#157629=CARTESIAN_POINT('Ctrl Pts',(2.79135860899994,11.6,-10.689528135));
#157630=CARTESIAN_POINT('Ctrl Pts',(2.79168855099994,15.2,-10.686396679));
#157631=CARTESIAN_POINT('Ctrl Pts',(2.79168855099994,11.6,-10.686396679));
#157632=CARTESIAN_POINT('Ctrl Pts',(2.79201541999994,15.2,-10.683270128));
#157633=CARTESIAN_POINT('Ctrl Pts',(2.79201541999994,11.6,-10.683270128));
#157634=CARTESIAN_POINT('Ctrl Pts',(2.79233922299994,15.2,-10.680148491));
#157635=CARTESIAN_POINT('Ctrl Pts',(2.79233922299994,11.6,-10.680148491));
#157636=CARTESIAN_POINT('Ctrl Pts',(2.79265996699994,15.2,-10.677031779));
#157637=CARTESIAN_POINT('Ctrl Pts',(2.79265996699994,11.6,-10.677031779));
#157638=CARTESIAN_POINT('Ctrl Pts',(2.79297765699994,15.2,-10.673919999));
#157639=CARTESIAN_POINT('Ctrl Pts',(2.79297765699994,11.6,-10.673919999));
#157640=CARTESIAN_POINT('Ctrl Pts',(2.79329229999994,15.2,-10.670813164));
#157641=CARTESIAN_POINT('Ctrl Pts',(2.79329229999994,11.6,-10.670813164));
#157642=CARTESIAN_POINT('Ctrl Pts',(2.79360390099994,15.2,-10.667711281));
#157643=CARTESIAN_POINT('Ctrl Pts',(2.79360390099994,11.6,-10.667711281));
#157644=CARTESIAN_POINT('Ctrl Pts',(2.79391246799995,15.2,-10.664614362));
#157645=CARTESIAN_POINT('Ctrl Pts',(2.79391246799995,11.6,-10.664614362));
#157646=CARTESIAN_POINT('Ctrl Pts',(2.79421800799994,15.2,-10.661522415));
#157647=CARTESIAN_POINT('Ctrl Pts',(2.79421800799994,11.6,-10.661522415));
#157648=CARTESIAN_POINT('Ctrl Pts',(2.79452052399995,15.2,-10.658435452));
#157649=CARTESIAN_POINT('Ctrl Pts',(2.79452052399995,11.6,-10.658435452));
#157650=CARTESIAN_POINT('Ctrl Pts',(2.79482002399994,15.2,-10.65535348));
#157651=CARTESIAN_POINT('Ctrl Pts',(2.79482002399994,11.6,-10.65535348));
#157652=CARTESIAN_POINT('Ctrl Pts',(2.79511651699994,15.2,-10.652276511));
#157653=CARTESIAN_POINT('Ctrl Pts',(2.79511651699994,11.6,-10.652276511));
#157654=CARTESIAN_POINT('Ctrl Pts',(2.79541000499994,15.2,-10.649204554));
#157655=CARTESIAN_POINT('Ctrl Pts',(2.79541000499994,11.6,-10.649204554));
#157656=CARTESIAN_POINT('Ctrl Pts',(2.79570049699994,15.2,-10.646137621));
#157657=CARTESIAN_POINT('Ctrl Pts',(2.79570049699994,11.6,-10.646137621));
#157658=CARTESIAN_POINT('Ctrl Pts',(2.79598799899994,15.2,-10.643075718));
#157659=CARTESIAN_POINT('Ctrl Pts',(2.79598799899994,11.6,-10.643075718));
#157660=CARTESIAN_POINT('Ctrl Pts',(2.79627251799994,15.2,-10.640018857));
#157661=CARTESIAN_POINT('Ctrl Pts',(2.79627251799994,11.6,-10.640018857));
#157662=CARTESIAN_POINT('Ctrl Pts',(2.79655405799994,15.2,-10.636967048));
#157663=CARTESIAN_POINT('Ctrl Pts',(2.79655405799994,11.6,-10.636967048));
#157664=CARTESIAN_POINT('Ctrl Pts',(2.79683262799994,15.2,-10.633920301));
#157665=CARTESIAN_POINT('Ctrl Pts',(2.79683262799994,11.6,-10.633920301));
#157666=CARTESIAN_POINT('Ctrl Pts',(2.79710823499994,15.2,-10.630878627));
#157667=CARTESIAN_POINT('Ctrl Pts',(2.79710823499994,11.6,-10.630878627));
#157668=CARTESIAN_POINT('Ctrl Pts',(2.79738088299994,15.2,-10.627842034));
#157669=CARTESIAN_POINT('Ctrl Pts',(2.79738088299994,11.6,-10.627842034));
#157670=CARTESIAN_POINT('Ctrl Pts',(2.79765057999994,15.2,-10.624810532));
#157671=CARTESIAN_POINT('Ctrl Pts',(2.79765057999994,11.6,-10.624810532));
#157672=CARTESIAN_POINT('Ctrl Pts',(2.79791733399994,15.2,-10.621784132));
#157673=CARTESIAN_POINT('Ctrl Pts',(2.79791733399994,11.6,-10.621784132));
#157674=CARTESIAN_POINT('Ctrl Pts',(2.79818114799995,15.2,-10.618762844));
#157675=CARTESIAN_POINT('Ctrl Pts',(2.79818114799995,11.6,-10.618762844));
#157676=CARTESIAN_POINT('Ctrl Pts',(2.79844203199994,15.2,-10.615746678));
#157677=CARTESIAN_POINT('Ctrl Pts',(2.79844203199994,11.6,-10.615746678));
#157678=CARTESIAN_POINT('Ctrl Pts',(2.79869999199994,15.2,-10.612735644));
#157679=CARTESIAN_POINT('Ctrl Pts',(2.79869999199994,11.6,-10.612735644));
#157680=CARTESIAN_POINT('Ctrl Pts',(2.79895503299994,15.2,-10.609729752));
#157681=CARTESIAN_POINT('Ctrl Pts',(2.79895503299994,11.6,-10.609729752));
#157682=CARTESIAN_POINT('Ctrl Pts',(2.79920716299995,15.2,-10.606729012));
#157683=CARTESIAN_POINT('Ctrl Pts',(2.79920716299995,11.6,-10.606729012));
#157684=CARTESIAN_POINT('Ctrl Pts',(2.79945638899994,15.2,-10.603733434));
#157685=CARTESIAN_POINT('Ctrl Pts',(2.79945638899994,11.6,-10.603733434));
#157686=CARTESIAN_POINT('Ctrl Pts',(2.79970271699994,15.2,-10.60074303));
#157687=CARTESIAN_POINT('Ctrl Pts',(2.79970271699994,11.6,-10.60074303));
#157688=CARTESIAN_POINT('Ctrl Pts',(2.79994615399994,15.2,-10.597757808));
#157689=CARTESIAN_POINT('Ctrl Pts',(2.79994615399994,11.6,-10.597757808));
#157690=CARTESIAN_POINT('Ctrl Pts',(2.80018670699994,15.2,-10.594777778));
#157691=CARTESIAN_POINT('Ctrl Pts',(2.80018670699994,11.6,-10.594777778));
#157692=CARTESIAN_POINT('Ctrl Pts',(2.80042438199994,15.2,-10.591802951));
#157693=CARTESIAN_POINT('Ctrl Pts',(2.80042438199994,11.6,-10.591802951));
#157694=CARTESIAN_POINT('Ctrl Pts',(2.80065918599994,15.2,-10.588833338));
#157695=CARTESIAN_POINT('Ctrl Pts',(2.80065918599994,11.6,-10.588833338));
#157696=CARTESIAN_POINT('Ctrl Pts',(2.80089112799994,15.2,-10.585868947));
#157697=CARTESIAN_POINT('Ctrl Pts',(2.80089112799994,11.6,-10.585868947));
#157698=CARTESIAN_POINT('Ctrl Pts',(2.80112021199994,15.2,-10.582909791));
#157699=CARTESIAN_POINT('Ctrl Pts',(2.80112021199994,11.6,-10.582909791));
#157700=CARTESIAN_POINT('Ctrl Pts',(2.80134644599995,15.2,-10.579955879));
#157701=CARTESIAN_POINT('Ctrl Pts',(2.80134644599995,11.6,-10.579955879));
#157702=CARTESIAN_POINT('Ctrl Pts',(2.80156983799994,15.2,-10.57700722));
#157703=CARTESIAN_POINT('Ctrl Pts',(2.80156983799994,11.6,-10.57700722));
#157704=CARTESIAN_POINT('Ctrl Pts',(2.80179039399994,15.2,-10.574063826));
#157705=CARTESIAN_POINT('Ctrl Pts',(2.80179039399994,11.6,-10.574063826));
#157706=CARTESIAN_POINT('Ctrl Pts',(2.80200812099995,15.2,-10.571125707));
#157707=CARTESIAN_POINT('Ctrl Pts',(2.80200812099995,11.6,-10.571125707));
#157708=CARTESIAN_POINT('Ctrl Pts',(2.80222302499994,15.2,-10.568192873));
#157709=CARTESIAN_POINT('Ctrl Pts',(2.80222302499994,11.6,-10.568192873));
#157710=CARTESIAN_POINT('Ctrl Pts',(2.80243511399994,15.2,-10.565265335));
#157711=CARTESIAN_POINT('Ctrl Pts',(2.80243511399994,11.6,-10.565265335));
#157712=CARTESIAN_POINT('Ctrl Pts',(2.80264439599994,15.2,-10.562343102));
#157713=CARTESIAN_POINT('Ctrl Pts',(2.80264439599994,11.6,-10.562343102));
#157714=CARTESIAN_POINT('Ctrl Pts',(2.80285087799995,15.2,-10.559426187));
#157715=CARTESIAN_POINT('Ctrl Pts',(2.80285087799995,11.6,-10.559426187));
#157716=CARTESIAN_POINT('Ctrl Pts',(2.80305456399994,15.2,-10.556514598));
#157717=CARTESIAN_POINT('Ctrl Pts',(2.80305456399994,11.6,-10.556514598));
#157718=CARTESIAN_POINT('Ctrl Pts',(2.80325546499995,15.2,-10.553608345));
#157719=CARTESIAN_POINT('Ctrl Pts',(2.80325546499995,11.6,-10.553608345));
#157720=CARTESIAN_POINT('Ctrl Pts',(2.80345358699994,15.2,-10.550707441));
#157721=CARTESIAN_POINT('Ctrl Pts',(2.80345358699994,11.6,-10.550707441));
#157722=CARTESIAN_POINT('Ctrl Pts',(2.80364893499994,15.2,-10.547811895));
#157723=CARTESIAN_POINT('Ctrl Pts',(2.80364893499994,11.6,-10.547811895));
#157724=CARTESIAN_POINT('Ctrl Pts',(2.80384151799994,15.2,-10.544921716));
#157725=CARTESIAN_POINT('Ctrl Pts',(2.80384151799994,11.6,-10.544921716));
#157726=CARTESIAN_POINT('Ctrl Pts',(2.80403134499994,15.2,-10.542036918));
#157727=CARTESIAN_POINT('Ctrl Pts',(2.80403134499994,11.6,-10.542036918));
#157728=CARTESIAN_POINT('Ctrl Pts',(2.80421841999994,15.2,-10.539157509));
#157729=CARTESIAN_POINT('Ctrl Pts',(2.80421841999994,11.6,-10.539157509));
#157730=CARTESIAN_POINT('Ctrl Pts',(2.80440275199994,15.2,-10.5362835));
#157731=CARTESIAN_POINT('Ctrl Pts',(2.80440275199994,11.6,-10.5362835));
#157732=CARTESIAN_POINT('Ctrl Pts',(2.80458434799994,15.2,-10.533414902));
#157733=CARTESIAN_POINT('Ctrl Pts',(2.80458434799994,11.6,-10.533414902));
#157734=CARTESIAN_POINT('Ctrl Pts',(2.80476321499994,15.2,-10.530551725));
#157735=CARTESIAN_POINT('Ctrl Pts',(2.80476321499994,11.6,-10.530551725));
#157736=CARTESIAN_POINT('Ctrl Pts',(2.80493936099994,15.2,-10.52769398));
#157737=CARTESIAN_POINT('Ctrl Pts',(2.80493936099994,11.6,-10.52769398));
#157738=CARTESIAN_POINT('Ctrl Pts',(2.80511279299994,15.2,-10.524841678));
#157739=CARTESIAN_POINT('Ctrl Pts',(2.80511279299994,11.6,-10.524841678));
#157740=CARTESIAN_POINT('Ctrl Pts',(2.80528351799994,15.2,-10.521994829));
#157741=CARTESIAN_POINT('Ctrl Pts',(2.80528351799994,11.6,-10.521994829));
#157742=CARTESIAN_POINT('Ctrl Pts',(2.80545154499994,15.2,-10.519153444));
#157743=CARTESIAN_POINT('Ctrl Pts',(2.80545154499994,11.6,-10.519153444));
#157744=CARTESIAN_POINT('Ctrl Pts',(2.80561687899994,15.2,-10.516317533));
#157745=CARTESIAN_POINT('Ctrl Pts',(2.80561687899994,11.6,-10.516317533));
#157746=CARTESIAN_POINT('Ctrl Pts',(2.80577952899994,15.2,-10.513487108));
#157747=CARTESIAN_POINT('Ctrl Pts',(2.80577952899994,11.6,-10.513487108));
#157748=CARTESIAN_POINT('Ctrl Pts',(2.80593950199994,15.2,-10.510662179));
#157749=CARTESIAN_POINT('Ctrl Pts',(2.80593950199994,11.6,-10.510662179));
#157750=CARTESIAN_POINT('Ctrl Pts',(2.80609680699994,15.2,-10.507842756));
#157751=CARTESIAN_POINT('Ctrl Pts',(2.80609680699994,11.6,-10.507842756));
#157752=CARTESIAN_POINT('Ctrl Pts',(2.80625144999994,15.2,-10.505028852));
#157753=CARTESIAN_POINT('Ctrl Pts',(2.80625144999994,11.6,-10.505028852));
#157754=CARTESIAN_POINT('Ctrl Pts',(2.80640343799994,15.2,-10.502220475));
#157755=CARTESIAN_POINT('Ctrl Pts',(2.80640343799994,11.6,-10.502220475));
#157756=CARTESIAN_POINT('Ctrl Pts',(2.80655278099994,15.2,-10.499417637));
#157757=CARTESIAN_POINT('Ctrl Pts',(2.80655278099994,11.6,-10.499417637));
#157758=CARTESIAN_POINT('Ctrl Pts',(2.80669948499995,15.2,-10.49662035));
#157759=CARTESIAN_POINT('Ctrl Pts',(2.80669948499995,11.6,-10.49662035));
#157760=CARTESIAN_POINT('Ctrl Pts',(2.80684355699994,15.2,-10.493828624));
#157761=CARTESIAN_POINT('Ctrl Pts',(2.80684355699994,11.6,-10.493828624));
#157762=CARTESIAN_POINT('Ctrl Pts',(2.80698500599994,15.2,-10.491042469));
#157763=CARTESIAN_POINT('Ctrl Pts',(2.80698500599994,11.6,-10.491042469));
#157764=CARTESIAN_POINT('Ctrl Pts',(2.80712383899994,15.2,-10.488261896));
#157765=CARTESIAN_POINT('Ctrl Pts',(2.80712383899994,11.6,-10.488261896));
#157766=CARTESIAN_POINT('Ctrl Pts',(2.80726006499994,15.2,-10.485486918));
#157767=CARTESIAN_POINT('Ctrl Pts',(2.80726006499994,11.6,-10.485486918));
#157768=CARTESIAN_POINT('Ctrl Pts',(2.80739368899994,15.2,-10.482717544));
#157769=CARTESIAN_POINT('Ctrl Pts',(2.80739368899994,11.6,-10.482717544));
#157770=CARTESIAN_POINT('Ctrl Pts',(2.80752472199994,15.2,-10.479953785));
#157771=CARTESIAN_POINT('Ctrl Pts',(2.80752472199994,11.6,-10.479953785));
#157772=CARTESIAN_POINT('Ctrl Pts',(2.80765316999994,15.2,-10.477195652));
#157773=CARTESIAN_POINT('Ctrl Pts',(2.80765316999994,11.6,-10.477195652));
#157774=CARTESIAN_POINT('Ctrl Pts',(2.80777904199994,15.2,-10.474443157));
#157775=CARTESIAN_POINT('Ctrl Pts',(2.80777904199994,11.6,-10.474443157));
#157776=CARTESIAN_POINT('Ctrl Pts',(2.80790234399994,15.2,-10.471696311));
#157777=CARTESIAN_POINT('Ctrl Pts',(2.80790234399994,11.6,-10.471696311));
#157778=CARTESIAN_POINT('Ctrl Pts',(2.80802308699994,15.2,-10.468955124));
#157779=CARTESIAN_POINT('Ctrl Pts',(2.80802308699994,11.6,-10.468955124));
#157780=CARTESIAN_POINT('Ctrl Pts',(2.80814127599994,15.2,-10.466219607));
#157781=CARTESIAN_POINT('Ctrl Pts',(2.80814127599994,11.6,-10.466219607));
#157782=CARTESIAN_POINT('Ctrl Pts',(2.80825691899994,15.2,-10.463489771));
#157783=CARTESIAN_POINT('Ctrl Pts',(2.80825691899994,11.6,-10.463489771));
#157784=CARTESIAN_POINT('Ctrl Pts',(2.80837002599994,15.2,-10.460765629));
#157785=CARTESIAN_POINT('Ctrl Pts',(2.80837002599994,11.6,-10.460765629));
#157786=CARTESIAN_POINT('Ctrl Pts',(2.80848060399994,15.2,-10.458047191));
#157787=CARTESIAN_POINT('Ctrl Pts',(2.80848060399994,11.6,-10.458047191));
#157788=CARTESIAN_POINT('Ctrl Pts',(2.80858866099994,15.2,-10.455334468));
#157789=CARTESIAN_POINT('Ctrl Pts',(2.80858866099994,11.6,-10.455334468));
#157790=CARTESIAN_POINT('Ctrl Pts',(2.80869420399994,15.2,-10.45262747));
#157791=CARTESIAN_POINT('Ctrl Pts',(2.80869420399994,11.6,-10.45262747));
#157792=CARTESIAN_POINT('Ctrl Pts',(2.80879724399994,15.2,-10.44992621));
#157793=CARTESIAN_POINT('Ctrl Pts',(2.80879724399994,11.6,-10.44992621));
#157794=CARTESIAN_POINT('Ctrl Pts',(2.80889778599994,15.2,-10.4472307));
#157795=CARTESIAN_POINT('Ctrl Pts',(2.80889778599994,11.6,-10.4472307));
#157796=CARTESIAN_POINT('Ctrl Pts',(2.80899583999994,15.2,-10.444540948));
#157797=CARTESIAN_POINT('Ctrl Pts',(2.80899583999994,11.6,-10.444540948));
#157798=CARTESIAN_POINT('Ctrl Pts',(2.80909141499994,15.2,-10.441856967));
#157799=CARTESIAN_POINT('Ctrl Pts',(2.80909141499994,11.6,-10.441856967));
#157800=CARTESIAN_POINT('Ctrl Pts',(2.80918451699995,15.2,-10.439178769));
#157801=CARTESIAN_POINT('Ctrl Pts',(2.80918451699995,11.6,-10.439178769));
#157802=CARTESIAN_POINT('Ctrl Pts',(2.80927515499994,15.2,-10.436506365));
#157803=CARTESIAN_POINT('Ctrl Pts',(2.80927515499994,11.6,-10.436506365));
#157804=CARTESIAN_POINT('Ctrl Pts',(2.80936333799994,15.2,-10.433839767));
#157805=CARTESIAN_POINT('Ctrl Pts',(2.80936333799994,11.6,-10.433839767));
#157806=CARTESIAN_POINT('Ctrl Pts',(2.80944907299994,15.2,-10.431178984));
#157807=CARTESIAN_POINT('Ctrl Pts',(2.80944907299994,11.6,-10.431178984));
#157808=CARTESIAN_POINT('Ctrl Pts',(2.80953236999995,15.2,-10.428524029));
#157809=CARTESIAN_POINT('Ctrl Pts',(2.80953236999995,11.6,-10.428524029));
#157810=CARTESIAN_POINT('Ctrl Pts',(2.80961323599994,15.2,-10.425874914));
#157811=CARTESIAN_POINT('Ctrl Pts',(2.80961323599994,11.6,-10.425874914));
#157812=CARTESIAN_POINT('Ctrl Pts',(2.80969167999995,15.2,-10.423231648));
#157813=CARTESIAN_POINT('Ctrl Pts',(2.80969167999995,11.6,-10.423231648));
#157814=CARTESIAN_POINT('Ctrl Pts',(2.80976771099994,15.2,-10.420594246));
#157815=CARTESIAN_POINT('Ctrl Pts',(2.80976771099994,11.6,-10.420594246));
#157816=CARTESIAN_POINT('Ctrl Pts',(2.80984133599994,15.2,-10.417962716));
#157817=CARTESIAN_POINT('Ctrl Pts',(2.80984133599994,11.6,-10.417962716));
#157818=CARTESIAN_POINT('Ctrl Pts',(2.80991256599994,15.2,-10.415337072));
#157819=CARTESIAN_POINT('Ctrl Pts',(2.80991256599994,11.6,-10.415337072));
#157820=CARTESIAN_POINT('Ctrl Pts',(2.80998140599994,15.2,-10.412717325));
#157821=CARTESIAN_POINT('Ctrl Pts',(2.80998140599994,11.6,-10.412717325));
#157822=CARTESIAN_POINT('Ctrl Pts',(2.81004786699994,15.2,-10.410103485));
#157823=CARTESIAN_POINT('Ctrl Pts',(2.81004786699994,11.6,-10.410103485));
#157824=CARTESIAN_POINT('Ctrl Pts',(2.81011195699994,15.2,-10.407495565));
#157825=CARTESIAN_POINT('Ctrl Pts',(2.81011195699994,11.6,-10.407495565));
#157826=CARTESIAN_POINT('Ctrl Pts',(2.81017368499994,15.2,-10.404893577));
#157827=CARTESIAN_POINT('Ctrl Pts',(2.81017368499994,11.6,-10.404893577));
#157828=CARTESIAN_POINT('Ctrl Pts',(2.81023305899994,15.2,-10.402297532));
#157829=CARTESIAN_POINT('Ctrl Pts',(2.81023305899994,11.6,-10.402297532));
#157830=CARTESIAN_POINT('Ctrl Pts',(2.81029008899994,15.2,-10.39970744));
#157831=CARTESIAN_POINT('Ctrl Pts',(2.81029008899994,11.6,-10.39970744));
#157832=CARTESIAN_POINT('Ctrl Pts',(2.81034478199994,15.2,-10.397123316));
#157833=CARTESIAN_POINT('Ctrl Pts',(2.81034478199994,11.6,-10.397123316));
#157834=CARTESIAN_POINT('Ctrl Pts',(2.81039714699994,15.2,-10.394545169));
#157835=CARTESIAN_POINT('Ctrl Pts',(2.81039714699994,11.6,-10.394545169));
#157836=CARTESIAN_POINT('Ctrl Pts',(2.81044719399994,15.2,-10.391973012));
#157837=CARTESIAN_POINT('Ctrl Pts',(2.81044719399994,11.6,-10.391973012));
#157838=CARTESIAN_POINT('Ctrl Pts',(2.81049492999994,15.2,-10.389406856));
#157839=CARTESIAN_POINT('Ctrl Pts',(2.81049492999994,11.6,-10.389406856));
#157840=CARTESIAN_POINT('Ctrl Pts',(2.81054036499994,15.2,-10.386846714));
#157841=CARTESIAN_POINT('Ctrl Pts',(2.81054036499994,11.6,-10.386846714));
#157842=CARTESIAN_POINT('Ctrl Pts',(2.81058350899994,15.2,-10.384292597));
#157843=CARTESIAN_POINT('Ctrl Pts',(2.81058350899994,11.6,-10.384292597));
#157844=CARTESIAN_POINT('Ctrl Pts',(2.81062436799994,15.2,-10.381744516));
#157845=CARTESIAN_POINT('Ctrl Pts',(2.81062436799994,11.6,-10.381744516));
#157846=CARTESIAN_POINT('Ctrl Pts',(2.81066295399994,15.2,-10.379202483));
#157847=CARTESIAN_POINT('Ctrl Pts',(2.81066295399994,11.6,-10.379202483));
#157848=CARTESIAN_POINT('Ctrl Pts',(2.81069927399995,15.2,-10.376666512));
#157849=CARTESIAN_POINT('Ctrl Pts',(2.81069927399995,11.6,-10.376666512));
#157850=CARTESIAN_POINT('Ctrl Pts',(2.81073333699994,15.2,-10.374136614));
#157851=CARTESIAN_POINT('Ctrl Pts',(2.81073333699994,11.6,-10.374136614));
#157852=CARTESIAN_POINT('Ctrl Pts',(2.81076515299994,15.2,-10.371612798));
#157853=CARTESIAN_POINT('Ctrl Pts',(2.81076515299994,11.6,-10.371612798));
#157854=CARTESIAN_POINT('Ctrl Pts',(2.81079472999994,15.2,-10.36909508));
#157855=CARTESIAN_POINT('Ctrl Pts',(2.81079472999994,11.6,-10.36909508));
#157856=CARTESIAN_POINT('Ctrl Pts',(2.81082207799995,15.2,-10.366583471));
#157857=CARTESIAN_POINT('Ctrl Pts',(2.81082207799995,11.6,-10.366583471));
#157858=CARTESIAN_POINT('Ctrl Pts',(2.81084720699994,15.2,-10.364077981));
#157859=CARTESIAN_POINT('Ctrl Pts',(2.81084720699994,11.6,-10.364077981));
#157860=CARTESIAN_POINT('Ctrl Pts',(2.81087012399994,15.2,-10.361578623));
#157861=CARTESIAN_POINT('Ctrl Pts',(2.81087012399994,11.6,-10.361578623));
#157862=CARTESIAN_POINT('Ctrl Pts',(2.81089083899994,15.2,-10.35908541));
#157863=CARTESIAN_POINT('Ctrl Pts',(2.81089083899994,11.6,-10.35908541));
#157864=CARTESIAN_POINT('Ctrl Pts',(2.81090936199994,15.2,-10.356598354));
#157865=CARTESIAN_POINT('Ctrl Pts',(2.81090936199994,11.6,-10.356598354));
#157866=CARTESIAN_POINT('Ctrl Pts',(2.81092570199994,15.2,-10.354117466));
#157867=CARTESIAN_POINT('Ctrl Pts',(2.81092570199994,11.6,-10.354117466));
#157868=CARTESIAN_POINT('Ctrl Pts',(2.81093986699994,15.2,-10.351642759));
#157869=CARTESIAN_POINT('Ctrl Pts',(2.81093986699994,11.6,-10.351642759));
#157870=CARTESIAN_POINT('Ctrl Pts',(2.81095186899994,15.2,-10.349174244));
#157871=CARTESIAN_POINT('Ctrl Pts',(2.81095186899994,11.6,-10.349174244));
#157872=CARTESIAN_POINT('Ctrl Pts',(2.81096171499994,15.2,-10.346711935));
#157873=CARTESIAN_POINT('Ctrl Pts',(2.81096171499994,11.6,-10.346711935));
#157874=CARTESIAN_POINT('Ctrl Pts',(2.81096941499994,15.2,-10.344255843));
#157875=CARTESIAN_POINT('Ctrl Pts',(2.81096941499994,11.6,-10.344255843));
#157876=CARTESIAN_POINT('Ctrl Pts',(2.81097497899994,15.2,-10.34180598));
#157877=CARTESIAN_POINT('Ctrl Pts',(2.81097497899994,11.6,-10.34180598));
#157878=CARTESIAN_POINT('Ctrl Pts',(2.81097841599995,15.2,-10.339362359));
#157879=CARTESIAN_POINT('Ctrl Pts',(2.81097841599995,11.6,-10.339362359));
#157880=CARTESIAN_POINT('Ctrl Pts',(2.81097973499994,15.2,-10.336924993));
#157881=CARTESIAN_POINT('Ctrl Pts',(2.81097973499994,11.6,-10.336924993));
#157882=CARTESIAN_POINT('Ctrl Pts',(2.81097894699994,15.2,-10.334493893));
#157883=CARTESIAN_POINT('Ctrl Pts',(2.81097894699994,11.6,-10.334493893));
#157884=CARTESIAN_POINT('Ctrl Pts',(2.81097606099994,15.2,-10.332069072));
#157885=CARTESIAN_POINT('Ctrl Pts',(2.81097606099994,11.6,-10.332069072));
#157886=CARTESIAN_POINT('Ctrl Pts',(2.81097108599994,15.2,-10.329650541));
#157887=CARTESIAN_POINT('Ctrl Pts',(2.81097108599994,11.6,-10.329650541));
#157888=CARTESIAN_POINT('Ctrl Pts',(2.81096403099995,15.2,-10.327238315));
#157889=CARTESIAN_POINT('Ctrl Pts',(2.81096403099995,11.6,-10.327238315));
#157890=CARTESIAN_POINT('Ctrl Pts',(2.81095490899995,15.2,-10.324832405));
#157891=CARTESIAN_POINT('Ctrl Pts',(2.81095490899995,11.6,-10.324832405));
#157892=CARTESIAN_POINT('Ctrl Pts',(2.81094372499994,15.2,-10.322432824));
#157893=CARTESIAN_POINT('Ctrl Pts',(2.81094372499994,11.6,-10.322432824));
#157894=CARTESIAN_POINT('Ctrl Pts',(2.81093049199994,15.2,-10.320039582));
#157895=CARTESIAN_POINT('Ctrl Pts',(2.81093049199994,11.6,-10.320039582));
#157896=CARTESIAN_POINT('Ctrl Pts',(2.81091521999994,15.2,-10.317652696));
#157897=CARTESIAN_POINT('Ctrl Pts',(2.81091521999994,11.6,-10.317652696));
#157898=CARTESIAN_POINT('Ctrl Pts',(2.81089791699995,15.2,-10.315272175));
#157899=CARTESIAN_POINT('Ctrl Pts',(2.81089791699995,11.6,-10.315272175));
#157900=CARTESIAN_POINT('Ctrl Pts',(2.81087859399994,15.2,-10.312898032));
#157901=CARTESIAN_POINT('Ctrl Pts',(2.81087859399994,11.6,-10.312898032));
#157902=CARTESIAN_POINT('Ctrl Pts',(2.81085726099994,15.2,-10.310530281));
#157903=CARTESIAN_POINT('Ctrl Pts',(2.81085726099994,11.6,-10.310530281));
#157904=CARTESIAN_POINT('Ctrl Pts',(2.81083392699994,15.2,-10.308168934));
#157905=CARTESIAN_POINT('Ctrl Pts',(2.81083392699994,11.6,-10.308168934));
#157906=CARTESIAN_POINT('Ctrl Pts',(2.81080860299994,15.2,-10.305814005));
#157907=CARTESIAN_POINT('Ctrl Pts',(2.81080860299994,11.6,-10.305814005));
#157908=CARTESIAN_POINT('Ctrl Pts',(2.81078129899994,15.2,-10.303465503));
#157909=CARTESIAN_POINT('Ctrl Pts',(2.81078129899994,11.6,-10.303465503));
#157910=CARTESIAN_POINT('Ctrl Pts',(2.81075202399995,15.2,-10.301123444));
#157911=CARTESIAN_POINT('Ctrl Pts',(2.81075202399995,11.6,-10.301123444));
#157912=CARTESIAN_POINT('Ctrl Pts',(2.81072078899995,15.2,-10.298787841));
#157913=CARTESIAN_POINT('Ctrl Pts',(2.81072078899995,11.6,-10.298787841));
#157914=CARTESIAN_POINT('Ctrl Pts',(2.81068760399994,15.2,-10.296458705));
#157915=CARTESIAN_POINT('Ctrl Pts',(2.81068760399994,11.6,-10.296458705));
#157916=CARTESIAN_POINT('Ctrl Pts',(2.81065247899994,15.2,-10.294136049));
#157917=CARTESIAN_POINT('Ctrl Pts',(2.81065247899994,11.6,-10.294136049));
#157918=CARTESIAN_POINT('Ctrl Pts',(2.81061542499994,15.2,-10.291819888));
#157919=CARTESIAN_POINT('Ctrl Pts',(2.81061542499994,11.6,-10.291819888));
#157920=CARTESIAN_POINT('Ctrl Pts',(2.81057645099994,15.2,-10.289510231));
#157921=CARTESIAN_POINT('Ctrl Pts',(2.81057645099994,11.6,-10.289510231));
#157922=CARTESIAN_POINT('Ctrl Pts',(2.81053556799994,15.2,-10.287207095));
#157923=CARTESIAN_POINT('Ctrl Pts',(2.81053556799994,11.6,-10.287207095));
#157924=CARTESIAN_POINT('Ctrl Pts',(2.81049278599995,15.2,-10.284910491));
#157925=CARTESIAN_POINT('Ctrl Pts',(2.81049278599995,11.6,-10.284910491));
#157926=CARTESIAN_POINT('Ctrl Pts',(2.81044811599994,15.2,-10.282620432));
#157927=CARTESIAN_POINT('Ctrl Pts',(2.81044811599994,11.6,-10.282620432));
#157928=CARTESIAN_POINT('Ctrl Pts',(2.81040156799994,15.2,-10.280336931));
#157929=CARTESIAN_POINT('Ctrl Pts',(2.81040156799994,11.6,-10.280336931));
#157930=CARTESIAN_POINT('Ctrl Pts',(2.81035315299994,15.2,-10.278060001));
#157931=CARTESIAN_POINT('Ctrl Pts',(2.81035315299994,11.6,-10.278060001));
#157932=CARTESIAN_POINT('Ctrl Pts',(2.81030287999994,15.2,-10.275789656));
#157933=CARTESIAN_POINT('Ctrl Pts',(2.81030287999994,11.6,-10.275789656));
#157934=CARTESIAN_POINT('Ctrl Pts',(2.81025076099994,15.2,-10.273525908));
#157935=CARTESIAN_POINT('Ctrl Pts',(2.81025076099994,11.6,-10.273525908));
#157936=CARTESIAN_POINT('Ctrl Pts',(2.81019680699994,15.2,-10.271268771));
#157937=CARTESIAN_POINT('Ctrl Pts',(2.81019680699994,11.6,-10.271268771));
#157938=CARTESIAN_POINT('Ctrl Pts',(2.81014102599995,15.2,-10.269018258));
#157939=CARTESIAN_POINT('Ctrl Pts',(2.81014102599995,11.6,-10.269018258));
#157940=CARTESIAN_POINT('Ctrl Pts',(2.81008343199994,15.2,-10.266774381));
#157941=CARTESIAN_POINT('Ctrl Pts',(2.81008343199994,11.6,-10.266774381));
#157942=CARTESIAN_POINT('Ctrl Pts',(2.81002403299994,15.2,-10.264537156));
#157943=CARTESIAN_POINT('Ctrl Pts',(2.81002403299994,11.6,-10.264537156));
#157944=CARTESIAN_POINT('Ctrl Pts',(2.80996284099994,15.2,-10.262306593));
#157945=CARTESIAN_POINT('Ctrl Pts',(2.80996284099994,11.6,-10.262306593));
#157946=CARTESIAN_POINT('Ctrl Pts',(2.80989986699994,15.2,-10.260082708));
#157947=CARTESIAN_POINT('Ctrl Pts',(2.80989986699994,11.6,-10.260082708));
#157948=CARTESIAN_POINT('Ctrl Pts',(2.80983512099994,15.2,-10.257865513));
#157949=CARTESIAN_POINT('Ctrl Pts',(2.80983512099994,11.6,-10.257865513));
#157950=CARTESIAN_POINT('Ctrl Pts',(2.80976861499994,15.2,-10.25565502));
#157951=CARTESIAN_POINT('Ctrl Pts',(2.80976861499994,11.6,-10.25565502));
#157952=CARTESIAN_POINT('Ctrl Pts',(2.80970035899994,15.2,-10.253451247));
#157953=CARTESIAN_POINT('Ctrl Pts',(2.80970035899994,11.6,-10.253451247));
#157954=CARTESIAN_POINT('Ctrl Pts',(2.80963036399994,15.2,-10.251254202));
#157955=CARTESIAN_POINT('Ctrl Pts',(2.80963036399994,11.6,-10.251254202));
#157956=CARTESIAN_POINT('Ctrl Pts',(2.80955864199994,15.2,-10.249063901));
#157957=CARTESIAN_POINT('Ctrl Pts',(2.80955864199994,11.6,-10.249063901));
#157958=CARTESIAN_POINT('Ctrl Pts',(2.80948520299994,15.2,-10.246880359));
#157959=CARTESIAN_POINT('Ctrl Pts',(2.80948520299994,11.6,-10.246880359));
#157960=CARTESIAN_POINT('Ctrl Pts',(2.80941005699994,15.2,-10.244703587));
#157961=CARTESIAN_POINT('Ctrl Pts',(2.80941005699994,11.6,-10.244703587));
#157962=CARTESIAN_POINT('Ctrl Pts',(2.80933321799994,15.2,-10.242533601));
#157963=CARTESIAN_POINT('Ctrl Pts',(2.80933321799994,11.6,-10.242533601));
#157964=CARTESIAN_POINT('Ctrl Pts',(2.80925469499994,15.2,-10.240370412));
#157965=CARTESIAN_POINT('Ctrl Pts',(2.80925469499994,11.6,-10.240370412));
#157966=CARTESIAN_POINT('Ctrl Pts',(2.80917449899994,15.2,-10.238214035));
#157967=CARTESIAN_POINT('Ctrl Pts',(2.80917449899994,11.6,-10.238214035));
#157968=CARTESIAN_POINT('Ctrl Pts',(2.80909264299994,15.2,-10.236064484));
#157969=CARTESIAN_POINT('Ctrl Pts',(2.80909264299994,11.6,-10.236064484));
#157970=CARTESIAN_POINT('Ctrl Pts',(2.80900913699994,15.2,-10.233921772));
#157971=CARTESIAN_POINT('Ctrl Pts',(2.80900913699994,11.6,-10.233921772));
#157972=CARTESIAN_POINT('Ctrl Pts',(2.80892399399994,15.2,-10.231785914));
#157973=CARTESIAN_POINT('Ctrl Pts',(2.80892399399994,11.6,-10.231785914));
#157974=CARTESIAN_POINT('Ctrl Pts',(2.80883722299994,15.2,-10.229656922));
#157975=CARTESIAN_POINT('Ctrl Pts',(2.80883722299994,11.6,-10.229656922));
#157976=CARTESIAN_POINT('Ctrl Pts',(2.80874883699994,15.2,-10.227534811));
#157977=CARTESIAN_POINT('Ctrl Pts',(2.80874883699994,11.6,-10.227534811));
#157978=CARTESIAN_POINT('Ctrl Pts',(2.80865884799995,15.2,-10.225419595));
#157979=CARTESIAN_POINT('Ctrl Pts',(2.80865884799995,11.6,-10.225419595));
#157980=CARTESIAN_POINT('Ctrl Pts',(2.80856726499994,15.2,-10.223311288));
#157981=CARTESIAN_POINT('Ctrl Pts',(2.80856726499994,11.6,-10.223311288));
#157982=CARTESIAN_POINT('Ctrl Pts',(2.80847410199994,15.2,-10.221209902));
#157983=CARTESIAN_POINT('Ctrl Pts',(2.80847410199994,11.6,-10.221209902));
#157984=CARTESIAN_POINT('Ctrl Pts',(2.80837936999994,15.2,-10.219115454));
#157985=CARTESIAN_POINT('Ctrl Pts',(2.80837936999994,11.6,-10.219115454));
#157986=CARTESIAN_POINT('Ctrl Pts',(2.80828307999994,15.2,-10.217027955));
#157987=CARTESIAN_POINT('Ctrl Pts',(2.80828307999994,11.6,-10.217027955));
#157988=CARTESIAN_POINT('Ctrl Pts',(2.80818524499994,15.2,-10.214947422));
#157989=CARTESIAN_POINT('Ctrl Pts',(2.80818524499994,11.6,-10.214947422));
#157990=CARTESIAN_POINT('Ctrl Pts',(2.80808587499994,15.2,-10.212873867));
#157991=CARTESIAN_POINT('Ctrl Pts',(2.80808587499994,11.6,-10.212873867));
#157992=CARTESIAN_POINT('Ctrl Pts',(2.80798498399994,15.2,-10.210807306));
#157993=CARTESIAN_POINT('Ctrl Pts',(2.80798498399994,11.6,-10.210807306));
#157994=CARTESIAN_POINT('Ctrl Pts',(2.80788258099995,15.2,-10.208747752));
#157995=CARTESIAN_POINT('Ctrl Pts',(2.80788258099995,11.6,-10.208747752));
#157996=CARTESIAN_POINT('Ctrl Pts',(2.80777868099995,15.2,-10.206695218));
#157997=CARTESIAN_POINT('Ctrl Pts',(2.80777868099995,11.6,-10.206695218));
#157998=CARTESIAN_POINT('Ctrl Pts',(2.80767329399994,15.2,-10.204649721));
#157999=CARTESIAN_POINT('Ctrl Pts',(2.80767329399994,11.6,-10.204649721));
#158000=CARTESIAN_POINT('Ctrl Pts',(2.80756643199994,15.2,-10.202611272));
#158001=CARTESIAN_POINT('Ctrl Pts',(2.80756643199994,11.6,-10.202611272));
#158002=CARTESIAN_POINT('Ctrl Pts',(2.80745810799994,15.2,-10.200579889));
#158003=CARTESIAN_POINT('Ctrl Pts',(2.80745810799994,11.6,-10.200579889));
#158004=CARTESIAN_POINT('Ctrl Pts',(2.80734833399995,15.2,-10.198555583));
#158005=CARTESIAN_POINT('Ctrl Pts',(2.80734833399995,11.6,-10.198555583));
#158006=CARTESIAN_POINT('Ctrl Pts',(2.80723712199995,15.2,-10.196538371));
#158007=CARTESIAN_POINT('Ctrl Pts',(2.80723712199995,11.6,-10.196538371));
#158008=CARTESIAN_POINT('Ctrl Pts',(2.80712448299994,15.2,-10.194528266));
#158009=CARTESIAN_POINT('Ctrl Pts',(2.80712448299994,11.6,-10.194528266));
#158010=CARTESIAN_POINT('Ctrl Pts',(2.80701043199994,15.2,-10.192525284));
#158011=CARTESIAN_POINT('Ctrl Pts',(2.80701043199994,11.6,-10.192525284));
#158012=CARTESIAN_POINT('Ctrl Pts',(2.80689497799994,15.2,-10.190529437));
#158013=CARTESIAN_POINT('Ctrl Pts',(2.80689497799994,11.6,-10.190529437));
#158014=CARTESIAN_POINT('Ctrl Pts',(2.80677813599994,15.2,-10.188540742));
#158015=CARTESIAN_POINT('Ctrl Pts',(2.80677813599994,11.6,-10.188540742));
#158016=CARTESIAN_POINT('Ctrl Pts',(2.80665991699995,15.2,-10.186559213));
#158017=CARTESIAN_POINT('Ctrl Pts',(2.80665991699995,11.6,-10.186559213));
#158018=CARTESIAN_POINT('Ctrl Pts',(2.80654033399995,15.2,-10.184584863));
#158019=CARTESIAN_POINT('Ctrl Pts',(2.80654033399995,11.6,-10.184584863));
#158020=CARTESIAN_POINT('Ctrl Pts',(2.80641939899994,15.2,-10.182617709));
#158021=CARTESIAN_POINT('Ctrl Pts',(2.80641939899994,11.6,-10.182617709));
#158022=CARTESIAN_POINT('Ctrl Pts',(2.80629712399994,15.2,-10.180657764));
#158023=CARTESIAN_POINT('Ctrl Pts',(2.80629712399994,11.6,-10.180657764));
#158024=CARTESIAN_POINT('Ctrl Pts',(2.80617352399994,15.2,-10.178705045));
#158025=CARTESIAN_POINT('Ctrl Pts',(2.80617352399994,11.6,-10.178705045));
#158026=CARTESIAN_POINT('Ctrl Pts',(2.80604860999994,15.2,-10.176759564));
#158027=CARTESIAN_POINT('Ctrl Pts',(2.80604860999994,11.6,-10.176759564));
#158028=CARTESIAN_POINT('Ctrl Pts',(2.80592239399994,15.2,-10.174821338));
#158029=CARTESIAN_POINT('Ctrl Pts',(2.80592239399994,11.6,-10.174821338));
#158030=CARTESIAN_POINT('Ctrl Pts',(2.80579489099994,15.2,-10.172890382));
#158031=CARTESIAN_POINT('Ctrl Pts',(2.80579489099994,11.6,-10.172890382));
#158032=CARTESIAN_POINT('Ctrl Pts',(2.80566611099994,15.2,-10.170966708));
#158033=CARTESIAN_POINT('Ctrl Pts',(2.80566611099994,11.6,-10.170966708));
#158034=CARTESIAN_POINT('Ctrl Pts',(2.80553606899994,15.2,-10.169050335));
#158035=CARTESIAN_POINT('Ctrl Pts',(2.80553606899994,11.6,-10.169050335));
#158036=CARTESIAN_POINT('Ctrl Pts',(2.80540477699994,15.2,-10.167141276));
#158037=CARTESIAN_POINT('Ctrl Pts',(2.80540477699994,11.6,-10.167141276));
#158038=CARTESIAN_POINT('Ctrl Pts',(2.80527224899994,15.2,-10.165239546));
#158039=CARTESIAN_POINT('Ctrl Pts',(2.80527224899994,11.6,-10.165239546));
#158040=CARTESIAN_POINT('Ctrl Pts',(2.80513849599994,15.2,-10.163345161));
#158041=CARTESIAN_POINT('Ctrl Pts',(2.80513849599994,11.6,-10.163345161));
#158042=CARTESIAN_POINT('Ctrl Pts',(2.80500353299994,15.2,-10.161458135));
#158043=CARTESIAN_POINT('Ctrl Pts',(2.80500353299994,11.6,-10.161458135));
#158044=CARTESIAN_POINT('Ctrl Pts',(2.80486737299994,15.2,-10.159578484));
#158045=CARTESIAN_POINT('Ctrl Pts',(2.80486737299994,11.6,-10.159578484));
#158046=CARTESIAN_POINT('Ctrl Pts',(2.80473002899994,15.2,-10.157706223));
#158047=CARTESIAN_POINT('Ctrl Pts',(2.80473002899994,11.6,-10.157706223));
#158048=CARTESIAN_POINT('Ctrl Pts',(2.80459151299994,15.2,-10.155841368));
#158049=CARTESIAN_POINT('Ctrl Pts',(2.80459151299994,11.6,-10.155841368));
#158050=CARTESIAN_POINT('Ctrl Pts',(2.80445183999994,15.2,-10.153983933));
#158051=CARTESIAN_POINT('Ctrl Pts',(2.80445183999994,11.6,-10.153983933));
#158052=CARTESIAN_POINT('Ctrl Pts',(2.80431102199994,15.2,-10.152133935));
#158053=CARTESIAN_POINT('Ctrl Pts',(2.80431102199994,11.6,-10.152133935));
#158054=CARTESIAN_POINT('Ctrl Pts',(2.80416907299994,15.2,-10.150291388));
#158055=CARTESIAN_POINT('Ctrl Pts',(2.80416907299994,11.6,-10.150291388));
#158056=CARTESIAN_POINT('Ctrl Pts',(2.80402600699994,15.2,-10.148456309));
#158057=CARTESIAN_POINT('Ctrl Pts',(2.80402600699994,11.6,-10.148456309));
#158058=CARTESIAN_POINT('Ctrl Pts',(2.80388183699994,15.2,-10.146628712));
#158059=CARTESIAN_POINT('Ctrl Pts',(2.80388183699994,11.6,-10.146628712));
#158060=CARTESIAN_POINT('Ctrl Pts',(2.80373657699994,15.2,-10.144808614));
#158061=CARTESIAN_POINT('Ctrl Pts',(2.80373657699994,11.6,-10.144808614));
#158062=CARTESIAN_POINT('Ctrl Pts',(2.80359023999994,15.2,-10.14299603));
#158063=CARTESIAN_POINT('Ctrl Pts',(2.80359023999994,11.6,-10.14299603));
#158064=CARTESIAN_POINT('Ctrl Pts',(2.80344283999994,15.2,-10.141190975));
#158065=CARTESIAN_POINT('Ctrl Pts',(2.80344283999994,11.6,-10.141190975));
#158066=CARTESIAN_POINT('Ctrl Pts',(2.80329439099994,15.2,-10.139393466));
#158067=CARTESIAN_POINT('Ctrl Pts',(2.80329439099994,11.6,-10.139393466));
#158068=CARTESIAN_POINT('Ctrl Pts',(2.80314490699995,15.2,-10.137603518));
#158069=CARTESIAN_POINT('Ctrl Pts',(2.80314490699995,11.6,-10.137603518));
#158070=CARTESIAN_POINT('Ctrl Pts',(2.80299440199994,15.2,-10.135821147));
#158071=CARTESIAN_POINT('Ctrl Pts',(2.80299440199994,11.6,-10.135821147));
#158072=CARTESIAN_POINT('Ctrl Pts',(2.80284288899994,15.2,-10.134046369));
#158073=CARTESIAN_POINT('Ctrl Pts',(2.80284288899994,11.6,-10.134046369));
#158074=CARTESIAN_POINT('Ctrl Pts',(2.80269038199994,15.2,-10.1322792));
#158075=CARTESIAN_POINT('Ctrl Pts',(2.80269038199994,11.6,-10.1322792));
#158076=CARTESIAN_POINT('Ctrl Pts',(2.80253689599995,15.2,-10.130519656));
#158077=CARTESIAN_POINT('Ctrl Pts',(2.80253689599995,11.6,-10.130519656));
#158078=CARTESIAN_POINT('Ctrl Pts',(2.80238244499994,15.2,-10.128767753));
#158079=CARTESIAN_POINT('Ctrl Pts',(2.80238244499994,11.6,-10.128767753));
#158080=CARTESIAN_POINT('Ctrl Pts',(2.80222704299995,15.2,-10.127023507));
#158081=CARTESIAN_POINT('Ctrl Pts',(2.80222704299995,11.6,-10.127023507));
#158082=CARTESIAN_POINT('Ctrl Pts',(2.80207070399995,15.2,-10.125286934));
#158083=CARTESIAN_POINT('Ctrl Pts',(2.80207070399995,11.6,-10.125286934));
#158084=CARTESIAN_POINT('Ctrl Pts',(2.80191344299995,15.2,-10.12355805));
#158085=CARTESIAN_POINT('Ctrl Pts',(2.80191344299995,11.6,-10.12355805));
#158086=CARTESIAN_POINT('Ctrl Pts',(2.80175527299994,15.2,-10.121836872));
#158087=CARTESIAN_POINT('Ctrl Pts',(2.80175527299994,11.6,-10.121836872));
#158088=CARTESIAN_POINT('Ctrl Pts',(2.80159621099994,15.2,-10.120123415));
#158089=CARTESIAN_POINT('Ctrl Pts',(2.80159621099994,11.6,-10.120123415));
#158090=CARTESIAN_POINT('Ctrl Pts',(2.80143626799994,15.2,-10.118417698));
#158091=CARTESIAN_POINT('Ctrl Pts',(2.80143626799994,11.6,-10.118417698));
#158092=CARTESIAN_POINT('Ctrl Pts',(2.80127546199994,15.2,-10.116719734));
#158093=CARTESIAN_POINT('Ctrl Pts',(2.80127546199994,11.6,-10.116719734));
#158094=CARTESIAN_POINT('Ctrl Pts',(2.80111380599994,15.2,-10.115029541));
#158095=CARTESIAN_POINT('Ctrl Pts',(2.80111380599994,11.6,-10.115029541));
#158096=CARTESIAN_POINT('Ctrl Pts',(2.80095131399994,15.2,-10.113347137));
#158097=CARTESIAN_POINT('Ctrl Pts',(2.80095131399994,11.6,-10.113347137));
#158098=CARTESIAN_POINT('Ctrl Pts',(2.80078800199994,15.2,-10.111672536));
#158099=CARTESIAN_POINT('Ctrl Pts',(2.80078800199994,11.6,-10.111672536));
#158100=CARTESIAN_POINT('Ctrl Pts',(2.80062388399994,15.2,-10.110005756));
#158101=CARTESIAN_POINT('Ctrl Pts',(2.80062388399994,11.6,-10.110005756));
#158102=CARTESIAN_POINT('Ctrl Pts',(2.80045897599994,15.2,-10.108346814));
#158103=CARTESIAN_POINT('Ctrl Pts',(2.80045897599994,11.6,-10.108346814));
#158104=CARTESIAN_POINT('Ctrl Pts',(2.80029329299994,15.2,-10.106695726));
#158105=CARTESIAN_POINT('Ctrl Pts',(2.80029329299994,11.6,-10.106695726));
#158106=CARTESIAN_POINT('Ctrl Pts',(2.80012684799994,15.2,-10.105052508));
#158107=CARTESIAN_POINT('Ctrl Pts',(2.80012684799994,11.6,-10.105052508));
#158108=CARTESIAN_POINT('Ctrl Pts',(2.79995965799994,15.2,-10.103417179));
#158109=CARTESIAN_POINT('Ctrl Pts',(2.79995965799994,11.6,-10.103417179));
#158110=CARTESIAN_POINT('Ctrl Pts',(2.79979173699994,15.2,-10.101789754));
#158111=CARTESIAN_POINT('Ctrl Pts',(2.79979173699994,11.6,-10.101789754));
#158112=CARTESIAN_POINT('Ctrl Pts',(2.79962310199994,15.2,-10.10017025));
#158113=CARTESIAN_POINT('Ctrl Pts',(2.79962310199994,11.6,-10.10017025));
#158114=CARTESIAN_POINT('Ctrl Pts',(2.79945376599994,15.2,-10.098558686));
#158115=CARTESIAN_POINT('Ctrl Pts',(2.79945376599994,11.6,-10.098558686));
#158116=CARTESIAN_POINT('Ctrl Pts',(2.79928374699994,15.2,-10.096955077));
#158117=CARTESIAN_POINT('Ctrl Pts',(2.79928374699994,11.6,-10.096955077));
#158118=CARTESIAN_POINT('Ctrl Pts',(2.79911305799994,15.2,-10.095359442));
#158119=CARTESIAN_POINT('Ctrl Pts',(2.79911305799994,11.6,-10.095359442));
#158120=CARTESIAN_POINT('Ctrl Pts',(2.79894171499994,15.2,-10.093771795));
#158121=CARTESIAN_POINT('Ctrl Pts',(2.79894171499994,11.6,-10.093771795));
#158122=CARTESIAN_POINT('Ctrl Pts',(2.79876973499994,15.2,-10.092192156));
#158123=CARTESIAN_POINT('Ctrl Pts',(2.79876973499994,11.6,-10.092192156));
#158124=CARTESIAN_POINT('Ctrl Pts',(2.79859713199994,15.2,-10.090620542));
#158125=CARTESIAN_POINT('Ctrl Pts',(2.79859713199994,11.6,-10.090620542));
#158126=CARTESIAN_POINT('Ctrl Pts',(2.79842392399994,15.2,-10.08905697));
#158127=CARTESIAN_POINT('Ctrl Pts',(2.79842392399994,11.6,-10.08905697));
#158128=CARTESIAN_POINT('Ctrl Pts',(2.79825012299994,15.2,-10.087501457));
#158129=CARTESIAN_POINT('Ctrl Pts',(2.79825012299994,11.6,-10.087501457));
#158130=CARTESIAN_POINT('Ctrl Pts',(2.79807574899994,15.2,-10.085954021));
#158131=CARTESIAN_POINT('Ctrl Pts',(2.79807574899994,11.6,-10.085954021));
#158132=CARTESIAN_POINT('Ctrl Pts',(2.79790081499995,15.2,-10.084414678));
#158133=CARTESIAN_POINT('Ctrl Pts',(2.79790081499995,11.6,-10.084414678));
#158134=CARTESIAN_POINT('Ctrl Pts',(2.79772533899994,15.2,-10.082883448));
#158135=CARTESIAN_POINT('Ctrl Pts',(2.79772533899994,11.6,-10.082883448));
#158136=CARTESIAN_POINT('Ctrl Pts',(2.79754933499994,15.2,-10.081360347));
#158137=CARTESIAN_POINT('Ctrl Pts',(2.79754933499994,11.6,-10.081360347));
#158138=CARTESIAN_POINT('Ctrl Pts',(2.79737282199994,15.2,-10.079845395));
#158139=CARTESIAN_POINT('Ctrl Pts',(2.79737282199994,11.6,-10.079845395));
#158140=CARTESIAN_POINT('Ctrl Pts',(2.79719581399994,15.2,-10.078338606));
#158141=CARTESIAN_POINT('Ctrl Pts',(2.79719581399994,11.6,-10.078338606));
#158142=CARTESIAN_POINT('Ctrl Pts',(2.79701832699994,15.2,-10.076840001));
#158143=CARTESIAN_POINT('Ctrl Pts',(2.79701832699994,11.6,-10.076840001));
#158144=CARTESIAN_POINT('Ctrl Pts',(2.79684037999994,15.2,-10.075349597));
#158145=CARTESIAN_POINT('Ctrl Pts',(2.79684037999994,11.6,-10.075349597));
#158146=CARTESIAN_POINT('Ctrl Pts',(2.79666198699994,15.2,-10.073867411));
#158147=CARTESIAN_POINT('Ctrl Pts',(2.79666198699994,11.6,-10.073867411));
#158148=CARTESIAN_POINT('Ctrl Pts',(2.79648316399994,15.2,-10.072393462));
#158149=CARTESIAN_POINT('Ctrl Pts',(2.79648316399994,11.6,-10.072393462));
#158150=CARTESIAN_POINT('Ctrl Pts',(2.79630393099994,15.2,-10.070927768));
#158151=CARTESIAN_POINT('Ctrl Pts',(2.79630393099994,11.6,-10.070927768));
#158152=CARTESIAN_POINT('Ctrl Pts',(2.79612430199994,15.2,-10.069470348));
#158153=CARTESIAN_POINT('Ctrl Pts',(2.79612430199994,11.6,-10.069470348));
#158154=CARTESIAN_POINT('Ctrl Pts',(2.79594429399994,15.2,-10.068021218));
#158155=CARTESIAN_POINT('Ctrl Pts',(2.79594429399994,11.6,-10.068021218));
#158156=CARTESIAN_POINT('Ctrl Pts',(2.79576392499994,15.2,-10.066580399));
#158157=CARTESIAN_POINT('Ctrl Pts',(2.79576392499994,11.6,-10.066580399));
#158158=CARTESIAN_POINT('Ctrl Pts',(2.79558320999994,15.2,-10.065147907));
#158159=CARTESIAN_POINT('Ctrl Pts',(2.79558320999994,11.6,-10.065147907));
#158160=CARTESIAN_POINT('Ctrl Pts',(2.79540216899994,15.2,-10.063723761));
#158161=CARTESIAN_POINT('Ctrl Pts',(2.79540216899994,11.6,-10.063723761));
#158162=CARTESIAN_POINT('Ctrl Pts',(2.79522081599994,15.2,-10.062307982));
#158163=CARTESIAN_POINT('Ctrl Pts',(2.79522081599994,11.6,-10.062307982));
#158164=CARTESIAN_POINT('Ctrl Pts',(2.79503916999994,15.2,-10.060900585));
#158165=CARTESIAN_POINT('Ctrl Pts',(2.79503916999994,11.6,-10.060900585));
#158166=CARTESIAN_POINT('Ctrl Pts',(2.79485724799994,15.2,-10.05950159));
#158167=CARTESIAN_POINT('Ctrl Pts',(2.79485724799994,11.6,-10.05950159));
#158168=CARTESIAN_POINT('Ctrl Pts',(2.79467506699994,15.2,-10.058111016));
#158169=CARTESIAN_POINT('Ctrl Pts',(2.79467506699994,11.6,-10.058111016));
#158170=CARTESIAN_POINT('Ctrl Pts',(2.79449264499994,15.2,-10.056728882));
#158171=CARTESIAN_POINT('Ctrl Pts',(2.79449264499994,11.6,-10.056728882));
#158172=CARTESIAN_POINT('Ctrl Pts',(2.79430999899994,15.2,-10.055355207));
#158173=CARTESIAN_POINT('Ctrl Pts',(2.79430999899994,11.6,-10.055355207));
#158174=CARTESIAN_POINT('Ctrl Pts',(2.79412714599995,15.2,-10.053990009));
#158175=CARTESIAN_POINT('Ctrl Pts',(2.79412714599995,11.6,-10.053990009));
#158176=CARTESIAN_POINT('Ctrl Pts',(2.79394410499994,15.2,-10.052633306));
#158177=CARTESIAN_POINT('Ctrl Pts',(2.79394410499994,11.6,-10.052633306));
#158178=CARTESIAN_POINT('Ctrl Pts',(2.79376089299994,15.2,-10.05128512));
#158179=CARTESIAN_POINT('Ctrl Pts',(2.79376089299994,11.6,-10.05128512));
#158180=CARTESIAN_POINT('Ctrl Pts',(2.79357752899994,15.2,-10.049945468));
#158181=CARTESIAN_POINT('Ctrl Pts',(2.79357752899994,11.6,-10.049945468));
#158182=CARTESIAN_POINT('Ctrl Pts',(2.79339402799994,15.2,-10.04861437));
#158183=CARTESIAN_POINT('Ctrl Pts',(2.79339402799994,11.6,-10.04861437));
#158184=CARTESIAN_POINT('Ctrl Pts',(2.79321041199994,15.2,-10.047291846));
#158185=CARTESIAN_POINT('Ctrl Pts',(2.79321041199994,11.6,-10.047291846));
#158186=CARTESIAN_POINT('Ctrl Pts',(2.79302669599995,15.2,-10.045977913));
#158187=CARTESIAN_POINT('Ctrl Pts',(2.79302669599995,11.6,-10.045977913));
#158188=CARTESIAN_POINT('Ctrl Pts',(2.79284289899994,15.2,-10.044672592));
#158189=CARTESIAN_POINT('Ctrl Pts',(2.79284289899994,11.6,-10.044672592));
#158190=CARTESIAN_POINT('Ctrl Pts',(2.79265904099995,15.2,-10.043375903));
#158191=CARTESIAN_POINT('Ctrl Pts',(2.79265904099995,11.6,-10.043375903));
#158192=CARTESIAN_POINT('Ctrl Pts',(2.79247513699994,15.2,-10.042087865));
#158193=CARTESIAN_POINT('Ctrl Pts',(2.79247513699994,11.6,-10.042087865));
#158194=CARTESIAN_POINT('Ctrl Pts',(2.79229120899994,15.2,-10.040808498));
#158195=CARTESIAN_POINT('Ctrl Pts',(2.79229120899994,11.6,-10.040808498));
#158196=CARTESIAN_POINT('Ctrl Pts',(2.79210727299994,15.2,-10.03953782));
#158197=CARTESIAN_POINT('Ctrl Pts',(2.79210727299994,11.6,-10.03953782));
#158198=CARTESIAN_POINT('Ctrl Pts',(2.79192334899995,15.2,-10.038275853));
#158199=CARTESIAN_POINT('Ctrl Pts',(2.79192334899995,11.6,-10.038275853));
#158200=CARTESIAN_POINT('Ctrl Pts',(2.79173945599994,15.2,-10.037022616));
#158201=CARTESIAN_POINT('Ctrl Pts',(2.79173945599994,11.6,-10.037022616));
#158202=CARTESIAN_POINT('Ctrl Pts',(2.79155561199994,15.2,-10.035778129));
#158203=CARTESIAN_POINT('Ctrl Pts',(2.79155561199994,11.6,-10.035778129));
#158204=CARTESIAN_POINT('Ctrl Pts',(2.79137183599994,15.2,-10.034542413));
#158205=CARTESIAN_POINT('Ctrl Pts',(2.79137183599994,11.6,-10.034542413));
#158206=CARTESIAN_POINT('Ctrl Pts',(2.79118814699994,15.2,-10.033315485));
#158207=CARTESIAN_POINT('Ctrl Pts',(2.79118814699994,11.6,-10.033315485));
#158208=CARTESIAN_POINT('Ctrl Pts',(2.79100456599994,15.2,-10.032097369));
#158209=CARTESIAN_POINT('Ctrl Pts',(2.79100456599994,11.6,-10.032097369));
#158210=CARTESIAN_POINT('Ctrl Pts',(2.79082110899994,15.2,-10.030888083));
#158211=CARTESIAN_POINT('Ctrl Pts',(2.79082110899994,11.6,-10.030888083));
#158212=CARTESIAN_POINT('Ctrl Pts',(2.79063779699994,15.2,-10.029687649));
#158213=CARTESIAN_POINT('Ctrl Pts',(2.79063779699994,11.6,-10.029687649));
#158214=CARTESIAN_POINT('Ctrl Pts',(2.79045464899994,15.2,-10.028496086));
#158215=CARTESIAN_POINT('Ctrl Pts',(2.79045464899994,11.6,-10.028496086));
#158216=CARTESIAN_POINT('Ctrl Pts',(2.79027168599994,15.2,-10.027313415));
#158217=CARTESIAN_POINT('Ctrl Pts',(2.79027168599994,11.6,-10.027313415));
#158218=CARTESIAN_POINT('Ctrl Pts',(2.79008892599995,15.2,-10.026139656));
#158219=CARTESIAN_POINT('Ctrl Pts',(2.79008892599995,11.6,-10.026139656));
#158220=CARTESIAN_POINT('Ctrl Pts',(2.78990638899994,15.2,-10.024974831));
#158221=CARTESIAN_POINT('Ctrl Pts',(2.78990638899994,11.6,-10.024974831));
#158222=CARTESIAN_POINT('Ctrl Pts',(2.78972409599994,15.2,-10.023818961));
#158223=CARTESIAN_POINT('Ctrl Pts',(2.78972409599994,11.6,-10.023818961));
#158224=CARTESIAN_POINT('Ctrl Pts',(2.78954206499994,15.2,-10.022672066));
#158225=CARTESIAN_POINT('Ctrl Pts',(2.78954206499994,11.6,-10.022672066));
#158226=CARTESIAN_POINT('Ctrl Pts',(2.78936031599994,15.2,-10.021534166));
#158227=CARTESIAN_POINT('Ctrl Pts',(2.78936031599994,11.6,-10.021534166));
#158228=CARTESIAN_POINT('Ctrl Pts',(2.78917887099994,15.2,-10.020405284));
#158229=CARTESIAN_POINT('Ctrl Pts',(2.78917887099994,11.6,-10.020405284));
#158230=CARTESIAN_POINT('Ctrl Pts',(2.78899774999994,15.2,-10.019285439));
#158231=CARTESIAN_POINT('Ctrl Pts',(2.78899774999994,11.6,-10.019285439));
#158232=CARTESIAN_POINT('Ctrl Pts',(2.78881697199994,15.2,-10.018174655));
#158233=CARTESIAN_POINT('Ctrl Pts',(2.78881697199994,11.6,-10.018174655));
#158234=CARTESIAN_POINT('Ctrl Pts',(2.78863655799995,15.2,-10.01707295));
#158235=CARTESIAN_POINT('Ctrl Pts',(2.78863655799995,11.6,-10.01707295));
#158236=CARTESIAN_POINT('Ctrl Pts',(2.78845652899995,15.2,-10.015980349));
#158237=CARTESIAN_POINT('Ctrl Pts',(2.78845652899995,11.6,-10.015980349));
#158238=CARTESIAN_POINT('Ctrl Pts',(2.78827690499994,15.2,-10.014896871));
#158239=CARTESIAN_POINT('Ctrl Pts',(2.78827690499994,11.6,-10.014896871));
#158240=CARTESIAN_POINT('Ctrl Pts',(2.78809770599994,15.2,-10.013822539));
#158241=CARTESIAN_POINT('Ctrl Pts',(2.78809770599994,11.6,-10.013822539));
#158242=CARTESIAN_POINT('Ctrl Pts',(2.78791895499995,15.2,-10.012757373));
#158243=CARTESIAN_POINT('Ctrl Pts',(2.78791895499995,11.6,-10.012757373));
#158244=CARTESIAN_POINT('Ctrl Pts',(2.78774067099994,15.2,-10.011701396));
#158245=CARTESIAN_POINT('Ctrl Pts',(2.78774067099994,11.6,-10.011701396));
#158246=CARTESIAN_POINT('Ctrl Pts',(2.78756287699994,15.2,-10.01065463));
#158247=CARTESIAN_POINT('Ctrl Pts',(2.78756287699994,11.6,-10.01065463));
#158248=CARTESIAN_POINT('Ctrl Pts',(2.78738559299994,15.2,-10.009617097));
#158249=CARTESIAN_POINT('Ctrl Pts',(2.78738559299994,11.6,-10.009617097));
#158250=CARTESIAN_POINT('Ctrl Pts',(2.78720883999994,15.2,-10.008588818));
#158251=CARTESIAN_POINT('Ctrl Pts',(2.78720883999994,11.6,-10.008588818));
#158252=CARTESIAN_POINT('Ctrl Pts',(2.78703263999994,15.2,-10.007569815));
#158253=CARTESIAN_POINT('Ctrl Pts',(2.78703263999994,11.6,-10.007569815));
#158254=CARTESIAN_POINT('Ctrl Pts',(2.78685701499994,15.2,-10.006560112));
#158255=CARTESIAN_POINT('Ctrl Pts',(2.78685701499994,11.6,-10.006560112));
#158256=CARTESIAN_POINT('Ctrl Pts',(2.78668198499994,15.2,-10.005559732));
#158257=CARTESIAN_POINT('Ctrl Pts',(2.78668198499994,11.6,-10.005559732));
#158258=CARTESIAN_POINT('Ctrl Pts',(2.78650757299994,15.2,-10.004568694));
#158259=CARTESIAN_POINT('Ctrl Pts',(2.78650757299994,11.6,-10.004568694));
#158260=CARTESIAN_POINT('Ctrl Pts',(2.78633380099994,15.2,-10.003587024));
#158261=CARTESIAN_POINT('Ctrl Pts',(2.78633380099994,11.6,-10.003587024));
#158262=CARTESIAN_POINT('Ctrl Pts',(2.78616069099995,15.2,-10.002614742));
#158263=CARTESIAN_POINT('Ctrl Pts',(2.78616069099995,11.6,-10.002614742));
#158264=CARTESIAN_POINT('Ctrl Pts',(2.78598826499994,15.2,-10.001651872));
#158265=CARTESIAN_POINT('Ctrl Pts',(2.78598826499994,11.6,-10.001651872));
#158266=CARTESIAN_POINT('Ctrl Pts',(2.78581654299995,15.2,-10.000698437));
#158267=CARTESIAN_POINT('Ctrl Pts',(2.78581654299995,11.6,-10.000698437));
#158268=CARTESIAN_POINT('Ctrl Pts',(2.78564555099994,15.2,-9.99975446000001));
#158269=CARTESIAN_POINT('Ctrl Pts',(2.78564555099994,11.6,-9.99975446000001));
#158270=CARTESIAN_POINT('Ctrl Pts',(2.78547531099994,15.2,-9.99881996400001));
#158271=CARTESIAN_POINT('Ctrl Pts',(2.78547531099994,11.6,-9.99881996400001));
#158272=CARTESIAN_POINT('Ctrl Pts',(2.78530584299994,15.2,-9.99789497200001));
#158273=CARTESIAN_POINT('Ctrl Pts',(2.78530584299994,11.6,-9.99789497200001));
#158274=CARTESIAN_POINT('Ctrl Pts',(2.78513717099994,15.2,-9.99697950700001));
#158275=CARTESIAN_POINT('Ctrl Pts',(2.78513717099994,11.6,-9.99697950700001));
#158276=CARTESIAN_POINT('Ctrl Pts',(2.78497028699995,15.2,-9.99607881000001));
#158277=CARTESIAN_POINT('Ctrl Pts',(2.78497028699995,11.6,-9.99607881000001));
#158278=CARTESIAN_POINT('Ctrl Pts',(2.78483763599994,15.2,-9.99536684600001));
#158279=CARTESIAN_POINT('Ctrl Pts',(2.78483763599994,11.6,-9.99536684600001));
#158280=CARTESIAN_POINT('Ctrl Pts',(2.78473876899994,15.2,-9.99483840000001));
#158281=CARTESIAN_POINT('Ctrl Pts',(2.78473876899994,11.6,-9.99483840000001));
#158282=CARTESIAN_POINT('Ctrl Pts',(2.78467334899994,15.2,-9.99448967800001));
#158283=CARTESIAN_POINT('Ctrl Pts',(2.78467334899994,11.6,-9.99448967800001));
#158284=CARTESIAN_POINT('Ctrl Pts',(2.78464115899994,15.2,-9.99431831700001));
#158285=CARTESIAN_POINT('Ctrl Pts',(2.78464115899994,11.6,-9.99431831700001));
#158286=CARTESIAN_POINT('',(2.78464115833177,12.2,-9.99431831666127));
#158287=CARTESIAN_POINT('',(2.78464115833177,15.2,-9.99431831666127));
#158288=CARTESIAN_POINT('',(2.78464115799995,12.2,-9.99431831600001));
#158289=CARTESIAN_POINT('Ctrl Pts',(2.71145515299994,12.2,-11.175777867));
#158290=CARTESIAN_POINT('Ctrl Pts',(2.71227322814856,12.2,-11.1720435063216));
#158291=CARTESIAN_POINT('Ctrl Pts',(2.71308567464298,12.2,-11.1683146746693));
#158292=CARTESIAN_POINT('Ctrl Pts',(2.71389248615398,12.2,-11.1645913879167));
#158293=CARTESIAN_POINT('Ctrl Pts',(2.71469929766498,12.2,-11.1608681011642));
#158294=CARTESIAN_POINT('Ctrl Pts',(2.71550047515118,12.2,-11.1571503540028));
#158295=CARTESIAN_POINT('Ctrl Pts',(2.71629602837101,12.2,-11.1534381629932));
#158296=CARTESIAN_POINT('Ctrl Pts',(2.71709158159084,12.2,-11.1497259719837));
#158297=CARTESIAN_POINT('Ctrl Pts',(2.7178815099234,12.2,-11.1460193377731));
#158298=CARTESIAN_POINT('Ctrl Pts',(2.718665831354,12.2,-11.1423182987818));
#158299=CARTESIAN_POINT('Ctrl Pts',(2.71945015292708,12.2,-11.1386172591182));
#158300=CARTESIAN_POINT('Ctrl Pts',(2.72022886944025,12.2,-11.1349218170144));
#158301=CARTESIAN_POINT('Ctrl Pts',(2.72100200242686,12.2,-11.1312320151873));
#158302=CARTESIAN_POINT('Ctrl Pts',(2.72229055721726,12.2,-11.1250823463691));
#158303=CARTESIAN_POINT('Ctrl Pts',(2.72356360362685,12.2,-11.1189483468318));
#158304=CARTESIAN_POINT('Ctrl Pts',(2.72482121918114,12.2,-11.1128301753747));
#158305=CARTESIAN_POINT('Ctrl Pts',(2.7255757884863,12.2,-11.1091592726339));
#158306=CARTESIAN_POINT('Ctrl Pts',(2.72632480281762,12.2,-11.1054940671912));
#158307=CARTESIAN_POINT('Ctrl Pts',(2.72706828016044,12.2,-11.1018345948087));
#158308=CARTESIAN_POINT('Ctrl Pts',(2.72781175750326,12.2,-11.0981751224262));
#158309=CARTESIAN_POINT('Ctrl Pts',(2.72854969754015,12.2,-11.0945213835527));
#158310=CARTESIAN_POINT('Ctrl Pts',(2.72928212034639,12.2,-11.0908734168108));
#158311=CARTESIAN_POINT('Ctrl Pts',(2.73001454315263,12.2,-11.0872254500688));
#158312=CARTESIAN_POINT('Ctrl Pts',(2.7307414481262,12.2,-11.0835832539512));
#158313=CARTESIAN_POINT('Ctrl Pts',(2.73146285451665,12.2,-11.07994686725));
#158314=CARTESIAN_POINT('Ctrl Pts',(2.73218426090711,12.2,-11.0763104805487));
#158315=CARTESIAN_POINT('Ctrl Pts',(2.73290016921445,12.2,-11.0726799035306));
#158316=CARTESIAN_POINT('Ctrl Pts',(2.73361059710579,12.2,-11.0690551704118));
#158317=CARTESIAN_POINT('Ctrl Pts',(2.73432102499712,12.2,-11.065430437293));
#158318=CARTESIAN_POINT('Ctrl Pts',(2.73502597318777,12.2,-11.0618115499989));
#158319=CARTESIAN_POINT('Ctrl Pts',(2.73572546007293,12.2,-11.0581985437407));
#158320=CARTESIAN_POINT('Ctrl Pts',(2.73642494695809,12.2,-11.0545855374825));
#158321=CARTESIAN_POINT('Ctrl Pts',(2.73711897324081,12.2,-11.050978414405));
#158322=CARTESIAN_POINT('Ctrl Pts',(2.73780755809153,12.2,-11.047377210285));
#158323=CARTESIAN_POINT('Ctrl Pts',(2.73849614306735,12.2,-11.0437760055109));
#158324=CARTESIAN_POINT('Ctrl Pts',(2.73917928739996,12.2,-11.0401807203383));
#158325=CARTESIAN_POINT('Ctrl Pts',(2.73985700941439,12.2,-11.0365913929842));
#158326=CARTESIAN_POINT('Ctrl Pts',(2.74053473130569,12.2,-11.0330020662821));
#158327=CARTESIAN_POINT('Ctrl Pts',(2.74120703188062,12.2,-11.029418696463));
#158328=CARTESIAN_POINT('Ctrl Pts',(2.74187392981425,12.2,-11.0258413208435));
#158329=CARTESIAN_POINT('Ctrl Pts',(2.74254082774788,12.2,-11.022263945224));
#158330=CARTESIAN_POINT('Ctrl Pts',(2.74320232467146,12.2,-11.0186925647334));
#158331=CARTESIAN_POINT('Ctrl Pts',(2.74385843898391,12.2,-11.0151272164717));
#158332=CARTESIAN_POINT('Ctrl Pts',(2.74451455329636,12.2,-11.0115618682101));
#158333=CARTESIAN_POINT('Ctrl Pts',(2.74516528453655,12.2,-11.0080025505236));
#158334=CARTESIAN_POINT('Ctrl Pts',(2.74581065526606,12.2,-11.0044493047615));
#158335=CARTESIAN_POINT('Ctrl Pts',(2.74645602599557,12.2,-11.0008960589995));
#158336=CARTESIAN_POINT('Ctrl Pts',(2.74709603415331,12.2,-10.9973488830412));
#158337=CARTESIAN_POINT('Ctrl Pts',(2.74773070146405,12.2,-10.9938078158361));
#158338=CARTESIAN_POINT('Ctrl Pts',(2.74836536877479,12.2,-10.9902667486308));
#158339=CARTESIAN_POINT('Ctrl Pts',(2.7489946944859,12.2,-10.9867317897085));
#158340=CARTESIAN_POINT('Ctrl Pts',(2.74961869888061,12.2,-10.9832029770443));
#158341=CARTESIAN_POINT('Ctrl Pts',(2.75024270338869,12.2,-10.9796741637389));
#158342=CARTESIAN_POINT('Ctrl Pts',(2.75086138659527,12.2,-10.9761514968936));
#158343=CARTESIAN_POINT('Ctrl Pts',(2.75147477010036,12.2,-10.9726350142167));
#158344=CARTESIAN_POINT('Ctrl Pts',(2.75208815349402,12.2,-10.9691185321786));
#158345=CARTESIAN_POINT('Ctrl Pts',(2.75269623685462,12.2,-10.9656082361236));
#158346=CARTESIAN_POINT('Ctrl Pts',(2.75329904074893,12.2,-10.9621041620848));
#158347=CARTESIAN_POINT('Ctrl Pts',(2.75390184464324,12.2,-10.958600088046));
#158348=CARTESIAN_POINT('Ctrl Pts',(2.75449936965271,12.2,-10.9551022388858));
#158349=CARTESIAN_POINT('Ctrl Pts',(2.75509163696718,12.2,-10.9516106502885));
#158350=CARTESIAN_POINT('Ctrl Pts',(2.75568390428166,12.2,-10.9481190616912));
#158351=CARTESIAN_POINT('Ctrl Pts',(2.75627091386792,12.2,-10.9446337351092));
#158352=CARTESIAN_POINT('Ctrl Pts',(2.75685268580778,12.2,-10.9411547090115));
#158353=CARTESIAN_POINT('Ctrl Pts',(2.75743445774765,12.2,-10.9376756829137));
#158354=CARTESIAN_POINT('Ctrl Pts',(2.75801099402459,12.2,-10.9342029577358));
#158355=CARTESIAN_POINT('Ctrl Pts',(2.75858231446262,12.2,-10.9307365721112));
#158356=CARTESIAN_POINT('Ctrl Pts',(2.75934407511585,12.2,-10.926114724192));
#158357=CARTESIAN_POINT('Ctrl Pts',(2.76009656536241,12.2,-10.921504147024));
#158358=CARTESIAN_POINT('Ctrl Pts',(2.76083983656899,12.2,-10.9169049331074));
#158359=CARTESIAN_POINT('Ctrl Pts',(2.76139728992328,12.2,-10.9134555229833));
#158360=CARTESIAN_POINT('Ctrl Pts',(2.76194955613456,12.2,-10.9100125053209));
#158361=CARTESIAN_POINT('Ctrl Pts',(2.76249665949214,12.2,-10.9065759177635));
#158362=CARTESIAN_POINT('Ctrl Pts',(2.76304376284973,12.2,-10.9031393302061));
#158363=CARTESIAN_POINT('Ctrl Pts',(2.76358570229987,12.2,-10.8997091746276));
#158364=CARTESIAN_POINT('Ctrl Pts',(2.76412250024116,12.2,-10.8962854894864));
#158365=CARTESIAN_POINT('Ctrl Pts',(2.76483823089456,12.2,-10.8917205755502));
#158366=CARTESIAN_POINT('Ctrl Pts',(2.76554482242137,12.2,-10.8871671644149));
#158367=CARTESIAN_POINT('Ctrl Pts',(2.76624232634735,12.2,-10.8826253517241));
#158368=CARTESIAN_POINT('Ctrl Pts',(2.76693983017829,12.2,-10.8780835396521));
#158369=CARTESIAN_POINT('Ctrl Pts',(2.76762824691041,12.2,-10.8735533249536));
#158370=CARTESIAN_POINT('Ctrl Pts',(2.76830763141102,12.2,-10.8690348023778));
#158371=CARTESIAN_POINT('Ctrl Pts',(2.76881716980962,12.2,-10.865645910292));
#158372=CARTESIAN_POINT('Ctrl Pts',(2.76932162752925,12.2,-10.8622635954499));
#158373=CARTESIAN_POINT('Ctrl Pts',(2.76982102791164,12.2,-10.8588878971948));
#158374=CARTESIAN_POINT('Ctrl Pts',(2.77032042829403,12.2,-10.8555121989397));
#158375=CARTESIAN_POINT('Ctrl Pts',(2.77081477072707,12.2,-10.8521431182784));
#158376=CARTESIAN_POINT('Ctrl Pts',(2.77130407866831,12.2,-10.848780694233));
#158377=CARTESIAN_POINT('Ctrl Pts',(2.77179338669844,12.2,-10.8454182695768));
#158378=CARTESIAN_POINT('Ctrl Pts',(2.77227766115215,12.2,-10.842062503039));
#158379=CARTESIAN_POINT('Ctrl Pts',(2.77275692463779,12.2,-10.8387134343032));
#158380=CARTESIAN_POINT('Ctrl Pts',(2.77323618803636,12.2,-10.8353643661758));
#158381=CARTESIAN_POINT('Ctrl Pts',(2.7737104404352,12.2,-10.8320219957314));
#158382=CARTESIAN_POINT('Ctrl Pts',(2.77417970637604,12.2,-10.8286863636448));
#158383=CARTESIAN_POINT('Ctrl Pts',(2.77464897231689,12.2,-10.8253507315583));
#158384=CARTESIAN_POINT('Ctrl Pts',(2.77511325149836,12.2,-10.8220218386413));
#158385=CARTESIAN_POINT('Ctrl Pts',(2.77557256798373,12.2,-10.8186997245386));
#158386=CARTESIAN_POINT('Ctrl Pts',(2.77603188446911,12.2,-10.8153776104359));
#158387=CARTESIAN_POINT('Ctrl Pts',(2.77648623906383,12.2,-10.8120622753145));
#158388=CARTESIAN_POINT('Ctrl Pts',(2.77693565454957,12.2,-10.808753760753));
#158389=CARTESIAN_POINT('Ctrl Pts',(2.77753487525164,12.2,-10.8043424076036));
#158390=CARTESIAN_POINT('Ctrl Pts',(2.77812531728372,12.2,-10.7999431812233));
#158391=CARTESIAN_POINT('Ctrl Pts',(2.77870703737009,12.2,-10.795556176041));
#158392=CARTESIAN_POINT('Ctrl Pts',(2.7792887573772,12.2,-10.7911691714565));
#158393=CARTESIAN_POINT('Ctrl Pts',(2.77986175804655,12.2,-10.7867943903342));
#158394=CARTESIAN_POINT('Ctrl Pts',(2.78042609594543,12.2,-10.7824319303567));
#158395=CARTESIAN_POINT('Ctrl Pts',(2.78099043392119,12.2,-10.7780694697848));
#158396=CARTESIAN_POINT('Ctrl Pts',(2.78154610997291,12.2,-10.7737193301949));
#158397=CARTESIAN_POINT('Ctrl Pts',(2.78209318402931,12.2,-10.7693816108539));
#158398=CARTESIAN_POINT('Ctrl Pts',(2.78264025801118,12.2,-10.765043892104));
#158399=CARTESIAN_POINT('Ctrl Pts',(2.78317873092156,12.2,-10.7607185945176));
#158400=CARTESIAN_POINT('Ctrl Pts',(2.78370866165657,12.2,-10.7564058158693));
#158401=CARTESIAN_POINT('Ctrl Pts',(2.78423859246379,12.2,-10.7520930366335));
#158402=CARTESIAN_POINT('Ctrl Pts',(2.78475998396721,12.2,-10.7477927764963));
#158403=CARTESIAN_POINT('Ctrl Pts',(2.78527289405016,12.2,-10.7435051378746));
#158404=CARTESIAN_POINT('Ctrl Pts',(2.78578580406323,12.2,-10.739217499837));
#158405=CARTESIAN_POINT('Ctrl Pts',(2.78629023460411,12.2,-10.7349424809897));
#158406=CARTESIAN_POINT('Ctrl Pts',(2.78678624847796,12.2,-10.7306801829019));
#158407=CARTESIAN_POINT('Ctrl Pts',(2.78728226241939,12.2,-10.7264178842333));
#158408=CARTESIAN_POINT('Ctrl Pts',(2.78776985765795,12.2,-10.7221683068366));
#158409=CARTESIAN_POINT('Ctrl Pts',(2.78824910023908,12.2,-10.7179315516621));
#158410=CARTESIAN_POINT('Ctrl Pts',(2.78872834275491,12.2,-10.7136947970648));
#158411=CARTESIAN_POINT('Ctrl Pts',(2.78919923138353,12.2,-10.7094708651316));
#158412=CARTESIAN_POINT('Ctrl Pts',(2.78966182945767,12.2,-10.7052598571968));
#158413=CARTESIAN_POINT('Ctrl Pts',(2.79024007709762,12.2,-10.6999960968479));
#158414=CARTESIAN_POINT('Ctrl Pts',(2.79080537129064,12.2,-10.6947525307299));
#158415=CARTESIAN_POINT('Ctrl Pts',(2.79135783965246,12.2,-10.6895293593564));
#158416=CARTESIAN_POINT('Ctrl Pts',(2.79179981436601,12.2,-10.6853508220298));
#158417=CARTESIAN_POINT('Ctrl Pts',(2.79223358019536,12.2,-10.681185338825));
#158418=CARTESIAN_POINT('Ctrl Pts',(2.79265920355136,12.2,-10.6770330117106));
#158419=CARTESIAN_POINT('Ctrl Pts',(2.79308482684937,12.2,-10.6728806851621));
#158420=CARTESIAN_POINT('Ctrl Pts',(2.79350230596012,12.2,-10.6687415149275));
#158421=CARTESIAN_POINT('Ctrl Pts',(2.7939117111497,12.2,-10.6646156057079));
#158422=CARTESIAN_POINT('Ctrl Pts',(2.79432111639506,12.2,-10.6604896959261));
#158423=CARTESIAN_POINT('Ctrl Pts',(2.7947224445076,12.2,-10.6563770470975));
#158424=CARTESIAN_POINT('Ctrl Pts',(2.79511576580858,12.2,-10.6522777640222));
#158425=CARTESIAN_POINT('Ctrl Pts',(2.79550908705596,12.2,-10.6481784815054));
#158426=CARTESIAN_POINT('Ctrl Pts',(2.79589439987109,12.2,-10.6440925658898));
#158427=CARTESIAN_POINT('Ctrl Pts',(2.79627177322994,12.2,-10.6400201206658));
#158428=CARTESIAN_POINT('Ctrl Pts',(2.7966491466402,12.2,-10.635947674887));
#158429=CARTESIAN_POINT('Ctrl Pts',(2.79701858100805,12.2,-10.6318887024788));
#158430=CARTESIAN_POINT('Ctrl Pts',(2.79738014524998,12.2,-10.6278433067583));
#158431=CARTESIAN_POINT('Ctrl Pts',(2.79774170949191,12.2,-10.6237979110378));
#158432=CARTESIAN_POINT('Ctrl Pts',(2.79809540441903,12.2,-10.6197660927828));
#158433=CARTESIAN_POINT('Ctrl Pts',(2.79844130104819,12.2,-10.615747960343));
#158434=CARTESIAN_POINT('Ctrl Pts',(2.79878719763023,12.2,-10.6117298284506));
#158435=CARTESIAN_POINT('Ctrl Pts',(2.79912529445218,12.2,-10.6077253810232));
#158436=CARTESIAN_POINT('Ctrl Pts',(2.79945566448123,12.2,-10.603734727793));
#158437=CARTESIAN_POINT('Ctrl Pts',(2.79995121954731,12.2,-10.5977487476758));
#158438=CARTESIAN_POINT('Ctrl Pts',(2.80042938649863,12.2,-10.5917938013158));
#158439=CARTESIAN_POINT('Ctrl Pts',(2.80089041348305,12.2,-10.5858702563623));
#158440=CARTESIAN_POINT('Ctrl Pts',(2.80119776483392,12.2,-10.5819212260345));
#158441=CARTESIAN_POINT('Ctrl Pts',(2.80149749733683,12.2,-10.5779861525192));
#158442=CARTESIAN_POINT('Ctrl Pts',(2.80178968674164,12.2,-10.57406514475));
#158443=CARTESIAN_POINT('Ctrl Pts',(2.80208187614646,12.2,-10.5701441369807));
#158444=CARTESIAN_POINT('Ctrl Pts',(2.80236651939483,12.2,-10.5662371951992));
#158445=CARTESIAN_POINT('Ctrl Pts',(2.80264369602029,12.2,-10.5623444308218));
#158446=CARTESIAN_POINT('Ctrl Pts',(2.80292087260798,12.2,-10.5584516669749));
#158447=CARTESIAN_POINT('Ctrl Pts',(2.80319057944224,12.2,-10.5545730792043));
#158448=CARTESIAN_POINT('Ctrl Pts',(2.80345289353313,12.2,-10.5507087805026));
#158449=CARTESIAN_POINT('Ctrl Pts',(2.80371520765975,12.2,-10.5468444812744));
#158450=CARTESIAN_POINT('Ctrl Pts',(2.80397012870549,12.2,-10.5429944693582));
#158451=CARTESIAN_POINT('Ctrl Pts',(2.80421773427379,12.2,-10.5391588583728));
#158452=CARTESIAN_POINT('Ctrl Pts',(2.80446533980835,12.2,-10.5353232479101));
#158453=CARTESIAN_POINT('Ctrl Pts',(2.80470562972165,12.2,-10.531502037576));
#158454=CARTESIAN_POINT('Ctrl Pts',(2.80493868248085,12.2,-10.527695341053));
#158455=CARTESIAN_POINT('Ctrl Pts',(2.80528826163553,12.2,-10.521985296009));
#158456=CARTESIAN_POINT('Ctrl Pts',(2.80562155570082,12.2,-10.5163079060207));
#158457=CARTESIAN_POINT('Ctrl Pts',(2.80593883494039,12.2,-10.5106635561402));
#158458=CARTESIAN_POINT('Ctrl Pts',(2.80615035445264,12.2,-10.5069006558781));
#158459=CARTESIAN_POINT('Ctrl Pts',(2.80635475585866,12.2,-10.5031524403812));
#158460=CARTESIAN_POINT('Ctrl Pts',(2.80655212125831,12.2,-10.4994190247333));
#158461=CARTESIAN_POINT('Ctrl Pts',(2.80674948665795,12.2,-10.4956856090854));
#158462=CARTESIAN_POINT('Ctrl Pts',(2.80693981379289,12.2,-10.4919669937559));
#158463=CARTESIAN_POINT('Ctrl Pts',(2.80712318724662,12.2,-10.4882632941111));
#158464=CARTESIAN_POINT('Ctrl Pts',(2.80730656067536,12.2,-10.4845595949709));
#158465=CARTESIAN_POINT('Ctrl Pts',(2.80748297848792,12.2,-10.4808708119328));
#158466=CARTESIAN_POINT('Ctrl Pts',(2.80765252597485,12.2,-10.4771970614941));
#158467=CARTESIAN_POINT('Ctrl Pts',(2.80782207348489,12.2,-10.4735233105549));
#158468=CARTESIAN_POINT('Ctrl Pts',(2.80798475053432,12.2,-10.4698645942013));
#158469=CARTESIAN_POINT('Ctrl Pts',(2.80814063954212,12.2,-10.4662210266709));
#158470=CARTESIAN_POINT('Ctrl Pts',(2.80829652852868,12.2,-10.462577459637));
#158471=CARTESIAN_POINT('Ctrl Pts',(2.8084456315328,12.2,-10.4589490453316));
#158472=CARTESIAN_POINT('Ctrl Pts',(2.8085880325216,12.2,-10.4553358995705));
#158473=CARTESIAN_POINT('Ctrl Pts',(2.8087304335298,12.2,-10.451722753317));
#158474=CARTESIAN_POINT('Ctrl Pts',(2.80886613339742,12.2,-10.4481248778725));
#158475=CARTESIAN_POINT('Ctrl Pts',(2.80899522024367,12.2,-10.4445423902219));
#158476=CARTESIAN_POINT('Ctrl Pts',(2.80912430707232,12.2,-10.4409599030593));
#158477=CARTESIAN_POINT('Ctrl Pts',(2.8092467797467,12.2,-10.4373928068956));
#158478=CARTESIAN_POINT('Ctrl Pts',(2.80936272601543,12.2,-10.4338412210738));
#158479=CARTESIAN_POINT('Ctrl Pts',(2.80947867229995,12.2,-10.4302896347681));
#158480=CARTESIAN_POINT('Ctrl Pts',(2.80958809251425,12.2,-10.4267535579004));
#158481=CARTESIAN_POINT('Ctrl Pts',(2.80969107674166,12.2,-10.423233113654));
#158482=CARTESIAN_POINT('Ctrl Pts',(2.80979406095505,12.2,-10.4197126698872));
#158483=CARTESIAN_POINT('Ctrl Pts',(2.80989060949194,12.2,-10.416207858894));
#158484=CARTESIAN_POINT('Ctrl Pts',(2.80998081121185,12.2,-10.4127188022813));
#158485=CARTESIAN_POINT('Ctrl Pts',(2.81007101294404,12.2,-10.4092297451933));
#158486=CARTESIAN_POINT('Ctrl Pts',(2.81015486936632,12.2,-10.4057564434743));
#158487=CARTESIAN_POINT('Ctrl Pts',(2.81023247298125,12.2,-10.4022990200091));
#158488=CARTESIAN_POINT('Ctrl Pts',(2.81031007658561,12.2,-10.398841597015));
#158489=CARTESIAN_POINT('Ctrl Pts',(2.8103814266579,12.2,-10.395400053215));
#158490=CARTESIAN_POINT('Ctrl Pts',(2.81044661626431,12.2,-10.3919745128267));
#158491=CARTESIAN_POINT('Ctrl Pts',(2.8105118058796,12.2,-10.3885489719717));
#158492=CARTESIAN_POINT('Ctrl Pts',(2.81057083531634,12.2,-10.3851394361035));
#158493=CARTESIAN_POINT('Ctrl Pts',(2.81062379970834,12.2,-10.3817460280143));
#158494=CARTESIAN_POINT('Ctrl Pts',(2.81069000519472,12.2,-10.377504268134));
#158495=CARTESIAN_POINT('Ctrl Pts',(2.81074673386461,12.2,-10.3732877113413));
#158496=CARTESIAN_POINT('Ctrl Pts',(2.81079417275301,12.2,-10.3690966069677));
#158497=CARTESIAN_POINT('Ctrl Pts',(2.81084161164142,12.2,-10.364905502594));
#158498=CARTESIAN_POINT('Ctrl Pts',(2.8108797625634,12.2,-10.3607398474113));
#158499=CARTESIAN_POINT('Ctrl Pts',(2.81090881624348,12.2,-10.356599895746));
#158500=CARTESIAN_POINT('Ctrl Pts',(2.81093786992356,12.2,-10.3524599440807));
#158501=CARTESIAN_POINT('Ctrl Pts',(2.81095782634017,12.2,-10.3483456940834));
#158502=CARTESIAN_POINT('Ctrl Pts',(2.81096888099288,12.2,-10.3442573997838));
#158503=CARTESIAN_POINT('Ctrl Pts',(2.8109799356456,12.2,-10.3401691054842));
#158504=CARTESIAN_POINT('Ctrl Pts',(2.81098208833315,12.2,-10.3361067688644));
#158505=CARTESIAN_POINT('Ctrl Pts',(2.81097553874911,12.2,-10.3320706440054));
#158506=CARTESIAN_POINT('Ctrl Pts',(2.81096898916506,12.2,-10.3280345191464));
#158507=CARTESIAN_POINT('Ctrl Pts',(2.81095373514755,12.2,-10.3240246086045));
#158508=CARTESIAN_POINT('Ctrl Pts',(2.81092998223019,12.2,-10.3200411704123));
#158509=CARTESIAN_POINT('Ctrl Pts',(2.81090622931283,12.2,-10.31605773222));
#158510=CARTESIAN_POINT('Ctrl Pts',(2.81087397636201,12.2,-10.3121007663448));
#158511=CARTESIAN_POINT('Ctrl Pts',(2.81083342948633,12.2,-10.3081705379442));
#158512=CARTESIAN_POINT('Ctrl Pts',(2.81079288261507,12.2,-10.304240309972));
#158513=CARTESIAN_POINT('Ctrl Pts',(2.81074404255054,12.2,-10.3003368164922));
#158514=CARTESIAN_POINT('Ctrl Pts',(2.81068711901574,12.2,-10.2964603255237));
#158515=CARTESIAN_POINT('Ctrl Pts',(2.81063019547474,12.2,-10.2925838341326));
#158516=CARTESIAN_POINT('Ctrl Pts',(2.81056518920885,12.2,-10.2887343451133));
#158517=CARTESIAN_POINT('Ctrl Pts',(2.81049231400116,12.2,-10.2849121277499));
#158518=CARTESIAN_POINT('Ctrl Pts',(2.81041943879347,12.2,-10.2810899103866));
#158519=CARTESIAN_POINT('Ctrl Pts',(2.81033869508631,12.2,-10.2772949636608));
#158520=CARTESIAN_POINT('Ctrl Pts',(2.8102503022352,12.2,-10.2735275611791));
#158521=CARTESIAN_POINT('Ctrl Pts',(2.81016190938409,12.2,-10.2697601586973));
#158522=CARTESIAN_POINT('Ctrl Pts',(2.8100658657063,12.2,-10.2660203007665));
#158523=CARTESIAN_POINT('Ctrl Pts',(2.80996239549835,12.2,-10.2623082627095));
#158524=CARTESIAN_POINT('Ctrl Pts',(2.80985892529041,12.2,-10.2585962246525));
#158525=CARTESIAN_POINT('Ctrl Pts',(2.80974802821282,12.2,-10.2549120077462));
#158526=CARTESIAN_POINT('Ctrl Pts',(2.80962993224098,12.2,-10.2512558882309));
#158527=CARTESIAN_POINT('Ctrl Pts',(2.80951183626913,12.2,-10.2475997687155));
#158528=CARTESIAN_POINT('Ctrl Pts',(2.80938654093395,12.2,-10.2439717513294));
#158529=CARTESIAN_POINT('Ctrl Pts',(2.8092542767667,12.2,-10.2403721149936));
#158530=CARTESIAN_POINT('Ctrl Pts',(2.80912201259945,12.2,-10.2367724786577));
#158531=CARTESIAN_POINT('Ctrl Pts',(2.80898278167219,12.2,-10.233201226061));
#158532=CARTESIAN_POINT('Ctrl Pts',(2.80883681924163,12.2,-10.2296586422416));
#158533=CARTESIAN_POINT('Ctrl Pts',(2.80869085681107,12.2,-10.2261160584222));
#158534=CARTESIAN_POINT('Ctrl Pts',(2.80853816385061,12.2,-10.2226021452027));
#158535=CARTESIAN_POINT('Ctrl Pts',(2.80837898051654,12.2,-10.219117191298));
#158536=CARTESIAN_POINT('Ctrl Pts',(2.80821979718247,12.2,-10.2156322373934));
#158537=CARTESIAN_POINT('Ctrl Pts',(2.80805412412789,12.2,-10.2121762447245));
#158538=CARTESIAN_POINT('Ctrl Pts',(2.80788220669701,12.2,-10.2087495068093));
#158539=CARTESIAN_POINT('Ctrl Pts',(2.80771028926613,12.2,-10.2053227688942));
#158540=CARTESIAN_POINT('Ctrl Pts',(2.80753212788264,12.2,-10.2019252858283));
#158541=CARTESIAN_POINT('Ctrl Pts',(2.80734797447955,12.2,-10.1985573562465));
#158542=CARTESIAN_POINT('Ctrl Pts',(2.80716382107645,12.2,-10.1951894266647));
#158543=CARTESIAN_POINT('Ctrl Pts',(2.80697367425405,12.2,-10.1918510513959));
#158544=CARTESIAN_POINT('Ctrl Pts',(2.80677779174387,12.2,-10.1885425331076));
#158545=CARTESIAN_POINT('Ctrl Pts',(2.8065035562467,12.2,-10.1839106077926));
#158546=CARTESIAN_POINT('Ctrl Pts',(2.80621807528634,12.2,-10.1793371986607));
#158547=CARTESIAN_POINT('Ctrl Pts',(2.80592207223594,12.2,-10.1748231558967));
#158548=CARTESIAN_POINT('Ctrl Pts',(2.80566835530597,12.2,-10.1709539759328));
#158549=CARTESIAN_POINT('Ctrl Pts',(2.80540690715243,12.2,-10.1671284092933));
#158550=CARTESIAN_POINT('Ctrl Pts',(2.80513819345728,12.2,-10.1633470004009));
#158551=CARTESIAN_POINT('Ctrl Pts',(2.80486947978653,12.2,-10.159565591852));
#158552=CARTESIAN_POINT('Ctrl Pts',(2.80459350390635,12.2,-10.1558283400574));
#158553=CARTESIAN_POINT('Ctrl Pts',(2.80431073924996,12.2,-10.1521357977749));
#158554=CARTESIAN_POINT('Ctrl Pts',(2.80402797459357,12.2,-10.1484432554925));
#158555=CARTESIAN_POINT('Ctrl Pts',(2.8037384244489,12.2,-10.1447954232169));
#158556=CARTESIAN_POINT('Ctrl Pts',(2.80344257777856,12.2,-10.1411928618319));
#158557=CARTESIAN_POINT('Ctrl Pts',(2.80314673108135,12.2,-10.1375903001196));
#158558=CARTESIAN_POINT('Ctrl Pts',(2.80284458940023,12.2,-10.1340330103888));
#158559=CARTESIAN_POINT('Ctrl Pts',(2.80253665471639,12.2,-10.1305215658672));
#158560=CARTESIAN_POINT('Ctrl Pts',(2.80222872006052,12.2,-10.1270101216646));
#158561=CARTESIAN_POINT('Ctrl Pts',(2.80191499338134,12.2,-10.1235445211729));
#158562=CARTESIAN_POINT('Ctrl Pts',(2.80159599080814,12.2,-10.1201253499484));
#158563=CARTESIAN_POINT('Ctrl Pts',(2.80127698823494,12.2,-10.1167061787239));
#158564=CARTESIAN_POINT('Ctrl Pts',(2.80095270991403,12.2,-10.1133334348042));
#158565=CARTESIAN_POINT('Ctrl Pts',(2.80062368650953,12.2,-10.110007715673));
#158566=CARTESIAN_POINT('Ctrl Pts',(2.80029466307514,12.2,-10.1066819962398));
#158567=CARTESIAN_POINT('Ctrl Pts',(2.79996089519015,12.2,-10.1034032999539));
#158568=CARTESIAN_POINT('Ctrl Pts',(2.79962292675478,12.2,-10.1001722346144));
#158569=CARTESIAN_POINT('Ctrl Pts',(2.79928495835011,12.2,-10.0969411695684));
#158570=CARTESIAN_POINT('Ctrl Pts',(2.79894278918881,12.2,-10.0937577355654));
#158571=CARTESIAN_POINT('Ctrl Pts',(2.79859698069979,12.2,-10.0906225524985));
#158572=CARTESIAN_POINT('Ctrl Pts',(2.79825117221078,12.2,-10.0874873694316));
#158573=CARTESIAN_POINT('Ctrl Pts',(2.79790172196454,12.2,-10.0844004344241));
#158574=CARTESIAN_POINT('Ctrl Pts',(2.79754920772748,12.2,-10.0813623843657));
#158575=CARTESIAN_POINT('Ctrl Pts',(2.7971966934584,12.2,-10.0783243340313));
#158576=CARTESIAN_POINT('Ctrl Pts',(2.79684111459727,12.2,-10.0753351655114));
#158577=CARTESIAN_POINT('Ctrl Pts',(2.79648306141092,12.2,-10.0723955254378));
#158578=CARTESIAN_POINT('Ctrl Pts',(2.79612500825709,12.2,-10.0694558856314));
#158579=CARTESIAN_POINT('Ctrl Pts',(2.79576448225877,12.2,-10.06656577444));
#158580=CARTESIAN_POINT('Ctrl Pts',(2.79540209102186,12.2,-10.0637258525454));
#158581=CARTESIAN_POINT('Ctrl Pts',(2.79503969978494,12.2,-10.0608859306507));
#158582=CARTESIAN_POINT('Ctrl Pts',(2.79467544327319,12.2,-10.0580961963021));
#158583=CARTESIAN_POINT('Ctrl Pts',(2.79430994728653,12.2,-10.0553573263994));
#158584=CARTESIAN_POINT('Ctrl Pts',(2.79394445129987,12.2,-10.0526184564967));
#158585=CARTESIAN_POINT('Ctrl Pts',(2.79357771622659,12.2,-10.0499304478117));
#158586=CARTESIAN_POINT('Ctrl Pts',(2.79321038707332,12.2,-10.0472939940706));
#158587=CARTESIAN_POINT('Ctrl Pts',(2.79284305788667,12.2,-10.0446575400901));
#158588=CARTESIAN_POINT('Ctrl Pts',(2.79247513274161,12.2,-10.0420726393062));
#158589=CARTESIAN_POINT('Ctrl Pts',(2.79210727597156,12.2,-10.0395399975871));
#158590=CARTESIAN_POINT('Ctrl Pts',(2.79173941923493,12.2,-10.0370073560981));
#158591=CARTESIAN_POINT('Ctrl Pts',(2.79137163194678,12.2,-10.034526975124));
#158592=CARTESIAN_POINT('Ctrl Pts',(2.79100459704178,12.2,-10.0320995765344));
#158593=CARTESIAN_POINT('Ctrl Pts',(2.79063756213678,12.2,-10.0296721779447));
#158594=CARTESIAN_POINT('Ctrl Pts',(2.79027127675155,12.2,-10.0272977614972));
#158595=CARTESIAN_POINT('Ctrl Pts',(2.78990645001471,12.2,-10.0249770699946));
#158596=CARTESIAN_POINT('Ctrl Pts',(2.78954162324473,12.2,-10.0226563782811));
#158597=CARTESIAN_POINT('Ctrl Pts',(2.78917825150261,12.2,-10.020389410239));
#158598=CARTESIAN_POINT('Ctrl Pts',(2.78881706296501,12.2,-10.0181769245944));
#158599=CARTESIAN_POINT('Ctrl Pts',(2.78845587446021,12.2,-10.0159644391507));
#158600=CARTESIAN_POINT('Ctrl Pts',(2.78809686787867,12.2,-10.0138064380068));
#158601=CARTESIAN_POINT('Ctrl Pts',(2.78774079347494,12.2,-10.0117036987499));
#158602=CARTESIAN_POINT('Ctrl Pts',(2.78738471907121,12.2,-10.009600959493));
#158603=CARTESIAN_POINT('Ctrl Pts',(2.78703157778039,12.2,-10.0075534820314));
#158604=CARTESIAN_POINT('Ctrl Pts',(2.78668213952542,12.2,-10.005562067751));
#158605=CARTESIAN_POINT('Ctrl Pts',(2.7863327012387,12.2,-10.0035706532898));
#158606=CARTESIAN_POINT('Ctrl Pts',(2.78598696746437,12.2,-10.0016352993104));
#158607=CARTESIAN_POINT('Ctrl Pts',(2.78564573894608,12.2,-9.99975683004517));
#158608=CARTESIAN_POINT('Ctrl Pts',(2.78530614810647,12.2,-9.99788737623124));
#158609=CARTESIAN_POINT('Ctrl Pts',(2.78497101114222,12.2,-9.99607425962044));
#158610=CARTESIAN_POINT('Ctrl Pts',(2.78464115899994,12.2,-9.99431831700001));
#158611=CARTESIAN_POINT('Ctrl Pts',(2.78464115899994,15.2,-9.99431831700001));
#158612=CARTESIAN_POINT('Ctrl Pts',(2.78497101114222,15.2,-9.99607425962044));
#158613=CARTESIAN_POINT('Ctrl Pts',(2.78530614810647,15.2,-9.99788737623122));
#158614=CARTESIAN_POINT('Ctrl Pts',(2.78564573894608,15.2,-9.99975683004517));
#158615=CARTESIAN_POINT('Ctrl Pts',(2.78598696746438,15.2,-10.0016352993104));
#158616=CARTESIAN_POINT('Ctrl Pts',(2.7863327012387,15.2,-10.0035706532898));
#158617=CARTESIAN_POINT('Ctrl Pts',(2.78668213952542,15.2,-10.005562067751));
#158618=CARTESIAN_POINT('Ctrl Pts',(2.78703157778039,15.2,-10.0075534820314));
#158619=CARTESIAN_POINT('Ctrl Pts',(2.78738471907121,15.2,-10.009600959493));
#158620=CARTESIAN_POINT('Ctrl Pts',(2.78774079347494,15.2,-10.0117036987499));
#158621=CARTESIAN_POINT('Ctrl Pts',(2.78809686787867,15.2,-10.0138064380068));
#158622=CARTESIAN_POINT('Ctrl Pts',(2.78845587446022,15.2,-10.0159644391507));
#158623=CARTESIAN_POINT('Ctrl Pts',(2.78881706296501,15.2,-10.0181769245944));
#158624=CARTESIAN_POINT('Ctrl Pts',(2.7891782515026,15.2,-10.0203894102389));
#158625=CARTESIAN_POINT('Ctrl Pts',(2.78954162324472,15.2,-10.0226563782811));
#158626=CARTESIAN_POINT('Ctrl Pts',(2.78990645001471,15.2,-10.0249770699945));
#158627=CARTESIAN_POINT('Ctrl Pts',(2.79027127675155,15.2,-10.0272977614972));
#158628=CARTESIAN_POINT('Ctrl Pts',(2.79063756213678,15.2,-10.0296721779447));
#158629=CARTESIAN_POINT('Ctrl Pts',(2.79100459704178,15.2,-10.0320995765344));
#158630=CARTESIAN_POINT('Ctrl Pts',(2.79137163194678,15.2,-10.034526975124));
#158631=CARTESIAN_POINT('Ctrl Pts',(2.79173941923493,15.2,-10.0370073560981));
#158632=CARTESIAN_POINT('Ctrl Pts',(2.79210727597156,15.2,-10.0395399975871));
#158633=CARTESIAN_POINT('Ctrl Pts',(2.79247513274161,15.2,-10.0420726393062));
#158634=CARTESIAN_POINT('Ctrl Pts',(2.79284305788667,15.2,-10.0446575400901));
#158635=CARTESIAN_POINT('Ctrl Pts',(2.79321038707332,15.2,-10.0472939940706));
#158636=CARTESIAN_POINT('Ctrl Pts',(2.79357771622659,15.2,-10.0499304478117));
#158637=CARTESIAN_POINT('Ctrl Pts',(2.79394445129986,15.2,-10.0526184564967));
#158638=CARTESIAN_POINT('Ctrl Pts',(2.79430994728653,15.2,-10.0553573263994));
#158639=CARTESIAN_POINT('Ctrl Pts',(2.79467544327319,15.2,-10.0580961963021));
#158640=CARTESIAN_POINT('Ctrl Pts',(2.79503969978494,15.2,-10.0608859306507));
#158641=CARTESIAN_POINT('Ctrl Pts',(2.79540209102186,15.2,-10.0637258525454));
#158642=CARTESIAN_POINT('Ctrl Pts',(2.79576448225877,15.2,-10.06656577444));
#158643=CARTESIAN_POINT('Ctrl Pts',(2.79612500825709,15.2,-10.0694558856313));
#158644=CARTESIAN_POINT('Ctrl Pts',(2.79648306141092,15.2,-10.0723955254378));
#158645=CARTESIAN_POINT('Ctrl Pts',(2.79684111459727,15.2,-10.0753351655114));
#158646=CARTESIAN_POINT('Ctrl Pts',(2.7971966934584,15.2,-10.0783243340313));
#158647=CARTESIAN_POINT('Ctrl Pts',(2.79754920772748,15.2,-10.0813623843657));
#158648=CARTESIAN_POINT('Ctrl Pts',(2.79790172196454,15.2,-10.0844004344241));
#158649=CARTESIAN_POINT('Ctrl Pts',(2.79825117221078,15.2,-10.0874873694316));
#158650=CARTESIAN_POINT('Ctrl Pts',(2.79859698069979,15.2,-10.0906225524985));
#158651=CARTESIAN_POINT('Ctrl Pts',(2.79894278918881,15.2,-10.0937577355654));
#158652=CARTESIAN_POINT('Ctrl Pts',(2.79928495835011,15.2,-10.0969411695684));
#158653=CARTESIAN_POINT('Ctrl Pts',(2.79962292675478,15.2,-10.1001722346144));
#158654=CARTESIAN_POINT('Ctrl Pts',(2.80001722324736,15.2,-10.1039418106971));
#158655=CARTESIAN_POINT('Ctrl Pts',(2.80040580174256,15.2,-10.1077762165708));
#158656=CARTESIAN_POINT('Ctrl Pts',(2.80078780049875,15.2,-10.1116744910597));
#158657=CARTESIAN_POINT('Ctrl Pts',(2.80111522798707,15.2,-10.1150158690196));
#158658=CARTESIAN_POINT('Ctrl Pts',(2.80143782025987,15.2,-10.1184041698702));
#158659=CARTESIAN_POINT('Ctrl Pts',(2.80175504991537,15.2,-10.1218388019089));
#158660=CARTESIAN_POINT('Ctrl Pts',(2.80207227959969,15.2,-10.1252734342596));
#158661=CARTESIAN_POINT('Ctrl Pts',(2.80238414665852,15.2,-10.1287543959148));
#158662=CARTESIAN_POINT('Ctrl Pts',(2.80269013725827,15.2,-10.1322811064423));
#158663=CARTESIAN_POINT('Ctrl Pts',(2.80299612783023,15.2,-10.1358078166495));
#158664=CARTESIAN_POINT('Ctrl Pts',(2.80329623959247,15.2,-10.1393802760467));
#158665=CARTESIAN_POINT('Ctrl Pts',(2.80358997424982,15.2,-10.142997912265));
#158666=CARTESIAN_POINT('Ctrl Pts',(2.80388370890717,15.2,-10.1466155484832));
#158667=CARTESIAN_POINT('Ctrl Pts',(2.80417106491244,15.2,-10.1502783615419));
#158668=CARTESIAN_POINT('Ctrl Pts',(2.80445155373605,15.2,-10.1539857918208));
#158669=CARTESIAN_POINT('Ctrl Pts',(2.80473204258513,15.2,-10.1576932224365));
#158670=CARTESIAN_POINT('Ctrl Pts',(2.80500566394831,15.2,-10.1614452697015));
#158671=CARTESIAN_POINT('Ctrl Pts',(2.80527194280903,15.2,-10.1652413826006));
#158672=CARTESIAN_POINT('Ctrl Pts',(2.80558260144359,15.2,-10.1696701804656));
#158673=CARTESIAN_POINT('Ctrl Pts',(2.80588326473474,15.2,-10.1741589572228));
#158674=CARTESIAN_POINT('Ctrl Pts',(2.8061731954812,15.2,-10.1787068541167));
#158675=CARTESIAN_POINT('Ctrl Pts',(2.80646312625024,15.2,-10.1832547513646));
#158676=CARTESIAN_POINT('Ctrl Pts',(2.80674232779444,15.2,-10.1878617700155));
#158677=CARTESIAN_POINT('Ctrl Pts',(2.80701008129985,15.2,-10.1925270677898));
#158678=CARTESIAN_POINT('Ctrl Pts',(2.80720133380074,15.2,-10.1958594232909));
#158679=CARTESIAN_POINT('Ctrl Pts',(2.80738674656107,15.2,-10.1992215137888));
#158680=CARTESIAN_POINT('Ctrl Pts',(2.80756606649163,15.2,-10.2026130384416));
#158681=CARTESIAN_POINT('Ctrl Pts',(2.80778125040047,15.2,-10.2066828678771));
#158682=CARTESIAN_POINT('Ctrl Pts',(2.80798765826097,15.2,-10.2107950804107));
#158683=CARTESIAN_POINT('Ctrl Pts',(2.80818486126419,15.2,-10.2149491661315));
#158684=CARTESIAN_POINT('Ctrl Pts',(2.80834919710618,15.2,-10.218410904358));
#158685=CARTESIAN_POINT('Ctrl Pts',(2.80850714112857,15.2,-10.2219017213103));
#158686=CARTESIAN_POINT('Ctrl Pts',(2.80865844953169,15.2,-10.2254213220033));
#158687=CARTESIAN_POINT('Ctrl Pts',(2.80880975793482,15.2,-10.2289409226962));
#158688=CARTESIAN_POINT('Ctrl Pts',(2.8089544304461,15.2,-10.2324893096455));
#158689=CARTESIAN_POINT('Ctrl Pts',(2.80909223051591,15.2,-10.2360661935328));
#158690=CARTESIAN_POINT('Ctrl Pts',(2.80923003058571,15.2,-10.2396430774202));
#158691=CARTESIAN_POINT('Ctrl Pts',(2.80936095711598,15.2,-10.2432484583982));
#158692=CARTESIAN_POINT('Ctrl Pts',(2.80948477628323,15.2,-10.2468820515396));
#158693=CARTESIAN_POINT('Ctrl Pts',(2.80960859545047,15.2,-10.2505156446811));
#158694=CARTESIAN_POINT('Ctrl Pts',(2.80972530584441,15.2,-10.2541774506333));
#158695=CARTESIAN_POINT('Ctrl Pts',(2.8098346809833,15.2,-10.2578671885499));
#158696=CARTESIAN_POINT('Ctrl Pts',(2.80994405612218,15.2,-10.2615569264666));
#158697=CARTESIAN_POINT('Ctrl Pts',(2.81004609506072,15.2,-10.2652745939627));
#158698=CARTESIAN_POINT('Ctrl Pts',(2.81014057270001,15.2,-10.2690199170353));
#158699=CARTESIAN_POINT('Ctrl Pts',(2.81023505033931,15.2,-10.2727652401079));
#158700=CARTESIAN_POINT('Ctrl Pts',(2.81032196679439,15.2,-10.2765382167139));
#158701=CARTESIAN_POINT('Ctrl Pts',(2.81040110123842,15.2,-10.280338574007));
#158702=CARTESIAN_POINT('Ctrl Pts',(2.81048023568246,15.2,-10.2841389313001));
#158703=CARTESIAN_POINT('Ctrl Pts',(2.81055158974336,15.2,-10.2879666677897));
#158704=CARTESIAN_POINT('Ctrl Pts',(2.81061494502073,15.2,-10.2918215143189));
#158705=CARTESIAN_POINT('Ctrl Pts',(2.81067830029809,15.2,-10.2956763608481));
#158706=CARTESIAN_POINT('Ctrl Pts',(2.81073365849251,15.2,-10.2995583151622));
#158707=CARTESIAN_POINT('Ctrl Pts',(2.81078080627208,15.2,-10.3034671141788));
#158708=CARTESIAN_POINT('Ctrl Pts',(2.81082795405164,15.2,-10.3073759131954));
#158709=CARTESIAN_POINT('Ctrl Pts',(2.81086689178798,15.2,-10.3113115518994));
#158710=CARTESIAN_POINT('Ctrl Pts',(2.81089741199562,15.2,-10.3152737700265));
#158711=CARTESIAN_POINT('Ctrl Pts',(2.81092793220327,15.2,-10.3192359881537));
#158712=CARTESIAN_POINT('Ctrl Pts',(2.81095003460243,15.2,-10.323224782873));
#158713=CARTESIAN_POINT('Ctrl Pts',(2.81096351418506,15.2,-10.3272398945418));
#158714=CARTESIAN_POINT('Ctrl Pts',(2.81097968968363,15.2,-10.3320580283693));
#158715=CARTESIAN_POINT('Ctrl Pts',(2.81098344974971,15.2,-10.3369140588243));
#158716=CARTESIAN_POINT('Ctrl Pts',(2.81097444724996,15.2,-10.3418075405022));
#158717=CARTESIAN_POINT('Ctrl Pts',(2.81096544475022,15.2,-10.34670102218));
#158718=CARTESIAN_POINT('Ctrl Pts',(2.81094368065831,15.2,-10.3516319539281));
#158719=CARTESIAN_POINT('Ctrl Pts',(2.81090881624348,15.2,-10.356599895746));
#158720=CARTESIAN_POINT('Ctrl Pts',(2.8108797625634,15.2,-10.3607398474113));
#158721=CARTESIAN_POINT('Ctrl Pts',(2.81084161164142,15.2,-10.364905502594));
#158722=CARTESIAN_POINT('Ctrl Pts',(2.81079417275301,15.2,-10.3690966069677));
#158723=CARTESIAN_POINT('Ctrl Pts',(2.81075622164022,15.2,-10.3724494906494));
#158724=CARTESIAN_POINT('Ctrl Pts',(2.81071232573732,15.2,-10.3758186640001));
#158725=CARTESIAN_POINT('Ctrl Pts',(2.81066238750935,15.2,-10.3792039989663));
#158726=CARTESIAN_POINT('Ctrl Pts',(2.8106124492882,15.2,-10.3825893334712));
#158727=CARTESIAN_POINT('Ctrl Pts',(2.81055646986062,15.2,-10.3859908288178));
#158728=CARTESIAN_POINT('Ctrl Pts',(2.81049435475499,15.2,-10.3894083592041));
#158729=CARTESIAN_POINT('Ctrl Pts',(2.8104167108666,15.2,-10.3936802725361));
#158730=CARTESIAN_POINT('Ctrl Pts',(2.81032947749463,15.2,-10.3979772409132));
#158731=CARTESIAN_POINT('Ctrl Pts',(2.81023247298125,15.2,-10.4022990200091));
#158732=CARTESIAN_POINT('Ctrl Pts',(2.81015486936632,15.2,-10.4057564434743));
#158733=CARTESIAN_POINT('Ctrl Pts',(2.81007101294404,15.2,-10.4092297451933));
#158734=CARTESIAN_POINT('Ctrl Pts',(2.80998081121184,15.2,-10.4127188022813));
#158735=CARTESIAN_POINT('Ctrl Pts',(2.80989060949194,15.2,-10.416207858894));
#158736=CARTESIAN_POINT('Ctrl Pts',(2.80979406095505,15.2,-10.4197126698872));
#158737=CARTESIAN_POINT('Ctrl Pts',(2.80969107674166,15.2,-10.423233113654));
#158738=CARTESIAN_POINT('Ctrl Pts',(2.80958809251425,15.2,-10.4267535579004));
#158739=CARTESIAN_POINT('Ctrl Pts',(2.80947867229995,15.2,-10.4302896347681));
#158740=CARTESIAN_POINT('Ctrl Pts',(2.80936272601543,15.2,-10.4338412210738));
#158741=CARTESIAN_POINT('Ctrl Pts',(2.8092467797467,15.2,-10.4373928068955));
#158742=CARTESIAN_POINT('Ctrl Pts',(2.80912430707232,15.2,-10.4409599030593));
#158743=CARTESIAN_POINT('Ctrl Pts',(2.80899522024367,15.2,-10.4445423902219));
#158744=CARTESIAN_POINT('Ctrl Pts',(2.80886613339742,15.2,-10.4481248778725));
#158745=CARTESIAN_POINT('Ctrl Pts',(2.8087304335298,15.2,-10.451722753317));
#158746=CARTESIAN_POINT('Ctrl Pts',(2.8085880325216,15.2,-10.4553358995705));
#158747=CARTESIAN_POINT('Ctrl Pts',(2.8084456315328,15.2,-10.4589490453316));
#158748=CARTESIAN_POINT('Ctrl Pts',(2.80829652852868,15.2,-10.462577459637));
#158749=CARTESIAN_POINT('Ctrl Pts',(2.80814063954212,15.2,-10.4662210266709));
#158750=CARTESIAN_POINT('Ctrl Pts',(2.80798475053432,15.2,-10.4698645942013));
#158751=CARTESIAN_POINT('Ctrl Pts',(2.80782207348489,15.2,-10.473523310555));
#158752=CARTESIAN_POINT('Ctrl Pts',(2.80765252597486,15.2,-10.4771970614941));
#158753=CARTESIAN_POINT('Ctrl Pts',(2.80748297848792,15.2,-10.4808708119328));
#158754=CARTESIAN_POINT('Ctrl Pts',(2.80730656067536,15.2,-10.4845595949709));
#158755=CARTESIAN_POINT('Ctrl Pts',(2.80712318724662,15.2,-10.4882632941111));
#158756=CARTESIAN_POINT('Ctrl Pts',(2.80693981379289,15.2,-10.4919669937559));
#158757=CARTESIAN_POINT('Ctrl Pts',(2.80674948665795,15.2,-10.4956856090854));
#158758=CARTESIAN_POINT('Ctrl Pts',(2.80655212125831,15.2,-10.4994190247333));
#158759=CARTESIAN_POINT('Ctrl Pts',(2.80635475585866,15.2,-10.5031524403812));
#158760=CARTESIAN_POINT('Ctrl Pts',(2.80615035445264,15.2,-10.5069006558781));
#158761=CARTESIAN_POINT('Ctrl Pts',(2.80593883494039,15.2,-10.5106635561402));
#158762=CARTESIAN_POINT('Ctrl Pts',(2.80572731545695,15.2,-10.5144264558896));
#158763=CARTESIAN_POINT('Ctrl Pts',(2.80550867889378,15.2,-10.5182040404485));
#158764=CARTESIAN_POINT('Ctrl Pts',(2.80528284346679,15.2,-10.521996194989));
#158765=CARTESIAN_POINT('Ctrl Pts',(2.80505700800904,15.2,-10.5257883500462));
#158766=CARTESIAN_POINT('Ctrl Pts',(2.80482397523285,15.2,-10.5295950755067));
#158767=CARTESIAN_POINT('Ctrl Pts',(2.80458366571901,15.2,-10.5334162578831));
#158768=CARTESIAN_POINT('Ctrl Pts',(2.80434335623791,15.2,-10.5372374397388));
#158769=CARTESIAN_POINT('Ctrl Pts',(2.80409576967998,15.2,-10.5410730777566));
#158770=CARTESIAN_POINT('Ctrl Pts',(2.80384082897908,15.2,-10.5449230608854));
#158771=CARTESIAN_POINT('Ctrl Pts',(2.80358588824344,15.2,-10.5487730445387));
#158772=CARTESIAN_POINT('Ctrl Pts',(2.80332359330906,15.2,-10.5526373721259));
#158773=CARTESIAN_POINT('Ctrl Pts',(2.80305386766913,15.2,-10.5565159325878));
#158774=CARTESIAN_POINT('Ctrl Pts',(2.80278414206595,15.2,-10.5603944925213));
#158775=CARTESIAN_POINT('Ctrl Pts',(2.8025069841383,15.2,-10.5642872834288));
#158776=CARTESIAN_POINT('Ctrl Pts',(2.80222232127317,15.2,-10.568194196664));
#158777=CARTESIAN_POINT('Ctrl Pts',(2.80193765836926,15.2,-10.5721011104316));
#158778=CARTESIAN_POINT('Ctrl Pts',(2.80164548692001,15.2,-10.5760221462147));
#158779=CARTESIAN_POINT('Ctrl Pts',(2.80134573545873,15.2,-10.5799571925968));
#158780=CARTESIAN_POINT('Ctrl Pts',(2.8010459840383,15.2,-10.5838922384427));
#158781=CARTESIAN_POINT('Ctrl Pts',(2.80073865119051,15.2,-10.5878412950827));
#158782=CARTESIAN_POINT('Ctrl Pts',(2.80042366431231,15.2,-10.5918042539));
#158783=CARTESIAN_POINT('Ctrl Pts',(2.80002993068235,15.2,-10.5967579528265));
#158784=CARTESIAN_POINT('Ctrl Pts',(2.79962423458771,15.2,-10.6017333720522));
#158785=CARTESIAN_POINT('Ctrl Pts',(2.79920643701889,15.2,-10.60673030219));
#158786=CARTESIAN_POINT('Ctrl Pts',(2.79878863945008,15.2,-10.6117272323277));
#158787=CARTESIAN_POINT('Ctrl Pts',(2.79835873998929,15.2,-10.6167456710605));
#158788=CARTESIAN_POINT('Ctrl Pts',(2.79791659908715,15.2,-10.6217854096705));
#158789=CARTESIAN_POINT('Ctrl Pts',(2.79756288634616,15.2,-10.6258172007782));
#158790=CARTESIAN_POINT('Ctrl Pts',(2.79720133915979,15.2,-10.629862623057));
#158791=CARTESIAN_POINT('Ctrl Pts',(2.7968318871947,15.2,-10.6339215695569));
#158792=CARTESIAN_POINT('Ctrl Pts',(2.79646243527994,15.2,-10.6379805155037));
#158793=CARTESIAN_POINT('Ctrl Pts',(2.79608507960679,15.2,-10.6420529884215));
#158794=CARTESIAN_POINT('Ctrl Pts',(2.79569974956418,15.2,-10.6461388779571));
#158795=CARTESIAN_POINT('Ctrl Pts',(2.79531441946906,15.2,-10.6502247680494));
#158796=CARTESIAN_POINT('Ctrl Pts',(2.79492111494227,15.2,-10.6543240776252));
#158797=CARTESIAN_POINT('Ctrl Pts',(2.79451976997542,15.2,-10.658436700128));
#158798=CARTESIAN_POINT('Ctrl Pts',(2.79411842506326,15.2,-10.6625493220704));
#158799=CARTESIAN_POINT('Ctrl Pts',(2.7937090362805,15.2,-10.6666752574268));
#158800=CARTESIAN_POINT('Ctrl Pts',(2.79329153959323,15.2,-10.6708144013649));
#158801=CARTESIAN_POINT('Ctrl Pts',(2.79287404284908,15.2,-10.6749535458669));
#158802=CARTESIAN_POINT('Ctrl Pts',(2.79244843563643,15.2,-10.6791058987179));
#158803=CARTESIAN_POINT('Ctrl Pts',(2.79201465349968,15.2,-10.6832713565195));
#158804=CARTESIAN_POINT('Ctrl Pts',(2.79158087142203,15.2,-10.6874368137535));
#158805=CARTESIAN_POINT('Ctrl Pts',(2.79113891289982,15.2,-10.6916153767586));
#158806=CARTESIAN_POINT('Ctrl Pts',(2.79068871354858,15.2,-10.6958069400813));
#158807=CARTESIAN_POINT('Ctrl Pts',(2.79023851413599,15.2,-10.6999985039751));
#158808=CARTESIAN_POINT('Ctrl Pts',(2.78978007311709,15.2,-10.7042030703534));
#158809=CARTESIAN_POINT('Ctrl Pts',(2.78931332525831,15.2,-10.70842053425));
#158810=CARTESIAN_POINT('Ctrl Pts',(2.78884657739954,15.2,-10.7126379981465));
#158811=CARTESIAN_POINT('Ctrl Pts',(2.78837152399258,15.2,-10.7168683615917));
#158812=CARTESIAN_POINT('Ctrl Pts',(2.7878881011876,15.2,-10.7211115214354));
#158813=CARTESIAN_POINT('Ctrl Pts',(2.78740467844849,15.2,-10.7253546807009));
#158814=CARTESIAN_POINT('Ctrl Pts',(2.786912884895,15.2,-10.7296106377989));
#158815=CARTESIAN_POINT('Ctrl Pts',(2.78641265893365,15.2,-10.7338792892471));
#158816=CARTESIAN_POINT('Ctrl Pts',(2.78578737643084,15.2,-10.7392151039935));
#158817=CARTESIAN_POINT('Ctrl Pts',(2.78514891843887,15.2,-10.7445707558777));
#158818=CARTESIAN_POINT('Ctrl Pts',(2.78449716100831,15.2,-10.749946048725));
#158819=CARTESIAN_POINT('Ctrl Pts',(2.78397575503545,15.2,-10.7542462832371));
#158820=CARTESIAN_POINT('Ctrl Pts',(2.78344583953104,15.2,-10.7585590878674));
#158821=CARTESIAN_POINT('Ctrl Pts',(2.78290735161193,15.2,-10.7628843617155));
#158822=CARTESIAN_POINT('Ctrl Pts',(2.78236886376619,15.2,-10.7672096349743));
#158823=CARTESIAN_POINT('Ctrl Pts',(2.78182180514631,15.2,-10.7715473781996));
#158824=CARTESIAN_POINT('Ctrl Pts',(2.78126611396702,15.2,-10.775897492197));
#158825=CARTESIAN_POINT('Ctrl Pts',(2.78071042271202,15.2,-10.7802476067871));
#158826=CARTESIAN_POINT('Ctrl Pts',(2.78014610013007,15.2,-10.7846100922089));
#158827=CARTESIAN_POINT('Ctrl Pts',(2.77957308493129,15.2,-10.7889848494486));
#158828=CARTESIAN_POINT('Ctrl Pts',(2.77900006981057,15.2,-10.7933596060922));
#158829=CARTESIAN_POINT('Ctrl Pts',(2.77841836502432,15.2,-10.7977466358703));
#158830=CARTESIAN_POINT('Ctrl Pts',(2.77782790857317,15.2,-10.8021458378988));
#158831=CARTESIAN_POINT('Ctrl Pts',(2.77723745204156,15.2,-10.8065450405266));
#158832=CARTESIAN_POINT('Ctrl Pts',(2.77663824584543,15.2,-10.810956418026));
#158833=CARTESIAN_POINT('Ctrl Pts',(2.77603023117004,15.2,-10.8153798721002));
#158834=CARTESIAN_POINT('Ctrl Pts',(2.77542221657749,15.2,-10.8198033255718));
#158835=CARTESIAN_POINT('Ctrl Pts',(2.77480539426876,15.2,-10.8242388543981));
#158836=CARTESIAN_POINT('Ctrl Pts',(2.77417970637605,15.2,-10.8286863636448));
#158837=CARTESIAN_POINT('Ctrl Pts',(2.7737104404352,15.2,-10.8320219957314));
#158838=CARTESIAN_POINT('Ctrl Pts',(2.77323618803636,15.2,-10.8353643661758));
#158839=CARTESIAN_POINT('Ctrl Pts',(2.77275692463779,15.2,-10.8387134343032));
#158840=CARTESIAN_POINT('Ctrl Pts',(2.77227766115215,15.2,-10.842062503039));
#158841=CARTESIAN_POINT('Ctrl Pts',(2.77179338669844,15.2,-10.8454182695767));
#158842=CARTESIAN_POINT('Ctrl Pts',(2.77130407866831,15.2,-10.848780694233));
#158843=CARTESIAN_POINT('Ctrl Pts',(2.77048856549216,15.2,-10.8543847339014));
#158844=CARTESIAN_POINT('Ctrl Pts',(2.76965906716166,15.2,-10.8600072646896));
#158845=CARTESIAN_POINT('Ctrl Pts',(2.76881547739365,15.2,-10.8656481027538));
#158846=CARTESIAN_POINT('Ctrl Pts',(2.76830932340411,15.2,-10.8690326064531));
#158847=CARTESIAN_POINT('Ctrl Pts',(2.76779809661315,15.2,-10.8724236997293));
#158848=CARTESIAN_POINT('Ctrl Pts',(2.76728177362075,15.2,-10.8758213439323));
#158849=CARTESIAN_POINT('Ctrl Pts',(2.76659334312055,15.2,-10.8803515351743));
#158850=CARTESIAN_POINT('Ctrl Pts',(2.76589585300763,15.2,-10.8848933709842));
#158851=CARTESIAN_POINT('Ctrl Pts',(2.76518924856599,15.2,-10.8894467576112));
#158852=CARTESIAN_POINT('Ctrl Pts',(2.76465929521069,15.2,-10.8928617977365));
#158853=CARTESIAN_POINT('Ctrl Pts',(2.76412421582788,15.2,-10.8962833349908));
#158854=CARTESIAN_POINT('Ctrl Pts',(2.76358398786278,15.2,-10.8997113293701));
#158855=CARTESIAN_POINT('Ctrl Pts',(2.76304375989769,15.2,-10.9031393237494));
#158856=CARTESIAN_POINT('Ctrl Pts',(2.76249838229929,15.2,-10.9065737765924));
#158857=CARTESIAN_POINT('Ctrl Pts',(2.76194783436166,15.2,-10.9100146467582));
#158858=CARTESIAN_POINT('Ctrl Pts',(2.76139728632402,15.2,-10.9134555175491));
#158859=CARTESIAN_POINT('Ctrl Pts',(2.76084156679326,15.2,-10.9169028060167));
#158860=CARTESIAN_POINT('Ctrl Pts',(2.7602806533777,15.2,-10.9203564737695));
#158861=CARTESIAN_POINT('Ctrl Pts',(2.75953276899345,15.2,-10.9249613630609));
#158862=CARTESIAN_POINT('Ctrl Pts',(2.75877565484929,15.2,-10.9295775922202));
#158863=CARTESIAN_POINT('Ctrl Pts',(2.75800925457921,15.2,-10.9342050688968));
#158864=CARTESIAN_POINT('Ctrl Pts',(2.75743445435055,15.2,-10.9376756765618));
#158865=CARTESIAN_POINT('Ctrl Pts',(2.75685443320387,15.2,-10.9411526111794));
#158866=CARTESIAN_POINT('Ctrl Pts',(2.7562691673215,15.2,-10.9446358331011));
#158867=CARTESIAN_POINT('Ctrl Pts',(2.75568390143913,15.2,-10.9481190550229));
#158868=CARTESIAN_POINT('Ctrl Pts',(2.75509339110749,15.2,-10.9516085654824));
#158869=CARTESIAN_POINT('Ctrl Pts',(2.75449761662986,15.2,-10.9551043237296));
#158870=CARTESIAN_POINT('Ctrl Pts',(2.75390184204398,15.2,-10.9586000826118));
#158871=CARTESIAN_POINT('Ctrl Pts',(2.75330080200663,15.2,-10.9621020915207));
#158872=CARTESIAN_POINT('Ctrl Pts',(2.7526944764178,15.2,-10.9656103103231));
#158873=CARTESIAN_POINT('Ctrl Pts',(2.75188604248293,15.2,-10.9702879343307));
#158874=CARTESIAN_POINT('Ctrl Pts',(2.75106820964095,15.2,-10.974976599273));
#158875=CARTESIAN_POINT('Ctrl Pts',(2.75024093054252,15.2,-10.9796762133326));
#158876=CARTESIAN_POINT('Ctrl Pts',(2.74962047119052,15.2,-10.9832009240373));
#158877=CARTESIAN_POINT('Ctrl Pts',(2.7489946975139,15.2,-10.9867317943249));
#158878=CARTESIAN_POINT('Ctrl Pts',(2.74836358912089,15.2,-10.9902687850289));
#158879=CARTESIAN_POINT('Ctrl Pts',(2.74773248061323,15.2,-10.9938057763754));
#158880=CARTESIAN_POINT('Ctrl Pts',(2.7470960371874,15.2,-10.9973488891737));
#158881=CARTESIAN_POINT('Ctrl Pts',(2.74645423913506,15.2,-11.0008980845237));
#158882=CARTESIAN_POINT('Ctrl Pts',(2.74559850859293,15.2,-11.0056303439157));
#158883=CARTESIAN_POINT('Ctrl Pts',(2.74473325802745,15.2,-11.0103734190054));
#158884=CARTESIAN_POINT('Ctrl Pts',(2.74385843898391,15.2,-11.0151272164717));
#158885=CARTESIAN_POINT('Ctrl Pts',(2.74320232467146,15.2,-11.0186925647334));
#158886=CARTESIAN_POINT('Ctrl Pts',(2.74254082774788,15.2,-11.022263945224));
#158887=CARTESIAN_POINT('Ctrl Pts',(2.74187392981425,15.2,-11.0258413208435));
#158888=CARTESIAN_POINT('Ctrl Pts',(2.74120703188062,15.2,-11.029418696463));
#158889=CARTESIAN_POINT('Ctrl Pts',(2.74053473130569,15.2,-11.0330020662821));
#158890=CARTESIAN_POINT('Ctrl Pts',(2.73985700941439,15.2,-11.0365913929842));
#158891=CARTESIAN_POINT('Ctrl Pts',(2.73917928739996,15.2,-11.0401807203384));
#158892=CARTESIAN_POINT('Ctrl Pts',(2.73849614306735,15.2,-11.0437760055109));
#158893=CARTESIAN_POINT('Ctrl Pts',(2.73780755809153,15.2,-11.047377210285));
#158894=CARTESIAN_POINT('Ctrl Pts',(2.73711897324081,15.2,-11.050978414405));
#158895=CARTESIAN_POINT('Ctrl Pts',(2.73642494695809,15.2,-11.0545855374825));
#158896=CARTESIAN_POINT('Ctrl Pts',(2.73572546007293,15.2,-11.0581985437407));
#158897=CARTESIAN_POINT('Ctrl Pts',(2.73502597318777,15.2,-11.061811549999));
#158898=CARTESIAN_POINT('Ctrl Pts',(2.73432102499712,15.2,-11.065430437293));
#158899=CARTESIAN_POINT('Ctrl Pts',(2.73361059710579,15.2,-11.0690551704118));
#158900=CARTESIAN_POINT('Ctrl Pts',(2.73290016921445,15.2,-11.0726799035306));
#158901=CARTESIAN_POINT('Ctrl Pts',(2.73218426090711,15.2,-11.0763104805487));
#158902=CARTESIAN_POINT('Ctrl Pts',(2.73146285451665,15.2,-11.07994686725));
#158903=CARTESIAN_POINT('Ctrl Pts',(2.7307414481262,15.2,-11.0835832539512));
#158904=CARTESIAN_POINT('Ctrl Pts',(2.73001454315263,15.2,-11.0872254500688));
#158905=CARTESIAN_POINT('Ctrl Pts',(2.72928212034639,15.2,-11.0908734168108));
#158906=CARTESIAN_POINT('Ctrl Pts',(2.72854969754015,15.2,-11.0945213835527));
#158907=CARTESIAN_POINT('Ctrl Pts',(2.72781175750326,15.2,-11.0981751224262));
#158908=CARTESIAN_POINT('Ctrl Pts',(2.72706828016044,15.2,-11.1018345948087));
#158909=CARTESIAN_POINT('Ctrl Pts',(2.72632480281762,15.2,-11.1054940671912));
#158910=CARTESIAN_POINT('Ctrl Pts',(2.7255757884863,15.2,-11.1091592726339));
#158911=CARTESIAN_POINT('Ctrl Pts',(2.72482121918114,15.2,-11.1128301753747));
#158912=CARTESIAN_POINT('Ctrl Pts',(2.7240666497389,15.2,-11.1165010787825));
#158913=CARTESIAN_POINT('Ctrl Pts',(2.72330652472843,15.2,-11.1201776796668));
#158914=CARTESIAN_POINT('Ctrl Pts',(2.72254082832472,15.2,-11.123859945036));
#158915=CARTESIAN_POINT('Ctrl Pts',(2.72177513206012,15.2,-11.1275422097363));
#158916=CARTESIAN_POINT('Ctrl Pts',(2.72100386497081,15.2,-11.1312301395697));
#158917=CARTESIAN_POINT('Ctrl Pts',(2.72022700716521,15.2,-11.1349236961443));
#158918=CARTESIAN_POINT('Ctrl Pts',(2.71945014935962,15.2,-11.1386172527189));
#158919=CARTESIAN_POINT('Ctrl Pts',(2.71866770180757,15.2,-11.1423164359544));
#158920=CARTESIAN_POINT('Ctrl Pts',(2.71787964049927,15.2,-11.146021201045));
#158921=CARTESIAN_POINT('Ctrl Pts',(2.71709157919096,15.2,-11.1497259661356));
#158922=CARTESIAN_POINT('Ctrl Pts',(2.7162979039086,15.2,-11.1534363114981));
#158923=CARTESIAN_POINT('Ctrl Pts',(2.71549860022571,15.2,-11.1571522050049));
#158924=CARTESIAN_POINT('Ctrl Pts',(2.71416642737248,15.2,-11.1633453610747));
#158925=CARTESIAN_POINT('Ctrl Pts',(2.71281861163052,15.2,-11.1695539323099));
#158926=CARTESIAN_POINT('Ctrl Pts',(2.71145515299994,15.2,-11.175777867));
#158927=CARTESIAN_POINT('Ctrl Pts',(1.76496130699994,15.2,-10.223773109));
#158928=CARTESIAN_POINT('Ctrl Pts',(1.76496130699994,11.6,-10.223773109));
#158929=CARTESIAN_POINT('Ctrl Pts',(1.76500562299994,15.2,-10.223941741));
#158930=CARTESIAN_POINT('Ctrl Pts',(1.76500562299994,11.6,-10.223941741));
#158931=CARTESIAN_POINT('Ctrl Pts',(1.76509588899994,15.2,-10.224284873));
#158932=CARTESIAN_POINT('Ctrl Pts',(1.76509588899994,11.6,-10.224284873));
#158933=CARTESIAN_POINT('Ctrl Pts',(1.76523291899994,15.2,-10.224804731));
#158934=CARTESIAN_POINT('Ctrl Pts',(1.76523291899994,11.6,-10.224804731));
#158935=CARTESIAN_POINT('Ctrl Pts',(1.76541803299994,15.2,-10.22550489));
#158936=CARTESIAN_POINT('Ctrl Pts',(1.76541803299994,11.6,-10.22550489));
#158937=CARTESIAN_POINT('Ctrl Pts',(1.76565305799994,15.2,-10.226390254));
#158938=CARTESIAN_POINT('Ctrl Pts',(1.76565305799994,11.6,-10.226390254));
#158939=CARTESIAN_POINT('Ctrl Pts',(1.76589279499994,15.2,-10.227289727));
#158940=CARTESIAN_POINT('Ctrl Pts',(1.76589279499994,11.6,-10.227289727));
#158941=CARTESIAN_POINT('Ctrl Pts',(1.76613589399994,15.2,-10.228198149));
#158942=CARTESIAN_POINT('Ctrl Pts',(1.76613589399994,11.6,-10.228198149));
#158943=CARTESIAN_POINT('Ctrl Pts',(1.76638236599994,15.2,-10.229115492));
#158944=CARTESIAN_POINT('Ctrl Pts',(1.76638236599994,11.6,-10.229115492));
#158945=CARTESIAN_POINT('Ctrl Pts',(1.76663221999994,15.2,-10.230041723));
#158946=CARTESIAN_POINT('Ctrl Pts',(1.76663221999994,11.6,-10.230041723));
#158947=CARTESIAN_POINT('Ctrl Pts',(1.76688546699994,15.2,-10.230976812));
#158948=CARTESIAN_POINT('Ctrl Pts',(1.76688546699994,11.6,-10.230976812));
#158949=CARTESIAN_POINT('Ctrl Pts',(1.76714211699994,15.2,-10.231920729));
#158950=CARTESIAN_POINT('Ctrl Pts',(1.76714211699994,11.6,-10.231920729));
#158951=CARTESIAN_POINT('Ctrl Pts',(1.76740218099994,15.2,-10.232873443));
#158952=CARTESIAN_POINT('Ctrl Pts',(1.76740218099994,11.6,-10.232873443));
#158953=CARTESIAN_POINT('Ctrl Pts',(1.76766566999994,15.2,-10.233834926));
#158954=CARTESIAN_POINT('Ctrl Pts',(1.76766566999994,11.6,-10.233834926));
#158955=CARTESIAN_POINT('Ctrl Pts',(1.76793259299994,15.2,-10.234805146));
#158956=CARTESIAN_POINT('Ctrl Pts',(1.76793259299994,11.6,-10.234805146));
#158957=CARTESIAN_POINT('Ctrl Pts',(1.76820295999994,15.2,-10.235784073));
#158958=CARTESIAN_POINT('Ctrl Pts',(1.76820295999994,11.6,-10.235784073));
#158959=CARTESIAN_POINT('Ctrl Pts',(1.76847678199994,15.2,-10.23677168));
#158960=CARTESIAN_POINT('Ctrl Pts',(1.76847678199994,11.6,-10.23677168));
#158961=CARTESIAN_POINT('Ctrl Pts',(1.76875406799994,15.2,-10.237767935));
#158962=CARTESIAN_POINT('Ctrl Pts',(1.76875406799994,11.6,-10.237767935));
#158963=CARTESIAN_POINT('Ctrl Pts',(1.76903482799994,15.2,-10.238772809));
#158964=CARTESIAN_POINT('Ctrl Pts',(1.76903482799994,11.6,-10.238772809));
#158965=CARTESIAN_POINT('Ctrl Pts',(1.76931907099994,15.2,-10.239786274));
#158966=CARTESIAN_POINT('Ctrl Pts',(1.76931907099994,11.6,-10.239786274));
#158967=CARTESIAN_POINT('Ctrl Pts',(1.76960680899994,15.2,-10.2408083));
#158968=CARTESIAN_POINT('Ctrl Pts',(1.76960680899994,11.6,-10.2408083));
#158969=CARTESIAN_POINT('Ctrl Pts',(1.76989805199994,15.2,-10.241838858));
#158970=CARTESIAN_POINT('Ctrl Pts',(1.76989805199994,11.6,-10.241838858));
#158971=CARTESIAN_POINT('Ctrl Pts',(1.77019280699994,15.2,-10.24287792));
#158972=CARTESIAN_POINT('Ctrl Pts',(1.77019280699994,11.6,-10.24287792));
#158973=CARTESIAN_POINT('Ctrl Pts',(1.77049108499994,15.2,-10.243925456));
#158974=CARTESIAN_POINT('Ctrl Pts',(1.77049108499994,11.6,-10.243925456));
#158975=CARTESIAN_POINT('Ctrl Pts',(1.77079289599994,15.2,-10.244981439));
#158976=CARTESIAN_POINT('Ctrl Pts',(1.77079289599994,11.6,-10.244981439));
#158977=CARTESIAN_POINT('Ctrl Pts',(1.77109824899994,15.2,-10.246045839));
#158978=CARTESIAN_POINT('Ctrl Pts',(1.77109824899994,11.6,-10.246045839));
#158979=CARTESIAN_POINT('Ctrl Pts',(1.77140715299994,15.2,-10.247118629));
#158980=CARTESIAN_POINT('Ctrl Pts',(1.77140715299994,11.6,-10.247118629));
#158981=CARTESIAN_POINT('Ctrl Pts',(1.77171961899994,15.2,-10.248199781));
#158982=CARTESIAN_POINT('Ctrl Pts',(1.77171961899994,11.6,-10.248199781));
#158983=CARTESIAN_POINT('Ctrl Pts',(1.77203565399994,15.2,-10.249289267));
#158984=CARTESIAN_POINT('Ctrl Pts',(1.77203565399994,11.6,-10.249289267));
#158985=CARTESIAN_POINT('Ctrl Pts',(1.77235526999994,15.2,-10.250387057));
#158986=CARTESIAN_POINT('Ctrl Pts',(1.77235526999994,11.6,-10.250387057));
#158987=CARTESIAN_POINT('Ctrl Pts',(1.77267847299994,15.2,-10.251493125));
#158988=CARTESIAN_POINT('Ctrl Pts',(1.77267847299994,11.6,-10.251493125));
#158989=CARTESIAN_POINT('Ctrl Pts',(1.77300527499994,15.2,-10.252607443));
#158990=CARTESIAN_POINT('Ctrl Pts',(1.77300527499994,11.6,-10.252607443));
#158991=CARTESIAN_POINT('Ctrl Pts',(1.77333568299994,15.2,-10.253729984));
#158992=CARTESIAN_POINT('Ctrl Pts',(1.77333568299994,11.6,-10.253729984));
#158993=CARTESIAN_POINT('Ctrl Pts',(1.77366970799994,15.2,-10.25486072));
#158994=CARTESIAN_POINT('Ctrl Pts',(1.77366970799994,11.6,-10.25486072));
#158995=CARTESIAN_POINT('Ctrl Pts',(1.77400735799994,15.2,-10.255999624));
#158996=CARTESIAN_POINT('Ctrl Pts',(1.77400735799994,11.6,-10.255999624));
#158997=CARTESIAN_POINT('Ctrl Pts',(1.77434864199994,15.2,-10.257146668));
#158998=CARTESIAN_POINT('Ctrl Pts',(1.77434864199994,11.6,-10.257146668));
#158999=CARTESIAN_POINT('Ctrl Pts',(1.77469356799994,15.2,-10.258301827));
#159000=CARTESIAN_POINT('Ctrl Pts',(1.77469356799994,11.6,-10.258301827));
#159001=CARTESIAN_POINT('Ctrl Pts',(1.77504214599994,15.2,-10.259465073));
#159002=CARTESIAN_POINT('Ctrl Pts',(1.77504214599994,11.6,-10.259465073));
#159003=CARTESIAN_POINT('Ctrl Pts',(1.77539438599994,15.2,-10.260636378));
#159004=CARTESIAN_POINT('Ctrl Pts',(1.77539438599994,11.6,-10.260636378));
#159005=CARTESIAN_POINT('Ctrl Pts',(1.77575029399994,15.2,-10.261815716));
#159006=CARTESIAN_POINT('Ctrl Pts',(1.77575029399994,11.6,-10.261815716));
#159007=CARTESIAN_POINT('Ctrl Pts',(1.77610987999994,15.2,-10.263003061));
#159008=CARTESIAN_POINT('Ctrl Pts',(1.77610987999994,11.6,-10.263003061));
#159009=CARTESIAN_POINT('Ctrl Pts',(1.77647315199994,15.2,-10.264198387));
#159010=CARTESIAN_POINT('Ctrl Pts',(1.77647315199994,11.6,-10.264198387));
#159011=CARTESIAN_POINT('Ctrl Pts',(1.77684011999994,15.2,-10.265401666));
#159012=CARTESIAN_POINT('Ctrl Pts',(1.77684011999994,11.6,-10.265401666));
#159013=CARTESIAN_POINT('Ctrl Pts',(1.77721079199994,15.2,-10.266612874));
#159014=CARTESIAN_POINT('Ctrl Pts',(1.77721079199994,11.6,-10.266612874));
#159015=CARTESIAN_POINT('Ctrl Pts',(1.77758517499994,15.2,-10.267831982));
#159016=CARTESIAN_POINT('Ctrl Pts',(1.77758517499994,11.6,-10.267831982));
#159017=CARTESIAN_POINT('Ctrl Pts',(1.77796327899994,15.2,-10.269058966));
#159018=CARTESIAN_POINT('Ctrl Pts',(1.77796327899994,11.6,-10.269058966));
#159019=CARTESIAN_POINT('Ctrl Pts',(1.77834511299995,15.2,-10.2702938));
#159020=CARTESIAN_POINT('Ctrl Pts',(1.77834511299995,11.6,-10.2702938));
#159021=CARTESIAN_POINT('Ctrl Pts',(1.77873068199994,15.2,-10.271536458));
#159022=CARTESIAN_POINT('Ctrl Pts',(1.77873068199994,11.6,-10.271536458));
#159023=CARTESIAN_POINT('Ctrl Pts',(1.77911999799994,15.2,-10.272786914));
#159024=CARTESIAN_POINT('Ctrl Pts',(1.77911999799994,11.6,-10.272786914));
#159025=CARTESIAN_POINT('Ctrl Pts',(1.77951306799994,15.2,-10.274045143));
#159026=CARTESIAN_POINT('Ctrl Pts',(1.77951306799994,11.6,-10.274045143));
#159027=CARTESIAN_POINT('Ctrl Pts',(1.77990989999994,15.2,-10.275311119));
#159028=CARTESIAN_POINT('Ctrl Pts',(1.77990989999994,11.6,-10.275311119));
#159029=CARTESIAN_POINT('Ctrl Pts',(1.78031050099994,15.2,-10.276584816));
#159030=CARTESIAN_POINT('Ctrl Pts',(1.78031050099994,11.6,-10.276584816));
#159031=CARTESIAN_POINT('Ctrl Pts',(1.78071487999994,15.2,-10.27786621));
#159032=CARTESIAN_POINT('Ctrl Pts',(1.78071487999994,11.6,-10.27786621));
#159033=CARTESIAN_POINT('Ctrl Pts',(1.78112304599994,15.2,-10.279155276));
#159034=CARTESIAN_POINT('Ctrl Pts',(1.78112304599994,11.6,-10.279155276));
#159035=CARTESIAN_POINT('Ctrl Pts',(1.78153500599994,15.2,-10.280451988));
#159036=CARTESIAN_POINT('Ctrl Pts',(1.78153500599994,11.6,-10.280451988));
#159037=CARTESIAN_POINT('Ctrl Pts',(1.78195076699994,15.2,-10.281756321));
#159038=CARTESIAN_POINT('Ctrl Pts',(1.78195076699994,11.6,-10.281756321));
#159039=CARTESIAN_POINT('Ctrl Pts',(1.78237033899994,15.2,-10.283068252));
#159040=CARTESIAN_POINT('Ctrl Pts',(1.78237033899994,11.6,-10.283068252));
#159041=CARTESIAN_POINT('Ctrl Pts',(1.78279372899994,15.2,-10.284387754));
#159042=CARTESIAN_POINT('Ctrl Pts',(1.78279372899994,11.6,-10.284387754));
#159043=CARTESIAN_POINT('Ctrl Pts',(1.78322094399994,15.2,-10.285714803));
#159044=CARTESIAN_POINT('Ctrl Pts',(1.78322094399994,11.6,-10.285714803));
#159045=CARTESIAN_POINT('Ctrl Pts',(1.78365199299995,15.2,-10.287049375));
#159046=CARTESIAN_POINT('Ctrl Pts',(1.78365199299995,11.6,-10.287049375));
#159047=CARTESIAN_POINT('Ctrl Pts',(1.78408688299994,15.2,-10.288391446));
#159048=CARTESIAN_POINT('Ctrl Pts',(1.78408688299994,11.6,-10.288391446));
#159049=CARTESIAN_POINT('Ctrl Pts',(1.78452562099994,15.2,-10.28974099));
#159050=CARTESIAN_POINT('Ctrl Pts',(1.78452562099994,11.6,-10.28974099));
#159051=CARTESIAN_POINT('Ctrl Pts',(1.78496821499994,15.2,-10.291097983));
#159052=CARTESIAN_POINT('Ctrl Pts',(1.78496821499994,11.6,-10.291097983));
#159053=CARTESIAN_POINT('Ctrl Pts',(1.78541467399994,15.2,-10.292462403));
#159054=CARTESIAN_POINT('Ctrl Pts',(1.78541467399994,11.6,-10.292462403));
#159055=CARTESIAN_POINT('Ctrl Pts',(1.78586500399994,15.2,-10.293834224));
#159056=CARTESIAN_POINT('Ctrl Pts',(1.78586500399994,11.6,-10.293834224));
#159057=CARTESIAN_POINT('Ctrl Pts',(1.78631921299994,15.2,-10.295213422));
#159058=CARTESIAN_POINT('Ctrl Pts',(1.78631921299994,11.6,-10.295213422));
#159059=CARTESIAN_POINT('Ctrl Pts',(1.78677730899994,15.2,-10.296599975));
#159060=CARTESIAN_POINT('Ctrl Pts',(1.78677730899994,11.6,-10.296599975));
#159061=CARTESIAN_POINT('Ctrl Pts',(1.78723929699994,15.2,-10.297993858));
#159062=CARTESIAN_POINT('Ctrl Pts',(1.78723929699994,11.6,-10.297993858));
#159063=CARTESIAN_POINT('Ctrl Pts',(1.78770518699994,15.2,-10.299395046));
#159064=CARTESIAN_POINT('Ctrl Pts',(1.78770518699994,11.6,-10.299395046));
#159065=CARTESIAN_POINT('Ctrl Pts',(1.78817498599994,15.2,-10.300803517));
#159066=CARTESIAN_POINT('Ctrl Pts',(1.78817498599994,11.6,-10.300803517));
#159067=CARTESIAN_POINT('Ctrl Pts',(1.78864869999994,15.2,-10.302219248));
#159068=CARTESIAN_POINT('Ctrl Pts',(1.78864869999994,11.6,-10.302219248));
#159069=CARTESIAN_POINT('Ctrl Pts',(1.78912633699994,15.2,-10.303642215));
#159070=CARTESIAN_POINT('Ctrl Pts',(1.78912633699994,11.6,-10.303642215));
#159071=CARTESIAN_POINT('Ctrl Pts',(1.78960790399994,15.2,-10.305072393));
#159072=CARTESIAN_POINT('Ctrl Pts',(1.78960790399994,11.6,-10.305072393));
#159073=CARTESIAN_POINT('Ctrl Pts',(1.79009340899994,15.2,-10.306509762));
#159074=CARTESIAN_POINT('Ctrl Pts',(1.79009340899994,11.6,-10.306509762));
#159075=CARTESIAN_POINT('Ctrl Pts',(1.79058285799994,15.2,-10.307954296));
#159076=CARTESIAN_POINT('Ctrl Pts',(1.79058285799994,11.6,-10.307954296));
#159077=CARTESIAN_POINT('Ctrl Pts',(1.79107625799994,15.2,-10.309405975));
#159078=CARTESIAN_POINT('Ctrl Pts',(1.79107625799994,11.6,-10.309405975));
#159079=CARTESIAN_POINT('Ctrl Pts',(1.79157361699994,15.2,-10.310864772));
#159080=CARTESIAN_POINT('Ctrl Pts',(1.79157361699994,11.6,-10.310864772));
#159081=CARTESIAN_POINT('Ctrl Pts',(1.79207494099994,15.2,-10.312330668));
#159082=CARTESIAN_POINT('Ctrl Pts',(1.79207494099994,11.6,-10.312330668));
#159083=CARTESIAN_POINT('Ctrl Pts',(1.79258023699994,15.2,-10.313803638));
#159084=CARTESIAN_POINT('Ctrl Pts',(1.79258023699994,11.6,-10.313803638));
#159085=CARTESIAN_POINT('Ctrl Pts',(1.79308951199994,15.2,-10.315283661));
#159086=CARTESIAN_POINT('Ctrl Pts',(1.79308951199994,11.6,-10.315283661));
#159087=CARTESIAN_POINT('Ctrl Pts',(1.79360277399994,15.2,-10.316770712));
#159088=CARTESIAN_POINT('Ctrl Pts',(1.79360277399994,11.6,-10.316770712));
#159089=CARTESIAN_POINT('Ctrl Pts',(1.79412002899994,15.2,-10.318264771));
#159090=CARTESIAN_POINT('Ctrl Pts',(1.79412002899994,11.6,-10.318264771));
#159091=CARTESIAN_POINT('Ctrl Pts',(1.79464128299994,15.2,-10.319765813));
#159092=CARTESIAN_POINT('Ctrl Pts',(1.79464128299994,11.6,-10.319765813));
#159093=CARTESIAN_POINT('Ctrl Pts',(1.79516654299994,15.2,-10.321273818));
#159094=CARTESIAN_POINT('Ctrl Pts',(1.79516654299994,11.6,-10.321273818));
#159095=CARTESIAN_POINT('Ctrl Pts',(1.79569581699994,15.2,-10.322788763));
#159096=CARTESIAN_POINT('Ctrl Pts',(1.79569581699994,11.6,-10.322788763));
#159097=CARTESIAN_POINT('Ctrl Pts',(1.79622910999994,15.2,-10.324310627));
#159098=CARTESIAN_POINT('Ctrl Pts',(1.79622910999994,11.6,-10.324310627));
#159099=CARTESIAN_POINT('Ctrl Pts',(1.79676642999994,15.2,-10.325839385));
#159100=CARTESIAN_POINT('Ctrl Pts',(1.79676642999994,11.6,-10.325839385));
#159101=CARTESIAN_POINT('Ctrl Pts',(1.79730778399994,15.2,-10.327375017));
#159102=CARTESIAN_POINT('Ctrl Pts',(1.79730778399994,11.6,-10.327375017));
#159103=CARTESIAN_POINT('Ctrl Pts',(1.79785317499994,15.2,-10.328917501));
#159104=CARTESIAN_POINT('Ctrl Pts',(1.79785317499994,11.6,-10.328917501));
#159105=CARTESIAN_POINT('Ctrl Pts',(1.79840261399994,15.2,-10.330466814));
#159106=CARTESIAN_POINT('Ctrl Pts',(1.79840261399994,11.6,-10.330466814));
#159107=CARTESIAN_POINT('Ctrl Pts',(1.79895610399994,15.2,-10.332022936));
#159108=CARTESIAN_POINT('Ctrl Pts',(1.79895610399994,11.6,-10.332022936));
#159109=CARTESIAN_POINT('Ctrl Pts',(1.79951365499994,15.2,-10.333585844));
#159110=CARTESIAN_POINT('Ctrl Pts',(1.79951365499994,11.6,-10.333585844));
#159111=CARTESIAN_POINT('Ctrl Pts',(1.80007526999994,15.2,-10.335155517));
#159112=CARTESIAN_POINT('Ctrl Pts',(1.80007526999994,11.6,-10.335155517));
#159113=CARTESIAN_POINT('Ctrl Pts',(1.80064095699994,15.2,-10.336731933));
#159114=CARTESIAN_POINT('Ctrl Pts',(1.80064095699994,11.6,-10.336731933));
#159115=CARTESIAN_POINT('Ctrl Pts',(1.80121072099994,15.2,-10.338315071));
#159116=CARTESIAN_POINT('Ctrl Pts',(1.80121072099994,11.6,-10.338315071));
#159117=CARTESIAN_POINT('Ctrl Pts',(1.80178457199994,15.2,-10.33990491));
#159118=CARTESIAN_POINT('Ctrl Pts',(1.80178457199994,11.6,-10.33990491));
#159119=CARTESIAN_POINT('Ctrl Pts',(1.80236250999994,15.2,-10.341501427));
#159120=CARTESIAN_POINT('Ctrl Pts',(1.80236250999994,11.6,-10.341501427));
#159121=CARTESIAN_POINT('Ctrl Pts',(1.80294454699994,15.2,-10.343104603));
#159122=CARTESIAN_POINT('Ctrl Pts',(1.80294454699994,11.6,-10.343104603));
#159123=CARTESIAN_POINT('Ctrl Pts',(1.80353068699994,15.2,-10.344714415));
#159124=CARTESIAN_POINT('Ctrl Pts',(1.80353068699994,11.6,-10.344714415));
#159125=CARTESIAN_POINT('Ctrl Pts',(1.80412093499994,15.2,-10.346330843));
#159126=CARTESIAN_POINT('Ctrl Pts',(1.80412093499994,11.6,-10.346330843));
#159127=CARTESIAN_POINT('Ctrl Pts',(1.80471529899994,15.2,-10.347953866));
#159128=CARTESIAN_POINT('Ctrl Pts',(1.80471529899994,11.6,-10.347953866));
#159129=CARTESIAN_POINT('Ctrl Pts',(1.80531378399994,15.2,-10.349583463));
#159130=CARTESIAN_POINT('Ctrl Pts',(1.80531378399994,11.6,-10.349583463));
#159131=CARTESIAN_POINT('Ctrl Pts',(1.80591639699994,15.2,-10.351219612));
#159132=CARTESIAN_POINT('Ctrl Pts',(1.80591639699994,11.6,-10.351219612));
#159133=CARTESIAN_POINT('Ctrl Pts',(1.80652314299994,15.2,-10.352862295));
#159134=CARTESIAN_POINT('Ctrl Pts',(1.80652314299994,11.6,-10.352862295));
#159135=CARTESIAN_POINT('Ctrl Pts',(1.80713402799994,15.2,-10.354511488));
#159136=CARTESIAN_POINT('Ctrl Pts',(1.80713402799994,11.6,-10.354511488));
#159137=CARTESIAN_POINT('Ctrl Pts',(1.80774905899994,15.2,-10.356167172));
#159138=CARTESIAN_POINT('Ctrl Pts',(1.80774905899994,11.6,-10.356167172));
#159139=CARTESIAN_POINT('Ctrl Pts',(1.80836823999994,15.2,-10.357829328));
#159140=CARTESIAN_POINT('Ctrl Pts',(1.80836823999994,11.6,-10.357829328));
#159141=CARTESIAN_POINT('Ctrl Pts',(1.80899157899994,15.2,-10.359497933));
#159142=CARTESIAN_POINT('Ctrl Pts',(1.80899157899994,11.6,-10.359497933));
#159143=CARTESIAN_POINT('Ctrl Pts',(1.80961908099994,15.2,-10.361172966));
#159144=CARTESIAN_POINT('Ctrl Pts',(1.80961908099994,11.6,-10.361172966));
#159145=CARTESIAN_POINT('Ctrl Pts',(1.81025075099994,15.2,-10.36285441));
#159146=CARTESIAN_POINT('Ctrl Pts',(1.81025075099994,11.6,-10.36285441));
#159147=CARTESIAN_POINT('Ctrl Pts',(1.81088659599994,15.2,-10.364542242));
#159148=CARTESIAN_POINT('Ctrl Pts',(1.81088659599994,11.6,-10.364542242));
#159149=CARTESIAN_POINT('Ctrl Pts',(1.81152661999994,15.2,-10.366236444));
#159150=CARTESIAN_POINT('Ctrl Pts',(1.81152661999994,11.6,-10.366236444));
#159151=CARTESIAN_POINT('Ctrl Pts',(1.81217083099994,15.2,-10.367936993));
#159152=CARTESIAN_POINT('Ctrl Pts',(1.81217083099994,11.6,-10.367936993));
#159153=CARTESIAN_POINT('Ctrl Pts',(1.81281923299994,15.2,-10.369643871));
#159154=CARTESIAN_POINT('Ctrl Pts',(1.81281923299994,11.6,-10.369643871));
#159155=CARTESIAN_POINT('Ctrl Pts',(1.81347183299994,15.2,-10.371357057));
#159156=CARTESIAN_POINT('Ctrl Pts',(1.81347183299994,11.6,-10.371357057));
#159157=CARTESIAN_POINT('Ctrl Pts',(1.81412863499994,15.2,-10.373076533));
#159158=CARTESIAN_POINT('Ctrl Pts',(1.81412863499994,11.6,-10.373076533));
#159159=CARTESIAN_POINT('Ctrl Pts',(1.81478964499994,15.2,-10.374802277));
#159160=CARTESIAN_POINT('Ctrl Pts',(1.81478964499994,11.6,-10.374802277));
#159161=CARTESIAN_POINT('Ctrl Pts',(1.81545486999994,15.2,-10.37653427));
#159162=CARTESIAN_POINT('Ctrl Pts',(1.81545486999994,11.6,-10.37653427));
#159163=CARTESIAN_POINT('Ctrl Pts',(1.81612431399994,15.2,-10.378272492));
#159164=CARTESIAN_POINT('Ctrl Pts',(1.81612431399994,11.6,-10.378272492));
#159165=CARTESIAN_POINT('Ctrl Pts',(1.81679798299994,15.2,-10.380016924));
#159166=CARTESIAN_POINT('Ctrl Pts',(1.81679798299994,11.6,-10.380016924));
#159167=CARTESIAN_POINT('Ctrl Pts',(1.81747588199994,15.2,-10.381767545));
#159168=CARTESIAN_POINT('Ctrl Pts',(1.81747588199994,11.6,-10.381767545));
#159169=CARTESIAN_POINT('Ctrl Pts',(1.81815801699994,15.2,-10.383524338));
#159170=CARTESIAN_POINT('Ctrl Pts',(1.81815801699994,11.6,-10.383524338));
#159171=CARTESIAN_POINT('Ctrl Pts',(1.81884439299994,15.2,-10.385287281));
#159172=CARTESIAN_POINT('Ctrl Pts',(1.81884439299994,11.6,-10.385287281));
#159173=CARTESIAN_POINT('Ctrl Pts',(1.81953501599994,15.2,-10.387056356));
#159174=CARTESIAN_POINT('Ctrl Pts',(1.81953501599994,11.6,-10.387056356));
#159175=CARTESIAN_POINT('Ctrl Pts',(1.82022989099994,15.2,-10.388831543));
#159176=CARTESIAN_POINT('Ctrl Pts',(1.82022989099994,11.6,-10.388831543));
#159177=CARTESIAN_POINT('Ctrl Pts',(1.82092902199994,15.2,-10.390612824));
#159178=CARTESIAN_POINT('Ctrl Pts',(1.82092902199994,11.6,-10.390612824));
#159179=CARTESIAN_POINT('Ctrl Pts',(1.82163241599994,15.2,-10.392400178));
#159180=CARTESIAN_POINT('Ctrl Pts',(1.82163241599994,11.6,-10.392400178));
#159181=CARTESIAN_POINT('Ctrl Pts',(1.82234007799994,15.2,-10.394193587));
#159182=CARTESIAN_POINT('Ctrl Pts',(1.82234007799994,11.6,-10.394193587));
#159183=CARTESIAN_POINT('Ctrl Pts',(1.82305201199994,15.2,-10.395993031));
#159184=CARTESIAN_POINT('Ctrl Pts',(1.82305201199994,11.6,-10.395993031));
#159185=CARTESIAN_POINT('Ctrl Pts',(1.82376822599994,15.2,-10.397798492));
#159186=CARTESIAN_POINT('Ctrl Pts',(1.82376822599994,11.6,-10.397798492));
#159187=CARTESIAN_POINT('Ctrl Pts',(1.82448872099994,15.2,-10.399609952));
#159188=CARTESIAN_POINT('Ctrl Pts',(1.82448872099994,11.6,-10.399609952));
#159189=CARTESIAN_POINT('Ctrl Pts',(1.82521350499994,15.2,-10.401427389));
#159190=CARTESIAN_POINT('Ctrl Pts',(1.82521350499994,11.6,-10.401427389));
#159191=CARTESIAN_POINT('Ctrl Pts',(1.82594258299994,15.2,-10.403250787));
#159192=CARTESIAN_POINT('Ctrl Pts',(1.82594258299994,11.6,-10.403250787));
#159193=CARTESIAN_POINT('Ctrl Pts',(1.82667595799994,15.2,-10.405080125));
#159194=CARTESIAN_POINT('Ctrl Pts',(1.82667595799994,11.6,-10.405080125));
#159195=CARTESIAN_POINT('Ctrl Pts',(1.82741363699994,15.2,-10.406915387));
#159196=CARTESIAN_POINT('Ctrl Pts',(1.82741363699994,11.6,-10.406915387));
#159197=CARTESIAN_POINT('Ctrl Pts',(1.82815562499994,15.2,-10.408756552));
#159198=CARTESIAN_POINT('Ctrl Pts',(1.82815562499994,11.6,-10.408756552));
#159199=CARTESIAN_POINT('Ctrl Pts',(1.82890192699994,15.2,-10.410603603));
#159200=CARTESIAN_POINT('Ctrl Pts',(1.82890192699994,11.6,-10.410603603));
#159201=CARTESIAN_POINT('Ctrl Pts',(1.82965254599994,15.2,-10.41245652));
#159202=CARTESIAN_POINT('Ctrl Pts',(1.82965254599994,11.6,-10.41245652));
#159203=CARTESIAN_POINT('Ctrl Pts',(1.83040748999994,15.2,-10.414315286));
#159204=CARTESIAN_POINT('Ctrl Pts',(1.83040748999994,11.6,-10.414315286));
#159205=CARTESIAN_POINT('Ctrl Pts',(1.83116676099994,15.2,-10.416179881));
#159206=CARTESIAN_POINT('Ctrl Pts',(1.83116676099994,11.6,-10.416179881));
#159207=CARTESIAN_POINT('Ctrl Pts',(1.83193036499994,15.2,-10.418050288));
#159208=CARTESIAN_POINT('Ctrl Pts',(1.83193036499994,11.6,-10.418050288));
#159209=CARTESIAN_POINT('Ctrl Pts',(1.83269830799994,15.2,-10.419926488));
#159210=CARTESIAN_POINT('Ctrl Pts',(1.83269830799994,11.6,-10.419926488));
#159211=CARTESIAN_POINT('Ctrl Pts',(1.83347059199994,15.2,-10.421808463));
#159212=CARTESIAN_POINT('Ctrl Pts',(1.83347059199994,11.6,-10.421808463));
#159213=CARTESIAN_POINT('Ctrl Pts',(1.83424722399994,15.2,-10.423696194));
#159214=CARTESIAN_POINT('Ctrl Pts',(1.83424722399994,11.6,-10.423696194));
#159215=CARTESIAN_POINT('Ctrl Pts',(1.83502820899994,15.2,-10.425589665));
#159216=CARTESIAN_POINT('Ctrl Pts',(1.83502820899994,11.6,-10.425589665));
#159217=CARTESIAN_POINT('Ctrl Pts',(1.83581354999994,15.2,-10.427488857));
#159218=CARTESIAN_POINT('Ctrl Pts',(1.83581354999994,11.6,-10.427488857));
#159219=CARTESIAN_POINT('Ctrl Pts',(1.83660325299994,15.2,-10.429393751));
#159220=CARTESIAN_POINT('Ctrl Pts',(1.83660325299994,11.6,-10.429393751));
#159221=CARTESIAN_POINT('Ctrl Pts',(1.83739732299994,15.2,-10.431304329));
#159222=CARTESIAN_POINT('Ctrl Pts',(1.83739732299994,11.6,-10.431304329));
#159223=CARTESIAN_POINT('Ctrl Pts',(1.83819576299994,15.2,-10.433220574));
#159224=CARTESIAN_POINT('Ctrl Pts',(1.83819576299994,11.6,-10.433220574));
#159225=CARTESIAN_POINT('Ctrl Pts',(1.83899857899994,15.2,-10.435142468));
#159226=CARTESIAN_POINT('Ctrl Pts',(1.83899857899994,11.6,-10.435142468));
#159227=CARTESIAN_POINT('Ctrl Pts',(1.83980577599994,15.2,-10.437069993));
#159228=CARTESIAN_POINT('Ctrl Pts',(1.83980577599994,11.6,-10.437069993));
#159229=CARTESIAN_POINT('Ctrl Pts',(1.84061735599994,15.2,-10.439003132));
#159230=CARTESIAN_POINT('Ctrl Pts',(1.84061735599994,11.6,-10.439003132));
#159231=CARTESIAN_POINT('Ctrl Pts',(1.84143332699994,15.2,-10.440941867));
#159232=CARTESIAN_POINT('Ctrl Pts',(1.84143332699994,11.6,-10.440941867));
#159233=CARTESIAN_POINT('Ctrl Pts',(1.84225369099994,15.2,-10.442886179));
#159234=CARTESIAN_POINT('Ctrl Pts',(1.84225369099994,11.6,-10.442886179));
#159235=CARTESIAN_POINT('Ctrl Pts',(1.84307845299994,15.2,-10.444836053));
#159236=CARTESIAN_POINT('Ctrl Pts',(1.84307845299994,11.6,-10.444836053));
#159237=CARTESIAN_POINT('Ctrl Pts',(1.84390761699994,15.2,-10.446791469));
#159238=CARTESIAN_POINT('Ctrl Pts',(1.84390761699994,11.6,-10.446791469));
#159239=CARTESIAN_POINT('Ctrl Pts',(1.84474118899994,15.2,-10.44875241));
#159240=CARTESIAN_POINT('Ctrl Pts',(1.84474118899994,11.6,-10.44875241));
#159241=CARTESIAN_POINT('Ctrl Pts',(1.84557917199994,15.2,-10.45071886));
#159242=CARTESIAN_POINT('Ctrl Pts',(1.84557917199994,11.6,-10.45071886));
#159243=CARTESIAN_POINT('Ctrl Pts',(1.84642157199994,15.2,-10.452690801));
#159244=CARTESIAN_POINT('Ctrl Pts',(1.84642157199994,11.6,-10.452690801));
#159245=CARTESIAN_POINT('Ctrl Pts',(1.84726839199994,15.2,-10.454668215));
#159246=CARTESIAN_POINT('Ctrl Pts',(1.84726839199994,11.6,-10.454668215));
#159247=CARTESIAN_POINT('Ctrl Pts',(1.84811963599994,15.2,-10.456651085));
#159248=CARTESIAN_POINT('Ctrl Pts',(1.84811963599994,11.6,-10.456651085));
#159249=CARTESIAN_POINT('Ctrl Pts',(1.84897530999994,15.2,-10.458639395));
#159250=CARTESIAN_POINT('Ctrl Pts',(1.84897530999994,11.6,-10.458639395));
#159251=CARTESIAN_POINT('Ctrl Pts',(1.84983541599994,15.2,-10.460633126));
#159252=CARTESIAN_POINT('Ctrl Pts',(1.84983541599994,11.6,-10.460633126));
#159253=CARTESIAN_POINT('Ctrl Pts',(1.85069995999994,15.2,-10.462632262));
#159254=CARTESIAN_POINT('Ctrl Pts',(1.85069995999994,11.6,-10.462632262));
#159255=CARTESIAN_POINT('Ctrl Pts',(1.85156894599994,15.2,-10.464636786));
#159256=CARTESIAN_POINT('Ctrl Pts',(1.85156894599994,11.6,-10.464636786));
#159257=CARTESIAN_POINT('Ctrl Pts',(1.85244237799994,15.2,-10.46664668));
#159258=CARTESIAN_POINT('Ctrl Pts',(1.85244237799994,11.6,-10.46664668));
#159259=CARTESIAN_POINT('Ctrl Pts',(1.85332025899994,15.2,-10.468661929));
#159260=CARTESIAN_POINT('Ctrl Pts',(1.85332025899994,11.6,-10.468661929));
#159261=CARTESIAN_POINT('Ctrl Pts',(1.85420259499994,15.2,-10.470682514));
#159262=CARTESIAN_POINT('Ctrl Pts',(1.85420259499994,11.6,-10.470682514));
#159263=CARTESIAN_POINT('Ctrl Pts',(1.85508938999994,15.2,-10.47270842));
#159264=CARTESIAN_POINT('Ctrl Pts',(1.85508938999994,11.6,-10.47270842));
#159265=CARTESIAN_POINT('Ctrl Pts',(1.85598064599994,15.2,-10.474739628));
#159266=CARTESIAN_POINT('Ctrl Pts',(1.85598064599994,11.6,-10.474739628));
#159267=CARTESIAN_POINT('Ctrl Pts',(1.85687636999994,15.2,-10.476776123));
#159268=CARTESIAN_POINT('Ctrl Pts',(1.85687636999994,11.6,-10.476776123));
#159269=CARTESIAN_POINT('Ctrl Pts',(1.85777656499994,15.2,-10.478817888));
#159270=CARTESIAN_POINT('Ctrl Pts',(1.85777656499994,11.6,-10.478817888));
#159271=CARTESIAN_POINT('Ctrl Pts',(1.85868123399994,15.2,-10.480864906));
#159272=CARTESIAN_POINT('Ctrl Pts',(1.85868123399994,11.6,-10.480864906));
#159273=CARTESIAN_POINT('Ctrl Pts',(1.85959038199994,15.2,-10.48291716));
#159274=CARTESIAN_POINT('Ctrl Pts',(1.85959038199994,11.6,-10.48291716));
#159275=CARTESIAN_POINT('Ctrl Pts',(1.86050401199994,15.2,-10.484974634));
#159276=CARTESIAN_POINT('Ctrl Pts',(1.86050401199994,11.6,-10.484974634));
#159277=CARTESIAN_POINT('Ctrl Pts',(1.86142212899994,15.2,-10.487037312));
#159278=CARTESIAN_POINT('Ctrl Pts',(1.86142212899994,11.6,-10.487037312));
#159279=CARTESIAN_POINT('Ctrl Pts',(1.86234473699994,15.2,-10.489105177));
#159280=CARTESIAN_POINT('Ctrl Pts',(1.86234473699994,11.6,-10.489105177));
#159281=CARTESIAN_POINT('Ctrl Pts',(1.86327183899994,15.2,-10.491178213));
#159282=CARTESIAN_POINT('Ctrl Pts',(1.86327183899994,11.6,-10.491178213));
#159283=CARTESIAN_POINT('Ctrl Pts',(1.86420344099994,15.2,-10.493256403));
#159284=CARTESIAN_POINT('Ctrl Pts',(1.86420344099994,11.6,-10.493256403));
#159285=CARTESIAN_POINT('Ctrl Pts',(1.86513954299994,15.2,-10.49533973));
#159286=CARTESIAN_POINT('Ctrl Pts',(1.86513954299994,11.6,-10.49533973));
#159287=CARTESIAN_POINT('Ctrl Pts',(1.86608015299994,15.2,-10.497428179));
#159288=CARTESIAN_POINT('Ctrl Pts',(1.86608015299994,11.6,-10.497428179));
#159289=CARTESIAN_POINT('Ctrl Pts',(1.86702527199994,15.2,-10.499521733));
#159290=CARTESIAN_POINT('Ctrl Pts',(1.86702527199994,11.6,-10.499521733));
#159291=CARTESIAN_POINT('Ctrl Pts',(1.86797490499994,15.2,-10.501620377));
#159292=CARTESIAN_POINT('Ctrl Pts',(1.86797490499994,11.6,-10.501620377));
#159293=CARTESIAN_POINT('Ctrl Pts',(1.86892905699994,15.2,-10.503724094));
#159294=CARTESIAN_POINT('Ctrl Pts',(1.86892905699994,11.6,-10.503724094));
#159295=CARTESIAN_POINT('Ctrl Pts',(1.86988772999995,15.2,-10.505832868));
#159296=CARTESIAN_POINT('Ctrl Pts',(1.86988772999995,11.6,-10.505832868));
#159297=CARTESIAN_POINT('Ctrl Pts',(1.87085092699994,15.2,-10.507946683));
#159298=CARTESIAN_POINT('Ctrl Pts',(1.87085092699994,11.6,-10.507946683));
#159299=CARTESIAN_POINT('Ctrl Pts',(1.87181865399994,15.2,-10.510065522));
#159300=CARTESIAN_POINT('Ctrl Pts',(1.87181865399994,11.6,-10.510065522));
#159301=CARTESIAN_POINT('Ctrl Pts',(1.87279091299994,15.2,-10.512189371));
#159302=CARTESIAN_POINT('Ctrl Pts',(1.87279091299994,11.6,-10.512189371));
#159303=CARTESIAN_POINT('Ctrl Pts',(1.87376770899994,15.2,-10.514318212));
#159304=CARTESIAN_POINT('Ctrl Pts',(1.87376770899994,11.6,-10.514318212));
#159305=CARTESIAN_POINT('Ctrl Pts',(1.87474904299994,15.2,-10.516452031));
#159306=CARTESIAN_POINT('Ctrl Pts',(1.87474904299994,11.6,-10.516452031));
#159307=CARTESIAN_POINT('Ctrl Pts',(1.87573492299994,15.2,-10.518590811));
#159308=CARTESIAN_POINT('Ctrl Pts',(1.87573492299994,11.6,-10.518590811));
#159309=CARTESIAN_POINT('Ctrl Pts',(1.87672534799994,15.2,-10.520734536));
#159310=CARTESIAN_POINT('Ctrl Pts',(1.87672534799994,11.6,-10.520734536));
#159311=CARTESIAN_POINT('Ctrl Pts',(1.87772032499994,15.2,-10.522883192));
#159312=CARTESIAN_POINT('Ctrl Pts',(1.87772032499994,11.6,-10.522883192));
#159313=CARTESIAN_POINT('Ctrl Pts',(1.87871985699994,15.2,-10.525036762));
#159314=CARTESIAN_POINT('Ctrl Pts',(1.87871985699994,11.6,-10.525036762));
#159315=CARTESIAN_POINT('Ctrl Pts',(1.87972394599994,15.2,-10.52719523));
#159316=CARTESIAN_POINT('Ctrl Pts',(1.87972394599994,11.6,-10.52719523));
#159317=CARTESIAN_POINT('Ctrl Pts',(1.88073259699994,15.2,-10.529358581));
#159318=CARTESIAN_POINT('Ctrl Pts',(1.88073259699994,11.6,-10.529358581));
#159319=CARTESIAN_POINT('Ctrl Pts',(1.88174581199994,15.2,-10.531526798));
#159320=CARTESIAN_POINT('Ctrl Pts',(1.88174581199994,11.6,-10.531526798));
#159321=CARTESIAN_POINT('Ctrl Pts',(1.88276359599994,15.2,-10.533699869));
#159322=CARTESIAN_POINT('Ctrl Pts',(1.88276359599994,11.6,-10.533699869));
#159323=CARTESIAN_POINT('Ctrl Pts',(1.88378595299994,15.2,-10.535877775));
#159324=CARTESIAN_POINT('Ctrl Pts',(1.88378595299994,11.6,-10.535877775));
#159325=CARTESIAN_POINT('Ctrl Pts',(1.88481288399994,15.2,-10.538060503));
#159326=CARTESIAN_POINT('Ctrl Pts',(1.88481288399994,11.6,-10.538060503));
#159327=CARTESIAN_POINT('Ctrl Pts',(1.88584439399994,15.2,-10.540248035));
#159328=CARTESIAN_POINT('Ctrl Pts',(1.88584439399994,11.6,-10.540248035));
#159329=CARTESIAN_POINT('Ctrl Pts',(1.88688048599994,15.2,-10.542440358));
#159330=CARTESIAN_POINT('Ctrl Pts',(1.88688048599994,11.6,-10.542440358));
#159331=CARTESIAN_POINT('Ctrl Pts',(1.88792116399994,15.2,-10.544637455));
#159332=CARTESIAN_POINT('Ctrl Pts',(1.88792116399994,11.6,-10.544637455));
#159333=CARTESIAN_POINT('Ctrl Pts',(1.88896643099994,15.2,-10.546839313));
#159334=CARTESIAN_POINT('Ctrl Pts',(1.88896643099994,11.6,-10.546839313));
#159335=CARTESIAN_POINT('Ctrl Pts',(1.89001628999994,15.2,-10.549045913));
#159336=CARTESIAN_POINT('Ctrl Pts',(1.89001628999994,11.6,-10.549045913));
#159337=CARTESIAN_POINT('Ctrl Pts',(1.89107074499994,15.2,-10.551257244));
#159338=CARTESIAN_POINT('Ctrl Pts',(1.89107074499994,11.6,-10.551257244));
#159339=CARTESIAN_POINT('Ctrl Pts',(1.89212979899994,15.2,-10.553473288));
#159340=CARTESIAN_POINT('Ctrl Pts',(1.89212979899994,11.6,-10.553473288));
#159341=CARTESIAN_POINT('Ctrl Pts',(1.89319345499994,15.2,-10.555694032));
#159342=CARTESIAN_POINT('Ctrl Pts',(1.89319345499994,11.6,-10.555694032));
#159343=CARTESIAN_POINT('Ctrl Pts',(1.89426171599994,15.2,-10.557919458));
#159344=CARTESIAN_POINT('Ctrl Pts',(1.89426171599994,11.6,-10.557919458));
#159345=CARTESIAN_POINT('Ctrl Pts',(1.89533458699994,15.2,-10.560149554));
#159346=CARTESIAN_POINT('Ctrl Pts',(1.89533458699994,11.6,-10.560149554));
#159347=CARTESIAN_POINT('Ctrl Pts',(1.89641206899994,15.2,-10.562384303));
#159348=CARTESIAN_POINT('Ctrl Pts',(1.89641206899994,11.6,-10.562384303));
#159349=CARTESIAN_POINT('Ctrl Pts',(1.89749416599994,15.2,-10.564623691));
#159350=CARTESIAN_POINT('Ctrl Pts',(1.89749416599994,11.6,-10.564623691));
#159351=CARTESIAN_POINT('Ctrl Pts',(1.89858088099994,15.2,-10.566867703));
#159352=CARTESIAN_POINT('Ctrl Pts',(1.89858088099994,11.6,-10.566867703));
#159353=CARTESIAN_POINT('Ctrl Pts',(1.89967221899994,15.2,-10.569116324));
#159354=CARTESIAN_POINT('Ctrl Pts',(1.89967221899994,11.6,-10.569116324));
#159355=CARTESIAN_POINT('Ctrl Pts',(1.90076818099994,15.2,-10.571369539));
#159356=CARTESIAN_POINT('Ctrl Pts',(1.90076818099994,11.6,-10.571369539));
#159357=CARTESIAN_POINT('Ctrl Pts',(1.90186877099994,15.2,-10.573627333));
#159358=CARTESIAN_POINT('Ctrl Pts',(1.90186877099994,11.6,-10.573627333));
#159359=CARTESIAN_POINT('Ctrl Pts',(1.90297399099994,15.2,-10.575889692));
#159360=CARTESIAN_POINT('Ctrl Pts',(1.90297399099994,11.6,-10.575889692));
#159361=CARTESIAN_POINT('Ctrl Pts',(1.90408384599994,15.2,-10.578156601));
#159362=CARTESIAN_POINT('Ctrl Pts',(1.90408384599994,11.6,-10.578156601));
#159363=CARTESIAN_POINT('Ctrl Pts',(1.90519833799994,15.2,-10.580428044));
#159364=CARTESIAN_POINT('Ctrl Pts',(1.90519833799994,11.6,-10.580428044));
#159365=CARTESIAN_POINT('Ctrl Pts',(1.90631746999994,15.2,-10.582704009));
#159366=CARTESIAN_POINT('Ctrl Pts',(1.90631746999994,11.6,-10.582704009));
#159367=CARTESIAN_POINT('Ctrl Pts',(1.90744124499994,15.2,-10.584984479));
#159368=CARTESIAN_POINT('Ctrl Pts',(1.90744124499994,11.6,-10.584984479));
#159369=CARTESIAN_POINT('Ctrl Pts',(1.90856966599994,15.2,-10.587269441));
#159370=CARTESIAN_POINT('Ctrl Pts',(1.90856966599994,11.6,-10.587269441));
#159371=CARTESIAN_POINT('Ctrl Pts',(1.90970273699994,15.2,-10.58955888));
#159372=CARTESIAN_POINT('Ctrl Pts',(1.90970273699994,11.6,-10.58955888));
#159373=CARTESIAN_POINT('Ctrl Pts',(1.91084045999994,15.2,-10.59185278));
#159374=CARTESIAN_POINT('Ctrl Pts',(1.91084045999994,11.6,-10.59185278));
#159375=CARTESIAN_POINT('Ctrl Pts',(1.91198283799994,15.2,-10.594151129));
#159376=CARTESIAN_POINT('Ctrl Pts',(1.91198283799994,11.6,-10.594151129));
#159377=CARTESIAN_POINT('Ctrl Pts',(1.91312987399994,15.2,-10.59645391));
#159378=CARTESIAN_POINT('Ctrl Pts',(1.91312987399994,11.6,-10.59645391));
#159379=CARTESIAN_POINT('Ctrl Pts',(1.91428157099994,15.2,-10.598761112));
#159380=CARTESIAN_POINT('Ctrl Pts',(1.91428157099994,11.6,-10.598761112));
#159381=CARTESIAN_POINT('Ctrl Pts',(1.91543793199994,15.2,-10.601072717));
#159382=CARTESIAN_POINT('Ctrl Pts',(1.91543793199994,11.6,-10.601072717));
#159383=CARTESIAN_POINT('Ctrl Pts',(1.91659895999994,15.2,-10.603388714));
#159384=CARTESIAN_POINT('Ctrl Pts',(1.91659895999994,11.6,-10.603388714));
#159385=CARTESIAN_POINT('Ctrl Pts',(1.91776465699994,15.2,-10.605709085));
#159386=CARTESIAN_POINT('Ctrl Pts',(1.91776465699994,11.6,-10.605709085));
#159387=CARTESIAN_POINT('Ctrl Pts',(1.91893502699994,15.2,-10.60803382));
#159388=CARTESIAN_POINT('Ctrl Pts',(1.91893502699994,11.6,-10.60803382));
#159389=CARTESIAN_POINT('Ctrl Pts',(1.92011007299994,15.2,-10.610362901));
#159390=CARTESIAN_POINT('Ctrl Pts',(1.92011007299994,11.6,-10.610362901));
#159391=CARTESIAN_POINT('Ctrl Pts',(1.92128979599994,15.2,-10.612696316));
#159392=CARTESIAN_POINT('Ctrl Pts',(1.92128979599994,11.6,-10.612696316));
#159393=CARTESIAN_POINT('Ctrl Pts',(1.92247420099994,15.2,-10.615034051));
#159394=CARTESIAN_POINT('Ctrl Pts',(1.92247420099994,11.6,-10.615034051));
#159395=CARTESIAN_POINT('Ctrl Pts',(1.92366328999994,15.2,-10.617376091));
#159396=CARTESIAN_POINT('Ctrl Pts',(1.92366328999994,11.6,-10.617376091));
#159397=CARTESIAN_POINT('Ctrl Pts',(1.92485706499994,15.2,-10.619722422));
#159398=CARTESIAN_POINT('Ctrl Pts',(1.92485706499994,11.6,-10.619722422));
#159399=CARTESIAN_POINT('Ctrl Pts',(1.92605552899994,15.2,-10.622073029));
#159400=CARTESIAN_POINT('Ctrl Pts',(1.92605552899994,11.6,-10.622073029));
#159401=CARTESIAN_POINT('Ctrl Pts',(1.92725868499994,15.2,-10.6244279));
#159402=CARTESIAN_POINT('Ctrl Pts',(1.92725868499994,11.6,-10.6244279));
#159403=CARTESIAN_POINT('Ctrl Pts',(1.92846653599994,15.2,-10.62678702));
#159404=CARTESIAN_POINT('Ctrl Pts',(1.92846653599994,11.6,-10.62678702));
#159405=CARTESIAN_POINT('Ctrl Pts',(1.92967908399994,15.2,-10.629150376));
#159406=CARTESIAN_POINT('Ctrl Pts',(1.92967908399994,11.6,-10.629150376));
#159407=CARTESIAN_POINT('Ctrl Pts',(1.93089633299994,15.2,-10.631517953));
#159408=CARTESIAN_POINT('Ctrl Pts',(1.93089633299994,11.6,-10.631517953));
#159409=CARTESIAN_POINT('Ctrl Pts',(1.93211828499994,15.2,-10.633889738));
#159410=CARTESIAN_POINT('Ctrl Pts',(1.93211828499994,11.6,-10.633889738));
#159411=CARTESIAN_POINT('Ctrl Pts',(1.93334494199994,15.2,-10.636265715));
#159412=CARTESIAN_POINT('Ctrl Pts',(1.93334494199994,11.6,-10.636265715));
#159413=CARTESIAN_POINT('Ctrl Pts',(1.93457630699994,15.2,-10.638645874));
#159414=CARTESIAN_POINT('Ctrl Pts',(1.93457630699994,11.6,-10.638645874));
#159415=CARTESIAN_POINT('Ctrl Pts',(1.93581238299994,15.2,-10.641030197));
#159416=CARTESIAN_POINT('Ctrl Pts',(1.93581238299994,11.6,-10.641030197));
#159417=CARTESIAN_POINT('Ctrl Pts',(1.93705317299994,15.2,-10.643418674));
#159418=CARTESIAN_POINT('Ctrl Pts',(1.93705317299994,11.6,-10.643418674));
#159419=CARTESIAN_POINT('Ctrl Pts',(1.93829867699994,15.2,-10.645811289));
#159420=CARTESIAN_POINT('Ctrl Pts',(1.93829867699994,11.6,-10.645811289));
#159421=CARTESIAN_POINT('Ctrl Pts',(1.93954889999994,15.2,-10.648208029));
#159422=CARTESIAN_POINT('Ctrl Pts',(1.93954889999994,11.6,-10.648208029));
#159423=CARTESIAN_POINT('Ctrl Pts',(1.94080384499994,15.2,-10.650608881));
#159424=CARTESIAN_POINT('Ctrl Pts',(1.94080384499994,11.6,-10.650608881));
#159425=CARTESIAN_POINT('Ctrl Pts',(1.94206351299994,15.2,-10.65301383));
#159426=CARTESIAN_POINT('Ctrl Pts',(1.94206351299994,11.6,-10.65301383));
#159427=CARTESIAN_POINT('Ctrl Pts',(1.94332790699994,15.2,-10.655422864));
#159428=CARTESIAN_POINT('Ctrl Pts',(1.94332790699994,11.6,-10.655422864));
#159429=CARTESIAN_POINT('Ctrl Pts',(1.94459702899994,15.2,-10.657835968));
#159430=CARTESIAN_POINT('Ctrl Pts',(1.94459702899994,11.6,-10.657835968));
#159431=CARTESIAN_POINT('Ctrl Pts',(1.94587088199994,15.2,-10.660253129));
#159432=CARTESIAN_POINT('Ctrl Pts',(1.94587088199994,11.6,-10.660253129));
#159433=CARTESIAN_POINT('Ctrl Pts',(1.94714946899994,15.2,-10.662674334));
#159434=CARTESIAN_POINT('Ctrl Pts',(1.94714946899994,11.6,-10.662674334));
#159435=CARTESIAN_POINT('Ctrl Pts',(1.94843279199994,15.2,-10.665099571));
#159436=CARTESIAN_POINT('Ctrl Pts',(1.94843279199994,11.6,-10.665099571));
#159437=CARTESIAN_POINT('Ctrl Pts',(1.94972085299994,15.2,-10.667528823));
#159438=CARTESIAN_POINT('Ctrl Pts',(1.94972085299994,11.6,-10.667528823));
#159439=CARTESIAN_POINT('Ctrl Pts',(1.95101365499994,15.2,-10.66996208));
#159440=CARTESIAN_POINT('Ctrl Pts',(1.95101365499994,11.6,-10.66996208));
#159441=CARTESIAN_POINT('Ctrl Pts',(1.95231119999994,15.2,-10.672399326));
#159442=CARTESIAN_POINT('Ctrl Pts',(1.95231119999994,11.6,-10.672399326));
#159443=CARTESIAN_POINT('Ctrl Pts',(1.95361349099994,15.2,-10.674840549));
#159444=CARTESIAN_POINT('Ctrl Pts',(1.95361349099994,11.6,-10.674840549));
#159445=CARTESIAN_POINT('Ctrl Pts',(1.95492052999994,15.2,-10.677285737));
#159446=CARTESIAN_POINT('Ctrl Pts',(1.95492052999994,11.6,-10.677285737));
#159447=CARTESIAN_POINT('Ctrl Pts',(1.95623231799994,15.2,-10.679734874));
#159448=CARTESIAN_POINT('Ctrl Pts',(1.95623231799994,11.6,-10.679734874));
#159449=CARTESIAN_POINT('Ctrl Pts',(1.95754885999994,15.2,-10.682187948));
#159450=CARTESIAN_POINT('Ctrl Pts',(1.95754885999994,11.6,-10.682187948));
#159451=CARTESIAN_POINT('Ctrl Pts',(1.95887015699994,15.2,-10.684644947));
#159452=CARTESIAN_POINT('Ctrl Pts',(1.95887015699994,11.6,-10.684644947));
#159453=CARTESIAN_POINT('Ctrl Pts',(1.96019620999994,15.2,-10.687105856));
#159454=CARTESIAN_POINT('Ctrl Pts',(1.96019620999994,11.6,-10.687105856));
#159455=CARTESIAN_POINT('Ctrl Pts',(1.96152702299994,15.2,-10.689570664));
#159456=CARTESIAN_POINT('Ctrl Pts',(1.96152702299994,11.6,-10.689570664));
#159457=CARTESIAN_POINT('Ctrl Pts',(1.96286259899994,15.2,-10.692039356));
#159458=CARTESIAN_POINT('Ctrl Pts',(1.96286259899994,11.6,-10.692039356));
#159459=CARTESIAN_POINT('Ctrl Pts',(1.96420293799994,15.2,-10.694511919));
#159460=CARTESIAN_POINT('Ctrl Pts',(1.96420293799994,11.6,-10.694511919));
#159461=CARTESIAN_POINT('Ctrl Pts',(1.96554804399994,15.2,-10.696988341));
#159462=CARTESIAN_POINT('Ctrl Pts',(1.96554804399994,11.6,-10.696988341));
#159463=CARTESIAN_POINT('Ctrl Pts',(1.96689791799994,15.2,-10.699468609));
#159464=CARTESIAN_POINT('Ctrl Pts',(1.96689791799994,11.6,-10.699468609));
#159465=CARTESIAN_POINT('Ctrl Pts',(1.96825256199994,15.2,-10.70195271));
#159466=CARTESIAN_POINT('Ctrl Pts',(1.96825256199994,11.6,-10.70195271));
#159467=CARTESIAN_POINT('Ctrl Pts',(1.96961197999994,15.2,-10.704440629));
#159468=CARTESIAN_POINT('Ctrl Pts',(1.96961197999994,11.6,-10.704440629));
#159469=CARTESIAN_POINT('Ctrl Pts',(1.97097617299994,15.2,-10.706932355));
#159470=CARTESIAN_POINT('Ctrl Pts',(1.97097617299994,11.6,-10.706932355));
#159471=CARTESIAN_POINT('Ctrl Pts',(1.97234514399994,15.2,-10.709427876));
#159472=CARTESIAN_POINT('Ctrl Pts',(1.97234514399994,11.6,-10.709427876));
#159473=CARTESIAN_POINT('Ctrl Pts',(1.97371889299994,15.2,-10.711927177));
#159474=CARTESIAN_POINT('Ctrl Pts',(1.97371889299994,11.6,-10.711927177));
#159475=CARTESIAN_POINT('Ctrl Pts',(1.97509742499994,15.2,-10.714430247));
#159476=CARTESIAN_POINT('Ctrl Pts',(1.97509742499994,11.6,-10.714430247));
#159477=CARTESIAN_POINT('Ctrl Pts',(1.97648073999994,15.2,-10.716937073));
#159478=CARTESIAN_POINT('Ctrl Pts',(1.97648073999994,11.6,-10.716937073));
#159479=CARTESIAN_POINT('Ctrl Pts',(1.97786884099994,15.2,-10.71944764));
#159480=CARTESIAN_POINT('Ctrl Pts',(1.97786884099994,11.6,-10.71944764));
#159481=CARTESIAN_POINT('Ctrl Pts',(1.97926172999994,15.2,-10.721961937));
#159482=CARTESIAN_POINT('Ctrl Pts',(1.97926172999994,11.6,-10.721961937));
#159483=CARTESIAN_POINT('Ctrl Pts',(1.98065940899994,15.2,-10.724479952));
#159484=CARTESIAN_POINT('Ctrl Pts',(1.98065940899994,11.6,-10.724479952));
#159485=CARTESIAN_POINT('Ctrl Pts',(1.98206188099994,15.2,-10.727001672));
#159486=CARTESIAN_POINT('Ctrl Pts',(1.98206188099994,11.6,-10.727001672));
#159487=CARTESIAN_POINT('Ctrl Pts',(1.98346914499994,15.2,-10.729527083));
#159488=CARTESIAN_POINT('Ctrl Pts',(1.98346914499994,11.6,-10.729527083));
#159489=CARTESIAN_POINT('Ctrl Pts',(1.98488120699994,15.2,-10.732056173));
#159490=CARTESIAN_POINT('Ctrl Pts',(1.98488120699994,11.6,-10.732056173));
#159491=CARTESIAN_POINT('Ctrl Pts',(1.98629806699994,15.2,-10.73458893));
#159492=CARTESIAN_POINT('Ctrl Pts',(1.98629806699994,11.6,-10.73458893));
#159493=CARTESIAN_POINT('Ctrl Pts',(1.98771972699994,15.2,-10.737125341));
#159494=CARTESIAN_POINT('Ctrl Pts',(1.98771972699994,11.6,-10.737125341));
#159495=CARTESIAN_POINT('Ctrl Pts',(1.98914618999994,15.2,-10.739665394));
#159496=CARTESIAN_POINT('Ctrl Pts',(1.98914618999994,11.6,-10.739665394));
#159497=CARTESIAN_POINT('Ctrl Pts',(1.99057745699994,15.2,-10.742209076));
#159498=CARTESIAN_POINT('Ctrl Pts',(1.99057745699994,11.6,-10.742209076));
#159499=CARTESIAN_POINT('Ctrl Pts',(1.99201352899994,15.2,-10.744756374));
#159500=CARTESIAN_POINT('Ctrl Pts',(1.99201352899994,11.6,-10.744756374));
#159501=CARTESIAN_POINT('Ctrl Pts',(1.99345441099994,15.2,-10.747307276));
#159502=CARTESIAN_POINT('Ctrl Pts',(1.99345441099994,11.6,-10.747307276));
#159503=CARTESIAN_POINT('Ctrl Pts',(1.99490010199994,15.2,-10.74986177));
#159504=CARTESIAN_POINT('Ctrl Pts',(1.99490010199994,11.6,-10.74986177));
#159505=CARTESIAN_POINT('Ctrl Pts',(1.99635060499994,15.2,-10.752419844));
#159506=CARTESIAN_POINT('Ctrl Pts',(1.99635060499994,11.6,-10.752419844));
#159507=CARTESIAN_POINT('Ctrl Pts',(1.99780592199994,15.2,-10.754981484));
#159508=CARTESIAN_POINT('Ctrl Pts',(1.99780592199994,11.6,-10.754981484));
#159509=CARTESIAN_POINT('Ctrl Pts',(1.99926605499994,15.2,-10.757546678));
#159510=CARTESIAN_POINT('Ctrl Pts',(1.99926605499994,11.6,-10.757546678));
#159511=CARTESIAN_POINT('Ctrl Pts',(2.00073100599994,15.2,-10.760115415));
#159512=CARTESIAN_POINT('Ctrl Pts',(2.00073100599994,11.6,-10.760115415));
#159513=CARTESIAN_POINT('Ctrl Pts',(2.00220077599994,15.2,-10.762687682));
#159514=CARTESIAN_POINT('Ctrl Pts',(2.00220077599994,11.6,-10.762687682));
#159515=CARTESIAN_POINT('Ctrl Pts',(2.00367536799994,15.2,-10.765263466));
#159516=CARTESIAN_POINT('Ctrl Pts',(2.00367536799994,11.6,-10.765263466));
#159517=CARTESIAN_POINT('Ctrl Pts',(2.00515478199994,15.2,-10.767842756));
#159518=CARTESIAN_POINT('Ctrl Pts',(2.00515478199994,11.6,-10.767842756));
#159519=CARTESIAN_POINT('Ctrl Pts',(2.00663902299994,15.2,-10.77042554));
#159520=CARTESIAN_POINT('Ctrl Pts',(2.00663902299994,11.6,-10.77042554));
#159521=CARTESIAN_POINT('Ctrl Pts',(2.00812808999994,15.2,-10.773011803));
#159522=CARTESIAN_POINT('Ctrl Pts',(2.00812808999994,11.6,-10.773011803));
#159523=CARTESIAN_POINT('Ctrl Pts',(2.00962198599994,15.2,-10.775601537));
#159524=CARTESIAN_POINT('Ctrl Pts',(2.00962198599994,11.6,-10.775601537));
#159525=CARTESIAN_POINT('Ctrl Pts',(2.01112071299994,15.2,-10.778194727));
#159526=CARTESIAN_POINT('Ctrl Pts',(2.01112071299994,11.6,-10.778194727));
#159527=CARTESIAN_POINT('Ctrl Pts',(2.01262427099994,15.2,-10.780791361));
#159528=CARTESIAN_POINT('Ctrl Pts',(2.01262427099994,11.6,-10.780791361));
#159529=CARTESIAN_POINT('Ctrl Pts',(2.01413266399994,15.2,-10.783391428));
#159530=CARTESIAN_POINT('Ctrl Pts',(2.01413266399994,11.6,-10.783391428));
#159531=CARTESIAN_POINT('Ctrl Pts',(2.01564589299994,15.2,-10.785994916));
#159532=CARTESIAN_POINT('Ctrl Pts',(2.01564589299994,11.6,-10.785994916));
#159533=CARTESIAN_POINT('Ctrl Pts',(2.01716395899994,15.2,-10.788601812));
#159534=CARTESIAN_POINT('Ctrl Pts',(2.01716395899994,11.6,-10.788601812));
#159535=CARTESIAN_POINT('Ctrl Pts',(2.01868686499994,15.2,-10.791212104));
#159536=CARTESIAN_POINT('Ctrl Pts',(2.01868686499994,11.6,-10.791212104));
#159537=CARTESIAN_POINT('Ctrl Pts',(2.02021461099994,15.2,-10.793825781));
#159538=CARTESIAN_POINT('Ctrl Pts',(2.02021461099994,11.6,-10.793825781));
#159539=CARTESIAN_POINT('Ctrl Pts',(2.02174720099995,15.2,-10.796442831));
#159540=CARTESIAN_POINT('Ctrl Pts',(2.02174720099995,11.6,-10.796442831));
#159541=CARTESIAN_POINT('Ctrl Pts',(2.02328463399994,15.2,-10.799063241));
#159542=CARTESIAN_POINT('Ctrl Pts',(2.02328463399994,11.6,-10.799063241));
#159543=CARTESIAN_POINT('Ctrl Pts',(2.02482691399994,15.2,-10.801687));
#159544=CARTESIAN_POINT('Ctrl Pts',(2.02482691399994,11.6,-10.801687));
#159545=CARTESIAN_POINT('Ctrl Pts',(2.02637404199994,15.2,-10.804314097));
#159546=CARTESIAN_POINT('Ctrl Pts',(2.02637404199994,11.6,-10.804314097));
#159547=CARTESIAN_POINT('Ctrl Pts',(2.02792601899994,15.2,-10.806944517));
#159548=CARTESIAN_POINT('Ctrl Pts',(2.02792601899994,11.6,-10.806944517));
#159549=CARTESIAN_POINT('Ctrl Pts',(2.02948284599994,15.2,-10.809578251));
#159550=CARTESIAN_POINT('Ctrl Pts',(2.02948284599994,11.6,-10.809578251));
#159551=CARTESIAN_POINT('Ctrl Pts',(2.03104452699994,15.2,-10.812215287));
#159552=CARTESIAN_POINT('Ctrl Pts',(2.03104452699994,11.6,-10.812215287));
#159553=CARTESIAN_POINT('Ctrl Pts',(2.03261106199994,15.2,-10.814855611));
#159554=CARTESIAN_POINT('Ctrl Pts',(2.03261106199994,11.6,-10.814855611));
#159555=CARTESIAN_POINT('Ctrl Pts',(2.03418245199994,15.2,-10.817499214));
#159556=CARTESIAN_POINT('Ctrl Pts',(2.03418245199994,11.6,-10.817499214));
#159557=CARTESIAN_POINT('Ctrl Pts',(2.03575870099994,15.2,-10.820146083));
#159558=CARTESIAN_POINT('Ctrl Pts',(2.03575870099994,11.6,-10.820146083));
#159559=CARTESIAN_POINT('Ctrl Pts',(2.03733980799994,15.2,-10.822796206));
#159560=CARTESIAN_POINT('Ctrl Pts',(2.03733980799994,11.6,-10.822796206));
#159561=CARTESIAN_POINT('Ctrl Pts',(2.03892577499994,15.2,-10.825449572));
#159562=CARTESIAN_POINT('Ctrl Pts',(2.03892577499994,11.6,-10.825449572));
#159563=CARTESIAN_POINT('Ctrl Pts',(2.04051660599994,15.2,-10.82810617));
#159564=CARTESIAN_POINT('Ctrl Pts',(2.04051660599994,11.6,-10.82810617));
#159565=CARTESIAN_POINT('Ctrl Pts',(2.04211229899994,15.2,-10.830765986));
#159566=CARTESIAN_POINT('Ctrl Pts',(2.04211229899994,11.6,-10.830765986));
#159567=CARTESIAN_POINT('Ctrl Pts',(2.04371285699994,15.2,-10.833429011));
#159568=CARTESIAN_POINT('Ctrl Pts',(2.04371285699994,11.6,-10.833429011));
#159569=CARTESIAN_POINT('Ctrl Pts',(2.04531828199995,15.2,-10.836095232));
#159570=CARTESIAN_POINT('Ctrl Pts',(2.04531828199995,11.6,-10.836095232));
#159571=CARTESIAN_POINT('Ctrl Pts',(2.04692857599994,15.2,-10.838764637));
#159572=CARTESIAN_POINT('Ctrl Pts',(2.04692857599994,11.6,-10.838764637));
#159573=CARTESIAN_POINT('Ctrl Pts',(2.04854373899995,15.2,-10.841437216));
#159574=CARTESIAN_POINT('Ctrl Pts',(2.04854373899995,11.6,-10.841437216));
#159575=CARTESIAN_POINT('Ctrl Pts',(2.05016377299994,15.2,-10.844112955));
#159576=CARTESIAN_POINT('Ctrl Pts',(2.05016377299994,11.6,-10.844112955));
#159577=CARTESIAN_POINT('Ctrl Pts',(2.05178868099994,15.2,-10.846791846));
#159578=CARTESIAN_POINT('Ctrl Pts',(2.05178868099994,11.6,-10.846791846));
#159579=CARTESIAN_POINT('Ctrl Pts',(2.05341846199994,15.2,-10.849473875));
#159580=CARTESIAN_POINT('Ctrl Pts',(2.05341846199994,11.6,-10.849473875));
#159581=CARTESIAN_POINT('Ctrl Pts',(2.05505311799994,15.2,-10.852159032));
#159582=CARTESIAN_POINT('Ctrl Pts',(2.05505311799994,11.6,-10.852159032));
#159583=CARTESIAN_POINT('Ctrl Pts',(2.05669265099994,15.2,-10.854847303));
#159584=CARTESIAN_POINT('Ctrl Pts',(2.05669265099994,11.6,-10.854847303));
#159585=CARTESIAN_POINT('Ctrl Pts',(2.05833706199994,15.2,-10.85753868));
#159586=CARTESIAN_POINT('Ctrl Pts',(2.05833706199994,11.6,-10.85753868));
#159587=CARTESIAN_POINT('Ctrl Pts',(2.05998635399994,15.2,-10.86023315));
#159588=CARTESIAN_POINT('Ctrl Pts',(2.05998635399994,11.6,-10.86023315));
#159589=CARTESIAN_POINT('Ctrl Pts',(2.06164052499994,15.2,-10.862930702));
#159590=CARTESIAN_POINT('Ctrl Pts',(2.06164052499994,11.6,-10.862930702));
#159591=CARTESIAN_POINT('Ctrl Pts',(2.06329958099994,15.2,-10.865631323));
#159592=CARTESIAN_POINT('Ctrl Pts',(2.06329958099994,11.6,-10.865631323));
#159593=CARTESIAN_POINT('Ctrl Pts',(2.06496351899994,15.2,-10.868335004));
#159594=CARTESIAN_POINT('Ctrl Pts',(2.06496351899994,11.6,-10.868335004));
#159595=CARTESIAN_POINT('Ctrl Pts',(2.06663234299994,15.2,-10.871041734));
#159596=CARTESIAN_POINT('Ctrl Pts',(2.06663234299994,11.6,-10.871041734));
#159597=CARTESIAN_POINT('Ctrl Pts',(2.06830605399994,15.2,-10.873751499));
#159598=CARTESIAN_POINT('Ctrl Pts',(2.06830605399994,11.6,-10.873751499));
#159599=CARTESIAN_POINT('Ctrl Pts',(2.06998465199994,15.2,-10.876464289));
#159600=CARTESIAN_POINT('Ctrl Pts',(2.06998465199994,11.6,-10.876464289));
#159601=CARTESIAN_POINT('Ctrl Pts',(2.07166813899994,15.2,-10.879180094));
#159602=CARTESIAN_POINT('Ctrl Pts',(2.07166813899994,11.6,-10.879180094));
#159603=CARTESIAN_POINT('Ctrl Pts',(2.07335651799994,15.2,-10.881898902));
#159604=CARTESIAN_POINT('Ctrl Pts',(2.07335651799994,11.6,-10.881898902));
#159605=CARTESIAN_POINT('Ctrl Pts',(2.07504978799994,15.2,-10.884620701));
#159606=CARTESIAN_POINT('Ctrl Pts',(2.07504978799994,11.6,-10.884620701));
#159607=CARTESIAN_POINT('Ctrl Pts',(2.07674794999994,15.2,-10.887345482));
#159608=CARTESIAN_POINT('Ctrl Pts',(2.07674794999994,11.6,-10.887345482));
#159609=CARTESIAN_POINT('Ctrl Pts',(2.07845100699994,15.2,-10.890073231));
#159610=CARTESIAN_POINT('Ctrl Pts',(2.07845100699994,11.6,-10.890073231));
#159611=CARTESIAN_POINT('Ctrl Pts',(2.08015896099994,15.2,-10.89280394));
#159612=CARTESIAN_POINT('Ctrl Pts',(2.08015896099994,11.6,-10.89280394));
#159613=CARTESIAN_POINT('Ctrl Pts',(2.08187181099994,15.2,-10.895537595));
#159614=CARTESIAN_POINT('Ctrl Pts',(2.08187181099994,11.6,-10.895537595));
#159615=CARTESIAN_POINT('Ctrl Pts',(2.08358955799994,15.2,-10.898274186));
#159616=CARTESIAN_POINT('Ctrl Pts',(2.08358955799994,11.6,-10.898274186));
#159617=CARTESIAN_POINT('Ctrl Pts',(2.08531220499994,15.2,-10.901013703));
#159618=CARTESIAN_POINT('Ctrl Pts',(2.08531220499994,11.6,-10.901013703));
#159619=CARTESIAN_POINT('Ctrl Pts',(2.08703975299994,15.2,-10.903756135));
#159620=CARTESIAN_POINT('Ctrl Pts',(2.08703975299994,11.6,-10.903756135));
#159621=CARTESIAN_POINT('Ctrl Pts',(2.08877220299994,15.2,-10.906501469));
#159622=CARTESIAN_POINT('Ctrl Pts',(2.08877220299994,11.6,-10.906501469));
#159623=CARTESIAN_POINT('Ctrl Pts',(2.09050955499994,15.2,-10.909249695));
#159624=CARTESIAN_POINT('Ctrl Pts',(2.09050955499994,11.6,-10.909249695));
#159625=CARTESIAN_POINT('Ctrl Pts',(2.09225181099994,15.2,-10.912000804));
#159626=CARTESIAN_POINT('Ctrl Pts',(2.09225181099994,11.6,-10.912000804));
#159627=CARTESIAN_POINT('Ctrl Pts',(2.09399897299994,15.2,-10.914754782));
#159628=CARTESIAN_POINT('Ctrl Pts',(2.09399897299994,11.6,-10.914754782));
#159629=CARTESIAN_POINT('Ctrl Pts',(2.09575104199994,15.2,-10.91751162));
#159630=CARTESIAN_POINT('Ctrl Pts',(2.09575104199994,11.6,-10.91751162));
#159631=CARTESIAN_POINT('Ctrl Pts',(2.09750801799994,15.2,-10.920271306));
#159632=CARTESIAN_POINT('Ctrl Pts',(2.09750801799994,11.6,-10.920271306));
#159633=CARTESIAN_POINT('Ctrl Pts',(2.09926990199994,15.2,-10.92303383));
#159634=CARTESIAN_POINT('Ctrl Pts',(2.09926990199994,11.6,-10.92303383));
#159635=CARTESIAN_POINT('Ctrl Pts',(2.10103669699994,15.2,-10.925799182));
#159636=CARTESIAN_POINT('Ctrl Pts',(2.10103669699994,11.6,-10.925799182));
#159637=CARTESIAN_POINT('Ctrl Pts',(2.10280840299994,15.2,-10.928567349));
#159638=CARTESIAN_POINT('Ctrl Pts',(2.10280840299994,11.6,-10.928567349));
#159639=CARTESIAN_POINT('Ctrl Pts',(2.10458501999994,15.2,-10.931338321));
#159640=CARTESIAN_POINT('Ctrl Pts',(2.10458501999994,11.6,-10.931338321));
#159641=CARTESIAN_POINT('Ctrl Pts',(2.10636655199994,15.2,-10.934112088));
#159642=CARTESIAN_POINT('Ctrl Pts',(2.10636655199994,11.6,-10.934112088));
#159643=CARTESIAN_POINT('Ctrl Pts',(2.10815299699994,15.2,-10.936888638));
#159644=CARTESIAN_POINT('Ctrl Pts',(2.10815299699994,11.6,-10.936888638));
#159645=CARTESIAN_POINT('Ctrl Pts',(2.10994435799994,15.2,-10.939667962));
#159646=CARTESIAN_POINT('Ctrl Pts',(2.10994435799994,11.6,-10.939667962));
#159647=CARTESIAN_POINT('Ctrl Pts',(2.11174063499994,15.2,-10.942450048));
#159648=CARTESIAN_POINT('Ctrl Pts',(2.11174063499994,11.6,-10.942450048));
#159649=CARTESIAN_POINT('Ctrl Pts',(2.11354182899994,15.2,-10.945234885));
#159650=CARTESIAN_POINT('Ctrl Pts',(2.11354182899994,11.6,-10.945234885));
#159651=CARTESIAN_POINT('Ctrl Pts',(2.11534794299994,15.2,-10.948022463));
#159652=CARTESIAN_POINT('Ctrl Pts',(2.11534794299994,11.6,-10.948022463));
#159653=CARTESIAN_POINT('Ctrl Pts',(2.11715897499994,15.2,-10.950812772));
#159654=CARTESIAN_POINT('Ctrl Pts',(2.11715897499994,11.6,-10.950812772));
#159655=CARTESIAN_POINT('Ctrl Pts',(2.11897492799995,15.2,-10.953605801));
#159656=CARTESIAN_POINT('Ctrl Pts',(2.11897492799995,11.6,-10.953605801));
#159657=CARTESIAN_POINT('Ctrl Pts',(2.12079580299994,15.2,-10.956401537));
#159658=CARTESIAN_POINT('Ctrl Pts',(2.12079580299994,11.6,-10.956401537));
#159659=CARTESIAN_POINT('Ctrl Pts',(2.12262159999994,15.2,-10.959199973));
#159660=CARTESIAN_POINT('Ctrl Pts',(2.12262159999994,11.6,-10.959199973));
#159661=CARTESIAN_POINT('Ctrl Pts',(2.12445232199994,15.2,-10.962001096));
#159662=CARTESIAN_POINT('Ctrl Pts',(2.12445232199994,11.6,-10.962001096));
#159663=CARTESIAN_POINT('Ctrl Pts',(2.12628796699994,15.2,-10.964804897));
#159664=CARTESIAN_POINT('Ctrl Pts',(2.12628796699994,11.6,-10.964804897));
#159665=CARTESIAN_POINT('Ctrl Pts',(2.12812853899994,15.2,-10.967611364));
#159666=CARTESIAN_POINT('Ctrl Pts',(2.12812853899994,11.6,-10.967611364));
#159667=CARTESIAN_POINT('Ctrl Pts',(2.12997403599994,15.2,-10.970420488));
#159668=CARTESIAN_POINT('Ctrl Pts',(2.12997403599994,11.6,-10.970420488));
#159669=CARTESIAN_POINT('Ctrl Pts',(2.13182446099994,15.2,-10.973232257));
#159670=CARTESIAN_POINT('Ctrl Pts',(2.13182446099994,11.6,-10.973232257));
#159671=CARTESIAN_POINT('Ctrl Pts',(2.13367981499994,15.2,-10.976046662));
#159672=CARTESIAN_POINT('Ctrl Pts',(2.13367981499994,11.6,-10.976046662));
#159673=CARTESIAN_POINT('Ctrl Pts',(2.13554009799994,15.2,-10.978863691));
#159674=CARTESIAN_POINT('Ctrl Pts',(2.13554009799994,11.6,-10.978863691));
#159675=CARTESIAN_POINT('Ctrl Pts',(2.13740531099994,15.2,-10.981683335));
#159676=CARTESIAN_POINT('Ctrl Pts',(2.13740531099994,11.6,-10.981683335));
#159677=CARTESIAN_POINT('Ctrl Pts',(2.13927545499994,15.2,-10.984505583));
#159678=CARTESIAN_POINT('Ctrl Pts',(2.13927545499994,11.6,-10.984505583));
#159679=CARTESIAN_POINT('Ctrl Pts',(2.14115053099994,15.2,-10.987330423));
#159680=CARTESIAN_POINT('Ctrl Pts',(2.14115053099994,11.6,-10.987330423));
#159681=CARTESIAN_POINT('Ctrl Pts',(2.14303053999994,15.2,-10.990157848));
#159682=CARTESIAN_POINT('Ctrl Pts',(2.14303053999994,11.6,-10.990157848));
#159683=CARTESIAN_POINT('Ctrl Pts',(2.14491548299994,15.2,-10.992987845));
#159684=CARTESIAN_POINT('Ctrl Pts',(2.14491548299994,11.6,-10.992987845));
#159685=CARTESIAN_POINT('Ctrl Pts',(2.14680536099995,15.2,-10.995820404));
#159686=CARTESIAN_POINT('Ctrl Pts',(2.14680536099995,11.6,-10.995820404));
#159687=CARTESIAN_POINT('Ctrl Pts',(2.14870017399994,15.2,-10.998655516));
#159688=CARTESIAN_POINT('Ctrl Pts',(2.14870017399994,11.6,-10.998655516));
#159689=CARTESIAN_POINT('Ctrl Pts',(2.15059992399994,15.2,-11.00149317));
#159690=CARTESIAN_POINT('Ctrl Pts',(2.15059992399994,11.6,-11.00149317));
#159691=CARTESIAN_POINT('Ctrl Pts',(2.15250460999994,15.2,-11.004333355));
#159692=CARTESIAN_POINT('Ctrl Pts',(2.15250460999994,11.6,-11.004333355));
#159693=CARTESIAN_POINT('Ctrl Pts',(2.15441423499994,15.2,-11.007176061));
#159694=CARTESIAN_POINT('Ctrl Pts',(2.15441423499994,11.6,-11.007176061));
#159695=CARTESIAN_POINT('Ctrl Pts',(2.15632879899994,15.2,-11.010021278));
#159696=CARTESIAN_POINT('Ctrl Pts',(2.15632879899994,11.6,-11.010021278));
#159697=CARTESIAN_POINT('Ctrl Pts',(2.15824830199994,15.2,-11.012868997));
#159698=CARTESIAN_POINT('Ctrl Pts',(2.15824830199994,11.6,-11.012868997));
#159699=CARTESIAN_POINT('Ctrl Pts',(2.16017274599994,15.2,-11.015719205));
#159700=CARTESIAN_POINT('Ctrl Pts',(2.16017274599994,11.6,-11.015719205));
#159701=CARTESIAN_POINT('Ctrl Pts',(2.16210213199994,15.2,-11.018571894));
#159702=CARTESIAN_POINT('Ctrl Pts',(2.16210213199994,11.6,-11.018571894));
#159703=CARTESIAN_POINT('Ctrl Pts',(2.16403645899994,15.2,-11.021427054));
#159704=CARTESIAN_POINT('Ctrl Pts',(2.16403645899994,11.6,-11.021427054));
#159705=CARTESIAN_POINT('Ctrl Pts',(2.16597572899994,15.2,-11.024284674));
#159706=CARTESIAN_POINT('Ctrl Pts',(2.16597572899994,11.6,-11.024284674));
#159707=CARTESIAN_POINT('Ctrl Pts',(2.16791994199994,15.2,-11.027144743));
#159708=CARTESIAN_POINT('Ctrl Pts',(2.16791994199994,11.6,-11.027144743));
#159709=CARTESIAN_POINT('Ctrl Pts',(2.16986909999994,15.2,-11.030007252));
#159710=CARTESIAN_POINT('Ctrl Pts',(2.16986909999994,11.6,-11.030007252));
#159711=CARTESIAN_POINT('Ctrl Pts',(2.17182320399994,15.2,-11.032872191));
#159712=CARTESIAN_POINT('Ctrl Pts',(2.17182320399994,11.6,-11.032872191));
#159713=CARTESIAN_POINT('Ctrl Pts',(2.17378225199994,15.2,-11.03573955));
#159714=CARTESIAN_POINT('Ctrl Pts',(2.17378225199994,11.6,-11.03573955));
#159715=CARTESIAN_POINT('Ctrl Pts',(2.17574624699994,15.2,-11.038609318));
#159716=CARTESIAN_POINT('Ctrl Pts',(2.17574624699994,11.6,-11.038609318));
#159717=CARTESIAN_POINT('Ctrl Pts',(2.17771518999994,15.2,-11.041481486));
#159718=CARTESIAN_POINT('Ctrl Pts',(2.17771518999994,11.6,-11.041481486));
#159719=CARTESIAN_POINT('Ctrl Pts',(2.17968908099994,15.2,-11.044356044));
#159720=CARTESIAN_POINT('Ctrl Pts',(2.17968908099994,11.6,-11.044356044));
#159721=CARTESIAN_POINT('Ctrl Pts',(2.18166791999994,15.2,-11.047232981));
#159722=CARTESIAN_POINT('Ctrl Pts',(2.18166791999994,11.6,-11.047232981));
#159723=CARTESIAN_POINT('Ctrl Pts',(2.18365170899994,15.2,-11.050112287));
#159724=CARTESIAN_POINT('Ctrl Pts',(2.18365170899994,11.6,-11.050112287));
#159725=CARTESIAN_POINT('Ctrl Pts',(2.18564044699994,15.2,-11.052993953));
#159726=CARTESIAN_POINT('Ctrl Pts',(2.18564044699994,11.6,-11.052993953));
#159727=CARTESIAN_POINT('Ctrl Pts',(2.18763413599994,15.2,-11.055877969));
#159728=CARTESIAN_POINT('Ctrl Pts',(2.18763413599994,11.6,-11.055877969));
#159729=CARTESIAN_POINT('Ctrl Pts',(2.18963277699994,15.2,-11.058764325));
#159730=CARTESIAN_POINT('Ctrl Pts',(2.18963277699994,11.6,-11.058764325));
#159731=CARTESIAN_POINT('Ctrl Pts',(2.19163636999994,15.2,-11.06165301));
#159732=CARTESIAN_POINT('Ctrl Pts',(2.19163636999994,11.6,-11.06165301));
#159733=CARTESIAN_POINT('Ctrl Pts',(2.19364491499995,15.2,-11.064544015));
#159734=CARTESIAN_POINT('Ctrl Pts',(2.19364491499995,11.6,-11.064544015));
#159735=CARTESIAN_POINT('Ctrl Pts',(2.19565841299994,15.2,-11.067437331));
#159736=CARTESIAN_POINT('Ctrl Pts',(2.19565841299994,11.6,-11.067437331));
#159737=CARTESIAN_POINT('Ctrl Pts',(2.19767686499994,15.2,-11.070332945));
#159738=CARTESIAN_POINT('Ctrl Pts',(2.19767686499994,11.6,-11.070332945));
#159739=CARTESIAN_POINT('Ctrl Pts',(2.19970027199994,15.2,-11.073230851));
#159740=CARTESIAN_POINT('Ctrl Pts',(2.19970027199994,11.6,-11.073230851));
#159741=CARTESIAN_POINT('Ctrl Pts',(2.20172863299994,15.2,-11.076131037));
#159742=CARTESIAN_POINT('Ctrl Pts',(2.20172863299994,11.6,-11.076131037));
#159743=CARTESIAN_POINT('Ctrl Pts',(2.20376195099994,15.2,-11.079033493));
#159744=CARTESIAN_POINT('Ctrl Pts',(2.20376195099994,11.6,-11.079033493));
#159745=CARTESIAN_POINT('Ctrl Pts',(2.20580022499994,15.2,-11.081938212));
#159746=CARTESIAN_POINT('Ctrl Pts',(2.20580022499994,11.6,-11.081938212));
#159747=CARTESIAN_POINT('Ctrl Pts',(2.20784345599994,15.2,-11.08484518));
#159748=CARTESIAN_POINT('Ctrl Pts',(2.20784345599994,11.6,-11.08484518));
#159749=CARTESIAN_POINT('Ctrl Pts',(2.20989164299994,15.2,-11.08775439));
#159750=CARTESIAN_POINT('Ctrl Pts',(2.20989164299994,11.6,-11.08775439));
#159751=CARTESIAN_POINT('Ctrl Pts',(2.21194478899994,15.2,-11.090665832));
#159752=CARTESIAN_POINT('Ctrl Pts',(2.21194478899994,11.6,-11.090665832));
#159753=CARTESIAN_POINT('Ctrl Pts',(2.21400289399994,15.2,-11.093579495));
#159754=CARTESIAN_POINT('Ctrl Pts',(2.21400289399994,11.6,-11.093579495));
#159755=CARTESIAN_POINT('Ctrl Pts',(2.21606595699994,15.2,-11.096495371));
#159756=CARTESIAN_POINT('Ctrl Pts',(2.21606595699994,11.6,-11.096495371));
#159757=CARTESIAN_POINT('Ctrl Pts',(2.21813398099994,15.2,-11.099413448));
#159758=CARTESIAN_POINT('Ctrl Pts',(2.21813398099994,11.6,-11.099413448));
#159759=CARTESIAN_POINT('Ctrl Pts',(2.22020696299994,15.2,-11.10233372));
#159760=CARTESIAN_POINT('Ctrl Pts',(2.22020696299994,11.6,-11.10233372));
#159761=CARTESIAN_POINT('Ctrl Pts',(2.22228490799994,15.2,-11.105256173));
#159762=CARTESIAN_POINT('Ctrl Pts',(2.22228490799994,11.6,-11.105256173));
#159763=CARTESIAN_POINT('Ctrl Pts',(2.22436781299994,15.2,-11.1081808));
#159764=CARTESIAN_POINT('Ctrl Pts',(2.22436781299994,11.6,-11.1081808));
#159765=CARTESIAN_POINT('Ctrl Pts',(2.22645567899994,15.2,-11.111107592));
#159766=CARTESIAN_POINT('Ctrl Pts',(2.22645567899994,11.6,-11.111107592));
#159767=CARTESIAN_POINT('Ctrl Pts',(2.22854850699994,15.2,-11.114036538));
#159768=CARTESIAN_POINT('Ctrl Pts',(2.22854850699994,11.6,-11.114036538));
#159769=CARTESIAN_POINT('Ctrl Pts',(2.23064629799994,15.2,-11.116967627));
#159770=CARTESIAN_POINT('Ctrl Pts',(2.23064629799994,11.6,-11.116967627));
#159771=CARTESIAN_POINT('Ctrl Pts',(2.23274905199994,15.2,-11.119900853));
#159772=CARTESIAN_POINT('Ctrl Pts',(2.23274905199994,11.6,-11.119900853));
#159773=CARTESIAN_POINT('Ctrl Pts',(2.23485676999994,15.2,-11.122836204));
#159774=CARTESIAN_POINT('Ctrl Pts',(2.23485676999994,11.6,-11.122836204));
#159775=CARTESIAN_POINT('Ctrl Pts',(2.23696945199995,15.2,-11.125773671));
#159776=CARTESIAN_POINT('Ctrl Pts',(2.23696945199995,11.6,-11.125773671));
#159777=CARTESIAN_POINT('Ctrl Pts',(2.23908709799994,15.2,-11.128713243));
#159778=CARTESIAN_POINT('Ctrl Pts',(2.23908709799994,11.6,-11.128713243));
#159779=CARTESIAN_POINT('Ctrl Pts',(2.24120970899994,15.2,-11.131654914));
#159780=CARTESIAN_POINT('Ctrl Pts',(2.24120970899994,11.6,-11.131654914));
#159781=CARTESIAN_POINT('Ctrl Pts',(2.24333728499994,15.2,-11.134598671));
#159782=CARTESIAN_POINT('Ctrl Pts',(2.24333728499994,11.6,-11.134598671));
#159783=CARTESIAN_POINT('Ctrl Pts',(2.24546982699994,15.2,-11.137544507));
#159784=CARTESIAN_POINT('Ctrl Pts',(2.24546982699994,11.6,-11.137544507));
#159785=CARTESIAN_POINT('Ctrl Pts',(2.24760733499994,15.2,-11.140492411));
#159786=CARTESIAN_POINT('Ctrl Pts',(2.24760733499994,11.6,-11.140492411));
#159787=CARTESIAN_POINT('Ctrl Pts',(2.24974980999994,15.2,-11.143442374));
#159788=CARTESIAN_POINT('Ctrl Pts',(2.24974980999994,11.6,-11.143442374));
#159789=CARTESIAN_POINT('Ctrl Pts',(2.25189725099994,15.2,-11.146394387));
#159790=CARTESIAN_POINT('Ctrl Pts',(2.25189725099994,11.6,-11.146394387));
#159791=CARTESIAN_POINT('Ctrl Pts',(2.25404965899994,15.2,-11.14934844));
#159792=CARTESIAN_POINT('Ctrl Pts',(2.25404965899994,11.6,-11.14934844));
#159793=CARTESIAN_POINT('Ctrl Pts',(2.25620703599994,15.2,-11.152304524));
#159794=CARTESIAN_POINT('Ctrl Pts',(2.25620703599994,11.6,-11.152304524));
#159795=CARTESIAN_POINT('Ctrl Pts',(2.25836937999994,15.2,-11.15526263));
#159796=CARTESIAN_POINT('Ctrl Pts',(2.25836937999994,11.6,-11.15526263));
#159797=CARTESIAN_POINT('Ctrl Pts',(2.26053669299994,15.2,-11.158222747));
#159798=CARTESIAN_POINT('Ctrl Pts',(2.26053669299994,11.6,-11.158222747));
#159799=CARTESIAN_POINT('Ctrl Pts',(2.26270897299994,15.2,-11.161184868));
#159800=CARTESIAN_POINT('Ctrl Pts',(2.26270897299994,11.6,-11.161184868));
#159801=CARTESIAN_POINT('Ctrl Pts',(2.26488622499994,15.2,-11.164148983));
#159802=CARTESIAN_POINT('Ctrl Pts',(2.26488622499994,11.6,-11.164148983));
#159803=CARTESIAN_POINT('Ctrl Pts',(2.26706844499994,15.2,-11.16711508));
#159804=CARTESIAN_POINT('Ctrl Pts',(2.26706844499994,11.6,-11.16711508));
#159805=CARTESIAN_POINT('Ctrl Pts',(2.26925563399994,15.2,-11.170083153));
#159806=CARTESIAN_POINT('Ctrl Pts',(2.26925563399994,11.6,-11.170083153));
#159807=CARTESIAN_POINT('Ctrl Pts',(2.27144779299994,15.2,-11.173053191));
#159808=CARTESIAN_POINT('Ctrl Pts',(2.27144779299994,11.6,-11.173053191));
#159809=CARTESIAN_POINT('Ctrl Pts',(2.27364492299994,15.2,-11.176025185));
#159810=CARTESIAN_POINT('Ctrl Pts',(2.27364492299994,11.6,-11.176025185));
#159811=CARTESIAN_POINT('Ctrl Pts',(2.27584702399994,15.2,-11.178999126));
#159812=CARTESIAN_POINT('Ctrl Pts',(2.27584702399994,11.6,-11.178999126));
#159813=CARTESIAN_POINT('Ctrl Pts',(2.27805409499994,15.2,-11.181975005));
#159814=CARTESIAN_POINT('Ctrl Pts',(2.27805409499994,11.6,-11.181975005));
#159815=CARTESIAN_POINT('Ctrl Pts',(2.28026613799994,15.2,-11.184952813));
#159816=CARTESIAN_POINT('Ctrl Pts',(2.28026613799994,11.6,-11.184952813));
#159817=CARTESIAN_POINT('Ctrl Pts',(2.28248315299994,15.2,-11.187932541));
#159818=CARTESIAN_POINT('Ctrl Pts',(2.28248315299994,11.6,-11.187932541));
#159819=CARTESIAN_POINT('Ctrl Pts',(2.28470513799994,15.2,-11.190914179));
#159820=CARTESIAN_POINT('Ctrl Pts',(2.28470513799994,11.6,-11.190914179));
#159821=CARTESIAN_POINT('Ctrl Pts',(2.28693209699994,15.2,-11.193897718));
#159822=CARTESIAN_POINT('Ctrl Pts',(2.28693209699994,11.6,-11.193897718));
#159823=CARTESIAN_POINT('Ctrl Pts',(2.28916402699994,15.2,-11.19688315));
#159824=CARTESIAN_POINT('Ctrl Pts',(2.28916402699994,11.6,-11.19688315));
#159825=CARTESIAN_POINT('Ctrl Pts',(2.29140092999994,15.2,-11.199870463));
#159826=CARTESIAN_POINT('Ctrl Pts',(2.29140092999994,11.6,-11.199870463));
#159827=CARTESIAN_POINT('Ctrl Pts',(2.29364280599994,15.2,-11.202859649));
#159828=CARTESIAN_POINT('Ctrl Pts',(2.29364280599994,11.6,-11.202859649));
#159829=CARTESIAN_POINT('Ctrl Pts',(2.29588965499994,15.2,-11.205850698));
#159830=CARTESIAN_POINT('Ctrl Pts',(2.29588965499994,11.6,-11.205850698));
#159831=CARTESIAN_POINT('Ctrl Pts',(2.29814147699994,15.2,-11.208843602));
#159832=CARTESIAN_POINT('Ctrl Pts',(2.29814147699994,11.6,-11.208843602));
#159833=CARTESIAN_POINT('Ctrl Pts',(2.30039827299994,15.2,-11.211838352));
#159834=CARTESIAN_POINT('Ctrl Pts',(2.30039827299994,11.6,-11.211838352));
#159835=CARTESIAN_POINT('Ctrl Pts',(2.30266004099994,15.2,-11.214834939));
#159836=CARTESIAN_POINT('Ctrl Pts',(2.30266004099994,11.6,-11.214834939));
#159837=CARTESIAN_POINT('Ctrl Pts',(2.30492678499994,15.2,-11.217833355));
#159838=CARTESIAN_POINT('Ctrl Pts',(2.30492678499994,11.6,-11.217833355));
#159839=CARTESIAN_POINT('Ctrl Pts',(2.30719850199994,15.2,-11.220833593));
#159840=CARTESIAN_POINT('Ctrl Pts',(2.30719850199994,11.6,-11.220833593));
#159841=CARTESIAN_POINT('Ctrl Pts',(2.30947519299994,15.2,-11.223835644));
#159842=CARTESIAN_POINT('Ctrl Pts',(2.30947519299994,11.6,-11.223835644));
#159843=CARTESIAN_POINT('Ctrl Pts',(2.31175685799994,15.2,-11.226839497));
#159844=CARTESIAN_POINT('Ctrl Pts',(2.31175685799994,11.6,-11.226839497));
#159845=CARTESIAN_POINT('Ctrl Pts',(2.31404349799994,15.2,-11.229845144));
#159846=CARTESIAN_POINT('Ctrl Pts',(2.31404349799994,11.6,-11.229845144));
#159847=CARTESIAN_POINT('Ctrl Pts',(2.31633511299994,15.2,-11.232852572));
#159848=CARTESIAN_POINT('Ctrl Pts',(2.31633511299994,11.6,-11.232852572));
#159849=CARTESIAN_POINT('Ctrl Pts',(2.31863170299994,15.2,-11.235861771));
#159850=CARTESIAN_POINT('Ctrl Pts',(2.31863170299994,11.6,-11.235861771));
#159851=CARTESIAN_POINT('Ctrl Pts',(2.32093326799994,15.2,-11.238872729));
#159852=CARTESIAN_POINT('Ctrl Pts',(2.32093326799994,11.6,-11.238872729));
#159853=CARTESIAN_POINT('Ctrl Pts',(2.32323980899994,15.2,-11.241885437));
#159854=CARTESIAN_POINT('Ctrl Pts',(2.32323980899994,11.6,-11.241885437));
#159855=CARTESIAN_POINT('Ctrl Pts',(2.32555132399995,15.2,-11.244899887));
#159856=CARTESIAN_POINT('Ctrl Pts',(2.32555132399995,11.6,-11.244899887));
#159857=CARTESIAN_POINT('Ctrl Pts',(2.32786781499994,15.2,-11.247916073));
#159858=CARTESIAN_POINT('Ctrl Pts',(2.32786781499994,11.6,-11.247916073));
#159859=CARTESIAN_POINT('Ctrl Pts',(2.33018928299995,15.2,-11.250933991));
#159860=CARTESIAN_POINT('Ctrl Pts',(2.33018928299995,11.6,-11.250933991));
#159861=CARTESIAN_POINT('Ctrl Pts',(2.33251572399995,15.2,-11.253953638));
#159862=CARTESIAN_POINT('Ctrl Pts',(2.33251572399995,11.6,-11.253953638));
#159863=CARTESIAN_POINT('Ctrl Pts',(2.33438085799994,15.2,-11.256370739));
#159864=CARTESIAN_POINT('Ctrl Pts',(2.33438085799994,11.6,-11.256370739));
#159865=CARTESIAN_POINT('Ctrl Pts',(2.33578194799994,15.2,-11.258184341));
#159866=CARTESIAN_POINT('Ctrl Pts',(2.33578194799994,11.6,-11.258184341));
#159867=CARTESIAN_POINT('Ctrl Pts',(2.33671700199995,15.2,-11.259393754));
#159868=CARTESIAN_POINT('Ctrl Pts',(2.33671700199995,11.6,-11.259393754));
#159869=CARTESIAN_POINT('Ctrl Pts',(2.33718477799994,15.2,-11.259998548));
#159870=CARTESIAN_POINT('Ctrl Pts',(2.33718477799994,11.6,-11.259998548));
#159871=CARTESIAN_POINT('Ctrl Pts',(1.76496130699994,15.2,-10.223773109));
#159872=CARTESIAN_POINT('Ctrl Pts',(1.76500562299994,15.2,-10.223941741));
#159873=CARTESIAN_POINT('Ctrl Pts',(1.76509588899994,15.2,-10.224284873));
#159874=CARTESIAN_POINT('Ctrl Pts',(1.76523291899994,15.2,-10.224804731));
#159875=CARTESIAN_POINT('Ctrl Pts',(1.76541803299994,15.2,-10.22550489));
#159876=CARTESIAN_POINT('Ctrl Pts',(1.76565305799994,15.2,-10.226390254));
#159877=CARTESIAN_POINT('Ctrl Pts',(1.76589279499994,15.2,-10.227289727));
#159878=CARTESIAN_POINT('Ctrl Pts',(1.76613589399994,15.2,-10.228198149));
#159879=CARTESIAN_POINT('Ctrl Pts',(1.76638236599994,15.2,-10.229115492));
#159880=CARTESIAN_POINT('Ctrl Pts',(1.76663221999994,15.2,-10.230041723));
#159881=CARTESIAN_POINT('Ctrl Pts',(1.76688546699994,15.2,-10.230976812));
#159882=CARTESIAN_POINT('Ctrl Pts',(1.76714211699994,15.2,-10.231920729));
#159883=CARTESIAN_POINT('Ctrl Pts',(1.76740218099994,15.2,-10.232873443));
#159884=CARTESIAN_POINT('Ctrl Pts',(1.76766566999994,15.2,-10.233834926));
#159885=CARTESIAN_POINT('Ctrl Pts',(1.76793259299994,15.2,-10.234805146));
#159886=CARTESIAN_POINT('Ctrl Pts',(1.76820295999994,15.2,-10.235784073));
#159887=CARTESIAN_POINT('Ctrl Pts',(1.76847678199994,15.2,-10.23677168));
#159888=CARTESIAN_POINT('Ctrl Pts',(1.76875406799994,15.2,-10.237767935));
#159889=CARTESIAN_POINT('Ctrl Pts',(1.76903482799994,15.2,-10.238772809));
#159890=CARTESIAN_POINT('Ctrl Pts',(1.76931907099994,15.2,-10.239786274));
#159891=CARTESIAN_POINT('Ctrl Pts',(1.76960680899994,15.2,-10.2408083));
#159892=CARTESIAN_POINT('Ctrl Pts',(1.76989805199994,15.2,-10.241838858));
#159893=CARTESIAN_POINT('Ctrl Pts',(1.77019280699994,15.2,-10.24287792));
#159894=CARTESIAN_POINT('Ctrl Pts',(1.77049108499994,15.2,-10.243925456));
#159895=CARTESIAN_POINT('Ctrl Pts',(1.77079289599994,15.2,-10.244981439));
#159896=CARTESIAN_POINT('Ctrl Pts',(1.77109824899994,15.2,-10.246045839));
#159897=CARTESIAN_POINT('Ctrl Pts',(1.77140715299994,15.2,-10.247118629));
#159898=CARTESIAN_POINT('Ctrl Pts',(1.77171961899994,15.2,-10.248199781));
#159899=CARTESIAN_POINT('Ctrl Pts',(1.77203565399994,15.2,-10.249289267));
#159900=CARTESIAN_POINT('Ctrl Pts',(1.77235526999994,15.2,-10.250387057));
#159901=CARTESIAN_POINT('Ctrl Pts',(1.77267847299994,15.2,-10.251493125));
#159902=CARTESIAN_POINT('Ctrl Pts',(1.77300527499994,15.2,-10.252607443));
#159903=CARTESIAN_POINT('Ctrl Pts',(1.77333568299994,15.2,-10.253729984));
#159904=CARTESIAN_POINT('Ctrl Pts',(1.77366970799994,15.2,-10.25486072));
#159905=CARTESIAN_POINT('Ctrl Pts',(1.77400735799994,15.2,-10.255999624));
#159906=CARTESIAN_POINT('Ctrl Pts',(1.77434864199994,15.2,-10.257146668));
#159907=CARTESIAN_POINT('Ctrl Pts',(1.77469356799994,15.2,-10.258301827));
#159908=CARTESIAN_POINT('Ctrl Pts',(1.77504214599994,15.2,-10.259465073));
#159909=CARTESIAN_POINT('Ctrl Pts',(1.77539438599994,15.2,-10.260636378));
#159910=CARTESIAN_POINT('Ctrl Pts',(1.77575029399994,15.2,-10.261815716));
#159911=CARTESIAN_POINT('Ctrl Pts',(1.77610987999994,15.2,-10.263003061));
#159912=CARTESIAN_POINT('Ctrl Pts',(1.77647315199994,15.2,-10.264198387));
#159913=CARTESIAN_POINT('Ctrl Pts',(1.77684011999994,15.2,-10.265401666));
#159914=CARTESIAN_POINT('Ctrl Pts',(1.77721079199994,15.2,-10.266612874));
#159915=CARTESIAN_POINT('Ctrl Pts',(1.77758517499994,15.2,-10.267831982));
#159916=CARTESIAN_POINT('Ctrl Pts',(1.77796327899994,15.2,-10.269058966));
#159917=CARTESIAN_POINT('Ctrl Pts',(1.77834511299995,15.2,-10.2702938));
#159918=CARTESIAN_POINT('Ctrl Pts',(1.77873068199994,15.2,-10.271536458));
#159919=CARTESIAN_POINT('Ctrl Pts',(1.77911999799994,15.2,-10.272786914));
#159920=CARTESIAN_POINT('Ctrl Pts',(1.77951306799994,15.2,-10.274045143));
#159921=CARTESIAN_POINT('Ctrl Pts',(1.77990989999994,15.2,-10.275311119));
#159922=CARTESIAN_POINT('Ctrl Pts',(1.78031050099994,15.2,-10.276584816));
#159923=CARTESIAN_POINT('Ctrl Pts',(1.78071487999994,15.2,-10.27786621));
#159924=CARTESIAN_POINT('Ctrl Pts',(1.78112304599994,15.2,-10.279155276));
#159925=CARTESIAN_POINT('Ctrl Pts',(1.78153500599994,15.2,-10.280451988));
#159926=CARTESIAN_POINT('Ctrl Pts',(1.78195076699994,15.2,-10.281756321));
#159927=CARTESIAN_POINT('Ctrl Pts',(1.78237033899994,15.2,-10.283068252));
#159928=CARTESIAN_POINT('Ctrl Pts',(1.78279372899994,15.2,-10.284387754));
#159929=CARTESIAN_POINT('Ctrl Pts',(1.78322094399994,15.2,-10.285714803));
#159930=CARTESIAN_POINT('Ctrl Pts',(1.78365199299995,15.2,-10.287049375));
#159931=CARTESIAN_POINT('Ctrl Pts',(1.78408688299994,15.2,-10.288391446));
#159932=CARTESIAN_POINT('Ctrl Pts',(1.78452562099994,15.2,-10.28974099));
#159933=CARTESIAN_POINT('Ctrl Pts',(1.78496821499994,15.2,-10.291097983));
#159934=CARTESIAN_POINT('Ctrl Pts',(1.78541467399994,15.2,-10.292462403));
#159935=CARTESIAN_POINT('Ctrl Pts',(1.78586500399994,15.2,-10.293834224));
#159936=CARTESIAN_POINT('Ctrl Pts',(1.78631921299994,15.2,-10.295213422));
#159937=CARTESIAN_POINT('Ctrl Pts',(1.78677730899994,15.2,-10.296599975));
#159938=CARTESIAN_POINT('Ctrl Pts',(1.78723929699994,15.2,-10.297993858));
#159939=CARTESIAN_POINT('Ctrl Pts',(1.78770518699994,15.2,-10.299395046));
#159940=CARTESIAN_POINT('Ctrl Pts',(1.78817498599994,15.2,-10.300803517));
#159941=CARTESIAN_POINT('Ctrl Pts',(1.78864869999994,15.2,-10.302219248));
#159942=CARTESIAN_POINT('Ctrl Pts',(1.78912633699994,15.2,-10.303642215));
#159943=CARTESIAN_POINT('Ctrl Pts',(1.78960790399994,15.2,-10.305072393));
#159944=CARTESIAN_POINT('Ctrl Pts',(1.79009340899994,15.2,-10.306509762));
#159945=CARTESIAN_POINT('Ctrl Pts',(1.79058285799994,15.2,-10.307954296));
#159946=CARTESIAN_POINT('Ctrl Pts',(1.79107625799994,15.2,-10.309405975));
#159947=CARTESIAN_POINT('Ctrl Pts',(1.79157361699994,15.2,-10.310864772));
#159948=CARTESIAN_POINT('Ctrl Pts',(1.79207494099994,15.2,-10.312330668));
#159949=CARTESIAN_POINT('Ctrl Pts',(1.79258023699994,15.2,-10.313803638));
#159950=CARTESIAN_POINT('Ctrl Pts',(1.79308951199994,15.2,-10.315283661));
#159951=CARTESIAN_POINT('Ctrl Pts',(1.79360277399994,15.2,-10.316770712));
#159952=CARTESIAN_POINT('Ctrl Pts',(1.79412002899994,15.2,-10.318264771));
#159953=CARTESIAN_POINT('Ctrl Pts',(1.79464128299994,15.2,-10.319765813));
#159954=CARTESIAN_POINT('Ctrl Pts',(1.79516654299994,15.2,-10.321273818));
#159955=CARTESIAN_POINT('Ctrl Pts',(1.79569581699994,15.2,-10.322788763));
#159956=CARTESIAN_POINT('Ctrl Pts',(1.79622910999994,15.2,-10.324310627));
#159957=CARTESIAN_POINT('Ctrl Pts',(1.79676642999994,15.2,-10.325839385));
#159958=CARTESIAN_POINT('Ctrl Pts',(1.79730778399994,15.2,-10.327375017));
#159959=CARTESIAN_POINT('Ctrl Pts',(1.79785317499994,15.2,-10.328917501));
#159960=CARTESIAN_POINT('Ctrl Pts',(1.79840261399994,15.2,-10.330466814));
#159961=CARTESIAN_POINT('Ctrl Pts',(1.79895610399994,15.2,-10.332022936));
#159962=CARTESIAN_POINT('Ctrl Pts',(1.79951365499994,15.2,-10.333585844));
#159963=CARTESIAN_POINT('Ctrl Pts',(1.80007526999994,15.2,-10.335155517));
#159964=CARTESIAN_POINT('Ctrl Pts',(1.80064095699994,15.2,-10.336731933));
#159965=CARTESIAN_POINT('Ctrl Pts',(1.80121072099994,15.2,-10.338315071));
#159966=CARTESIAN_POINT('Ctrl Pts',(1.80178457199994,15.2,-10.33990491));
#159967=CARTESIAN_POINT('Ctrl Pts',(1.80236250999994,15.2,-10.341501427));
#159968=CARTESIAN_POINT('Ctrl Pts',(1.80294454699994,15.2,-10.343104603));
#159969=CARTESIAN_POINT('Ctrl Pts',(1.80353068699994,15.2,-10.344714415));
#159970=CARTESIAN_POINT('Ctrl Pts',(1.80412093499994,15.2,-10.346330843));
#159971=CARTESIAN_POINT('Ctrl Pts',(1.80471529899994,15.2,-10.347953866));
#159972=CARTESIAN_POINT('Ctrl Pts',(1.80531378399994,15.2,-10.349583463));
#159973=CARTESIAN_POINT('Ctrl Pts',(1.80591639699994,15.2,-10.351219612));
#159974=CARTESIAN_POINT('Ctrl Pts',(1.80652314299994,15.2,-10.352862295));
#159975=CARTESIAN_POINT('Ctrl Pts',(1.80713402799994,15.2,-10.354511488));
#159976=CARTESIAN_POINT('Ctrl Pts',(1.80774905899994,15.2,-10.356167172));
#159977=CARTESIAN_POINT('Ctrl Pts',(1.80836823999994,15.2,-10.357829328));
#159978=CARTESIAN_POINT('Ctrl Pts',(1.80899157899994,15.2,-10.359497933));
#159979=CARTESIAN_POINT('Ctrl Pts',(1.80961908099994,15.2,-10.361172966));
#159980=CARTESIAN_POINT('Ctrl Pts',(1.81025075099994,15.2,-10.36285441));
#159981=CARTESIAN_POINT('Ctrl Pts',(1.81088659599994,15.2,-10.364542242));
#159982=CARTESIAN_POINT('Ctrl Pts',(1.81152661999994,15.2,-10.366236444));
#159983=CARTESIAN_POINT('Ctrl Pts',(1.81217083099994,15.2,-10.367936993));
#159984=CARTESIAN_POINT('Ctrl Pts',(1.81281923299994,15.2,-10.369643871));
#159985=CARTESIAN_POINT('Ctrl Pts',(1.81347183299994,15.2,-10.371357057));
#159986=CARTESIAN_POINT('Ctrl Pts',(1.81412863499994,15.2,-10.373076533));
#159987=CARTESIAN_POINT('Ctrl Pts',(1.81478964499994,15.2,-10.374802277));
#159988=CARTESIAN_POINT('Ctrl Pts',(1.81545486999994,15.2,-10.37653427));
#159989=CARTESIAN_POINT('Ctrl Pts',(1.81612431399994,15.2,-10.378272492));
#159990=CARTESIAN_POINT('Ctrl Pts',(1.81679798299994,15.2,-10.380016924));
#159991=CARTESIAN_POINT('Ctrl Pts',(1.81747588199994,15.2,-10.381767545));
#159992=CARTESIAN_POINT('Ctrl Pts',(1.81815801699994,15.2,-10.383524338));
#159993=CARTESIAN_POINT('Ctrl Pts',(1.81884439299994,15.2,-10.385287281));
#159994=CARTESIAN_POINT('Ctrl Pts',(1.81953501599994,15.2,-10.387056356));
#159995=CARTESIAN_POINT('Ctrl Pts',(1.82022989099994,15.2,-10.388831543));
#159996=CARTESIAN_POINT('Ctrl Pts',(1.82092902199994,15.2,-10.390612824));
#159997=CARTESIAN_POINT('Ctrl Pts',(1.82163241599994,15.2,-10.392400178));
#159998=CARTESIAN_POINT('Ctrl Pts',(1.82234007799994,15.2,-10.394193587));
#159999=CARTESIAN_POINT('Ctrl Pts',(1.82305201199994,15.2,-10.395993031));
#160000=CARTESIAN_POINT('Ctrl Pts',(1.82376822599994,15.2,-10.397798492));
#160001=CARTESIAN_POINT('Ctrl Pts',(1.82448872099994,15.2,-10.399609952));
#160002=CARTESIAN_POINT('Ctrl Pts',(1.82521350499994,15.2,-10.401427389));
#160003=CARTESIAN_POINT('Ctrl Pts',(1.82594258299994,15.2,-10.403250787));
#160004=CARTESIAN_POINT('Ctrl Pts',(1.82667595799994,15.2,-10.405080125));
#160005=CARTESIAN_POINT('Ctrl Pts',(1.82741363699994,15.2,-10.406915387));
#160006=CARTESIAN_POINT('Ctrl Pts',(1.82815562499994,15.2,-10.408756552));
#160007=CARTESIAN_POINT('Ctrl Pts',(1.82890192699994,15.2,-10.410603603));
#160008=CARTESIAN_POINT('Ctrl Pts',(1.82965254599994,15.2,-10.41245652));
#160009=CARTESIAN_POINT('Ctrl Pts',(1.83040748999994,15.2,-10.414315286));
#160010=CARTESIAN_POINT('Ctrl Pts',(1.83116676099994,15.2,-10.416179881));
#160011=CARTESIAN_POINT('Ctrl Pts',(1.83193036499994,15.2,-10.418050288));
#160012=CARTESIAN_POINT('Ctrl Pts',(1.83269830799994,15.2,-10.419926488));
#160013=CARTESIAN_POINT('Ctrl Pts',(1.83347059199994,15.2,-10.421808463));
#160014=CARTESIAN_POINT('Ctrl Pts',(1.83424722399994,15.2,-10.423696194));
#160015=CARTESIAN_POINT('Ctrl Pts',(1.83502820899994,15.2,-10.425589665));
#160016=CARTESIAN_POINT('Ctrl Pts',(1.83581354999994,15.2,-10.427488857));
#160017=CARTESIAN_POINT('Ctrl Pts',(1.83660325299994,15.2,-10.429393751));
#160018=CARTESIAN_POINT('Ctrl Pts',(1.83739732299994,15.2,-10.431304329));
#160019=CARTESIAN_POINT('Ctrl Pts',(1.83819576299994,15.2,-10.433220574));
#160020=CARTESIAN_POINT('Ctrl Pts',(1.83899857899994,15.2,-10.435142468));
#160021=CARTESIAN_POINT('Ctrl Pts',(1.83980577599994,15.2,-10.437069993));
#160022=CARTESIAN_POINT('Ctrl Pts',(1.84061735599994,15.2,-10.439003132));
#160023=CARTESIAN_POINT('Ctrl Pts',(1.84143332699994,15.2,-10.440941867));
#160024=CARTESIAN_POINT('Ctrl Pts',(1.84225369099994,15.2,-10.442886179));
#160025=CARTESIAN_POINT('Ctrl Pts',(1.84307845299994,15.2,-10.444836053));
#160026=CARTESIAN_POINT('Ctrl Pts',(1.84390761699994,15.2,-10.446791469));
#160027=CARTESIAN_POINT('Ctrl Pts',(1.84474118899994,15.2,-10.44875241));
#160028=CARTESIAN_POINT('Ctrl Pts',(1.84557917199994,15.2,-10.45071886));
#160029=CARTESIAN_POINT('Ctrl Pts',(1.84642157199994,15.2,-10.452690801));
#160030=CARTESIAN_POINT('Ctrl Pts',(1.84726839199994,15.2,-10.454668215));
#160031=CARTESIAN_POINT('Ctrl Pts',(1.84811963599994,15.2,-10.456651085));
#160032=CARTESIAN_POINT('Ctrl Pts',(1.84897530999994,15.2,-10.458639395));
#160033=CARTESIAN_POINT('Ctrl Pts',(1.84983541599994,15.2,-10.460633126));
#160034=CARTESIAN_POINT('Ctrl Pts',(1.85069995999994,15.2,-10.462632262));
#160035=CARTESIAN_POINT('Ctrl Pts',(1.85156894599994,15.2,-10.464636786));
#160036=CARTESIAN_POINT('Ctrl Pts',(1.85244237799994,15.2,-10.46664668));
#160037=CARTESIAN_POINT('Ctrl Pts',(1.85332025899994,15.2,-10.468661929));
#160038=CARTESIAN_POINT('Ctrl Pts',(1.85420259499994,15.2,-10.470682514));
#160039=CARTESIAN_POINT('Ctrl Pts',(1.85508938999994,15.2,-10.47270842));
#160040=CARTESIAN_POINT('Ctrl Pts',(1.85598064599994,15.2,-10.474739628));
#160041=CARTESIAN_POINT('Ctrl Pts',(1.85687636999994,15.2,-10.476776123));
#160042=CARTESIAN_POINT('Ctrl Pts',(1.85777656499994,15.2,-10.478817888));
#160043=CARTESIAN_POINT('Ctrl Pts',(1.85868123399994,15.2,-10.480864906));
#160044=CARTESIAN_POINT('Ctrl Pts',(1.85959038199994,15.2,-10.48291716));
#160045=CARTESIAN_POINT('Ctrl Pts',(1.86050401199994,15.2,-10.484974634));
#160046=CARTESIAN_POINT('Ctrl Pts',(1.86142212899994,15.2,-10.487037312));
#160047=CARTESIAN_POINT('Ctrl Pts',(1.86234473699994,15.2,-10.489105177));
#160048=CARTESIAN_POINT('Ctrl Pts',(1.86327183899994,15.2,-10.491178213));
#160049=CARTESIAN_POINT('Ctrl Pts',(1.86420344099994,15.2,-10.493256403));
#160050=CARTESIAN_POINT('Ctrl Pts',(1.86513954299994,15.2,-10.49533973));
#160051=CARTESIAN_POINT('Ctrl Pts',(1.86608015299994,15.2,-10.497428179));
#160052=CARTESIAN_POINT('Ctrl Pts',(1.86702527199994,15.2,-10.499521733));
#160053=CARTESIAN_POINT('Ctrl Pts',(1.86797490499994,15.2,-10.501620377));
#160054=CARTESIAN_POINT('Ctrl Pts',(1.86892905699994,15.2,-10.503724094));
#160055=CARTESIAN_POINT('Ctrl Pts',(1.86988772999995,15.2,-10.505832868));
#160056=CARTESIAN_POINT('Ctrl Pts',(1.87085092699994,15.2,-10.507946683));
#160057=CARTESIAN_POINT('Ctrl Pts',(1.87181865399994,15.2,-10.510065522));
#160058=CARTESIAN_POINT('Ctrl Pts',(1.87279091299994,15.2,-10.512189371));
#160059=CARTESIAN_POINT('Ctrl Pts',(1.87376770899994,15.2,-10.514318212));
#160060=CARTESIAN_POINT('Ctrl Pts',(1.87474904299994,15.2,-10.516452031));
#160061=CARTESIAN_POINT('Ctrl Pts',(1.87573492299994,15.2,-10.518590811));
#160062=CARTESIAN_POINT('Ctrl Pts',(1.87672534799994,15.2,-10.520734536));
#160063=CARTESIAN_POINT('Ctrl Pts',(1.87772032499994,15.2,-10.522883192));
#160064=CARTESIAN_POINT('Ctrl Pts',(1.87871985699994,15.2,-10.525036762));
#160065=CARTESIAN_POINT('Ctrl Pts',(1.87972394599994,15.2,-10.52719523));
#160066=CARTESIAN_POINT('Ctrl Pts',(1.88073259699994,15.2,-10.529358581));
#160067=CARTESIAN_POINT('Ctrl Pts',(1.88174581199994,15.2,-10.531526798));
#160068=CARTESIAN_POINT('Ctrl Pts',(1.88276359599994,15.2,-10.533699869));
#160069=CARTESIAN_POINT('Ctrl Pts',(1.88378595299994,15.2,-10.535877775));
#160070=CARTESIAN_POINT('Ctrl Pts',(1.88481288399994,15.2,-10.538060503));
#160071=CARTESIAN_POINT('Ctrl Pts',(1.88584439399994,15.2,-10.540248035));
#160072=CARTESIAN_POINT('Ctrl Pts',(1.88688048599994,15.2,-10.542440358));
#160073=CARTESIAN_POINT('Ctrl Pts',(1.88792116399994,15.2,-10.544637455));
#160074=CARTESIAN_POINT('Ctrl Pts',(1.88896643099994,15.2,-10.546839313));
#160075=CARTESIAN_POINT('Ctrl Pts',(1.89001628999994,15.2,-10.549045913));
#160076=CARTESIAN_POINT('Ctrl Pts',(1.89107074499994,15.2,-10.551257244));
#160077=CARTESIAN_POINT('Ctrl Pts',(1.89212979899994,15.2,-10.553473288));
#160078=CARTESIAN_POINT('Ctrl Pts',(1.89319345499994,15.2,-10.555694032));
#160079=CARTESIAN_POINT('Ctrl Pts',(1.89426171599994,15.2,-10.557919458));
#160080=CARTESIAN_POINT('Ctrl Pts',(1.89533458699994,15.2,-10.560149554));
#160081=CARTESIAN_POINT('Ctrl Pts',(1.89641206899994,15.2,-10.562384303));
#160082=CARTESIAN_POINT('Ctrl Pts',(1.89749416599994,15.2,-10.564623691));
#160083=CARTESIAN_POINT('Ctrl Pts',(1.89858088099994,15.2,-10.566867703));
#160084=CARTESIAN_POINT('Ctrl Pts',(1.89967221899994,15.2,-10.569116324));
#160085=CARTESIAN_POINT('Ctrl Pts',(1.90076818099994,15.2,-10.571369539));
#160086=CARTESIAN_POINT('Ctrl Pts',(1.90186877099994,15.2,-10.573627333));
#160087=CARTESIAN_POINT('Ctrl Pts',(1.90297399099994,15.2,-10.575889692));
#160088=CARTESIAN_POINT('Ctrl Pts',(1.90408384599994,15.2,-10.578156601));
#160089=CARTESIAN_POINT('Ctrl Pts',(1.90519833799994,15.2,-10.580428044));
#160090=CARTESIAN_POINT('Ctrl Pts',(1.90631746999994,15.2,-10.582704009));
#160091=CARTESIAN_POINT('Ctrl Pts',(1.90744124499994,15.2,-10.584984479));
#160092=CARTESIAN_POINT('Ctrl Pts',(1.90856966599994,15.2,-10.587269441));
#160093=CARTESIAN_POINT('Ctrl Pts',(1.90970273699994,15.2,-10.58955888));
#160094=CARTESIAN_POINT('Ctrl Pts',(1.91084045999994,15.2,-10.59185278));
#160095=CARTESIAN_POINT('Ctrl Pts',(1.91198283799994,15.2,-10.594151129));
#160096=CARTESIAN_POINT('Ctrl Pts',(1.91312987399994,15.2,-10.59645391));
#160097=CARTESIAN_POINT('Ctrl Pts',(1.91428157099994,15.2,-10.598761112));
#160098=CARTESIAN_POINT('Ctrl Pts',(1.91543793199994,15.2,-10.601072717));
#160099=CARTESIAN_POINT('Ctrl Pts',(1.91659895999994,15.2,-10.603388714));
#160100=CARTESIAN_POINT('Ctrl Pts',(1.91776465699994,15.2,-10.605709085));
#160101=CARTESIAN_POINT('Ctrl Pts',(1.91893502699994,15.2,-10.60803382));
#160102=CARTESIAN_POINT('Ctrl Pts',(1.92011007299994,15.2,-10.610362901));
#160103=CARTESIAN_POINT('Ctrl Pts',(1.92128979599994,15.2,-10.612696316));
#160104=CARTESIAN_POINT('Ctrl Pts',(1.92247420099994,15.2,-10.615034051));
#160105=CARTESIAN_POINT('Ctrl Pts',(1.92366328999994,15.2,-10.617376091));
#160106=CARTESIAN_POINT('Ctrl Pts',(1.92485706499994,15.2,-10.619722422));
#160107=CARTESIAN_POINT('Ctrl Pts',(1.92605552899994,15.2,-10.622073029));
#160108=CARTESIAN_POINT('Ctrl Pts',(1.92725868499994,15.2,-10.6244279));
#160109=CARTESIAN_POINT('Ctrl Pts',(1.92846653599994,15.2,-10.62678702));
#160110=CARTESIAN_POINT('Ctrl Pts',(1.92967908399994,15.2,-10.629150376));
#160111=CARTESIAN_POINT('Ctrl Pts',(1.93089633299994,15.2,-10.631517953));
#160112=CARTESIAN_POINT('Ctrl Pts',(1.93211828499994,15.2,-10.633889738));
#160113=CARTESIAN_POINT('Ctrl Pts',(1.93334494199994,15.2,-10.636265715));
#160114=CARTESIAN_POINT('Ctrl Pts',(1.93457630699994,15.2,-10.638645874));
#160115=CARTESIAN_POINT('Ctrl Pts',(1.93581238299994,15.2,-10.641030197));
#160116=CARTESIAN_POINT('Ctrl Pts',(1.93705317299994,15.2,-10.643418674));
#160117=CARTESIAN_POINT('Ctrl Pts',(1.93829867699994,15.2,-10.645811289));
#160118=CARTESIAN_POINT('Ctrl Pts',(1.93954889999994,15.2,-10.648208029));
#160119=CARTESIAN_POINT('Ctrl Pts',(1.94080384499994,15.2,-10.650608881));
#160120=CARTESIAN_POINT('Ctrl Pts',(1.94206351299994,15.2,-10.65301383));
#160121=CARTESIAN_POINT('Ctrl Pts',(1.94332790699994,15.2,-10.655422864));
#160122=CARTESIAN_POINT('Ctrl Pts',(1.94459702899994,15.2,-10.657835968));
#160123=CARTESIAN_POINT('Ctrl Pts',(1.94587088199994,15.2,-10.660253129));
#160124=CARTESIAN_POINT('Ctrl Pts',(1.94714946899994,15.2,-10.662674334));
#160125=CARTESIAN_POINT('Ctrl Pts',(1.94843279199994,15.2,-10.665099571));
#160126=CARTESIAN_POINT('Ctrl Pts',(1.94972085299994,15.2,-10.667528823));
#160127=CARTESIAN_POINT('Ctrl Pts',(1.95101365499994,15.2,-10.66996208));
#160128=CARTESIAN_POINT('Ctrl Pts',(1.95231119999994,15.2,-10.672399326));
#160129=CARTESIAN_POINT('Ctrl Pts',(1.95361349099994,15.2,-10.674840549));
#160130=CARTESIAN_POINT('Ctrl Pts',(1.95492052999994,15.2,-10.677285737));
#160131=CARTESIAN_POINT('Ctrl Pts',(1.95623231799994,15.2,-10.679734874));
#160132=CARTESIAN_POINT('Ctrl Pts',(1.95754885999994,15.2,-10.682187948));
#160133=CARTESIAN_POINT('Ctrl Pts',(1.95887015699994,15.2,-10.684644947));
#160134=CARTESIAN_POINT('Ctrl Pts',(1.96019620999994,15.2,-10.687105856));
#160135=CARTESIAN_POINT('Ctrl Pts',(1.96152702299994,15.2,-10.689570664));
#160136=CARTESIAN_POINT('Ctrl Pts',(1.96286259899994,15.2,-10.692039356));
#160137=CARTESIAN_POINT('Ctrl Pts',(1.96420293799994,15.2,-10.694511919));
#160138=CARTESIAN_POINT('Ctrl Pts',(1.96554804399994,15.2,-10.696988341));
#160139=CARTESIAN_POINT('Ctrl Pts',(1.96689791799994,15.2,-10.699468609));
#160140=CARTESIAN_POINT('Ctrl Pts',(1.96825256199994,15.2,-10.70195271));
#160141=CARTESIAN_POINT('Ctrl Pts',(1.96961197999994,15.2,-10.704440629));
#160142=CARTESIAN_POINT('Ctrl Pts',(1.97097617299994,15.2,-10.706932355));
#160143=CARTESIAN_POINT('Ctrl Pts',(1.97234514399994,15.2,-10.709427876));
#160144=CARTESIAN_POINT('Ctrl Pts',(1.97371889299994,15.2,-10.711927177));
#160145=CARTESIAN_POINT('Ctrl Pts',(1.97509742499994,15.2,-10.714430247));
#160146=CARTESIAN_POINT('Ctrl Pts',(1.97648073999994,15.2,-10.716937073));
#160147=CARTESIAN_POINT('Ctrl Pts',(1.97786884099994,15.2,-10.71944764));
#160148=CARTESIAN_POINT('Ctrl Pts',(1.97926172999994,15.2,-10.721961937));
#160149=CARTESIAN_POINT('Ctrl Pts',(1.98065940899994,15.2,-10.724479952));
#160150=CARTESIAN_POINT('Ctrl Pts',(1.98206188099994,15.2,-10.727001672));
#160151=CARTESIAN_POINT('Ctrl Pts',(1.98346914499994,15.2,-10.729527083));
#160152=CARTESIAN_POINT('Ctrl Pts',(1.98488120699994,15.2,-10.732056173));
#160153=CARTESIAN_POINT('Ctrl Pts',(1.98629806699994,15.2,-10.73458893));
#160154=CARTESIAN_POINT('Ctrl Pts',(1.98771972699994,15.2,-10.737125341));
#160155=CARTESIAN_POINT('Ctrl Pts',(1.98914618999994,15.2,-10.739665394));
#160156=CARTESIAN_POINT('Ctrl Pts',(1.99057745699994,15.2,-10.742209076));
#160157=CARTESIAN_POINT('Ctrl Pts',(1.99201352899994,15.2,-10.744756374));
#160158=CARTESIAN_POINT('Ctrl Pts',(1.99345441099994,15.2,-10.747307276));
#160159=CARTESIAN_POINT('Ctrl Pts',(1.99490010199994,15.2,-10.74986177));
#160160=CARTESIAN_POINT('Ctrl Pts',(1.99635060499994,15.2,-10.752419844));
#160161=CARTESIAN_POINT('Ctrl Pts',(1.99780592199994,15.2,-10.754981484));
#160162=CARTESIAN_POINT('Ctrl Pts',(1.99926605499994,15.2,-10.757546678));
#160163=CARTESIAN_POINT('Ctrl Pts',(2.00073100599994,15.2,-10.760115415));
#160164=CARTESIAN_POINT('Ctrl Pts',(2.00220077599994,15.2,-10.762687682));
#160165=CARTESIAN_POINT('Ctrl Pts',(2.00367536799994,15.2,-10.765263466));
#160166=CARTESIAN_POINT('Ctrl Pts',(2.00515478199994,15.2,-10.767842756));
#160167=CARTESIAN_POINT('Ctrl Pts',(2.00663902299994,15.2,-10.77042554));
#160168=CARTESIAN_POINT('Ctrl Pts',(2.00812808999994,15.2,-10.773011803));
#160169=CARTESIAN_POINT('Ctrl Pts',(2.00962198599994,15.2,-10.775601537));
#160170=CARTESIAN_POINT('Ctrl Pts',(2.01112071299994,15.2,-10.778194727));
#160171=CARTESIAN_POINT('Ctrl Pts',(2.01262427099994,15.2,-10.780791361));
#160172=CARTESIAN_POINT('Ctrl Pts',(2.01413266399994,15.2,-10.783391428));
#160173=CARTESIAN_POINT('Ctrl Pts',(2.01564589299994,15.2,-10.785994916));
#160174=CARTESIAN_POINT('Ctrl Pts',(2.01716395899994,15.2,-10.788601812));
#160175=CARTESIAN_POINT('Ctrl Pts',(2.01868686499994,15.2,-10.791212104));
#160176=CARTESIAN_POINT('Ctrl Pts',(2.02021461099994,15.2,-10.793825781));
#160177=CARTESIAN_POINT('Ctrl Pts',(2.02174720099995,15.2,-10.796442831));
#160178=CARTESIAN_POINT('Ctrl Pts',(2.02328463399994,15.2,-10.799063241));
#160179=CARTESIAN_POINT('Ctrl Pts',(2.02482691399994,15.2,-10.801687));
#160180=CARTESIAN_POINT('Ctrl Pts',(2.02637404199994,15.2,-10.804314097));
#160181=CARTESIAN_POINT('Ctrl Pts',(2.02792601899994,15.2,-10.806944517));
#160182=CARTESIAN_POINT('Ctrl Pts',(2.02948284599994,15.2,-10.809578251));
#160183=CARTESIAN_POINT('Ctrl Pts',(2.03104452699994,15.2,-10.812215287));
#160184=CARTESIAN_POINT('Ctrl Pts',(2.03261106199994,15.2,-10.814855611));
#160185=CARTESIAN_POINT('Ctrl Pts',(2.03418245199994,15.2,-10.817499214));
#160186=CARTESIAN_POINT('Ctrl Pts',(2.03575870099994,15.2,-10.820146083));
#160187=CARTESIAN_POINT('Ctrl Pts',(2.03733980799994,15.2,-10.822796206));
#160188=CARTESIAN_POINT('Ctrl Pts',(2.03892577499994,15.2,-10.825449572));
#160189=CARTESIAN_POINT('Ctrl Pts',(2.04051660599994,15.2,-10.82810617));
#160190=CARTESIAN_POINT('Ctrl Pts',(2.04211229899994,15.2,-10.830765986));
#160191=CARTESIAN_POINT('Ctrl Pts',(2.04371285699994,15.2,-10.833429011));
#160192=CARTESIAN_POINT('Ctrl Pts',(2.04531828199995,15.2,-10.836095232));
#160193=CARTESIAN_POINT('Ctrl Pts',(2.04692857599994,15.2,-10.838764637));
#160194=CARTESIAN_POINT('Ctrl Pts',(2.04854373899995,15.2,-10.841437216));
#160195=CARTESIAN_POINT('Ctrl Pts',(2.05016377299994,15.2,-10.844112955));
#160196=CARTESIAN_POINT('Ctrl Pts',(2.05178868099994,15.2,-10.846791846));
#160197=CARTESIAN_POINT('Ctrl Pts',(2.05341846199994,15.2,-10.849473875));
#160198=CARTESIAN_POINT('Ctrl Pts',(2.05505311799994,15.2,-10.852159032));
#160199=CARTESIAN_POINT('Ctrl Pts',(2.05669265099994,15.2,-10.854847303));
#160200=CARTESIAN_POINT('Ctrl Pts',(2.05833706199994,15.2,-10.85753868));
#160201=CARTESIAN_POINT('Ctrl Pts',(2.05998635399994,15.2,-10.86023315));
#160202=CARTESIAN_POINT('Ctrl Pts',(2.06164052499994,15.2,-10.862930702));
#160203=CARTESIAN_POINT('Ctrl Pts',(2.06329958099994,15.2,-10.865631323));
#160204=CARTESIAN_POINT('Ctrl Pts',(2.06496351899994,15.2,-10.868335004));
#160205=CARTESIAN_POINT('Ctrl Pts',(2.06663234299994,15.2,-10.871041734));
#160206=CARTESIAN_POINT('Ctrl Pts',(2.06830605399994,15.2,-10.873751499));
#160207=CARTESIAN_POINT('Ctrl Pts',(2.06998465199994,15.2,-10.876464289));
#160208=CARTESIAN_POINT('Ctrl Pts',(2.07166813899994,15.2,-10.879180094));
#160209=CARTESIAN_POINT('Ctrl Pts',(2.07335651799994,15.2,-10.881898902));
#160210=CARTESIAN_POINT('Ctrl Pts',(2.07504978799994,15.2,-10.884620701));
#160211=CARTESIAN_POINT('Ctrl Pts',(2.07674794999994,15.2,-10.887345482));
#160212=CARTESIAN_POINT('Ctrl Pts',(2.07845100699994,15.2,-10.890073231));
#160213=CARTESIAN_POINT('Ctrl Pts',(2.08015896099994,15.2,-10.89280394));
#160214=CARTESIAN_POINT('Ctrl Pts',(2.08187181099994,15.2,-10.895537595));
#160215=CARTESIAN_POINT('Ctrl Pts',(2.08358955799994,15.2,-10.898274186));
#160216=CARTESIAN_POINT('Ctrl Pts',(2.08531220499994,15.2,-10.901013703));
#160217=CARTESIAN_POINT('Ctrl Pts',(2.08703975299994,15.2,-10.903756135));
#160218=CARTESIAN_POINT('Ctrl Pts',(2.08877220299994,15.2,-10.906501469));
#160219=CARTESIAN_POINT('Ctrl Pts',(2.09050955499994,15.2,-10.909249695));
#160220=CARTESIAN_POINT('Ctrl Pts',(2.09225181099994,15.2,-10.912000804));
#160221=CARTESIAN_POINT('Ctrl Pts',(2.09399897299994,15.2,-10.914754782));
#160222=CARTESIAN_POINT('Ctrl Pts',(2.09575104199994,15.2,-10.91751162));
#160223=CARTESIAN_POINT('Ctrl Pts',(2.09750801799994,15.2,-10.920271306));
#160224=CARTESIAN_POINT('Ctrl Pts',(2.09926990199994,15.2,-10.92303383));
#160225=CARTESIAN_POINT('Ctrl Pts',(2.10103669699994,15.2,-10.925799182));
#160226=CARTESIAN_POINT('Ctrl Pts',(2.10280840299994,15.2,-10.928567349));
#160227=CARTESIAN_POINT('Ctrl Pts',(2.10458501999994,15.2,-10.931338321));
#160228=CARTESIAN_POINT('Ctrl Pts',(2.10636655199994,15.2,-10.934112088));
#160229=CARTESIAN_POINT('Ctrl Pts',(2.10815299699994,15.2,-10.936888638));
#160230=CARTESIAN_POINT('Ctrl Pts',(2.10994435799994,15.2,-10.939667962));
#160231=CARTESIAN_POINT('Ctrl Pts',(2.11174063499994,15.2,-10.942450048));
#160232=CARTESIAN_POINT('Ctrl Pts',(2.11354182899994,15.2,-10.945234885));
#160233=CARTESIAN_POINT('Ctrl Pts',(2.11534794299994,15.2,-10.948022463));
#160234=CARTESIAN_POINT('Ctrl Pts',(2.11715897499994,15.2,-10.950812772));
#160235=CARTESIAN_POINT('Ctrl Pts',(2.11897492799995,15.2,-10.953605801));
#160236=CARTESIAN_POINT('Ctrl Pts',(2.12079580299994,15.2,-10.956401537));
#160237=CARTESIAN_POINT('Ctrl Pts',(2.12262159999994,15.2,-10.959199973));
#160238=CARTESIAN_POINT('Ctrl Pts',(2.12445232199994,15.2,-10.962001096));
#160239=CARTESIAN_POINT('Ctrl Pts',(2.12628796699994,15.2,-10.964804897));
#160240=CARTESIAN_POINT('Ctrl Pts',(2.12812853899994,15.2,-10.967611364));
#160241=CARTESIAN_POINT('Ctrl Pts',(2.12997403599994,15.2,-10.970420488));
#160242=CARTESIAN_POINT('Ctrl Pts',(2.13182446099994,15.2,-10.973232257));
#160243=CARTESIAN_POINT('Ctrl Pts',(2.13367981499994,15.2,-10.976046662));
#160244=CARTESIAN_POINT('Ctrl Pts',(2.13554009799994,15.2,-10.978863691));
#160245=CARTESIAN_POINT('Ctrl Pts',(2.13740531099994,15.2,-10.981683335));
#160246=CARTESIAN_POINT('Ctrl Pts',(2.13927545499994,15.2,-10.984505583));
#160247=CARTESIAN_POINT('Ctrl Pts',(2.14115053099994,15.2,-10.987330423));
#160248=CARTESIAN_POINT('Ctrl Pts',(2.14303053999994,15.2,-10.990157848));
#160249=CARTESIAN_POINT('Ctrl Pts',(2.14491548299994,15.2,-10.992987845));
#160250=CARTESIAN_POINT('Ctrl Pts',(2.14680536099995,15.2,-10.995820404));
#160251=CARTESIAN_POINT('Ctrl Pts',(2.14870017399994,15.2,-10.998655516));
#160252=CARTESIAN_POINT('Ctrl Pts',(2.15059992399994,15.2,-11.00149317));
#160253=CARTESIAN_POINT('Ctrl Pts',(2.15250460999994,15.2,-11.004333355));
#160254=CARTESIAN_POINT('Ctrl Pts',(2.15441423499994,15.2,-11.007176061));
#160255=CARTESIAN_POINT('Ctrl Pts',(2.15632879899994,15.2,-11.010021278));
#160256=CARTESIAN_POINT('Ctrl Pts',(2.15824830199994,15.2,-11.012868997));
#160257=CARTESIAN_POINT('Ctrl Pts',(2.16017274599994,15.2,-11.015719205));
#160258=CARTESIAN_POINT('Ctrl Pts',(2.16210213199994,15.2,-11.018571894));
#160259=CARTESIAN_POINT('Ctrl Pts',(2.16403645899994,15.2,-11.021427054));
#160260=CARTESIAN_POINT('Ctrl Pts',(2.16597572899994,15.2,-11.024284674));
#160261=CARTESIAN_POINT('Ctrl Pts',(2.16791994199994,15.2,-11.027144743));
#160262=CARTESIAN_POINT('Ctrl Pts',(2.16986909999994,15.2,-11.030007252));
#160263=CARTESIAN_POINT('Ctrl Pts',(2.17182320399994,15.2,-11.032872191));
#160264=CARTESIAN_POINT('Ctrl Pts',(2.17378225199994,15.2,-11.03573955));
#160265=CARTESIAN_POINT('Ctrl Pts',(2.17574624699994,15.2,-11.038609318));
#160266=CARTESIAN_POINT('Ctrl Pts',(2.17771518999994,15.2,-11.041481486));
#160267=CARTESIAN_POINT('Ctrl Pts',(2.17968908099994,15.2,-11.044356044));
#160268=CARTESIAN_POINT('Ctrl Pts',(2.18166791999994,15.2,-11.047232981));
#160269=CARTESIAN_POINT('Ctrl Pts',(2.18365170899994,15.2,-11.050112287));
#160270=CARTESIAN_POINT('Ctrl Pts',(2.18564044699994,15.2,-11.052993953));
#160271=CARTESIAN_POINT('Ctrl Pts',(2.18763413599994,15.2,-11.055877969));
#160272=CARTESIAN_POINT('Ctrl Pts',(2.18963277699994,15.2,-11.058764325));
#160273=CARTESIAN_POINT('Ctrl Pts',(2.19163636999994,15.2,-11.06165301));
#160274=CARTESIAN_POINT('Ctrl Pts',(2.19364491499995,15.2,-11.064544015));
#160275=CARTESIAN_POINT('Ctrl Pts',(2.19565841299994,15.2,-11.067437331));
#160276=CARTESIAN_POINT('Ctrl Pts',(2.19767686499994,15.2,-11.070332945));
#160277=CARTESIAN_POINT('Ctrl Pts',(2.19970027199994,15.2,-11.073230851));
#160278=CARTESIAN_POINT('Ctrl Pts',(2.20172863299994,15.2,-11.076131037));
#160279=CARTESIAN_POINT('Ctrl Pts',(2.20376195099994,15.2,-11.079033493));
#160280=CARTESIAN_POINT('Ctrl Pts',(2.20580022499994,15.2,-11.081938212));
#160281=CARTESIAN_POINT('Ctrl Pts',(2.20784345599994,15.2,-11.08484518));
#160282=CARTESIAN_POINT('Ctrl Pts',(2.20989164299994,15.2,-11.08775439));
#160283=CARTESIAN_POINT('Ctrl Pts',(2.21194478899994,15.2,-11.090665832));
#160284=CARTESIAN_POINT('Ctrl Pts',(2.21400289399994,15.2,-11.093579495));
#160285=CARTESIAN_POINT('Ctrl Pts',(2.21606595699994,15.2,-11.096495371));
#160286=CARTESIAN_POINT('Ctrl Pts',(2.21813398099994,15.2,-11.099413448));
#160287=CARTESIAN_POINT('Ctrl Pts',(2.22020696299994,15.2,-11.10233372));
#160288=CARTESIAN_POINT('Ctrl Pts',(2.22228490799994,15.2,-11.105256173));
#160289=CARTESIAN_POINT('Ctrl Pts',(2.22436781299994,15.2,-11.1081808));
#160290=CARTESIAN_POINT('Ctrl Pts',(2.22645567899994,15.2,-11.111107592));
#160291=CARTESIAN_POINT('Ctrl Pts',(2.22854850699994,15.2,-11.114036538));
#160292=CARTESIAN_POINT('Ctrl Pts',(2.23064629799994,15.2,-11.116967627));
#160293=CARTESIAN_POINT('Ctrl Pts',(2.23274905199994,15.2,-11.119900853));
#160294=CARTESIAN_POINT('Ctrl Pts',(2.23485676999994,15.2,-11.122836204));
#160295=CARTESIAN_POINT('Ctrl Pts',(2.23696945199995,15.2,-11.125773671));
#160296=CARTESIAN_POINT('Ctrl Pts',(2.23908709799994,15.2,-11.128713243));
#160297=CARTESIAN_POINT('Ctrl Pts',(2.24120970899994,15.2,-11.131654914));
#160298=CARTESIAN_POINT('Ctrl Pts',(2.24333728499994,15.2,-11.134598671));
#160299=CARTESIAN_POINT('Ctrl Pts',(2.24546982699994,15.2,-11.137544507));
#160300=CARTESIAN_POINT('Ctrl Pts',(2.24760733499994,15.2,-11.140492411));
#160301=CARTESIAN_POINT('Ctrl Pts',(2.24974980999994,15.2,-11.143442374));
#160302=CARTESIAN_POINT('Ctrl Pts',(2.25189725099994,15.2,-11.146394387));
#160303=CARTESIAN_POINT('Ctrl Pts',(2.25404965899994,15.2,-11.14934844));
#160304=CARTESIAN_POINT('Ctrl Pts',(2.25620703599994,15.2,-11.152304524));
#160305=CARTESIAN_POINT('Ctrl Pts',(2.25836937999994,15.2,-11.15526263));
#160306=CARTESIAN_POINT('Ctrl Pts',(2.26053669299994,15.2,-11.158222747));
#160307=CARTESIAN_POINT('Ctrl Pts',(2.26270897299994,15.2,-11.161184868));
#160308=CARTESIAN_POINT('Ctrl Pts',(2.26488622499994,15.2,-11.164148983));
#160309=CARTESIAN_POINT('Ctrl Pts',(2.26706844499994,15.2,-11.16711508));
#160310=CARTESIAN_POINT('Ctrl Pts',(2.26925563399994,15.2,-11.170083153));
#160311=CARTESIAN_POINT('Ctrl Pts',(2.27144779299994,15.2,-11.173053191));
#160312=CARTESIAN_POINT('Ctrl Pts',(2.27364492299994,15.2,-11.176025185));
#160313=CARTESIAN_POINT('Ctrl Pts',(2.27584702399994,15.2,-11.178999126));
#160314=CARTESIAN_POINT('Ctrl Pts',(2.27805409499994,15.2,-11.181975005));
#160315=CARTESIAN_POINT('Ctrl Pts',(2.28026613799994,15.2,-11.184952813));
#160316=CARTESIAN_POINT('Ctrl Pts',(2.28248315299994,15.2,-11.187932541));
#160317=CARTESIAN_POINT('Ctrl Pts',(2.28470513799994,15.2,-11.190914179));
#160318=CARTESIAN_POINT('Ctrl Pts',(2.28693209699994,15.2,-11.193897718));
#160319=CARTESIAN_POINT('Ctrl Pts',(2.28916402699994,15.2,-11.19688315));
#160320=CARTESIAN_POINT('Ctrl Pts',(2.29140092999994,15.2,-11.199870463));
#160321=CARTESIAN_POINT('Ctrl Pts',(2.29364280599994,15.2,-11.202859649));
#160322=CARTESIAN_POINT('Ctrl Pts',(2.29588965499994,15.2,-11.205850698));
#160323=CARTESIAN_POINT('Ctrl Pts',(2.29814147699994,15.2,-11.208843602));
#160324=CARTESIAN_POINT('Ctrl Pts',(2.30039827299994,15.2,-11.211838352));
#160325=CARTESIAN_POINT('Ctrl Pts',(2.30266004099994,15.2,-11.214834939));
#160326=CARTESIAN_POINT('Ctrl Pts',(2.30492678499994,15.2,-11.217833355));
#160327=CARTESIAN_POINT('Ctrl Pts',(2.30719850199994,15.2,-11.220833593));
#160328=CARTESIAN_POINT('Ctrl Pts',(2.30947519299994,15.2,-11.223835644));
#160329=CARTESIAN_POINT('Ctrl Pts',(2.31175685799994,15.2,-11.226839497));
#160330=CARTESIAN_POINT('Ctrl Pts',(2.31404349799994,15.2,-11.229845144));
#160331=CARTESIAN_POINT('Ctrl Pts',(2.31633511299994,15.2,-11.232852572));
#160332=CARTESIAN_POINT('Ctrl Pts',(2.31863170299994,15.2,-11.235861771));
#160333=CARTESIAN_POINT('Ctrl Pts',(2.32093326799994,15.2,-11.238872729));
#160334=CARTESIAN_POINT('Ctrl Pts',(2.32323980899994,15.2,-11.241885437));
#160335=CARTESIAN_POINT('Ctrl Pts',(2.32555132399995,15.2,-11.244899887));
#160336=CARTESIAN_POINT('Ctrl Pts',(2.32786781499994,15.2,-11.247916073));
#160337=CARTESIAN_POINT('Ctrl Pts',(2.33018928299995,15.2,-11.250933991));
#160338=CARTESIAN_POINT('Ctrl Pts',(2.33251572399995,15.2,-11.253953638));
#160339=CARTESIAN_POINT('Ctrl Pts',(2.33438085799994,15.2,-11.256370739));
#160340=CARTESIAN_POINT('Ctrl Pts',(2.33578194799994,15.2,-11.258184341));
#160341=CARTESIAN_POINT('Ctrl Pts',(2.33671700199995,15.2,-11.259393754));
#160342=CARTESIAN_POINT('Ctrl Pts',(2.33718477799994,15.2,-11.259998548));
#160343=CARTESIAN_POINT('Ctrl Pts',(1.76496130699994,12.2,-10.223773109));
#160344=CARTESIAN_POINT('Ctrl Pts',(1.76500562299994,12.2,-10.223941741));
#160345=CARTESIAN_POINT('Ctrl Pts',(1.76509588899994,12.2,-10.224284873));
#160346=CARTESIAN_POINT('Ctrl Pts',(1.76523291899994,12.2,-10.224804731));
#160347=CARTESIAN_POINT('Ctrl Pts',(1.76541803299994,12.2,-10.22550489));
#160348=CARTESIAN_POINT('Ctrl Pts',(1.76565305799994,12.2,-10.226390254));
#160349=CARTESIAN_POINT('Ctrl Pts',(1.76589279499994,12.2,-10.227289727));
#160350=CARTESIAN_POINT('Ctrl Pts',(1.76613589399994,12.2,-10.228198149));
#160351=CARTESIAN_POINT('Ctrl Pts',(1.76638236599994,12.2,-10.229115492));
#160352=CARTESIAN_POINT('Ctrl Pts',(1.76663221999994,12.2,-10.230041723));
#160353=CARTESIAN_POINT('Ctrl Pts',(1.76688546699994,12.2,-10.230976812));
#160354=CARTESIAN_POINT('Ctrl Pts',(1.76714211699994,12.2,-10.231920729));
#160355=CARTESIAN_POINT('Ctrl Pts',(1.76740218099994,12.2,-10.232873443));
#160356=CARTESIAN_POINT('Ctrl Pts',(1.76766566999994,12.2,-10.233834926));
#160357=CARTESIAN_POINT('Ctrl Pts',(1.76793259299994,12.2,-10.234805146));
#160358=CARTESIAN_POINT('Ctrl Pts',(1.76820295999994,12.2,-10.235784073));
#160359=CARTESIAN_POINT('Ctrl Pts',(1.76847678199994,12.2,-10.23677168));
#160360=CARTESIAN_POINT('Ctrl Pts',(1.76875406799994,12.2,-10.237767935));
#160361=CARTESIAN_POINT('Ctrl Pts',(1.76903482799994,12.2,-10.238772809));
#160362=CARTESIAN_POINT('Ctrl Pts',(1.76931907099994,12.2,-10.239786274));
#160363=CARTESIAN_POINT('Ctrl Pts',(1.76960680899994,12.2,-10.2408083));
#160364=CARTESIAN_POINT('Ctrl Pts',(1.76989805199994,12.2,-10.241838858));
#160365=CARTESIAN_POINT('Ctrl Pts',(1.77019280699994,12.2,-10.24287792));
#160366=CARTESIAN_POINT('Ctrl Pts',(1.77049108499994,12.2,-10.243925456));
#160367=CARTESIAN_POINT('Ctrl Pts',(1.77079289599994,12.2,-10.244981439));
#160368=CARTESIAN_POINT('Ctrl Pts',(1.77109824899994,12.2,-10.246045839));
#160369=CARTESIAN_POINT('Ctrl Pts',(1.77140715299994,12.2,-10.247118629));
#160370=CARTESIAN_POINT('Ctrl Pts',(1.77171961899994,12.2,-10.248199781));
#160371=CARTESIAN_POINT('Ctrl Pts',(1.77203565399994,12.2,-10.249289267));
#160372=CARTESIAN_POINT('Ctrl Pts',(1.77235526999994,12.2,-10.250387057));
#160373=CARTESIAN_POINT('Ctrl Pts',(1.77267847299994,12.2,-10.251493125));
#160374=CARTESIAN_POINT('Ctrl Pts',(1.77300527499994,12.2,-10.252607443));
#160375=CARTESIAN_POINT('Ctrl Pts',(1.77333568299994,12.2,-10.253729984));
#160376=CARTESIAN_POINT('Ctrl Pts',(1.77366970799994,12.2,-10.25486072));
#160377=CARTESIAN_POINT('Ctrl Pts',(1.77400735799994,12.2,-10.255999624));
#160378=CARTESIAN_POINT('Ctrl Pts',(1.77434864199994,12.2,-10.257146668));
#160379=CARTESIAN_POINT('Ctrl Pts',(1.77469356799994,12.2,-10.258301827));
#160380=CARTESIAN_POINT('Ctrl Pts',(1.77504214599994,12.2,-10.259465073));
#160381=CARTESIAN_POINT('Ctrl Pts',(1.77539438599994,12.2,-10.260636378));
#160382=CARTESIAN_POINT('Ctrl Pts',(1.77575029399994,12.2,-10.261815716));
#160383=CARTESIAN_POINT('Ctrl Pts',(1.77610987999994,12.2,-10.263003061));
#160384=CARTESIAN_POINT('Ctrl Pts',(1.77647315199994,12.2,-10.264198387));
#160385=CARTESIAN_POINT('Ctrl Pts',(1.77684011999994,12.2,-10.265401666));
#160386=CARTESIAN_POINT('Ctrl Pts',(1.77721079199994,12.2,-10.266612874));
#160387=CARTESIAN_POINT('Ctrl Pts',(1.77758517499994,12.2,-10.267831982));
#160388=CARTESIAN_POINT('Ctrl Pts',(1.77796327899994,12.2,-10.269058966));
#160389=CARTESIAN_POINT('Ctrl Pts',(1.77834511299995,12.2,-10.2702938));
#160390=CARTESIAN_POINT('Ctrl Pts',(1.77873068199994,12.2,-10.271536458));
#160391=CARTESIAN_POINT('Ctrl Pts',(1.77911999799994,12.2,-10.272786914));
#160392=CARTESIAN_POINT('Ctrl Pts',(1.77951306799994,12.2,-10.274045143));
#160393=CARTESIAN_POINT('Ctrl Pts',(1.77990989999994,12.2,-10.275311119));
#160394=CARTESIAN_POINT('Ctrl Pts',(1.78031050099994,12.2,-10.276584816));
#160395=CARTESIAN_POINT('Ctrl Pts',(1.78071487999994,12.2,-10.27786621));
#160396=CARTESIAN_POINT('Ctrl Pts',(1.78112304599994,12.2,-10.279155276));
#160397=CARTESIAN_POINT('Ctrl Pts',(1.78153500599994,12.2,-10.280451988));
#160398=CARTESIAN_POINT('Ctrl Pts',(1.78195076699994,12.2,-10.281756321));
#160399=CARTESIAN_POINT('Ctrl Pts',(1.78237033899994,12.2,-10.283068252));
#160400=CARTESIAN_POINT('Ctrl Pts',(1.78279372899994,12.2,-10.284387754));
#160401=CARTESIAN_POINT('Ctrl Pts',(1.78322094399994,12.2,-10.285714803));
#160402=CARTESIAN_POINT('Ctrl Pts',(1.78365199299995,12.2,-10.287049375));
#160403=CARTESIAN_POINT('Ctrl Pts',(1.78408688299994,12.2,-10.288391446));
#160404=CARTESIAN_POINT('Ctrl Pts',(1.78452562099994,12.2,-10.28974099));
#160405=CARTESIAN_POINT('Ctrl Pts',(1.78496821499994,12.2,-10.291097983));
#160406=CARTESIAN_POINT('Ctrl Pts',(1.78541467399994,12.2,-10.292462403));
#160407=CARTESIAN_POINT('Ctrl Pts',(1.78586500399994,12.2,-10.293834224));
#160408=CARTESIAN_POINT('Ctrl Pts',(1.78631921299994,12.2,-10.295213422));
#160409=CARTESIAN_POINT('Ctrl Pts',(1.78677730899994,12.2,-10.296599975));
#160410=CARTESIAN_POINT('Ctrl Pts',(1.78723929699994,12.2,-10.297993858));
#160411=CARTESIAN_POINT('Ctrl Pts',(1.78770518699994,12.2,-10.299395046));
#160412=CARTESIAN_POINT('Ctrl Pts',(1.78817498599994,12.2,-10.300803517));
#160413=CARTESIAN_POINT('Ctrl Pts',(1.78864869999994,12.2,-10.302219248));
#160414=CARTESIAN_POINT('Ctrl Pts',(1.78912633699994,12.2,-10.303642215));
#160415=CARTESIAN_POINT('Ctrl Pts',(1.78960790399994,12.2,-10.305072393));
#160416=CARTESIAN_POINT('Ctrl Pts',(1.79009340899994,12.2,-10.306509762));
#160417=CARTESIAN_POINT('Ctrl Pts',(1.79058285799994,12.2,-10.307954296));
#160418=CARTESIAN_POINT('Ctrl Pts',(1.79107625799994,12.2,-10.309405975));
#160419=CARTESIAN_POINT('Ctrl Pts',(1.79157361699994,12.2,-10.310864772));
#160420=CARTESIAN_POINT('Ctrl Pts',(1.79207494099994,12.2,-10.312330668));
#160421=CARTESIAN_POINT('Ctrl Pts',(1.79258023699994,12.2,-10.313803638));
#160422=CARTESIAN_POINT('Ctrl Pts',(1.79308951199994,12.2,-10.315283661));
#160423=CARTESIAN_POINT('Ctrl Pts',(1.79360277399994,12.2,-10.316770712));
#160424=CARTESIAN_POINT('Ctrl Pts',(1.79412002899994,12.2,-10.318264771));
#160425=CARTESIAN_POINT('Ctrl Pts',(1.79464128299994,12.2,-10.319765813));
#160426=CARTESIAN_POINT('Ctrl Pts',(1.79516654299994,12.2,-10.321273818));
#160427=CARTESIAN_POINT('Ctrl Pts',(1.79569581699994,12.2,-10.322788763));
#160428=CARTESIAN_POINT('Ctrl Pts',(1.79622910999994,12.2,-10.324310627));
#160429=CARTESIAN_POINT('Ctrl Pts',(1.79676642999994,12.2,-10.325839385));
#160430=CARTESIAN_POINT('Ctrl Pts',(1.79730778399994,12.2,-10.327375017));
#160431=CARTESIAN_POINT('Ctrl Pts',(1.79785317499994,12.2,-10.328917501));
#160432=CARTESIAN_POINT('Ctrl Pts',(1.79840261399994,12.2,-10.330466814));
#160433=CARTESIAN_POINT('Ctrl Pts',(1.79895610399994,12.2,-10.332022936));
#160434=CARTESIAN_POINT('Ctrl Pts',(1.79951365499994,12.2,-10.333585844));
#160435=CARTESIAN_POINT('Ctrl Pts',(1.80007526999994,12.2,-10.335155517));
#160436=CARTESIAN_POINT('Ctrl Pts',(1.80064095699994,12.2,-10.336731933));
#160437=CARTESIAN_POINT('Ctrl Pts',(1.80121072099994,12.2,-10.338315071));
#160438=CARTESIAN_POINT('Ctrl Pts',(1.80178457199994,12.2,-10.33990491));
#160439=CARTESIAN_POINT('Ctrl Pts',(1.80236250999994,12.2,-10.341501427));
#160440=CARTESIAN_POINT('Ctrl Pts',(1.80294454699994,12.2,-10.343104603));
#160441=CARTESIAN_POINT('Ctrl Pts',(1.80353068699994,12.2,-10.344714415));
#160442=CARTESIAN_POINT('Ctrl Pts',(1.80412093499994,12.2,-10.346330843));
#160443=CARTESIAN_POINT('Ctrl Pts',(1.80471529899994,12.2,-10.347953866));
#160444=CARTESIAN_POINT('Ctrl Pts',(1.80531378399994,12.2,-10.349583463));
#160445=CARTESIAN_POINT('Ctrl Pts',(1.80591639699994,12.2,-10.351219612));
#160446=CARTESIAN_POINT('Ctrl Pts',(1.80652314299994,12.2,-10.352862295));
#160447=CARTESIAN_POINT('Ctrl Pts',(1.80713402799994,12.2,-10.354511488));
#160448=CARTESIAN_POINT('Ctrl Pts',(1.80774905899994,12.2,-10.356167172));
#160449=CARTESIAN_POINT('Ctrl Pts',(1.80836823999994,12.2,-10.357829328));
#160450=CARTESIAN_POINT('Ctrl Pts',(1.80899157899994,12.2,-10.359497933));
#160451=CARTESIAN_POINT('Ctrl Pts',(1.80961908099994,12.2,-10.361172966));
#160452=CARTESIAN_POINT('Ctrl Pts',(1.81025075099994,12.2,-10.36285441));
#160453=CARTESIAN_POINT('Ctrl Pts',(1.81088659599994,12.2,-10.364542242));
#160454=CARTESIAN_POINT('Ctrl Pts',(1.81152661999994,12.2,-10.366236444));
#160455=CARTESIAN_POINT('Ctrl Pts',(1.81217083099994,12.2,-10.367936993));
#160456=CARTESIAN_POINT('Ctrl Pts',(1.81281923299994,12.2,-10.369643871));
#160457=CARTESIAN_POINT('Ctrl Pts',(1.81347183299994,12.2,-10.371357057));
#160458=CARTESIAN_POINT('Ctrl Pts',(1.81412863499994,12.2,-10.373076533));
#160459=CARTESIAN_POINT('Ctrl Pts',(1.81478964499994,12.2,-10.374802277));
#160460=CARTESIAN_POINT('Ctrl Pts',(1.81545486999994,12.2,-10.37653427));
#160461=CARTESIAN_POINT('Ctrl Pts',(1.81612431399994,12.2,-10.378272492));
#160462=CARTESIAN_POINT('Ctrl Pts',(1.81679798299994,12.2,-10.380016924));
#160463=CARTESIAN_POINT('Ctrl Pts',(1.81747588199994,12.2,-10.381767545));
#160464=CARTESIAN_POINT('Ctrl Pts',(1.81815801699994,12.2,-10.383524338));
#160465=CARTESIAN_POINT('Ctrl Pts',(1.81884439299994,12.2,-10.385287281));
#160466=CARTESIAN_POINT('Ctrl Pts',(1.81953501599994,12.2,-10.387056356));
#160467=CARTESIAN_POINT('Ctrl Pts',(1.82022989099994,12.2,-10.388831543));
#160468=CARTESIAN_POINT('Ctrl Pts',(1.82092902199994,12.2,-10.390612824));
#160469=CARTESIAN_POINT('Ctrl Pts',(1.82163241599994,12.2,-10.392400178));
#160470=CARTESIAN_POINT('Ctrl Pts',(1.82234007799994,12.2,-10.394193587));
#160471=CARTESIAN_POINT('Ctrl Pts',(1.82305201199994,12.2,-10.395993031));
#160472=CARTESIAN_POINT('Ctrl Pts',(1.82376822599994,12.2,-10.397798492));
#160473=CARTESIAN_POINT('Ctrl Pts',(1.82448872099994,12.2,-10.399609952));
#160474=CARTESIAN_POINT('Ctrl Pts',(1.82521350499994,12.2,-10.401427389));
#160475=CARTESIAN_POINT('Ctrl Pts',(1.82594258299994,12.2,-10.403250787));
#160476=CARTESIAN_POINT('Ctrl Pts',(1.82667595799994,12.2,-10.405080125));
#160477=CARTESIAN_POINT('Ctrl Pts',(1.82741363699994,12.2,-10.406915387));
#160478=CARTESIAN_POINT('Ctrl Pts',(1.82815562499994,12.2,-10.408756552));
#160479=CARTESIAN_POINT('Ctrl Pts',(1.82890192699994,12.2,-10.410603603));
#160480=CARTESIAN_POINT('Ctrl Pts',(1.82965254599994,12.2,-10.41245652));
#160481=CARTESIAN_POINT('Ctrl Pts',(1.83040748999994,12.2,-10.414315286));
#160482=CARTESIAN_POINT('Ctrl Pts',(1.83116676099994,12.2,-10.416179881));
#160483=CARTESIAN_POINT('Ctrl Pts',(1.83193036499994,12.2,-10.418050288));
#160484=CARTESIAN_POINT('Ctrl Pts',(1.83269830799994,12.2,-10.419926488));
#160485=CARTESIAN_POINT('Ctrl Pts',(1.83347059199994,12.2,-10.421808463));
#160486=CARTESIAN_POINT('Ctrl Pts',(1.83424722399994,12.2,-10.423696194));
#160487=CARTESIAN_POINT('Ctrl Pts',(1.83502820899994,12.2,-10.425589665));
#160488=CARTESIAN_POINT('Ctrl Pts',(1.83581354999994,12.2,-10.427488857));
#160489=CARTESIAN_POINT('Ctrl Pts',(1.83660325299994,12.2,-10.429393751));
#160490=CARTESIAN_POINT('Ctrl Pts',(1.83739732299994,12.2,-10.431304329));
#160491=CARTESIAN_POINT('Ctrl Pts',(1.83819576299994,12.2,-10.433220574));
#160492=CARTESIAN_POINT('Ctrl Pts',(1.83899857899994,12.2,-10.435142468));
#160493=CARTESIAN_POINT('Ctrl Pts',(1.83980577599994,12.2,-10.437069993));
#160494=CARTESIAN_POINT('Ctrl Pts',(1.84061735599994,12.2,-10.439003132));
#160495=CARTESIAN_POINT('Ctrl Pts',(1.84143332699994,12.2,-10.440941867));
#160496=CARTESIAN_POINT('Ctrl Pts',(1.84225369099994,12.2,-10.442886179));
#160497=CARTESIAN_POINT('Ctrl Pts',(1.84307845299994,12.2,-10.444836053));
#160498=CARTESIAN_POINT('Ctrl Pts',(1.84390761699994,12.2,-10.446791469));
#160499=CARTESIAN_POINT('Ctrl Pts',(1.84474118899994,12.2,-10.44875241));
#160500=CARTESIAN_POINT('Ctrl Pts',(1.84557917199994,12.2,-10.45071886));
#160501=CARTESIAN_POINT('Ctrl Pts',(1.84642157199994,12.2,-10.452690801));
#160502=CARTESIAN_POINT('Ctrl Pts',(1.84726839199994,12.2,-10.454668215));
#160503=CARTESIAN_POINT('Ctrl Pts',(1.84811963599994,12.2,-10.456651085));
#160504=CARTESIAN_POINT('Ctrl Pts',(1.84897530999994,12.2,-10.458639395));
#160505=CARTESIAN_POINT('Ctrl Pts',(1.84983541599994,12.2,-10.460633126));
#160506=CARTESIAN_POINT('Ctrl Pts',(1.85069995999994,12.2,-10.462632262));
#160507=CARTESIAN_POINT('Ctrl Pts',(1.85156894599994,12.2,-10.464636786));
#160508=CARTESIAN_POINT('Ctrl Pts',(1.85244237799994,12.2,-10.46664668));
#160509=CARTESIAN_POINT('Ctrl Pts',(1.85332025899994,12.2,-10.468661929));
#160510=CARTESIAN_POINT('Ctrl Pts',(1.85420259499994,12.2,-10.470682514));
#160511=CARTESIAN_POINT('Ctrl Pts',(1.85508938999994,12.2,-10.47270842));
#160512=CARTESIAN_POINT('Ctrl Pts',(1.85598064599994,12.2,-10.474739628));
#160513=CARTESIAN_POINT('Ctrl Pts',(1.85687636999994,12.2,-10.476776123));
#160514=CARTESIAN_POINT('Ctrl Pts',(1.85777656499994,12.2,-10.478817888));
#160515=CARTESIAN_POINT('Ctrl Pts',(1.85868123399994,12.2,-10.480864906));
#160516=CARTESIAN_POINT('Ctrl Pts',(1.85959038199994,12.2,-10.48291716));
#160517=CARTESIAN_POINT('Ctrl Pts',(1.86050401199994,12.2,-10.484974634));
#160518=CARTESIAN_POINT('Ctrl Pts',(1.86142212899994,12.2,-10.487037312));
#160519=CARTESIAN_POINT('Ctrl Pts',(1.86234473699994,12.2,-10.489105177));
#160520=CARTESIAN_POINT('Ctrl Pts',(1.86327183899994,12.2,-10.491178213));
#160521=CARTESIAN_POINT('Ctrl Pts',(1.86420344099994,12.2,-10.493256403));
#160522=CARTESIAN_POINT('Ctrl Pts',(1.86513954299994,12.2,-10.49533973));
#160523=CARTESIAN_POINT('Ctrl Pts',(1.86608015299994,12.2,-10.497428179));
#160524=CARTESIAN_POINT('Ctrl Pts',(1.86702527199994,12.2,-10.499521733));
#160525=CARTESIAN_POINT('Ctrl Pts',(1.86797490499994,12.2,-10.501620377));
#160526=CARTESIAN_POINT('Ctrl Pts',(1.86892905699994,12.2,-10.503724094));
#160527=CARTESIAN_POINT('Ctrl Pts',(1.86988772999995,12.2,-10.505832868));
#160528=CARTESIAN_POINT('Ctrl Pts',(1.87085092699994,12.2,-10.507946683));
#160529=CARTESIAN_POINT('Ctrl Pts',(1.87181865399994,12.2,-10.510065522));
#160530=CARTESIAN_POINT('Ctrl Pts',(1.87279091299994,12.2,-10.512189371));
#160531=CARTESIAN_POINT('Ctrl Pts',(1.87376770899994,12.2,-10.514318212));
#160532=CARTESIAN_POINT('Ctrl Pts',(1.87474904299994,12.2,-10.516452031));
#160533=CARTESIAN_POINT('Ctrl Pts',(1.87573492299994,12.2,-10.518590811));
#160534=CARTESIAN_POINT('Ctrl Pts',(1.87672534799994,12.2,-10.520734536));
#160535=CARTESIAN_POINT('Ctrl Pts',(1.87772032499994,12.2,-10.522883192));
#160536=CARTESIAN_POINT('Ctrl Pts',(1.87871985699994,12.2,-10.525036762));
#160537=CARTESIAN_POINT('Ctrl Pts',(1.87972394599994,12.2,-10.52719523));
#160538=CARTESIAN_POINT('Ctrl Pts',(1.88073259699994,12.2,-10.529358581));
#160539=CARTESIAN_POINT('Ctrl Pts',(1.88174581199994,12.2,-10.531526798));
#160540=CARTESIAN_POINT('Ctrl Pts',(1.88276359599994,12.2,-10.533699869));
#160541=CARTESIAN_POINT('Ctrl Pts',(1.88378595299994,12.2,-10.535877775));
#160542=CARTESIAN_POINT('Ctrl Pts',(1.88481288399994,12.2,-10.538060503));
#160543=CARTESIAN_POINT('Ctrl Pts',(1.88584439399994,12.2,-10.540248035));
#160544=CARTESIAN_POINT('Ctrl Pts',(1.88688048599994,12.2,-10.542440358));
#160545=CARTESIAN_POINT('Ctrl Pts',(1.88792116399994,12.2,-10.544637455));
#160546=CARTESIAN_POINT('Ctrl Pts',(1.88896643099994,12.2,-10.546839313));
#160547=CARTESIAN_POINT('Ctrl Pts',(1.89001628999994,12.2,-10.549045913));
#160548=CARTESIAN_POINT('Ctrl Pts',(1.89107074499994,12.2,-10.551257244));
#160549=CARTESIAN_POINT('Ctrl Pts',(1.89212979899994,12.2,-10.553473288));
#160550=CARTESIAN_POINT('Ctrl Pts',(1.89319345499994,12.2,-10.555694032));
#160551=CARTESIAN_POINT('Ctrl Pts',(1.89426171599994,12.2,-10.557919458));
#160552=CARTESIAN_POINT('Ctrl Pts',(1.89533458699994,12.2,-10.560149554));
#160553=CARTESIAN_POINT('Ctrl Pts',(1.89641206899994,12.2,-10.562384303));
#160554=CARTESIAN_POINT('Ctrl Pts',(1.89749416599994,12.2,-10.564623691));
#160555=CARTESIAN_POINT('Ctrl Pts',(1.89858088099994,12.2,-10.566867703));
#160556=CARTESIAN_POINT('Ctrl Pts',(1.89967221899994,12.2,-10.569116324));
#160557=CARTESIAN_POINT('Ctrl Pts',(1.90076818099994,12.2,-10.571369539));
#160558=CARTESIAN_POINT('Ctrl Pts',(1.90186877099994,12.2,-10.573627333));
#160559=CARTESIAN_POINT('Ctrl Pts',(1.90297399099994,12.2,-10.575889692));
#160560=CARTESIAN_POINT('Ctrl Pts',(1.90408384599994,12.2,-10.578156601));
#160561=CARTESIAN_POINT('Ctrl Pts',(1.90519833799994,12.2,-10.580428044));
#160562=CARTESIAN_POINT('Ctrl Pts',(1.90631746999994,12.2,-10.582704009));
#160563=CARTESIAN_POINT('Ctrl Pts',(1.90744124499994,12.2,-10.584984479));
#160564=CARTESIAN_POINT('Ctrl Pts',(1.90856966599994,12.2,-10.587269441));
#160565=CARTESIAN_POINT('Ctrl Pts',(1.90970273699994,12.2,-10.58955888));
#160566=CARTESIAN_POINT('Ctrl Pts',(1.91084045999994,12.2,-10.59185278));
#160567=CARTESIAN_POINT('Ctrl Pts',(1.91198283799994,12.2,-10.594151129));
#160568=CARTESIAN_POINT('Ctrl Pts',(1.91312987399994,12.2,-10.59645391));
#160569=CARTESIAN_POINT('Ctrl Pts',(1.91428157099994,12.2,-10.598761112));
#160570=CARTESIAN_POINT('Ctrl Pts',(1.91543793199994,12.2,-10.601072717));
#160571=CARTESIAN_POINT('Ctrl Pts',(1.91659895999994,12.2,-10.603388714));
#160572=CARTESIAN_POINT('Ctrl Pts',(1.91776465699994,12.2,-10.605709085));
#160573=CARTESIAN_POINT('Ctrl Pts',(1.91893502699994,12.2,-10.60803382));
#160574=CARTESIAN_POINT('Ctrl Pts',(1.92011007299994,12.2,-10.610362901));
#160575=CARTESIAN_POINT('Ctrl Pts',(1.92128979599994,12.2,-10.612696316));
#160576=CARTESIAN_POINT('Ctrl Pts',(1.92247420099994,12.2,-10.615034051));
#160577=CARTESIAN_POINT('Ctrl Pts',(1.92366328999994,12.2,-10.617376091));
#160578=CARTESIAN_POINT('Ctrl Pts',(1.92485706499994,12.2,-10.619722422));
#160579=CARTESIAN_POINT('Ctrl Pts',(1.92605552899994,12.2,-10.622073029));
#160580=CARTESIAN_POINT('Ctrl Pts',(1.92725868499994,12.2,-10.6244279));
#160581=CARTESIAN_POINT('Ctrl Pts',(1.92846653599994,12.2,-10.62678702));
#160582=CARTESIAN_POINT('Ctrl Pts',(1.92967908399994,12.2,-10.629150376));
#160583=CARTESIAN_POINT('Ctrl Pts',(1.93089633299994,12.2,-10.631517953));
#160584=CARTESIAN_POINT('Ctrl Pts',(1.93211828499994,12.2,-10.633889738));
#160585=CARTESIAN_POINT('Ctrl Pts',(1.93334494199994,12.2,-10.636265715));
#160586=CARTESIAN_POINT('Ctrl Pts',(1.93457630699994,12.2,-10.638645874));
#160587=CARTESIAN_POINT('Ctrl Pts',(1.93581238299994,12.2,-10.641030197));
#160588=CARTESIAN_POINT('Ctrl Pts',(1.93705317299994,12.2,-10.643418674));
#160589=CARTESIAN_POINT('Ctrl Pts',(1.93829867699994,12.2,-10.645811289));
#160590=CARTESIAN_POINT('Ctrl Pts',(1.93954889999994,12.2,-10.648208029));
#160591=CARTESIAN_POINT('Ctrl Pts',(1.94080384499994,12.2,-10.650608881));
#160592=CARTESIAN_POINT('Ctrl Pts',(1.94206351299994,12.2,-10.65301383));
#160593=CARTESIAN_POINT('Ctrl Pts',(1.94332790699994,12.2,-10.655422864));
#160594=CARTESIAN_POINT('Ctrl Pts',(1.94459702899994,12.2,-10.657835968));
#160595=CARTESIAN_POINT('Ctrl Pts',(1.94587088199994,12.2,-10.660253129));
#160596=CARTESIAN_POINT('Ctrl Pts',(1.94714946899994,12.2,-10.662674334));
#160597=CARTESIAN_POINT('Ctrl Pts',(1.94843279199994,12.2,-10.665099571));
#160598=CARTESIAN_POINT('Ctrl Pts',(1.94972085299994,12.2,-10.667528823));
#160599=CARTESIAN_POINT('Ctrl Pts',(1.95101365499994,12.2,-10.66996208));
#160600=CARTESIAN_POINT('Ctrl Pts',(1.95231119999994,12.2,-10.672399326));
#160601=CARTESIAN_POINT('Ctrl Pts',(1.95361349099994,12.2,-10.674840549));
#160602=CARTESIAN_POINT('Ctrl Pts',(1.95492052999994,12.2,-10.677285737));
#160603=CARTESIAN_POINT('Ctrl Pts',(1.95623231799994,12.2,-10.679734874));
#160604=CARTESIAN_POINT('Ctrl Pts',(1.95754885999994,12.2,-10.682187948));
#160605=CARTESIAN_POINT('Ctrl Pts',(1.95887015699994,12.2,-10.684644947));
#160606=CARTESIAN_POINT('Ctrl Pts',(1.96019620999994,12.2,-10.687105856));
#160607=CARTESIAN_POINT('Ctrl Pts',(1.96152702299994,12.2,-10.689570664));
#160608=CARTESIAN_POINT('Ctrl Pts',(1.96286259899994,12.2,-10.692039356));
#160609=CARTESIAN_POINT('Ctrl Pts',(1.96420293799994,12.2,-10.694511919));
#160610=CARTESIAN_POINT('Ctrl Pts',(1.96554804399994,12.2,-10.696988341));
#160611=CARTESIAN_POINT('Ctrl Pts',(1.96689791799994,12.2,-10.699468609));
#160612=CARTESIAN_POINT('Ctrl Pts',(1.96825256199994,12.2,-10.70195271));
#160613=CARTESIAN_POINT('Ctrl Pts',(1.96961197999994,12.2,-10.704440629));
#160614=CARTESIAN_POINT('Ctrl Pts',(1.97097617299994,12.2,-10.706932355));
#160615=CARTESIAN_POINT('Ctrl Pts',(1.97234514399994,12.2,-10.709427876));
#160616=CARTESIAN_POINT('Ctrl Pts',(1.97371889299994,12.2,-10.711927177));
#160617=CARTESIAN_POINT('Ctrl Pts',(1.97509742499994,12.2,-10.714430247));
#160618=CARTESIAN_POINT('Ctrl Pts',(1.97648073999994,12.2,-10.716937073));
#160619=CARTESIAN_POINT('Ctrl Pts',(1.97786884099994,12.2,-10.71944764));
#160620=CARTESIAN_POINT('Ctrl Pts',(1.97926172999994,12.2,-10.721961937));
#160621=CARTESIAN_POINT('Ctrl Pts',(1.98065940899994,12.2,-10.724479952));
#160622=CARTESIAN_POINT('Ctrl Pts',(1.98206188099994,12.2,-10.727001672));
#160623=CARTESIAN_POINT('Ctrl Pts',(1.98346914499994,12.2,-10.729527083));
#160624=CARTESIAN_POINT('Ctrl Pts',(1.98488120699994,12.2,-10.732056173));
#160625=CARTESIAN_POINT('Ctrl Pts',(1.98629806699994,12.2,-10.73458893));
#160626=CARTESIAN_POINT('Ctrl Pts',(1.98771972699994,12.2,-10.737125341));
#160627=CARTESIAN_POINT('Ctrl Pts',(1.98914618999994,12.2,-10.739665394));
#160628=CARTESIAN_POINT('Ctrl Pts',(1.99057745699994,12.2,-10.742209076));
#160629=CARTESIAN_POINT('Ctrl Pts',(1.99201352899994,12.2,-10.744756374));
#160630=CARTESIAN_POINT('Ctrl Pts',(1.99345441099994,12.2,-10.747307276));
#160631=CARTESIAN_POINT('Ctrl Pts',(1.99490010199994,12.2,-10.74986177));
#160632=CARTESIAN_POINT('Ctrl Pts',(1.99635060499994,12.2,-10.752419844));
#160633=CARTESIAN_POINT('Ctrl Pts',(1.99780592199994,12.2,-10.754981484));
#160634=CARTESIAN_POINT('Ctrl Pts',(1.99926605499994,12.2,-10.757546678));
#160635=CARTESIAN_POINT('Ctrl Pts',(2.00073100599994,12.2,-10.760115415));
#160636=CARTESIAN_POINT('Ctrl Pts',(2.00220077599994,12.2,-10.762687682));
#160637=CARTESIAN_POINT('Ctrl Pts',(2.00367536799994,12.2,-10.765263466));
#160638=CARTESIAN_POINT('Ctrl Pts',(2.00515478199994,12.2,-10.767842756));
#160639=CARTESIAN_POINT('Ctrl Pts',(2.00663902299994,12.2,-10.77042554));
#160640=CARTESIAN_POINT('Ctrl Pts',(2.00812808999994,12.2,-10.773011803));
#160641=CARTESIAN_POINT('Ctrl Pts',(2.00962198599994,12.2,-10.775601537));
#160642=CARTESIAN_POINT('Ctrl Pts',(2.01112071299994,12.2,-10.778194727));
#160643=CARTESIAN_POINT('Ctrl Pts',(2.01262427099994,12.2,-10.780791361));
#160644=CARTESIAN_POINT('Ctrl Pts',(2.01413266399994,12.2,-10.783391428));
#160645=CARTESIAN_POINT('Ctrl Pts',(2.01564589299994,12.2,-10.785994916));
#160646=CARTESIAN_POINT('Ctrl Pts',(2.01716395899994,12.2,-10.788601812));
#160647=CARTESIAN_POINT('Ctrl Pts',(2.01868686499994,12.2,-10.791212104));
#160648=CARTESIAN_POINT('Ctrl Pts',(2.02021461099994,12.2,-10.793825781));
#160649=CARTESIAN_POINT('Ctrl Pts',(2.02174720099995,12.2,-10.796442831));
#160650=CARTESIAN_POINT('Ctrl Pts',(2.02328463399994,12.2,-10.799063241));
#160651=CARTESIAN_POINT('Ctrl Pts',(2.02482691399994,12.2,-10.801687));
#160652=CARTESIAN_POINT('Ctrl Pts',(2.02637404199994,12.2,-10.804314097));
#160653=CARTESIAN_POINT('Ctrl Pts',(2.02792601899994,12.2,-10.806944517));
#160654=CARTESIAN_POINT('Ctrl Pts',(2.02948284599994,12.2,-10.809578251));
#160655=CARTESIAN_POINT('Ctrl Pts',(2.03104452699994,12.2,-10.812215287));
#160656=CARTESIAN_POINT('Ctrl Pts',(2.03261106199994,12.2,-10.814855611));
#160657=CARTESIAN_POINT('Ctrl Pts',(2.03418245199994,12.2,-10.817499214));
#160658=CARTESIAN_POINT('Ctrl Pts',(2.03575870099994,12.2,-10.820146083));
#160659=CARTESIAN_POINT('Ctrl Pts',(2.03733980799994,12.2,-10.822796206));
#160660=CARTESIAN_POINT('Ctrl Pts',(2.03892577499994,12.2,-10.825449572));
#160661=CARTESIAN_POINT('Ctrl Pts',(2.04051660599994,12.2,-10.82810617));
#160662=CARTESIAN_POINT('Ctrl Pts',(2.04211229899994,12.2,-10.830765986));
#160663=CARTESIAN_POINT('Ctrl Pts',(2.04371285699994,12.2,-10.833429011));
#160664=CARTESIAN_POINT('Ctrl Pts',(2.04531828199995,12.2,-10.836095232));
#160665=CARTESIAN_POINT('Ctrl Pts',(2.04692857599994,12.2,-10.838764637));
#160666=CARTESIAN_POINT('Ctrl Pts',(2.04854373899995,12.2,-10.841437216));
#160667=CARTESIAN_POINT('Ctrl Pts',(2.05016377299994,12.2,-10.844112955));
#160668=CARTESIAN_POINT('Ctrl Pts',(2.05178868099994,12.2,-10.846791846));
#160669=CARTESIAN_POINT('Ctrl Pts',(2.05341846199994,12.2,-10.849473875));
#160670=CARTESIAN_POINT('Ctrl Pts',(2.05505311799994,12.2,-10.852159032));
#160671=CARTESIAN_POINT('Ctrl Pts',(2.05669265099994,12.2,-10.854847303));
#160672=CARTESIAN_POINT('Ctrl Pts',(2.05833706199994,12.2,-10.85753868));
#160673=CARTESIAN_POINT('Ctrl Pts',(2.05998635399994,12.2,-10.86023315));
#160674=CARTESIAN_POINT('Ctrl Pts',(2.06164052499994,12.2,-10.862930702));
#160675=CARTESIAN_POINT('Ctrl Pts',(2.06329958099994,12.2,-10.865631323));
#160676=CARTESIAN_POINT('Ctrl Pts',(2.06496351899994,12.2,-10.868335004));
#160677=CARTESIAN_POINT('Ctrl Pts',(2.06663234299994,12.2,-10.871041734));
#160678=CARTESIAN_POINT('Ctrl Pts',(2.06830605399994,12.2,-10.873751499));
#160679=CARTESIAN_POINT('Ctrl Pts',(2.06998465199994,12.2,-10.876464289));
#160680=CARTESIAN_POINT('Ctrl Pts',(2.07166813899994,12.2,-10.879180094));
#160681=CARTESIAN_POINT('Ctrl Pts',(2.07335651799994,12.2,-10.881898902));
#160682=CARTESIAN_POINT('Ctrl Pts',(2.07504978799994,12.2,-10.884620701));
#160683=CARTESIAN_POINT('Ctrl Pts',(2.07674794999994,12.2,-10.887345482));
#160684=CARTESIAN_POINT('Ctrl Pts',(2.07845100699994,12.2,-10.890073231));
#160685=CARTESIAN_POINT('Ctrl Pts',(2.08015896099994,12.2,-10.89280394));
#160686=CARTESIAN_POINT('Ctrl Pts',(2.08187181099994,12.2,-10.895537595));
#160687=CARTESIAN_POINT('Ctrl Pts',(2.08358955799994,12.2,-10.898274186));
#160688=CARTESIAN_POINT('Ctrl Pts',(2.08531220499994,12.2,-10.901013703));
#160689=CARTESIAN_POINT('Ctrl Pts',(2.08703975299994,12.2,-10.903756135));
#160690=CARTESIAN_POINT('Ctrl Pts',(2.08877220299994,12.2,-10.906501469));
#160691=CARTESIAN_POINT('Ctrl Pts',(2.09050955499994,12.2,-10.909249695));
#160692=CARTESIAN_POINT('Ctrl Pts',(2.09225181099994,12.2,-10.912000804));
#160693=CARTESIAN_POINT('Ctrl Pts',(2.09399897299994,12.2,-10.914754782));
#160694=CARTESIAN_POINT('Ctrl Pts',(2.09575104199994,12.2,-10.91751162));
#160695=CARTESIAN_POINT('Ctrl Pts',(2.09750801799994,12.2,-10.920271306));
#160696=CARTESIAN_POINT('Ctrl Pts',(2.09926990199994,12.2,-10.92303383));
#160697=CARTESIAN_POINT('Ctrl Pts',(2.10103669699994,12.2,-10.925799182));
#160698=CARTESIAN_POINT('Ctrl Pts',(2.10280840299994,12.2,-10.928567349));
#160699=CARTESIAN_POINT('Ctrl Pts',(2.10458501999994,12.2,-10.931338321));
#160700=CARTESIAN_POINT('Ctrl Pts',(2.10636655199994,12.2,-10.934112088));
#160701=CARTESIAN_POINT('Ctrl Pts',(2.10815299699994,12.2,-10.936888638));
#160702=CARTESIAN_POINT('Ctrl Pts',(2.10994435799994,12.2,-10.939667962));
#160703=CARTESIAN_POINT('Ctrl Pts',(2.11174063499994,12.2,-10.942450048));
#160704=CARTESIAN_POINT('Ctrl Pts',(2.11354182899994,12.2,-10.945234885));
#160705=CARTESIAN_POINT('Ctrl Pts',(2.11534794299994,12.2,-10.948022463));
#160706=CARTESIAN_POINT('Ctrl Pts',(2.11715897499994,12.2,-10.950812772));
#160707=CARTESIAN_POINT('Ctrl Pts',(2.11897492799995,12.2,-10.953605801));
#160708=CARTESIAN_POINT('Ctrl Pts',(2.12079580299994,12.2,-10.956401537));
#160709=CARTESIAN_POINT('Ctrl Pts',(2.12262159999994,12.2,-10.959199973));
#160710=CARTESIAN_POINT('Ctrl Pts',(2.12445232199994,12.2,-10.962001096));
#160711=CARTESIAN_POINT('Ctrl Pts',(2.12628796699994,12.2,-10.964804897));
#160712=CARTESIAN_POINT('Ctrl Pts',(2.12812853899994,12.2,-10.967611364));
#160713=CARTESIAN_POINT('Ctrl Pts',(2.12997403599994,12.2,-10.970420488));
#160714=CARTESIAN_POINT('Ctrl Pts',(2.13182446099994,12.2,-10.973232257));
#160715=CARTESIAN_POINT('Ctrl Pts',(2.13367981499994,12.2,-10.976046662));
#160716=CARTESIAN_POINT('Ctrl Pts',(2.13554009799994,12.2,-10.978863691));
#160717=CARTESIAN_POINT('Ctrl Pts',(2.13740531099994,12.2,-10.981683335));
#160718=CARTESIAN_POINT('Ctrl Pts',(2.13927545499994,12.2,-10.984505583));
#160719=CARTESIAN_POINT('Ctrl Pts',(2.14115053099994,12.2,-10.987330423));
#160720=CARTESIAN_POINT('Ctrl Pts',(2.14303053999994,12.2,-10.990157848));
#160721=CARTESIAN_POINT('Ctrl Pts',(2.14491548299994,12.2,-10.992987845));
#160722=CARTESIAN_POINT('Ctrl Pts',(2.14680536099995,12.2,-10.995820404));
#160723=CARTESIAN_POINT('Ctrl Pts',(2.14870017399994,12.2,-10.998655516));
#160724=CARTESIAN_POINT('Ctrl Pts',(2.15059992399994,12.2,-11.00149317));
#160725=CARTESIAN_POINT('Ctrl Pts',(2.15250460999994,12.2,-11.004333355));
#160726=CARTESIAN_POINT('Ctrl Pts',(2.15441423499994,12.2,-11.007176061));
#160727=CARTESIAN_POINT('Ctrl Pts',(2.15632879899994,12.2,-11.010021278));
#160728=CARTESIAN_POINT('Ctrl Pts',(2.15824830199994,12.2,-11.012868997));
#160729=CARTESIAN_POINT('Ctrl Pts',(2.16017274599994,12.2,-11.015719205));
#160730=CARTESIAN_POINT('Ctrl Pts',(2.16210213199994,12.2,-11.018571894));
#160731=CARTESIAN_POINT('Ctrl Pts',(2.16403645899994,12.2,-11.021427054));
#160732=CARTESIAN_POINT('Ctrl Pts',(2.16597572899994,12.2,-11.024284674));
#160733=CARTESIAN_POINT('Ctrl Pts',(2.16791994199994,12.2,-11.027144743));
#160734=CARTESIAN_POINT('Ctrl Pts',(2.16986909999994,12.2,-11.030007252));
#160735=CARTESIAN_POINT('Ctrl Pts',(2.17182320399994,12.2,-11.032872191));
#160736=CARTESIAN_POINT('Ctrl Pts',(2.17378225199994,12.2,-11.03573955));
#160737=CARTESIAN_POINT('Ctrl Pts',(2.17574624699994,12.2,-11.038609318));
#160738=CARTESIAN_POINT('Ctrl Pts',(2.17771518999994,12.2,-11.041481486));
#160739=CARTESIAN_POINT('Ctrl Pts',(2.17968908099994,12.2,-11.044356044));
#160740=CARTESIAN_POINT('Ctrl Pts',(2.18166791999994,12.2,-11.047232981));
#160741=CARTESIAN_POINT('Ctrl Pts',(2.18365170899994,12.2,-11.050112287));
#160742=CARTESIAN_POINT('Ctrl Pts',(2.18564044699994,12.2,-11.052993953));
#160743=CARTESIAN_POINT('Ctrl Pts',(2.18763413599994,12.2,-11.055877969));
#160744=CARTESIAN_POINT('Ctrl Pts',(2.18963277699994,12.2,-11.058764325));
#160745=CARTESIAN_POINT('Ctrl Pts',(2.19163636999994,12.2,-11.06165301));
#160746=CARTESIAN_POINT('Ctrl Pts',(2.19364491499995,12.2,-11.064544015));
#160747=CARTESIAN_POINT('Ctrl Pts',(2.19565841299994,12.2,-11.067437331));
#160748=CARTESIAN_POINT('Ctrl Pts',(2.19767686499994,12.2,-11.070332945));
#160749=CARTESIAN_POINT('Ctrl Pts',(2.19970027199994,12.2,-11.073230851));
#160750=CARTESIAN_POINT('Ctrl Pts',(2.20172863299994,12.2,-11.076131037));
#160751=CARTESIAN_POINT('Ctrl Pts',(2.20376195099994,12.2,-11.079033493));
#160752=CARTESIAN_POINT('Ctrl Pts',(2.20580022499994,12.2,-11.081938212));
#160753=CARTESIAN_POINT('Ctrl Pts',(2.20784345599994,12.2,-11.08484518));
#160754=CARTESIAN_POINT('Ctrl Pts',(2.20989164299994,12.2,-11.08775439));
#160755=CARTESIAN_POINT('Ctrl Pts',(2.21194478899994,12.2,-11.090665832));
#160756=CARTESIAN_POINT('Ctrl Pts',(2.21400289399994,12.2,-11.093579495));
#160757=CARTESIAN_POINT('Ctrl Pts',(2.21606595699994,12.2,-11.096495371));
#160758=CARTESIAN_POINT('Ctrl Pts',(2.21813398099994,12.2,-11.099413448));
#160759=CARTESIAN_POINT('Ctrl Pts',(2.22020696299994,12.2,-11.10233372));
#160760=CARTESIAN_POINT('Ctrl Pts',(2.22228490799994,12.2,-11.105256173));
#160761=CARTESIAN_POINT('Ctrl Pts',(2.22436781299994,12.2,-11.1081808));
#160762=CARTESIAN_POINT('Ctrl Pts',(2.22645567899994,12.2,-11.111107592));
#160763=CARTESIAN_POINT('Ctrl Pts',(2.22854850699994,12.2,-11.114036538));
#160764=CARTESIAN_POINT('Ctrl Pts',(2.23064629799994,12.2,-11.116967627));
#160765=CARTESIAN_POINT('Ctrl Pts',(2.23274905199994,12.2,-11.119900853));
#160766=CARTESIAN_POINT('Ctrl Pts',(2.23485676999994,12.2,-11.122836204));
#160767=CARTESIAN_POINT('Ctrl Pts',(2.23696945199995,12.2,-11.125773671));
#160768=CARTESIAN_POINT('Ctrl Pts',(2.23908709799994,12.2,-11.128713243));
#160769=CARTESIAN_POINT('Ctrl Pts',(2.24120970899994,12.2,-11.131654914));
#160770=CARTESIAN_POINT('Ctrl Pts',(2.24333728499994,12.2,-11.134598671));
#160771=CARTESIAN_POINT('Ctrl Pts',(2.24546982699994,12.2,-11.137544507));
#160772=CARTESIAN_POINT('Ctrl Pts',(2.24760733499994,12.2,-11.140492411));
#160773=CARTESIAN_POINT('Ctrl Pts',(2.24974980999994,12.2,-11.143442374));
#160774=CARTESIAN_POINT('Ctrl Pts',(2.25189725099994,12.2,-11.146394387));
#160775=CARTESIAN_POINT('Ctrl Pts',(2.25404965899994,12.2,-11.14934844));
#160776=CARTESIAN_POINT('Ctrl Pts',(2.25620703599994,12.2,-11.152304524));
#160777=CARTESIAN_POINT('Ctrl Pts',(2.25836937999994,12.2,-11.15526263));
#160778=CARTESIAN_POINT('Ctrl Pts',(2.26053669299994,12.2,-11.158222747));
#160779=CARTESIAN_POINT('Ctrl Pts',(2.26270897299994,12.2,-11.161184868));
#160780=CARTESIAN_POINT('Ctrl Pts',(2.26488622499994,12.2,-11.164148983));
#160781=CARTESIAN_POINT('Ctrl Pts',(2.26706844499994,12.2,-11.16711508));
#160782=CARTESIAN_POINT('Ctrl Pts',(2.26925563399994,12.2,-11.170083153));
#160783=CARTESIAN_POINT('Ctrl Pts',(2.27144779299994,12.2,-11.173053191));
#160784=CARTESIAN_POINT('Ctrl Pts',(2.27364492299994,12.2,-11.176025185));
#160785=CARTESIAN_POINT('Ctrl Pts',(2.27584702399994,12.2,-11.178999126));
#160786=CARTESIAN_POINT('Ctrl Pts',(2.27805409499994,12.2,-11.181975005));
#160787=CARTESIAN_POINT('Ctrl Pts',(2.28026613799994,12.2,-11.184952813));
#160788=CARTESIAN_POINT('Ctrl Pts',(2.28248315299994,12.2,-11.187932541));
#160789=CARTESIAN_POINT('Ctrl Pts',(2.28470513799994,12.2,-11.190914179));
#160790=CARTESIAN_POINT('Ctrl Pts',(2.28693209699994,12.2,-11.193897718));
#160791=CARTESIAN_POINT('Ctrl Pts',(2.28916402699994,12.2,-11.19688315));
#160792=CARTESIAN_POINT('Ctrl Pts',(2.29140092999994,12.2,-11.199870463));
#160793=CARTESIAN_POINT('Ctrl Pts',(2.29364280599994,12.2,-11.202859649));
#160794=CARTESIAN_POINT('Ctrl Pts',(2.29588965499994,12.2,-11.205850698));
#160795=CARTESIAN_POINT('Ctrl Pts',(2.29814147699994,12.2,-11.208843602));
#160796=CARTESIAN_POINT('Ctrl Pts',(2.30039827299994,12.2,-11.211838352));
#160797=CARTESIAN_POINT('Ctrl Pts',(2.30266004099994,12.2,-11.214834939));
#160798=CARTESIAN_POINT('Ctrl Pts',(2.30492678499994,12.2,-11.217833355));
#160799=CARTESIAN_POINT('Ctrl Pts',(2.30719850199994,12.2,-11.220833593));
#160800=CARTESIAN_POINT('Ctrl Pts',(2.30947519299994,12.2,-11.223835644));
#160801=CARTESIAN_POINT('Ctrl Pts',(2.31175685799994,12.2,-11.226839497));
#160802=CARTESIAN_POINT('Ctrl Pts',(2.31404349799994,12.2,-11.229845144));
#160803=CARTESIAN_POINT('Ctrl Pts',(2.31633511299994,12.2,-11.232852572));
#160804=CARTESIAN_POINT('Ctrl Pts',(2.31863170299994,12.2,-11.235861771));
#160805=CARTESIAN_POINT('Ctrl Pts',(2.32093326799994,12.2,-11.238872729));
#160806=CARTESIAN_POINT('Ctrl Pts',(2.32323980899994,12.2,-11.241885437));
#160807=CARTESIAN_POINT('Ctrl Pts',(2.32555132399995,12.2,-11.244899887));
#160808=CARTESIAN_POINT('Ctrl Pts',(2.32786781499994,12.2,-11.247916073));
#160809=CARTESIAN_POINT('Ctrl Pts',(2.33018928299995,12.2,-11.250933991));
#160810=CARTESIAN_POINT('Ctrl Pts',(2.33251572399995,12.2,-11.253953638));
#160811=CARTESIAN_POINT('Ctrl Pts',(2.33438085799994,12.2,-11.256370739));
#160812=CARTESIAN_POINT('Ctrl Pts',(2.33578194799994,12.2,-11.258184341));
#160813=CARTESIAN_POINT('Ctrl Pts',(2.33671700199995,12.2,-11.259393754));
#160814=CARTESIAN_POINT('Ctrl Pts',(2.33718477799994,12.2,-11.259998548));
#160815=CARTESIAN_POINT('Origin',(-5.66257110645729E-14,15.2,-1.77635683940025E-14));
#160816=CARTESIAN_POINT('',(3.20199116203656,15.2,-9.8685296574462));
#160817=CARTESIAN_POINT('',(3.20199116203656,12.2,-9.8685296574462));
#160818=CARTESIAN_POINT('',(3.20199116199994,15.2,-9.86852965700001));
#160819=CARTESIAN_POINT('Origin',(-5.66257110645729E-14,12.2,-1.77635683940025E-14));
#160820=CARTESIAN_POINT('Origin',(-5.66257110645729E-14,15.2,-1.77635683940025E-14));
#160821=CARTESIAN_POINT('Origin',(-5.66257110645729E-14,15.2,-1.77635683940025E-14));
#160822=CARTESIAN_POINT('',(3.91586047899994,15.2,-10.812771925));
#160823=CARTESIAN_POINT('',(4.27433546799994,15.2,-10.676144262));
#160824=CARTESIAN_POINT('Origin',(-5.66257110645729E-14,15.2,-1.77635683940025E-14));
#160825=CARTESIAN_POINT('',(4.27433546799994,12.2,-10.676144262));
#160826=CARTESIAN_POINT('',(4.27433546799994,15.2,-10.676144262));
#160827=CARTESIAN_POINT('',(3.91586047899994,12.2,-10.812771925));
#160828=CARTESIAN_POINT('Origin',(-5.66257110645729E-14,12.2,-1.77635683940025E-14));
#160829=CARTESIAN_POINT('',(3.91586047899994,15.2,-10.812771925));
#160830=CARTESIAN_POINT('Ctrl Pts',(3.20199116199994,15.2,-9.86852965800001));
#160831=CARTESIAN_POINT('Ctrl Pts',(3.20199116199994,11.6,-9.86852965800001));
#160832=CARTESIAN_POINT('Ctrl Pts',(3.20205902599994,15.2,-9.86869026600001));
#160833=CARTESIAN_POINT('Ctrl Pts',(3.20205902599994,11.6,-9.86869026600001));
#160834=CARTESIAN_POINT('Ctrl Pts',(3.20219720499994,15.2,-9.86901706000001));
#160835=CARTESIAN_POINT('Ctrl Pts',(3.20219720499994,11.6,-9.86901706000001));
#160836=CARTESIAN_POINT('Ctrl Pts',(3.20240682399994,15.2,-9.86951212500001));
#160837=CARTESIAN_POINT('Ctrl Pts',(3.20240682399994,11.6,-9.86951212500001));
#160838=CARTESIAN_POINT('Ctrl Pts',(3.20268969699995,15.2,-9.87017881300001));
#160839=CARTESIAN_POINT('Ctrl Pts',(3.20268969699995,11.6,-9.87017881300001));
#160840=CARTESIAN_POINT('Ctrl Pts',(3.20304832999994,15.2,-9.87102171600001));
#160841=CARTESIAN_POINT('Ctrl Pts',(3.20304832999994,11.6,-9.87102171600001));
#160842=CARTESIAN_POINT('Ctrl Pts',(3.20341363499994,15.2,-9.87187791600001));
#160843=CARTESIAN_POINT('Ctrl Pts',(3.20341363499994,11.6,-9.87187791600001));
#160844=CARTESIAN_POINT('Ctrl Pts',(3.20378354199994,15.2,-9.87274249600001));
#160845=CARTESIAN_POINT('Ctrl Pts',(3.20378354199994,11.6,-9.87274249600001));
#160846=CARTESIAN_POINT('Ctrl Pts',(3.20415805699994,15.2,-9.87361542400001));
#160847=CARTESIAN_POINT('Ctrl Pts',(3.20415805699994,11.6,-9.87361542400001));
#160848=CARTESIAN_POINT('Ctrl Pts',(3.20453718399994,15.2,-9.87449667000002));
#160849=CARTESIAN_POINT('Ctrl Pts',(3.20453718399994,11.6,-9.87449667000002));
#160850=CARTESIAN_POINT('Ctrl Pts',(3.20492092999995,15.2,-9.87538620000001));
#160851=CARTESIAN_POINT('Ctrl Pts',(3.20492092999995,11.6,-9.87538620000001));
#160852=CARTESIAN_POINT('Ctrl Pts',(3.20530930299994,15.2,-9.87628398500001));
#160853=CARTESIAN_POINT('Ctrl Pts',(3.20530930299994,11.6,-9.87628398500001));
#160854=CARTESIAN_POINT('Ctrl Pts',(3.20570230499994,15.2,-9.87718999100001));
#160855=CARTESIAN_POINT('Ctrl Pts',(3.20570230499994,11.6,-9.87718999100001));
#160856=CARTESIAN_POINT('Ctrl Pts',(3.20609994399994,15.2,-9.87810418800001));
#160857=CARTESIAN_POINT('Ctrl Pts',(3.20609994399994,11.6,-9.87810418800001));
#160858=CARTESIAN_POINT('Ctrl Pts',(3.20650222799994,15.2,-9.87902654500001));
#160859=CARTESIAN_POINT('Ctrl Pts',(3.20650222799994,11.6,-9.87902654500001));
#160860=CARTESIAN_POINT('Ctrl Pts',(3.20690915899994,15.2,-9.87995703200001));
#160861=CARTESIAN_POINT('Ctrl Pts',(3.20690915899994,11.6,-9.87995703200001));
#160862=CARTESIAN_POINT('Ctrl Pts',(3.20732074299994,15.2,-9.88089561700001));
#160863=CARTESIAN_POINT('Ctrl Pts',(3.20732074299994,11.6,-9.88089561700001));
#160864=CARTESIAN_POINT('Ctrl Pts',(3.20773698899994,15.2,-9.88184227000001));
#160865=CARTESIAN_POINT('Ctrl Pts',(3.20773698899994,11.6,-9.88184227000001));
#160866=CARTESIAN_POINT('Ctrl Pts',(3.20815789999994,15.2,-9.88279696000001));
#160867=CARTESIAN_POINT('Ctrl Pts',(3.20815789999994,11.6,-9.88279696000001));
#160868=CARTESIAN_POINT('Ctrl Pts',(3.20858348199994,15.2,-9.88375965700001));
#160869=CARTESIAN_POINT('Ctrl Pts',(3.20858348199994,11.6,-9.88375965700001));
#160870=CARTESIAN_POINT('Ctrl Pts',(3.20901374099994,15.2,-9.88473033000002));
#160871=CARTESIAN_POINT('Ctrl Pts',(3.20901374099994,11.6,-9.88473033000002));
#160872=CARTESIAN_POINT('Ctrl Pts',(3.20944868199994,15.2,-9.88570895100001));
#160873=CARTESIAN_POINT('Ctrl Pts',(3.20944868199994,11.6,-9.88570895100001));
#160874=CARTESIAN_POINT('Ctrl Pts',(3.20988831099994,15.2,-9.88669548800001));
#160875=CARTESIAN_POINT('Ctrl Pts',(3.20988831099994,11.6,-9.88669548800001));
#160876=CARTESIAN_POINT('Ctrl Pts',(3.21033263399995,15.2,-9.88768991300001));
#160877=CARTESIAN_POINT('Ctrl Pts',(3.21033263399995,11.6,-9.88768991300001));
#160878=CARTESIAN_POINT('Ctrl Pts',(3.21078165499994,15.2,-9.88869219500001));
#160879=CARTESIAN_POINT('Ctrl Pts',(3.21078165499994,11.6,-9.88869219500001));
#160880=CARTESIAN_POINT('Ctrl Pts',(3.21123537899994,15.2,-9.88970230500001));
#160881=CARTESIAN_POINT('Ctrl Pts',(3.21123537899994,11.6,-9.88970230500001));
#160882=CARTESIAN_POINT('Ctrl Pts',(3.21169381299995,15.2,-9.89072021500001));
#160883=CARTESIAN_POINT('Ctrl Pts',(3.21169381299995,11.6,-9.89072021500001));
#160884=CARTESIAN_POINT('Ctrl Pts',(3.21215696199994,15.2,-9.89174589300001));
#160885=CARTESIAN_POINT('Ctrl Pts',(3.21215696199994,11.6,-9.89174589300001));
#160886=CARTESIAN_POINT('Ctrl Pts',(3.21262482999995,15.2,-9.89277931200001));
#160887=CARTESIAN_POINT('Ctrl Pts',(3.21262482999995,11.6,-9.89277931200001));
#160888=CARTESIAN_POINT('Ctrl Pts',(3.21309742399994,15.2,-9.89382044200001));
#160889=CARTESIAN_POINT('Ctrl Pts',(3.21309742399994,11.6,-9.89382044200001));
#160890=CARTESIAN_POINT('Ctrl Pts',(3.21357474799994,15.2,-9.89486925600001));
#160891=CARTESIAN_POINT('Ctrl Pts',(3.21357474799994,11.6,-9.89486925600001));
#160892=CARTESIAN_POINT('Ctrl Pts',(3.21405680799994,15.2,-9.89592572400001));
#160893=CARTESIAN_POINT('Ctrl Pts',(3.21405680799994,11.6,-9.89592572400001));
#160894=CARTESIAN_POINT('Ctrl Pts',(3.21454360799994,15.2,-9.89698981600001));
#160895=CARTESIAN_POINT('Ctrl Pts',(3.21454360799994,11.6,-9.89698981600001));
#160896=CARTESIAN_POINT('Ctrl Pts',(3.21503515299994,15.2,-9.89806150600001));
#160897=CARTESIAN_POINT('Ctrl Pts',(3.21503515299994,11.6,-9.89806150600001));
#160898=CARTESIAN_POINT('Ctrl Pts',(3.21553144899994,15.2,-9.89914076600001));
#160899=CARTESIAN_POINT('Ctrl Pts',(3.21553144899994,11.6,-9.89914076600001));
#160900=CARTESIAN_POINT('Ctrl Pts',(3.21603250099994,15.2,-9.90022756600001));
#160901=CARTESIAN_POINT('Ctrl Pts',(3.21603250099994,11.6,-9.90022756600001));
#160902=CARTESIAN_POINT('Ctrl Pts',(3.21653831299994,15.2,-9.90132187800001));
#160903=CARTESIAN_POINT('Ctrl Pts',(3.21653831299994,11.6,-9.90132187800001));
#160904=CARTESIAN_POINT('Ctrl Pts',(3.21704888999994,15.2,-9.90242367500001));
#160905=CARTESIAN_POINT('Ctrl Pts',(3.21704888999994,11.6,-9.90242367500001));
#160906=CARTESIAN_POINT('Ctrl Pts',(3.21756423699994,15.2,-9.90353292900001));
#160907=CARTESIAN_POINT('Ctrl Pts',(3.21756423699994,11.6,-9.90353292900001));
#160908=CARTESIAN_POINT('Ctrl Pts',(3.21808435999994,15.2,-9.90464961300001));
#160909=CARTESIAN_POINT('Ctrl Pts',(3.21808435999994,11.6,-9.90464961300001));
#160910=CARTESIAN_POINT('Ctrl Pts',(3.21860926299995,15.2,-9.90577369800001));
#160911=CARTESIAN_POINT('Ctrl Pts',(3.21860926299995,11.6,-9.90577369800001));
#160912=CARTESIAN_POINT('Ctrl Pts',(3.21913895099994,15.2,-9.90690515700001));
#160913=CARTESIAN_POINT('Ctrl Pts',(3.21913895099994,11.6,-9.90690515700001));
#160914=CARTESIAN_POINT('Ctrl Pts',(3.21967342799995,15.2,-9.90804396500001));
#160915=CARTESIAN_POINT('Ctrl Pts',(3.21967342799995,11.6,-9.90804396500001));
#160916=CARTESIAN_POINT('Ctrl Pts',(3.22021269999994,15.2,-9.90919009100001));
#160917=CARTESIAN_POINT('Ctrl Pts',(3.22021269999994,11.6,-9.90919009100001));
#160918=CARTESIAN_POINT('Ctrl Pts',(3.22075676999994,15.2,-9.91034351100001));
#160919=CARTESIAN_POINT('Ctrl Pts',(3.22075676999994,11.6,-9.91034351100001));
#160920=CARTESIAN_POINT('Ctrl Pts',(3.22130564299994,15.2,-9.91150419600001));
#160921=CARTESIAN_POINT('Ctrl Pts',(3.22130564299994,11.6,-9.91150419600001));
#160922=CARTESIAN_POINT('Ctrl Pts',(3.22185932499994,15.2,-9.91267212100001));
#160923=CARTESIAN_POINT('Ctrl Pts',(3.22185932499994,11.6,-9.91267212100001));
#160924=CARTESIAN_POINT('Ctrl Pts',(3.22241781899994,15.2,-9.91384725700001));
#160925=CARTESIAN_POINT('Ctrl Pts',(3.22241781899994,11.6,-9.91384725700001));
#160926=CARTESIAN_POINT('Ctrl Pts',(3.22298112999994,15.2,-9.91502958000001));
#160927=CARTESIAN_POINT('Ctrl Pts',(3.22298112999994,11.6,-9.91502958000001));
#160928=CARTESIAN_POINT('Ctrl Pts',(3.22354926399994,15.2,-9.91621906300001));
#160929=CARTESIAN_POINT('Ctrl Pts',(3.22354926399994,11.6,-9.91621906300001));
#160930=CARTESIAN_POINT('Ctrl Pts',(3.22412222299994,15.2,-9.91741567800001));
#160931=CARTESIAN_POINT('Ctrl Pts',(3.22412222299994,11.6,-9.91741567800001));
#160932=CARTESIAN_POINT('Ctrl Pts',(3.22470001299994,15.2,-9.91861939900001));
#160933=CARTESIAN_POINT('Ctrl Pts',(3.22470001299994,11.6,-9.91861939900001));
#160934=CARTESIAN_POINT('Ctrl Pts',(3.22528263699994,15.2,-9.91983020100001));
#160935=CARTESIAN_POINT('Ctrl Pts',(3.22528263699994,11.6,-9.91983020100001));
#160936=CARTESIAN_POINT('Ctrl Pts',(3.22587010199994,15.2,-9.92104805800001));
#160937=CARTESIAN_POINT('Ctrl Pts',(3.22587010199994,11.6,-9.92104805800001));
#160938=CARTESIAN_POINT('Ctrl Pts',(3.22646240999994,15.2,-9.92227294400001));
#160939=CARTESIAN_POINT('Ctrl Pts',(3.22646240999994,11.6,-9.92227294400001));
#160940=CARTESIAN_POINT('Ctrl Pts',(3.22705956599994,15.2,-9.92350483200001));
#160941=CARTESIAN_POINT('Ctrl Pts',(3.22705956599994,11.6,-9.92350483200001));
#160942=CARTESIAN_POINT('Ctrl Pts',(3.22766157399994,15.2,-9.92474369700002));
#160943=CARTESIAN_POINT('Ctrl Pts',(3.22766157399994,11.6,-9.92474369700002));
#160944=CARTESIAN_POINT('Ctrl Pts',(3.22826843899994,15.2,-9.92598951400001));
#160945=CARTESIAN_POINT('Ctrl Pts',(3.22826843899994,11.6,-9.92598951400001));
#160946=CARTESIAN_POINT('Ctrl Pts',(3.22888016499994,15.2,-9.92724225700002));
#160947=CARTESIAN_POINT('Ctrl Pts',(3.22888016499994,11.6,-9.92724225700002));
#160948=CARTESIAN_POINT('Ctrl Pts',(3.22949675499994,15.2,-9.92850190100001));
#160949=CARTESIAN_POINT('Ctrl Pts',(3.22949675499994,11.6,-9.92850190100001));
#160950=CARTESIAN_POINT('Ctrl Pts',(3.23011821499994,15.2,-9.92976841900001));
#160951=CARTESIAN_POINT('Ctrl Pts',(3.23011821499994,11.6,-9.92976841900001));
#160952=CARTESIAN_POINT('Ctrl Pts',(3.23074454799994,15.2,-9.93104178700001));
#160953=CARTESIAN_POINT('Ctrl Pts',(3.23074454799994,11.6,-9.93104178700001));
#160954=CARTESIAN_POINT('Ctrl Pts',(3.23137575799994,15.2,-9.93232198200001));
#160955=CARTESIAN_POINT('Ctrl Pts',(3.23137575799994,11.6,-9.93232198200001));
#160956=CARTESIAN_POINT('Ctrl Pts',(3.23201184999995,15.2,-9.93360897500001));
#160957=CARTESIAN_POINT('Ctrl Pts',(3.23201184999995,11.6,-9.93360897500001));
#160958=CARTESIAN_POINT('Ctrl Pts',(3.23265282699994,15.2,-9.93490274500001));
#160959=CARTESIAN_POINT('Ctrl Pts',(3.23265282699994,11.6,-9.93490274500001));
#160960=CARTESIAN_POINT('Ctrl Pts',(3.23329869199994,15.2,-9.93620326500001));
#160961=CARTESIAN_POINT('Ctrl Pts',(3.23329869199994,11.6,-9.93620326500001));
#160962=CARTESIAN_POINT('Ctrl Pts',(3.23394945199994,15.2,-9.93751051000001));
#160963=CARTESIAN_POINT('Ctrl Pts',(3.23394945199994,11.6,-9.93751051000001));
#160964=CARTESIAN_POINT('Ctrl Pts',(3.23460510899995,15.2,-9.93882445600001));
#160965=CARTESIAN_POINT('Ctrl Pts',(3.23460510899995,11.6,-9.93882445600001));
#160966=CARTESIAN_POINT('Ctrl Pts',(3.23526566599994,15.2,-9.94014508000001));
#160967=CARTESIAN_POINT('Ctrl Pts',(3.23526566599994,11.6,-9.94014508000001));
#160968=CARTESIAN_POINT('Ctrl Pts',(3.23593112999994,15.2,-9.94147235600001));
#160969=CARTESIAN_POINT('Ctrl Pts',(3.23593112999994,11.6,-9.94147235600001));
#160970=CARTESIAN_POINT('Ctrl Pts',(3.23660150199995,15.2,-9.94280625900001));
#160971=CARTESIAN_POINT('Ctrl Pts',(3.23660150199995,11.6,-9.94280625900001));
#160972=CARTESIAN_POINT('Ctrl Pts',(3.23727678699994,15.2,-9.94414676800002));
#160973=CARTESIAN_POINT('Ctrl Pts',(3.23727678699994,11.6,-9.94414676800002));
#160974=CARTESIAN_POINT('Ctrl Pts',(3.23795698799994,15.2,-9.94549385500001));
#160975=CARTESIAN_POINT('Ctrl Pts',(3.23795698799994,11.6,-9.94549385500001));
#160976=CARTESIAN_POINT('Ctrl Pts',(3.23864210899994,15.2,-9.94684749900001));
#160977=CARTESIAN_POINT('Ctrl Pts',(3.23864210899994,11.6,-9.94684749900001));
#160978=CARTESIAN_POINT('Ctrl Pts',(3.23933215499994,15.2,-9.94820767400001));
#160979=CARTESIAN_POINT('Ctrl Pts',(3.23933215499994,11.6,-9.94820767400001));
#160980=CARTESIAN_POINT('Ctrl Pts',(3.24002712899994,15.2,-9.94957435800002));
#160981=CARTESIAN_POINT('Ctrl Pts',(3.24002712899994,11.6,-9.94957435800002));
#160982=CARTESIAN_POINT('Ctrl Pts',(3.24072703299994,15.2,-9.95094752600002));
#160983=CARTESIAN_POINT('Ctrl Pts',(3.24072703299994,11.6,-9.95094752600002));
#160984=CARTESIAN_POINT('Ctrl Pts',(3.24143187299994,15.2,-9.95232715500001));
#160985=CARTESIAN_POINT('Ctrl Pts',(3.24143187299994,11.6,-9.95232715500001));
#160986=CARTESIAN_POINT('Ctrl Pts',(3.24214165199994,15.2,-9.95371322200001));
#160987=CARTESIAN_POINT('Ctrl Pts',(3.24214165199994,11.6,-9.95371322200001));
#160988=CARTESIAN_POINT('Ctrl Pts',(3.24285637299994,15.2,-9.95510570200001));
#160989=CARTESIAN_POINT('Ctrl Pts',(3.24285637299994,11.6,-9.95510570200001));
#160990=CARTESIAN_POINT('Ctrl Pts',(3.24357603899994,15.2,-9.95650457300002));
#160991=CARTESIAN_POINT('Ctrl Pts',(3.24357603899994,11.6,-9.95650457300002));
#160992=CARTESIAN_POINT('Ctrl Pts',(3.24430065599994,15.2,-9.95790981100001));
#160993=CARTESIAN_POINT('Ctrl Pts',(3.24430065599994,11.6,-9.95790981100001));
#160994=CARTESIAN_POINT('Ctrl Pts',(3.24503022499994,15.2,-9.95932139400001));
#160995=CARTESIAN_POINT('Ctrl Pts',(3.24503022499994,11.6,-9.95932139400001));
#160996=CARTESIAN_POINT('Ctrl Pts',(3.24576475099994,15.2,-9.96073929700001));
#160997=CARTESIAN_POINT('Ctrl Pts',(3.24576475099994,11.6,-9.96073929700001));
#160998=CARTESIAN_POINT('Ctrl Pts',(3.24650423699994,15.2,-9.96216349800001));
#160999=CARTESIAN_POINT('Ctrl Pts',(3.24650423699994,11.6,-9.96216349800001));
#161000=CARTESIAN_POINT('Ctrl Pts',(3.24724868499994,15.2,-9.96359397500001));
#161001=CARTESIAN_POINT('Ctrl Pts',(3.24724868499994,11.6,-9.96359397500001));
#161002=CARTESIAN_POINT('Ctrl Pts',(3.24799810099994,15.2,-9.96503070400001));
#161003=CARTESIAN_POINT('Ctrl Pts',(3.24799810099994,11.6,-9.96503070400001));
#161004=CARTESIAN_POINT('Ctrl Pts',(3.24875248699994,15.2,-9.96647366400001));
#161005=CARTESIAN_POINT('Ctrl Pts',(3.24875248699994,11.6,-9.96647366400001));
#161006=CARTESIAN_POINT('Ctrl Pts',(3.24951184599994,15.2,-9.96792282900001));
#161007=CARTESIAN_POINT('Ctrl Pts',(3.24951184599994,11.6,-9.96792282900001));
#161008=CARTESIAN_POINT('Ctrl Pts',(3.25027618199994,15.2,-9.96937818000001));
#161009=CARTESIAN_POINT('Ctrl Pts',(3.25027618199994,11.6,-9.96937818000001));
#161010=CARTESIAN_POINT('Ctrl Pts',(3.25104549799994,15.2,-9.97083969300001));
#161011=CARTESIAN_POINT('Ctrl Pts',(3.25104549799994,11.6,-9.97083969300001));
#161012=CARTESIAN_POINT('Ctrl Pts',(3.25181979799994,15.2,-9.97230734500001));
#161013=CARTESIAN_POINT('Ctrl Pts',(3.25181979799994,11.6,-9.97230734500001));
#161014=CARTESIAN_POINT('Ctrl Pts',(3.25259908499994,15.2,-9.97378111500001));
#161015=CARTESIAN_POINT('Ctrl Pts',(3.25259908499994,11.6,-9.97378111500001));
#161016=CARTESIAN_POINT('Ctrl Pts',(3.25338336099994,15.2,-9.97526098000001));
#161017=CARTESIAN_POINT('Ctrl Pts',(3.25338336099994,11.6,-9.97526098000001));
#161018=CARTESIAN_POINT('Ctrl Pts',(3.25417263099995,15.2,-9.97674691700001));
#161019=CARTESIAN_POINT('Ctrl Pts',(3.25417263099995,11.6,-9.97674691700001));
#161020=CARTESIAN_POINT('Ctrl Pts',(3.25496689699994,15.2,-9.97823890700001));
#161021=CARTESIAN_POINT('Ctrl Pts',(3.25496689699994,11.6,-9.97823890700001));
#161022=CARTESIAN_POINT('Ctrl Pts',(3.25576616299994,15.2,-9.97973692400001));
#161023=CARTESIAN_POINT('Ctrl Pts',(3.25576616299994,11.6,-9.97973692400001));
#161024=CARTESIAN_POINT('Ctrl Pts',(3.25657042999994,15.2,-9.98124094900001));
#161025=CARTESIAN_POINT('Ctrl Pts',(3.25657042999994,11.6,-9.98124094900001));
#161026=CARTESIAN_POINT('Ctrl Pts',(3.25737970399994,15.2,-9.98275096000001));
#161027=CARTESIAN_POINT('Ctrl Pts',(3.25737970399994,11.6,-9.98275096000001));
#161028=CARTESIAN_POINT('Ctrl Pts',(3.25819398599994,15.2,-9.98426693500001));
#161029=CARTESIAN_POINT('Ctrl Pts',(3.25819398599994,11.6,-9.98426693500001));
#161030=CARTESIAN_POINT('Ctrl Pts',(3.25901327999994,15.2,-9.98578885000001));
#161031=CARTESIAN_POINT('Ctrl Pts',(3.25901327999994,11.6,-9.98578885000001));
#161032=CARTESIAN_POINT('Ctrl Pts',(3.25983758999994,15.2,-9.98731668600001));
#161033=CARTESIAN_POINT('Ctrl Pts',(3.25983758999994,11.6,-9.98731668600001));
#161034=CARTESIAN_POINT('Ctrl Pts',(3.26066691699994,15.2,-9.98885042200001));
#161035=CARTESIAN_POINT('Ctrl Pts',(3.26066691699994,11.6,-9.98885042200001));
#161036=CARTESIAN_POINT('Ctrl Pts',(3.26150126499994,15.2,-9.99039003500001));
#161037=CARTESIAN_POINT('Ctrl Pts',(3.26150126499994,11.6,-9.99039003500001));
#161038=CARTESIAN_POINT('Ctrl Pts',(3.26234063699995,15.2,-9.99193550400001));
#161039=CARTESIAN_POINT('Ctrl Pts',(3.26234063699995,11.6,-9.99193550400001));
#161040=CARTESIAN_POINT('Ctrl Pts',(3.26318503599994,15.2,-9.99348680800001));
#161041=CARTESIAN_POINT('Ctrl Pts',(3.26318503599994,11.6,-9.99348680800001));
#161042=CARTESIAN_POINT('Ctrl Pts',(3.26403446499994,15.2,-9.99504392600001));
#161043=CARTESIAN_POINT('Ctrl Pts',(3.26403446499994,11.6,-9.99504392600001));
#161044=CARTESIAN_POINT('Ctrl Pts',(3.26488892599994,15.2,-9.99660683600001));
#161045=CARTESIAN_POINT('Ctrl Pts',(3.26488892599994,11.6,-9.99660683600001));
#161046=CARTESIAN_POINT('Ctrl Pts',(3.26574842199994,15.2,-9.99817551900001));
#161047=CARTESIAN_POINT('Ctrl Pts',(3.26574842199994,11.6,-9.99817551900001));
#161048=CARTESIAN_POINT('Ctrl Pts',(3.26661295799994,15.2,-9.99974995100001));
#161049=CARTESIAN_POINT('Ctrl Pts',(3.26661295799994,11.6,-9.99974995100001));
#161050=CARTESIAN_POINT('Ctrl Pts',(3.26748253399994,15.2,-10.001330114));
#161051=CARTESIAN_POINT('Ctrl Pts',(3.26748253399994,11.6,-10.001330114));
#161052=CARTESIAN_POINT('Ctrl Pts',(3.26835715399994,15.2,-10.002915985));
#161053=CARTESIAN_POINT('Ctrl Pts',(3.26835715399994,11.6,-10.002915985));
#161054=CARTESIAN_POINT('Ctrl Pts',(3.26923682099994,15.2,-10.004507545));
#161055=CARTESIAN_POINT('Ctrl Pts',(3.26923682099994,11.6,-10.004507545));
#161056=CARTESIAN_POINT('Ctrl Pts',(3.27012153799994,15.2,-10.006104772));
#161057=CARTESIAN_POINT('Ctrl Pts',(3.27012153799994,11.6,-10.006104772));
#161058=CARTESIAN_POINT('Ctrl Pts',(3.27101130699994,15.2,-10.007707647));
#161059=CARTESIAN_POINT('Ctrl Pts',(3.27101130699994,11.6,-10.007707647));
#161060=CARTESIAN_POINT('Ctrl Pts',(3.27190612999994,15.2,-10.009316148));
#161061=CARTESIAN_POINT('Ctrl Pts',(3.27190612999994,11.6,-10.009316148));
#161062=CARTESIAN_POINT('Ctrl Pts',(3.27280601099994,15.2,-10.010930254));
#161063=CARTESIAN_POINT('Ctrl Pts',(3.27280601099994,11.6,-10.010930254));
#161064=CARTESIAN_POINT('Ctrl Pts',(3.27371095399994,15.2,-10.012549947));
#161065=CARTESIAN_POINT('Ctrl Pts',(3.27371095399994,11.6,-10.012549947));
#161066=CARTESIAN_POINT('Ctrl Pts',(3.27462095799994,15.2,-10.014175204));
#161067=CARTESIAN_POINT('Ctrl Pts',(3.27462095799994,11.6,-10.014175204));
#161068=CARTESIAN_POINT('Ctrl Pts',(3.27553602799994,15.2,-10.015806007));
#161069=CARTESIAN_POINT('Ctrl Pts',(3.27553602799994,11.6,-10.015806007));
#161070=CARTESIAN_POINT('Ctrl Pts',(3.27645616799995,15.2,-10.017442335));
#161071=CARTESIAN_POINT('Ctrl Pts',(3.27645616799995,11.6,-10.017442335));
#161072=CARTESIAN_POINT('Ctrl Pts',(3.27738137599995,15.2,-10.019084168));
#161073=CARTESIAN_POINT('Ctrl Pts',(3.27738137599995,11.6,-10.019084168));
#161074=CARTESIAN_POINT('Ctrl Pts',(3.27831165899994,15.2,-10.020731486));
#161075=CARTESIAN_POINT('Ctrl Pts',(3.27831165899994,11.6,-10.020731486));
#161076=CARTESIAN_POINT('Ctrl Pts',(3.27924701799994,15.2,-10.022384268));
#161077=CARTESIAN_POINT('Ctrl Pts',(3.27924701799994,11.6,-10.022384268));
#161078=CARTESIAN_POINT('Ctrl Pts',(3.28018745599994,15.2,-10.024042495));
#161079=CARTESIAN_POINT('Ctrl Pts',(3.28018745599994,11.6,-10.024042495));
#161080=CARTESIAN_POINT('Ctrl Pts',(3.28113297399995,15.2,-10.025706148));
#161081=CARTESIAN_POINT('Ctrl Pts',(3.28113297399995,11.6,-10.025706148));
#161082=CARTESIAN_POINT('Ctrl Pts',(3.28208357499994,15.2,-10.027375206));
#161083=CARTESIAN_POINT('Ctrl Pts',(3.28208357499994,11.6,-10.027375206));
#161084=CARTESIAN_POINT('Ctrl Pts',(3.28303926199994,15.2,-10.02904965));
#161085=CARTESIAN_POINT('Ctrl Pts',(3.28303926199994,11.6,-10.02904965));
#161086=CARTESIAN_POINT('Ctrl Pts',(3.28400003899994,15.2,-10.03072946));
#161087=CARTESIAN_POINT('Ctrl Pts',(3.28400003899994,11.6,-10.03072946));
#161088=CARTESIAN_POINT('Ctrl Pts',(3.28496590599994,15.2,-10.032414616));
#161089=CARTESIAN_POINT('Ctrl Pts',(3.28496590599994,11.6,-10.032414616));
#161090=CARTESIAN_POINT('Ctrl Pts',(3.28593686499994,15.2,-10.0341051));
#161091=CARTESIAN_POINT('Ctrl Pts',(3.28593686499994,11.6,-10.0341051));
#161092=CARTESIAN_POINT('Ctrl Pts',(3.28691291999994,15.2,-10.035800892));
#161093=CARTESIAN_POINT('Ctrl Pts',(3.28691291999994,11.6,-10.035800892));
#161094=CARTESIAN_POINT('Ctrl Pts',(3.28789407299994,15.2,-10.037501971));
#161095=CARTESIAN_POINT('Ctrl Pts',(3.28789407299994,11.6,-10.037501971));
#161096=CARTESIAN_POINT('Ctrl Pts',(3.28888032599994,15.2,-10.039208319));
#161097=CARTESIAN_POINT('Ctrl Pts',(3.28888032599994,11.6,-10.039208319));
#161098=CARTESIAN_POINT('Ctrl Pts',(3.28987168199995,15.2,-10.040919917));
#161099=CARTESIAN_POINT('Ctrl Pts',(3.28987168199995,11.6,-10.040919917));
#161100=CARTESIAN_POINT('Ctrl Pts',(3.29086814199994,15.2,-10.042636746));
#161101=CARTESIAN_POINT('Ctrl Pts',(3.29086814199994,11.6,-10.042636746));
#161102=CARTESIAN_POINT('Ctrl Pts',(3.29186971099994,15.2,-10.044358787));
#161103=CARTESIAN_POINT('Ctrl Pts',(3.29186971099994,11.6,-10.044358787));
#161104=CARTESIAN_POINT('Ctrl Pts',(3.29287638699994,15.2,-10.04608602));
#161105=CARTESIAN_POINT('Ctrl Pts',(3.29287638699994,11.6,-10.04608602));
#161106=CARTESIAN_POINT('Ctrl Pts',(3.29388817699994,15.2,-10.047818426));
#161107=CARTESIAN_POINT('Ctrl Pts',(3.29388817699994,11.6,-10.047818426));
#161108=CARTESIAN_POINT('Ctrl Pts',(3.29490507899994,15.2,-10.049555987));
#161109=CARTESIAN_POINT('Ctrl Pts',(3.29490507899994,11.6,-10.049555987));
#161110=CARTESIAN_POINT('Ctrl Pts',(3.29592709799994,15.2,-10.051298684));
#161111=CARTESIAN_POINT('Ctrl Pts',(3.29592709799994,11.6,-10.051298684));
#161112=CARTESIAN_POINT('Ctrl Pts',(3.29695423399994,15.2,-10.053046497));
#161113=CARTESIAN_POINT('Ctrl Pts',(3.29695423399994,11.6,-10.053046497));
#161114=CARTESIAN_POINT('Ctrl Pts',(3.29798649099994,15.2,-10.054799409));
#161115=CARTESIAN_POINT('Ctrl Pts',(3.29798649099994,11.6,-10.054799409));
#161116=CARTESIAN_POINT('Ctrl Pts',(3.29902387099994,15.2,-10.0565574));
#161117=CARTESIAN_POINT('Ctrl Pts',(3.29902387099994,11.6,-10.0565574));
#161118=CARTESIAN_POINT('Ctrl Pts',(3.30006637499995,15.2,-10.058320452));
#161119=CARTESIAN_POINT('Ctrl Pts',(3.30006637499995,11.6,-10.058320452));
#161120=CARTESIAN_POINT('Ctrl Pts',(3.30111400599994,15.2,-10.060088546));
#161121=CARTESIAN_POINT('Ctrl Pts',(3.30111400599994,11.6,-10.060088546));
#161122=CARTESIAN_POINT('Ctrl Pts',(3.30216676499994,15.2,-10.061861665));
#161123=CARTESIAN_POINT('Ctrl Pts',(3.30216676499994,11.6,-10.061861665));
#161124=CARTESIAN_POINT('Ctrl Pts',(3.30322465599994,15.2,-10.063639788));
#161125=CARTESIAN_POINT('Ctrl Pts',(3.30322465599994,11.6,-10.063639788));
#161126=CARTESIAN_POINT('Ctrl Pts',(3.30428767999994,15.2,-10.065422899));
#161127=CARTESIAN_POINT('Ctrl Pts',(3.30428767999994,11.6,-10.065422899));
#161128=CARTESIAN_POINT('Ctrl Pts',(3.30535583799994,15.2,-10.067210978));
#161129=CARTESIAN_POINT('Ctrl Pts',(3.30535583799994,11.6,-10.067210978));
#161130=CARTESIAN_POINT('Ctrl Pts',(3.30642913399994,15.2,-10.069004008));
#161131=CARTESIAN_POINT('Ctrl Pts',(3.30642913399994,11.6,-10.069004008));
#161132=CARTESIAN_POINT('Ctrl Pts',(3.30750756699994,15.2,-10.070801971));
#161133=CARTESIAN_POINT('Ctrl Pts',(3.30750756699994,11.6,-10.070801971));
#161134=CARTESIAN_POINT('Ctrl Pts',(3.30859114299995,15.2,-10.072604847));
#161135=CARTESIAN_POINT('Ctrl Pts',(3.30859114299995,11.6,-10.072604847));
#161136=CARTESIAN_POINT('Ctrl Pts',(3.30967986099994,15.2,-10.074412619));
#161137=CARTESIAN_POINT('Ctrl Pts',(3.30967986099994,11.6,-10.074412619));
#161138=CARTESIAN_POINT('Ctrl Pts',(3.31077372499994,15.2,-10.07622527));
#161139=CARTESIAN_POINT('Ctrl Pts',(3.31077372499994,11.6,-10.07622527));
#161140=CARTESIAN_POINT('Ctrl Pts',(3.31187273499994,15.2,-10.07804278));
#161141=CARTESIAN_POINT('Ctrl Pts',(3.31187273499994,11.6,-10.07804278));
#161142=CARTESIAN_POINT('Ctrl Pts',(3.31297689299995,15.2,-10.079865133));
#161143=CARTESIAN_POINT('Ctrl Pts',(3.31297689299995,11.6,-10.079865133));
#161144=CARTESIAN_POINT('Ctrl Pts',(3.31408620199994,15.2,-10.081692309));
#161145=CARTESIAN_POINT('Ctrl Pts',(3.31408620199994,11.6,-10.081692309));
#161146=CARTESIAN_POINT('Ctrl Pts',(3.31520066299994,15.2,-10.083524293));
#161147=CARTESIAN_POINT('Ctrl Pts',(3.31520066299994,11.6,-10.083524293));
#161148=CARTESIAN_POINT('Ctrl Pts',(3.31632027899994,15.2,-10.085361064));
#161149=CARTESIAN_POINT('Ctrl Pts',(3.31632027899994,11.6,-10.085361064));
#161150=CARTESIAN_POINT('Ctrl Pts',(3.31744505099994,15.2,-10.087202608));
#161151=CARTESIAN_POINT('Ctrl Pts',(3.31744505099994,11.6,-10.087202608));
#161152=CARTESIAN_POINT('Ctrl Pts',(3.31857498099994,15.2,-10.089048904));
#161153=CARTESIAN_POINT('Ctrl Pts',(3.31857498099994,11.6,-10.089048904));
#161154=CARTESIAN_POINT('Ctrl Pts',(3.31971006999995,15.2,-10.090899936));
#161155=CARTESIAN_POINT('Ctrl Pts',(3.31971006999995,11.6,-10.090899936));
#161156=CARTESIAN_POINT('Ctrl Pts',(3.32085032099994,15.2,-10.092755686));
#161157=CARTESIAN_POINT('Ctrl Pts',(3.32085032099994,11.6,-10.092755686));
#161158=CARTESIAN_POINT('Ctrl Pts',(3.32199573599994,15.2,-10.094616137));
#161159=CARTESIAN_POINT('Ctrl Pts',(3.32199573599994,11.6,-10.094616137));
#161160=CARTESIAN_POINT('Ctrl Pts',(3.32314631399994,15.2,-10.096481272));
#161161=CARTESIAN_POINT('Ctrl Pts',(3.32314631399994,11.6,-10.096481272));
#161162=CARTESIAN_POINT('Ctrl Pts',(3.32430206099994,15.2,-10.098351072));
#161163=CARTESIAN_POINT('Ctrl Pts',(3.32430206099994,11.6,-10.098351072));
#161164=CARTESIAN_POINT('Ctrl Pts',(3.32546297499994,15.2,-10.100225521));
#161165=CARTESIAN_POINT('Ctrl Pts',(3.32546297499994,11.6,-10.100225521));
#161166=CARTESIAN_POINT('Ctrl Pts',(3.32662905999995,15.2,-10.102104602));
#161167=CARTESIAN_POINT('Ctrl Pts',(3.32662905999995,11.6,-10.102104602));
#161168=CARTESIAN_POINT('Ctrl Pts',(3.32780031599994,15.2,-10.103988296));
#161169=CARTESIAN_POINT('Ctrl Pts',(3.32780031599994,11.6,-10.103988296));
#161170=CARTESIAN_POINT('Ctrl Pts',(3.32897674599994,15.2,-10.105876587));
#161171=CARTESIAN_POINT('Ctrl Pts',(3.32897674599994,11.6,-10.105876587));
#161172=CARTESIAN_POINT('Ctrl Pts',(3.33015835099994,15.2,-10.10776946));
#161173=CARTESIAN_POINT('Ctrl Pts',(3.33015835099994,11.6,-10.10776946));
#161174=CARTESIAN_POINT('Ctrl Pts',(3.33134513299994,15.2,-10.109666894));
#161175=CARTESIAN_POINT('Ctrl Pts',(3.33134513299994,11.6,-10.109666894));
#161176=CARTESIAN_POINT('Ctrl Pts',(3.33253709299994,15.2,-10.111568874));
#161177=CARTESIAN_POINT('Ctrl Pts',(3.33253709299994,11.6,-10.111568874));
#161178=CARTESIAN_POINT('Ctrl Pts',(3.33373423399994,15.2,-10.113475383));
#161179=CARTESIAN_POINT('Ctrl Pts',(3.33373423399994,11.6,-10.113475383));
#161180=CARTESIAN_POINT('Ctrl Pts',(3.33493655499994,15.2,-10.115386404));
#161181=CARTESIAN_POINT('Ctrl Pts',(3.33493655499994,11.6,-10.115386404));
#161182=CARTESIAN_POINT('Ctrl Pts',(3.33614405999994,15.2,-10.117301921));
#161183=CARTESIAN_POINT('Ctrl Pts',(3.33614405999994,11.6,-10.117301921));
#161184=CARTESIAN_POINT('Ctrl Pts',(3.33735674999994,15.2,-10.119221915));
#161185=CARTESIAN_POINT('Ctrl Pts',(3.33735674999994,11.6,-10.119221915));
#161186=CARTESIAN_POINT('Ctrl Pts',(3.33857462499994,15.2,-10.121146371));
#161187=CARTESIAN_POINT('Ctrl Pts',(3.33857462499994,11.6,-10.121146371));
#161188=CARTESIAN_POINT('Ctrl Pts',(3.33979768899995,15.2,-10.123075272));
#161189=CARTESIAN_POINT('Ctrl Pts',(3.33979768899995,11.6,-10.123075272));
#161190=CARTESIAN_POINT('Ctrl Pts',(3.34102594099994,15.2,-10.125008601));
#161191=CARTESIAN_POINT('Ctrl Pts',(3.34102594099994,11.6,-10.125008601));
#161192=CARTESIAN_POINT('Ctrl Pts',(3.34225938399995,15.2,-10.126946341));
#161193=CARTESIAN_POINT('Ctrl Pts',(3.34225938399995,11.6,-10.126946341));
#161194=CARTESIAN_POINT('Ctrl Pts',(3.34349802099994,15.2,-10.128888477));
#161195=CARTESIAN_POINT('Ctrl Pts',(3.34349802099994,11.6,-10.128888477));
#161196=CARTESIAN_POINT('Ctrl Pts',(3.34474184999995,15.2,-10.130834991));
#161197=CARTESIAN_POINT('Ctrl Pts',(3.34474184999995,11.6,-10.130834991));
#161198=CARTESIAN_POINT('Ctrl Pts',(3.34599087399994,15.2,-10.132785867));
#161199=CARTESIAN_POINT('Ctrl Pts',(3.34599087399994,11.6,-10.132785867));
#161200=CARTESIAN_POINT('Ctrl Pts',(3.34724509499994,15.2,-10.134741089));
#161201=CARTESIAN_POINT('Ctrl Pts',(3.34724509499994,11.6,-10.134741089));
#161202=CARTESIAN_POINT('Ctrl Pts',(3.34850451299994,15.2,-10.13670064));
#161203=CARTESIAN_POINT('Ctrl Pts',(3.34850451299994,11.6,-10.13670064));
#161204=CARTESIAN_POINT('Ctrl Pts',(3.34976913199994,15.2,-10.138664504));
#161205=CARTESIAN_POINT('Ctrl Pts',(3.34976913199994,11.6,-10.138664504));
#161206=CARTESIAN_POINT('Ctrl Pts',(3.35103895099994,15.2,-10.140632665));
#161207=CARTESIAN_POINT('Ctrl Pts',(3.35103895099994,11.6,-10.140632665));
#161208=CARTESIAN_POINT('Ctrl Pts',(3.35231397199995,15.2,-10.142605106));
#161209=CARTESIAN_POINT('Ctrl Pts',(3.35231397199995,11.6,-10.142605106));
#161210=CARTESIAN_POINT('Ctrl Pts',(3.35359419599994,15.2,-10.14458181));
#161211=CARTESIAN_POINT('Ctrl Pts',(3.35359419599994,11.6,-10.14458181));
#161212=CARTESIAN_POINT('Ctrl Pts',(3.35487962399994,15.2,-10.146562764));
#161213=CARTESIAN_POINT('Ctrl Pts',(3.35487962399994,11.6,-10.146562764));
#161214=CARTESIAN_POINT('Ctrl Pts',(3.35617025999994,15.2,-10.148547949));
#161215=CARTESIAN_POINT('Ctrl Pts',(3.35617025999994,11.6,-10.148547949));
#161216=CARTESIAN_POINT('Ctrl Pts',(3.35746610199994,15.2,-10.15053735));
#161217=CARTESIAN_POINT('Ctrl Pts',(3.35746610199994,11.6,-10.15053735));
#161218=CARTESIAN_POINT('Ctrl Pts',(3.35876715299994,15.2,-10.152530951));
#161219=CARTESIAN_POINT('Ctrl Pts',(3.35876715299994,11.6,-10.152530951));
#161220=CARTESIAN_POINT('Ctrl Pts',(3.36007341499994,15.2,-10.154528737));
#161221=CARTESIAN_POINT('Ctrl Pts',(3.36007341499994,11.6,-10.154528737));
#161222=CARTESIAN_POINT('Ctrl Pts',(3.36138488699994,15.2,-10.156530691));
#161223=CARTESIAN_POINT('Ctrl Pts',(3.36138488699994,11.6,-10.156530691));
#161224=CARTESIAN_POINT('Ctrl Pts',(3.36270157099994,15.2,-10.158536796));
#161225=CARTESIAN_POINT('Ctrl Pts',(3.36270157099994,11.6,-10.158536796));
#161226=CARTESIAN_POINT('Ctrl Pts',(3.36402346899995,15.2,-10.160547038));
#161227=CARTESIAN_POINT('Ctrl Pts',(3.36402346899995,11.6,-10.160547038));
#161228=CARTESIAN_POINT('Ctrl Pts',(3.36535058199994,15.2,-10.1625614));
#161229=CARTESIAN_POINT('Ctrl Pts',(3.36535058199994,11.6,-10.1625614));
#161230=CARTESIAN_POINT('Ctrl Pts',(3.36668291199994,15.2,-10.164579868));
#161231=CARTESIAN_POINT('Ctrl Pts',(3.36668291199994,11.6,-10.164579868));
#161232=CARTESIAN_POINT('Ctrl Pts',(3.36802045799995,15.2,-10.166602424));
#161233=CARTESIAN_POINT('Ctrl Pts',(3.36802045799995,11.6,-10.166602424));
#161234=CARTESIAN_POINT('Ctrl Pts',(3.36936322299994,15.2,-10.168629055));
#161235=CARTESIAN_POINT('Ctrl Pts',(3.36936322299994,11.6,-10.168629055));
#161236=CARTESIAN_POINT('Ctrl Pts',(3.37071120799994,15.2,-10.170659743));
#161237=CARTESIAN_POINT('Ctrl Pts',(3.37071120799994,11.6,-10.170659743));
#161238=CARTESIAN_POINT('Ctrl Pts',(3.37206441299994,15.2,-10.172694474));
#161239=CARTESIAN_POINT('Ctrl Pts',(3.37206441299994,11.6,-10.172694474));
#161240=CARTESIAN_POINT('Ctrl Pts',(3.37342283999994,15.2,-10.174733232));
#161241=CARTESIAN_POINT('Ctrl Pts',(3.37342283999994,11.6,-10.174733232));
#161242=CARTESIAN_POINT('Ctrl Pts',(3.37478648999994,15.2,-10.176776001));
#161243=CARTESIAN_POINT('Ctrl Pts',(3.37478648999994,11.6,-10.176776001));
#161244=CARTESIAN_POINT('Ctrl Pts',(3.37615536399994,15.2,-10.178822767));
#161245=CARTESIAN_POINT('Ctrl Pts',(3.37615536399994,11.6,-10.178822767));
#161246=CARTESIAN_POINT('Ctrl Pts',(3.37752946399994,15.2,-10.180873512));
#161247=CARTESIAN_POINT('Ctrl Pts',(3.37752946399994,11.6,-10.180873512));
#161248=CARTESIAN_POINT('Ctrl Pts',(3.37890878999994,15.2,-10.182928223));
#161249=CARTESIAN_POINT('Ctrl Pts',(3.37890878999994,11.6,-10.182928223));
#161250=CARTESIAN_POINT('Ctrl Pts',(3.38029334199994,15.2,-10.184986883));
#161251=CARTESIAN_POINT('Ctrl Pts',(3.38029334199994,11.6,-10.184986883));
#161252=CARTESIAN_POINT('Ctrl Pts',(3.38168312399994,15.2,-10.18704948));
#161253=CARTESIAN_POINT('Ctrl Pts',(3.38168312399994,11.6,-10.18704948));
#161254=CARTESIAN_POINT('Ctrl Pts',(3.38307813499994,15.2,-10.189115995));
#161255=CARTESIAN_POINT('Ctrl Pts',(3.38307813499994,11.6,-10.189115995));
#161256=CARTESIAN_POINT('Ctrl Pts',(3.38447837599994,15.2,-10.191186414));
#161257=CARTESIAN_POINT('Ctrl Pts',(3.38447837599994,11.6,-10.191186414));
#161258=CARTESIAN_POINT('Ctrl Pts',(3.38588384799994,15.2,-10.193260724));
#161259=CARTESIAN_POINT('Ctrl Pts',(3.38588384799994,11.6,-10.193260724));
#161260=CARTESIAN_POINT('Ctrl Pts',(3.38729455299994,15.2,-10.195338907));
#161261=CARTESIAN_POINT('Ctrl Pts',(3.38729455299994,11.6,-10.195338907));
#161262=CARTESIAN_POINT('Ctrl Pts',(3.38871049099994,15.2,-10.197420949));
#161263=CARTESIAN_POINT('Ctrl Pts',(3.38871049099994,11.6,-10.197420949));
#161264=CARTESIAN_POINT('Ctrl Pts',(3.39013166399994,15.2,-10.199506834));
#161265=CARTESIAN_POINT('Ctrl Pts',(3.39013166399994,11.6,-10.199506834));
#161266=CARTESIAN_POINT('Ctrl Pts',(3.39155807199994,15.2,-10.201596549));
#161267=CARTESIAN_POINT('Ctrl Pts',(3.39155807199994,11.6,-10.201596549));
#161268=CARTESIAN_POINT('Ctrl Pts',(3.39298971599994,15.2,-10.203690078));
#161269=CARTESIAN_POINT('Ctrl Pts',(3.39298971599994,11.6,-10.203690078));
#161270=CARTESIAN_POINT('Ctrl Pts',(3.39442659799994,15.2,-10.205787407));
#161271=CARTESIAN_POINT('Ctrl Pts',(3.39442659799994,11.6,-10.205787407));
#161272=CARTESIAN_POINT('Ctrl Pts',(3.39586871699994,15.2,-10.20788852));
#161273=CARTESIAN_POINT('Ctrl Pts',(3.39586871699994,11.6,-10.20788852));
#161274=CARTESIAN_POINT('Ctrl Pts',(3.39731607599994,15.2,-10.209993402));
#161275=CARTESIAN_POINT('Ctrl Pts',(3.39731607599994,11.6,-10.209993402));
#161276=CARTESIAN_POINT('Ctrl Pts',(3.39876867499994,15.2,-10.21210204));
#161277=CARTESIAN_POINT('Ctrl Pts',(3.39876867499994,11.6,-10.21210204));
#161278=CARTESIAN_POINT('Ctrl Pts',(3.40022651399994,15.2,-10.214214417));
#161279=CARTESIAN_POINT('Ctrl Pts',(3.40022651399994,11.6,-10.214214417));
#161280=CARTESIAN_POINT('Ctrl Pts',(3.40168959499994,15.2,-10.21633052));
#161281=CARTESIAN_POINT('Ctrl Pts',(3.40168959499994,11.6,-10.21633052));
#161282=CARTESIAN_POINT('Ctrl Pts',(3.40315791799994,15.2,-10.218450334));
#161283=CARTESIAN_POINT('Ctrl Pts',(3.40315791799994,11.6,-10.218450334));
#161284=CARTESIAN_POINT('Ctrl Pts',(3.40463148499994,15.2,-10.220573843));
#161285=CARTESIAN_POINT('Ctrl Pts',(3.40463148499994,11.6,-10.220573843));
#161286=CARTESIAN_POINT('Ctrl Pts',(3.40611029499994,15.2,-10.222701034));
#161287=CARTESIAN_POINT('Ctrl Pts',(3.40611029499994,11.6,-10.222701034));
#161288=CARTESIAN_POINT('Ctrl Pts',(3.40759435099995,15.2,-10.224831893));
#161289=CARTESIAN_POINT('Ctrl Pts',(3.40759435099995,11.6,-10.224831893));
#161290=CARTESIAN_POINT('Ctrl Pts',(3.40908365299994,15.2,-10.226966403));
#161291=CARTESIAN_POINT('Ctrl Pts',(3.40908365299994,11.6,-10.226966403));
#161292=CARTESIAN_POINT('Ctrl Pts',(3.41057820099994,15.2,-10.229104552));
#161293=CARTESIAN_POINT('Ctrl Pts',(3.41057820099994,11.6,-10.229104552));
#161294=CARTESIAN_POINT('Ctrl Pts',(3.41207799599994,15.2,-10.231246323));
#161295=CARTESIAN_POINT('Ctrl Pts',(3.41207799599994,11.6,-10.231246323));
#161296=CARTESIAN_POINT('Ctrl Pts',(3.41358303899994,15.2,-10.233391704));
#161297=CARTESIAN_POINT('Ctrl Pts',(3.41358303899994,11.6,-10.233391704));
#161298=CARTESIAN_POINT('Ctrl Pts',(3.41509333199994,15.2,-10.235540681));
#161299=CARTESIAN_POINT('Ctrl Pts',(3.41509333199994,11.6,-10.235540681));
#161300=CARTESIAN_POINT('Ctrl Pts',(3.41660887299994,15.2,-10.237693237));
#161301=CARTESIAN_POINT('Ctrl Pts',(3.41660887299994,11.6,-10.237693237));
#161302=CARTESIAN_POINT('Ctrl Pts',(3.41812966599994,15.2,-10.239849361));
#161303=CARTESIAN_POINT('Ctrl Pts',(3.41812966599994,11.6,-10.239849361));
#161304=CARTESIAN_POINT('Ctrl Pts',(3.41965570899994,15.2,-10.242009036));
#161305=CARTESIAN_POINT('Ctrl Pts',(3.41965570899994,11.6,-10.242009036));
#161306=CARTESIAN_POINT('Ctrl Pts',(3.42118700299994,15.2,-10.244172248));
#161307=CARTESIAN_POINT('Ctrl Pts',(3.42118700299994,11.6,-10.244172248));
#161308=CARTESIAN_POINT('Ctrl Pts',(3.42272355099994,15.2,-10.246338985));
#161309=CARTESIAN_POINT('Ctrl Pts',(3.42272355099994,11.6,-10.246338985));
#161310=CARTESIAN_POINT('Ctrl Pts',(3.42426535099994,15.2,-10.24850923));
#161311=CARTESIAN_POINT('Ctrl Pts',(3.42426535099994,11.6,-10.24850923));
#161312=CARTESIAN_POINT('Ctrl Pts',(3.42581240499995,15.2,-10.250682971));
#161313=CARTESIAN_POINT('Ctrl Pts',(3.42581240499995,11.6,-10.250682971));
#161314=CARTESIAN_POINT('Ctrl Pts',(3.42736471299995,15.2,-10.252860194));
#161315=CARTESIAN_POINT('Ctrl Pts',(3.42736471299995,11.6,-10.252860194));
#161316=CARTESIAN_POINT('Ctrl Pts',(3.42892227699994,15.2,-10.255040883));
#161317=CARTESIAN_POINT('Ctrl Pts',(3.42892227699994,11.6,-10.255040883));
#161318=CARTESIAN_POINT('Ctrl Pts',(3.43048509499994,15.2,-10.257225027));
#161319=CARTESIAN_POINT('Ctrl Pts',(3.43048509499994,11.6,-10.257225027));
#161320=CARTESIAN_POINT('Ctrl Pts',(3.43205317099994,15.2,-10.259412609));
#161321=CARTESIAN_POINT('Ctrl Pts',(3.43205317099994,11.6,-10.259412609));
#161322=CARTESIAN_POINT('Ctrl Pts',(3.43362650399994,15.2,-10.261603617));
#161323=CARTESIAN_POINT('Ctrl Pts',(3.43362650399994,11.6,-10.261603617));
#161324=CARTESIAN_POINT('Ctrl Pts',(3.43520509299994,15.2,-10.263798037));
#161325=CARTESIAN_POINT('Ctrl Pts',(3.43520509299994,11.6,-10.263798037));
#161326=CARTESIAN_POINT('Ctrl Pts',(3.43678893999994,15.2,-10.265995854));
#161327=CARTESIAN_POINT('Ctrl Pts',(3.43678893999994,11.6,-10.265995854));
#161328=CARTESIAN_POINT('Ctrl Pts',(3.43837804699994,15.2,-10.268197055));
#161329=CARTESIAN_POINT('Ctrl Pts',(3.43837804699994,11.6,-10.268197055));
#161330=CARTESIAN_POINT('Ctrl Pts',(3.43997241199994,15.2,-10.270401626));
#161331=CARTESIAN_POINT('Ctrl Pts',(3.43997241199994,11.6,-10.270401626));
#161332=CARTESIAN_POINT('Ctrl Pts',(3.44157203699994,15.2,-10.272609553));
#161333=CARTESIAN_POINT('Ctrl Pts',(3.44157203699994,11.6,-10.272609553));
#161334=CARTESIAN_POINT('Ctrl Pts',(3.44317692299994,15.2,-10.274820824));
#161335=CARTESIAN_POINT('Ctrl Pts',(3.44317692299994,11.6,-10.274820824));
#161336=CARTESIAN_POINT('Ctrl Pts',(3.44478706899995,15.2,-10.277035423));
#161337=CARTESIAN_POINT('Ctrl Pts',(3.44478706899995,11.6,-10.277035423));
#161338=CARTESIAN_POINT('Ctrl Pts',(3.44640247599994,15.2,-10.279253337));
#161339=CARTESIAN_POINT('Ctrl Pts',(3.44640247599994,11.6,-10.279253337));
#161340=CARTESIAN_POINT('Ctrl Pts',(3.44802314499994,15.2,-10.281474553));
#161341=CARTESIAN_POINT('Ctrl Pts',(3.44802314499994,11.6,-10.281474553));
#161342=CARTESIAN_POINT('Ctrl Pts',(3.44964907799994,15.2,-10.283699057));
#161343=CARTESIAN_POINT('Ctrl Pts',(3.44964907799994,11.6,-10.283699057));
#161344=CARTESIAN_POINT('Ctrl Pts',(3.45128027199994,15.2,-10.285926837));
#161345=CARTESIAN_POINT('Ctrl Pts',(3.45128027199994,11.6,-10.285926837));
#161346=CARTESIAN_POINT('Ctrl Pts',(3.45291672899994,15.2,-10.288157876));
#161347=CARTESIAN_POINT('Ctrl Pts',(3.45291672899994,11.6,-10.288157876));
#161348=CARTESIAN_POINT('Ctrl Pts',(3.45455844999994,15.2,-10.290392164));
#161349=CARTESIAN_POINT('Ctrl Pts',(3.45455844999994,11.6,-10.290392164));
#161350=CARTESIAN_POINT('Ctrl Pts',(3.45620543599995,15.2,-10.292629685));
#161351=CARTESIAN_POINT('Ctrl Pts',(3.45620543599995,11.6,-10.292629685));
#161352=CARTESIAN_POINT('Ctrl Pts',(3.45785768599994,15.2,-10.294870428));
#161353=CARTESIAN_POINT('Ctrl Pts',(3.45785768599994,11.6,-10.294870428));
#161354=CARTESIAN_POINT('Ctrl Pts',(3.45951520099995,15.2,-10.297114378));
#161355=CARTESIAN_POINT('Ctrl Pts',(3.45951520099995,11.6,-10.297114378));
#161356=CARTESIAN_POINT('Ctrl Pts',(3.46117798099994,15.2,-10.299361521));
#161357=CARTESIAN_POINT('Ctrl Pts',(3.46117798099994,11.6,-10.299361521));
#161358=CARTESIAN_POINT('Ctrl Pts',(3.46284602699995,15.2,-10.301611846));
#161359=CARTESIAN_POINT('Ctrl Pts',(3.46284602699995,11.6,-10.301611846));
#161360=CARTESIAN_POINT('Ctrl Pts',(3.46451933999994,15.2,-10.303865339));
#161361=CARTESIAN_POINT('Ctrl Pts',(3.46451933999994,11.6,-10.303865339));
#161362=CARTESIAN_POINT('Ctrl Pts',(3.46619791799994,15.2,-10.306121984));
#161363=CARTESIAN_POINT('Ctrl Pts',(3.46619791799994,11.6,-10.306121984));
#161364=CARTESIAN_POINT('Ctrl Pts',(3.46788176499994,15.2,-10.308381772));
#161365=CARTESIAN_POINT('Ctrl Pts',(3.46788176499994,11.6,-10.308381772));
#161366=CARTESIAN_POINT('Ctrl Pts',(3.46957087699994,15.2,-10.310644687));
#161367=CARTESIAN_POINT('Ctrl Pts',(3.46957087699994,11.6,-10.310644687));
#161368=CARTESIAN_POINT('Ctrl Pts',(3.47126525899994,15.2,-10.312910717));
#161369=CARTESIAN_POINT('Ctrl Pts',(3.47126525899994,11.6,-10.312910717));
#161370=CARTESIAN_POINT('Ctrl Pts',(3.47296490699994,15.2,-10.315179847));
#161371=CARTESIAN_POINT('Ctrl Pts',(3.47296490699994,11.6,-10.315179847));
#161372=CARTESIAN_POINT('Ctrl Pts',(3.47466982399995,15.2,-10.317452067));
#161373=CARTESIAN_POINT('Ctrl Pts',(3.47466982399995,11.6,-10.317452067));
#161374=CARTESIAN_POINT('Ctrl Pts',(3.47638000999994,15.2,-10.319727362));
#161375=CARTESIAN_POINT('Ctrl Pts',(3.47638000999994,11.6,-10.319727362));
#161376=CARTESIAN_POINT('Ctrl Pts',(3.47809546499994,15.2,-10.322005719));
#161377=CARTESIAN_POINT('Ctrl Pts',(3.47809546499994,11.6,-10.322005719));
#161378=CARTESIAN_POINT('Ctrl Pts',(3.47981618899994,15.2,-10.324287126));
#161379=CARTESIAN_POINT('Ctrl Pts',(3.47981618899994,11.6,-10.324287126));
#161380=CARTESIAN_POINT('Ctrl Pts',(3.48154218299995,15.2,-10.326571569));
#161381=CARTESIAN_POINT('Ctrl Pts',(3.48154218299995,11.6,-10.326571569));
#161382=CARTESIAN_POINT('Ctrl Pts',(3.48327344499994,15.2,-10.328859035));
#161383=CARTESIAN_POINT('Ctrl Pts',(3.48327344499994,11.6,-10.328859035));
#161384=CARTESIAN_POINT('Ctrl Pts',(3.48500997899994,15.2,-10.331149511));
#161385=CARTESIAN_POINT('Ctrl Pts',(3.48500997899994,11.6,-10.331149511));
#161386=CARTESIAN_POINT('Ctrl Pts',(3.48675178199994,15.2,-10.333442986));
#161387=CARTESIAN_POINT('Ctrl Pts',(3.48675178199994,11.6,-10.333442986));
#161388=CARTESIAN_POINT('Ctrl Pts',(3.48849885699994,15.2,-10.335739446));
#161389=CARTESIAN_POINT('Ctrl Pts',(3.48849885699994,11.6,-10.335739446));
#161390=CARTESIAN_POINT('Ctrl Pts',(3.49025120099994,15.2,-10.338038877));
#161391=CARTESIAN_POINT('Ctrl Pts',(3.49025120099994,11.6,-10.338038877));
#161392=CARTESIAN_POINT('Ctrl Pts',(3.49200881699995,15.2,-10.340341267));
#161393=CARTESIAN_POINT('Ctrl Pts',(3.49200881699995,11.6,-10.340341267));
#161394=CARTESIAN_POINT('Ctrl Pts',(3.49377170499995,15.2,-10.342646604));
#161395=CARTESIAN_POINT('Ctrl Pts',(3.49377170499995,11.6,-10.342646604));
#161396=CARTESIAN_POINT('Ctrl Pts',(3.49553986299994,15.2,-10.344954875));
#161397=CARTESIAN_POINT('Ctrl Pts',(3.49553986299994,11.6,-10.344954875));
#161398=CARTESIAN_POINT('Ctrl Pts',(3.49731329299994,15.2,-10.347266067));
#161399=CARTESIAN_POINT('Ctrl Pts',(3.49731329299994,11.6,-10.347266067));
#161400=CARTESIAN_POINT('Ctrl Pts',(3.49909199599994,15.2,-10.349580167));
#161401=CARTESIAN_POINT('Ctrl Pts',(3.49909199599994,11.6,-10.349580167));
#161402=CARTESIAN_POINT('Ctrl Pts',(3.50087596999994,15.2,-10.351897163));
#161403=CARTESIAN_POINT('Ctrl Pts',(3.50087596999994,11.6,-10.351897163));
#161404=CARTESIAN_POINT('Ctrl Pts',(3.50266521599994,15.2,-10.354217042));
#161405=CARTESIAN_POINT('Ctrl Pts',(3.50266521599994,11.6,-10.354217042));
#161406=CARTESIAN_POINT('Ctrl Pts',(3.50445973399994,15.2,-10.356539792));
#161407=CARTESIAN_POINT('Ctrl Pts',(3.50445973399994,11.6,-10.356539792));
#161408=CARTESIAN_POINT('Ctrl Pts',(3.50625952499994,15.2,-10.358865399));
#161409=CARTESIAN_POINT('Ctrl Pts',(3.50625952499994,11.6,-10.358865399));
#161410=CARTESIAN_POINT('Ctrl Pts',(3.50806458899994,15.2,-10.361193853));
#161411=CARTESIAN_POINT('Ctrl Pts',(3.50806458899994,11.6,-10.361193853));
#161412=CARTESIAN_POINT('Ctrl Pts',(3.50987492499994,15.2,-10.363525138));
#161413=CARTESIAN_POINT('Ctrl Pts',(3.50987492499994,11.6,-10.363525138));
#161414=CARTESIAN_POINT('Ctrl Pts',(3.51169053399994,15.2,-10.365859245));
#161415=CARTESIAN_POINT('Ctrl Pts',(3.51169053399994,11.6,-10.365859245));
#161416=CARTESIAN_POINT('Ctrl Pts',(3.51351141599994,15.2,-10.36819616));
#161417=CARTESIAN_POINT('Ctrl Pts',(3.51351141599994,11.6,-10.36819616));
#161418=CARTESIAN_POINT('Ctrl Pts',(3.51533757099994,15.2,-10.37053587));
#161419=CARTESIAN_POINT('Ctrl Pts',(3.51533757099994,11.6,-10.37053587));
#161420=CARTESIAN_POINT('Ctrl Pts',(3.51716899799994,15.2,-10.372878365));
#161421=CARTESIAN_POINT('Ctrl Pts',(3.51716899799994,11.6,-10.372878365));
#161422=CARTESIAN_POINT('Ctrl Pts',(3.51900569999994,15.2,-10.375223629));
#161423=CARTESIAN_POINT('Ctrl Pts',(3.51900569999994,11.6,-10.375223629));
#161424=CARTESIAN_POINT('Ctrl Pts',(3.52084767399994,15.2,-10.377571653));
#161425=CARTESIAN_POINT('Ctrl Pts',(3.52084767399994,11.6,-10.377571653));
#161426=CARTESIAN_POINT('Ctrl Pts',(3.52269492199994,15.2,-10.379922422));
#161427=CARTESIAN_POINT('Ctrl Pts',(3.52269492199994,11.6,-10.379922422));
#161428=CARTESIAN_POINT('Ctrl Pts',(3.52454744299994,15.2,-10.382275926));
#161429=CARTESIAN_POINT('Ctrl Pts',(3.52454744299994,11.6,-10.382275926));
#161430=CARTESIAN_POINT('Ctrl Pts',(3.52640523699994,15.2,-10.384632152));
#161431=CARTESIAN_POINT('Ctrl Pts',(3.52640523699994,11.6,-10.384632152));
#161432=CARTESIAN_POINT('Ctrl Pts',(3.52826830499994,15.2,-10.386991088));
#161433=CARTESIAN_POINT('Ctrl Pts',(3.52826830499994,11.6,-10.386991088));
#161434=CARTESIAN_POINT('Ctrl Pts',(3.53013664599994,15.2,-10.38935272));
#161435=CARTESIAN_POINT('Ctrl Pts',(3.53013664599994,11.6,-10.38935272));
#161436=CARTESIAN_POINT('Ctrl Pts',(3.53201025999994,15.2,-10.391717039));
#161437=CARTESIAN_POINT('Ctrl Pts',(3.53201025999994,11.6,-10.391717039));
#161438=CARTESIAN_POINT('Ctrl Pts',(3.53388914899994,15.2,-10.394084031));
#161439=CARTESIAN_POINT('Ctrl Pts',(3.53388914899994,11.6,-10.394084031));
#161440=CARTESIAN_POINT('Ctrl Pts',(3.53577330999994,15.2,-10.396453683));
#161441=CARTESIAN_POINT('Ctrl Pts',(3.53577330999994,11.6,-10.396453683));
#161442=CARTESIAN_POINT('Ctrl Pts',(3.53766274399994,15.2,-10.398825985));
#161443=CARTESIAN_POINT('Ctrl Pts',(3.53766274399994,11.6,-10.398825985));
#161444=CARTESIAN_POINT('Ctrl Pts',(3.53955745299994,15.2,-10.401200923));
#161445=CARTESIAN_POINT('Ctrl Pts',(3.53955745299994,11.6,-10.401200923));
#161446=CARTESIAN_POINT('Ctrl Pts',(3.54145743399994,15.2,-10.403578486));
#161447=CARTESIAN_POINT('Ctrl Pts',(3.54145743399994,11.6,-10.403578486));
#161448=CARTESIAN_POINT('Ctrl Pts',(3.54336268899994,15.2,-10.405958663));
#161449=CARTESIAN_POINT('Ctrl Pts',(3.54336268899994,11.6,-10.405958663));
#161450=CARTESIAN_POINT('Ctrl Pts',(3.54527321699994,15.2,-10.408341441));
#161451=CARTESIAN_POINT('Ctrl Pts',(3.54527321699994,11.6,-10.408341441));
#161452=CARTESIAN_POINT('Ctrl Pts',(3.54718901799994,15.2,-10.410726808));
#161453=CARTESIAN_POINT('Ctrl Pts',(3.54718901799994,11.6,-10.410726808));
#161454=CARTESIAN_POINT('Ctrl Pts',(3.54911009199994,15.2,-10.413114751));
#161455=CARTESIAN_POINT('Ctrl Pts',(3.54911009199994,11.6,-10.413114751));
#161456=CARTESIAN_POINT('Ctrl Pts',(3.55103643899994,15.2,-10.41550526));
#161457=CARTESIAN_POINT('Ctrl Pts',(3.55103643899994,11.6,-10.41550526));
#161458=CARTESIAN_POINT('Ctrl Pts',(3.55296805999994,15.2,-10.417898323));
#161459=CARTESIAN_POINT('Ctrl Pts',(3.55296805999994,11.6,-10.417898323));
#161460=CARTESIAN_POINT('Ctrl Pts',(3.55490495199994,15.2,-10.420293927));
#161461=CARTESIAN_POINT('Ctrl Pts',(3.55490495199994,11.6,-10.420293927));
#161462=CARTESIAN_POINT('Ctrl Pts',(3.55684711799995,15.2,-10.422692061));
#161463=CARTESIAN_POINT('Ctrl Pts',(3.55684711799995,11.6,-10.422692061));
#161464=CARTESIAN_POINT('Ctrl Pts',(3.55879455699994,15.2,-10.425092713));
#161465=CARTESIAN_POINT('Ctrl Pts',(3.55879455699994,11.6,-10.425092713));
#161466=CARTESIAN_POINT('Ctrl Pts',(3.56074726699994,15.2,-10.427495871));
#161467=CARTESIAN_POINT('Ctrl Pts',(3.56074726699994,11.6,-10.427495871));
#161468=CARTESIAN_POINT('Ctrl Pts',(3.56270524999994,15.2,-10.429901524));
#161469=CARTESIAN_POINT('Ctrl Pts',(3.56270524999994,11.6,-10.429901524));
#161470=CARTESIAN_POINT('Ctrl Pts',(3.56466850499995,15.2,-10.432309659));
#161471=CARTESIAN_POINT('Ctrl Pts',(3.56466850499995,11.6,-10.432309659));
#161472=CARTESIAN_POINT('Ctrl Pts',(3.56663703199994,15.2,-10.434720266));
#161473=CARTESIAN_POINT('Ctrl Pts',(3.56663703199994,11.6,-10.434720266));
#161474=CARTESIAN_POINT('Ctrl Pts',(3.56861083099994,15.2,-10.437133332));
#161475=CARTESIAN_POINT('Ctrl Pts',(3.56861083099994,11.6,-10.437133332));
#161476=CARTESIAN_POINT('Ctrl Pts',(3.57058990199994,15.2,-10.439548846));
#161477=CARTESIAN_POINT('Ctrl Pts',(3.57058990199994,11.6,-10.439548846));
#161478=CARTESIAN_POINT('Ctrl Pts',(3.57257424399994,15.2,-10.441966796));
#161479=CARTESIAN_POINT('Ctrl Pts',(3.57257424399994,11.6,-10.441966796));
#161480=CARTESIAN_POINT('Ctrl Pts',(3.57456385699995,15.2,-10.444387171));
#161481=CARTESIAN_POINT('Ctrl Pts',(3.57456385699995,11.6,-10.444387171));
#161482=CARTESIAN_POINT('Ctrl Pts',(3.57655874199994,15.2,-10.446809959));
#161483=CARTESIAN_POINT('Ctrl Pts',(3.57655874199994,11.6,-10.446809959));
#161484=CARTESIAN_POINT('Ctrl Pts',(3.57855889699994,15.2,-10.449235148));
#161485=CARTESIAN_POINT('Ctrl Pts',(3.57855889699994,11.6,-10.449235148));
#161486=CARTESIAN_POINT('Ctrl Pts',(3.58056432299994,15.2,-10.451662727));
#161487=CARTESIAN_POINT('Ctrl Pts',(3.58056432299994,11.6,-10.451662727));
#161488=CARTESIAN_POINT('Ctrl Pts',(3.58257501999994,15.2,-10.454092686));
#161489=CARTESIAN_POINT('Ctrl Pts',(3.58257501999994,11.6,-10.454092686));
#161490=CARTESIAN_POINT('Ctrl Pts',(3.58459098699994,15.2,-10.456525011));
#161491=CARTESIAN_POINT('Ctrl Pts',(3.58459098699994,11.6,-10.456525011));
#161492=CARTESIAN_POINT('Ctrl Pts',(3.58661222399994,15.2,-10.458959692));
#161493=CARTESIAN_POINT('Ctrl Pts',(3.58661222399994,11.6,-10.458959692));
#161494=CARTESIAN_POINT('Ctrl Pts',(3.58863872999994,15.2,-10.461396718));
#161495=CARTESIAN_POINT('Ctrl Pts',(3.58863872999994,11.6,-10.461396718));
#161496=CARTESIAN_POINT('Ctrl Pts',(3.59067050699994,15.2,-10.463836075));
#161497=CARTESIAN_POINT('Ctrl Pts',(3.59067050699994,11.6,-10.463836075));
#161498=CARTESIAN_POINT('Ctrl Pts',(3.59270755199994,15.2,-10.466277755));
#161499=CARTESIAN_POINT('Ctrl Pts',(3.59270755199994,11.6,-10.466277755));
#161500=CARTESIAN_POINT('Ctrl Pts',(3.59474986599994,15.2,-10.468721745));
#161501=CARTESIAN_POINT('Ctrl Pts',(3.59474986599994,11.6,-10.468721745));
#161502=CARTESIAN_POINT('Ctrl Pts',(3.59679744899994,15.2,-10.471168034));
#161503=CARTESIAN_POINT('Ctrl Pts',(3.59679744899994,11.6,-10.471168034));
#161504=CARTESIAN_POINT('Ctrl Pts',(3.59885029999994,15.2,-10.473616611));
#161505=CARTESIAN_POINT('Ctrl Pts',(3.59885029999994,11.6,-10.473616611));
#161506=CARTESIAN_POINT('Ctrl Pts',(3.60090841999994,15.2,-10.476067464));
#161507=CARTESIAN_POINT('Ctrl Pts',(3.60090841999994,11.6,-10.476067464));
#161508=CARTESIAN_POINT('Ctrl Pts',(3.60297180699995,15.2,-10.478520582));
#161509=CARTESIAN_POINT('Ctrl Pts',(3.60297180699995,11.6,-10.478520582));
#161510=CARTESIAN_POINT('Ctrl Pts',(3.60504046199994,15.2,-10.480975954));
#161511=CARTESIAN_POINT('Ctrl Pts',(3.60504046199994,11.6,-10.480975954));
#161512=CARTESIAN_POINT('Ctrl Pts',(3.60711438399994,15.2,-10.483433569));
#161513=CARTESIAN_POINT('Ctrl Pts',(3.60711438399994,11.6,-10.483433569));
#161514=CARTESIAN_POINT('Ctrl Pts',(3.60919357199994,15.2,-10.485893415));
#161515=CARTESIAN_POINT('Ctrl Pts',(3.60919357199994,11.6,-10.485893415));
#161516=CARTESIAN_POINT('Ctrl Pts',(3.61127802799994,15.2,-10.488355482));
#161517=CARTESIAN_POINT('Ctrl Pts',(3.61127802799994,11.6,-10.488355482));
#161518=CARTESIAN_POINT('Ctrl Pts',(3.61336774899994,15.2,-10.490819758));
#161519=CARTESIAN_POINT('Ctrl Pts',(3.61336774899994,11.6,-10.490819758));
#161520=CARTESIAN_POINT('Ctrl Pts',(3.61546273499994,15.2,-10.493286233));
#161521=CARTESIAN_POINT('Ctrl Pts',(3.61546273499994,11.6,-10.493286233));
#161522=CARTESIAN_POINT('Ctrl Pts',(3.61756298799994,15.2,-10.495754894));
#161523=CARTESIAN_POINT('Ctrl Pts',(3.61756298799994,11.6,-10.495754894));
#161524=CARTESIAN_POINT('Ctrl Pts',(3.61966850599994,15.2,-10.498225732));
#161525=CARTESIAN_POINT('Ctrl Pts',(3.61966850599994,11.6,-10.498225732));
#161526=CARTESIAN_POINT('Ctrl Pts',(3.62177928799994,15.2,-10.500698735));
#161527=CARTESIAN_POINT('Ctrl Pts',(3.62177928799994,11.6,-10.500698735));
#161528=CARTESIAN_POINT('Ctrl Pts',(3.62389533499994,15.2,-10.503173891));
#161529=CARTESIAN_POINT('Ctrl Pts',(3.62389533499994,11.6,-10.503173891));
#161530=CARTESIAN_POINT('Ctrl Pts',(3.62601664499994,15.2,-10.505651191));
#161531=CARTESIAN_POINT('Ctrl Pts',(3.62601664499994,11.6,-10.505651191));
#161532=CARTESIAN_POINT('Ctrl Pts',(3.62814321899994,15.2,-10.508130623));
#161533=CARTESIAN_POINT('Ctrl Pts',(3.62814321899994,11.6,-10.508130623));
#161534=CARTESIAN_POINT('Ctrl Pts',(3.63027505499994,15.2,-10.510612176));
#161535=CARTESIAN_POINT('Ctrl Pts',(3.63027505499994,11.6,-10.510612176));
#161536=CARTESIAN_POINT('Ctrl Pts',(3.63241215499994,15.2,-10.513095839));
#161537=CARTESIAN_POINT('Ctrl Pts',(3.63241215499994,11.6,-10.513095839));
#161538=CARTESIAN_POINT('Ctrl Pts',(3.63455451699994,15.2,-10.515581602));
#161539=CARTESIAN_POINT('Ctrl Pts',(3.63455451699994,11.6,-10.515581602));
#161540=CARTESIAN_POINT('Ctrl Pts',(3.63670213999994,15.2,-10.518069453));
#161541=CARTESIAN_POINT('Ctrl Pts',(3.63670213999994,11.6,-10.518069453));
#161542=CARTESIAN_POINT('Ctrl Pts',(3.63885502399994,15.2,-10.520559382));
#161543=CARTESIAN_POINT('Ctrl Pts',(3.63885502399994,11.6,-10.520559382));
#161544=CARTESIAN_POINT('Ctrl Pts',(3.64101316999994,15.2,-10.523051377));
#161545=CARTESIAN_POINT('Ctrl Pts',(3.64101316999994,11.6,-10.523051377));
#161546=CARTESIAN_POINT('Ctrl Pts',(3.64317657699994,15.2,-10.525545429));
#161547=CARTESIAN_POINT('Ctrl Pts',(3.64317657699994,11.6,-10.525545429));
#161548=CARTESIAN_POINT('Ctrl Pts',(3.64534524299994,15.2,-10.528041526));
#161549=CARTESIAN_POINT('Ctrl Pts',(3.64534524299994,11.6,-10.528041526));
#161550=CARTESIAN_POINT('Ctrl Pts',(3.64751916799994,15.2,-10.530539657));
#161551=CARTESIAN_POINT('Ctrl Pts',(3.64751916799994,11.6,-10.530539657));
#161552=CARTESIAN_POINT('Ctrl Pts',(3.64969835399994,15.2,-10.533039812));
#161553=CARTESIAN_POINT('Ctrl Pts',(3.64969835399994,11.6,-10.533039812));
#161554=CARTESIAN_POINT('Ctrl Pts',(3.65188279699994,15.2,-10.53554198));
#161555=CARTESIAN_POINT('Ctrl Pts',(3.65188279699994,11.6,-10.53554198));
#161556=CARTESIAN_POINT('Ctrl Pts',(3.65407249799994,15.2,-10.538046151));
#161557=CARTESIAN_POINT('Ctrl Pts',(3.65407249799994,11.6,-10.538046151));
#161558=CARTESIAN_POINT('Ctrl Pts',(3.65626745699994,15.2,-10.540552312));
#161559=CARTESIAN_POINT('Ctrl Pts',(3.65626745699994,11.6,-10.540552312));
#161560=CARTESIAN_POINT('Ctrl Pts',(3.65846767199994,15.2,-10.543060456));
#161561=CARTESIAN_POINT('Ctrl Pts',(3.65846767199994,11.6,-10.543060456));
#161562=CARTESIAN_POINT('Ctrl Pts',(3.66067314499994,15.2,-10.545570569));
#161563=CARTESIAN_POINT('Ctrl Pts',(3.66067314499994,11.6,-10.545570569));
#161564=CARTESIAN_POINT('Ctrl Pts',(3.66288387299994,15.2,-10.548082642));
#161565=CARTESIAN_POINT('Ctrl Pts',(3.66288387299994,11.6,-10.548082642));
#161566=CARTESIAN_POINT('Ctrl Pts',(3.66509985699994,15.2,-10.550596665));
#161567=CARTESIAN_POINT('Ctrl Pts',(3.66509985699994,11.6,-10.550596665));
#161568=CARTESIAN_POINT('Ctrl Pts',(3.66732109599994,15.2,-10.553112626));
#161569=CARTESIAN_POINT('Ctrl Pts',(3.66732109599994,11.6,-10.553112626));
#161570=CARTESIAN_POINT('Ctrl Pts',(3.66954758799994,15.2,-10.555630515));
#161571=CARTESIAN_POINT('Ctrl Pts',(3.66954758799994,11.6,-10.555630515));
#161572=CARTESIAN_POINT('Ctrl Pts',(3.67177933599994,15.2,-10.558150321));
#161573=CARTESIAN_POINT('Ctrl Pts',(3.67177933599994,11.6,-10.558150321));
#161574=CARTESIAN_POINT('Ctrl Pts',(3.67401633599994,15.2,-10.560672035));
#161575=CARTESIAN_POINT('Ctrl Pts',(3.67401633599994,11.6,-10.560672035));
#161576=CARTESIAN_POINT('Ctrl Pts',(3.67625858899994,15.2,-10.563195645));
#161577=CARTESIAN_POINT('Ctrl Pts',(3.67625858899994,11.6,-10.563195645));
#161578=CARTESIAN_POINT('Ctrl Pts',(3.67850609399994,15.2,-10.565721142));
#161579=CARTESIAN_POINT('Ctrl Pts',(3.67850609399994,11.6,-10.565721142));
#161580=CARTESIAN_POINT('Ctrl Pts',(3.68075885099994,15.2,-10.568248513));
#161581=CARTESIAN_POINT('Ctrl Pts',(3.68075885099994,11.6,-10.568248513));
#161582=CARTESIAN_POINT('Ctrl Pts',(3.68301685699994,15.2,-10.57077775));
#161583=CARTESIAN_POINT('Ctrl Pts',(3.68301685699994,11.6,-10.57077775));
#161584=CARTESIAN_POINT('Ctrl Pts',(3.68528011599994,15.2,-10.573308843));
#161585=CARTESIAN_POINT('Ctrl Pts',(3.68528011599994,11.6,-10.573308843));
#161586=CARTESIAN_POINT('Ctrl Pts',(3.68754862299994,15.2,-10.57584178));
#161587=CARTESIAN_POINT('Ctrl Pts',(3.68754862299994,11.6,-10.57584178));
#161588=CARTESIAN_POINT('Ctrl Pts',(3.68982237999994,15.2,-10.578376549));
#161589=CARTESIAN_POINT('Ctrl Pts',(3.68982237999994,11.6,-10.578376549));
#161590=CARTESIAN_POINT('Ctrl Pts',(3.69210138499994,15.2,-10.580913144));
#161591=CARTESIAN_POINT('Ctrl Pts',(3.69210138499994,11.6,-10.580913144));
#161592=CARTESIAN_POINT('Ctrl Pts',(3.69438563799994,15.2,-10.583451551));
#161593=CARTESIAN_POINT('Ctrl Pts',(3.69438563799994,11.6,-10.583451551));
#161594=CARTESIAN_POINT('Ctrl Pts',(3.69667513799994,15.2,-10.585991763));
#161595=CARTESIAN_POINT('Ctrl Pts',(3.69667513799994,11.6,-10.585991763));
#161596=CARTESIAN_POINT('Ctrl Pts',(3.69896988599994,15.2,-10.588533766));
#161597=CARTESIAN_POINT('Ctrl Pts',(3.69896988599994,11.6,-10.588533766));
#161598=CARTESIAN_POINT('Ctrl Pts',(3.70126987899994,15.2,-10.591077552));
#161599=CARTESIAN_POINT('Ctrl Pts',(3.70126987899994,11.6,-10.591077552));
#161600=CARTESIAN_POINT('Ctrl Pts',(3.70357511699994,15.2,-10.593623111));
#161601=CARTESIAN_POINT('Ctrl Pts',(3.70357511699994,11.6,-10.593623111));
#161602=CARTESIAN_POINT('Ctrl Pts',(3.70588559899994,15.2,-10.596170432));
#161603=CARTESIAN_POINT('Ctrl Pts',(3.70588559899994,11.6,-10.596170432));
#161604=CARTESIAN_POINT('Ctrl Pts',(3.70820132699994,15.2,-10.598719505));
#161605=CARTESIAN_POINT('Ctrl Pts',(3.70820132699994,11.6,-10.598719505));
#161606=CARTESIAN_POINT('Ctrl Pts',(3.71052229599994,15.2,-10.601270319));
#161607=CARTESIAN_POINT('Ctrl Pts',(3.71052229599994,11.6,-10.601270319));
#161608=CARTESIAN_POINT('Ctrl Pts',(3.71284850899994,15.2,-10.603822866));
#161609=CARTESIAN_POINT('Ctrl Pts',(3.71284850899994,11.6,-10.603822866));
#161610=CARTESIAN_POINT('Ctrl Pts',(3.71517996399994,15.2,-10.606377133));
#161611=CARTESIAN_POINT('Ctrl Pts',(3.71517996399994,11.6,-10.606377133));
#161612=CARTESIAN_POINT('Ctrl Pts',(3.71751665899994,15.2,-10.608933112));
#161613=CARTESIAN_POINT('Ctrl Pts',(3.71751665899994,11.6,-10.608933112));
#161614=CARTESIAN_POINT('Ctrl Pts',(3.71985859599994,15.2,-10.611490793));
#161615=CARTESIAN_POINT('Ctrl Pts',(3.71985859599994,11.6,-10.611490793));
#161616=CARTESIAN_POINT('Ctrl Pts',(3.72220577199994,15.2,-10.614050164));
#161617=CARTESIAN_POINT('Ctrl Pts',(3.72220577199994,11.6,-10.614050164));
#161618=CARTESIAN_POINT('Ctrl Pts',(3.72455818799994,15.2,-10.616611217));
#161619=CARTESIAN_POINT('Ctrl Pts',(3.72455818799994,11.6,-10.616611217));
#161620=CARTESIAN_POINT('Ctrl Pts',(3.72691584199994,15.2,-10.61917394));
#161621=CARTESIAN_POINT('Ctrl Pts',(3.72691584199994,11.6,-10.61917394));
#161622=CARTESIAN_POINT('Ctrl Pts',(3.72927873299994,15.2,-10.621738325));
#161623=CARTESIAN_POINT('Ctrl Pts',(3.72927873299994,11.6,-10.621738325));
#161624=CARTESIAN_POINT('Ctrl Pts',(3.73164686099994,15.2,-10.62430436));
#161625=CARTESIAN_POINT('Ctrl Pts',(3.73164686099994,11.6,-10.62430436));
#161626=CARTESIAN_POINT('Ctrl Pts',(3.73402022599994,15.2,-10.626872037));
#161627=CARTESIAN_POINT('Ctrl Pts',(3.73402022599994,11.6,-10.626872037));
#161628=CARTESIAN_POINT('Ctrl Pts',(3.73639882499994,15.2,-10.629441346));
#161629=CARTESIAN_POINT('Ctrl Pts',(3.73639882499994,11.6,-10.629441346));
#161630=CARTESIAN_POINT('Ctrl Pts',(3.73878265999994,15.2,-10.632012274));
#161631=CARTESIAN_POINT('Ctrl Pts',(3.73878265999994,11.6,-10.632012274));
#161632=CARTESIAN_POINT('Ctrl Pts',(3.74117172899994,15.2,-10.634584815));
#161633=CARTESIAN_POINT('Ctrl Pts',(3.74117172899994,11.6,-10.634584815));
#161634=CARTESIAN_POINT('Ctrl Pts',(3.74356602999994,15.2,-10.637158956));
#161635=CARTESIAN_POINT('Ctrl Pts',(3.74356602999994,11.6,-10.637158956));
#161636=CARTESIAN_POINT('Ctrl Pts',(3.74596556399994,15.2,-10.63973469));
#161637=CARTESIAN_POINT('Ctrl Pts',(3.74596556399994,11.6,-10.63973469));
#161638=CARTESIAN_POINT('Ctrl Pts',(3.74837032999995,15.2,-10.642312004));
#161639=CARTESIAN_POINT('Ctrl Pts',(3.74837032999995,11.6,-10.642312004));
#161640=CARTESIAN_POINT('Ctrl Pts',(3.75078032599994,15.2,-10.64489089));
#161641=CARTESIAN_POINT('Ctrl Pts',(3.75078032599994,11.6,-10.64489089));
#161642=CARTESIAN_POINT('Ctrl Pts',(3.75319555299995,15.2,-10.647471338));
#161643=CARTESIAN_POINT('Ctrl Pts',(3.75319555299995,11.6,-10.647471338));
#161644=CARTESIAN_POINT('Ctrl Pts',(3.75561600799994,15.2,-10.650053339));
#161645=CARTESIAN_POINT('Ctrl Pts',(3.75561600799994,11.6,-10.650053339));
#161646=CARTESIAN_POINT('Ctrl Pts',(3.75804169099994,15.2,-10.652636882));
#161647=CARTESIAN_POINT('Ctrl Pts',(3.75804169099994,11.6,-10.652636882));
#161648=CARTESIAN_POINT('Ctrl Pts',(3.76047260299994,15.2,-10.655221957));
#161649=CARTESIAN_POINT('Ctrl Pts',(3.76047260299994,11.6,-10.655221957));
#161650=CARTESIAN_POINT('Ctrl Pts',(3.76290874199994,15.2,-10.657808554));
#161651=CARTESIAN_POINT('Ctrl Pts',(3.76290874199994,11.6,-10.657808554));
#161652=CARTESIAN_POINT('Ctrl Pts',(3.76535010599994,15.2,-10.660396666));
#161653=CARTESIAN_POINT('Ctrl Pts',(3.76535010599994,11.6,-10.660396666));
#161654=CARTESIAN_POINT('Ctrl Pts',(3.76779669499994,15.2,-10.66298628));
#161655=CARTESIAN_POINT('Ctrl Pts',(3.76779669499994,11.6,-10.66298628));
#161656=CARTESIAN_POINT('Ctrl Pts',(3.77024850799994,15.2,-10.665577387));
#161657=CARTESIAN_POINT('Ctrl Pts',(3.77024850799994,11.6,-10.665577387));
#161658=CARTESIAN_POINT('Ctrl Pts',(3.77270554499994,15.2,-10.668169979));
#161659=CARTESIAN_POINT('Ctrl Pts',(3.77270554499994,11.6,-10.668169979));
#161660=CARTESIAN_POINT('Ctrl Pts',(3.77516780399994,15.2,-10.670764045));
#161661=CARTESIAN_POINT('Ctrl Pts',(3.77516780399994,11.6,-10.670764045));
#161662=CARTESIAN_POINT('Ctrl Pts',(3.77763528499994,15.2,-10.673359575));
#161663=CARTESIAN_POINT('Ctrl Pts',(3.77763528499994,11.6,-10.673359575));
#161664=CARTESIAN_POINT('Ctrl Pts',(3.78010798799994,15.2,-10.675956561));
#161665=CARTESIAN_POINT('Ctrl Pts',(3.78010798799994,11.6,-10.675956561));
#161666=CARTESIAN_POINT('Ctrl Pts',(3.78258590899994,15.2,-10.678554991));
#161667=CARTESIAN_POINT('Ctrl Pts',(3.78258590899994,11.6,-10.678554991));
#161668=CARTESIAN_POINT('Ctrl Pts',(3.78506904999994,15.2,-10.681154858));
#161669=CARTESIAN_POINT('Ctrl Pts',(3.78506904999994,11.6,-10.681154858));
#161670=CARTESIAN_POINT('Ctrl Pts',(3.78755740999994,15.2,-10.68375615));
#161671=CARTESIAN_POINT('Ctrl Pts',(3.78755740999994,11.6,-10.68375615));
#161672=CARTESIAN_POINT('Ctrl Pts',(3.79005098599994,15.2,-10.686358859));
#161673=CARTESIAN_POINT('Ctrl Pts',(3.79005098599994,11.6,-10.686358859));
#161674=CARTESIAN_POINT('Ctrl Pts',(3.79254977799994,15.2,-10.688962975));
#161675=CARTESIAN_POINT('Ctrl Pts',(3.79254977799994,11.6,-10.688962975));
#161676=CARTESIAN_POINT('Ctrl Pts',(3.79505378699994,15.2,-10.691568489));
#161677=CARTESIAN_POINT('Ctrl Pts',(3.79505378699994,11.6,-10.691568489));
#161678=CARTESIAN_POINT('Ctrl Pts',(3.79756300899994,15.2,-10.69417539));
#161679=CARTESIAN_POINT('Ctrl Pts',(3.79756300899994,11.6,-10.69417539));
#161680=CARTESIAN_POINT('Ctrl Pts',(3.80007744599994,15.2,-10.696783671));
#161681=CARTESIAN_POINT('Ctrl Pts',(3.80007744599994,11.6,-10.696783671));
#161682=CARTESIAN_POINT('Ctrl Pts',(3.80259709499994,15.2,-10.69939332));
#161683=CARTESIAN_POINT('Ctrl Pts',(3.80259709499994,11.6,-10.69939332));
#161684=CARTESIAN_POINT('Ctrl Pts',(3.80512195499994,15.2,-10.702004329));
#161685=CARTESIAN_POINT('Ctrl Pts',(3.80512195499994,11.6,-10.702004329));
#161686=CARTESIAN_POINT('Ctrl Pts',(3.80765202699994,15.2,-10.704616687));
#161687=CARTESIAN_POINT('Ctrl Pts',(3.80765202699994,11.6,-10.704616687));
#161688=CARTESIAN_POINT('Ctrl Pts',(3.81018730899994,15.2,-10.707230387));
#161689=CARTESIAN_POINT('Ctrl Pts',(3.81018730899994,11.6,-10.707230387));
#161690=CARTESIAN_POINT('Ctrl Pts',(3.81272779999994,15.2,-10.709845418));
#161691=CARTESIAN_POINT('Ctrl Pts',(3.81272779999994,11.6,-10.709845418));
#161692=CARTESIAN_POINT('Ctrl Pts',(3.81527349799994,15.2,-10.712461771));
#161693=CARTESIAN_POINT('Ctrl Pts',(3.81527349799994,11.6,-10.712461771));
#161694=CARTESIAN_POINT('Ctrl Pts',(3.81782440399994,15.2,-10.715079437));
#161695=CARTESIAN_POINT('Ctrl Pts',(3.81782440399994,11.6,-10.715079437));
#161696=CARTESIAN_POINT('Ctrl Pts',(3.82038051599995,15.2,-10.717698405));
#161697=CARTESIAN_POINT('Ctrl Pts',(3.82038051599995,11.6,-10.717698405));
#161698=CARTESIAN_POINT('Ctrl Pts',(3.82294183299994,15.2,-10.720318668));
#161699=CARTESIAN_POINT('Ctrl Pts',(3.82294183299994,11.6,-10.720318668));
#161700=CARTESIAN_POINT('Ctrl Pts',(3.82550835399994,15.2,-10.722940215));
#161701=CARTESIAN_POINT('Ctrl Pts',(3.82550835399994,11.6,-10.722940215));
#161702=CARTESIAN_POINT('Ctrl Pts',(3.82808007799994,15.2,-10.725563038));
#161703=CARTESIAN_POINT('Ctrl Pts',(3.82808007799994,11.6,-10.725563038));
#161704=CARTESIAN_POINT('Ctrl Pts',(3.83065700499994,15.2,-10.728187126));
#161705=CARTESIAN_POINT('Ctrl Pts',(3.83065700499994,11.6,-10.728187126));
#161706=CARTESIAN_POINT('Ctrl Pts',(3.83323913199995,15.2,-10.730812471));
#161707=CARTESIAN_POINT('Ctrl Pts',(3.83323913199995,11.6,-10.730812471));
#161708=CARTESIAN_POINT('Ctrl Pts',(3.83582646099994,15.2,-10.733439064));
#161709=CARTESIAN_POINT('Ctrl Pts',(3.83582646099994,11.6,-10.733439064));
#161710=CARTESIAN_POINT('Ctrl Pts',(3.83841898699994,15.2,-10.736066894));
#161711=CARTESIAN_POINT('Ctrl Pts',(3.83841898699994,11.6,-10.736066894));
#161712=CARTESIAN_POINT('Ctrl Pts',(3.84101671199994,15.2,-10.738695953));
#161713=CARTESIAN_POINT('Ctrl Pts',(3.84101671199994,11.6,-10.738695953));
#161714=CARTESIAN_POINT('Ctrl Pts',(3.84361963499994,15.2,-10.741326232));
#161715=CARTESIAN_POINT('Ctrl Pts',(3.84361963499994,11.6,-10.741326232));
#161716=CARTESIAN_POINT('Ctrl Pts',(3.84622775399994,15.2,-10.743957723));
#161717=CARTESIAN_POINT('Ctrl Pts',(3.84622775399994,11.6,-10.743957723));
#161718=CARTESIAN_POINT('Ctrl Pts',(3.84884106699994,15.2,-10.746590413));
#161719=CARTESIAN_POINT('Ctrl Pts',(3.84884106699994,11.6,-10.746590413));
#161720=CARTESIAN_POINT('Ctrl Pts',(3.85145957499994,15.2,-10.749224299));
#161721=CARTESIAN_POINT('Ctrl Pts',(3.85145957499994,11.6,-10.749224299));
#161722=CARTESIAN_POINT('Ctrl Pts',(3.85408327599994,15.2,-10.751859366));
#161723=CARTESIAN_POINT('Ctrl Pts',(3.85408327599994,11.6,-10.751859366));
#161724=CARTESIAN_POINT('Ctrl Pts',(3.85671216899994,15.2,-10.754495609));
#161725=CARTESIAN_POINT('Ctrl Pts',(3.85671216899994,11.6,-10.754495609));
#161726=CARTESIAN_POINT('Ctrl Pts',(3.85934625299994,15.2,-10.757133015));
#161727=CARTESIAN_POINT('Ctrl Pts',(3.85934625299994,11.6,-10.757133015));
#161728=CARTESIAN_POINT('Ctrl Pts',(3.86198552599994,15.2,-10.759771578));
#161729=CARTESIAN_POINT('Ctrl Pts',(3.86198552599994,11.6,-10.759771578));
#161730=CARTESIAN_POINT('Ctrl Pts',(3.86462998899994,15.2,-10.762411286));
#161731=CARTESIAN_POINT('Ctrl Pts',(3.86462998899994,11.6,-10.762411286));
#161732=CARTESIAN_POINT('Ctrl Pts',(3.86727963799994,15.2,-10.765052131));
#161733=CARTESIAN_POINT('Ctrl Pts',(3.86727963799994,11.6,-10.765052131));
#161734=CARTESIAN_POINT('Ctrl Pts',(3.86993447399994,15.2,-10.767694104));
#161735=CARTESIAN_POINT('Ctrl Pts',(3.86993447399994,11.6,-10.767694104));
#161736=CARTESIAN_POINT('Ctrl Pts',(3.87259449699994,15.2,-10.770337195));
#161737=CARTESIAN_POINT('Ctrl Pts',(3.87259449699994,11.6,-10.770337195));
#161738=CARTESIAN_POINT('Ctrl Pts',(3.87525970299994,15.2,-10.772981398));
#161739=CARTESIAN_POINT('Ctrl Pts',(3.87525970299994,11.6,-10.772981398));
#161740=CARTESIAN_POINT('Ctrl Pts',(3.87793009299994,15.2,-10.775626704));
#161741=CARTESIAN_POINT('Ctrl Pts',(3.87793009299994,11.6,-10.775626704));
#161742=CARTESIAN_POINT('Ctrl Pts',(3.88060566599994,15.2,-10.778273105));
#161743=CARTESIAN_POINT('Ctrl Pts',(3.88060566599994,11.6,-10.778273105));
#161744=CARTESIAN_POINT('Ctrl Pts',(3.88328641999994,15.2,-10.780920592));
#161745=CARTESIAN_POINT('Ctrl Pts',(3.88328641999994,11.6,-10.780920592));
#161746=CARTESIAN_POINT('Ctrl Pts',(3.88597235399994,15.2,-10.783569155));
#161747=CARTESIAN_POINT('Ctrl Pts',(3.88597235399994,11.6,-10.783569155));
#161748=CARTESIAN_POINT('Ctrl Pts',(3.88866346799994,15.2,-10.786218787));
#161749=CARTESIAN_POINT('Ctrl Pts',(3.88866346799994,11.6,-10.786218787));
#161750=CARTESIAN_POINT('Ctrl Pts',(3.89135975899995,15.2,-10.788869473));
#161751=CARTESIAN_POINT('Ctrl Pts',(3.89135975899995,11.6,-10.788869473));
#161752=CARTESIAN_POINT('Ctrl Pts',(3.89406122599994,15.2,-10.791521204));
#161753=CARTESIAN_POINT('Ctrl Pts',(3.89406122599994,11.6,-10.791521204));
#161754=CARTESIAN_POINT('Ctrl Pts',(3.89676786899994,15.2,-10.794173967));
#161755=CARTESIAN_POINT('Ctrl Pts',(3.89676786899994,11.6,-10.794173967));
#161756=CARTESIAN_POINT('Ctrl Pts',(3.89947968399994,15.2,-10.796827756));
#161757=CARTESIAN_POINT('Ctrl Pts',(3.89947968399994,11.6,-10.796827756));
#161758=CARTESIAN_POINT('Ctrl Pts',(3.90219667399994,15.2,-10.79948256));
#161759=CARTESIAN_POINT('Ctrl Pts',(3.90219667399994,11.6,-10.79948256));
#161760=CARTESIAN_POINT('Ctrl Pts',(3.90491883499994,15.2,-10.802138374));
#161761=CARTESIAN_POINT('Ctrl Pts',(3.90491883499994,11.6,-10.802138374));
#161762=CARTESIAN_POINT('Ctrl Pts',(3.90764616599994,15.2,-10.804795195));
#161763=CARTESIAN_POINT('Ctrl Pts',(3.90764616599994,11.6,-10.804795195));
#161764=CARTESIAN_POINT('Ctrl Pts',(3.91037866899994,15.2,-10.807453018));
#161765=CARTESIAN_POINT('Ctrl Pts',(3.91037866899994,11.6,-10.807453018));
#161766=CARTESIAN_POINT('Ctrl Pts',(3.91256880799994,15.2,-10.80958008));
#161767=CARTESIAN_POINT('Ctrl Pts',(3.91256880799994,11.6,-10.80958008));
#161768=CARTESIAN_POINT('Ctrl Pts',(3.91421373899994,15.2,-10.811175827));
#161769=CARTESIAN_POINT('Ctrl Pts',(3.91421373899994,11.6,-10.811175827));
#161770=CARTESIAN_POINT('Ctrl Pts',(3.91531139299994,15.2,-10.812239859));
#161771=CARTESIAN_POINT('Ctrl Pts',(3.91531139299994,11.6,-10.812239859));
#161772=CARTESIAN_POINT('Ctrl Pts',(3.91586047899994,15.2,-10.812771925));
#161773=CARTESIAN_POINT('Ctrl Pts',(3.91586047899994,11.6,-10.812771925));
#161774=CARTESIAN_POINT('Ctrl Pts',(3.20199116199994,15.2,-9.86852965800001));
#161775=CARTESIAN_POINT('Ctrl Pts',(3.20268657132788,15.2,-9.87017542455285));
#161776=CARTESIAN_POINT('Ctrl Pts',(3.20340918399116,15.2,-9.87187175340483));
#161777=CARTESIAN_POINT('Ctrl Pts',(3.20415920994276,15.2,-9.8736175032754));
#161778=CARTESIAN_POINT('Ctrl Pts',(3.20491285289861,15.2,-9.87537167203426));
#161779=CARTESIAN_POINT('Ctrl Pts',(3.20569417410877,15.2,-9.87717573863291));
#161780=CARTESIAN_POINT('Ctrl Pts',(3.20650338986158,15.2,-9.87902857766262));
#161781=CARTESIAN_POINT('Ctrl Pts',(3.2073126055409,15.2,-9.88088141652404));
#161782=CARTESIAN_POINT('Ctrl Pts',(3.20814971062299,15.2,-9.8827830280374));
#161783=CARTESIAN_POINT('Ctrl Pts',(3.20901491150822,15.2,-9.88473231696659));
#161784=CARTESIAN_POINT('Ctrl Pts',(3.20988011239345,15.2,-9.88668160589576));
#161785=CARTESIAN_POINT('Ctrl Pts',(3.21077340789157,15.1999999999999,-9.88867857373555));
#161786=CARTESIAN_POINT('Ctrl Pts',(3.21169499165248,15.2,-9.89072215684402));
#161787=CARTESIAN_POINT('Ctrl Pts',(3.2126165754971,15.2,-9.89276574013813));
#161788=CARTESIAN_POINT('Ctrl Pts',(3.21356644839295,15.2,-9.89485593809657));
#161789=CARTESIAN_POINT('Ctrl Pts',(3.21454479436487,15.2,-9.89699171571608));
#161790=CARTESIAN_POINT('Ctrl Pts',(3.21552314024793,15.2,-9.89912749314159));
#161791=CARTESIAN_POINT('Ctrl Pts',(3.21652996018322,15.2,-9.9013088532216));
#161792=CARTESIAN_POINT('Ctrl Pts',(3.2175654309837,15.2,-9.90353478648428));
#161793=CARTESIAN_POINT('Ctrl Pts',(3.21860090178418,15.2,-9.90576071974695));
#161794=CARTESIAN_POINT('Ctrl Pts',(3.21966502682308,15.2,-9.90803122674332));
#161795=CARTESIAN_POINT('Ctrl Pts',(3.22075797069878,15.2,-9.91034532715734));
#161796=CARTESIAN_POINT('Ctrl Pts',(3.22185091467376,15.2,-9.91265942778154));
#161797=CARTESIAN_POINT('Ctrl Pts',(3.22297268103564,15.2,-9.91501712288619));
#161798=CARTESIAN_POINT('Ctrl Pts',(3.22412343085033,15.2,-9.91741745476992));
#161799=CARTESIAN_POINT('Ctrl Pts',(3.2252741805605,15.2,-9.91981778643561));
#161800=CARTESIAN_POINT('Ctrl Pts',(3.22645391460024,15.2,-9.92226075746568));
#161801=CARTESIAN_POINT('Ctrl Pts',(3.22766278830756,15.2,-9.9247454351272));
#161802=CARTESIAN_POINT('Ctrl Pts',(3.2288716620149,15.2,-9.92723011278871));
#161803=CARTESIAN_POINT('Ctrl Pts',(3.23010967579493,15.2,-9.92975649768857));
#161804=CARTESIAN_POINT('Ctrl Pts',(3.23137697841428,15.2,-9.93232368142687));
#161805=CARTESIAN_POINT('Ctrl Pts',(3.23264428103363,15.2,-9.93489086516516));
#161806=CARTESIAN_POINT('Ctrl Pts',(3.23394087093888,15.2,-9.93749884706859));
#161807=CARTESIAN_POINT('Ctrl Pts',(3.23526689255536,15.2,-9.94014674271966));
#161808=CARTESIAN_POINT('Ctrl Pts',(3.23659291429229,15.2,-9.94279463861126));
#161809=CARTESIAN_POINT('Ctrl Pts',(3.23794836657372,15.2,-9.94548244614007));
#161810=CARTESIAN_POINT('Ctrl Pts',(3.23933338706717,15.2,-9.94820930137372));
#161811=CARTESIAN_POINT('Ctrl Pts',(3.2407184074348,15.2,-9.95093615635967));
#161812=CARTESIAN_POINT('Ctrl Pts',(3.24213299317023,15.2,-9.95370205968793));
#161813=CARTESIAN_POINT('Ctrl Pts',(3.24357727670757,15.2,-9.95650616476535));
#161814=CARTESIAN_POINT('Ctrl Pts',(3.24502156024492,15.2,-9.95931026984277));
#161815=CARTESIAN_POINT('Ctrl Pts',(3.24649554098433,15.2,-9.96215257641826));
#161816=CARTESIAN_POINT('Ctrl Pts',(3.24799934334432,15.2,-9.9650322613944));
#161817=CARTESIAN_POINT('Ctrl Pts',(3.2495031458409,15.2,-9.96791194663211));
#161818=CARTESIAN_POINT('Ctrl Pts',(3.25103676869038,15.2,-9.97082900758185));
#161819=CARTESIAN_POINT('Ctrl Pts',(3.25260033236023,15.2,-9.97378263891107));
#161820=CARTESIAN_POINT('Ctrl Pts',(3.25416389588806,15.2,-9.976736269972));
#161821=CARTESIAN_POINT('Ctrl Pts',(3.25575739965917,15.2,-9.97972646891152));
#161822=CARTESIAN_POINT('Ctrl Pts',(3.25738095602416,15.2,-9.98275245098191));
#161823=CARTESIAN_POINT('Ctrl Pts',(3.25900451238914,15.2,-9.9857784330523));
#161824=CARTESIAN_POINT('Ctrl Pts',(3.2606581221296,15.2,-9.98884019302732));
#161825=CARTESIAN_POINT('Ctrl Pts',(3.26234189356637,15.2,-9.99193696241241));
#161826=CARTESIAN_POINT('Ctrl Pts',(3.26402566515607,15.2,-9.99503373207878));
#161827=CARTESIAN_POINT('Ctrl Pts',(3.26573959839307,15.2,-9.99816551050694));
#161828=CARTESIAN_POINT('Ctrl Pts',(3.26748379516036,15.2,-10.0013315413396));
#161829=CARTESIAN_POINT('Ctrl Pts',(3.26922799176922,15.2,-10.0044975718848));
#161830=CARTESIAN_POINT('Ctrl Pts',(3.27100245227379,15.2,-10.0076978552424));
#161831=CARTESIAN_POINT('Ctrl Pts',(3.27280727645822,15.2,-10.0109316507083));
#161832=CARTESIAN_POINT('Ctrl Pts',(3.27491290478269,15.2,-10.014704412281));
#161833=CARTESIAN_POINT('Ctrl Pts',(3.27705985754708,15.2,-10.0185227891761));
#161834=CARTESIAN_POINT('Ctrl Pts',(3.27924828791476,15.2,-10.0223856295703));
#161835=CARTESIAN_POINT('Ctrl Pts',(3.28112408527542,15.2,-10.0256966354507));
#161836=CARTESIAN_POINT('Ctrl Pts',(3.28303035258691,15.2,-10.0290403112726));
#161837=CARTESIAN_POINT('Ctrl Pts',(3.28496717901655,15.2,-10.0324159479833));
#161838=CARTESIAN_POINT('Ctrl Pts',(3.28722680996841,15.2,-10.0363541910169));
#161839=CARTESIAN_POINT('Ctrl Pts',(3.28952803487752,15.2,-10.0403359358679));
#161840=CARTESIAN_POINT('Ctrl Pts',(3.29187098801924,15.2,-10.044360085342));
#161841=CARTESIAN_POINT('Ctrl Pts',(3.29354452595155,15.2,-10.0472344777788));
#161842=CARTESIAN_POINT('Ctrl Pts',(3.29523935320595,15.2,-10.0501305038409));
#161843=CARTESIAN_POINT('Ctrl Pts',(3.2969555144577,15.2,-10.0530477721065));
#161844=CARTESIAN_POINT('Ctrl Pts',(3.29867167570945,15.2,-10.0559650403722));
#161845=CARTESIAN_POINT('Ctrl Pts',(3.30040917285599,15.2,-10.0589035506631));
#161846=CARTESIAN_POINT('Ctrl Pts',(3.30216804820496,15.2,-10.0618629164287));
#161847=CARTESIAN_POINT('Ctrl Pts',(3.30392692336221,15.2,-10.0648222818718));
#161848=CARTESIAN_POINT('Ctrl Pts',(3.30570717814016,15.2,-10.067802502614));
#161849=CARTESIAN_POINT('Ctrl Pts',(3.3075088524559,15.2,-10.0708031988825));
#161850=CARTESIAN_POINT('Ctrl Pts',(3.30931052696803,15.2,-10.073803895478));
#161851=CARTESIAN_POINT('Ctrl Pts',(3.31113362438261,15.2,-10.0768250666594));
#161852=CARTESIAN_POINT('Ctrl Pts',(3.31297818049196,15.2,-10.0798663383938));
#161853=CARTESIAN_POINT('Ctrl Pts',(3.31482273660131,15.2,-10.0829076101283));
#161854=CARTESIAN_POINT('Ctrl Pts',(3.3166887543436,15.2,-10.0859689831676));
#161855=CARTESIAN_POINT('Ctrl Pts',(3.31857627054752,15.2,-10.0890500876257));
#161856=CARTESIAN_POINT('Ctrl Pts',(3.32046378675144,15.2,-10.0921311920838));
#161857=CARTESIAN_POINT('Ctrl Pts',(3.32237280170266,15.2,-10.0952320288304));
#161858=CARTESIAN_POINT('Ctrl Pts',(3.32430335267376,15.2,-10.0983522340377));
#161859=CARTESIAN_POINT('Ctrl Pts',(3.32623390364487,15.2,-10.101472439245));
#161860=CARTESIAN_POINT('Ctrl Pts',(3.32818598907207,15.2,-10.1046120134278));
#161861=CARTESIAN_POINT('Ctrl Pts',(3.33015964511261,15.2,-10.1077706000935));
#161862=CARTESIAN_POINT('Ctrl Pts',(3.33213330115316,15.2,-10.1109291867592));
#161863=CARTESIAN_POINT('Ctrl Pts',(3.33412852699525,15.2,-10.1141067834615));
#161864=CARTESIAN_POINT('Ctrl Pts',(3.33614535624046,15.2,-10.1173030402816));
#161865=CARTESIAN_POINT('Ctrl Pts',(3.33816218548567,15.2,-10.1204992971016));
#161866=CARTESIAN_POINT('Ctrl Pts',(3.34020061572211,15.2,-10.1237142122666));
#161867=CARTESIAN_POINT('Ctrl Pts',(3.34226068245822,15.2,-10.126947439975));
#161868=CARTESIAN_POINT('Ctrl Pts',(3.34432074919432,15.2,-10.1301806676833));
#161869=CARTESIAN_POINT('Ctrl Pts',(3.34640244882476,15.2,-10.1334322079591));
#161870=CARTESIAN_POINT('Ctrl Pts',(3.34850581320937,15.2,-10.1367017182518));
#161871=CARTESIAN_POINT('Ctrl Pts',(3.35060917759399,15.2,-10.1399712285444));
#161872=CARTESIAN_POINT('Ctrl Pts',(3.3527342059504,15.2,-10.1432587085264));
#161873=CARTESIAN_POINT('Ctrl Pts',(3.35488092609042,15.2,-10.1465638219996));
#161874=CARTESIAN_POINT('Ctrl Pts',(3.35702764623043,15.2,-10.1498689354727));
#161875=CARTESIAN_POINT('Ctrl Pts',(3.35919605986436,15.2,-10.1531916819787));
#161876=CARTESIAN_POINT('Ctrl Pts',(3.36138619014326,15.2,-10.1565317289935));
#161877=CARTESIAN_POINT('Ctrl Pts',(3.36357632042216,15.2,-10.1598717760083));
#161878=CARTESIAN_POINT('Ctrl Pts',(3.36578817010052,15.2,-10.163229122581));
#161879=CARTESIAN_POINT('Ctrl Pts',(3.36802176287943,15.2,-10.1666034429291));
#161880=CARTESIAN_POINT('Ctrl Pts',(3.37025535565835,15.2,-10.1699777632772));
#161881=CARTESIAN_POINT('Ctrl Pts',(3.3725106926157,15.2,-10.1733690568298));
#161882=CARTESIAN_POINT('Ctrl Pts',(3.37478779627264,15.2,-10.1767770006123));
#161883=CARTESIAN_POINT('Ctrl Pts',(3.37706489992957,15.2,-10.1801849443948));
#161884=CARTESIAN_POINT('Ctrl Pts',(3.37936377073499,15.2,-10.1836095356154));
#161885=CARTESIAN_POINT('Ctrl Pts',(3.3816844315701,15.2,-10.1870504599917));
#161886=CARTESIAN_POINT('Ctrl Pts',(3.38354096008642,15.2,-10.1898031992677));
#161887=CARTESIAN_POINT('Ctrl Pts',(3.38541143248982,15.2,-10.1925663900674));
#161888=CARTESIAN_POINT('Ctrl Pts',(3.38729586111264,15.2,-10.1953398715067));
#161889=CARTESIAN_POINT('Ctrl Pts',(3.38918028999221,15.2,-10.1981133533238));
#161890=CARTESIAN_POINT('Ctrl Pts',(3.39107867482927,15.2,-10.2008971244294));
#161891=CARTESIAN_POINT('Ctrl Pts',(3.39299102575246,15.2,-10.2036910283888));
#161892=CARTESIAN_POINT('Ctrl Pts',(3.3949033764151,15.2,-10.2064849319675));
#161893=CARTESIAN_POINT('Ctrl Pts',(3.39682969290649,15.2,-10.2092889664507));
#161894=CARTESIAN_POINT('Ctrl Pts',(3.39876998485807,15.2,-10.2121029745534));
#161895=CARTESIAN_POINT('Ctrl Pts',(3.40071027707402,15.2,-10.2149169830394));
#161896=CARTESIAN_POINT('Ctrl Pts',(3.40266454439163,15.2,-10.2177409650683));
#161897=CARTESIAN_POINT('Ctrl Pts',(3.40463279594426,15.2,-10.2205747637234));
#161898=CARTESIAN_POINT('Ctrl Pts',(3.40660104722872,15.2,-10.2234085619924));
#161899=CARTESIAN_POINT('Ctrl Pts',(3.4085832837472,15.2,-10.2262521788303));
#161900=CARTESIAN_POINT('Ctrl Pts',(3.4105795124603,15.2,-10.2291054571277));
#161901=CARTESIAN_POINT('Ctrl Pts',(3.41257574144538,15.2,-10.2319587358138));
#161902=CARTESIAN_POINT('Ctrl Pts',(3.4145859632265,15.2,-10.23482167725));
#161903=CARTESIAN_POINT('Ctrl Pts',(3.4166101861155,15.2,-10.2376941291849));
#161904=CARTESIAN_POINT('Ctrl Pts',(3.41863440872871,15.2,-10.2405665807285));
#161905=CARTESIAN_POINT('Ctrl Pts',(3.42067263186689,15.2,-10.243448542084));
#161906=CARTESIAN_POINT('Ctrl Pts',(3.42272486369769,15.2,-10.2463398615689));
#161907=CARTESIAN_POINT('Ctrl Pts',(3.42477709580811,15.2,-10.2492311814478));
#161908=CARTESIAN_POINT('Ctrl Pts',(3.42684333565066,15.2,-10.252131859419));
#161909=CARTESIAN_POINT('Ctrl Pts',(3.42892359055131,15.2,-10.255041746702));
#161910=CARTESIAN_POINT('Ctrl Pts',(3.43100384516853,15.2,-10.2579516335884));
#161911=CARTESIAN_POINT('Ctrl Pts',(3.43309811644008,15.2,-10.2608707295837));
#161912=CARTESIAN_POINT('Ctrl Pts',(3.43520640715519,15.2,-10.2637988857879));
#161913=CARTESIAN_POINT('Ctrl Pts',(3.43731469815756,15.2,-10.266727042391));
#161914=CARTESIAN_POINT('Ctrl Pts',(3.43943701145012,15.2,-10.2696642583616));
#161915=CARTESIAN_POINT('Ctrl Pts',(3.44157335223322,15.2,-10.2726103889666));
#161916=CARTESIAN_POINT('Ctrl Pts',(3.44370969301631,15.2,-10.2755565195716));
#161917=CARTESIAN_POINT('Ctrl Pts',(3.44586005991494,15.2,-10.2785115634499));
#161918=CARTESIAN_POINT('Ctrl Pts',(3.44802446131211,15.2,-10.2814753755012));
#161919=CARTESIAN_POINT('Ctrl Pts',(3.45018886241438,15.2,-10.2844391871487));
#161920=CARTESIAN_POINT('Ctrl Pts',(3.45236729506773,15.2,-10.2874117680198));
#161921=CARTESIAN_POINT('Ctrl Pts',(3.45455976623173,15.2,-10.2903929722896));
#161922=CARTESIAN_POINT('Ctrl Pts',(3.45675223769445,15.2,-10.2933741769656));
#161923=CARTESIAN_POINT('Ctrl Pts',(3.45895874696272,15.2,-10.2963640061898));
#161924=CARTESIAN_POINT('Ctrl Pts',(3.46117929786295,15.2,-10.2993623169652));
#161925=CARTESIAN_POINT('Ctrl Pts',(3.46339984846063,15.2,-10.3023606273321));
#161926=CARTESIAN_POINT('Ctrl Pts',(3.46563444193705,15.2,-10.3053674200062));
#161927=CARTESIAN_POINT('Ctrl Pts',(3.46788308114119,15.2,-10.3083825535369));
#161928=CARTESIAN_POINT('Ctrl Pts',(3.47013172065172,15.2,-10.3113976874785));
#161929=CARTESIAN_POINT('Ctrl Pts',(3.47239440600795,15.2,-10.3144211607781));
#161930=CARTESIAN_POINT('Ctrl Pts',(3.47467114158033,15.2,-10.3174528362066));
#161931=CARTESIAN_POINT('Ctrl Pts',(3.47694787684251,15.2,-10.3204845112221));
#161932=CARTESIAN_POINT('Ctrl Pts',(3.47923866260649,15.2,-10.3235243868617));
#161933=CARTESIAN_POINT('Ctrl Pts',(3.4815434998616,15.2,-10.3265723245009));
#161934=CARTESIAN_POINT('Ctrl Pts',(3.48384833743075,15.2,-10.3296202625554));
#161935=CARTESIAN_POINT('Ctrl Pts',(3.48616722836268,15.2,-10.3326762629608));
#161936=CARTESIAN_POINT('Ctrl Pts',(3.48850017449074,15.2,-10.3357401890172));
#161937=CARTESIAN_POINT('Ctrl Pts',(3.49083312030094,15.2,-10.3388041146561));
#161938=CARTESIAN_POINT('Ctrl Pts',(3.49318012189196,15.2,-10.3418759643461));
#161939=CARTESIAN_POINT('Ctrl Pts',(3.49554118064903,15.2,-10.3449556048032));
#161940=CARTESIAN_POINT('Ctrl Pts',(3.4979022397278,15.2,-10.3480352456798));
#161941=CARTESIAN_POINT('Ctrl Pts',(3.50027735801699,15.2,-10.3511226752617));
#161942=CARTESIAN_POINT('Ctrl Pts',(3.50266653420367,15.2,-10.3542177599864));
#161943=CARTESIAN_POINT('Ctrl Pts',(3.50505571006482,15.2,-10.3573128442894));
#161944=CARTESIAN_POINT('Ctrl Pts',(3.50745894632316,15.2,-10.3604155831493));
#161945=CARTESIAN_POINT('Ctrl Pts',(3.50987624284634,15.2,-10.3635258429498));
#161946=CARTESIAN_POINT('Ctrl Pts',(3.51229353969887,15.2,-10.3666361031741));
#161947=CARTESIAN_POINT('Ctrl Pts',(3.51472489722379,15.2,-10.3697538858481));
#161948=CARTESIAN_POINT('Ctrl Pts',(3.51717031670156,15.2,-10.3728790573104));
#161949=CARTESIAN_POINT('Ctrl Pts',(3.51961573584613,15.2,-10.376004228347));
#161950=CARTESIAN_POINT('Ctrl Pts',(3.52207521766857,15.2,-10.3791367876413));
#161951=CARTESIAN_POINT('Ctrl Pts',(3.52454876085381,15.2,-10.382276605995));
#161952=CARTESIAN_POINT('Ctrl Pts',(3.52702230437607,15.2,-10.3854164247765));
#161953=CARTESIAN_POINT('Ctrl Pts',(3.52950990996076,15.2,-10.3885635012531));
#161954=CARTESIAN_POINT('Ctrl Pts',(3.53201157870822,15.2,-10.3917177072583));
#161955=CARTESIAN_POINT('Ctrl Pts',(3.53451324745567,15.2,-10.3948719132636));
#161956=CARTESIAN_POINT('Ctrl Pts',(3.53702897803809,15.2,-10.3980332468168));
#161957=CARTESIAN_POINT('Ctrl Pts',(3.53955877145519,15.2,-10.401201579768));
#161958=CARTESIAN_POINT('Ctrl Pts',(3.54272101305421,15.2,-10.4051619957411));
#161959=CARTESIAN_POINT('Ctrl Pts',(3.54590522643969,15.2,-10.4091333511977));
#161960=CARTESIAN_POINT('Ctrl Pts',(3.5491114106776,15.2,-10.4131153930042));
#161961=CARTESIAN_POINT('Ctrl Pts',(3.55167635785825,15.2,-10.4163010261889));
#161962=CARTESIAN_POINT('Ctrl Pts',(3.55425536660671,15.2,-10.4194935014115));
#161963=CARTESIAN_POINT('Ctrl Pts',(3.55684843623979,15.2,-10.4226926904978));
#161964=CARTESIAN_POINT('Ctrl Pts',(3.55944150622618,15.2,-10.42589188002));
#161965=CARTESIAN_POINT('Ctrl Pts',(3.56204863528416,15.2,-10.4290977839356));
#161966=CARTESIAN_POINT('Ctrl Pts',(3.56466982342846,15.2,-10.4323102775002));
#161967=CARTESIAN_POINT('Ctrl Pts',(3.56729101121562,15.2,-10.4355227706272));
#161968=CARTESIAN_POINT('Ctrl Pts',(3.56992625837039,15.2,-10.4387418535199));
#161969=CARTESIAN_POINT('Ctrl Pts',(3.57257556154178,15.2,-10.441967401978));
#161970=CARTESIAN_POINT('Ctrl Pts',(3.57522486507413,15.2,-10.4451929508756));
#161971=CARTESIAN_POINT('Ctrl Pts',(3.57788822557147,15.2,-10.4484249647644));
#161972=CARTESIAN_POINT('Ctrl Pts',(3.58056564113014,15.2,-10.4516633224366));
#161973=CARTESIAN_POINT('Ctrl Pts',(3.58324305632402,15.2,-10.4549016796675));
#161974=CARTESIAN_POINT('Ctrl Pts',(3.58593452576483,15.2,-10.4581463800227));
#161975=CARTESIAN_POINT('Ctrl Pts',(3.58864004748718,15.2,-10.4613973005343));
#161976=CARTESIAN_POINT('Ctrl Pts',(3.59134556957816,15.2,-10.4646482214888));
#161977=CARTESIAN_POINT('Ctrl Pts',(3.59406514342359,15.2,-10.467905363358));
#161978=CARTESIAN_POINT('Ctrl Pts',(3.59679876624016,15.2,-10.4711686062585));
#161979=CARTESIAN_POINT('Ctrl Pts',(3.59953238868429,15.2,-10.4744318487143));
#161980=CARTESIAN_POINT('Ctrl Pts',(3.60228006054934,15.2,-10.4777011909822));
#161981=CARTESIAN_POINT('Ctrl Pts',(3.60504177834923,15.2,-10.4809765142664));
#161982=CARTESIAN_POINT('Ctrl Pts',(3.6078034965254,15.2,-10.484251837997));
#161983=CARTESIAN_POINT('Ctrl Pts',(3.61057926056401,15.2,-10.4875331417587));
#161984=CARTESIAN_POINT('Ctrl Pts',(3.61336906549476,15.2,-10.4908203079938));
#161985=CARTESIAN_POINT('Ctrl Pts',(3.61615887004539,15.2,-10.494107473781));
#161986=CARTESIAN_POINT('Ctrl Pts',(3.61896271805152,15.2,-10.4974005015059));
#161987=CARTESIAN_POINT('Ctrl Pts',(3.62178060376417,15.2,-10.5006992727356));
#161988=CARTESIAN_POINT('Ctrl Pts',(3.62459848986076,15.2,-10.5039980444149));
#161989=CARTESIAN_POINT('Ctrl Pts',(3.62743041346709,15.2,-10.5073025604818));
#161990=CARTESIAN_POINT('Ctrl Pts',(3.6302763709685,15.2,-10.5106127035106));
#161991=CARTESIAN_POINT('Ctrl Pts',(3.63312232808215,15.2,-10.5139228460884));
#161992=CARTESIAN_POINT('Ctrl Pts',(3.6359823192497,15.2,-10.517238616754));
#161993=CARTESIAN_POINT('Ctrl Pts',(3.63885633901333,15.2,-10.520559897982));
#161994=CARTESIAN_POINT('Ctrl Pts',(3.64173035916854,15.2,-10.5238811796624));
#161995=CARTESIAN_POINT('Ctrl Pts',(3.64461840915283,15.2,-10.5272079733101));
#161996=CARTESIAN_POINT('Ctrl Pts',(3.64752048319988,15.2,-10.5305401629917));
#161997=CARTESIAN_POINT('Ctrl Pts',(3.65042255724694,15.2,-10.5338723526733));
#161998=CARTESIAN_POINT('Ctrl Pts',(3.65333865535118,15.2,-10.5372099392222));
#161999=CARTESIAN_POINT('Ctrl Pts',(3.6562687715123,15.2,-10.5405528082382));
#162000=CARTESIAN_POINT('Ctrl Pts',(3.65846635843353,15.2,-10.5430599597725));
#162001=CARTESIAN_POINT('Ctrl Pts',(3.66067183138046,15.2,-10.5455700828517));
#162002=CARTESIAN_POINT('Ctrl Pts',(3.66288518741153,15.2,-10.5480831299696));
#162003=CARTESIAN_POINT('Ctrl Pts',(3.6650985434426,15.2,-10.5505961770875));
#162004=CARTESIAN_POINT('Ctrl Pts',(3.66731978230663,15.2,-10.5531121479659));
#162005=CARTESIAN_POINT('Ctrl Pts',(3.66954890218466,15.2,-10.5556309945413));
#162006=CARTESIAN_POINT('Ctrl Pts',(3.6717780220627,15.2,-10.5581498411167));
#162007=CARTESIAN_POINT('Ctrl Pts',(3.67401502313145,15.2,-10.560671564225));
#162008=CARTESIAN_POINT('Ctrl Pts',(3.67625990200822,15.2,-10.5631961167167));
#162009=CARTESIAN_POINT('Ctrl Pts',(3.67850478088499,15.2,-10.5657206692083));
#162010=CARTESIAN_POINT('Ctrl Pts',(3.6807575375531,15.2,-10.5682480497164));
#162011=CARTESIAN_POINT('Ctrl Pts',(3.68301816992861,15.2,-10.5707782137076));
#162012=CARTESIAN_POINT('Ctrl Pts',(3.68527880230413,15.2,-10.5733083776987));
#162013=CARTESIAN_POINT('Ctrl Pts',(3.68754731062943,15.2,-10.5758413237418));
#162014=CARTESIAN_POINT('Ctrl Pts',(3.68982369157621,15.2,-10.5783770049428));
#162015=CARTESIAN_POINT('Ctrl Pts',(3.692100072523,15.2,-10.5809126861437));
#162016=CARTESIAN_POINT('Ctrl Pts',(3.69438432563456,15.2,-10.5834511037554));
#162017=CARTESIAN_POINT('Ctrl Pts',(3.69667644946688,15.2,-10.585992210246));
#162018=CARTESIAN_POINT('Ctrl Pts',(3.6989685737156,15.2,-10.5885333171983));
#162019=CARTESIAN_POINT('Ctrl Pts',(3.70126856814986,15.2,-10.591077112568));
#162020=CARTESIAN_POINT('Ctrl Pts',(3.70357642852801,15.2,-10.5936235520635));
#162021=CARTESIAN_POINT('Ctrl Pts',(3.7058842884869,15.2,-10.5961699910963));
#162022=CARTESIAN_POINT('Ctrl Pts',(3.7082000162537,15.2,-10.598719072954));
#162023=CARTESIAN_POINT('Ctrl Pts',(3.71052360721163,15.2,-10.6012707524865));
#162024=CARTESIAN_POINT('Ctrl Pts',(3.71284719816956,15.2,-10.603822432019));
#162025=CARTESIAN_POINT('Ctrl Pts',(3.71517865357636,15.2,-10.6063767084836));
#162026=CARTESIAN_POINT('Ctrl Pts',(3.71751796946035,15.2,-10.6089335374856));
#162027=CARTESIAN_POINT('Ctrl Pts',(3.71985728534434,15.2,-10.6114903664877));
#162028=CARTESIAN_POINT('Ctrl Pts',(3.722204462706,15.2,-10.6140497474458));
#162029=CARTESIAN_POINT('Ctrl Pts',(3.72455949750608,15.2,-10.616611634531));
#162030=CARTESIAN_POINT('Ctrl Pts',(3.72691453230618,15.2,-10.6191735216162));
#162031=CARTESIAN_POINT('Ctrl Pts',(3.72927742367842,15.2,-10.621737915047));
#162032=CARTESIAN_POINT('Ctrl Pts',(3.73164816996661,15.2,-10.6243047702036));
#162033=CARTESIAN_POINT('Ctrl Pts',(3.7340189162548,15.2,-10.6268716253601));
#162034=CARTESIAN_POINT('Ctrl Pts',(3.73639751623409,15.2,-10.6294409430165));
#162035=CARTESIAN_POINT('Ctrl Pts',(3.73878396797965,15.2,-10.632012676631));
#162036=CARTESIAN_POINT('Ctrl Pts',(3.74117042015876,15.2,-10.6345844107128));
#162037=CARTESIAN_POINT('Ctrl Pts',(3.74356472229005,15.2,-10.6371585621036));
#162038=CARTESIAN_POINT('Ctrl Pts',(3.74596687251523,15.2,-10.6397350856033));
#162039=CARTESIAN_POINT('Ctrl Pts',(3.74836902230402,15.2,-10.6423116086351));
#162040=CARTESIAN_POINT('Ctrl Pts',(3.7507790195839,15.2,-10.6448905030306));
#162041=CARTESIAN_POINT('Ctrl Pts',(3.75319686049276,15.2,-10.6474717267328));
#162042=CARTESIAN_POINT('Ctrl Pts',(3.75561470140162,15.2,-10.6500529504349));
#162043=CARTESIAN_POINT('Ctrl Pts',(3.75804038476968,15.2,-10.652636502609));
#162044=CARTESIAN_POINT('Ctrl Pts',(3.76047391001527,15.2,-10.6552223378069));
#162045=CARTESIAN_POINT('Ctrl Pts',(3.76290743526087,15.2,-10.6578081730048));
#162046=CARTESIAN_POINT('Ctrl Pts',(3.76534880013888,15.2,-10.6603962935608));
#162047=CARTESIAN_POINT('Ctrl Pts',(3.76779800100822,15.2,-10.6629866532583));
#162048=CARTESIAN_POINT('Ctrl Pts',(3.77024720187756,15.2,-10.6655770129559));
#162049=CARTESIAN_POINT('Ctrl Pts',(3.77270423932158,15.2,-10.6681696135783));
#162050=CARTESIAN_POINT('Ctrl Pts',(3.77516910923135,15.2,-10.6707644107339));
#162051=CARTESIAN_POINT('Ctrl Pts',(3.77763397914112,15.2,-10.6733592078894));
#162052=CARTESIAN_POINT('Ctrl Pts',(3.78010668248367,15.2,-10.6759562020281));
#162053=CARTESIAN_POINT('Ctrl Pts',(3.78258721343414,15.2,-10.6785553496417));
#162054=CARTESIAN_POINT('Ctrl Pts',(3.78506774483524,15.2,-10.6811544977275));
#162055=CARTESIAN_POINT('Ctrl Pts',(3.78755610614688,15.2,-10.6837557992389));
#162056=CARTESIAN_POINT('Ctrl Pts',(3.7900522905524,15.2,-10.6863592113259));
#162057=CARTESIAN_POINT('Ctrl Pts',(3.79254847450444,15.2,-10.6889626229399));
#162058=CARTESIAN_POINT('Ctrl Pts',(3.79505248370082,15.2,-10.6915681452188));
#162059=CARTESIAN_POINT('Ctrl Pts',(3.79756431319427,15.2,-10.6941757354629));
#162060=CARTESIAN_POINT('Ctrl Pts',(3.80007614268773,15.2,-10.6967833257069));
#162061=CARTESIAN_POINT('Ctrl Pts',(3.80259579238333,15.2,-10.6993929839127));
#162062=CARTESIAN_POINT('Ctrl Pts',(3.80512325825051,15.2,-10.702004666568));
#162063=CARTESIAN_POINT('Ctrl Pts',(3.80765072411769,15.2,-10.7046163492233));
#162064=CARTESIAN_POINT('Ctrl Pts',(3.81018600740895,15.2,-10.707230057345));
#162065=CARTESIAN_POINT('Ctrl Pts',(3.81272910177488,15.2,-10.7098457485));
#162066=CARTESIAN_POINT('Ctrl Pts',(3.81527219614082,15.2,-10.712461439655));
#162067=CARTESIAN_POINT('Ctrl Pts',(3.8178231026481,15.2,-10.7150791137765));
#162068=CARTESIAN_POINT('Ctrl Pts',(3.82038181697112,15.2,-10.7176987284312));
#162069=CARTESIAN_POINT('Ctrl Pts',(3.82294053129414,15.2,-10.7203183430858));
#162070=CARTESIAN_POINT('Ctrl Pts',(3.82550705281773,15.2,-10.7229398990236));
#162071=CARTESIAN_POINT('Ctrl Pts',(3.8280813782269,15.2,-10.7255633537674));
#162072=CARTESIAN_POINT('Ctrl Pts',(3.83065570363607,15.2,-10.7281868085113));
#162073=CARTESIAN_POINT('Ctrl Pts',(3.83323783246379,15.2,-10.7308121620896));
#162074=CARTESIAN_POINT('Ctrl Pts',(3.83582775974363,15.2,-10.7334393727023));
#162075=CARTESIAN_POINT('Ctrl Pts',(3.83841768749397,15.2,-10.7360665837922));
#162076=CARTESIAN_POINT('Ctrl Pts',(3.84101541335483,15.2,-10.7386956510243));
#162077=CARTESIAN_POINT('Ctrl Pts',(3.8436209345679,15.2,-10.7413265355319));
#162078=CARTESIAN_POINT('Ctrl Pts',(3.84622645530763,15.2,-10.7439574195615));
#162079=CARTESIAN_POINT('Ctrl Pts',(3.84883976926361,15.2,-10.7465901190494));
#162080=CARTESIAN_POINT('Ctrl Pts',(3.85146087354406,15.2,-10.7492245946205));
#162081=CARTESIAN_POINT('Ctrl Pts',(3.8540819778245,15.2,-10.7518590701916));
#162082=CARTESIAN_POINT('Ctrl Pts',(3.85671087190274,15.2,-10.7544953205363));
#162083=CARTESIAN_POINT('Ctrl Pts',(3.85934755027729,15.2,-10.7571333042024));
#162084=CARTESIAN_POINT('Ctrl Pts',(3.86198422865183,15.2,-10.7597712878685));
#162085=CARTESIAN_POINT('Ctrl Pts',(3.86462869228184,15.2,-10.7624110048649));
#162086=CARTESIAN_POINT('Ctrl Pts',(3.86728093473915,15.2,-10.7650524129893));
#162087=CARTESIAN_POINT('Ctrl Pts',(3.86993317719647,15.2,-10.7676938211136));
#162088=CARTESIAN_POINT('Ctrl Pts',(3.87259320079017,15.2,-10.7703369197747));
#162089=CARTESIAN_POINT('Ctrl Pts',(3.87526099869257,15.2,-10.7729816734701));
#162090=CARTESIAN_POINT('Ctrl Pts',(3.87792879659497,15.2,-10.7756264271655));
#162091=CARTESIAN_POINT('Ctrl Pts',(3.88060437056348,15.2,-10.7782728362525));
#162092=CARTESIAN_POINT('Ctrl Pts',(3.88328771442326,15.2,-10.7809208604477));
#162093=CARTESIAN_POINT('Ctrl Pts',(3.88597105877052,15.2,-10.783568885124));
#162094=CARTESIAN_POINT('Ctrl Pts',(3.88866217424496,15.2,-10.7862185268258));
#162095=CARTESIAN_POINT('Ctrl Pts',(3.89136105359659,15.2,-10.7888697347946));
#162096=CARTESIAN_POINT('Ctrl Pts',(3.89405993245792,15.2,-10.7915209422819));
#162097=CARTESIAN_POINT('Ctrl Pts',(3.89676657572058,15.2,-10.7941737144439));
#162098=CARTESIAN_POINT('Ctrl Pts',(3.8994809782168,15.2,-10.7968280103136));
#162099=CARTESIAN_POINT('Ctrl Pts',(3.90219538071302,15.2,-10.7994823061832));
#162100=CARTESIAN_POINT('Ctrl Pts',(3.90491754234274,15.2,-10.8021381240576));
#162101=CARTESIAN_POINT('Ctrl Pts',(3.90764745926926,15.2,-10.804795445851));
#162102=CARTESIAN_POINT('Ctrl Pts',(3.91037737619578,15.2,-10.8074527676443));
#162103=CARTESIAN_POINT('Ctrl Pts',(3.91311504850119,15.2,-10.8101115945167));
#162104=CARTESIAN_POINT('Ctrl Pts',(3.91586047899994,15.2,-10.812771925));
#162105=CARTESIAN_POINT('Ctrl Pts',(3.20199116199994,12.2,-9.86852965800001));
#162106=CARTESIAN_POINT('Ctrl Pts',(3.20268657132788,12.2,-9.87017542455285));
#162107=CARTESIAN_POINT('Ctrl Pts',(3.20340918399116,12.2,-9.87187175340483));
#162108=CARTESIAN_POINT('Ctrl Pts',(3.20415920994276,12.2,-9.8736175032754));
#162109=CARTESIAN_POINT('Ctrl Pts',(3.20491285289861,12.2,-9.87537167203426));
#162110=CARTESIAN_POINT('Ctrl Pts',(3.20569417410877,12.2,-9.87717573863291));
#162111=CARTESIAN_POINT('Ctrl Pts',(3.20650338986158,12.2,-9.87902857766262));
#162112=CARTESIAN_POINT('Ctrl Pts',(3.2073126055409,12.2,-9.88088141652404));
#162113=CARTESIAN_POINT('Ctrl Pts',(3.20814971062299,12.2,-9.8827830280374));
#162114=CARTESIAN_POINT('Ctrl Pts',(3.20901491150822,12.2,-9.88473231696659));
#162115=CARTESIAN_POINT('Ctrl Pts',(3.20988011239345,12.2,-9.88668160589576));
#162116=CARTESIAN_POINT('Ctrl Pts',(3.21077340789157,12.2,-9.88867857373555));
#162117=CARTESIAN_POINT('Ctrl Pts',(3.21169499165248,12.2,-9.89072215684402));
#162118=CARTESIAN_POINT('Ctrl Pts',(3.2126165754971,12.2,-9.89276574013813));
#162119=CARTESIAN_POINT('Ctrl Pts',(3.21356644839295,12.2,-9.89485593809657));
#162120=CARTESIAN_POINT('Ctrl Pts',(3.21454479436487,12.2,-9.89699171571608));
#162121=CARTESIAN_POINT('Ctrl Pts',(3.21552314024793,12.2,-9.89912749314159));
#162122=CARTESIAN_POINT('Ctrl Pts',(3.21652996018322,12.2,-9.9013088532216));
#162123=CARTESIAN_POINT('Ctrl Pts',(3.2175654309837,12.2,-9.90353478648428));
#162124=CARTESIAN_POINT('Ctrl Pts',(3.21860090178418,12.2,-9.90576071974695));
#162125=CARTESIAN_POINT('Ctrl Pts',(3.21966502682308,12.2,-9.90803122674332));
#162126=CARTESIAN_POINT('Ctrl Pts',(3.22075797069878,12.2,-9.91034532715734));
#162127=CARTESIAN_POINT('Ctrl Pts',(3.22185091467376,12.2,-9.91265942778154));
#162128=CARTESIAN_POINT('Ctrl Pts',(3.22297268103564,12.2,-9.91501712288619));
#162129=CARTESIAN_POINT('Ctrl Pts',(3.22412343085033,12.2,-9.91741745476992));
#162130=CARTESIAN_POINT('Ctrl Pts',(3.2252741805605,12.2,-9.91981778643561));
#162131=CARTESIAN_POINT('Ctrl Pts',(3.22645391460024,12.2,-9.92226075746568));
#162132=CARTESIAN_POINT('Ctrl Pts',(3.22766278830756,12.2,-9.9247454351272));
#162133=CARTESIAN_POINT('Ctrl Pts',(3.2288716620149,12.2,-9.92723011278871));
#162134=CARTESIAN_POINT('Ctrl Pts',(3.23010967579493,12.2,-9.92975649768857));
#162135=CARTESIAN_POINT('Ctrl Pts',(3.23137697841428,12.2,-9.93232368142687));
#162136=CARTESIAN_POINT('Ctrl Pts',(3.23264428103363,12.2,-9.93489086516516));
#162137=CARTESIAN_POINT('Ctrl Pts',(3.23394087093888,12.2,-9.93749884706859));
#162138=CARTESIAN_POINT('Ctrl Pts',(3.23526689255536,12.2,-9.94014674271966));
#162139=CARTESIAN_POINT('Ctrl Pts',(3.23659291429229,12.2,-9.94279463861126));
#162140=CARTESIAN_POINT('Ctrl Pts',(3.23794836657372,12.2,-9.94548244614007));
#162141=CARTESIAN_POINT('Ctrl Pts',(3.23933338706717,12.2,-9.94820930137372));
#162142=CARTESIAN_POINT('Ctrl Pts',(3.2407184074348,12.2,-9.95093615635967));
#162143=CARTESIAN_POINT('Ctrl Pts',(3.24213299317023,12.2,-9.95370205968793));
#162144=CARTESIAN_POINT('Ctrl Pts',(3.24357727670757,12.2,-9.95650616476534));
#162145=CARTESIAN_POINT('Ctrl Pts',(3.24502156024491,12.2,-9.95931026984276));
#162146=CARTESIAN_POINT('Ctrl Pts',(3.24649554098433,12.2,-9.96215257641826));
#162147=CARTESIAN_POINT('Ctrl Pts',(3.24799934334432,12.2,-9.9650322613944));
#162148=CARTESIAN_POINT('Ctrl Pts',(3.2495031458409,12.2,-9.96791194663211));
#162149=CARTESIAN_POINT('Ctrl Pts',(3.25103676869038,12.2,-9.97082900758185));
#162150=CARTESIAN_POINT('Ctrl Pts',(3.25260033236023,12.2,-9.97378263891107));
#162151=CARTESIAN_POINT('Ctrl Pts',(3.25416389588806,12.2,-9.976736269972));
#162152=CARTESIAN_POINT('Ctrl Pts',(3.25575739965918,12.2,-9.97972646891153));
#162153=CARTESIAN_POINT('Ctrl Pts',(3.25738095602416,12.2,-9.98275245098191));
#162154=CARTESIAN_POINT('Ctrl Pts',(3.25900451238914,12.2,-9.9857784330523));
#162155=CARTESIAN_POINT('Ctrl Pts',(3.26065812212961,12.2,-9.98884019302732));
#162156=CARTESIAN_POINT('Ctrl Pts',(3.26234189356637,12.2,-9.99193696241241));
#162157=CARTESIAN_POINT('Ctrl Pts',(3.26402566515607,12.2,-9.99503373207879));
#162158=CARTESIAN_POINT('Ctrl Pts',(3.26573959839308,12.2,-9.99816551050695));
#162159=CARTESIAN_POINT('Ctrl Pts',(3.26748379516037,12.2,-10.0013315413397));
#162160=CARTESIAN_POINT('Ctrl Pts',(3.26922799176922,12.2,-10.0044975718848));
#162161=CARTESIAN_POINT('Ctrl Pts',(3.27100245227379,12.2,-10.0076978552424));
#162162=CARTESIAN_POINT('Ctrl Pts',(3.27280727645822,12.2,-10.0109316507083));
#162163=CARTESIAN_POINT('Ctrl Pts',(3.27461210064265,12.2,-10.0141654461741));
#162164=CARTESIAN_POINT('Ctrl Pts',(3.27644728547917,12.2,-10.0174327549877));
#162165=CARTESIAN_POINT('Ctrl Pts',(3.27831292783616,12.2,-10.0207328516975));
#162166=CARTESIAN_POINT('Ctrl Pts',(3.28017857036261,12.2,-10.0240329487069));
#162167=CARTESIAN_POINT('Ctrl Pts',(3.28207466745283,12.2,-10.0273658338645));
#162168=CARTESIAN_POINT('Ctrl Pts',(3.28400131172657,12.2,-10.0307307968834));
#162169=CARTESIAN_POINT('Ctrl Pts',(3.28592795582531,12.2,-10.0340957595966));
#162170=CARTESIAN_POINT('Ctrl Pts',(3.28788514159727,12.2,-10.0374928010271));
#162171=CARTESIAN_POINT('Ctrl Pts',(3.28987295803413,12.2,-10.0409212247515));
#162172=CARTESIAN_POINT('Ctrl Pts',(3.29186077447099,12.2,-10.0443496484759));
#162173=CARTESIAN_POINT('Ctrl Pts',(3.29387922191414,12.2,-10.0478094560464));
#162174=CARTESIAN_POINT('Ctrl Pts',(3.29592837717168,12.2,-10.0512999628349));
#162175=CARTESIAN_POINT('Ctrl Pts',(3.29763600661501,12.2,-10.0542087185976));
#162176=CARTESIAN_POINT('Ctrl Pts',(3.29936496256444,12.2,-10.0571387938304));
#162177=CARTESIAN_POINT('Ctrl Pts',(3.30111528791055,12.2,-10.0600898020238));
#162178=CARTESIAN_POINT('Ctrl Pts',(3.30286561325665,12.2,-10.0630408102171));
#162179=CARTESIAN_POINT('Ctrl Pts',(3.30463731045194,12.2,-10.0660127496903));
#162180=CARTESIAN_POINT('Ctrl Pts',(3.30643041830724,12.2,-10.0690052412317));
#162181=CARTESIAN_POINT('Ctrl Pts',(3.30822352616255,12.2,-10.071997732773));
#162182=CARTESIAN_POINT('Ctrl Pts',(3.31003804832766,12.2,-10.0750107740499));
#162183=CARTESIAN_POINT('Ctrl Pts',(3.31187402200822,12.2,-10.0780439907166));
#162184=CARTESIAN_POINT('Ctrl Pts',(3.31370999568878,12.2,-10.0810772073833));
#162185=CARTESIAN_POINT('Ctrl Pts',(3.31556742194232,12.2,-10.0841305985987));
#162186=CARTESIAN_POINT('Ctrl Pts',(3.31744634049258,12.2,-10.0872037960433));
#162187=CARTESIAN_POINT('Ctrl Pts',(3.31932525904285,12.2,-10.0902769934879));
#162188=CARTESIAN_POINT('Ctrl Pts',(3.32122566853014,12.2,-10.0933699950749));
#162189=CARTESIAN_POINT('Ctrl Pts',(3.32314760630905,12.2,-10.0964824384786));
#162190=CARTESIAN_POINT('Ctrl Pts',(3.32506954408795,12.2,-10.0995948818824));
#162191=CARTESIAN_POINT('Ctrl Pts',(3.32701301051074,12.2,-10.1027267651552));
#162192=CARTESIAN_POINT('Ctrl Pts',(3.32897803988687,12.2,-10.1058777326562));
#162193=CARTESIAN_POINT('Ctrl Pts',(3.33094306926299,12.2,-10.1090287001571));
#162194=CARTESIAN_POINT('Ctrl Pts',(3.33292966242571,12.2,-10.1121987489485));
#162195=CARTESIAN_POINT('Ctrl Pts',(3.33493785120809,12.2,-10.1153875283452));
#162196=CARTESIAN_POINT('Ctrl Pts',(3.33694603999046,12.2,-10.1185763077419));
#162197=CARTESIAN_POINT('Ctrl Pts',(3.33897582609978,12.2,-10.121783815576));
#162198=CARTESIAN_POINT('Ctrl Pts',(3.34102723901821,12.2,-10.1250097041886));
#162199=CARTESIAN_POINT('Ctrl Pts',(3.34307865193664,12.2,-10.1282355928012));
#162200=CARTESIAN_POINT('Ctrl Pts',(3.34515169511101,12.2,-10.1314798631419));
#162201=CARTESIAN_POINT('Ctrl Pts',(3.34724639455722,12.2,-10.134742171685));
#162202=CARTESIAN_POINT('Ctrl Pts',(3.34934109377511,12.2,-10.1380044798726));
#162203=CARTESIAN_POINT('Ctrl Pts',(3.3514574532995,12.2,-10.1412848262684));
#162204=CARTESIAN_POINT('Ctrl Pts',(3.35359549674524,12.2,-10.1445828720186));
#162205=CARTESIAN_POINT('Ctrl Pts',(3.35573354042403,12.2,-10.1478809181283));
#162206=CARTESIAN_POINT('Ctrl Pts',(3.3578932721719,12.2,-10.1511966642599));
#162207=CARTESIAN_POINT('Ctrl Pts',(3.36007471723956,12.2,-10.154529778564));
#162208=CARTESIAN_POINT('Ctrl Pts',(3.36225616230723,12.2,-10.1578628928681));
#162209=CARTESIAN_POINT('Ctrl Pts',(3.36445931893843,12.2,-10.1612133717553));
#162210=CARTESIAN_POINT('Ctrl Pts',(3.36668421574221,12.2,-10.1645808896012));
#162211=CARTESIAN_POINT('Ctrl Pts',(3.36890911254599,12.2,-10.167948407447));
#162212=CARTESIAN_POINT('Ctrl Pts',(3.37115574773594,12.2,-10.1713329637864));
#162213=CARTESIAN_POINT('Ctrl Pts',(3.37342414548664,12.2,-10.1747342343719));
#162214=CARTESIAN_POINT('Ctrl Pts',(3.37569254323735,12.2,-10.1781355049573));
#162215=CARTESIAN_POINT('Ctrl Pts',(3.37798270409996,12.2,-10.1815534882874));
#162216=CARTESIAN_POINT('Ctrl Pts',(3.38029464930715,12.2,-10.1849878669671));
#162217=CARTESIAN_POINT('Ctrl Pts',(3.38260659451435,12.2,-10.1884222456468));
#162218=CARTESIAN_POINT('Ctrl Pts',(3.38494032514155,12.2,-10.1918730194242));
#162219=CARTESIAN_POINT('Ctrl Pts',(3.38729586111264,12.2,-10.1953398715067));
#162220=CARTESIAN_POINT('Ctrl Pts',(3.38965139708372,12.2,-10.1988067235892));
#162221=CARTESIAN_POINT('Ctrl Pts',(3.39202873963218,12.2,-10.2022896534767));
#162222=CARTESIAN_POINT('Ctrl Pts',(3.39442790728192,12.2,-10.2057883530064));
#162223=CARTESIAN_POINT('Ctrl Pts',(3.39634724150631,12.2,-10.2085873127827));
#162224=CARTESIAN_POINT('Ctrl Pts',(3.39828054458294,12.2,-10.2113963636784));
#162225=CARTESIAN_POINT('Ctrl Pts',(3.40022782480161,12.2,-10.2142153489442));
#162226=CARTESIAN_POINT('Ctrl Pts',(3.40217510475497,12.2,-10.2170343338259));
#162227=CARTESIAN_POINT('Ctrl Pts',(3.40413636230927,12.2,-10.2198632526979));
#162228=CARTESIAN_POINT('Ctrl Pts',(3.40611160631355,12.2,-10.222701950743));
#162229=CARTESIAN_POINT('Ctrl Pts',(3.40808685058695,12.2,-10.2255406491748));
#162230=CARTESIAN_POINT('Ctrl Pts',(3.41007608258852,12.2,-10.2283891257098));
#162231=CARTESIAN_POINT('Ctrl Pts',(3.41207930829898,12.2,-10.2312472258981));
#162232=CARTESIAN_POINT('Ctrl Pts',(3.4140825337365,12.2,-10.2341053256969));
#162233=CARTESIAN_POINT('Ctrl Pts',(3.41609975458148,12.2,-10.2369730511646));
#162234=CARTESIAN_POINT('Ctrl Pts',(3.41813097835897,12.2,-10.2398502485399));
#162235=CARTESIAN_POINT('Ctrl Pts',(3.42016220241321,12.2,-10.2427274463072));
#162236=CARTESIAN_POINT('Ctrl Pts',(3.42220742842744,12.2,-10.2456141148395));
#162237=CARTESIAN_POINT('Ctrl Pts',(3.4242666646517,12.2,-10.2485101042202));
#162238=CARTESIAN_POINT('Ctrl Pts',(3.42632590059539,12.2,-10.2514060932062));
#162239=CARTESIAN_POINT('Ctrl Pts',(3.42839914638966,12.2,-10.2543114038233));
#162240=CARTESIAN_POINT('Ctrl Pts',(3.43048640915543,12.2,-10.2572258861188));
#162241=CARTESIAN_POINT('Ctrl Pts',(3.43257367220559,12.2,-10.2601403688113));
#162242=CARTESIAN_POINT('Ctrl Pts',(3.43467495235674,12.2,-10.2630640229044));
#162243=CARTESIAN_POINT('Ctrl Pts',(3.43679025513961,12.2,-10.2659967002315));
#162244=CARTESIAN_POINT('Ctrl Pts',(3.43890555763427,12.2,-10.268929377159));
#162245=CARTESIAN_POINT('Ctrl Pts',(3.44103488317611,12.2,-10.2718710773958));
#162246=CARTESIAN_POINT('Ctrl Pts',(3.44317823766613,12.2,-10.2748216555426));
#162247=CARTESIAN_POINT('Ctrl Pts',(3.44532159244817,12.2,-10.2777722340913));
#162248=CARTESIAN_POINT('Ctrl Pts',(3.44747897522034,12.2,-10.2807316880628));
#162249=CARTESIAN_POINT('Ctrl Pts',(3.44965039329304,12.2,-10.2836998759603));
#162250=CARTESIAN_POINT('Ctrl Pts',(3.45182181106988,12.2,-10.2866680634534));
#162251=CARTESIAN_POINT('Ctrl Pts',(3.45400726117153,12.2,-10.2896449823346));
#162252=CARTESIAN_POINT('Ctrl Pts',(3.45620675165695,12.2,-10.2926304899785));
#162253=CARTESIAN_POINT('Ctrl Pts',(3.45840624244204,12.2,-10.2956159980292));
#162254=CARTESIAN_POINT('Ctrl Pts',(3.46061977099237,12.2,-10.298610094153));
#162255=CARTESIAN_POINT('Ctrl Pts',(3.46284734372488,12.2,-10.3016126379833));
#162256=CARTESIAN_POINT('Ctrl Pts',(3.4650749164574,12.2,-10.3046151818136));
#162257=CARTESIAN_POINT('Ctrl Pts',(3.46731653194711,12.2,-10.3076261708866));
#162258=CARTESIAN_POINT('Ctrl Pts',(3.46957219479369,12.2,-10.3106454662186));
#162259=CARTESIAN_POINT('Ctrl Pts',(3.47182785733294,12.2,-10.3136647611393));
#162260=CARTESIAN_POINT('Ctrl Pts',(3.47409756675805,12.2,-10.3166923611296));
#162261=CARTESIAN_POINT('Ctrl Pts',(3.47638132724833,12.2,-10.3197281275062));
#162262=CARTESIAN_POINT('Ctrl Pts',(3.47866508804978,12.2,-10.3227638942965));
#162263=CARTESIAN_POINT('Ctrl Pts',(3.48096289913657,12.2,-10.3258078278485));
#162264=CARTESIAN_POINT('Ctrl Pts',(3.48327476331955,12.2,-10.3288597880156));
#162265=CARTESIAN_POINT('Ctrl Pts',(3.48558662718754,12.2,-10.331911747767));
#162266=CARTESIAN_POINT('Ctrl Pts',(3.48791254547593,12.2,-10.3349717374172));
#162267=CARTESIAN_POINT('Ctrl Pts',(3.49025251878373,12.2,-10.3380396164993));
#162268=CARTESIAN_POINT('Ctrl Pts',(3.49259249241036,12.2,-10.3411074959993));
#162269=CARTESIAN_POINT('Ctrl Pts',(3.49494652270889,12.2,-10.3441832675219));
#162270=CARTESIAN_POINT('Ctrl Pts',(3.49731461156859,12.2,-10.3472667944558));
#162271=CARTESIAN_POINT('Ctrl Pts',(3.49968270010564,12.2,-10.3503503209696));
#162272=CARTESIAN_POINT('Ctrl Pts',(3.50206484618705,12.2,-10.3534416029506));
#162273=CARTESIAN_POINT('Ctrl Pts',(3.5044610520458,12.2,-10.3565405060301));
#162274=CARTESIAN_POINT('Ctrl Pts',(3.50745630961409,12.2,-10.3604141351961));
#162275=CARTESIAN_POINT('Ctrl Pts',(3.51047353661352,12.2,-10.364299672618));
#162276=CARTESIAN_POINT('Ctrl Pts',(3.51351273404293,12.2,-10.3681968585202));
#162277=CARTESIAN_POINT('Ctrl Pts',(3.51594409211897,12.2,-10.3713146074118));
#162278=CARTESIAN_POINT('Ctrl Pts',(3.51838951118483,12.2,-10.3744398121406));
#162279=CARTESIAN_POINT('Ctrl Pts',(3.52084899283185,12.2,-10.3775723397462));
#162280=CARTESIAN_POINT('Ctrl Pts',(3.52330847414376,12.2,-10.3807048669251));
#162281=CARTESIAN_POINT('Ctrl Pts',(3.52578201731481,12.2,-10.3838447179866));
#162282=CARTESIAN_POINT('Ctrl Pts',(3.52826962305499,12.2,-10.3869917617845));
#162283=CARTESIAN_POINT('Ctrl Pts',(3.53075722913411,12.2,-10.3901388060111));
#162284=CARTESIAN_POINT('Ctrl Pts',(3.53325889815932,12.2,-10.3932930442191));
#162285=CARTESIAN_POINT('Ctrl Pts',(3.53577462846402,12.2,-10.3964543457252));
#162286=CARTESIAN_POINT('Ctrl Pts',(3.53829035842594,12.2,-10.3996156468005));
#162287=CARTESIAN_POINT('Ctrl Pts',(3.54082015177394,12.2,-10.402784011055));
#162288=CARTESIAN_POINT('Ctrl Pts',(3.54336400684231,12.2,-10.4059593127392));
#162289=CARTESIAN_POINT('Ctrl Pts',(3.54590786225728,12.2,-10.4091346148559));
#162290=CARTESIAN_POINT('Ctrl Pts',(3.54846577876086,12.2,-10.4123168516944));
#162291=CARTESIAN_POINT('Ctrl Pts',(3.55103775746831,12.2,-10.4155058984938));
#162292=CARTESIAN_POINT('Ctrl Pts',(3.55360973582534,12.2,-10.4186949448587));
#162293=CARTESIAN_POINT('Ctrl Pts',(3.55619577523877,12.2,-10.421890800525));
#162294=CARTESIAN_POINT('Ctrl Pts',(3.55879587435811,12.2,-10.4250933389847));
#162295=CARTESIAN_POINT('Ctrl Pts',(3.56139597383172,12.2,-10.4282958778808));
#162296=CARTESIAN_POINT('Ctrl Pts',(3.56401013252331,12.2,-10.4315050999247));
#162297=CARTESIAN_POINT('Ctrl Pts',(3.56663834999989,12.2,-10.4347208807667));
#162298=CARTESIAN_POINT('Ctrl Pts',(3.56926656747646,12.2,-10.4379366616086));
#162299=CARTESIAN_POINT('Ctrl Pts',(3.57190884331856,12.2,-10.4411590006013));
#162300=CARTESIAN_POINT('Ctrl Pts',(3.57456517540921,12.2,-10.4443877747779));
#162301=CARTESIAN_POINT('Ctrl Pts',(3.57722150713793,12.2,-10.4476165485146));
#162302=CARTESIAN_POINT('Ctrl Pts',(3.57989189510259,12.2,-10.4508517564481));
#162303=CARTESIAN_POINT('Ctrl Pts',(3.5825763375064,12.2,-10.4540932775311));
#162304=CARTESIAN_POINT('Ctrl Pts',(3.58526078027596,12.2,-10.4573347990558));
#162305=CARTESIAN_POINT('Ctrl Pts',(3.58795927643857,12.2,-10.4605826325624));
#162306=CARTESIAN_POINT('Ctrl Pts',(3.59067182447673,12.2,-10.4638366562404));
#162307=CARTESIAN_POINT('Ctrl Pts',(3.5933843721453,12.2,-10.467090679475));
#162308=CARTESIAN_POINT('Ctrl Pts',(3.59611096994815,12.2,-10.4703508946199));
#162309=CARTESIAN_POINT('Ctrl Pts',(3.59885161700098,12.2,-10.4736171797414));
#162310=CARTESIAN_POINT('Ctrl Pts',(3.60159226442721,12.2,-10.4768834653079));
#162311=CARTESIAN_POINT('Ctrl Pts',(3.60434696058074,12.2,-10.4801558207883));
#162312=CARTESIAN_POINT('Ctrl Pts',(3.60711570092673,12.2,-10.4834341272424));
#162313=CARTESIAN_POINT('Ctrl Pts',(3.60988444089548,12.2,-10.4867124332498));
#162314=CARTESIAN_POINT('Ctrl Pts',(3.61266722571761,12.2,-10.4899966900893));
#162315=CARTESIAN_POINT('Ctrl Pts',(3.61546405148805,12.2,-10.4932867792644));
#162316=CARTESIAN_POINT('Ctrl Pts',(3.61826087763956,12.2,-10.4965768688878));
#162317=CARTESIAN_POINT('Ctrl Pts',(3.62107174623998,12.2,-10.499872790898));
#162318=CARTESIAN_POINT('Ctrl Pts',(3.62389665100596,12.2,-10.503174427245));
#162319=CARTESIAN_POINT('Ctrl Pts',(3.62672155538705,12.2,-10.5064760631421));
#162320=CARTESIAN_POINT('Ctrl Pts',(3.62956049568624,12.2,-10.509783414164));
#162321=CARTESIAN_POINT('Ctrl Pts',(3.63241347009432,12.2,-10.5130963635026));
#162322=CARTESIAN_POINT('Ctrl Pts',(3.63526644489112,12.2,-10.5164093132926));
#162323=CARTESIAN_POINT('Ctrl Pts',(3.63813345015262,12.2,-10.5197278611486));
#162324=CARTESIAN_POINT('Ctrl Pts',(3.64101448547721,12.2,-10.5230518914968));
#162325=CARTESIAN_POINT('Ctrl Pts',(3.64461577943667,12.2,-10.5272069292056));
#162326=CARTESIAN_POINT('Ctrl Pts',(3.64823899165949,12.2,-10.531370533428));
#162327=CARTESIAN_POINT('Ctrl Pts',(3.65188411173008,12.2,-10.5355424809979));
#162328=CARTESIAN_POINT('Ctrl Pts',(3.65480020754816,12.2,-10.5388800387809));
#162329=CARTESIAN_POINT('Ctrl Pts',(3.65773032456201,12.2,-10.5422229356683));
#162330=CARTESIAN_POINT('Ctrl Pts',(3.66067445835609,12.2,-10.5455710585059));
#162331=CARTESIAN_POINT('Ctrl Pts',(3.66288255880193,12.2,-10.5480821507481));
#162332=CARTESIAN_POINT('Ctrl Pts',(3.66509854334697,12.2,-10.5505961834098));
#162333=CARTESIAN_POINT('Ctrl Pts',(3.66732240880676,12.2,-10.553113107443));
#162334=CARTESIAN_POINT('Ctrl Pts',(3.66954627467056,12.2,-10.5556300319334));
#162335=CARTESIAN_POINT('Ctrl Pts',(3.67177802289491,12.2,-10.5581498480829));
#162336=CARTESIAN_POINT('Ctrl Pts',(3.67401764972147,12.2,-10.5606725095749));
#162337=CARTESIAN_POINT('Ctrl Pts',(3.67625727614117,12.2,-10.5631951706087));
#162338=CARTESIAN_POINT('Ctrl Pts',(3.67850478209378,12.2,-10.5657206766006));
#162339=CARTESIAN_POINT('Ctrl Pts',(3.68076016355419,12.2,-10.568248979759));
#162340=CARTESIAN_POINT('Ctrl Pts',(3.6830155450146,12.2,-10.5707772829173));
#162341=CARTESIAN_POINT('Ctrl Pts',(3.68527880354079,12.2,-10.5733083858828));
#162342=CARTESIAN_POINT('Ctrl Pts',(3.68754993546862,12.2,-10.5758422380523));
#162343=CARTESIAN_POINT('Ctrl Pts',(3.68982106739646,12.2,-10.5783760902218));
#162344=CARTESIAN_POINT('Ctrl Pts',(3.69210007333722,12.2,-10.5809126936451));
#162345=CARTESIAN_POINT('Ctrl Pts',(3.69438694976448,12.2,-10.5834520021894));
#162346=CARTESIAN_POINT('Ctrl Pts',(3.69667382619174,12.2,-10.5859913107336));
#162347=CARTESIAN_POINT('Ctrl Pts',(3.69896857461671,12.2,-10.588533323432));
#162348=CARTESIAN_POINT('Ctrl Pts',(3.70127118999071,12.2,-10.5910779949643));
#162349=CARTESIAN_POINT('Ctrl Pts',(3.7035738053647,12.2,-10.5936226664967));
#162350=CARTESIAN_POINT('Ctrl Pts',(3.70588428847979,12.2,-10.5961699971038));
#162351=CARTESIAN_POINT('Ctrl Pts',(3.70820263681116,12.2,-10.5987199397191));
#162352=CARTESIAN_POINT('Ctrl Pts',(3.71052098556369,12.2,-10.6012698827977));
#162353=CARTESIAN_POINT('Ctrl Pts',(3.71284719920176,12.2,-10.6038224389186));
#162354=CARTESIAN_POINT('Ctrl Pts',(3.71518127454206,12.2,-10.6063775615403));
#162355=CARTESIAN_POINT('Ctrl Pts',(3.71751534945832,12.2,-10.6089326836979));
#162356=CARTESIAN_POINT('Ctrl Pts',(3.71985728643833,12.2,-10.6114903737602));
#162357=CARTESIAN_POINT('Ctrl Pts',(3.72220708242959,12.2,-10.614050584962));
#162358=CARTESIAN_POINT('Ctrl Pts',(3.72455687842085,12.2,-10.6166107961639));
#162359=CARTESIAN_POINT('Ctrl Pts',(3.72691453309312,12.2,-10.6191735287393));
#162360=CARTESIAN_POINT('Ctrl Pts',(3.72928004250786,12.2,-10.621738737813));
#162361=CARTESIAN_POINT('Ctrl Pts',(3.7316455519226,12.2,-10.6243039468867));
#162362=CARTESIAN_POINT('Ctrl Pts',(3.73401891705308,12.2,-10.6268716331934));
#162363=CARTESIAN_POINT('Ctrl Pts',(3.73640013396655,12.2,-10.6294417508083));
#162364=CARTESIAN_POINT('Ctrl Pts',(3.73878135088002,12.2,-10.6320118684233));
#162365=CARTESIAN_POINT('Ctrl Pts',(3.74117042055986,12.2,-10.6345844173465));
#162366=CARTESIAN_POINT('Ctrl Pts',(3.74356733797209,12.2,-10.6371593539194));
#162367=CARTESIAN_POINT('Ctrl Pts',(3.74596425538433,12.2,-10.6397342904923));
#162368=CARTESIAN_POINT('Ctrl Pts',(3.74836902180121,12.2,-10.642311613766));
#162369=CARTESIAN_POINT('Ctrl Pts',(3.75078163324985,12.2,-10.6448912800092));
#162370=CARTESIAN_POINT('Ctrl Pts',(3.75319424469849,12.2,-10.6474709462525));
#162371=CARTESIAN_POINT('Ctrl Pts',(3.75561470032649,12.2,-10.6500529563642));
#162372=CARTESIAN_POINT('Ctrl Pts',(3.75804299769553,12.2,-10.6526372644366));
#162373=CARTESIAN_POINT('Ctrl Pts',(3.76047129550572,12.2,-10.6552215729786));
#162374=CARTESIAN_POINT('Ctrl Pts',(3.76290743595977,12.2,-10.6578081796378));
#162375=CARTESIAN_POINT('Ctrl Pts',(3.76535141277436,12.2,-10.6603970420977));
#162376=CARTESIAN_POINT('Ctrl Pts',(3.76779538914495,12.2,-10.6629859040873));
#162377=CARTESIAN_POINT('Ctrl Pts',(3.77024720295681,12.2,-10.6655770197601));
#162378=CARTESIAN_POINT('Ctrl Pts',(3.77270685078479,12.2,-10.668170347791));
#162379=CARTESIAN_POINT('Ctrl Pts',(3.77516649861278,12.2,-10.670763675822));
#162380=CARTESIAN_POINT('Ctrl Pts',(3.77763398072316,12.2,-10.6733592149277));
#162381=CARTESIAN_POINT('Ctrl Pts',(3.78010929254988,12.2,-10.6759569220417));
#162382=CARTESIAN_POINT('Ctrl Pts',(3.78258460437661,12.2,-10.6785546291556));
#162383=CARTESIAN_POINT('Ctrl Pts',(3.78506774596969,12.2,-10.6811545042945));
#162384=CARTESIAN_POINT('Ctrl Pts',(3.7875587137535,12.2,-10.6837565039497));
#162385=CARTESIAN_POINT('Ctrl Pts',(3.79004968153732,12.2,-10.686358503605));
#162386=CARTESIAN_POINT('Ctrl Pts',(3.79254847436508,12.2,-10.6889626284939));
#162387=CARTESIAN_POINT('Ctrl Pts',(3.795055089815,12.2,-10.6915688352791));
#162388=CARTESIAN_POINT('Ctrl Pts',(3.79756170526491,12.2,-10.6941750420644));
#162389=CARTESIAN_POINT('Ctrl Pts',(3.80007614280942,12.2,-10.6967833312927));
#162390=CARTESIAN_POINT('Ctrl Pts',(3.80259839721671,12.2,-10.6993936594059));
#162391=CARTESIAN_POINT('Ctrl Pts',(3.80512065208222,12.2,-10.7020039879934));
#162392=CARTESIAN_POINT('Ctrl Pts',(3.80765072504991,12.2,-10.7046163552897));
#162393=CARTESIAN_POINT('Ctrl Pts',(3.81018861179482,12.2,-10.7072307203366));
#162394=CARTESIAN_POINT('Ctrl Pts',(3.81357246001961,12.2,-10.7107165396076));
#162395=CARTESIAN_POINT('Ctrl Pts',(3.81697019802871,12.2,-10.7142059090503));
#162396=CARTESIAN_POINT('Ctrl Pts',(3.82038181697112,12.2,-10.7176987284312));
#162397=CARTESIAN_POINT('Ctrl Pts',(3.82294053129414,12.2,-10.7203183430858));
#162398=CARTESIAN_POINT('Ctrl Pts',(3.82550705281773,12.2,-10.7229398990236));
#162399=CARTESIAN_POINT('Ctrl Pts',(3.8280813782269,12.2,-10.7255633537674));
#162400=CARTESIAN_POINT('Ctrl Pts',(3.83065570363607,12.2,-10.7281868085113));
#162401=CARTESIAN_POINT('Ctrl Pts',(3.83323783246379,12.2,-10.7308121620896));
#162402=CARTESIAN_POINT('Ctrl Pts',(3.83582775974363,12.2,-10.7334393727023));
#162403=CARTESIAN_POINT('Ctrl Pts',(3.83841768749397,12.2,-10.7360665837922));
#162404=CARTESIAN_POINT('Ctrl Pts',(3.84101541335483,12.2,-10.7386956510243));
#162405=CARTESIAN_POINT('Ctrl Pts',(3.8436209345679,12.2,-10.7413265355319));
#162406=CARTESIAN_POINT('Ctrl Pts',(3.84622645530763,12.2,-10.7439574195615));
#162407=CARTESIAN_POINT('Ctrl Pts',(3.84883976926361,12.2,-10.7465901190494));
#162408=CARTESIAN_POINT('Ctrl Pts',(3.85146087354406,12.2,-10.7492245946205));
#162409=CARTESIAN_POINT('Ctrl Pts',(3.8540819778245,12.2,-10.7518590701916));
#162410=CARTESIAN_POINT('Ctrl Pts',(3.85671087190274,12.2,-10.7544953205363));
#162411=CARTESIAN_POINT('Ctrl Pts',(3.85934755027728,12.2,-10.7571333042024));
#162412=CARTESIAN_POINT('Ctrl Pts',(3.86286312128368,12.2,-10.7606506155975));
#162413=CARTESIAN_POINT('Ctrl Pts',(3.8663925313172,12.2,-10.7641710081345));
#162414=CARTESIAN_POINT('Ctrl Pts',(3.86993577013724,12.2,-10.7676943829573));
#162415=CARTESIAN_POINT('Ctrl Pts',(3.87259319985574,12.2,-10.7703369146744));
#162416=CARTESIAN_POINT('Ctrl Pts',(3.87525840755974,12.2,-10.772981125142));
#162417=CARTESIAN_POINT('Ctrl Pts',(3.87793138932427,12.2,-10.7756269783185));
#162418=CARTESIAN_POINT('Ctrl Pts',(3.88060437060321,12.2,-10.7782728310142));
#162419=CARTESIAN_POINT('Ctrl Pts',(3.88328512549008,12.2,-10.7809203259849));
#162420=CARTESIAN_POINT('Ctrl Pts',(3.88597364926807,12.2,-10.7835694224721));
#162421=CARTESIAN_POINT('Ctrl Pts',(3.88866217304606,12.2,-10.7862185189593));
#162422=CARTESIAN_POINT('Ctrl Pts',(3.89135846522161,12.2,-10.7888692159367));
#162423=CARTESIAN_POINT('Ctrl Pts',(3.89406251996902,12.2,-10.7915214620607));
#162424=CARTESIAN_POINT('Ctrl Pts',(3.89676657471642,12.2,-10.7941737081848));
#162425=CARTESIAN_POINT('Ctrl Pts',(3.89947839156725,12.2,-10.796827503932));
#162426=CARTESIAN_POINT('Ctrl Pts',(3.90219796677242,12.2,-10.7994828125143));
#162427=CARTESIAN_POINT('Ctrl Pts',(3.90673059227906,12.2,-10.8039083269788));
#162428=CARTESIAN_POINT('Ctrl Pts',(3.91128476133577,12.2,-10.8083380407001));
#162429=CARTESIAN_POINT('Ctrl Pts',(3.91586047899994,12.2,-10.812771925));
#162430=CARTESIAN_POINT('Ctrl Pts',(4.27433546799994,15.2,-10.676144262));
#162431=CARTESIAN_POINT('Ctrl Pts',(4.27433546799994,11.6,-10.676144262));
#162432=CARTESIAN_POINT('Ctrl Pts',(4.27439112799994,15.2,-10.675381706));
#162433=CARTESIAN_POINT('Ctrl Pts',(4.27439112799994,11.6,-10.675381706));
#162434=CARTESIAN_POINT('Ctrl Pts',(4.27450212599994,15.2,-10.673857013));
#162435=CARTESIAN_POINT('Ctrl Pts',(4.27450212599994,11.6,-10.673857013));
#162436=CARTESIAN_POINT('Ctrl Pts',(4.27466766699994,15.2,-10.671571231));
#162437=CARTESIAN_POINT('Ctrl Pts',(4.27466766699994,11.6,-10.671571231));
#162438=CARTESIAN_POINT('Ctrl Pts',(4.27488647299994,15.2,-10.668526034));
#162439=CARTESIAN_POINT('Ctrl Pts',(4.27488647299994,11.6,-10.668526034));
#162440=CARTESIAN_POINT('Ctrl Pts',(4.27515678899994,15.2,-10.664723728));
#162441=CARTESIAN_POINT('Ctrl Pts',(4.27515678899994,11.6,-10.664723728));
#162442=CARTESIAN_POINT('Ctrl Pts',(4.27542391299994,15.2,-10.660925613));
#162443=CARTESIAN_POINT('Ctrl Pts',(4.27542391299994,11.6,-10.660925613));
#162444=CARTESIAN_POINT('Ctrl Pts',(4.27568784799994,15.2,-10.65713169));
#162445=CARTESIAN_POINT('Ctrl Pts',(4.27568784799994,11.6,-10.65713169));
#162446=CARTESIAN_POINT('Ctrl Pts',(4.27594859599994,15.2,-10.653341964));
#162447=CARTESIAN_POINT('Ctrl Pts',(4.27594859599994,11.6,-10.653341964));
#162448=CARTESIAN_POINT('Ctrl Pts',(4.27620615899994,15.2,-10.649556439));
#162449=CARTESIAN_POINT('Ctrl Pts',(4.27620615899994,11.6,-10.649556439));
#162450=CARTESIAN_POINT('Ctrl Pts',(4.27646054199994,15.2,-10.645775121));
#162451=CARTESIAN_POINT('Ctrl Pts',(4.27646054199994,11.6,-10.645775121));
#162452=CARTESIAN_POINT('Ctrl Pts',(4.27671175199994,15.2,-10.641998021));
#162453=CARTESIAN_POINT('Ctrl Pts',(4.27671175199994,11.6,-10.641998021));
#162454=CARTESIAN_POINT('Ctrl Pts',(4.27695979299994,15.2,-10.638225143));
#162455=CARTESIAN_POINT('Ctrl Pts',(4.27695979299994,11.6,-10.638225143));
#162456=CARTESIAN_POINT('Ctrl Pts',(4.27720467299994,15.2,-10.6344565));
#162457=CARTESIAN_POINT('Ctrl Pts',(4.27720467299994,11.6,-10.6344565));
#162458=CARTESIAN_POINT('Ctrl Pts',(4.27744639699995,15.2,-10.630692101));
#162459=CARTESIAN_POINT('Ctrl Pts',(4.27744639699995,11.6,-10.630692101));
#162460=CARTESIAN_POINT('Ctrl Pts',(4.27768497199995,15.2,-10.626931954));
#162461=CARTESIAN_POINT('Ctrl Pts',(4.27768497199995,11.6,-10.626931954));
#162462=CARTESIAN_POINT('Ctrl Pts',(4.27792040199994,15.2,-10.623176065));
#162463=CARTESIAN_POINT('Ctrl Pts',(4.27792040199994,11.6,-10.623176065));
#162464=CARTESIAN_POINT('Ctrl Pts',(4.27815269399995,15.2,-10.619424443));
#162465=CARTESIAN_POINT('Ctrl Pts',(4.27815269399995,11.6,-10.619424443));
#162466=CARTESIAN_POINT('Ctrl Pts',(4.27838185099994,15.2,-10.615677095));
#162467=CARTESIAN_POINT('Ctrl Pts',(4.27838185099994,11.6,-10.615677095));
#162468=CARTESIAN_POINT('Ctrl Pts',(4.27860787799994,15.2,-10.611934026));
#162469=CARTESIAN_POINT('Ctrl Pts',(4.27860787799994,11.6,-10.611934026));
#162470=CARTESIAN_POINT('Ctrl Pts',(4.27883078099994,15.2,-10.608195244));
#162471=CARTESIAN_POINT('Ctrl Pts',(4.27883078099994,11.6,-10.608195244));
#162472=CARTESIAN_POINT('Ctrl Pts',(4.27905056299995,15.2,-10.604460756));
#162473=CARTESIAN_POINT('Ctrl Pts',(4.27905056299995,11.6,-10.604460756));
#162474=CARTESIAN_POINT('Ctrl Pts',(4.27926722999994,15.2,-10.600730569));
#162475=CARTESIAN_POINT('Ctrl Pts',(4.27926722999994,11.6,-10.600730569));
#162476=CARTESIAN_POINT('Ctrl Pts',(4.27948078599994,15.2,-10.59700469));
#162477=CARTESIAN_POINT('Ctrl Pts',(4.27948078599994,11.6,-10.59700469));
#162478=CARTESIAN_POINT('Ctrl Pts',(4.27969123899994,15.2,-10.593283128));
#162479=CARTESIAN_POINT('Ctrl Pts',(4.27969123899994,11.6,-10.593283128));
#162480=CARTESIAN_POINT('Ctrl Pts',(4.27989859299994,15.2,-10.589565891));
#162481=CARTESIAN_POINT('Ctrl Pts',(4.27989859299994,11.6,-10.589565891));
#162482=CARTESIAN_POINT('Ctrl Pts',(4.28010285399994,15.2,-10.585852985));
#162483=CARTESIAN_POINT('Ctrl Pts',(4.28010285399994,11.6,-10.585852985));
#162484=CARTESIAN_POINT('Ctrl Pts',(4.28030402699994,15.2,-10.58214442));
#162485=CARTESIAN_POINT('Ctrl Pts',(4.28030402699994,11.6,-10.58214442));
#162486=CARTESIAN_POINT('Ctrl Pts',(4.28050211699994,15.2,-10.578440202));
#162487=CARTESIAN_POINT('Ctrl Pts',(4.28050211699994,11.6,-10.578440202));
#162488=CARTESIAN_POINT('Ctrl Pts',(4.28069712999995,15.2,-10.574740338));
#162489=CARTESIAN_POINT('Ctrl Pts',(4.28069712999995,11.6,-10.574740338));
#162490=CARTESIAN_POINT('Ctrl Pts',(4.28088907099994,15.2,-10.571044837));
#162491=CARTESIAN_POINT('Ctrl Pts',(4.28088907099994,11.6,-10.571044837));
#162492=CARTESIAN_POINT('Ctrl Pts',(4.28107794499994,15.2,-10.567353704));
#162493=CARTESIAN_POINT('Ctrl Pts',(4.28107794499994,11.6,-10.567353704));
#162494=CARTESIAN_POINT('Ctrl Pts',(4.28126375699994,15.2,-10.563666949));
#162495=CARTESIAN_POINT('Ctrl Pts',(4.28126375699994,11.6,-10.563666949));
#162496=CARTESIAN_POINT('Ctrl Pts',(4.28144651399994,15.2,-10.559984579));
#162497=CARTESIAN_POINT('Ctrl Pts',(4.28144651399994,11.6,-10.559984579));
#162498=CARTESIAN_POINT('Ctrl Pts',(4.28162621799994,15.2,-10.5563066));
#162499=CARTESIAN_POINT('Ctrl Pts',(4.28162621799994,11.6,-10.5563066));
#162500=CARTESIAN_POINT('Ctrl Pts',(4.28180287799994,15.2,-10.552633021));
#162501=CARTESIAN_POINT('Ctrl Pts',(4.28180287799994,11.6,-10.552633021));
#162502=CARTESIAN_POINT('Ctrl Pts',(4.28197649799994,15.2,-10.548963849));
#162503=CARTESIAN_POINT('Ctrl Pts',(4.28197649799994,11.6,-10.548963849));
#162504=CARTESIAN_POINT('Ctrl Pts',(4.28214708299994,15.2,-10.545299093));
#162505=CARTESIAN_POINT('Ctrl Pts',(4.28214708299994,11.6,-10.545299093));
#162506=CARTESIAN_POINT('Ctrl Pts',(4.28231463999994,15.2,-10.541638759));
#162507=CARTESIAN_POINT('Ctrl Pts',(4.28231463999994,11.6,-10.541638759));
#162508=CARTESIAN_POINT('Ctrl Pts',(4.28247917299994,15.2,-10.537982854));
#162509=CARTESIAN_POINT('Ctrl Pts',(4.28247917299994,11.6,-10.537982854));
#162510=CARTESIAN_POINT('Ctrl Pts',(4.28264068799994,15.2,-10.534331388));
#162511=CARTESIAN_POINT('Ctrl Pts',(4.28264068799994,11.6,-10.534331388));
#162512=CARTESIAN_POINT('Ctrl Pts',(4.28279918999994,15.2,-10.530684367));
#162513=CARTESIAN_POINT('Ctrl Pts',(4.28279918999994,11.6,-10.530684367));
#162514=CARTESIAN_POINT('Ctrl Pts',(4.28295468599994,15.2,-10.5270418));
#162515=CARTESIAN_POINT('Ctrl Pts',(4.28295468599994,11.6,-10.5270418));
#162516=CARTESIAN_POINT('Ctrl Pts',(4.28310717999994,15.2,-10.523403692));
#162517=CARTESIAN_POINT('Ctrl Pts',(4.28310717999994,11.6,-10.523403692));
#162518=CARTESIAN_POINT('Ctrl Pts',(4.28325667799994,15.2,-10.519770053));
#162519=CARTESIAN_POINT('Ctrl Pts',(4.28325667799994,11.6,-10.519770053));
#162520=CARTESIAN_POINT('Ctrl Pts',(4.28340318699994,15.2,-10.51614089));
#162521=CARTESIAN_POINT('Ctrl Pts',(4.28340318699994,11.6,-10.51614089));
#162522=CARTESIAN_POINT('Ctrl Pts',(4.28354670899994,15.2,-10.512516211));
#162523=CARTESIAN_POINT('Ctrl Pts',(4.28354670899994,11.6,-10.512516211));
#162524=CARTESIAN_POINT('Ctrl Pts',(4.28368725299995,15.2,-10.508896023));
#162525=CARTESIAN_POINT('Ctrl Pts',(4.28368725299995,11.6,-10.508896023));
#162526=CARTESIAN_POINT('Ctrl Pts',(4.28382482299994,15.2,-10.505280333));
#162527=CARTESIAN_POINT('Ctrl Pts',(4.28382482299994,11.6,-10.505280333));
#162528=CARTESIAN_POINT('Ctrl Pts',(4.28395942599994,15.2,-10.501669151));
#162529=CARTESIAN_POINT('Ctrl Pts',(4.28395942599994,11.6,-10.501669151));
#162530=CARTESIAN_POINT('Ctrl Pts',(4.28409106599995,15.2,-10.498062482));
#162531=CARTESIAN_POINT('Ctrl Pts',(4.28409106599995,11.6,-10.498062482));
#162532=CARTESIAN_POINT('Ctrl Pts',(4.28421974899994,15.2,-10.494460336));
#162533=CARTESIAN_POINT('Ctrl Pts',(4.28421974899994,11.6,-10.494460336));
#162534=CARTESIAN_POINT('Ctrl Pts',(4.28434548199994,15.2,-10.490862719));
#162535=CARTESIAN_POINT('Ctrl Pts',(4.28434548199994,11.6,-10.490862719));
#162536=CARTESIAN_POINT('Ctrl Pts',(4.28446826999994,15.2,-10.48726964));
#162537=CARTESIAN_POINT('Ctrl Pts',(4.28446826999994,11.6,-10.48726964));
#162538=CARTESIAN_POINT('Ctrl Pts',(4.28458811799994,15.2,-10.483681106));
#162539=CARTESIAN_POINT('Ctrl Pts',(4.28458811799994,11.6,-10.483681106));
#162540=CARTESIAN_POINT('Ctrl Pts',(4.28470503199994,15.2,-10.480097126));
#162541=CARTESIAN_POINT('Ctrl Pts',(4.28470503199994,11.6,-10.480097126));
#162542=CARTESIAN_POINT('Ctrl Pts',(4.28481901899994,15.2,-10.476517706));
#162543=CARTESIAN_POINT('Ctrl Pts',(4.28481901899994,11.6,-10.476517706));
#162544=CARTESIAN_POINT('Ctrl Pts',(4.28493008199994,15.2,-10.472942854));
#162545=CARTESIAN_POINT('Ctrl Pts',(4.28493008199994,11.6,-10.472942854));
#162546=CARTESIAN_POINT('Ctrl Pts',(4.28503822999994,15.2,-10.469372579));
#162547=CARTESIAN_POINT('Ctrl Pts',(4.28503822999994,11.6,-10.469372579));
#162548=CARTESIAN_POINT('Ctrl Pts',(4.28514346699994,15.2,-10.465806888));
#162549=CARTESIAN_POINT('Ctrl Pts',(4.28514346699994,11.6,-10.465806888));
#162550=CARTESIAN_POINT('Ctrl Pts',(4.28524579799994,15.2,-10.462245789));
#162551=CARTESIAN_POINT('Ctrl Pts',(4.28524579799994,11.6,-10.462245789));
#162552=CARTESIAN_POINT('Ctrl Pts',(4.28534523099994,15.2,-10.458689288));
#162553=CARTESIAN_POINT('Ctrl Pts',(4.28534523099994,11.6,-10.458689288));
#162554=CARTESIAN_POINT('Ctrl Pts',(4.28544177099994,15.2,-10.455137397));
#162555=CARTESIAN_POINT('Ctrl Pts',(4.28544177099994,11.6,-10.455137397));
#162556=CARTESIAN_POINT('Ctrl Pts',(4.28553542399994,15.2,-10.451590119));
#162557=CARTESIAN_POINT('Ctrl Pts',(4.28553542399994,11.6,-10.451590119));
#162558=CARTESIAN_POINT('Ctrl Pts',(4.28562619399994,15.2,-10.448047466));
#162559=CARTESIAN_POINT('Ctrl Pts',(4.28562619399994,11.6,-10.448047466));
#162560=CARTESIAN_POINT('Ctrl Pts',(4.28571408899994,15.2,-10.444509443));
#162561=CARTESIAN_POINT('Ctrl Pts',(4.28571408899994,11.6,-10.444509443));
#162562=CARTESIAN_POINT('Ctrl Pts',(4.28579911599994,15.2,-10.440976059));
#162563=CARTESIAN_POINT('Ctrl Pts',(4.28579911599994,11.6,-10.440976059));
#162564=CARTESIAN_POINT('Ctrl Pts',(4.28588127799994,15.2,-10.437447322));
#162565=CARTESIAN_POINT('Ctrl Pts',(4.28588127799994,11.6,-10.437447322));
#162566=CARTESIAN_POINT('Ctrl Pts',(4.28596058199994,15.2,-10.43392324));
#162567=CARTESIAN_POINT('Ctrl Pts',(4.28596058199994,11.6,-10.43392324));
#162568=CARTESIAN_POINT('Ctrl Pts',(4.28603703499994,15.2,-10.430403819));
#162569=CARTESIAN_POINT('Ctrl Pts',(4.28603703499994,11.6,-10.430403819));
#162570=CARTESIAN_POINT('Ctrl Pts',(4.28611064099994,15.2,-10.426889069));
#162571=CARTESIAN_POINT('Ctrl Pts',(4.28611064099994,11.6,-10.426889069));
#162572=CARTESIAN_POINT('Ctrl Pts',(4.28618140799994,15.2,-10.423378997));
#162573=CARTESIAN_POINT('Ctrl Pts',(4.28618140799994,11.6,-10.423378997));
#162574=CARTESIAN_POINT('Ctrl Pts',(4.28624934099994,15.2,-10.419873612));
#162575=CARTESIAN_POINT('Ctrl Pts',(4.28624934099994,11.6,-10.419873612));
#162576=CARTESIAN_POINT('Ctrl Pts',(4.28631444799994,15.2,-10.41637292));
#162577=CARTESIAN_POINT('Ctrl Pts',(4.28631444799994,11.6,-10.41637292));
#162578=CARTESIAN_POINT('Ctrl Pts',(4.28637673099994,15.2,-10.41287693));
#162579=CARTESIAN_POINT('Ctrl Pts',(4.28637673099994,11.6,-10.41287693));
#162580=CARTESIAN_POINT('Ctrl Pts',(4.28643619899994,15.2,-10.40938565));
#162581=CARTESIAN_POINT('Ctrl Pts',(4.28643619899994,11.6,-10.40938565));
#162582=CARTESIAN_POINT('Ctrl Pts',(4.28649285899994,15.2,-10.405899088));
#162583=CARTESIAN_POINT('Ctrl Pts',(4.28649285899994,11.6,-10.405899088));
#162584=CARTESIAN_POINT('Ctrl Pts',(4.28654671399994,15.2,-10.402417252));
#162585=CARTESIAN_POINT('Ctrl Pts',(4.28654671399994,11.6,-10.402417252));
#162586=CARTESIAN_POINT('Ctrl Pts',(4.28659777199994,15.2,-10.398940149));
#162587=CARTESIAN_POINT('Ctrl Pts',(4.28659777199994,11.6,-10.398940149));
#162588=CARTESIAN_POINT('Ctrl Pts',(4.28664603899994,15.2,-10.395467789));
#162589=CARTESIAN_POINT('Ctrl Pts',(4.28664603899994,11.6,-10.395467789));
#162590=CARTESIAN_POINT('Ctrl Pts',(4.28669152099994,15.2,-10.392000178));
#162591=CARTESIAN_POINT('Ctrl Pts',(4.28669152099994,11.6,-10.392000178));
#162592=CARTESIAN_POINT('Ctrl Pts',(4.28673422399994,15.2,-10.388537325));
#162593=CARTESIAN_POINT('Ctrl Pts',(4.28673422399994,11.6,-10.388537325));
#162594=CARTESIAN_POINT('Ctrl Pts',(4.28677415499994,15.2,-10.385079237));
#162595=CARTESIAN_POINT('Ctrl Pts',(4.28677415499994,11.6,-10.385079237));
#162596=CARTESIAN_POINT('Ctrl Pts',(4.28681131899994,15.2,-10.381625923));
#162597=CARTESIAN_POINT('Ctrl Pts',(4.28681131899994,11.6,-10.381625923));
#162598=CARTESIAN_POINT('Ctrl Pts',(4.28684572299994,15.2,-10.378177391));
#162599=CARTESIAN_POINT('Ctrl Pts',(4.28684572299994,11.6,-10.378177391));
#162600=CARTESIAN_POINT('Ctrl Pts',(4.28687737399994,15.2,-10.374733649));
#162601=CARTESIAN_POINT('Ctrl Pts',(4.28687737399994,11.6,-10.374733649));
#162602=CARTESIAN_POINT('Ctrl Pts',(4.28690627599994,15.2,-10.371294704));
#162603=CARTESIAN_POINT('Ctrl Pts',(4.28690627599994,11.6,-10.371294704));
#162604=CARTESIAN_POINT('Ctrl Pts',(4.28693243799994,15.2,-10.367860566));
#162605=CARTESIAN_POINT('Ctrl Pts',(4.28693243799994,11.6,-10.367860566));
#162606=CARTESIAN_POINT('Ctrl Pts',(4.28695586299995,15.2,-10.364431241));
#162607=CARTESIAN_POINT('Ctrl Pts',(4.28695586299995,11.6,-10.364431241));
#162608=CARTESIAN_POINT('Ctrl Pts',(4.28697656099994,15.2,-10.361006739));
#162609=CARTESIAN_POINT('Ctrl Pts',(4.28697656099994,11.6,-10.361006739));
#162610=CARTESIAN_POINT('Ctrl Pts',(4.28699453599994,15.2,-10.357587066));
#162611=CARTESIAN_POINT('Ctrl Pts',(4.28699453599994,11.6,-10.357587066));
#162612=CARTESIAN_POINT('Ctrl Pts',(4.28700979599994,15.2,-10.354172232));
#162613=CARTESIAN_POINT('Ctrl Pts',(4.28700979599994,11.6,-10.354172232));
#162614=CARTESIAN_POINT('Ctrl Pts',(4.28702234599994,15.2,-10.350762244));
#162615=CARTESIAN_POINT('Ctrl Pts',(4.28702234599994,11.6,-10.350762244));
#162616=CARTESIAN_POINT('Ctrl Pts',(4.28703219199994,15.2,-10.34735711));
#162617=CARTESIAN_POINT('Ctrl Pts',(4.28703219199994,11.6,-10.34735711));
#162618=CARTESIAN_POINT('Ctrl Pts',(4.28703934099994,15.2,-10.343956839));
#162619=CARTESIAN_POINT('Ctrl Pts',(4.28703934099994,11.6,-10.343956839));
#162620=CARTESIAN_POINT('Ctrl Pts',(4.28704380099994,15.2,-10.340561439));
#162621=CARTESIAN_POINT('Ctrl Pts',(4.28704380099994,11.6,-10.340561439));
#162622=CARTESIAN_POINT('Ctrl Pts',(4.28704557599994,15.2,-10.337170918));
#162623=CARTESIAN_POINT('Ctrl Pts',(4.28704557599994,11.6,-10.337170918));
#162624=CARTESIAN_POINT('Ctrl Pts',(4.28704467399994,15.2,-10.333785284));
#162625=CARTESIAN_POINT('Ctrl Pts',(4.28704467399994,11.6,-10.333785284));
#162626=CARTESIAN_POINT('Ctrl Pts',(4.28704110099994,15.2,-10.330404544));
#162627=CARTESIAN_POINT('Ctrl Pts',(4.28704110099994,11.6,-10.330404544));
#162628=CARTESIAN_POINT('Ctrl Pts',(4.28703486299994,15.2,-10.327028709));
#162629=CARTESIAN_POINT('Ctrl Pts',(4.28703486299994,11.6,-10.327028709));
#162630=CARTESIAN_POINT('Ctrl Pts',(4.28702596899995,15.2,-10.323657784));
#162631=CARTESIAN_POINT('Ctrl Pts',(4.28702596899995,11.6,-10.323657784));
#162632=CARTESIAN_POINT('Ctrl Pts',(4.28701442199994,15.2,-10.320291779));
#162633=CARTESIAN_POINT('Ctrl Pts',(4.28701442199994,11.6,-10.320291779));
#162634=CARTESIAN_POINT('Ctrl Pts',(4.28700022999995,15.2,-10.316930704));
#162635=CARTESIAN_POINT('Ctrl Pts',(4.28700022999995,11.6,-10.316930704));
#162636=CARTESIAN_POINT('Ctrl Pts',(4.28698340099994,15.2,-10.313574564));
#162637=CARTESIAN_POINT('Ctrl Pts',(4.28698340099994,11.6,-10.313574564));
#162638=CARTESIAN_POINT('Ctrl Pts',(4.28696393999994,15.2,-10.310223367));
#162639=CARTESIAN_POINT('Ctrl Pts',(4.28696393999994,11.6,-10.310223367));
#162640=CARTESIAN_POINT('Ctrl Pts',(4.28694185399995,15.2,-10.306877123));
#162641=CARTESIAN_POINT('Ctrl Pts',(4.28694185399995,11.6,-10.306877123));
#162642=CARTESIAN_POINT('Ctrl Pts',(4.28691714999994,15.2,-10.303535842));
#162643=CARTESIAN_POINT('Ctrl Pts',(4.28691714999994,11.6,-10.303535842));
#162644=CARTESIAN_POINT('Ctrl Pts',(4.28688983399994,15.2,-10.300199528));
#162645=CARTESIAN_POINT('Ctrl Pts',(4.28688983399994,11.6,-10.300199528));
#162646=CARTESIAN_POINT('Ctrl Pts',(4.28685991299994,15.2,-10.296868192));
#162647=CARTESIAN_POINT('Ctrl Pts',(4.28685991299994,11.6,-10.296868192));
#162648=CARTESIAN_POINT('Ctrl Pts',(4.28682739499994,15.2,-10.293541843));
#162649=CARTESIAN_POINT('Ctrl Pts',(4.28682739499994,11.6,-10.293541843));
#162650=CARTESIAN_POINT('Ctrl Pts',(4.28679228399994,15.2,-10.290220487));
#162651=CARTESIAN_POINT('Ctrl Pts',(4.28679228399994,11.6,-10.290220487));
#162652=CARTESIAN_POINT('Ctrl Pts',(4.28675458899994,15.2,-10.286904133));
#162653=CARTESIAN_POINT('Ctrl Pts',(4.28675458899994,11.6,-10.286904133));
#162654=CARTESIAN_POINT('Ctrl Pts',(4.28671431599995,15.2,-10.283592791));
#162655=CARTESIAN_POINT('Ctrl Pts',(4.28671431599995,11.6,-10.283592791));
#162656=CARTESIAN_POINT('Ctrl Pts',(4.28667147199994,15.2,-10.280286467));
#162657=CARTESIAN_POINT('Ctrl Pts',(4.28667147199994,11.6,-10.280286467));
#162658=CARTESIAN_POINT('Ctrl Pts',(4.28662606299994,15.2,-10.276985171));
#162659=CARTESIAN_POINT('Ctrl Pts',(4.28662606299994,11.6,-10.276985171));
#162660=CARTESIAN_POINT('Ctrl Pts',(4.28657809699994,15.2,-10.273688909));
#162661=CARTESIAN_POINT('Ctrl Pts',(4.28657809699994,11.6,-10.273688909));
#162662=CARTESIAN_POINT('Ctrl Pts',(4.28652757999994,15.2,-10.270397694));
#162663=CARTESIAN_POINT('Ctrl Pts',(4.28652757999994,11.6,-10.270397694));
#162664=CARTESIAN_POINT('Ctrl Pts',(4.28647451899994,15.2,-10.26711153));
#162665=CARTESIAN_POINT('Ctrl Pts',(4.28647451899994,11.6,-10.26711153));
#162666=CARTESIAN_POINT('Ctrl Pts',(4.28641892199995,15.2,-10.263830426));
#162667=CARTESIAN_POINT('Ctrl Pts',(4.28641892199995,11.6,-10.263830426));
#162668=CARTESIAN_POINT('Ctrl Pts',(4.28636079499995,15.2,-10.260554392));
#162669=CARTESIAN_POINT('Ctrl Pts',(4.28636079499995,11.6,-10.260554392));
#162670=CARTESIAN_POINT('Ctrl Pts',(4.28630014399995,15.2,-10.257283436));
#162671=CARTESIAN_POINT('Ctrl Pts',(4.28630014399995,11.6,-10.257283436));
#162672=CARTESIAN_POINT('Ctrl Pts',(4.28623697699994,15.2,-10.254017565));
#162673=CARTESIAN_POINT('Ctrl Pts',(4.28623697699994,11.6,-10.254017565));
#162674=CARTESIAN_POINT('Ctrl Pts',(4.28617130099994,15.2,-10.25075679));
#162675=CARTESIAN_POINT('Ctrl Pts',(4.28617130099994,11.6,-10.25075679));
#162676=CARTESIAN_POINT('Ctrl Pts',(4.28610312299995,15.2,-10.247501117));
#162677=CARTESIAN_POINT('Ctrl Pts',(4.28610312299995,11.6,-10.247501117));
#162678=CARTESIAN_POINT('Ctrl Pts',(4.28603244999994,15.2,-10.244250556));
#162679=CARTESIAN_POINT('Ctrl Pts',(4.28603244999994,11.6,-10.244250556));
#162680=CARTESIAN_POINT('Ctrl Pts',(4.28595928899994,15.2,-10.241005114));
#162681=CARTESIAN_POINT('Ctrl Pts',(4.28595928899994,11.6,-10.241005114));
#162682=CARTESIAN_POINT('Ctrl Pts',(4.28588364699994,15.2,-10.237764801));
#162683=CARTESIAN_POINT('Ctrl Pts',(4.28588364699994,11.6,-10.237764801));
#162684=CARTESIAN_POINT('Ctrl Pts',(4.28580552999995,15.2,-10.234529625));
#162685=CARTESIAN_POINT('Ctrl Pts',(4.28580552999995,11.6,-10.234529625));
#162686=CARTESIAN_POINT('Ctrl Pts',(4.28572494699995,15.2,-10.231299594));
#162687=CARTESIAN_POINT('Ctrl Pts',(4.28572494699995,11.6,-10.231299594));
#162688=CARTESIAN_POINT('Ctrl Pts',(4.28564190399995,15.2,-10.228074718));
#162689=CARTESIAN_POINT('Ctrl Pts',(4.28564190399995,11.6,-10.228074718));
#162690=CARTESIAN_POINT('Ctrl Pts',(4.28555640899994,15.2,-10.224855003));
#162691=CARTESIAN_POINT('Ctrl Pts',(4.28555640899994,11.6,-10.224855003));
#162692=CARTESIAN_POINT('Ctrl Pts',(4.28546846799994,15.2,-10.22164046));
#162693=CARTESIAN_POINT('Ctrl Pts',(4.28546846799994,11.6,-10.22164046));
#162694=CARTESIAN_POINT('Ctrl Pts',(4.28537808899994,15.2,-10.218431097));
#162695=CARTESIAN_POINT('Ctrl Pts',(4.28537808899994,11.6,-10.218431097));
#162696=CARTESIAN_POINT('Ctrl Pts',(4.28528527899994,15.2,-10.215226921));
#162697=CARTESIAN_POINT('Ctrl Pts',(4.28528527899994,11.6,-10.215226921));
#162698=CARTESIAN_POINT('Ctrl Pts',(4.28519004399995,15.2,-10.212027942));
#162699=CARTESIAN_POINT('Ctrl Pts',(4.28519004399995,11.6,-10.212027942));
#162700=CARTESIAN_POINT('Ctrl Pts',(4.28509239399994,15.2,-10.208834168));
#162701=CARTESIAN_POINT('Ctrl Pts',(4.28509239399994,11.6,-10.208834168));
#162702=CARTESIAN_POINT('Ctrl Pts',(4.28499233399994,15.2,-10.205645608));
#162703=CARTESIAN_POINT('Ctrl Pts',(4.28499233399994,11.6,-10.205645608));
#162704=CARTESIAN_POINT('Ctrl Pts',(4.28488987199994,15.2,-10.20246227));
#162705=CARTESIAN_POINT('Ctrl Pts',(4.28488987199994,11.6,-10.20246227));
#162706=CARTESIAN_POINT('Ctrl Pts',(4.28478501599994,15.2,-10.199284164));
#162707=CARTESIAN_POINT('Ctrl Pts',(4.28478501599994,11.6,-10.199284164));
#162708=CARTESIAN_POINT('Ctrl Pts',(4.28467777299994,15.2,-10.196111298));
#162709=CARTESIAN_POINT('Ctrl Pts',(4.28467777299994,11.6,-10.196111298));
#162710=CARTESIAN_POINT('Ctrl Pts',(4.28456814799994,15.2,-10.19294368));
#162711=CARTESIAN_POINT('Ctrl Pts',(4.28456814799994,11.6,-10.19294368));
#162712=CARTESIAN_POINT('Ctrl Pts',(4.28445615199994,15.2,-10.189781319));
#162713=CARTESIAN_POINT('Ctrl Pts',(4.28445615199994,11.6,-10.189781319));
#162714=CARTESIAN_POINT('Ctrl Pts',(4.28434179099995,15.2,-10.186624223));
#162715=CARTESIAN_POINT('Ctrl Pts',(4.28434179099995,11.6,-10.186624223));
#162716=CARTESIAN_POINT('Ctrl Pts',(4.28422507099994,15.2,-10.183472403));
#162717=CARTESIAN_POINT('Ctrl Pts',(4.28422507099994,11.6,-10.183472403));
#162718=CARTESIAN_POINT('Ctrl Pts',(4.28410600199994,15.2,-10.180325865));
#162719=CARTESIAN_POINT('Ctrl Pts',(4.28410600199994,11.6,-10.180325865));
#162720=CARTESIAN_POINT('Ctrl Pts',(4.28398458899994,15.2,-10.177184619));
#162721=CARTESIAN_POINT('Ctrl Pts',(4.28398458899994,11.6,-10.177184619));
#162722=CARTESIAN_POINT('Ctrl Pts',(4.28386084099994,15.2,-10.174048674));
#162723=CARTESIAN_POINT('Ctrl Pts',(4.28386084099994,11.6,-10.174048674));
#162724=CARTESIAN_POINT('Ctrl Pts',(4.28373476599995,15.2,-10.170918038));
#162725=CARTESIAN_POINT('Ctrl Pts',(4.28373476599995,11.6,-10.170918038));
#162726=CARTESIAN_POINT('Ctrl Pts',(4.28360636999995,15.2,-10.16779272));
#162727=CARTESIAN_POINT('Ctrl Pts',(4.28360636999995,11.6,-10.16779272));
#162728=CARTESIAN_POINT('Ctrl Pts',(4.28347566099994,15.2,-10.16467273));
#162729=CARTESIAN_POINT('Ctrl Pts',(4.28347566099994,11.6,-10.16467273));
#162730=CARTESIAN_POINT('Ctrl Pts',(4.28334264699994,15.2,-10.161558075));
#162731=CARTESIAN_POINT('Ctrl Pts',(4.28334264699994,11.6,-10.161558075));
#162732=CARTESIAN_POINT('Ctrl Pts',(4.28320733599994,15.2,-10.158448763));
#162733=CARTESIAN_POINT('Ctrl Pts',(4.28320733599994,11.6,-10.158448763));
#162734=CARTESIAN_POINT('Ctrl Pts',(4.28306973599994,15.2,-10.155344806));
#162735=CARTESIAN_POINT('Ctrl Pts',(4.28306973599994,11.6,-10.155344806));
#162736=CARTESIAN_POINT('Ctrl Pts',(4.28292985199994,15.2,-10.152246211));
#162737=CARTESIAN_POINT('Ctrl Pts',(4.28292985199994,11.6,-10.152246211));
#162738=CARTESIAN_POINT('Ctrl Pts',(4.28278769399994,15.2,-10.149152985));
#162739=CARTESIAN_POINT('Ctrl Pts',(4.28278769399994,11.6,-10.149152985));
#162740=CARTESIAN_POINT('Ctrl Pts',(4.28264326899995,15.2,-10.146065141));
#162741=CARTESIAN_POINT('Ctrl Pts',(4.28264326899995,11.6,-10.146065141));
#162742=CARTESIAN_POINT('Ctrl Pts',(4.28249658599994,15.2,-10.142982685));
#162743=CARTESIAN_POINT('Ctrl Pts',(4.28249658599994,11.6,-10.142982685));
#162744=CARTESIAN_POINT('Ctrl Pts',(4.28234765099995,15.2,-10.139905626));
#162745=CARTESIAN_POINT('Ctrl Pts',(4.28234765099995,11.6,-10.139905626));
#162746=CARTESIAN_POINT('Ctrl Pts',(4.28219647199994,15.2,-10.136833973));
#162747=CARTESIAN_POINT('Ctrl Pts',(4.28219647199994,11.6,-10.136833973));
#162748=CARTESIAN_POINT('Ctrl Pts',(4.28204305799994,15.2,-10.133767736));
#162749=CARTESIAN_POINT('Ctrl Pts',(4.28204305799994,11.6,-10.133767736));
#162750=CARTESIAN_POINT('Ctrl Pts',(4.28188741599994,15.2,-10.130706922));
#162751=CARTESIAN_POINT('Ctrl Pts',(4.28188741599994,11.6,-10.130706922));
#162752=CARTESIAN_POINT('Ctrl Pts',(4.28172955299994,15.2,-10.127651542));
#162753=CARTESIAN_POINT('Ctrl Pts',(4.28172955299994,11.6,-10.127651542));
#162754=CARTESIAN_POINT('Ctrl Pts',(4.28156947799994,15.2,-10.124601604));
#162755=CARTESIAN_POINT('Ctrl Pts',(4.28156947799994,11.6,-10.124601604));
#162756=CARTESIAN_POINT('Ctrl Pts',(4.28140719899995,15.2,-10.121557117));
#162757=CARTESIAN_POINT('Ctrl Pts',(4.28140719899995,11.6,-10.121557117));
#162758=CARTESIAN_POINT('Ctrl Pts',(4.28124272399994,15.2,-10.11851809));
#162759=CARTESIAN_POINT('Ctrl Pts',(4.28124272399994,11.6,-10.11851809));
#162760=CARTESIAN_POINT('Ctrl Pts',(4.28107605999995,15.2,-10.115484533));
#162761=CARTESIAN_POINT('Ctrl Pts',(4.28107605999995,11.6,-10.115484533));
#162762=CARTESIAN_POINT('Ctrl Pts',(4.28090721599994,15.2,-10.112456452));
#162763=CARTESIAN_POINT('Ctrl Pts',(4.28090721599994,11.6,-10.112456452));
#162764=CARTESIAN_POINT('Ctrl Pts',(4.28073619899994,15.2,-10.109433858));
#162765=CARTESIAN_POINT('Ctrl Pts',(4.28073619899994,11.6,-10.109433858));
#162766=CARTESIAN_POINT('Ctrl Pts',(4.28056301799994,15.2,-10.106416761));
#162767=CARTESIAN_POINT('Ctrl Pts',(4.28056301799994,11.6,-10.106416761));
#162768=CARTESIAN_POINT('Ctrl Pts',(4.28038768099994,15.2,-10.103405168));
#162769=CARTESIAN_POINT('Ctrl Pts',(4.28038768099994,11.6,-10.103405168));
#162770=CARTESIAN_POINT('Ctrl Pts',(4.28021019399994,15.2,-10.100399089));
#162771=CARTESIAN_POINT('Ctrl Pts',(4.28021019399994,11.6,-10.100399089));
#162772=CARTESIAN_POINT('Ctrl Pts',(4.28003056799994,15.2,-10.097398535));
#162773=CARTESIAN_POINT('Ctrl Pts',(4.28003056799994,11.6,-10.097398535));
#162774=CARTESIAN_POINT('Ctrl Pts',(4.27984880999994,15.2,-10.094403512));
#162775=CARTESIAN_POINT('Ctrl Pts',(4.27984880999994,11.6,-10.094403512));
#162776=CARTESIAN_POINT('Ctrl Pts',(4.27966492699994,15.2,-10.091414029));
#162777=CARTESIAN_POINT('Ctrl Pts',(4.27966492699994,11.6,-10.091414029));
#162778=CARTESIAN_POINT('Ctrl Pts',(4.27947892899994,15.2,-10.088430099));
#162779=CARTESIAN_POINT('Ctrl Pts',(4.27947892899994,11.6,-10.088430099));
#162780=CARTESIAN_POINT('Ctrl Pts',(4.27929082299995,15.2,-10.085451726));
#162781=CARTESIAN_POINT('Ctrl Pts',(4.27929082299995,11.6,-10.085451726));
#162782=CARTESIAN_POINT('Ctrl Pts',(4.27910061799994,15.2,-10.082478923));
#162783=CARTESIAN_POINT('Ctrl Pts',(4.27910061799994,11.6,-10.082478923));
#162784=CARTESIAN_POINT('Ctrl Pts',(4.27890832199994,15.2,-10.079511697));
#162785=CARTESIAN_POINT('Ctrl Pts',(4.27890832199994,11.6,-10.079511697));
#162786=CARTESIAN_POINT('Ctrl Pts',(4.27871394199994,15.2,-10.076550058));
#162787=CARTESIAN_POINT('Ctrl Pts',(4.27871394199994,11.6,-10.076550058));
#162788=CARTESIAN_POINT('Ctrl Pts',(4.27851748899994,15.2,-10.073594016));
#162789=CARTESIAN_POINT('Ctrl Pts',(4.27851748899994,11.6,-10.073594016));
#162790=CARTESIAN_POINT('Ctrl Pts',(4.27831896899994,15.2,-10.070643579));
#162791=CARTESIAN_POINT('Ctrl Pts',(4.27831896899994,11.6,-10.070643579));
#162792=CARTESIAN_POINT('Ctrl Pts',(4.27811839099994,15.2,-10.067698756));
#162793=CARTESIAN_POINT('Ctrl Pts',(4.27811839099994,11.6,-10.067698756));
#162794=CARTESIAN_POINT('Ctrl Pts',(4.27791576299995,15.2,-10.064759557));
#162795=CARTESIAN_POINT('Ctrl Pts',(4.27791576299995,11.6,-10.064759557));
#162796=CARTESIAN_POINT('Ctrl Pts',(4.27771109499994,15.2,-10.061825991));
#162797=CARTESIAN_POINT('Ctrl Pts',(4.27771109499994,11.6,-10.061825991));
#162798=CARTESIAN_POINT('Ctrl Pts',(4.27750439299994,15.2,-10.058898068));
#162799=CARTESIAN_POINT('Ctrl Pts',(4.27750439299994,11.6,-10.058898068));
#162800=CARTESIAN_POINT('Ctrl Pts',(4.27729566799994,15.2,-10.055975796));
#162801=CARTESIAN_POINT('Ctrl Pts',(4.27729566799994,11.6,-10.055975796));
#162802=CARTESIAN_POINT('Ctrl Pts',(4.27708492699994,15.2,-10.053059184));
#162803=CARTESIAN_POINT('Ctrl Pts',(4.27708492699994,11.6,-10.053059184));
#162804=CARTESIAN_POINT('Ctrl Pts',(4.27687217899994,15.2,-10.050148243));
#162805=CARTESIAN_POINT('Ctrl Pts',(4.27687217899994,11.6,-10.050148243));
#162806=CARTESIAN_POINT('Ctrl Pts',(4.27665743099995,15.2,-10.047242982));
#162807=CARTESIAN_POINT('Ctrl Pts',(4.27665743099995,11.6,-10.047242982));
#162808=CARTESIAN_POINT('Ctrl Pts',(4.27644069399994,15.2,-10.044343408));
#162809=CARTESIAN_POINT('Ctrl Pts',(4.27644069399994,11.6,-10.044343408));
#162810=CARTESIAN_POINT('Ctrl Pts',(4.27622197599994,15.2,-10.041449533));
#162811=CARTESIAN_POINT('Ctrl Pts',(4.27622197599994,11.6,-10.041449533));
#162812=CARTESIAN_POINT('Ctrl Pts',(4.27600128399994,15.2,-10.038561366));
#162813=CARTESIAN_POINT('Ctrl Pts',(4.27600128399994,11.6,-10.038561366));
#162814=CARTESIAN_POINT('Ctrl Pts',(4.27577862799995,15.2,-10.035678915));
#162815=CARTESIAN_POINT('Ctrl Pts',(4.27577862799995,11.6,-10.035678915));
#162816=CARTESIAN_POINT('Ctrl Pts',(4.27555401599994,15.2,-10.03280219));
#162817=CARTESIAN_POINT('Ctrl Pts',(4.27555401599994,11.6,-10.03280219));
#162818=CARTESIAN_POINT('Ctrl Pts',(4.27532745799994,15.2,-10.029931202));
#162819=CARTESIAN_POINT('Ctrl Pts',(4.27532745799994,11.6,-10.029931202));
#162820=CARTESIAN_POINT('Ctrl Pts',(4.27509896099994,15.2,-10.027065958));
#162821=CARTESIAN_POINT('Ctrl Pts',(4.27509896099994,11.6,-10.027065958));
#162822=CARTESIAN_POINT('Ctrl Pts',(4.27486853499994,15.2,-10.024206469));
#162823=CARTESIAN_POINT('Ctrl Pts',(4.27486853499994,11.6,-10.024206469));
#162824=CARTESIAN_POINT('Ctrl Pts',(4.27463618899994,15.2,-10.021352744));
#162825=CARTESIAN_POINT('Ctrl Pts',(4.27463618899994,11.6,-10.021352744));
#162826=CARTESIAN_POINT('Ctrl Pts',(4.27440193099994,15.2,-10.018504791));
#162827=CARTESIAN_POINT('Ctrl Pts',(4.27440193099994,11.6,-10.018504791));
#162828=CARTESIAN_POINT('Ctrl Pts',(4.27416576899994,15.2,-10.015662622));
#162829=CARTESIAN_POINT('Ctrl Pts',(4.27416576899994,11.6,-10.015662622));
#162830=CARTESIAN_POINT('Ctrl Pts',(4.27392771399994,15.2,-10.012826247));
#162831=CARTESIAN_POINT('Ctrl Pts',(4.27392771399994,11.6,-10.012826247));
#162832=CARTESIAN_POINT('Ctrl Pts',(4.27368777299994,15.2,-10.009995672));
#162833=CARTESIAN_POINT('Ctrl Pts',(4.27368777299994,11.6,-10.009995672));
#162834=CARTESIAN_POINT('Ctrl Pts',(4.27344595599994,15.2,-10.007170909));
#162835=CARTESIAN_POINT('Ctrl Pts',(4.27344595599994,11.6,-10.007170909));
#162836=CARTESIAN_POINT('Ctrl Pts',(4.27320227199994,15.2,-10.004351967));
#162837=CARTESIAN_POINT('Ctrl Pts',(4.27320227199994,11.6,-10.004351967));
#162838=CARTESIAN_POINT('Ctrl Pts',(4.27295672999994,15.2,-10.001538855));
#162839=CARTESIAN_POINT('Ctrl Pts',(4.27295672999994,11.6,-10.001538855));
#162840=CARTESIAN_POINT('Ctrl Pts',(4.27270933899994,15.2,-9.99873158300001));
#162841=CARTESIAN_POINT('Ctrl Pts',(4.27270933899994,11.6,-9.99873158300001));
#162842=CARTESIAN_POINT('Ctrl Pts',(4.27246010699994,15.2,-9.99593016200001));
#162843=CARTESIAN_POINT('Ctrl Pts',(4.27246010699994,11.6,-9.99593016200001));
#162844=CARTESIAN_POINT('Ctrl Pts',(4.27220904299995,15.2,-9.99313460000001));
#162845=CARTESIAN_POINT('Ctrl Pts',(4.27220904299995,11.6,-9.99313460000001));
#162846=CARTESIAN_POINT('Ctrl Pts',(4.27195615799994,15.2,-9.99034490700001));
#162847=CARTESIAN_POINT('Ctrl Pts',(4.27195615799994,11.6,-9.99034490700001));
#162848=CARTESIAN_POINT('Ctrl Pts',(4.27170145999994,15.2,-9.98756109200001));
#162849=CARTESIAN_POINT('Ctrl Pts',(4.27170145999994,11.6,-9.98756109200001));
#162850=CARTESIAN_POINT('Ctrl Pts',(4.27144495799994,15.2,-9.98478316600002));
#162851=CARTESIAN_POINT('Ctrl Pts',(4.27144495799994,11.6,-9.98478316600002));
#162852=CARTESIAN_POINT('Ctrl Pts',(4.27118666199994,15.2,-9.98201113800001));
#162853=CARTESIAN_POINT('Ctrl Pts',(4.27118666199994,11.6,-9.98201113800001));
#162854=CARTESIAN_POINT('Ctrl Pts',(4.27092657999994,15.2,-9.97924501800002));
#162855=CARTESIAN_POINT('Ctrl Pts',(4.27092657999994,11.6,-9.97924501800002));
#162856=CARTESIAN_POINT('Ctrl Pts',(4.27066472199995,15.2,-9.97648481500001));
#162857=CARTESIAN_POINT('Ctrl Pts',(4.27066472199995,11.6,-9.97648481500001));
#162858=CARTESIAN_POINT('Ctrl Pts',(4.27040109699994,15.2,-9.97373053900001));
#162859=CARTESIAN_POINT('Ctrl Pts',(4.27040109699994,11.6,-9.97373053900001));
#162860=CARTESIAN_POINT('Ctrl Pts',(4.27013571399994,15.2,-9.97098220000001));
#162861=CARTESIAN_POINT('Ctrl Pts',(4.27013571399994,11.6,-9.97098220000001));
#162862=CARTESIAN_POINT('Ctrl Pts',(4.26986858399994,15.2,-9.96823980900001));
#162863=CARTESIAN_POINT('Ctrl Pts',(4.26986858399994,11.6,-9.96823980900001));
#162864=CARTESIAN_POINT('Ctrl Pts',(4.26959971399994,15.2,-9.96550337300001));
#162865=CARTESIAN_POINT('Ctrl Pts',(4.26959971399994,11.6,-9.96550337300001));
#162866=CARTESIAN_POINT('Ctrl Pts',(4.26932911499994,15.2,-9.96277290400001));
#162867=CARTESIAN_POINT('Ctrl Pts',(4.26932911499994,11.6,-9.96277290400001));
#162868=CARTESIAN_POINT('Ctrl Pts',(4.26905679699995,15.2,-9.96004841000001));
#162869=CARTESIAN_POINT('Ctrl Pts',(4.26905679699995,11.6,-9.96004841000001));
#162870=CARTESIAN_POINT('Ctrl Pts',(4.26878276699994,15.2,-9.95732990400001));
#162871=CARTESIAN_POINT('Ctrl Pts',(4.26878276699994,11.6,-9.95732990400001));
#162872=CARTESIAN_POINT('Ctrl Pts',(4.26850703699994,15.2,-9.95461739200001));
#162873=CARTESIAN_POINT('Ctrl Pts',(4.26850703699994,11.6,-9.95461739200001));
#162874=CARTESIAN_POINT('Ctrl Pts',(4.26822961499994,15.2,-9.95191088700001));
#162875=CARTESIAN_POINT('Ctrl Pts',(4.26822961499994,11.6,-9.95191088700001));
#162876=CARTESIAN_POINT('Ctrl Pts',(4.26795051099994,15.2,-9.94921039700001));
#162877=CARTESIAN_POINT('Ctrl Pts',(4.26795051099994,11.6,-9.94921039700001));
#162878=CARTESIAN_POINT('Ctrl Pts',(4.26766973499995,15.2,-9.94651593200001));
#162879=CARTESIAN_POINT('Ctrl Pts',(4.26766973499995,11.6,-9.94651593200001));
#162880=CARTESIAN_POINT('Ctrl Pts',(4.26738729599994,15.2,-9.94382750400001));
#162881=CARTESIAN_POINT('Ctrl Pts',(4.26738729599994,11.6,-9.94382750400001));
#162882=CARTESIAN_POINT('Ctrl Pts',(4.26710320399994,15.2,-9.94114512000001));
#162883=CARTESIAN_POINT('Ctrl Pts',(4.26710320399994,11.6,-9.94114512000001));
#162884=CARTESIAN_POINT('Ctrl Pts',(4.26681746899995,15.2,-9.93846879200001));
#162885=CARTESIAN_POINT('Ctrl Pts',(4.26681746899995,11.6,-9.93846879200001));
#162886=CARTESIAN_POINT('Ctrl Pts',(4.26653009999994,15.2,-9.93579852900002));
#162887=CARTESIAN_POINT('Ctrl Pts',(4.26653009999994,11.6,-9.93579852900002));
#162888=CARTESIAN_POINT('Ctrl Pts',(4.26624110699994,15.2,-9.93313434100001));
#162889=CARTESIAN_POINT('Ctrl Pts',(4.26624110699994,11.6,-9.93313434100001));
#162890=CARTESIAN_POINT('Ctrl Pts',(4.26595049999994,15.2,-9.93047623900001));
#162891=CARTESIAN_POINT('Ctrl Pts',(4.26595049999994,11.6,-9.93047623900001));
#162892=CARTESIAN_POINT('Ctrl Pts',(4.26565828799994,15.2,-9.92782423300001));
#162893=CARTESIAN_POINT('Ctrl Pts',(4.26565828799994,11.6,-9.92782423300001));
#162894=CARTESIAN_POINT('Ctrl Pts',(4.26536448299994,15.2,-9.92517833100001));
#162895=CARTESIAN_POINT('Ctrl Pts',(4.26536448299994,11.6,-9.92517833100001));
#162896=CARTESIAN_POINT('Ctrl Pts',(4.26506909199994,15.2,-9.92253854600001));
#162897=CARTESIAN_POINT('Ctrl Pts',(4.26506909199994,11.6,-9.92253854600001));
#162898=CARTESIAN_POINT('Ctrl Pts',(4.26477212699994,15.2,-9.91990488600001));
#162899=CARTESIAN_POINT('Ctrl Pts',(4.26477212699994,11.6,-9.91990488600001));
#162900=CARTESIAN_POINT('Ctrl Pts',(4.26447359699995,15.2,-9.91727736200001));
#162901=CARTESIAN_POINT('Ctrl Pts',(4.26447359699995,11.6,-9.91727736200001));
#162902=CARTESIAN_POINT('Ctrl Pts',(4.26417351199994,15.2,-9.91465598400001));
#162903=CARTESIAN_POINT('Ctrl Pts',(4.26417351199994,11.6,-9.91465598400001));
#162904=CARTESIAN_POINT('Ctrl Pts',(4.26387188299994,15.2,-9.91204076200001));
#162905=CARTESIAN_POINT('Ctrl Pts',(4.26387188299994,11.6,-9.91204076200001));
#162906=CARTESIAN_POINT('Ctrl Pts',(4.26356871799995,15.2,-9.90943170600001));
#162907=CARTESIAN_POINT('Ctrl Pts',(4.26356871799995,11.6,-9.90943170600001));
#162908=CARTESIAN_POINT('Ctrl Pts',(4.26326402899995,15.2,-9.90682882600001));
#162909=CARTESIAN_POINT('Ctrl Pts',(4.26326402899995,11.6,-9.90682882600001));
#162910=CARTESIAN_POINT('Ctrl Pts',(4.26295782599994,15.2,-9.90423213400001));
#162911=CARTESIAN_POINT('Ctrl Pts',(4.26295782599994,11.6,-9.90423213400001));
#162912=CARTESIAN_POINT('Ctrl Pts',(4.26265011799994,15.2,-9.90164163800001));
#162913=CARTESIAN_POINT('Ctrl Pts',(4.26265011799994,11.6,-9.90164163800001));
#162914=CARTESIAN_POINT('Ctrl Pts',(4.26234091599994,15.2,-9.89905734900001));
#162915=CARTESIAN_POINT('Ctrl Pts',(4.26234091599994,11.6,-9.89905734900001));
#162916=CARTESIAN_POINT('Ctrl Pts',(4.26203022999994,15.2,-9.89647927800001));
#162917=CARTESIAN_POINT('Ctrl Pts',(4.26203022999994,11.6,-9.89647927800001));
#162918=CARTESIAN_POINT('Ctrl Pts',(4.26171806999994,15.2,-9.89390743400001));
#162919=CARTESIAN_POINT('Ctrl Pts',(4.26171806999994,11.6,-9.89390743400001));
#162920=CARTESIAN_POINT('Ctrl Pts',(4.26140444699994,15.2,-9.89134182800001));
#162921=CARTESIAN_POINT('Ctrl Pts',(4.26140444699994,11.6,-9.89134182800001));
#162922=CARTESIAN_POINT('Ctrl Pts',(4.26108937099994,15.2,-9.88878247200001));
#162923=CARTESIAN_POINT('Ctrl Pts',(4.26108937099994,11.6,-9.88878247200001));
#162924=CARTESIAN_POINT('Ctrl Pts',(4.26077285199994,15.2,-9.88622937300001));
#162925=CARTESIAN_POINT('Ctrl Pts',(4.26077285199994,11.6,-9.88622937300001));
#162926=CARTESIAN_POINT('Ctrl Pts',(4.26045489999994,15.2,-9.88368254300001));
#162927=CARTESIAN_POINT('Ctrl Pts',(4.26045489999994,11.6,-9.88368254300001));
#162928=CARTESIAN_POINT('Ctrl Pts',(4.26013552699995,15.2,-9.88114199300002));
#162929=CARTESIAN_POINT('Ctrl Pts',(4.26013552699995,11.6,-9.88114199300002));
#162930=CARTESIAN_POINT('Ctrl Pts',(4.25981474299994,15.2,-9.87860773300001));
#162931=CARTESIAN_POINT('Ctrl Pts',(4.25981474299994,11.6,-9.87860773300001));
#162932=CARTESIAN_POINT('Ctrl Pts',(4.25949255699994,15.2,-9.87607977400001));
#162933=CARTESIAN_POINT('Ctrl Pts',(4.25949255699994,11.6,-9.87607977400001));
#162934=CARTESIAN_POINT('Ctrl Pts',(4.25916897999994,15.2,-9.87355812500001));
#162935=CARTESIAN_POINT('Ctrl Pts',(4.25916897999994,11.6,-9.87355812500001));
#162936=CARTESIAN_POINT('Ctrl Pts',(4.25884402299994,15.2,-9.87104279600001));
#162937=CARTESIAN_POINT('Ctrl Pts',(4.25884402299994,11.6,-9.87104279600001));
#162938=CARTESIAN_POINT('Ctrl Pts',(4.25851769899994,15.2,-9.86853380100001));
#162939=CARTESIAN_POINT('Ctrl Pts',(4.25851769899994,11.6,-9.86853380100001));
#162940=CARTESIAN_POINT('Ctrl Pts',(4.25819001399994,15.2,-9.86603114700001));
#162941=CARTESIAN_POINT('Ctrl Pts',(4.25819001399994,11.6,-9.86603114700001));
#162942=CARTESIAN_POINT('Ctrl Pts',(4.25786098199994,15.2,-9.86353484700001));
#162943=CARTESIAN_POINT('Ctrl Pts',(4.25786098199994,11.6,-9.86353484700001));
#162944=CARTESIAN_POINT('Ctrl Pts',(4.25753061199994,15.2,-9.86104490900001));
#162945=CARTESIAN_POINT('Ctrl Pts',(4.25753061199994,11.6,-9.86104490900001));
#162946=CARTESIAN_POINT('Ctrl Pts',(4.25719891699995,15.2,-9.85856134500001));
#162947=CARTESIAN_POINT('Ctrl Pts',(4.25719891699995,11.6,-9.85856134500001));
#162948=CARTESIAN_POINT('Ctrl Pts',(4.25686590399994,15.2,-9.85608416600001));
#162949=CARTESIAN_POINT('Ctrl Pts',(4.25686590399994,11.6,-9.85608416600001));
#162950=CARTESIAN_POINT('Ctrl Pts',(4.25653158899994,15.2,-9.85361338200001));
#162951=CARTESIAN_POINT('Ctrl Pts',(4.25653158899994,11.6,-9.85361338200001));
#162952=CARTESIAN_POINT('Ctrl Pts',(4.25619597799994,15.2,-9.85114900400001));
#162953=CARTESIAN_POINT('Ctrl Pts',(4.25619597799994,11.6,-9.85114900400001));
#162954=CARTESIAN_POINT('Ctrl Pts',(4.25585908399994,15.2,-9.84869104300001));
#162955=CARTESIAN_POINT('Ctrl Pts',(4.25585908399994,11.6,-9.84869104300001));
#162956=CARTESIAN_POINT('Ctrl Pts',(4.25552091799995,15.2,-9.84623950800001));
#162957=CARTESIAN_POINT('Ctrl Pts',(4.25552091799995,11.6,-9.84623950800001));
#162958=CARTESIAN_POINT('Ctrl Pts',(4.25518148999994,15.2,-9.84379441200001));
#162959=CARTESIAN_POINT('Ctrl Pts',(4.25518148999994,11.6,-9.84379441200001));
#162960=CARTESIAN_POINT('Ctrl Pts',(4.25484081299994,15.2,-9.84135576400002));
#162961=CARTESIAN_POINT('Ctrl Pts',(4.25484081299994,11.6,-9.84135576400002));
#162962=CARTESIAN_POINT('Ctrl Pts',(4.25449889699994,15.2,-9.83892357600001));
#162963=CARTESIAN_POINT('Ctrl Pts',(4.25449889699994,11.6,-9.83892357600001));
#162964=CARTESIAN_POINT('Ctrl Pts',(4.25415575199994,15.2,-9.83649785800001));
#162965=CARTESIAN_POINT('Ctrl Pts',(4.25415575199994,11.6,-9.83649785800001));
#162966=CARTESIAN_POINT('Ctrl Pts',(4.25381139099995,15.2,-9.83407862100002));
#162967=CARTESIAN_POINT('Ctrl Pts',(4.25381139099995,11.6,-9.83407862100002));
#162968=CARTESIAN_POINT('Ctrl Pts',(4.25346582399994,15.2,-9.83166587500001));
#162969=CARTESIAN_POINT('Ctrl Pts',(4.25346582399994,11.6,-9.83166587500001));
#162970=CARTESIAN_POINT('Ctrl Pts',(4.25311906099994,15.2,-9.82925963300001));
#162971=CARTESIAN_POINT('Ctrl Pts',(4.25311906099994,11.6,-9.82925963300001));
#162972=CARTESIAN_POINT('Ctrl Pts',(4.25277111699994,15.2,-9.82685990200001));
#162973=CARTESIAN_POINT('Ctrl Pts',(4.25277111699994,11.6,-9.82685990200001));
#162974=CARTESIAN_POINT('Ctrl Pts',(4.25242199899994,15.2,-9.82446669800001));
#162975=CARTESIAN_POINT('Ctrl Pts',(4.25242199899994,11.6,-9.82446669800001));
#162976=CARTESIAN_POINT('Ctrl Pts',(4.25207172199995,15.2,-9.82208002900001));
#162977=CARTESIAN_POINT('Ctrl Pts',(4.25207172199995,11.6,-9.82208002900001));
#162978=CARTESIAN_POINT('Ctrl Pts',(4.25172029399994,15.2,-9.81969990500001));
#162979=CARTESIAN_POINT('Ctrl Pts',(4.25172029399994,11.6,-9.81969990500001));
#162980=CARTESIAN_POINT('Ctrl Pts',(4.25136772899994,15.2,-9.81732633900001));
#162981=CARTESIAN_POINT('Ctrl Pts',(4.25136772899994,11.6,-9.81732633900001));
#162982=CARTESIAN_POINT('Ctrl Pts',(4.25101403699994,15.2,-9.81495934100001));
#162983=CARTESIAN_POINT('Ctrl Pts',(4.25101403699994,11.6,-9.81495934100001));
#162984=CARTESIAN_POINT('Ctrl Pts',(4.25065923099995,15.2,-9.81259892200001));
#162985=CARTESIAN_POINT('Ctrl Pts',(4.25065923099995,11.6,-9.81259892200001));
#162986=CARTESIAN_POINT('Ctrl Pts',(4.25030331999994,15.2,-9.81024509500001));
#162987=CARTESIAN_POINT('Ctrl Pts',(4.25030331999994,11.6,-9.81024509500001));
#162988=CARTESIAN_POINT('Ctrl Pts',(4.24994631899995,15.2,-9.80789786800001));
#162989=CARTESIAN_POINT('Ctrl Pts',(4.24994631899995,11.6,-9.80789786800001));
#162990=CARTESIAN_POINT('Ctrl Pts',(4.24958823599995,15.2,-9.80555725300001));
#162991=CARTESIAN_POINT('Ctrl Pts',(4.24958823599995,11.6,-9.80555725300001));
#162992=CARTESIAN_POINT('Ctrl Pts',(4.24922908599994,15.2,-9.80322326100001));
#162993=CARTESIAN_POINT('Ctrl Pts',(4.24922908599994,11.6,-9.80322326100001));
#162994=CARTESIAN_POINT('Ctrl Pts',(4.24886887799994,15.2,-9.80089590500001));
#162995=CARTESIAN_POINT('Ctrl Pts',(4.24886887799994,11.6,-9.80089590500001));
#162996=CARTESIAN_POINT('Ctrl Pts',(4.24850762499995,15.2,-9.79857519500001));
#162997=CARTESIAN_POINT('Ctrl Pts',(4.24850762499995,11.6,-9.79857519500001));
#162998=CARTESIAN_POINT('Ctrl Pts',(4.24814533899994,15.2,-9.79626114200001));
#162999=CARTESIAN_POINT('Ctrl Pts',(4.24814533899994,11.6,-9.79626114200001));
#163000=CARTESIAN_POINT('Ctrl Pts',(4.24778202999994,15.2,-9.79395375600001));
#163001=CARTESIAN_POINT('Ctrl Pts',(4.24778202999994,11.6,-9.79395375600001));
#163002=CARTESIAN_POINT('Ctrl Pts',(4.24741771199994,15.2,-9.79165305000001));
#163003=CARTESIAN_POINT('Ctrl Pts',(4.24741771199994,11.6,-9.79165305000001));
#163004=CARTESIAN_POINT('Ctrl Pts',(4.24705239599994,15.2,-9.78935903500001));
#163005=CARTESIAN_POINT('Ctrl Pts',(4.24705239599994,11.6,-9.78935903500001));
#163006=CARTESIAN_POINT('Ctrl Pts',(4.24668609599994,15.2,-9.78707172100002));
#163007=CARTESIAN_POINT('Ctrl Pts',(4.24668609599994,11.6,-9.78707172100002));
#163008=CARTESIAN_POINT('Ctrl Pts',(4.24631881999994,15.2,-9.78479112100001));
#163009=CARTESIAN_POINT('Ctrl Pts',(4.24631881999994,11.6,-9.78479112100001));
#163010=CARTESIAN_POINT('Ctrl Pts',(4.24595058199994,15.2,-9.78251724500001));
#163011=CARTESIAN_POINT('Ctrl Pts',(4.24595058199994,11.6,-9.78251724500001));
#163012=CARTESIAN_POINT('Ctrl Pts',(4.24558139499995,15.2,-9.78025010500001));
#163013=CARTESIAN_POINT('Ctrl Pts',(4.24558139499995,11.6,-9.78025010500001));
#163014=CARTESIAN_POINT('Ctrl Pts',(4.24521126999994,15.2,-9.77798971300001));
#163015=CARTESIAN_POINT('Ctrl Pts',(4.24521126999994,11.6,-9.77798971300001));
#163016=CARTESIAN_POINT('Ctrl Pts',(4.24484021999994,15.2,-9.77573608000001));
#163017=CARTESIAN_POINT('Ctrl Pts',(4.24484021999994,11.6,-9.77573608000001));
#163018=CARTESIAN_POINT('Ctrl Pts',(4.24446825699994,15.2,-9.77348921500001));
#163019=CARTESIAN_POINT('Ctrl Pts',(4.24446825699994,11.6,-9.77348921500001));
#163020=CARTESIAN_POINT('Ctrl Pts',(4.24409539199995,15.2,-9.77124913400001));
#163021=CARTESIAN_POINT('Ctrl Pts',(4.24409539199995,11.6,-9.77124913400001));
#163022=CARTESIAN_POINT('Ctrl Pts',(4.24372163899995,15.2,-9.76901584600001));
#163023=CARTESIAN_POINT('Ctrl Pts',(4.24372163899995,11.6,-9.76901584600001));
#163024=CARTESIAN_POINT('Ctrl Pts',(4.24334700899994,15.2,-9.76678936100001));
#163025=CARTESIAN_POINT('Ctrl Pts',(4.24334700899994,11.6,-9.76678936100001));
#163026=CARTESIAN_POINT('Ctrl Pts',(4.24297151499994,15.2,-9.76456969300001));
#163027=CARTESIAN_POINT('Ctrl Pts',(4.24297151499994,11.6,-9.76456969300001));
#163028=CARTESIAN_POINT('Ctrl Pts',(4.24259516999994,15.2,-9.76235685300001));
#163029=CARTESIAN_POINT('Ctrl Pts',(4.24259516999994,11.6,-9.76235685300001));
#163030=CARTESIAN_POINT('Ctrl Pts',(4.24221798499994,15.2,-9.76015085200001));
#163031=CARTESIAN_POINT('Ctrl Pts',(4.24221798499994,11.6,-9.76015085200001));
#163032=CARTESIAN_POINT('Ctrl Pts',(4.24183997499994,15.2,-9.75795170200001));
#163033=CARTESIAN_POINT('Ctrl Pts',(4.24183997499994,11.6,-9.75795170200001));
#163034=CARTESIAN_POINT('Ctrl Pts',(4.24146114899994,15.2,-9.75575941500001));
#163035=CARTESIAN_POINT('Ctrl Pts',(4.24146114899994,11.6,-9.75575941500001));
#163036=CARTESIAN_POINT('Ctrl Pts',(4.24108152199994,15.2,-9.75357400100001));
#163037=CARTESIAN_POINT('Ctrl Pts',(4.24108152199994,11.6,-9.75357400100001));
#163038=CARTESIAN_POINT('Ctrl Pts',(4.24070110699994,15.2,-9.75139547400001));
#163039=CARTESIAN_POINT('Ctrl Pts',(4.24070110699994,11.6,-9.75139547400001));
#163040=CARTESIAN_POINT('Ctrl Pts',(4.24031991699994,15.2,-9.74922384400001));
#163041=CARTESIAN_POINT('Ctrl Pts',(4.24031991699994,11.6,-9.74922384400001));
#163042=CARTESIAN_POINT('Ctrl Pts',(4.23993796199994,15.2,-9.74705912500001));
#163043=CARTESIAN_POINT('Ctrl Pts',(4.23993796199994,11.6,-9.74705912500001));
#163044=CARTESIAN_POINT('Ctrl Pts',(4.23955525799994,15.2,-9.74490132500001));
#163045=CARTESIAN_POINT('Ctrl Pts',(4.23955525799994,11.6,-9.74490132500001));
#163046=CARTESIAN_POINT('Ctrl Pts',(4.23917181499994,15.2,-9.74275045900001));
#163047=CARTESIAN_POINT('Ctrl Pts',(4.23917181499994,11.6,-9.74275045900001));
#163048=CARTESIAN_POINT('Ctrl Pts',(4.23878764799994,15.2,-9.74060653900001));
#163049=CARTESIAN_POINT('Ctrl Pts',(4.23878764799994,11.6,-9.74060653900001));
#163050=CARTESIAN_POINT('Ctrl Pts',(4.23840276899994,15.2,-9.73846957500001));
#163051=CARTESIAN_POINT('Ctrl Pts',(4.23840276899994,11.6,-9.73846957500001));
#163052=CARTESIAN_POINT('Ctrl Pts',(4.23801719099994,15.2,-9.73633957900001));
#163053=CARTESIAN_POINT('Ctrl Pts',(4.23801719099994,11.6,-9.73633957900001));
#163054=CARTESIAN_POINT('Ctrl Pts',(4.23763092899994,15.2,-9.73421656400001));
#163055=CARTESIAN_POINT('Ctrl Pts',(4.23763092899994,11.6,-9.73421656400001));
#163056=CARTESIAN_POINT('Ctrl Pts',(4.23724399199994,15.2,-9.73210054100001));
#163057=CARTESIAN_POINT('Ctrl Pts',(4.23724399199994,11.6,-9.73210054100001));
#163058=CARTESIAN_POINT('Ctrl Pts',(4.23685639699994,15.2,-9.72999152300001));
#163059=CARTESIAN_POINT('Ctrl Pts',(4.23685639699994,11.6,-9.72999152300001));
#163060=CARTESIAN_POINT('Ctrl Pts',(4.23646815499994,15.2,-9.72788952200001));
#163061=CARTESIAN_POINT('Ctrl Pts',(4.23646815499994,11.6,-9.72788952200001));
#163062=CARTESIAN_POINT('Ctrl Pts',(4.23607928099995,15.2,-9.72579454900002));
#163063=CARTESIAN_POINT('Ctrl Pts',(4.23607928099995,11.6,-9.72579454900002));
#163064=CARTESIAN_POINT('Ctrl Pts',(4.23568978699994,15.2,-9.72370661700001));
#163065=CARTESIAN_POINT('Ctrl Pts',(4.23568978699994,11.6,-9.72370661700001));
#163066=CARTESIAN_POINT('Ctrl Pts',(4.23529968599994,15.2,-9.72162573800001));
#163067=CARTESIAN_POINT('Ctrl Pts',(4.23529968599994,11.6,-9.72162573800001));
#163068=CARTESIAN_POINT('Ctrl Pts',(4.23490899199995,15.2,-9.71955192300001));
#163069=CARTESIAN_POINT('Ctrl Pts',(4.23490899199995,11.6,-9.71955192300001));
#163070=CARTESIAN_POINT('Ctrl Pts',(4.23451771999994,15.2,-9.71748518500001));
#163071=CARTESIAN_POINT('Ctrl Pts',(4.23451771999994,11.6,-9.71748518500001));
#163072=CARTESIAN_POINT('Ctrl Pts',(4.23412588099994,15.2,-9.71542553700001));
#163073=CARTESIAN_POINT('Ctrl Pts',(4.23412588099994,11.6,-9.71542553700001));
#163074=CARTESIAN_POINT('Ctrl Pts',(4.23373348799994,15.2,-9.71337299000002));
#163075=CARTESIAN_POINT('Ctrl Pts',(4.23373348799994,11.6,-9.71337299000002));
#163076=CARTESIAN_POINT('Ctrl Pts',(4.23334055899994,15.2,-9.71132755800001));
#163077=CARTESIAN_POINT('Ctrl Pts',(4.23334055899994,11.6,-9.71132755800001));
#163078=CARTESIAN_POINT('Ctrl Pts',(4.23294710199994,15.2,-9.70928925100001));
#163079=CARTESIAN_POINT('Ctrl Pts',(4.23294710199994,11.6,-9.70928925100001));
#163080=CARTESIAN_POINT('Ctrl Pts',(4.23255313499994,15.2,-9.70725808200001));
#163081=CARTESIAN_POINT('Ctrl Pts',(4.23255313499994,11.6,-9.70725808200001));
#163082=CARTESIAN_POINT('Ctrl Pts',(4.23215866999994,15.2,-9.70523406400001));
#163083=CARTESIAN_POINT('Ctrl Pts',(4.23215866999994,11.6,-9.70523406400001));
#163084=CARTESIAN_POINT('Ctrl Pts',(4.23176372199995,15.2,-9.70321720900001));
#163085=CARTESIAN_POINT('Ctrl Pts',(4.23176372199995,11.6,-9.70321720900001));
#163086=CARTESIAN_POINT('Ctrl Pts',(4.23136830199994,15.2,-9.70120753000001));
#163087=CARTESIAN_POINT('Ctrl Pts',(4.23136830199994,11.6,-9.70120753000001));
#163088=CARTESIAN_POINT('Ctrl Pts',(4.23097242799995,15.2,-9.69920503800001));
#163089=CARTESIAN_POINT('Ctrl Pts',(4.23097242799995,11.6,-9.69920503800001));
#163090=CARTESIAN_POINT('Ctrl Pts',(4.23057610999995,15.2,-9.69720974700001));
#163091=CARTESIAN_POINT('Ctrl Pts',(4.23057610999995,11.6,-9.69720974700001));
#163092=CARTESIAN_POINT('Ctrl Pts',(4.23017936499994,15.2,-9.69522166900001));
#163093=CARTESIAN_POINT('Ctrl Pts',(4.23017936499994,11.6,-9.69522166900001));
#163094=CARTESIAN_POINT('Ctrl Pts',(4.22978220499994,15.2,-9.69324081500002));
#163095=CARTESIAN_POINT('Ctrl Pts',(4.22978220499994,11.6,-9.69324081500002));
#163096=CARTESIAN_POINT('Ctrl Pts',(4.22938464599994,15.2,-9.69126720100001));
#163097=CARTESIAN_POINT('Ctrl Pts',(4.22938464599994,11.6,-9.69126720100001));
#163098=CARTESIAN_POINT('Ctrl Pts',(4.22898670099995,15.2,-9.68930083700001));
#163099=CARTESIAN_POINT('Ctrl Pts',(4.22898670099995,11.6,-9.68930083700001));
#163100=CARTESIAN_POINT('Ctrl Pts',(4.22858838299994,15.2,-9.68734173600001));
#163101=CARTESIAN_POINT('Ctrl Pts',(4.22858838299994,11.6,-9.68734173600001));
#163102=CARTESIAN_POINT('Ctrl Pts',(4.22818970999994,15.2,-9.68538991100001));
#163103=CARTESIAN_POINT('Ctrl Pts',(4.22818970999994,11.6,-9.68538991100001));
#163104=CARTESIAN_POINT('Ctrl Pts',(4.22779069299995,15.2,-9.68344537500001));
#163105=CARTESIAN_POINT('Ctrl Pts',(4.22779069299995,11.6,-9.68344537500001));
#163106=CARTESIAN_POINT('Ctrl Pts',(4.22739134799994,15.2,-9.68150814100001));
#163107=CARTESIAN_POINT('Ctrl Pts',(4.22739134799994,11.6,-9.68150814100001));
#163108=CARTESIAN_POINT('Ctrl Pts',(4.22699168899995,15.2,-9.67957822000001));
#163109=CARTESIAN_POINT('Ctrl Pts',(4.22699168899995,11.6,-9.67957822000001));
#163110=CARTESIAN_POINT('Ctrl Pts',(4.22659172899994,15.2,-9.67765562600001));
#163111=CARTESIAN_POINT('Ctrl Pts',(4.22659172899994,11.6,-9.67765562600001));
#163112=CARTESIAN_POINT('Ctrl Pts',(4.22619148699994,15.2,-9.67574037200001));
#163113=CARTESIAN_POINT('Ctrl Pts',(4.22619148699994,11.6,-9.67574037200001));
#163114=CARTESIAN_POINT('Ctrl Pts',(4.22579097299994,15.2,-9.67383247200001));
#163115=CARTESIAN_POINT('Ctrl Pts',(4.22579097299994,11.6,-9.67383247200001));
#163116=CARTESIAN_POINT('Ctrl Pts',(4.22539020299994,15.2,-9.67193193700002));
#163117=CARTESIAN_POINT('Ctrl Pts',(4.22539020299994,11.6,-9.67193193700002));
#163118=CARTESIAN_POINT('Ctrl Pts',(4.22498919399994,15.2,-9.67003878000001));
#163119=CARTESIAN_POINT('Ctrl Pts',(4.22498919399994,11.6,-9.67003878000001));
#163120=CARTESIAN_POINT('Ctrl Pts',(4.22458795699994,15.2,-9.66815301400001));
#163121=CARTESIAN_POINT('Ctrl Pts',(4.22458795699994,11.6,-9.66815301400001));
#163122=CARTESIAN_POINT('Ctrl Pts',(4.22418651099994,15.2,-9.66627465400001));
#163123=CARTESIAN_POINT('Ctrl Pts',(4.22418651099994,11.6,-9.66627465400001));
#163124=CARTESIAN_POINT('Ctrl Pts',(4.22378486799994,15.2,-9.66440371000001));
#163125=CARTESIAN_POINT('Ctrl Pts',(4.22378486799994,11.6,-9.66440371000001));
#163126=CARTESIAN_POINT('Ctrl Pts',(4.22338304399995,15.2,-9.66254019800001));
#163127=CARTESIAN_POINT('Ctrl Pts',(4.22338304399995,11.6,-9.66254019800001));
#163128=CARTESIAN_POINT('Ctrl Pts',(4.22298105399994,15.2,-9.66068412900001));
#163129=CARTESIAN_POINT('Ctrl Pts',(4.22298105399994,11.6,-9.66068412900001));
#163130=CARTESIAN_POINT('Ctrl Pts',(4.22257891299994,15.2,-9.65883551800001));
#163131=CARTESIAN_POINT('Ctrl Pts',(4.22257891299994,11.6,-9.65883551800001));
#163132=CARTESIAN_POINT('Ctrl Pts',(4.22217663599994,15.2,-9.65699437700001));
#163133=CARTESIAN_POINT('Ctrl Pts',(4.22217663599994,11.6,-9.65699437700001));
#163134=CARTESIAN_POINT('Ctrl Pts',(4.22177423899995,15.2,-9.65516071900001));
#163135=CARTESIAN_POINT('Ctrl Pts',(4.22177423899995,11.6,-9.65516071900001));
#163136=CARTESIAN_POINT('Ctrl Pts',(4.22137173599994,15.2,-9.65333455800001));
#163137=CARTESIAN_POINT('Ctrl Pts',(4.22137173599994,11.6,-9.65333455800001));
#163138=CARTESIAN_POINT('Ctrl Pts',(4.22096914499994,15.2,-9.65151590700002));
#163139=CARTESIAN_POINT('Ctrl Pts',(4.22096914499994,11.6,-9.65151590700002));
#163140=CARTESIAN_POINT('Ctrl Pts',(4.22056647799994,15.2,-9.64970478000001));
#163141=CARTESIAN_POINT('Ctrl Pts',(4.22056647799994,11.6,-9.64970478000001));
#163142=CARTESIAN_POINT('Ctrl Pts',(4.22016375199994,15.2,-9.64790119000002));
#163143=CARTESIAN_POINT('Ctrl Pts',(4.22016375199994,11.6,-9.64790119000002));
#163144=CARTESIAN_POINT('Ctrl Pts',(4.21976098299994,15.2,-9.64610514900002));
#163145=CARTESIAN_POINT('Ctrl Pts',(4.21976098299994,11.6,-9.64610514900002));
#163146=CARTESIAN_POINT('Ctrl Pts',(4.21935818699995,15.2,-9.64431667300002));
#163147=CARTESIAN_POINT('Ctrl Pts',(4.21935818699995,11.6,-9.64431667300002));
#163148=CARTESIAN_POINT('Ctrl Pts',(4.21895537899994,15.2,-9.64253577300001));
#163149=CARTESIAN_POINT('Ctrl Pts',(4.21895537899994,11.6,-9.64253577300001));
#163150=CARTESIAN_POINT('Ctrl Pts',(4.21855257299994,15.2,-9.64076246400002));
#163151=CARTESIAN_POINT('Ctrl Pts',(4.21855257299994,11.6,-9.64076246400002));
#163152=CARTESIAN_POINT('Ctrl Pts',(4.21814978799994,15.2,-9.63899675900001));
#163153=CARTESIAN_POINT('Ctrl Pts',(4.21814978799994,11.6,-9.63899675900001));
#163154=CARTESIAN_POINT('Ctrl Pts',(4.21774703799994,15.2,-9.63723867200001));
#163155=CARTESIAN_POINT('Ctrl Pts',(4.21774703799994,11.6,-9.63723867200001));
#163156=CARTESIAN_POINT('Ctrl Pts',(4.21734433799995,15.2,-9.63548821700002));
#163157=CARTESIAN_POINT('Ctrl Pts',(4.21734433799995,11.6,-9.63548821700002));
#163158=CARTESIAN_POINT('Ctrl Pts',(4.21694170799995,15.2,-9.63374540800002));
#163159=CARTESIAN_POINT('Ctrl Pts',(4.21694170799995,11.6,-9.63374540800002));
#163160=CARTESIAN_POINT('Ctrl Pts',(4.21653915999994,15.2,-9.63201025700002));
#163161=CARTESIAN_POINT('Ctrl Pts',(4.21653915999994,11.6,-9.63201025700002));
#163162=CARTESIAN_POINT('Ctrl Pts',(4.21613671099994,15.2,-9.63028277900002));
#163163=CARTESIAN_POINT('Ctrl Pts',(4.21613671099994,11.6,-9.63028277900002));
#163164=CARTESIAN_POINT('Ctrl Pts',(4.21573437799994,15.2,-9.62856298800002));
#163165=CARTESIAN_POINT('Ctrl Pts',(4.21573437799994,11.6,-9.62856298800002));
#163166=CARTESIAN_POINT('Ctrl Pts',(4.21533217699994,15.2,-9.62685089700001));
#163167=CARTESIAN_POINT('Ctrl Pts',(4.21533217699994,11.6,-9.62685089700001));
#163168=CARTESIAN_POINT('Ctrl Pts',(4.21493012499994,15.2,-9.62514652000002));
#163169=CARTESIAN_POINT('Ctrl Pts',(4.21493012499994,11.6,-9.62514652000002));
#163170=CARTESIAN_POINT('Ctrl Pts',(4.21452823699994,15.2,-9.62344987300002));
#163171=CARTESIAN_POINT('Ctrl Pts',(4.21452823699994,11.6,-9.62344987300002));
#163172=CARTESIAN_POINT('Ctrl Pts',(4.21412653099994,15.2,-9.62176096700002));
#163173=CARTESIAN_POINT('Ctrl Pts',(4.21412653099994,11.6,-9.62176096700002));
#163174=CARTESIAN_POINT('Ctrl Pts',(4.21372502199994,15.2,-9.62007981800001));
#163175=CARTESIAN_POINT('Ctrl Pts',(4.21372502199994,11.6,-9.62007981800001));
#163176=CARTESIAN_POINT('Ctrl Pts',(4.21332372799994,15.2,-9.61840643900001));
#163177=CARTESIAN_POINT('Ctrl Pts',(4.21332372799994,11.6,-9.61840643900001));
#163178=CARTESIAN_POINT('Ctrl Pts',(4.21292266499994,15.2,-9.61674084500002));
#163179=CARTESIAN_POINT('Ctrl Pts',(4.21292266499994,11.6,-9.61674084500002));
#163180=CARTESIAN_POINT('Ctrl Pts',(4.21252184899994,15.2,-9.61508305000002));
#163181=CARTESIAN_POINT('Ctrl Pts',(4.21252184899994,11.6,-9.61508305000002));
#163182=CARTESIAN_POINT('Ctrl Pts',(4.21212129899994,15.2,-9.61343306700002));
#163183=CARTESIAN_POINT('Ctrl Pts',(4.21212129899994,11.6,-9.61343306700002));
#163184=CARTESIAN_POINT('Ctrl Pts',(4.21172102999994,15.2,-9.61179091100002));
#163185=CARTESIAN_POINT('Ctrl Pts',(4.21172102999994,11.6,-9.61179091100002));
#163186=CARTESIAN_POINT('Ctrl Pts',(4.21132105999994,15.2,-9.61015659800001));
#163187=CARTESIAN_POINT('Ctrl Pts',(4.21132105999994,11.6,-9.61015659800001));
#163188=CARTESIAN_POINT('Ctrl Pts',(4.21092140599994,15.2,-9.60853014000002));
#163189=CARTESIAN_POINT('Ctrl Pts',(4.21092140599994,11.6,-9.60853014000002));
#163190=CARTESIAN_POINT('Ctrl Pts',(4.21052208399994,15.2,-9.60691155200001));
#163191=CARTESIAN_POINT('Ctrl Pts',(4.21052208399994,11.6,-9.60691155200001));
#163192=CARTESIAN_POINT('Ctrl Pts',(4.21012311199994,15.2,-9.60530084900002));
#163193=CARTESIAN_POINT('Ctrl Pts',(4.21012311199994,11.6,-9.60530084900002));
#163194=CARTESIAN_POINT('Ctrl Pts',(4.20972450799994,15.2,-9.60369804500001));
#163195=CARTESIAN_POINT('Ctrl Pts',(4.20972450799994,11.6,-9.60369804500001));
#163196=CARTESIAN_POINT('Ctrl Pts',(4.20932628699994,15.2,-9.60210315400002));
#163197=CARTESIAN_POINT('Ctrl Pts',(4.20932628699994,11.6,-9.60210315400002));
#163198=CARTESIAN_POINT('Ctrl Pts',(4.20892846999994,15.2,-9.60051619200001));
#163199=CARTESIAN_POINT('Ctrl Pts',(4.20892846999994,11.6,-9.60051619200001));
#163200=CARTESIAN_POINT('Ctrl Pts',(4.20853107099994,15.2,-9.59893717100002));
#163201=CARTESIAN_POINT('Ctrl Pts',(4.20853107099994,11.6,-9.59893717100002));
#163202=CARTESIAN_POINT('Ctrl Pts',(4.20813410999994,15.2,-9.59736611000002));
#163203=CARTESIAN_POINT('Ctrl Pts',(4.20813410999994,11.6,-9.59736611000002));
#163204=CARTESIAN_POINT('Ctrl Pts',(4.20773760299994,15.2,-9.59580302000001));
#163205=CARTESIAN_POINT('Ctrl Pts',(4.20773760299994,11.6,-9.59580302000001));
#163206=CARTESIAN_POINT('Ctrl Pts',(4.20734156899994,15.2,-9.59424791600001));
#163207=CARTESIAN_POINT('Ctrl Pts',(4.20734156899994,11.6,-9.59424791600001));
#163208=CARTESIAN_POINT('Ctrl Pts',(4.20694602499994,15.2,-9.59270081500001));
#163209=CARTESIAN_POINT('Ctrl Pts',(4.20694602499994,11.6,-9.59270081500001));
#163210=CARTESIAN_POINT('Ctrl Pts',(4.20655098899995,15.2,-9.59116173000002));
#163211=CARTESIAN_POINT('Ctrl Pts',(4.20655098899995,11.6,-9.59116173000002));
#163212=CARTESIAN_POINT('Ctrl Pts',(4.20615647899994,15.2,-9.58963067600001));
#163213=CARTESIAN_POINT('Ctrl Pts',(4.20615647899994,11.6,-9.58963067600001));
#163214=CARTESIAN_POINT('Ctrl Pts',(4.20576251399994,15.2,-9.58810766900001));
#163215=CARTESIAN_POINT('Ctrl Pts',(4.20576251399994,11.6,-9.58810766900001));
#163216=CARTESIAN_POINT('Ctrl Pts',(4.20536911099994,15.2,-9.58659272300002));
#163217=CARTESIAN_POINT('Ctrl Pts',(4.20536911099994,11.6,-9.58659272300002));
#163218=CARTESIAN_POINT('Ctrl Pts',(4.20497628799995,15.2,-9.58508585300001));
#163219=CARTESIAN_POINT('Ctrl Pts',(4.20497628799995,11.6,-9.58508585300001));
#163220=CARTESIAN_POINT('Ctrl Pts',(4.20458406399994,15.2,-9.58358707500001));
#163221=CARTESIAN_POINT('Ctrl Pts',(4.20458406399994,11.6,-9.58358707500001));
#163222=CARTESIAN_POINT('Ctrl Pts',(4.20419245599994,15.2,-9.58209640400002));
#163223=CARTESIAN_POINT('Ctrl Pts',(4.20419245599994,11.6,-9.58209640400002));
#163224=CARTESIAN_POINT('Ctrl Pts',(4.20380148499994,15.2,-9.58061385400002));
#163225=CARTESIAN_POINT('Ctrl Pts',(4.20380148499994,11.6,-9.58061385400002));
#163226=CARTESIAN_POINT('Ctrl Pts',(4.20341116699994,15.2,-9.57913944200002));
#163227=CARTESIAN_POINT('Ctrl Pts',(4.20341116699994,11.6,-9.57913944200002));
#163228=CARTESIAN_POINT('Ctrl Pts',(4.20302152299994,15.2,-9.57767318000002));
#163229=CARTESIAN_POINT('Ctrl Pts',(4.20302152299994,11.6,-9.57767318000002));
#163230=CARTESIAN_POINT('Ctrl Pts',(4.20263256899994,15.2,-9.57621508900001));
#163231=CARTESIAN_POINT('Ctrl Pts',(4.20263256899994,11.6,-9.57621508900001));
#163232=CARTESIAN_POINT('Ctrl Pts',(4.20224432599994,15.2,-9.57476517800002));
#163233=CARTESIAN_POINT('Ctrl Pts',(4.20224432599994,11.6,-9.57476517800002));
#163234=CARTESIAN_POINT('Ctrl Pts',(4.20185681099994,15.2,-9.57332346700002));
#163235=CARTESIAN_POINT('Ctrl Pts',(4.20185681099994,11.6,-9.57332346700002));
#163236=CARTESIAN_POINT('Ctrl Pts',(4.20147004499994,15.2,-9.57188997100002));
#163237=CARTESIAN_POINT('Ctrl Pts',(4.20147004499994,11.6,-9.57188997100002));
#163238=CARTESIAN_POINT('Ctrl Pts',(4.20108404499994,15.2,-9.57046470300002));
#163239=CARTESIAN_POINT('Ctrl Pts',(4.20108404499994,11.6,-9.57046470300002));
#163240=CARTESIAN_POINT('Ctrl Pts',(4.20069883099994,15.2,-9.56904768000001));
#163241=CARTESIAN_POINT('Ctrl Pts',(4.20069883099994,11.6,-9.56904768000001));
#163242=CARTESIAN_POINT('Ctrl Pts',(4.20031442399995,15.2,-9.56763891900002));
#163243=CARTESIAN_POINT('Ctrl Pts',(4.20031442399995,11.6,-9.56763891900002));
#163244=CARTESIAN_POINT('Ctrl Pts',(4.19993083999994,15.2,-9.56623843500001));
#163245=CARTESIAN_POINT('Ctrl Pts',(4.19993083999994,11.6,-9.56623843500001));
#163246=CARTESIAN_POINT('Ctrl Pts',(4.19954810099994,15.2,-9.56484624100002));
#163247=CARTESIAN_POINT('Ctrl Pts',(4.19954810099994,11.6,-9.56484624100002));
#163248=CARTESIAN_POINT('Ctrl Pts',(4.19916622499994,15.2,-9.56346235600002));
#163249=CARTESIAN_POINT('Ctrl Pts',(4.19916622499994,11.6,-9.56346235600002));
#163250=CARTESIAN_POINT('Ctrl Pts',(4.19878523199994,15.2,-9.56208679600002));
#163251=CARTESIAN_POINT('Ctrl Pts',(4.19878523199994,11.6,-9.56208679600002));
#163252=CARTESIAN_POINT('Ctrl Pts',(4.19840514099994,15.2,-9.56071957500002));
#163253=CARTESIAN_POINT('Ctrl Pts',(4.19840514099994,11.6,-9.56071957500002));
#163254=CARTESIAN_POINT('Ctrl Pts',(4.19802597299994,15.2,-9.55936071100002));
#163255=CARTESIAN_POINT('Ctrl Pts',(4.19802597299994,11.6,-9.55936071100002));
#163256=CARTESIAN_POINT('Ctrl Pts',(4.19764774699994,15.2,-9.55801021800001));
#163257=CARTESIAN_POINT('Ctrl Pts',(4.19764774699994,11.6,-9.55801021800001));
#163258=CARTESIAN_POINT('Ctrl Pts',(4.19727048399994,15.2,-9.55666811400001));
#163259=CARTESIAN_POINT('Ctrl Pts',(4.19727048399994,11.6,-9.55666811400001));
#163260=CARTESIAN_POINT('Ctrl Pts',(4.19689420199994,15.2,-9.55533441300001));
#163261=CARTESIAN_POINT('Ctrl Pts',(4.19689420199994,11.6,-9.55533441300001));
#163262=CARTESIAN_POINT('Ctrl Pts',(4.19651892299994,15.2,-9.55400913400002));
#163263=CARTESIAN_POINT('Ctrl Pts',(4.19651892299994,11.6,-9.55400913400002));
#163264=CARTESIAN_POINT('Ctrl Pts',(4.19614466599994,15.2,-9.55269229000002));
#163265=CARTESIAN_POINT('Ctrl Pts',(4.19614466599994,11.6,-9.55269229000002));
#163266=CARTESIAN_POINT('Ctrl Pts',(4.19577145099994,15.2,-9.55138390000002));
#163267=CARTESIAN_POINT('Ctrl Pts',(4.19577145099994,11.6,-9.55138390000002));
#163268=CARTESIAN_POINT('Ctrl Pts',(4.19539930099995,15.2,-9.55008398000002));
#163269=CARTESIAN_POINT('Ctrl Pts',(4.19539930099995,11.6,-9.55008398000002));
#163270=CARTESIAN_POINT('Ctrl Pts',(4.19502823399994,15.2,-9.54879254600002));
#163271=CARTESIAN_POINT('Ctrl Pts',(4.19502823399994,11.6,-9.54879254600002));
#163272=CARTESIAN_POINT('Ctrl Pts',(4.19465827099994,15.2,-9.54750961300002));
#163273=CARTESIAN_POINT('Ctrl Pts',(4.19465827099994,11.6,-9.54750961300002));
#163274=CARTESIAN_POINT('Ctrl Pts',(4.19428943299994,15.2,-9.54623520100002));
#163275=CARTESIAN_POINT('Ctrl Pts',(4.19428943299994,11.6,-9.54623520100002));
#163276=CARTESIAN_POINT('Ctrl Pts',(4.19392174099994,15.2,-9.54496932300002));
#163277=CARTESIAN_POINT('Ctrl Pts',(4.19392174099994,11.6,-9.54496932300002));
#163278=CARTESIAN_POINT('Ctrl Pts',(4.19355521499994,15.2,-9.54371199800002));
#163279=CARTESIAN_POINT('Ctrl Pts',(4.19355521499994,11.6,-9.54371199800002));
#163280=CARTESIAN_POINT('Ctrl Pts',(4.19318987699994,15.2,-9.54246324200002));
#163281=CARTESIAN_POINT('Ctrl Pts',(4.19318987699994,11.6,-9.54246324200002));
#163282=CARTESIAN_POINT('Ctrl Pts',(4.19282574799994,15.2,-9.54122307200001));
#163283=CARTESIAN_POINT('Ctrl Pts',(4.19282574799994,11.6,-9.54122307200001));
#163284=CARTESIAN_POINT('Ctrl Pts',(4.19246284799994,15.2,-9.53999150600002));
#163285=CARTESIAN_POINT('Ctrl Pts',(4.19246284799994,11.6,-9.53999150600002));
#163286=CARTESIAN_POINT('Ctrl Pts',(4.19210119999994,15.2,-9.53876855900001));
#163287=CARTESIAN_POINT('Ctrl Pts',(4.19210119999994,11.6,-9.53876855900001));
#163288=CARTESIAN_POINT('Ctrl Pts',(4.19174082499994,15.2,-9.53755424900002));
#163289=CARTESIAN_POINT('Ctrl Pts',(4.19174082499994,11.6,-9.53755424900002));
#163290=CARTESIAN_POINT('Ctrl Pts',(4.19138174199994,15.2,-9.53634859200001));
#163291=CARTESIAN_POINT('Ctrl Pts',(4.19138174199994,11.6,-9.53634859200001));
#163292=CARTESIAN_POINT('Ctrl Pts',(4.19102397699994,15.2,-9.53515160700002));
#163293=CARTESIAN_POINT('Ctrl Pts',(4.19102397699994,11.6,-9.53515160700002));
#163294=CARTESIAN_POINT('Ctrl Pts',(4.19066754799994,15.2,-9.53396331100001));
#163295=CARTESIAN_POINT('Ctrl Pts',(4.19066754799994,11.6,-9.53396331100001));
#163296=CARTESIAN_POINT('Ctrl Pts',(4.19031247699994,15.2,-9.53278371900002));
#163297=CARTESIAN_POINT('Ctrl Pts',(4.19031247699994,11.6,-9.53278371900002));
#163298=CARTESIAN_POINT('Ctrl Pts',(4.18995878899994,15.2,-9.53161285200002));
#163299=CARTESIAN_POINT('Ctrl Pts',(4.18995878899994,11.6,-9.53161285200002));
#163300=CARTESIAN_POINT('Ctrl Pts',(4.18960650399994,15.2,-9.53045072400002));
#163301=CARTESIAN_POINT('Ctrl Pts',(4.18960650399994,11.6,-9.53045072400002));
#163302=CARTESIAN_POINT('Ctrl Pts',(4.18925564299994,15.2,-9.52929735300001));
#163303=CARTESIAN_POINT('Ctrl Pts',(4.18925564299994,11.6,-9.52929735300001));
#163304=CARTESIAN_POINT('Ctrl Pts',(4.18890623099994,15.2,-9.52815275900001));
#163305=CARTESIAN_POINT('Ctrl Pts',(4.18890623099994,11.6,-9.52815275900001));
#163306=CARTESIAN_POINT('Ctrl Pts',(4.18855828699995,15.2,-9.52701695700001));
#163307=CARTESIAN_POINT('Ctrl Pts',(4.18855828699995,11.6,-9.52701695700001));
#163308=CARTESIAN_POINT('Ctrl Pts',(4.18821183699994,15.2,-9.52588996600002));
#163309=CARTESIAN_POINT('Ctrl Pts',(4.18821183699994,11.6,-9.52588996600002));
#163310=CARTESIAN_POINT('Ctrl Pts',(4.18786690099994,15.2,-9.52477180400002));
#163311=CARTESIAN_POINT('Ctrl Pts',(4.18786690099994,11.6,-9.52477180400002));
#163312=CARTESIAN_POINT('Ctrl Pts',(4.18752350299994,15.2,-9.52366248700002));
#163313=CARTESIAN_POINT('Ctrl Pts',(4.18752350299994,11.6,-9.52366248700002));
#163314=CARTESIAN_POINT('Ctrl Pts',(4.18718166499994,15.2,-9.52256203500001));
#163315=CARTESIAN_POINT('Ctrl Pts',(4.18718166499994,11.6,-9.52256203500001));
#163316=CARTESIAN_POINT('Ctrl Pts',(4.18684140999994,15.2,-9.52147046600002));
#163317=CARTESIAN_POINT('Ctrl Pts',(4.18684140999994,11.6,-9.52147046600002));
#163318=CARTESIAN_POINT('Ctrl Pts',(4.18650276099994,15.2,-9.52038779600001));
#163319=CARTESIAN_POINT('Ctrl Pts',(4.18650276099994,11.6,-9.52038779600001));
#163320=CARTESIAN_POINT('Ctrl Pts',(4.18616574199994,15.2,-9.51931404500002));
#163321=CARTESIAN_POINT('Ctrl Pts',(4.18616574199994,11.6,-9.51931404500002));
#163322=CARTESIAN_POINT('Ctrl Pts',(4.18583037599995,15.2,-9.51824923000002));
#163323=CARTESIAN_POINT('Ctrl Pts',(4.18583037599995,11.6,-9.51824923000002));
#163324=CARTESIAN_POINT('Ctrl Pts',(4.18549668599994,15.2,-9.51719337100002));
#163325=CARTESIAN_POINT('Ctrl Pts',(4.18549668599994,11.6,-9.51719337100002));
#163326=CARTESIAN_POINT('Ctrl Pts',(4.18516469499994,15.2,-9.51614648400002));
#163327=CARTESIAN_POINT('Ctrl Pts',(4.18516469499994,11.6,-9.51614648400002));
#163328=CARTESIAN_POINT('Ctrl Pts',(4.18483442699995,15.2,-9.51510858900001));
#163329=CARTESIAN_POINT('Ctrl Pts',(4.18483442699995,11.6,-9.51510858900001));
#163330=CARTESIAN_POINT('Ctrl Pts',(4.18450590599994,15.2,-9.51407970500001));
#163331=CARTESIAN_POINT('Ctrl Pts',(4.18450590599994,11.6,-9.51407970500001));
#163332=CARTESIAN_POINT('Ctrl Pts',(4.18417915599994,15.2,-9.51305984900002));
#163333=CARTESIAN_POINT('Ctrl Pts',(4.18417915599994,11.6,-9.51305984900002));
#163334=CARTESIAN_POINT('Ctrl Pts',(4.18385420099994,15.2,-9.51204904000001));
#163335=CARTESIAN_POINT('Ctrl Pts',(4.18385420099994,11.6,-9.51204904000001));
#163336=CARTESIAN_POINT('Ctrl Pts',(4.18353106499994,15.2,-9.51104729700001));
#163337=CARTESIAN_POINT('Ctrl Pts',(4.18353106499994,11.6,-9.51104729700001));
#163338=CARTESIAN_POINT('Ctrl Pts',(4.18320977199994,15.2,-9.51005463900002));
#163339=CARTESIAN_POINT('Ctrl Pts',(4.18320977199994,11.6,-9.51005463900002));
#163340=CARTESIAN_POINT('Ctrl Pts',(4.18289034599994,15.2,-9.50907108500001));
#163341=CARTESIAN_POINT('Ctrl Pts',(4.18289034599994,11.6,-9.50907108500001));
#163342=CARTESIAN_POINT('Ctrl Pts',(4.18257281199994,15.2,-9.50809665400002));
#163343=CARTESIAN_POINT('Ctrl Pts',(4.18257281199994,11.6,-9.50809665400002));
#163344=CARTESIAN_POINT('Ctrl Pts',(4.18225719599994,15.2,-9.50713136500001));
#163345=CARTESIAN_POINT('Ctrl Pts',(4.18225719599994,11.6,-9.50713136500001));
#163346=CARTESIAN_POINT('Ctrl Pts',(4.18194351899994,15.2,-9.50617523600001));
#163347=CARTESIAN_POINT('Ctrl Pts',(4.18194351899994,11.6,-9.50617523600001));
#163348=CARTESIAN_POINT('Ctrl Pts',(4.18163180999994,15.2,-9.50522828700001));
#163349=CARTESIAN_POINT('Ctrl Pts',(4.18163180999994,11.6,-9.50522828700001));
#163350=CARTESIAN_POINT('Ctrl Pts',(4.18132209099995,15.2,-9.50429053800002));
#163351=CARTESIAN_POINT('Ctrl Pts',(4.18132209099995,11.6,-9.50429053800002));
#163352=CARTESIAN_POINT('Ctrl Pts',(4.18101438899994,15.2,-9.50336200800002));
#163353=CARTESIAN_POINT('Ctrl Pts',(4.18101438899994,11.6,-9.50336200800002));
#163354=CARTESIAN_POINT('Ctrl Pts',(4.18070872899994,15.2,-9.50244271600001));
#163355=CARTESIAN_POINT('Ctrl Pts',(4.18070872899994,11.6,-9.50244271600001));
#163356=CARTESIAN_POINT('Ctrl Pts',(4.18040513599994,15.2,-9.50153268300001));
#163357=CARTESIAN_POINT('Ctrl Pts',(4.18040513599994,11.6,-9.50153268300001));
#163358=CARTESIAN_POINT('Ctrl Pts',(4.18010363499994,15.2,-9.50063192600001));
#163359=CARTESIAN_POINT('Ctrl Pts',(4.18010363499994,11.6,-9.50063192600001));
#163360=CARTESIAN_POINT('Ctrl Pts',(4.17980425199994,15.2,-9.49974046600002));
#163361=CARTESIAN_POINT('Ctrl Pts',(4.17980425199994,11.6,-9.49974046600002));
#163362=CARTESIAN_POINT('Ctrl Pts',(4.17950701299994,15.2,-9.49885832400001));
#163363=CARTESIAN_POINT('Ctrl Pts',(4.17950701299994,11.6,-9.49885832400001));
#163364=CARTESIAN_POINT('Ctrl Pts',(4.17921364399994,15.2,-9.49799054600001));
#163365=CARTESIAN_POINT('Ctrl Pts',(4.17921364399994,11.6,-9.49799054600001));
#163366=CARTESIAN_POINT('Ctrl Pts',(4.17898101999994,15.2,-9.49730470700001));
#163367=CARTESIAN_POINT('Ctrl Pts',(4.17898101999994,11.6,-9.49730470700001));
#163368=CARTESIAN_POINT('Ctrl Pts',(4.17880795399994,15.2,-9.49679570900001));
#163369=CARTESIAN_POINT('Ctrl Pts',(4.17880795399994,11.6,-9.49679570900001));
#163370=CARTESIAN_POINT('Ctrl Pts',(4.17869357199994,15.2,-9.49645984600001));
#163371=CARTESIAN_POINT('Ctrl Pts',(4.17869357199994,11.6,-9.49645984600001));
#163372=CARTESIAN_POINT('Ctrl Pts',(4.17863732199994,15.2,-9.49629481100001));
#163373=CARTESIAN_POINT('Ctrl Pts',(4.17863732199994,11.6,-9.49629481100001));
#163374=CARTESIAN_POINT('',(4.17863732208248,12.2,-9.4962948105209));
#163375=CARTESIAN_POINT('',(4.17863732208248,15.2,-9.4962948105209));
#163376=CARTESIAN_POINT('',(4.17863732199994,12.2,-9.49629481000001));
#163377=CARTESIAN_POINT('Ctrl Pts',(4.27433546799994,12.2,-10.676144262));
#163378=CARTESIAN_POINT('Ctrl Pts',(4.2746137680505,12.2,-10.6723314813074));
#163379=CARTESIAN_POINT('Ctrl Pts',(4.2748872709057,12.2,-10.6685249864456));
#163380=CARTESIAN_POINT('Ctrl Pts',(4.2751559909999,12.2,-10.6647247761647));
#163381=CARTESIAN_POINT('Ctrl Pts',(4.2754247110941,12.2,-10.6609245658837));
#163382=CARTESIAN_POINT('Ctrl Pts',(4.27568864392904,12.2,-10.6571306401352));
#163383=CARTESIAN_POINT('Ctrl Pts',(4.27594779972479,12.2,-10.6533430149995));
#163384=CARTESIAN_POINT('Ctrl Pts',(4.27620695552054,12.2,-10.6495553898638));
#163385=CARTESIAN_POINT('Ctrl Pts',(4.27646133373731,12.2,-10.6457740655533));
#163386=CARTESIAN_POINT('Ctrl Pts',(4.27671095972889,12.2,-10.6419990773979));
#163387=CARTESIAN_POINT('Ctrl Pts',(4.27696058576582,12.2,-10.6382240885568));
#163388=CARTESIAN_POINT('Ctrl Pts',(4.27720545978473,12.2,-10.6344554361257));
#163389=CARTESIAN_POINT('Ctrl Pts',(4.27744560977733,12.2,-10.6306931631631));
#163390=CARTESIAN_POINT('Ctrl Pts',(4.27768575972629,12.2,-10.626930890884));
#163391=CARTESIAN_POINT('Ctrl Pts',(4.27792118546717,12.2,-10.6231749954379));
#163392=CARTESIAN_POINT('Ctrl Pts',(4.27815191029171,12.2,-10.6194255110747));
#163393=CARTESIAN_POINT('Ctrl Pts',(4.27845954337713,12.2,-10.6144261988175));
#163394=CARTESIAN_POINT('Ctrl Pts',(4.27875881764401,12.2,-10.6094382810372));
#163395=CARTESIAN_POINT('Ctrl Pts',(4.27904978419104,12.2,-10.6044618319721));
#163396=CARTESIAN_POINT('Ctrl Pts',(4.27934075077772,12.2,-10.5994853822291));
#163397=CARTESIAN_POINT('Ctrl Pts',(4.27962340913847,12.2,-10.5945204014255));
#163398=CARTESIAN_POINT('Ctrl Pts',(4.279897819764,12.2,-10.5895669733785));
#163399=CARTESIAN_POINT('Ctrl Pts',(4.28010362771445,12.2,-10.5858519026807));
#163400=CARTESIAN_POINT('Ctrl Pts',(4.28030479579045,12.2,-10.5821433307155));
#163401=CARTESIAN_POINT('Ctrl Pts',(4.28050134774165,12.2,-10.5784412905166));
#163402=CARTESIAN_POINT('Ctrl Pts',(4.28069789969284,12.2,-10.5747392503178));
#163403=CARTESIAN_POINT('Ctrl Pts',(4.28088983600255,12.2,-10.5710437420354));
#163404=CARTESIAN_POINT('Ctrl Pts',(4.28107717949615,12.2,-10.5673547988772));
#163405=CARTESIAN_POINT('Ctrl Pts',(4.28132697084363,12.2,-10.5624362075528));
#163406=CARTESIAN_POINT('Ctrl Pts',(4.28156859751846,12.2,-10.5575292890111));
#163407=CARTESIAN_POINT('Ctrl Pts',(4.28180211804215,12.2,-10.5526341220564));
#163408=CARTESIAN_POINT('Ctrl Pts',(4.28197725841901,12.2,-10.5489627471738));
#163409=CARTESIAN_POINT('Ctrl Pts',(4.28214783862442,12.2,-10.5452979845345));
#163410=CARTESIAN_POINT('Ctrl Pts',(4.28231388403466,12.2,-10.5416398658764));
#163411=CARTESIAN_POINT('Ctrl Pts',(4.28247992944491,12.2,-10.5379817472182));
#163412=CARTESIAN_POINT('Ctrl Pts',(4.28264143902235,12.2,-10.5343302737509));
#163413=CARTESIAN_POINT('Ctrl Pts',(4.28279843847498,12.2,-10.5306854804666));
#163414=CARTESIAN_POINT('Ctrl Pts',(4.28295543792761,12.2,-10.5270406871824));
#163415=CARTESIAN_POINT('Ctrl Pts',(4.28310792682209,12.2,-10.5234025726479));
#163416=CARTESIAN_POINT('Ctrl Pts',(4.2832559306921,12.2,-10.5197711724042));
#163417=CARTESIAN_POINT('Ctrl Pts',(4.28340393456211,12.2,-10.5161397721606));
#163418=CARTESIAN_POINT('Ctrl Pts',(4.28354745203728,12.2,-10.5125150865667));
#163419=CARTESIAN_POINT('Ctrl Pts',(4.28368650949803,12.2,-10.508897148225));
#163420=CARTESIAN_POINT('Ctrl Pts',(4.28382556695877,12.2,-10.5052792098833));
#163421=CARTESIAN_POINT('Ctrl Pts',(4.28396016469238,12.2,-10.5016680202057));
#163422=CARTESIAN_POINT('Ctrl Pts',(4.28409032672993,12.2,-10.4980636135024));
#163423=CARTESIAN_POINT('Ctrl Pts',(4.28422048879112,12.2,-10.4944592061443));
#163424=CARTESIAN_POINT('Ctrl Pts',(4.28434621655939,12.2,-10.4908615818381));
#163425=CARTESIAN_POINT('Ctrl Pts',(4.28446753503475,12.2,-10.4872707754838));
#163426=CARTESIAN_POINT('Ctrl Pts',(4.28458885348807,12.2,-10.4836799697819));
#163427=CARTESIAN_POINT('Ctrl Pts',(4.28470576256664,12.2,-10.4800959827796));
#163428=CARTESIAN_POINT('Ctrl Pts',(4.28481828806217,12.2,-10.4765188476185));
#163429=CARTESIAN_POINT('Ctrl Pts',(4.2849308135577,12.2,-10.4729417124574));
#163430=CARTESIAN_POINT('Ctrl Pts',(4.28503895598708,12.2,-10.4693714302705));
#163431=CARTESIAN_POINT('Ctrl Pts',(4.28514274052498,12.2,-10.4658080359833));
#163432=CARTESIAN_POINT('Ctrl Pts',(4.28524652506287,12.2,-10.4622446416961));
#163433=CARTESIAN_POINT('Ctrl Pts',(4.28534595230928,12.2,-10.4586881344586));
#163434=CARTESIAN_POINT('Ctrl Pts',(4.28544104922287,12.2,-10.455138550712));
#163435=CARTESIAN_POINT('Ctrl Pts',(4.28553614613646,12.2,-10.4515889669654));
#163436=CARTESIAN_POINT('Ctrl Pts',(4.28562691053153,12.2,-10.4480463062664));
#163437=CARTESIAN_POINT('Ctrl Pts',(4.28571337194987,12.2,-10.4445106034258));
#163438=CARTESIAN_POINT('Ctrl Pts',(4.28582865385147,12.2,-10.4397963325434));
#163439=CARTESIAN_POINT('Ctrl Pts',(4.28593628328645,12.2,-10.4350944329854));
#163440=CARTESIAN_POINT('Ctrl Pts',(4.28603632329141,12.2,-10.4304049863417));
#163441=CARTESIAN_POINT('Ctrl Pts',(4.28611135328832,12.2,-10.4268879016785));
#163442=CARTESIAN_POINT('Ctrl Pts',(4.28618211403573,12.2,-10.4233778230227));
#163443=CARTESIAN_POINT('Ctrl Pts',(4.28624863444998,12.2,-10.419874785275));
#163444=CARTESIAN_POINT('Ctrl Pts',(4.28631515486423,12.2,-10.4163717475272));
#163445=CARTESIAN_POINT('Ctrl Pts',(4.28637743254532,12.2,-10.4128757500875));
#163446=CARTESIAN_POINT('Ctrl Pts',(4.28643549696024,12.2,-10.4093868298804));
#163447=CARTESIAN_POINT('Ctrl Pts',(4.28649356137516,12.2,-10.4058979096732));
#163448=CARTESIAN_POINT('Ctrl Pts',(4.28654741123916,12.2,-10.4024160662705));
#163449=CARTESIAN_POINT('Ctrl Pts',(4.28659707424032,12.2,-10.398941335389));
#163450=CARTESIAN_POINT('Ctrl Pts',(4.28664673724149,12.2,-10.3954666045075));
#163451=CARTESIAN_POINT('Ctrl Pts',(4.28669221347523,12.2,-10.3919989867296));
#163452=CARTESIAN_POINT('Ctrl Pts',(4.2867335309743,12.2,-10.388538517021));
#163453=CARTESIAN_POINT('Ctrl Pts',(4.28677484848087,12.2,-10.3850780466838));
#163454=CARTESIAN_POINT('Ctrl Pts',(4.2868120067696,12.2,-10.3816247246152));
#163455=CARTESIAN_POINT('Ctrl Pts',(4.28684503473217,12.2,-10.3781785877404));
#163456=CARTESIAN_POINT('Ctrl Pts',(4.28690008132845,12.2,-10.372435027117));
#163457=CARTESIAN_POINT('Ctrl Pts',(4.28694365195511,12.2,-10.3667114235912));
#163458=CARTESIAN_POINT('Ctrl Pts',(4.28697588028752,12.2,-10.3610079455373));
#163459=CARTESIAN_POINT('Ctrl Pts',(4.28699521728626,12.2,-10.3575858588293));
#163460=CARTESIAN_POINT('Ctrl Pts',(4.28701047146908,12.2,-10.3541710171863));
#163461=CARTESIAN_POINT('Ctrl Pts',(4.28702167001043,12.2,-10.3507634568491));
#163462=CARTESIAN_POINT('Ctrl Pts',(4.28703286855178,12.2,-10.3473558965118));
#163463=CARTESIAN_POINT('Ctrl Pts',(4.28704001178405,12.2,-10.3439556180897));
#163464=CARTESIAN_POINT('Ctrl Pts',(4.28704312978358,12.2,-10.3405626583803));
#163465=CARTESIAN_POINT('Ctrl Pts',(4.28704624778312,12.2,-10.3371696986708));
#163466=CARTESIAN_POINT('Ctrl Pts',(4.28704533964979,12.2,-10.3337840569105));
#163467=CARTESIAN_POINT('Ctrl Pts',(4.28704043477497,12.2,-10.3304057702));
#163468=CARTESIAN_POINT('Ctrl Pts',(4.28703552990015,12.2,-10.3270274834894));
#163469=CARTESIAN_POINT('Ctrl Pts',(4.28702662958383,12.2,-10.3236565510785));
#163470=CARTESIAN_POINT('Ctrl Pts',(4.28701376075131,12.2,-10.320293011825));
#163471=CARTESIAN_POINT('Ctrl Pts',(4.28700089191879,12.2,-10.3169294725716));
#163472=CARTESIAN_POINT('Ctrl Pts',(4.28698405667044,12.2,-10.3135733256111));
#163473=CARTESIAN_POINT('Ctrl Pts',(4.28696328375395,12.2,-10.3102246058979));
#163474=CARTESIAN_POINT('Ctrl Pts',(4.28694251083746,12.2,-10.3068758861848));
#163475=CARTESIAN_POINT('Ctrl Pts',(4.28691780063797,12.2,-10.3035345972566));
#163476=CARTESIAN_POINT('Ctrl Pts',(4.28688918276454,12.2,-10.3002007732101));
#163477=CARTESIAN_POINT('Ctrl Pts',(4.2868510255965,12.2,-10.2957556740776));
#163478=CARTESIAN_POINT('Ctrl Pts',(4.28680592245558,12.2,-10.2913238493185));
#163479=CARTESIAN_POINT('Ctrl Pts',(4.28675394450831,12.2,-10.2869053859666));
#163480=CARTESIAN_POINT('Ctrl Pts',(4.28670196656103,12.2,-10.2824869226147));
#163481=CARTESIAN_POINT('Ctrl Pts',(4.28664311386295,12.2,-10.2780818205838));
#163482=CARTESIAN_POINT('Ctrl Pts',(4.28657745924757,12.2,-10.2736901699569));
#163483=CARTESIAN_POINT('Ctrl Pts',(4.28649539099176,12.2,-10.2682006075709));
#163484=CARTESIAN_POINT('Ctrl Pts',(4.28640269561802,12.2,-10.2627320619871));
#163485=CARTESIAN_POINT('Ctrl Pts',(4.28629951500513,12.2,-10.2572847079958));
#163486=CARTESIAN_POINT('Ctrl Pts',(4.28621697050132,12.2,-10.2529268240903));
#163487=CARTESIAN_POINT('Ctrl Pts',(4.28612771656075,12.2,-10.2485825037332));
#163488=CARTESIAN_POINT('Ctrl Pts',(4.28603182799997,12.2,-10.244251835775));
#163489=CARTESIAN_POINT('Ctrl Pts',(4.28593593943919,12.2,-10.2399211678167));
#163490=CARTESIAN_POINT('Ctrl Pts',(4.28583341522764,12.2,-10.2356041526906));
#163491=CARTESIAN_POINT('Ctrl Pts',(4.2857243319988,12.2,-10.231300882013));
#163492=CARTESIAN_POINT('Ctrl Pts',(4.28561524878483,12.2,-10.2269976119218));
#163493=CARTESIAN_POINT('Ctrl Pts',(4.28549960651005,12.2,-10.22270808517));
#163494=CARTESIAN_POINT('Ctrl Pts',(4.28537748124172,12.2,-10.2184323937779));
#163495=CARTESIAN_POINT('Ctrl Pts',(4.28525535595675,12.2,-10.2141567018032));
#163496=CARTESIAN_POINT('Ctrl Pts',(4.28512674726368,12.2,-10.2098948440522));
#163497=CARTESIAN_POINT('Ctrl Pts',(4.28499173347789,12.2,-10.2056469128221));
#163498=CARTESIAN_POINT('Ctrl Pts',(4.2848567197105,12.2,-10.2013989821708));
#163499=CARTESIAN_POINT('Ctrl Pts',(4.28471530159672,12.2,-10.1971649792982));
#163500=CARTESIAN_POINT('Ctrl Pts',(4.28456755522032,12.2,-10.1929449945867));
#163501=CARTESIAN_POINT('Ctrl Pts',(4.28441980882379,12.2,-10.1887250093003));
#163502=CARTESIAN_POINT('Ctrl Pts',(4.28426573658285,12.2,-10.1845190427645));
#163503=CARTESIAN_POINT('Ctrl Pts',(4.28410541601,12.2,-10.1803271873834));
#163504=CARTESIAN_POINT('Ctrl Pts',(4.283945095459,12.2,-10.1761353325735));
#163505=CARTESIAN_POINT('Ctrl Pts',(4.28377852752729,12.2,-10.1719575896982));
#163506=CARTESIAN_POINT('Ctrl Pts',(4.28360579176403,12.2,-10.1677940523155));
#163507=CARTESIAN_POINT('Ctrl Pts',(4.28343305597724,12.2,-10.1636305143654));
#163508=CARTESIAN_POINT('Ctrl Pts',(4.28325415353694,12.2,-10.1594811802754));
#163509=CARTESIAN_POINT('Ctrl Pts',(4.28306916502645,12.2,-10.155346146162));
#163510=CARTESIAN_POINT('Ctrl Pts',(4.28288417654118,12.2,-10.1512111126121));
#163511=CARTESIAN_POINT('Ctrl Pts',(4.2826931009273,12.2,-10.1470903770499));
#163512=CARTESIAN_POINT('Ctrl Pts',(4.2824960230452,12.2,-10.1429840348459));
#163513=CARTESIAN_POINT('Ctrl Pts',(4.28224967567244,12.2,-10.1378511066713));
#163514=CARTESIAN_POINT('Ctrl Pts',(4.2819939471612,12.2,-10.1327406666618));
#163515=CARTESIAN_POINT('Ctrl Pts',(4.28172900000891,12.2,-10.1276529028412));
#163516=CARTESIAN_POINT('Ctrl Pts',(4.28151704227552,12.2,-10.1235826915628));
#163517=CARTESIAN_POINT('Ctrl Pts',(4.28129918608864,12.2,-10.1195269929862));
#163518=CARTESIAN_POINT('Ctrl Pts',(4.28107551496496,12.2,-10.1154859017114));
#163519=CARTESIAN_POINT('Ctrl Pts',(4.2807959260756,12.2,-10.1104345378932));
#163520=CARTESIAN_POINT('Ctrl Pts',(4.28050725211425,12.2,-10.1054059961993));
#163521=CARTESIAN_POINT('Ctrl Pts',(4.28020965919712,12.2,-10.1004004698811));
#163522=CARTESIAN_POINT('Ctrl Pts',(4.27997158488287,12.2,-10.0963960491538));
#163523=CARTESIAN_POINT('Ctrl Pts',(4.27972780382215,12.2,-10.092406356499));
#163524=CARTESIAN_POINT('Ctrl Pts',(4.27947840205279,12.2,-10.0884314889018));
#163525=CARTESIAN_POINT('Ctrl Pts',(4.27922900024945,12.2,-10.0844566207631));
#163526=CARTESIAN_POINT('Ctrl Pts',(4.2789739780904,12.2,-10.0804965767916));
#163527=CARTESIAN_POINT('Ctrl Pts',(4.27871342368695,12.2,-10.0765514569109));
#163528=CARTESIAN_POINT('Ctrl Pts',(4.278452869319,12.2,-10.0726063375677));
#163529=CARTESIAN_POINT('Ctrl Pts',(4.27818678276605,12.2,-10.068676141191));
#163530=CARTESIAN_POINT('Ctrl Pts',(4.27791525301103,12.2,-10.0647609658984));
#163531=CARTESIAN_POINT('Ctrl Pts',(4.27764372321901,12.2,-10.0608457900724));
#163532=CARTESIAN_POINT('Ctrl Pts',(4.2773667503609,12.2,-10.0569456361822));
#163533=CARTESIAN_POINT('Ctrl Pts',(4.27708442523311,12.2,-10.0530606017306));
#163534=CARTESIAN_POINT('Ctrl Pts',(4.27680210014377,12.2,-10.0491755678084));
#163535=CARTESIAN_POINT('Ctrl Pts',(4.27651442160393,12.2,-10.0453056540305));
#163536=CARTESIAN_POINT('Ctrl Pts',(4.27622148257286,12.2,-10.0414509606219));
#163537=CARTESIAN_POINT('Ctrl Pts',(4.27592854350188,12.2,-10.037596266688));
#163538=CARTESIAN_POINT('Ctrl Pts',(4.27563034234705,12.2,-10.0337567919084));
#163539=CARTESIAN_POINT('Ctrl Pts',(4.27532697327497,12.2,-10.0299326380333));
#163540=CARTESIAN_POINT('Ctrl Pts',(4.27502360420288,12.2,-10.0261084841582));
#163541=CARTESIAN_POINT('Ctrl Pts',(4.27471506726908,12.2,-10.0222996500127));
#163542=CARTESIAN_POINT('Ctrl Pts',(4.27440145497368,12.2,-10.0185062363631));
#163543=CARTESIAN_POINT('Ctrl Pts',(4.27408784272103,12.2,-10.0147128232303));
#163544=CARTESIAN_POINT('Ctrl Pts',(4.27376915555851,12.2,-10.0109348329621));
#163545=CARTESIAN_POINT('Ctrl Pts',(4.27344548925018,12.2,-10.0071723642525));
#163546=CARTESIAN_POINT('Ctrl Pts',(4.27312182289776,12.2,-10.0034098950303));
#163547=CARTESIAN_POINT('Ctrl Pts',(4.27279317853633,12.2,-9.99966294735831));
#163548=CARTESIAN_POINT('Ctrl Pts',(4.2724596489621,12.2,-9.99593162615656));
#163549=CARTESIAN_POINT('Ctrl Pts',(4.27212611943331,12.2,-9.9922003054632));
#163550=CARTESIAN_POINT('Ctrl Pts',(4.2717877071496,12.2,-9.98848460878722));
#163551=CARTESIAN_POINT('Ctrl Pts',(4.27144450951131,12.2,-9.98478464081091));
#163552=CARTESIAN_POINT('Ctrl Pts',(4.27110131182625,12.2,-9.98108467233047));
#163553=CARTESIAN_POINT('Ctrl Pts',(4.27075332839156,12.2,-9.97740043194123));
#163554=CARTESIAN_POINT('Ctrl Pts',(4.27040065746543,12.2,-9.97373202272606));
#163555=CARTESIAN_POINT('Ctrl Pts',(4.27004798658734,12.2,-9.97006361401071));
#163556=CARTESIAN_POINT('Ctrl Pts',(4.26969062894684,12.2,-9.96641103862611));
#163557=CARTESIAN_POINT('Ctrl Pts',(4.26932868525451,12.2,-9.96277439808907));
#163558=CARTESIAN_POINT('Ctrl Pts',(4.26896674151286,12.2,-9.95913775705652));
#163559=CARTESIAN_POINT('Ctrl Pts',(4.26860021071232,12.2,-9.95551705300081));
#163560=CARTESIAN_POINT('Ctrl Pts',(4.26822919446959,12.2,-9.95191239047209));
#163561=CARTESIAN_POINT('Ctrl Pts',(4.2678581782774,12.2,-9.9483077284345));
#163562=CARTESIAN_POINT('Ctrl Pts',(4.26748267689538,12.2,-9.94471910788127));
#163563=CARTESIAN_POINT('Ctrl Pts',(4.26710279329673,12.2,-9.94114663449343));
#163564=CARTESIAN_POINT('Ctrl Pts',(4.26662793875959,12.2,-9.93668104239357));
#163565=CARTESIAN_POINT('Ctrl Pts',(4.2661462359204,12.2,-9.93224068120685));
#163566=CARTESIAN_POINT('Ctrl Pts',(4.26565788974019,12.2,-9.9278257593305));
#163567=CARTESIAN_POINT('Ctrl Pts',(4.26526721277473,12.2,-9.92429382163693));
#163568=CARTESIAN_POINT('Ctrl Pts',(4.26487228374765,12.2,-9.92077816529257));
#163569=CARTESIAN_POINT('Ctrl Pts',(4.26447320822563,12.2,-9.91727889821404));
#163570=CARTESIAN_POINT('Ctrl Pts',(4.26407413275798,12.2,-9.91377963161228));
#163571=CARTESIAN_POINT('Ctrl Pts',(4.26367091081518,12.2,-9.91029675358315));
#163572=CARTESIAN_POINT('Ctrl Pts',(4.2632636505507,12.2,-9.9068303734697));
#163573=CARTESIAN_POINT('Ctrl Pts',(4.26285639023073,12.2,-9.90336399288394));
#163574=CARTESIAN_POINT('Ctrl Pts',(4.2624450909972,12.2,-9.89991411022768));
#163575=CARTESIAN_POINT('Ctrl Pts',(4.26202986147431,12.2,-9.8964808344861));
#163576=CARTESIAN_POINT('Ctrl Pts',(4.261614632008,12.2,-9.89304755921231));
#163577=CARTESIAN_POINT('Ctrl Pts',(4.26119547324526,12.2,-9.88963089191018));
#163578=CARTESIAN_POINT('Ctrl Pts',(4.26077249383578,12.2,-9.88623094079752));
#163579=CARTESIAN_POINT('Ctrl Pts',(4.26034951436868,12.2,-9.88283098922162));
#163580=CARTESIAN_POINT('Ctrl Pts',(4.25992271671955,12.2,-9.8794477559825));
#163581=CARTESIAN_POINT('Ctrl Pts',(4.25949220924966,12.2,-9.87608135150599));
#163582=CARTESIAN_POINT('Ctrl Pts',(4.25906170183844,12.2,-9.87271494748816));
#163583=CARTESIAN_POINT('Ctrl Pts',(4.25862748729927,12.2,-9.86936537056578));
#163584=CARTESIAN_POINT('Ctrl Pts',(4.25818967727987,12.2,-9.86603273600318));
#163585=CARTESIAN_POINT('Ctrl Pts',(4.25775186720083,12.2,-9.86270010098649));
#163586=CARTESIAN_POINT('Ctrl Pts',(4.25731046255198,12.2,-9.85938440577137));
#163587=CARTESIAN_POINT('Ctrl Pts',(4.25686557841663,12.2,-9.85608576475827));
#163588=CARTESIAN_POINT('Ctrl Pts',(4.25630947327774,12.2,-9.85196246371662));
#163589=CARTESIAN_POINT('Ctrl Pts',(4.25574793029668,12.2,-9.84786580924946));
#163590=CARTESIAN_POINT('Ctrl Pts',(4.25518117772465,12.2,-9.84379602402273));
#163591=CARTESIAN_POINT('Ctrl Pts',(4.25461442515262,12.2,-9.83972623879599));
#163592=CARTESIAN_POINT('Ctrl Pts',(4.25404246493468,12.2,-9.83568332263054));
#163593=CARTESIAN_POINT('Ctrl Pts',(4.25346552500386,12.2,-9.83166750068747));
#163594=CARTESIAN_POINT('Ctrl Pts',(4.25277319711204,12.2,-9.82684851453089));
#163595=CARTESIAN_POINT('Ctrl Pts',(4.25207370237079,12.2,-9.82206854334627));
#163596=CARTESIAN_POINT('Ctrl Pts',(4.25136744731342,12.2,-9.8173279812668));
#163597=CARTESIAN_POINT('Ctrl Pts',(4.25077890141088,12.2,-9.8133775127237));
#163598=CARTESIAN_POINT('Ctrl Pts',(4.25018566173878,12.2,-9.80945441318965));
#163599=CARTESIAN_POINT('Ctrl Pts',(4.24958796923902,12.2,-9.80555890902155));
#163600=CARTESIAN_POINT('Ctrl Pts',(4.24899027673925,12.2,-9.80166340485343));
#163601=CARTESIAN_POINT('Ctrl Pts',(4.24838813182525,12.2,-9.79779550100289));
#163602=CARTESIAN_POINT('Ctrl Pts',(4.24778177772528,12.2,-9.79395542598537));
#163603=CARTESIAN_POINT('Ctrl Pts',(4.24717542362532,12.2,-9.79011535096786));
#163604=CARTESIAN_POINT('Ctrl Pts',(4.24656486389995,12.2,-9.78630310733326));
#163605=CARTESIAN_POINT('Ctrl Pts',(4.24595034473329,12.2,-9.78251892899994));
#163606=CARTESIAN_POINT('Ctrl Pts',(4.24533582556662,12.2,-9.77873475066662));
#163607=CARTESIAN_POINT('Ctrl Pts',(4.24471734990801,12.2,-9.77497863845365));
#163608=CARTESIAN_POINT('Ctrl Pts',(4.24409516997461,12.2,-9.77125083225624));
#163609=CARTESIAN_POINT('Ctrl Pts',(4.24347299004122,12.2,-9.76752302605884));
#163610=CARTESIAN_POINT('Ctrl Pts',(4.24284710615895,12.2,-9.76382352200855));
#163611=CARTESIAN_POINT('Ctrl Pts',(4.24221777865877,12.2,-9.76015256451003));
#163612=CARTESIAN_POINT('Ctrl Pts',(4.24158845115859,12.2,-9.75648160701152));
#163613=CARTESIAN_POINT('Ctrl Pts',(4.24095567811962,12.2,-9.75283919410117));
#163614=CARTESIAN_POINT('Ctrl Pts',(4.24031972575834,12.2,-9.74922557146379));
#163615=CARTESIAN_POINT('Ctrl Pts',(4.23968377339707,12.2,-9.74561194882641));
#163616=CARTESIAN_POINT('Ctrl Pts',(4.23904463977991,12.2,-9.7420271150351));
#163617=CARTESIAN_POINT('Ctrl Pts',(4.23840259419208,12.2,-9.7384713165956));
#163618=CARTESIAN_POINT('Ctrl Pts',(4.23776054860424,12.2,-9.73491551815611));
#163619=CARTESIAN_POINT('Ctrl Pts',(4.23711559168213,12.2,-9.73138875522341));
#163620=CARTESIAN_POINT('Ctrl Pts',(4.23646799689025,12.2,-9.72789127855915));
#163621=CARTESIAN_POINT('Ctrl Pts',(4.23582040209837,12.2,-9.72439380189489));
#163622=CARTESIAN_POINT('Ctrl Pts',(4.23517016901478,12.2,-9.72092561036443));
#163623=CARTESIAN_POINT('Ctrl Pts',(4.23451757818126,12.2,-9.71748695703351));
#163624=CARTESIAN_POINT('Ctrl Pts',(4.23386498741887,12.2,-9.71404830407741));
#163625=CARTESIAN_POINT('Ctrl Pts',(4.23321003533077,12.2,-9.7106391905816));
#163626=CARTESIAN_POINT('Ctrl Pts',(4.23255301061089,12.2,-9.70725987018364));
#163627=CARTESIAN_POINT('Ctrl Pts',(4.23189598581939,12.2,-9.70388054941731));
#163628=CARTESIAN_POINT('Ctrl Pts',(4.23123688711402,12.2,-9.70053102324771));
#163629=CARTESIAN_POINT('Ctrl Pts',(4.23057600329473,12.2,-9.6972115506758));
#163630=CARTESIAN_POINT('Ctrl Pts',(4.22991511947543,12.2,-9.6938920781039));
#163631=CARTESIAN_POINT('Ctrl Pts',(4.22925245145457,12.2,-9.69060265873774));
#163632=CARTESIAN_POINT('Ctrl Pts',(4.22858829426871,12.2,-9.68734355537837));
#163633=CARTESIAN_POINT('Ctrl Pts',(4.22779130560224,12.2,-9.68343263113398));
#163634=CARTESIAN_POINT('Ctrl Pts',(4.22699217283975,12.2,-9.67956536218024));
#163635=CARTESIAN_POINT('Ctrl Pts',(4.22619141896266,12.2,-9.67574221005821));
#163636=CARTESIAN_POINT('Ctrl Pts',(4.22539066515831,12.2,-9.67191905828345));
#163637=CARTESIAN_POINT('Ctrl Pts',(4.22458828713237,12.2,-9.66814002158775));
#163638=CARTESIAN_POINT('Ctrl Pts',(4.22378482274125,12.2,-9.66440556795657));
#163639=CARTESIAN_POINT('Ctrl Pts',(4.22298135835012,12.2,-9.6606711143254));
#163640=CARTESIAN_POINT('Ctrl Pts',(4.22217680546455,12.2,-9.65698124532664));
#163641=CARTESIAN_POINT('Ctrl Pts',(4.22137171399382,12.2,-9.6533364357071));
#163642=CARTESIAN_POINT('Ctrl Pts',(4.22056662244997,12.2,-9.64969162575649));
#163643=CARTESIAN_POINT('Ctrl Pts',(4.21976099074771,12.2,-9.64609187720316));
#163644=CARTESIAN_POINT('Ctrl Pts',(4.2189553794538,12.2,-9.64253767034587));
#163645=CARTESIAN_POINT('Ctrl Pts',(4.21814976823306,12.2,-9.6389834638114));
#163646=CARTESIAN_POINT('Ctrl Pts',(4.21734417884347,12.2,-9.63547480150858));
#163647=CARTESIAN_POINT('Ctrl Pts',(4.21653918470607,12.2,-9.63201217505308));
#163648=CARTESIAN_POINT('Ctrl Pts',(4.21573419056868,12.2,-9.62854954859757));
#163649=CARTESIAN_POINT('Ctrl Pts',(4.21492979253959,12.2,-9.62513295887173));
#163650=CARTESIAN_POINT('Ctrl Pts',(4.21412658031872,12.2,-9.6217629064088));
#163651=CARTESIAN_POINT('Ctrl Pts',(4.21332336809785,12.2,-9.61839285394588));
#163652=CARTESIAN_POINT('Ctrl Pts',(4.21252134088321,12.2,-9.61506933862457));
#163653=CARTESIAN_POINT('Ctrl Pts',(4.21172110482883,12.2,-9.61179287207375));
#163654=CARTESIAN_POINT('Ctrl Pts',(4.21092086870177,12.2,-9.60851640522533));
#163655=CARTESIAN_POINT('Ctrl Pts',(4.21012242302485,12.2,-9.60528698688144));
#163656=CARTESIAN_POINT('Ctrl Pts',(4.20932638789823,12.2,-9.60210513604339));
#163657=CARTESIAN_POINT('Ctrl Pts',(4.20853035284392,12.2,-9.59892328549437));
#163658=CARTESIAN_POINT('Ctrl Pts',(4.20773672901444,12.2,-9.59578900274161));
#163659=CARTESIAN_POINT('Ctrl Pts',(4.20694615204304,12.2,-9.592702819185));
#163660=CARTESIAN_POINT('Ctrl Pts',(4.20615557507164,12.2,-9.5896166356284));
#163661=CARTESIAN_POINT('Ctrl Pts',(4.20536804692382,12.2,-9.58657854854552));
#163662=CARTESIAN_POINT('Ctrl Pts',(4.20458421811871,12.2,-9.58358910206746));
#163663=CARTESIAN_POINT('Ctrl Pts',(4.20380038924239,12.2,-9.58059965531785));
#163664=CARTESIAN_POINT('Ctrl Pts',(4.20302026286642,12.2,-9.57765884703963));
#163665=CARTESIAN_POINT('Ctrl Pts',(4.202244507991,12.2,-9.57476722780085));
#163666=CARTESIAN_POINT('Ctrl Pts',(4.20146875318605,12.2,-9.57187560882474));
#163667=CARTESIAN_POINT('Ctrl Pts',(4.20069737085927,12.2,-9.56903318279588));
#163668=CARTESIAN_POINT('Ctrl Pts',(4.19993105121695,12.2,-9.5662405075512));
#163669=CARTESIAN_POINT('Ctrl Pts',(4.19916473157463,12.2,-9.56344783230653));
#163670=CARTESIAN_POINT('Ctrl Pts',(4.19840347353022,12.2,-9.56070490974903));
#163671=CARTESIAN_POINT('Ctrl Pts',(4.19764798780728,12.2,-9.55801231551009));
#163672=CARTESIAN_POINT('Ctrl Pts',(4.19689250201572,12.2,-9.5553197210266));
#163673=CARTESIAN_POINT('Ctrl Pts',(4.19614278553032,12.2,-9.55267745292545));
#163674=CARTESIAN_POINT('Ctrl Pts',(4.19539957170305,12.2,-9.55008610124103));
#163675=CARTESIAN_POINT('Ctrl Pts',(4.1946563579433,12.2,-9.54749474979199));
#163676=CARTESIAN_POINT('Ctrl Pts',(4.19391964279843,12.2,-9.54495431150118));
#163677=CARTESIAN_POINT('Ctrl Pts',(4.1931901792416,12.2,-9.54246538850825));
#163678=CARTESIAN_POINT('Ctrl Pts',(4.19246071568476,12.2,-9.53997646551533));
#163679=CARTESIAN_POINT('Ctrl Pts',(4.19173850177923,12.2,-9.537539057833));
#163680=CARTESIAN_POINT('Ctrl Pts',(4.19102431110237,12.2,-9.53515377946413));
#163681=CARTESIAN_POINT('Ctrl Pts',(4.19031012036064,12.2,-9.53276850087861));
#163682=CARTESIAN_POINT('Ctrl Pts',(4.18960395026966,12.2,-9.53043535007207));
#163683=CARTESIAN_POINT('Ctrl Pts',(4.18890659798225,12.2,-9.52815495678469));
#163684=CARTESIAN_POINT('Ctrl Pts',(4.18820924575818,12.2,-9.52587456370444));
#163685=CARTESIAN_POINT('Ctrl Pts',(4.18752071156967,12.2,-9.52364692671298));
#163686=CARTESIAN_POINT('Ctrl Pts',(4.18684181150795,12.2,-9.52147269078225));
#163687=CARTESIAN_POINT('Ctrl Pts',(4.18616291144622,12.2,-9.51929845485151));
#163688=CARTESIAN_POINT('Ctrl Pts',(4.18549364876241,12.2,-9.51717761777342));
#163689=CARTESIAN_POINT('Ctrl Pts',(4.18483486378587,12.2,-9.51511084184611));
#163690=CARTESIAN_POINT('Ctrl Pts',(4.18417607874951,12.2,-9.51304406573107));
#163691=CARTESIAN_POINT('Ctrl Pts',(4.18352777472325,12.2,-9.51103134747431));
#163692=CARTESIAN_POINT('Ctrl Pts',(4.18289081893893,12.2,-9.50907336553681));
#163693=CARTESIAN_POINT('Ctrl Pts',(4.18225386321247,12.2,-9.50711538377718));
#163694=CARTESIAN_POINT('Ctrl Pts',(4.18162825727706,12.2,-9.50521213601322));
#163695=CARTESIAN_POINT('Ctrl Pts',(4.18101489946655,12.2,-9.50336431741611));
#163696=CARTESIAN_POINT('Ctrl Pts',(4.18020003270377,12.2,-9.50090942741129));
#163697=CARTESIAN_POINT('Ctrl Pts',(4.17940677983145,12.2,-9.4985523660795));
#163698=CARTESIAN_POINT('Ctrl Pts',(4.17863732199994,12.2,-9.49629481100001));
#163699=CARTESIAN_POINT('Ctrl Pts',(4.17863732199994,15.2,-9.49629481100001));
#163700=CARTESIAN_POINT('Ctrl Pts',(4.1792137204524,15.2,-9.49798593844179));
#163701=CARTESIAN_POINT('Ctrl Pts',(4.17980347320419,15.2,-9.49973290552696));
#163702=CARTESIAN_POINT('Ctrl Pts',(4.18040565894231,15.2,-9.5015350018359));
#163703=CARTESIAN_POINT('Ctrl Pts',(4.18101074872444,15.2,-9.50334578876415));
#163704=CARTESIAN_POINT('Ctrl Pts',(4.18162839197776,15.2,-9.50521224016538));
#163705=CARTESIAN_POINT('Ctrl Pts',(4.18225768087749,15.2,-9.50713365520259));
#163706=CARTESIAN_POINT('Ctrl Pts',(4.18288696972008,15.2,-9.50905507006526));
#163707=CARTESIAN_POINT('Ctrl Pts',(4.18352790377333,15.2,-9.51103144898949));
#163708=CARTESIAN_POINT('Ctrl Pts',(4.18417960475002,15.2,-9.5130621107502));
#163709=CARTESIAN_POINT('Ctrl Pts',(4.18483130572671,15.2,-9.5150927725109));
#163710=CARTESIAN_POINT('Ctrl Pts',(4.18549377400967,15.2,-9.51717771587551));
#163711=CARTESIAN_POINT('Ctrl Pts',(4.18616615518491,15.2,-9.51931627881818));
#163712=CARTESIAN_POINT('Ctrl Pts',(4.18683853642122,15.2,-9.52145484195509));
#163713=CARTESIAN_POINT('Ctrl Pts',(4.18752083323699,15.2,-9.52364702318536));
#163714=CARTESIAN_POINT('Ctrl Pts',(4.18821221560862,15.2,-9.52589217347798));
#163715=CARTESIAN_POINT('Ctrl Pts',(4.18890359791745,15.2,-9.52813732356665));
#163716=CARTESIAN_POINT('Ctrl Pts',(4.1896040674811,15.2,-9.53043544418394));
#163717=CARTESIAN_POINT('Ctrl Pts',(4.19031282270859,15.2,-9.53278590019266));
#163718=CARTESIAN_POINT('Ctrl Pts',(4.19102157793607,15.2,-9.53513635620139));
#163719=CARTESIAN_POINT('Ctrl Pts',(4.19173861663712,15.2,-9.53753915048277));
#163720=CARTESIAN_POINT('Ctrl Pts',(4.19246316094381,15.2,-9.53999366064137));
#163721=CARTESIAN_POINT('Ctrl Pts',(4.19318770531631,15.2,-9.5424481710229));
#163722=CARTESIAN_POINT('Ctrl Pts',(4.19391975478974,15.2,-9.54495440107748));
#163723=CARTESIAN_POINT('Ctrl Pts',(4.19465855233046,15.2,-9.54751174347036));
#163724=CARTESIAN_POINT('Ctrl Pts',(4.19539734980408,15.2,-9.55006908563093));
#163725=CARTESIAN_POINT('Ctrl Pts',(4.19614289520964,15.2,-9.55267754135616));
#163726=CARTESIAN_POINT('Ctrl Pts',(4.19689445276592,15.2,-9.55533651859505));
#163727=CARTESIAN_POINT('Ctrl Pts',(4.19777126996042,15.2,-9.55843865886813));
#163728=CARTESIAN_POINT('Ctrl Pts',(4.19865626969675,15.2,-9.5616095630426));
#163729=CARTESIAN_POINT('Ctrl Pts',(4.19954831684995,15.2,-9.56484831852753));
#163730=CARTESIAN_POINT('Ctrl Pts',(4.20031292865584,15.2,-9.56762439451339));
#163731=CARTESIAN_POINT('Ctrl Pts',(4.20108272045344,15.2,-9.57045031632587));
#163732=CARTESIAN_POINT('Ctrl Pts',(4.20185699825882,15.2,-9.57332552089018));
#163733=CARTESIAN_POINT('Ctrl Pts',(4.20263127606421,15.2,-9.57620072545449));
#163734=CARTESIAN_POINT('Ctrl Pts',(4.20341003927757,15.2,-9.5791252158066));
#163735=CARTESIAN_POINT('Ctrl Pts',(4.20419261516564,15.2,-9.58209843411309));
#163736=CARTESIAN_POINT('Ctrl Pts',(4.2049751910537,15.2,-9.58507165241958));
#163737=CARTESIAN_POINT('Ctrl Pts',(4.20576157753445,15.2,-9.58809360112182));
#163738=CARTESIAN_POINT('Ctrl Pts',(4.20655112042221,15.2,-9.59116373742363));
#163739=CARTESIAN_POINT('Ctrl Pts',(4.20734066338169,15.2,-9.59423387400432));
#163740=CARTESIAN_POINT('Ctrl Pts',(4.20813336138319,15.2,-9.59735219688979));
#163741=CARTESIAN_POINT('Ctrl Pts',(4.20892857459329,15.2,-9.60051817748102));
#163742=CARTESIAN_POINT('Ctrl Pts',(4.20972378773116,15.2,-9.60368415778465));
#163743=CARTESIAN_POINT('Ctrl Pts',(4.21052151772717,15.2,-9.60689779296794));
#163744=CARTESIAN_POINT('Ctrl Pts',(4.21132113894804,15.2,-9.61015856159742));
#163745=CARTESIAN_POINT('Ctrl Pts',(4.21212076016891,15.2,-9.61341933022692));
#163746=CARTESIAN_POINT('Ctrl Pts',(4.21292227550836,15.2,-9.61672723460936));
#163747=CARTESIAN_POINT('Ctrl Pts',(4.21372507564577,15.2,-9.62008176015097));
#163748=CARTESIAN_POINT('Ctrl Pts',(4.2145278758561,15.2,-9.62343628599729));
#163749=CARTESIAN_POINT('Ctrl Pts',(4.21533196074159,15.2,-9.62683743398984));
#163750=CARTESIAN_POINT('Ctrl Pts',(4.21613674003548,15.2,-9.63028470092968));
#163751=CARTESIAN_POINT('Ctrl Pts',(4.21694151925626,15.2,-9.63373196755639));
#163752=CARTESIAN_POINT('Ctrl Pts',(4.21774698998353,15.2,-9.63722535336929));
#163753=CARTESIAN_POINT('Ctrl Pts',(4.21855257820791,15.2,-9.64076436500666));
#163754=CARTESIAN_POINT('Ctrl Pts',(4.21935816643229,15.2,-9.64430337664403));
#163755=CARTESIAN_POINT('Ctrl Pts',(4.22016387039973,15.2,-9.64788801198091));
#163756=CARTESIAN_POINT('Ctrl Pts',(4.22096912595384,15.2,-9.65151778759597));
#163757=CARTESIAN_POINT('Ctrl Pts',(4.2217743815811,15.2,-9.65514756354075));
#163758=CARTESIAN_POINT('Ctrl Pts',(4.22257919099379,15.2,-9.65882247991873));
#163759=CARTESIAN_POINT('Ctrl Pts',(4.2233830025777,15.2,-9.6625420591432));
#163760=CARTESIAN_POINT('Ctrl Pts',(4.2241868140886,15.2,-9.6662616380298));
#163761=CARTESIAN_POINT('Ctrl Pts',(4.2249896277874,15.2,-9.67002588040497));
#163762=CARTESIAN_POINT('Ctrl Pts',(4.22579090900828,15.2,-9.67383431326659));
#163763=CARTESIAN_POINT('Ctrl Pts',(4.22659219022916,15.2,-9.67764274612822));
#163764=CARTESIAN_POINT('Ctrl Pts',(4.22739193620345,15.2,-9.68149537398921));
#163765=CARTESIAN_POINT('Ctrl Pts',(4.22818962396444,15.2,-9.68539173287312));
#163766=CARTESIAN_POINT('Ctrl Pts',(4.22885436378942,15.2,-9.68863869872768));
#163767=CARTESIAN_POINT('Ctrl Pts',(4.22951767568436,15.2,-9.69191603336874));
#163768=CARTESIAN_POINT('Ctrl Pts',(4.23017926124,15.2,-9.69522347482548));
#163769=CARTESIAN_POINT('Ctrl Pts',(4.23084084679565,15.2,-9.69853091628222));
#163770=CARTESIAN_POINT('Ctrl Pts',(4.23150070681236,15.2,-9.70186846210921));
#163771=CARTESIAN_POINT('Ctrl Pts',(4.23215854917358,15.2,-9.70523585453823));
#163772=CARTESIAN_POINT('Ctrl Pts',(4.2328163915348,15.2,-9.70860324696723));
#163773=CARTESIAN_POINT('Ctrl Pts',(4.23347221802439,15.2,-9.71200048482705));
#163774=CARTESIAN_POINT('Ctrl Pts',(4.23412574254126,15.2,-9.71542731227307));
#163775=CARTESIAN_POINT('Ctrl Pts',(4.23477926705812,15.2,-9.7188541397191));
#163776=CARTESIAN_POINT('Ctrl Pts',(4.2354304877444,15.2,-9.72231055681104));
#163777=CARTESIAN_POINT('Ctrl Pts',(4.23607912600828,15.2,-9.7257963092416));
#163778=CARTESIAN_POINT('Ctrl Pts',(4.23672776427217,15.2,-9.72928206167215));
#163779=CARTESIAN_POINT('Ctrl Pts',(4.23737382161406,15.2,-9.73279715005236));
#163780=CARTESIAN_POINT('Ctrl Pts',(4.2380170199503,15.2,-9.73634132423521));
#163781=CARTESIAN_POINT('Ctrl Pts',(4.23866021828655,15.2,-9.73988549841805));
#163782=CARTESIAN_POINT('Ctrl Pts',(4.23930056071399,15.2,-9.74345875747307));
#163783=CARTESIAN_POINT('Ctrl Pts',(4.23993777474161,15.2,-9.74706085504403));
#163784=CARTESIAN_POINT('Ctrl Pts',(4.24057498876922,15.2,-9.75066295261499));
#163785=CARTESIAN_POINT('Ctrl Pts',(4.24120907609136,15.2,-9.75429388866574));
#163786=CARTESIAN_POINT('Ctrl Pts',(4.24183977109118,15.2,-9.75795341797278));
#163787=CARTESIAN_POINT('Ctrl Pts',(4.242470466091,15.2,-9.76161294727982));
#163788=CARTESIAN_POINT('Ctrl Pts',(4.24309776897477,15.2,-9.76530107119382));
#163789=CARTESIAN_POINT('Ctrl Pts',(4.243721419839,15.2,-9.7690175472148));
#163790=CARTESIAN_POINT('Ctrl Pts',(4.24434507070324,15.2,-9.77273402323579));
#163791=CARTESIAN_POINT('Ctrl Pts',(4.24496506893086,15.2,-9.77647885074671));
#163792=CARTESIAN_POINT('Ctrl Pts',(4.2455811605972,15.2,-9.78025179248512));
#163793=CARTESIAN_POINT('Ctrl Pts',(4.24619725226355,15.2,-9.78402473422354));
#163794=CARTESIAN_POINT('Ctrl Pts',(4.2468094360076,15.2,-9.78782579053184));
#163795=CARTESIAN_POINT('Ctrl Pts',(4.24741746260448,15.2,-9.79165472324244));
#163796=CARTESIAN_POINT('Ctrl Pts',(4.24802548913509,15.2,-9.7954836555357));
#163797=CARTESIAN_POINT('Ctrl Pts',(4.24862935804764,15.2,-9.79934046482307));
#163798=CARTESIAN_POINT('Ctrl Pts',(4.24922882145488,15.2,-9.80322491946687));
#163799=CARTESIAN_POINT('Ctrl Pts',(4.24982828492747,15.2,-9.80710937453407));
#163800=CARTESIAN_POINT('Ctrl Pts',(4.25042334491679,15.2,-9.81102147275356));
#163801=CARTESIAN_POINT('Ctrl Pts',(4.25101375838939,15.2,-9.81496098525133));
#163802=CARTESIAN_POINT('Ctrl Pts',(4.25160417186199,15.2,-9.8189004977491));
#163803=CARTESIAN_POINT('Ctrl Pts',(4.25218994001802,15.2,-9.82286742232974));
#163804=CARTESIAN_POINT('Ctrl Pts',(4.25277082349064,15.2,-9.82686153316086));
#163805=CARTESIAN_POINT('Ctrl Pts',(4.25335170696326,15.2,-9.83085564399197));
#163806=CARTESIAN_POINT('Ctrl Pts',(4.25392770711035,15.2,-9.83487693929639));
#163807=CARTESIAN_POINT('Ctrl Pts',(4.25449858970867,15.2,-9.83892519303844));
#163808=CARTESIAN_POINT('Ctrl Pts',(4.25506947230699,15.2,-9.84297344678047));
#163809=CARTESIAN_POINT('Ctrl Pts',(4.25563523802966,15.2,-9.84704866018881));
#163810=CARTESIAN_POINT('Ctrl Pts',(4.25619565719661,15.2,-9.85115060796518));
#163811=CARTESIAN_POINT('Ctrl Pts',(4.25675607636355,15.2,-9.85525255574156));
#163812=CARTESIAN_POINT('Ctrl Pts',(4.25731114735814,15.2,-9.85938124031862));
#163813=CARTESIAN_POINT('Ctrl Pts',(4.25786064749732,15.2,-9.86353643726169));
#163814=CARTESIAN_POINT('Ctrl Pts',(4.25830024763262,15.2,-9.86686059499732));
#163815=CARTESIAN_POINT('Ctrl Pts',(4.25873628036784,15.2,-9.87020172116841));
#163816=CARTESIAN_POINT('Ctrl Pts',(4.25916863507934,15.2,-9.87355970552063));
#163817=CARTESIAN_POINT('Ctrl Pts',(4.25960098973194,15.2,-9.87691768941533));
#163818=CARTESIAN_POINT('Ctrl Pts',(4.2600296626219,15.2,-9.88029252749288));
#163819=CARTESIAN_POINT('Ctrl Pts',(4.26045454469852,15.2,-9.88368411271452));
#163820=CARTESIAN_POINT('Ctrl Pts',(4.26098564733772,15.2,-9.88792359458814));
#163821=CARTESIAN_POINT('Ctrl Pts',(4.26151082459899,15.2,-9.89218924004301));
#163822=CARTESIAN_POINT('Ctrl Pts',(4.26202986147431,15.2,-9.89648083448611));
#163823=CARTESIAN_POINT('Ctrl Pts',(4.2624450909972,15.2,-9.89991411022769));
#163824=CARTESIAN_POINT('Ctrl Pts',(4.26285639023073,15.2,-9.90336399288395));
#163825=CARTESIAN_POINT('Ctrl Pts',(4.2632636505507,15.2,-9.9068303734697));
#163826=CARTESIAN_POINT('Ctrl Pts',(4.26367091081518,15.2,-9.91029675358314));
#163827=CARTESIAN_POINT('Ctrl Pts',(4.26407413275798,15.2,-9.91377963161227));
#163828=CARTESIAN_POINT('Ctrl Pts',(4.26447320822563,15.2,-9.91727889821404));
#163829=CARTESIAN_POINT('Ctrl Pts',(4.26487228374766,15.2,-9.92077816529258));
#163830=CARTESIAN_POINT('Ctrl Pts',(4.26526721277474,15.2,-9.92429382163696));
#163831=CARTESIAN_POINT('Ctrl Pts',(4.26565788974019,15.2,-9.9278257593305));
#163832=CARTESIAN_POINT('Ctrl Pts',(4.2661462359204,15.2,-9.93224068120682));
#163833=CARTESIAN_POINT('Ctrl Pts',(4.26662793875959,15.2,-9.93668104239357));
#163834=CARTESIAN_POINT('Ctrl Pts',(4.26710279329673,15.2,-9.94114663449343));
#163835=CARTESIAN_POINT('Ctrl Pts',(4.26748267689538,15.2,-9.94471910788126));
#163836=CARTESIAN_POINT('Ctrl Pts',(4.2678581782774,15.2,-9.94830772843448));
#163837=CARTESIAN_POINT('Ctrl Pts',(4.26822919446959,15.2,-9.95191239047209));
#163838=CARTESIAN_POINT('Ctrl Pts',(4.26860021071233,15.2,-9.95551705300083));
#163839=CARTESIAN_POINT('Ctrl Pts',(4.26896674151286,15.2,-9.95913775705649));
#163840=CARTESIAN_POINT('Ctrl Pts',(4.26932868525451,15.2,-9.96277439808907));
#163841=CARTESIAN_POINT('Ctrl Pts',(4.26969062894684,15.2,-9.96641103862614));
#163842=CARTESIAN_POINT('Ctrl Pts',(4.27004798658734,15.2,-9.97006361401073));
#163843=CARTESIAN_POINT('Ctrl Pts',(4.27040065746543,15.2,-9.97373202272606));
#163844=CARTESIAN_POINT('Ctrl Pts',(4.27075332839156,15.2,-9.97740043194123));
#163845=CARTESIAN_POINT('Ctrl Pts',(4.27110131182625,15.2,-9.98108467233046));
#163846=CARTESIAN_POINT('Ctrl Pts',(4.27144450951131,15.2,-9.9847846408109));
#163847=CARTESIAN_POINT('Ctrl Pts',(4.2717877071496,15.2,-9.98848460878723));
#163848=CARTESIAN_POINT('Ctrl Pts',(4.27212611943331,15.2,-9.99220030546318));
#163849=CARTESIAN_POINT('Ctrl Pts',(4.2724596489621,15.2,-9.99593162615656));
#163850=CARTESIAN_POINT('Ctrl Pts',(4.27279317853633,15.2,-9.99966294735833));
#163851=CARTESIAN_POINT('Ctrl Pts',(4.27312182289776,15.2,-10.0034098950303));
#163852=CARTESIAN_POINT('Ctrl Pts',(4.27344548925018,15.2,-10.0071723642525));
#163853=CARTESIAN_POINT('Ctrl Pts',(4.27376915555851,15.2,-10.0109348329621));
#163854=CARTESIAN_POINT('Ctrl Pts',(4.27408784272103,15.2,-10.0147128232303));
#163855=CARTESIAN_POINT('Ctrl Pts',(4.27440145497369,15.2,-10.0185062363631));
#163856=CARTESIAN_POINT('Ctrl Pts',(4.27471506726908,15.2,-10.0222996500127));
#163857=CARTESIAN_POINT('Ctrl Pts',(4.27502360420288,15.2,-10.0261084841582));
#163858=CARTESIAN_POINT('Ctrl Pts',(4.27532697327497,15.2,-10.0299326380333));
#163859=CARTESIAN_POINT('Ctrl Pts',(4.27563034234705,15.2,-10.0337567919083));
#163860=CARTESIAN_POINT('Ctrl Pts',(4.27592854350188,15.2,-10.037596266688));
#163861=CARTESIAN_POINT('Ctrl Pts',(4.27622148257286,15.2,-10.0414509606219));
#163862=CARTESIAN_POINT('Ctrl Pts',(4.27651442160393,15.2,-10.0453056540305));
#163863=CARTESIAN_POINT('Ctrl Pts',(4.27680210014377,15.2,-10.0491755678084));
#163864=CARTESIAN_POINT('Ctrl Pts',(4.27708442523311,15.2,-10.0530606017306));
#163865=CARTESIAN_POINT('Ctrl Pts',(4.27743733162362,15.2,-10.0579168945304));
#163866=CARTESIAN_POINT('Ctrl Pts',(4.27778187476663,15.2,-10.0627968116444));
#163867=CARTESIAN_POINT('Ctrl Pts',(4.27811787851663,15.2,-10.0677001619916));
#163868=CARTESIAN_POINT('Ctrl Pts',(4.27838668153128,15.2,-10.0716228424832));
#163869=CARTESIAN_POINT('Ctrl Pts',(4.27865001806196,15.2,-10.0755605186237));
#163870=CARTESIAN_POINT('Ctrl Pts',(4.27890780107544,15.2,-10.0795130943962));
#163871=CARTESIAN_POINT('Ctrl Pts',(4.2791655840538,15.2,-10.0834656696302));
#163872=CARTESIAN_POINT('Ctrl Pts',(4.27941781185492,15.2,-10.0874331430909));
#163873=CARTESIAN_POINT('Ctrl Pts',(4.2796643982248,15.2,-10.0914154171722));
#163874=CARTESIAN_POINT('Ctrl Pts',(4.27991098462826,15.2,-10.0953976917962));
#163875=CARTESIAN_POINT('Ctrl Pts',(4.2801519285123,15.2,-10.0993947667774));
#163876=CARTESIAN_POINT('Ctrl Pts',(4.28038714358009,15.2,-10.1034065471642));
#163877=CARTESIAN_POINT('Ctrl Pts',(4.28062235861583,15.2,-10.1074183270044));
#163878=CARTESIAN_POINT('Ctrl Pts',(4.28085184387175,15.2,-10.1114448109872));
#163879=CARTESIAN_POINT('Ctrl Pts',(4.28107551496496,15.2,-10.1154859017114));
#163880=CARTESIAN_POINT('Ctrl Pts',(4.28135510385433,15.2,-10.1205372655297));
#163881=CARTESIAN_POINT('Ctrl Pts',(4.28162560769345,15.2,-10.1256114531291));
#163882=CARTESIAN_POINT('Ctrl Pts',(4.28188686074949,15.2,-10.1307082801418));
#163883=CARTESIAN_POINT('Ctrl Pts',(4.28209586320572,15.2,-10.1347857419742));
#163884=CARTESIAN_POINT('Ctrl Pts',(4.28229894513625,15.2,-10.1388776920824));
#163885=CARTESIAN_POINT('Ctrl Pts',(4.2824960230452,15.2,-10.1429840348459));
#163886=CARTESIAN_POINT('Ctrl Pts',(4.2826931009273,15.2,-10.1470903770499));
#163887=CARTESIAN_POINT('Ctrl Pts',(4.28288417654118,15.2,-10.1512111126121));
#163888=CARTESIAN_POINT('Ctrl Pts',(4.28306916502645,15.2,-10.1553461461621));
#163889=CARTESIAN_POINT('Ctrl Pts',(4.28330040065195,15.2,-10.160514938522));
#163890=CARTESIAN_POINT('Ctrl Pts',(4.28352212755776,15.2,-10.1657060734881));
#163891=CARTESIAN_POINT('Ctrl Pts',(4.28373418575271,15.2,-10.1709193671675));
#163892=CARTESIAN_POINT('Ctrl Pts',(4.28394624394766,15.2,-10.1761326608469));
#163893=CARTESIAN_POINT('Ctrl Pts',(4.28414863489341,15.2,-10.1813681131122));
#163894=CARTESIAN_POINT('Ctrl Pts',(4.2843412012832,15.2,-10.1866255419554));
#163895=CARTESIAN_POINT('Ctrl Pts',(4.28449525440343,15.2,-10.1908314852593));
#163896=CARTESIAN_POINT('Ctrl Pts',(4.2846430205827,15.2,-10.1950514940156));
#163897=CARTESIAN_POINT('Ctrl Pts',(4.28478441925642,15.2,-10.1992854746922));
#163898=CARTESIAN_POINT('Ctrl Pts',(4.28492581791087,15.2,-10.203519454792));
#163899=CARTESIAN_POINT('Ctrl Pts',(4.28506085104115,15.2,-10.2077674088704));
#163900=CARTESIAN_POINT('Ctrl Pts',(4.28518944019773,15.2,-10.21202924291));
#163901=CARTESIAN_POINT('Ctrl Pts',(4.28535017665659,15.2,-10.217356535895));
#163902=CARTESIAN_POINT('Ctrl Pts',(4.28550084362145,15.2,-10.2227055169449));
#163903=CARTESIAN_POINT('Ctrl Pts',(4.28564129098323,15.2,-10.2280760082887));
#163904=CARTESIAN_POINT('Ctrl Pts',(4.28578173834501,15.2,-10.2334464996325));
#163905=CARTESIAN_POINT('Ctrl Pts',(4.28591196730553,15.2,-10.2388385011222));
#163906=CARTESIAN_POINT('Ctrl Pts',(4.28603182799997,15.2,-10.244251835775));
#163907=CARTESIAN_POINT('Ctrl Pts',(4.28612771656075,15.2,-10.2485825037332));
#163908=CARTESIAN_POINT('Ctrl Pts',(4.28621697050132,15.2,-10.2529268240903));
#163909=CARTESIAN_POINT('Ctrl Pts',(4.28629951500513,15.2,-10.2572847079958));
#163910=CARTESIAN_POINT('Ctrl Pts',(4.28638205949769,15.2,-10.2616425913076));
#163911=CARTESIAN_POINT('Ctrl Pts',(4.2864578928469,15.2,-10.2660140385161));
#163912=CARTESIAN_POINT('Ctrl Pts',(4.28652694400826,15.2,-10.2703989567886));
#163913=CARTESIAN_POINT('Ctrl Pts',(4.28659599517902,15.2,-10.2747838756586));
#163914=CARTESIAN_POINT('Ctrl Pts',(4.28665826263726,15.2,-10.2791822695684));
#163915=CARTESIAN_POINT('Ctrl Pts',(4.28671367325069,15.2,-10.2835940462546));
#163916=CARTESIAN_POINT('Ctrl Pts',(4.28676908385657,15.2,-10.2880058223398));
#163917=CARTESIAN_POINT('Ctrl Pts',(4.28681763838279,15.2,-10.2924309828926));
#163918=CARTESIAN_POINT('Ctrl Pts',(4.28685926371317,15.2,-10.2968694383622));
#163919=CARTESIAN_POINT('Ctrl Pts',(4.28689048271238,15.2,-10.3001982801156));
#163920=CARTESIAN_POINT('Ctrl Pts',(4.28691780502797,15.2,-10.3035346010917));
#163921=CARTESIAN_POINT('Ctrl Pts',(4.28694119948707,15.2,-10.3068783630531));
#163922=CARTESIAN_POINT('Ctrl Pts',(4.28698019025367,15.2,-10.3124512998579));
#163923=CARTESIAN_POINT('Ctrl Pts',(4.2870082723871,15.2,-10.3180449066895));
#163924=CARTESIAN_POINT('Ctrl Pts',(4.28702530579046,15.2,-10.3236590136329));
#163925=CARTESIAN_POINT('Ctrl Pts',(4.2870355258321,15.2,-10.3270274776766));
#163926=CARTESIAN_POINT('Ctrl Pts',(4.28704176924902,15.2,-10.3304033206697));
#163927=CARTESIAN_POINT('Ctrl Pts',(4.28704400624948,15.2,-10.3337865067958));
#163928=CARTESIAN_POINT('Ctrl Pts',(4.28704624325035,15.2,-10.3371696935365));
#163929=CARTESIAN_POINT('Ctrl Pts',(4.28704447371677,15.2,-10.3405602221626));
#163930=CARTESIAN_POINT('Ctrl Pts',(4.28703866871537,15.2,-10.3439580574907));
#163931=CARTESIAN_POINT('Ctrl Pts',(4.28702899371551,15.2,-10.3496211149306));
#163932=CARTESIAN_POINT('Ctrl Pts',(4.28700810861641,15.2,-10.3553044681051));
#163933=CARTESIAN_POINT('Ctrl Pts',(4.28697588028752,15.2,-10.3610079455373));
#163934=CARTESIAN_POINT('Ctrl Pts',(4.28695654328526,15.2,-10.364430032867));
#163935=CARTESIAN_POINT('Ctrl Pts',(4.28693312344853,15.2,-10.367859365132));
#163936=CARTESIAN_POINT('Ctrl Pts',(4.28690559094397,15.2,-10.3712959064658));
#163937=CARTESIAN_POINT('Ctrl Pts',(4.28686888094622,15.2,-10.375877960537));
#163938=CARTESIAN_POINT('Ctrl Pts',(4.28682486059943,15.2,-10.3804728301037));
#163939=CARTESIAN_POINT('Ctrl Pts',(4.28677346327077,15.2,-10.3850804301151));
#163940=CARTESIAN_POINT('Ctrl Pts',(4.28673491527254,15.2,-10.3885361302806));
#163941=CARTESIAN_POINT('Ctrl Pts',(4.28669221775916,15.2,-10.3919989906822));
#163942=CARTESIAN_POINT('Ctrl Pts',(4.286645342759,15.2,-10.3954689756037));
#163943=CARTESIAN_POINT('Ctrl Pts',(4.28659846775884,15.2,-10.3989389605252));
#163944=CARTESIAN_POINT('Ctrl Pts',(4.28654741575944,15.2,-10.4024160704847));
#163945=CARTESIAN_POINT('Ctrl Pts',(4.28649215780368,15.2,-10.4059002687321));
#163946=CARTESIAN_POINT('Ctrl Pts',(4.28643689983789,15.2,-10.4093844676125));
#163947=CARTESIAN_POINT('Ctrl Pts',(4.28637743751258,15.2,-10.4128757554532));
#163948=CARTESIAN_POINT('Ctrl Pts',(4.28631374204442,15.2,-10.4163740962543));
#163949=CARTESIAN_POINT('Ctrl Pts',(4.28622881477281,15.2,-10.4210385495965));
#163950=CARTESIAN_POINT('Ctrl Pts',(4.28613636328274,15.2,-10.425715540337));
#163951=CARTESIAN_POINT('Ctrl Pts',(4.28603632329141,15.2,-10.4304049863417));
#163952=CARTESIAN_POINT('Ctrl Pts',(4.28596129329451,15.2,-10.433922071005));
#163953=CARTESIAN_POINT('Ctrl Pts',(4.28588199471675,15.2,-10.4374461601862));
#163954=CARTESIAN_POINT('Ctrl Pts',(4.28579839979944,15.2,-10.4409772200669));
#163955=CARTESIAN_POINT('Ctrl Pts',(4.28571480488213,15.2,-10.4445082799475));
#163956=CARTESIAN_POINT('Ctrl Pts',(4.28562691529946,15.2,-10.4480463097569));
#163957=CARTESIAN_POINT('Ctrl Pts',(4.28553470330341,15.2,-10.4515912744188));
#163958=CARTESIAN_POINT('Ctrl Pts',(4.2854424912906,15.2,-10.4551362397248));
#163959=CARTESIAN_POINT('Ctrl Pts',(4.2853459560099,15.2,-10.4586881395576));
#163960=CARTESIAN_POINT('Ctrl Pts',(4.28524507345298,15.2,-10.4622469393258));
#163961=CARTESIAN_POINT('Ctrl Pts',(4.28511056340763,15.2,-10.4669920046058));
#163962=CARTESIAN_POINT('Ctrl Pts',(4.28496832204939,15.2,-10.471749334287));
#163963=CARTESIAN_POINT('Ctrl Pts',(4.28481828806217,15.2,-10.4765188476185));
#163964=CARTESIAN_POINT('Ctrl Pts',(4.28470576256664,15.2,-10.4800959827796));
#163965=CARTESIAN_POINT('Ctrl Pts',(4.28458885348807,15.2,-10.4836799697819));
#163966=CARTESIAN_POINT('Ctrl Pts',(4.28446753503475,15.2,-10.4872707754838));
#163967=CARTESIAN_POINT('Ctrl Pts',(4.28434621655939,15.2,-10.4908615818381));
#163968=CARTESIAN_POINT('Ctrl Pts',(4.28422048879112,15.2,-10.4944592061443));
#163969=CARTESIAN_POINT('Ctrl Pts',(4.28409032672993,15.2,-10.4980636135024));
#163970=CARTESIAN_POINT('Ctrl Pts',(4.28391677735442,15.2,-10.5028694888885));
#163971=CARTESIAN_POINT('Ctrl Pts',(4.28373534249934,15.2,-10.5076874235641));
#163972=CARTESIAN_POINT('Ctrl Pts',(4.28354596445844,15.2,-10.5125173337467));
#163973=CARTESIAN_POINT('Ctrl Pts',(4.28340393092131,15.2,-10.5161397665481));
#163974=CARTESIAN_POINT('Ctrl Pts',(4.28325742756048,15.2,-10.5197689361698));
#163975=CARTESIAN_POINT('Ctrl Pts',(4.28310643102469,15.2,-10.5234048088288));
#163976=CARTESIAN_POINT('Ctrl Pts',(4.2829554344889,15.2,-10.5270406814878));
#163977=CARTESIAN_POINT('Ctrl Pts',(4.28279994379509,15.2,-10.5306832557379));
#163978=CARTESIAN_POINT('Ctrl Pts',(4.28263993480152,15.2,-10.5343324984795));
#163979=CARTESIAN_POINT('Ctrl Pts',(4.28247992577888,15.2,-10.5379817418839));
#163980=CARTESIAN_POINT('Ctrl Pts',(4.28231539742164,15.2,-10.5416376543152));
#163981=CARTESIAN_POINT('Ctrl Pts',(4.28214632593811,15.2,-10.5453001993067));
#163982=CARTESIAN_POINT('Ctrl Pts',(4.2819772544853,15.2,-10.5489627436329));
#163983=CARTESIAN_POINT('Ctrl Pts',(4.28180363946841,15.2,-10.5526319223104));
#163984=CARTESIAN_POINT('Ctrl Pts',(4.28162545692379,15.2,-10.5563077006945));
#163985=CARTESIAN_POINT('Ctrl Pts',(4.28144727437917,15.2,-10.5599834790787));
#163986=CARTESIAN_POINT('Ctrl Pts',(4.28126452298974,15.2,-10.563665855719));
#163987=CARTESIAN_POINT('Ctrl Pts',(4.28107717949615,15.2,-10.5673547988772));
#163988=CARTESIAN_POINT('Ctrl Pts',(4.28088983600255,15.2,-10.5710437420354));
#163989=CARTESIAN_POINT('Ctrl Pts',(4.28069789969284,15.2,-10.5747392503178));
#163990=CARTESIAN_POINT('Ctrl Pts',(4.28050134774165,15.2,-10.5784412905166));
#163991=CARTESIAN_POINT('Ctrl Pts',(4.28030479579045,15.2,-10.5821433307155));
#163992=CARTESIAN_POINT('Ctrl Pts',(4.28010362771445,15.2,-10.5858519026807));
#163993=CARTESIAN_POINT('Ctrl Pts',(4.279897819764,15.2,-10.5895669733785));
#163994=CARTESIAN_POINT('Ctrl Pts',(4.27969201181354,15.2,-10.5932820440763));
#163995=CARTESIAN_POINT('Ctrl Pts',(4.27948156432727,15.2,-10.597003612912));
#163996=CARTESIAN_POINT('Ctrl Pts',(4.27926645232488,15.2,-10.6007316452954));
#163997=CARTESIAN_POINT('Ctrl Pts',(4.27905134032249,15.2,-10.6044596776788));
#163998=CARTESIAN_POINT('Ctrl Pts',(4.27883156239011,15.2,-10.6081941721879));
#163999=CARTESIAN_POINT('Ctrl Pts',(4.27860709702391,15.2,-10.6119350969261));
#164000=CARTESIAN_POINT('Ctrl Pts',(4.27838263161692,15.2,-10.6156760223439));
#164001=CARTESIAN_POINT('Ctrl Pts',(4.27815347886695,15.2,-10.6194233771719));
#164002=CARTESIAN_POINT('Ctrl Pts',(4.27791961741566,15.2,-10.6231771325516));
#164003=CARTESIAN_POINT('Ctrl Pts',(4.27768575600685,15.2,-10.6269308872494));
#164004=CARTESIAN_POINT('Ctrl Pts',(4.27744718648162,15.2,-10.6306910412469));
#164005=CARTESIAN_POINT('Ctrl Pts',(4.27720388399004,15.2,-10.6344575614023));
#164006=CARTESIAN_POINT('Ctrl Pts',(4.27696058149847,15.2,-10.6382240815577));
#164007=CARTESIAN_POINT('Ctrl Pts',(4.27671254567506,15.2,-10.6419969671902));
#164008=CARTESIAN_POINT('Ctrl Pts',(4.27645974872475,15.2,-10.6457761754451));
#164009=CARTESIAN_POINT('Ctrl Pts',(4.27620695177443,15.2,-10.6495553837));
#164010=CARTESIAN_POINT('Ctrl Pts',(4.27594939290852,15.2,-10.6533409152338));
#164011=CARTESIAN_POINT('Ctrl Pts',(4.27568705125021,15.2,-10.6571327392382));
#164012=CARTESIAN_POINT('Ctrl Pts',(4.27524981513715,15.2,-10.6634524461419));
#164013=CARTESIAN_POINT('Ctrl Pts',(4.27479930143439,15.2,-10.6697896272814));
#164014=CARTESIAN_POINT('Ctrl Pts',(4.27433546799994,15.2,-10.676144262));
#164015=CARTESIAN_POINT('Origin',(-5.66257110645729E-14,15.2,-1.77635683940025E-14));
#164016=CARTESIAN_POINT('',(4.57383771044509,15.2,-9.312391400561));
#164017=CARTESIAN_POINT('',(4.57383771044509,12.2,-9.31239140056099));
#164018=CARTESIAN_POINT('',(4.57383770999994,15.2,-9.31239140000002));
#164019=CARTESIAN_POINT('Origin',(-5.66257110645729E-14,12.2,-1.77635683940025E-14));
#164020=CARTESIAN_POINT('Origin',(-5.66257110645729E-14,15.2,-1.77635683940025E-14));
#164021=CARTESIAN_POINT('Origin',(-5.66257110645729E-14,15.2,-1.77635683940025E-14));
#164022=CARTESIAN_POINT('',(5.41482055299994,15.2,-10.145428447));
#164023=CARTESIAN_POINT('',(5.75020264099994,15.2,-9.95917514500001));
#164024=CARTESIAN_POINT('Origin',(-5.66257110645729E-14,15.2,-1.77635683940025E-14));
#164025=CARTESIAN_POINT('',(5.75020264099994,12.2,-9.95917514500001));
#164026=CARTESIAN_POINT('',(5.75020264099994,15.2,-9.95917514500001));
#164027=CARTESIAN_POINT('',(5.41482055299994,12.2,-10.145428447));
#164028=CARTESIAN_POINT('Origin',(-5.66257110645729E-14,12.2,-1.77635683940025E-14));
#164029=CARTESIAN_POINT('',(5.41482055299994,15.2,-10.145428447));
#164030=CARTESIAN_POINT('Ctrl Pts',(5.75020264099994,15.2,-9.95917514500001));
#164031=CARTESIAN_POINT('Ctrl Pts',(5.75020264099994,11.6,-9.95917514500001));
#164032=CARTESIAN_POINT('Ctrl Pts',(5.75014921099994,15.2,-9.95841243000001));
#164033=CARTESIAN_POINT('Ctrl Pts',(5.75014921099994,11.6,-9.95841243000001));
#164034=CARTESIAN_POINT('Ctrl Pts',(5.75004209299995,15.2,-9.95688746000001));
#164035=CARTESIAN_POINT('Ctrl Pts',(5.75004209299995,11.6,-9.95688746000001));
#164036=CARTESIAN_POINT('Ctrl Pts',(5.74988064799995,15.2,-9.95460138400001));
#164037=CARTESIAN_POINT('Ctrl Pts',(5.74988064799995,11.6,-9.95460138400001));
#164038=CARTESIAN_POINT('Ctrl Pts',(5.74966384999994,15.2,-9.95155604500001));
#164039=CARTESIAN_POINT('Ctrl Pts',(5.74966384999994,11.6,-9.95155604500001));
#164040=CARTESIAN_POINT('Ctrl Pts',(5.74939028899994,15.2,-9.94775397100001));
#164041=CARTESIAN_POINT('Ctrl Pts',(5.74939028899994,11.6,-9.94775397100001));
#164042=CARTESIAN_POINT('Ctrl Pts',(5.74911416699995,15.2,-9.94395649900001));
#164043=CARTESIAN_POINT('Ctrl Pts',(5.74911416699995,11.6,-9.94395649900001));
#164044=CARTESIAN_POINT('Ctrl Pts',(5.74883548399994,15.2,-9.94016363100001));
#164045=CARTESIAN_POINT('Ctrl Pts',(5.74883548399994,11.6,-9.94016363100001));
#164046=CARTESIAN_POINT('Ctrl Pts',(5.74855424299994,15.2,-9.93637537100001));
#164047=CARTESIAN_POINT('Ctrl Pts',(5.74855424299994,11.6,-9.93637537100001));
#164048=CARTESIAN_POINT('Ctrl Pts',(5.74827044899994,15.2,-9.93259172100001));
#164049=CARTESIAN_POINT('Ctrl Pts',(5.74827044899994,11.6,-9.93259172100001));
#164050=CARTESIAN_POINT('Ctrl Pts',(5.74798410499994,15.2,-9.92881269000001));
#164051=CARTESIAN_POINT('Ctrl Pts',(5.74798410499994,11.6,-9.92881269000001));
#164052=CARTESIAN_POINT('Ctrl Pts',(5.74769521999994,15.2,-9.92503828300001));
#164053=CARTESIAN_POINT('Ctrl Pts',(5.74769521999994,11.6,-9.92503828300001));
#164054=CARTESIAN_POINT('Ctrl Pts',(5.74740379999994,15.2,-9.92126850900001));
#164055=CARTESIAN_POINT('Ctrl Pts',(5.74740379999994,11.6,-9.92126850900001));
#164056=CARTESIAN_POINT('Ctrl Pts',(5.74710985299995,15.2,-9.91750337600001));
#164057=CARTESIAN_POINT('Ctrl Pts',(5.74710985299995,11.6,-9.91750337600001));
#164058=CARTESIAN_POINT('Ctrl Pts',(5.74681338699994,15.2,-9.91374289100001));
#164059=CARTESIAN_POINT('Ctrl Pts',(5.74681338699994,11.6,-9.91374289100001));
#164060=CARTESIAN_POINT('Ctrl Pts',(5.74651440799995,15.2,-9.90998706400001));
#164061=CARTESIAN_POINT('Ctrl Pts',(5.74651440799995,11.6,-9.90998706400001));
#164062=CARTESIAN_POINT('Ctrl Pts',(5.74621292399994,15.2,-9.90623590000001));
#164063=CARTESIAN_POINT('Ctrl Pts',(5.74621292399994,11.6,-9.90623590000001));
#164064=CARTESIAN_POINT('Ctrl Pts',(5.74590893999994,15.2,-9.90248940500001));
#164065=CARTESIAN_POINT('Ctrl Pts',(5.74590893999994,11.6,-9.90248940500001));
#164066=CARTESIAN_POINT('Ctrl Pts',(5.74560246199994,15.2,-9.89874758700001));
#164067=CARTESIAN_POINT('Ctrl Pts',(5.74560246199994,11.6,-9.89874758700001));
#164068=CARTESIAN_POINT('Ctrl Pts',(5.74529349399994,15.2,-9.89501045000001));
#164069=CARTESIAN_POINT('Ctrl Pts',(5.74529349399994,11.6,-9.89501045000001));
#164070=CARTESIAN_POINT('Ctrl Pts',(5.74498204299994,15.2,-9.89127800100001));
#164071=CARTESIAN_POINT('Ctrl Pts',(5.74498204299994,11.6,-9.89127800100001));
#164072=CARTESIAN_POINT('Ctrl Pts',(5.74466811499994,15.2,-9.88755024700001));
#164073=CARTESIAN_POINT('Ctrl Pts',(5.74466811499994,11.6,-9.88755024700001));
#164074=CARTESIAN_POINT('Ctrl Pts',(5.74435171599994,15.2,-9.88382719300001));
#164075=CARTESIAN_POINT('Ctrl Pts',(5.74435171599994,11.6,-9.88382719300001));
#164076=CARTESIAN_POINT('Ctrl Pts',(5.74403285199995,15.2,-9.88010884600001));
#164077=CARTESIAN_POINT('Ctrl Pts',(5.74403285199995,11.6,-9.88010884600001));
#164078=CARTESIAN_POINT('Ctrl Pts',(5.74371152899994,15.2,-9.87639521400001));
#164079=CARTESIAN_POINT('Ctrl Pts',(5.74371152899994,11.6,-9.87639521400001));
#164080=CARTESIAN_POINT('Ctrl Pts',(5.74338775399994,15.2,-9.87268630200001));
#164081=CARTESIAN_POINT('Ctrl Pts',(5.74338775399994,11.6,-9.87268630200001));
#164082=CARTESIAN_POINT('Ctrl Pts',(5.74306153399994,15.2,-9.86898212000001));
#164083=CARTESIAN_POINT('Ctrl Pts',(5.74306153399994,11.6,-9.86898212000001));
#164084=CARTESIAN_POINT('Ctrl Pts',(5.74273287599994,15.2,-9.86528267200001));
#164085=CARTESIAN_POINT('Ctrl Pts',(5.74273287599994,11.6,-9.86528267200001));
#164086=CARTESIAN_POINT('Ctrl Pts',(5.74240178399994,15.2,-9.86158796700001));
#164087=CARTESIAN_POINT('Ctrl Pts',(5.74240178399994,11.6,-9.86158796700001));
#164088=CARTESIAN_POINT('Ctrl Pts',(5.74206826599994,15.2,-9.85789800900001));
#164089=CARTESIAN_POINT('Ctrl Pts',(5.74206826599994,11.6,-9.85789800900001));
#164090=CARTESIAN_POINT('Ctrl Pts',(5.74173232899994,15.2,-9.85421280600001));
#164091=CARTESIAN_POINT('Ctrl Pts',(5.74173232899994,11.6,-9.85421280600001));
#164092=CARTESIAN_POINT('Ctrl Pts',(5.74139397699994,15.2,-9.85053236500001));
#164093=CARTESIAN_POINT('Ctrl Pts',(5.74139397699994,11.6,-9.85053236500001));
#164094=CARTESIAN_POINT('Ctrl Pts',(5.74105321799995,15.2,-9.84685669200001));
#164095=CARTESIAN_POINT('Ctrl Pts',(5.74105321799995,11.6,-9.84685669200001));
#164096=CARTESIAN_POINT('Ctrl Pts',(5.74071005799994,15.2,-9.84318579400002));
#164097=CARTESIAN_POINT('Ctrl Pts',(5.74071005799994,11.6,-9.84318579400002));
#164098=CARTESIAN_POINT('Ctrl Pts',(5.74036450299994,15.2,-9.83951967700001));
#164099=CARTESIAN_POINT('Ctrl Pts',(5.74036450299994,11.6,-9.83951967700001));
#164100=CARTESIAN_POINT('Ctrl Pts',(5.74001655999995,15.2,-9.83585834800001));
#164101=CARTESIAN_POINT('Ctrl Pts',(5.74001655999995,11.6,-9.83585834800001));
#164102=CARTESIAN_POINT('Ctrl Pts',(5.73966623499994,15.2,-9.83220181600001));
#164103=CARTESIAN_POINT('Ctrl Pts',(5.73966623499994,11.6,-9.83220181600001));
#164104=CARTESIAN_POINT('Ctrl Pts',(5.73931353499994,15.2,-9.82855008400001));
#164105=CARTESIAN_POINT('Ctrl Pts',(5.73931353499994,11.6,-9.82855008400001));
#164106=CARTESIAN_POINT('Ctrl Pts',(5.73895846599994,15.2,-9.82490316000001));
#164107=CARTESIAN_POINT('Ctrl Pts',(5.73895846599994,11.6,-9.82490316000001));
#164108=CARTESIAN_POINT('Ctrl Pts',(5.73860103599994,15.2,-9.82126105300001));
#164109=CARTESIAN_POINT('Ctrl Pts',(5.73860103599994,11.6,-9.82126105300001));
#164110=CARTESIAN_POINT('Ctrl Pts',(5.73824124899994,15.2,-9.81762376700001));
#164111=CARTESIAN_POINT('Ctrl Pts',(5.73824124899994,11.6,-9.81762376700001));
#164112=CARTESIAN_POINT('Ctrl Pts',(5.73787911299994,15.2,-9.81399131000001));
#164113=CARTESIAN_POINT('Ctrl Pts',(5.73787911299994,11.6,-9.81399131000001));
#164114=CARTESIAN_POINT('Ctrl Pts',(5.73751463399994,15.2,-9.81036368900001));
#164115=CARTESIAN_POINT('Ctrl Pts',(5.73751463399994,11.6,-9.81036368900001));
#164116=CARTESIAN_POINT('Ctrl Pts',(5.73714781999994,15.2,-9.80674091000001));
#164117=CARTESIAN_POINT('Ctrl Pts',(5.73714781999994,11.6,-9.80674091000001));
#164118=CARTESIAN_POINT('Ctrl Pts',(5.73677867499994,15.2,-9.80312298100001));
#164119=CARTESIAN_POINT('Ctrl Pts',(5.73677867499994,11.6,-9.80312298100001));
#164120=CARTESIAN_POINT('Ctrl Pts',(5.73640720799995,15.2,-9.79950990700001));
#164121=CARTESIAN_POINT('Ctrl Pts',(5.73640720799995,11.6,-9.79950990700001));
#164122=CARTESIAN_POINT('Ctrl Pts',(5.73603342399994,15.2,-9.79590169600001));
#164123=CARTESIAN_POINT('Ctrl Pts',(5.73603342399994,11.6,-9.79590169600001));
#164124=CARTESIAN_POINT('Ctrl Pts',(5.73565733099994,15.2,-9.79229835400002));
#164125=CARTESIAN_POINT('Ctrl Pts',(5.73565733099994,11.6,-9.79229835400002));
#164126=CARTESIAN_POINT('Ctrl Pts',(5.73527893499994,15.2,-9.78869989000001));
#164127=CARTESIAN_POINT('Ctrl Pts',(5.73527893499994,11.6,-9.78869989000001));
#164128=CARTESIAN_POINT('Ctrl Pts',(5.73489824299994,15.2,-9.78510630700001));
#164129=CARTESIAN_POINT('Ctrl Pts',(5.73489824299994,11.6,-9.78510630700001));
#164130=CARTESIAN_POINT('Ctrl Pts',(5.73451525999994,15.2,-9.78151761500001));
#164131=CARTESIAN_POINT('Ctrl Pts',(5.73451525999994,11.6,-9.78151761500001));
#164132=CARTESIAN_POINT('Ctrl Pts',(5.73412999599994,15.2,-9.77793382000001));
#164133=CARTESIAN_POINT('Ctrl Pts',(5.73412999599994,11.6,-9.77793382000001));
#164134=CARTESIAN_POINT('Ctrl Pts',(5.73374245399994,15.2,-9.77435492900001));
#164135=CARTESIAN_POINT('Ctrl Pts',(5.73374245399994,11.6,-9.77435492900001));
#164136=CARTESIAN_POINT('Ctrl Pts',(5.73335264299994,15.2,-9.77078094800001));
#164137=CARTESIAN_POINT('Ctrl Pts',(5.73335264299994,11.6,-9.77078094800001));
#164138=CARTESIAN_POINT('Ctrl Pts',(5.73296056899995,15.2,-9.76721188400001));
#164139=CARTESIAN_POINT('Ctrl Pts',(5.73296056899995,11.6,-9.76721188400001));
#164140=CARTESIAN_POINT('Ctrl Pts',(5.73256623999994,15.2,-9.76364774500001));
#164141=CARTESIAN_POINT('Ctrl Pts',(5.73256623999994,11.6,-9.76364774500001));
#164142=CARTESIAN_POINT('Ctrl Pts',(5.73216966099994,15.2,-9.76008853600001));
#164143=CARTESIAN_POINT('Ctrl Pts',(5.73216966099994,11.6,-9.76008853600001));
#164144=CARTESIAN_POINT('Ctrl Pts',(5.73177084099994,15.2,-9.75653426500001));
#164145=CARTESIAN_POINT('Ctrl Pts',(5.73177084099994,11.6,-9.75653426500001));
#164146=CARTESIAN_POINT('Ctrl Pts',(5.73136978399994,15.2,-9.75298493900001));
#164147=CARTESIAN_POINT('Ctrl Pts',(5.73136978399994,11.6,-9.75298493900001));
#164148=CARTESIAN_POINT('Ctrl Pts',(5.73096649899995,15.2,-9.74944056400001));
#164149=CARTESIAN_POINT('Ctrl Pts',(5.73096649899995,11.6,-9.74944056400001));
#164150=CARTESIAN_POINT('Ctrl Pts',(5.73056099299994,15.2,-9.74590114900001));
#164151=CARTESIAN_POINT('Ctrl Pts',(5.73056099299994,11.6,-9.74590114900001));
#164152=CARTESIAN_POINT('Ctrl Pts',(5.73015327099994,15.2,-9.74236669900001));
#164153=CARTESIAN_POINT('Ctrl Pts',(5.73015327099994,11.6,-9.74236669900001));
#164154=CARTESIAN_POINT('Ctrl Pts',(5.72974333999994,15.2,-9.73883722000001));
#164155=CARTESIAN_POINT('Ctrl Pts',(5.72974333999994,11.6,-9.73883722000001));
#164156=CARTESIAN_POINT('Ctrl Pts',(5.72933120899994,15.2,-9.73531272100001));
#164157=CARTESIAN_POINT('Ctrl Pts',(5.72933120899994,11.6,-9.73531272100001));
#164158=CARTESIAN_POINT('Ctrl Pts',(5.72891688399994,15.2,-9.73179320900002));
#164159=CARTESIAN_POINT('Ctrl Pts',(5.72891688399994,11.6,-9.73179320900002));
#164160=CARTESIAN_POINT('Ctrl Pts',(5.72850037199994,15.2,-9.72827868900001));
#164161=CARTESIAN_POINT('Ctrl Pts',(5.72850037199994,11.6,-9.72827868900001));
#164162=CARTESIAN_POINT('Ctrl Pts',(5.72808167899994,15.2,-9.72476917000001));
#164163=CARTESIAN_POINT('Ctrl Pts',(5.72808167899994,11.6,-9.72476917000001));
#164164=CARTESIAN_POINT('Ctrl Pts',(5.72766081399994,15.2,-9.72126465700001));
#164165=CARTESIAN_POINT('Ctrl Pts',(5.72766081399994,11.6,-9.72126465700001));
#164166=CARTESIAN_POINT('Ctrl Pts',(5.72723778199995,15.2,-9.71776515800001));
#164167=CARTESIAN_POINT('Ctrl Pts',(5.72723778199995,11.6,-9.71776515800001));
#164168=CARTESIAN_POINT('Ctrl Pts',(5.72681258999994,15.2,-9.71427068000001));
#164169=CARTESIAN_POINT('Ctrl Pts',(5.72681258999994,11.6,-9.71427068000001));
#164170=CARTESIAN_POINT('Ctrl Pts',(5.72638524699995,15.2,-9.71078123000001));
#164171=CARTESIAN_POINT('Ctrl Pts',(5.72638524699995,11.6,-9.71078123000001));
#164172=CARTESIAN_POINT('Ctrl Pts',(5.72595575799995,15.2,-9.70729681500002));
#164173=CARTESIAN_POINT('Ctrl Pts',(5.72595575799995,11.6,-9.70729681500002));
#164174=CARTESIAN_POINT('Ctrl Pts',(5.72552413199994,15.2,-9.70381744100001));
#164175=CARTESIAN_POINT('Ctrl Pts',(5.72552413199994,11.6,-9.70381744100001));
#164176=CARTESIAN_POINT('Ctrl Pts',(5.72509037399994,15.2,-9.70034311500001));
#164177=CARTESIAN_POINT('Ctrl Pts',(5.72509037399994,11.6,-9.70034311500001));
#164178=CARTESIAN_POINT('Ctrl Pts',(5.72465449299995,15.2,-9.69687384600001));
#164179=CARTESIAN_POINT('Ctrl Pts',(5.72465449299995,11.6,-9.69687384600001));
#164180=CARTESIAN_POINT('Ctrl Pts',(5.72421649499995,15.2,-9.69340963900001));
#164181=CARTESIAN_POINT('Ctrl Pts',(5.72421649499995,11.6,-9.69340963900001));
#164182=CARTESIAN_POINT('Ctrl Pts',(5.72377638699994,15.2,-9.68995050200001));
#164183=CARTESIAN_POINT('Ctrl Pts',(5.72377638699994,11.6,-9.68995050200001));
#164184=CARTESIAN_POINT('Ctrl Pts',(5.72333417799994,15.2,-9.68649644100001));
#164185=CARTESIAN_POINT('Ctrl Pts',(5.72333417799994,11.6,-9.68649644100001));
#164186=CARTESIAN_POINT('Ctrl Pts',(5.72288987299994,15.2,-9.68304746400001));
#164187=CARTESIAN_POINT('Ctrl Pts',(5.72288987299994,11.6,-9.68304746400001));
#164188=CARTESIAN_POINT('Ctrl Pts',(5.72244347999994,15.2,-9.67960357800001));
#164189=CARTESIAN_POINT('Ctrl Pts',(5.72244347999994,11.6,-9.67960357800001));
#164190=CARTESIAN_POINT('Ctrl Pts',(5.72199500699995,15.2,-9.67616478900001));
#164191=CARTESIAN_POINT('Ctrl Pts',(5.72199500699995,11.6,-9.67616478900001));
#164192=CARTESIAN_POINT('Ctrl Pts',(5.72154445999995,15.2,-9.67273110600001));
#164193=CARTESIAN_POINT('Ctrl Pts',(5.72154445999995,11.6,-9.67273110600001));
#164194=CARTESIAN_POINT('Ctrl Pts',(5.72109184699994,15.2,-9.66930253400001));
#164195=CARTESIAN_POINT('Ctrl Pts',(5.72109184699994,11.6,-9.66930253400001));
#164196=CARTESIAN_POINT('Ctrl Pts',(5.72063717499995,15.2,-9.66587908100001));
#164197=CARTESIAN_POINT('Ctrl Pts',(5.72063717499995,11.6,-9.66587908100001));
#164198=CARTESIAN_POINT('Ctrl Pts',(5.72018045099995,15.2,-9.66246075400001));
#164199=CARTESIAN_POINT('Ctrl Pts',(5.72018045099995,11.6,-9.66246075400001));
#164200=CARTESIAN_POINT('Ctrl Pts',(5.71972168399995,15.2,-9.65904755900001));
#164201=CARTESIAN_POINT('Ctrl Pts',(5.71972168399995,11.6,-9.65904755900001));
#164202=CARTESIAN_POINT('Ctrl Pts',(5.71926087999994,15.2,-9.65563950500002));
#164203=CARTESIAN_POINT('Ctrl Pts',(5.71926087999994,11.6,-9.65563950500002));
#164204=CARTESIAN_POINT('Ctrl Pts',(5.71879804599994,15.2,-9.65223659800002));
#164205=CARTESIAN_POINT('Ctrl Pts',(5.71879804599994,11.6,-9.65223659800002));
#164206=CARTESIAN_POINT('Ctrl Pts',(5.71833318999994,15.2,-9.64883884500002));
#164207=CARTESIAN_POINT('Ctrl Pts',(5.71833318999994,11.6,-9.64883884500002));
#164208=CARTESIAN_POINT('Ctrl Pts',(5.71786631899994,15.2,-9.64544625300002));
#164209=CARTESIAN_POINT('Ctrl Pts',(5.71786631899994,11.6,-9.64544625300002));
#164210=CARTESIAN_POINT('Ctrl Pts',(5.71739744199995,15.2,-9.64205883000002));
#164211=CARTESIAN_POINT('Ctrl Pts',(5.71739744199995,11.6,-9.64205883000002));
#164212=CARTESIAN_POINT('Ctrl Pts',(5.71692656399994,15.2,-9.63867658200002));
#164213=CARTESIAN_POINT('Ctrl Pts',(5.71692656399994,11.6,-9.63867658200002));
#164214=CARTESIAN_POINT('Ctrl Pts',(5.71645369399994,15.2,-9.63529951700002));
#164215=CARTESIAN_POINT('Ctrl Pts',(5.71645369399994,11.6,-9.63529951700002));
#164216=CARTESIAN_POINT('Ctrl Pts',(5.71597883899994,15.2,-9.63192764200001));
#164217=CARTESIAN_POINT('Ctrl Pts',(5.71597883899994,11.6,-9.63192764200001));
#164218=CARTESIAN_POINT('Ctrl Pts',(5.71550200799994,15.2,-9.62856096300002));
#164219=CARTESIAN_POINT('Ctrl Pts',(5.71550200799994,11.6,-9.62856096300002));
#164220=CARTESIAN_POINT('Ctrl Pts',(5.71502320499994,15.2,-9.62519948800002));
#164221=CARTESIAN_POINT('Ctrl Pts',(5.71502320499994,11.6,-9.62519948800002));
#164222=CARTESIAN_POINT('Ctrl Pts',(5.71454244099994,15.2,-9.62184322500002));
#164223=CARTESIAN_POINT('Ctrl Pts',(5.71454244099994,11.6,-9.62184322500002));
#164224=CARTESIAN_POINT('Ctrl Pts',(5.71405972199994,15.2,-9.61849218000001));
#164225=CARTESIAN_POINT('Ctrl Pts',(5.71405972199994,11.6,-9.61849218000001));
#164226=CARTESIAN_POINT('Ctrl Pts',(5.71357505599994,15.2,-9.61514636100001));
#164227=CARTESIAN_POINT('Ctrl Pts',(5.71357505599994,11.6,-9.61514636100001));
#164228=CARTESIAN_POINT('Ctrl Pts',(5.71308845099994,15.2,-9.61180577300001));
#164229=CARTESIAN_POINT('Ctrl Pts',(5.71308845099994,11.6,-9.61180577300001));
#164230=CARTESIAN_POINT('Ctrl Pts',(5.71259991299994,15.2,-9.60847042600001));
#164231=CARTESIAN_POINT('Ctrl Pts',(5.71259991299994,11.6,-9.60847042600001));
#164232=CARTESIAN_POINT('Ctrl Pts',(5.71210945199994,15.2,-9.60514032600001));
#164233=CARTESIAN_POINT('Ctrl Pts',(5.71210945199994,11.6,-9.60514032600001));
#164234=CARTESIAN_POINT('Ctrl Pts',(5.71161707499994,15.2,-9.60181548000002));
#164235=CARTESIAN_POINT('Ctrl Pts',(5.71161707499994,11.6,-9.60181548000002));
#164236=CARTESIAN_POINT('Ctrl Pts',(5.71112278699994,15.2,-9.59849589500001));
#164237=CARTESIAN_POINT('Ctrl Pts',(5.71112278699994,11.6,-9.59849589500001));
#164238=CARTESIAN_POINT('Ctrl Pts',(5.71062659999994,15.2,-9.59518158000002));
#164239=CARTESIAN_POINT('Ctrl Pts',(5.71062659999994,11.6,-9.59518158000002));
#164240=CARTESIAN_POINT('Ctrl Pts',(5.71012851799994,15.2,-9.59187253900001));
#164241=CARTESIAN_POINT('Ctrl Pts',(5.71012851799994,11.6,-9.59187253900001));
#164242=CARTESIAN_POINT('Ctrl Pts',(5.70962855099994,15.2,-9.58856878200002));
#164243=CARTESIAN_POINT('Ctrl Pts',(5.70962855099994,11.6,-9.58856878200002));
#164244=CARTESIAN_POINT('Ctrl Pts',(5.70912670599995,15.2,-9.58527031600001));
#164245=CARTESIAN_POINT('Ctrl Pts',(5.70912670599995,11.6,-9.58527031600001));
#164246=CARTESIAN_POINT('Ctrl Pts',(5.70862299199995,15.2,-9.58197714600002));
#164247=CARTESIAN_POINT('Ctrl Pts',(5.70862299199995,11.6,-9.58197714600002));
#164248=CARTESIAN_POINT('Ctrl Pts',(5.70811741599995,15.2,-9.57868928200002));
#164249=CARTESIAN_POINT('Ctrl Pts',(5.70811741599995,11.6,-9.57868928200002));
#164250=CARTESIAN_POINT('Ctrl Pts',(5.70760998399994,15.2,-9.57540673000001));
#164251=CARTESIAN_POINT('Ctrl Pts',(5.70760998399994,11.6,-9.57540673000001));
#164252=CARTESIAN_POINT('Ctrl Pts',(5.70710070599994,15.2,-9.57212949500001));
#164253=CARTESIAN_POINT('Ctrl Pts',(5.70710070599994,11.6,-9.57212949500001));
#164254=CARTESIAN_POINT('Ctrl Pts',(5.70658958999994,15.2,-9.56885759000001));
#164255=CARTESIAN_POINT('Ctrl Pts',(5.70658958999994,11.6,-9.56885759000001));
#164256=CARTESIAN_POINT('Ctrl Pts',(5.70607664199994,15.2,-9.56559101600002));
#164257=CARTESIAN_POINT('Ctrl Pts',(5.70607664199994,11.6,-9.56559101600002));
#164258=CARTESIAN_POINT('Ctrl Pts',(5.70556187299994,15.2,-9.56232978500001));
#164259=CARTESIAN_POINT('Ctrl Pts',(5.70556187299994,11.6,-9.56232978500001));
#164260=CARTESIAN_POINT('Ctrl Pts',(5.70504528799994,15.2,-9.55907390100002));
#164261=CARTESIAN_POINT('Ctrl Pts',(5.70504528799994,11.6,-9.55907390100002));
#164262=CARTESIAN_POINT('Ctrl Pts',(5.70452689699994,15.2,-9.55582337400001));
#164263=CARTESIAN_POINT('Ctrl Pts',(5.70452689699994,11.6,-9.55582337400001));
#164264=CARTESIAN_POINT('Ctrl Pts',(5.70400670599994,15.2,-9.55257821000002));
#164265=CARTESIAN_POINT('Ctrl Pts',(5.70400670599994,11.6,-9.55257821000002));
#164266=CARTESIAN_POINT('Ctrl Pts',(5.70348472499995,15.2,-9.54933841600001));
#164267=CARTESIAN_POINT('Ctrl Pts',(5.70348472499995,11.6,-9.54933841600001));
#164268=CARTESIAN_POINT('Ctrl Pts',(5.70296095999995,15.2,-9.54610399900002));
#164269=CARTESIAN_POINT('Ctrl Pts',(5.70296095999995,11.6,-9.54610399900002));
#164270=CARTESIAN_POINT('Ctrl Pts',(5.70243542199995,15.2,-9.54287496800001));
#164271=CARTESIAN_POINT('Ctrl Pts',(5.70243542199995,11.6,-9.54287496800001));
#164272=CARTESIAN_POINT('Ctrl Pts',(5.70190811599995,15.2,-9.53965133000001));
#164273=CARTESIAN_POINT('Ctrl Pts',(5.70190811599995,11.6,-9.53965133000001));
#164274=CARTESIAN_POINT('Ctrl Pts',(5.70137905199994,15.2,-9.53643309100002));
#164275=CARTESIAN_POINT('Ctrl Pts',(5.70137905199994,11.6,-9.53643309100002));
#164276=CARTESIAN_POINT('Ctrl Pts',(5.70084823799994,15.2,-9.53322025800002));
#164277=CARTESIAN_POINT('Ctrl Pts',(5.70084823799994,11.6,-9.53322025800002));
#164278=CARTESIAN_POINT('Ctrl Pts',(5.70031568099994,15.2,-9.53001284100001));
#164279=CARTESIAN_POINT('Ctrl Pts',(5.70031568099994,11.6,-9.53001284100001));
#164280=CARTESIAN_POINT('Ctrl Pts',(5.69978138899994,15.2,-9.52681084500002));
#164281=CARTESIAN_POINT('Ctrl Pts',(5.69978138899994,11.6,-9.52681084500002));
#164282=CARTESIAN_POINT('Ctrl Pts',(5.69924537299995,15.2,-9.52361427900002));
#164283=CARTESIAN_POINT('Ctrl Pts',(5.69924537299995,11.6,-9.52361427900002));
#164284=CARTESIAN_POINT('Ctrl Pts',(5.69870763799995,15.2,-9.52042315000002));
#164285=CARTESIAN_POINT('Ctrl Pts',(5.69870763799995,11.6,-9.52042315000002));
#164286=CARTESIAN_POINT('Ctrl Pts',(5.69816819399994,15.2,-9.51723746400001));
#164287=CARTESIAN_POINT('Ctrl Pts',(5.69816819399994,11.6,-9.51723746400001));
#164288=CARTESIAN_POINT('Ctrl Pts',(5.69762704799994,15.2,-9.51405723000001));
#164289=CARTESIAN_POINT('Ctrl Pts',(5.69762704799994,11.6,-9.51405723000001));
#164290=CARTESIAN_POINT('Ctrl Pts',(5.69708420999994,15.2,-9.51088245500002));
#164291=CARTESIAN_POINT('Ctrl Pts',(5.69708420999994,11.6,-9.51088245500002));
#164292=CARTESIAN_POINT('Ctrl Pts',(5.69653968699994,15.2,-9.50771314600001));
#164293=CARTESIAN_POINT('Ctrl Pts',(5.69653968699994,11.6,-9.50771314600001));
#164294=CARTESIAN_POINT('Ctrl Pts',(5.69599348799994,15.2,-9.50454931200002));
#164295=CARTESIAN_POINT('Ctrl Pts',(5.69599348799994,11.6,-9.50454931200002));
#164296=CARTESIAN_POINT('Ctrl Pts',(5.69544561999995,15.2,-9.50139095900001));
#164297=CARTESIAN_POINT('Ctrl Pts',(5.69544561999995,11.6,-9.50139095900001));
#164298=CARTESIAN_POINT('Ctrl Pts',(5.69489609299994,15.2,-9.49823809400002));
#164299=CARTESIAN_POINT('Ctrl Pts',(5.69489609299994,11.6,-9.49823809400002));
#164300=CARTESIAN_POINT('Ctrl Pts',(5.69434491599995,15.2,-9.49509072500001));
#164301=CARTESIAN_POINT('Ctrl Pts',(5.69434491599995,11.6,-9.49509072500001));
#164302=CARTESIAN_POINT('Ctrl Pts',(5.69379209399995,15.2,-9.49194886000001));
#164303=CARTESIAN_POINT('Ctrl Pts',(5.69379209399995,11.6,-9.49194886000001));
#164304=CARTESIAN_POINT('Ctrl Pts',(5.69323763999994,15.2,-9.48881250600002));
#164305=CARTESIAN_POINT('Ctrl Pts',(5.69323763999994,11.6,-9.48881250600002));
#164306=CARTESIAN_POINT('Ctrl Pts',(5.69268155899994,15.2,-9.48568167100002));
#164307=CARTESIAN_POINT('Ctrl Pts',(5.69268155899994,11.6,-9.48568167100002));
#164308=CARTESIAN_POINT('Ctrl Pts',(5.69212386099994,15.2,-9.48255636200001));
#164309=CARTESIAN_POINT('Ctrl Pts',(5.69212386099994,11.6,-9.48255636200001));
#164310=CARTESIAN_POINT('Ctrl Pts',(5.69156455399994,15.2,-9.47943658700002));
#164311=CARTESIAN_POINT('Ctrl Pts',(5.69156455399994,11.6,-9.47943658700002));
#164312=CARTESIAN_POINT('Ctrl Pts',(5.69100364599994,15.2,-9.47632235300001));
#164313=CARTESIAN_POINT('Ctrl Pts',(5.69100364599994,11.6,-9.47632235300001));
#164314=CARTESIAN_POINT('Ctrl Pts',(5.69044114799994,15.2,-9.47321366800002));
#164315=CARTESIAN_POINT('Ctrl Pts',(5.69044114799994,11.6,-9.47321366800002));
#164316=CARTESIAN_POINT('Ctrl Pts',(5.68987706599994,15.2,-9.47011053900002));
#164317=CARTESIAN_POINT('Ctrl Pts',(5.68987706599994,11.6,-9.47011053900002));
#164318=CARTESIAN_POINT('Ctrl Pts',(5.68931140899994,15.2,-9.46701297400002));
#164319=CARTESIAN_POINT('Ctrl Pts',(5.68931140899994,11.6,-9.46701297400002));
#164320=CARTESIAN_POINT('Ctrl Pts',(5.68874418599995,15.2,-9.46392098000001));
#164321=CARTESIAN_POINT('Ctrl Pts',(5.68874418599995,11.6,-9.46392098000001));
#164322=CARTESIAN_POINT('Ctrl Pts',(5.68817540599994,15.2,-9.46083456600002));
#164323=CARTESIAN_POINT('Ctrl Pts',(5.68817540599994,11.6,-9.46083456600002));
#164324=CARTESIAN_POINT('Ctrl Pts',(5.68760507799994,15.2,-9.45775373800002));
#164325=CARTESIAN_POINT('Ctrl Pts',(5.68760507799994,11.6,-9.45775373800002));
#164326=CARTESIAN_POINT('Ctrl Pts',(5.68703320999995,15.2,-9.45467850400001));
#164327=CARTESIAN_POINT('Ctrl Pts',(5.68703320999995,11.6,-9.45467850400001));
#164328=CARTESIAN_POINT('Ctrl Pts',(5.68645981099994,15.2,-9.45160887100002));
#164329=CARTESIAN_POINT('Ctrl Pts',(5.68645981099994,11.6,-9.45160887100002));
#164330=CARTESIAN_POINT('Ctrl Pts',(5.68588488999994,15.2,-9.44854484900001));
#164331=CARTESIAN_POINT('Ctrl Pts',(5.68588488999994,11.6,-9.44854484900001));
#164332=CARTESIAN_POINT('Ctrl Pts',(5.68530845499994,15.2,-9.44548644300001));
#164333=CARTESIAN_POINT('Ctrl Pts',(5.68530845499994,11.6,-9.44548644300001));
#164334=CARTESIAN_POINT('Ctrl Pts',(5.68473051499994,15.2,-9.44243366200002));
#164335=CARTESIAN_POINT('Ctrl Pts',(5.68473051499994,11.6,-9.44243366200002));
#164336=CARTESIAN_POINT('Ctrl Pts',(5.68415107899994,15.2,-9.43938651300002));
#164337=CARTESIAN_POINT('Ctrl Pts',(5.68415107899994,11.6,-9.43938651300002));
#164338=CARTESIAN_POINT('Ctrl Pts',(5.68357015699994,15.2,-9.43634500500002));
#164339=CARTESIAN_POINT('Ctrl Pts',(5.68357015699994,11.6,-9.43634500500002));
#164340=CARTESIAN_POINT('Ctrl Pts',(5.68298775599994,15.2,-9.43330914300001));
#164341=CARTESIAN_POINT('Ctrl Pts',(5.68298775599994,11.6,-9.43330914300001));
#164342=CARTESIAN_POINT('Ctrl Pts',(5.68240388599994,15.2,-9.43027893700001));
#164343=CARTESIAN_POINT('Ctrl Pts',(5.68240388599994,11.6,-9.43027893700001));
#164344=CARTESIAN_POINT('Ctrl Pts',(5.68181855599994,15.2,-9.42725439300002));
#164345=CARTESIAN_POINT('Ctrl Pts',(5.68181855599994,11.6,-9.42725439300002));
#164346=CARTESIAN_POINT('Ctrl Pts',(5.68123177399994,15.2,-9.42423552100001));
#164347=CARTESIAN_POINT('Ctrl Pts',(5.68123177399994,11.6,-9.42423552100001));
#164348=CARTESIAN_POINT('Ctrl Pts',(5.68064354999994,15.2,-9.42122232700001));
#164349=CARTESIAN_POINT('Ctrl Pts',(5.68064354999994,11.6,-9.42122232700001));
#164350=CARTESIAN_POINT('Ctrl Pts',(5.68005389299994,15.2,-9.41821481800002));
#164351=CARTESIAN_POINT('Ctrl Pts',(5.68005389299994,11.6,-9.41821481800002));
#164352=CARTESIAN_POINT('Ctrl Pts',(5.67946281099994,15.2,-9.41521300400002));
#164353=CARTESIAN_POINT('Ctrl Pts',(5.67946281099994,11.6,-9.41521300400002));
#164354=CARTESIAN_POINT('Ctrl Pts',(5.67887031499994,15.2,-9.41221689100002));
#164355=CARTESIAN_POINT('Ctrl Pts',(5.67887031499994,11.6,-9.41221689100002));
#164356=CARTESIAN_POINT('Ctrl Pts',(5.67827641199995,15.2,-9.40922648700001));
#164357=CARTESIAN_POINT('Ctrl Pts',(5.67827641199995,11.6,-9.40922648700001));
#164358=CARTESIAN_POINT('Ctrl Pts',(5.67768111099994,15.2,-9.40624180000002));
#164359=CARTESIAN_POINT('Ctrl Pts',(5.67768111099994,11.6,-9.40624180000002));
#164360=CARTESIAN_POINT('Ctrl Pts',(5.67708442399995,15.2,-9.40326283800001));
#164361=CARTESIAN_POINT('Ctrl Pts',(5.67708442399995,11.6,-9.40326283800001));
#164362=CARTESIAN_POINT('Ctrl Pts',(5.67648635699994,15.2,-9.40028960800002));
#164363=CARTESIAN_POINT('Ctrl Pts',(5.67648635699994,11.6,-9.40028960800002));
#164364=CARTESIAN_POINT('Ctrl Pts',(5.67588692199994,15.2,-9.39732211900001));
#164365=CARTESIAN_POINT('Ctrl Pts',(5.67588692199994,11.6,-9.39732211900001));
#164366=CARTESIAN_POINT('Ctrl Pts',(5.67528612499995,15.2,-9.39436037700002));
#164367=CARTESIAN_POINT('Ctrl Pts',(5.67528612499995,11.6,-9.39436037700002));
#164368=CARTESIAN_POINT('Ctrl Pts',(5.67468397799994,15.2,-9.39140439100001));
#164369=CARTESIAN_POINT('Ctrl Pts',(5.67468397799994,11.6,-9.39140439100001));
#164370=CARTESIAN_POINT('Ctrl Pts',(5.67408048899994,15.2,-9.38845416900002));
#164371=CARTESIAN_POINT('Ctrl Pts',(5.67408048899994,11.6,-9.38845416900002));
#164372=CARTESIAN_POINT('Ctrl Pts',(5.67347566799994,15.2,-9.38550971800002));
#164373=CARTESIAN_POINT('Ctrl Pts',(5.67347566799994,11.6,-9.38550971800002));
#164374=CARTESIAN_POINT('Ctrl Pts',(5.67286952299994,15.2,-9.38257104700002));
#164375=CARTESIAN_POINT('Ctrl Pts',(5.67286952299994,11.6,-9.38257104700002));
#164376=CARTESIAN_POINT('Ctrl Pts',(5.67226206399994,15.2,-9.37963816300002));
#164377=CARTESIAN_POINT('Ctrl Pts',(5.67226206399994,11.6,-9.37963816300002));
#164378=CARTESIAN_POINT('Ctrl Pts',(5.67165330199994,15.2,-9.37671107400002));
#164379=CARTESIAN_POINT('Ctrl Pts',(5.67165330199994,11.6,-9.37671107400002));
#164380=CARTESIAN_POINT('Ctrl Pts',(5.67104324399994,15.2,-9.37378978800002));
#164381=CARTESIAN_POINT('Ctrl Pts',(5.67104324399994,11.6,-9.37378978800002));
#164382=CARTESIAN_POINT('Ctrl Pts',(5.67043190099994,15.2,-9.37087431300002));
#164383=CARTESIAN_POINT('Ctrl Pts',(5.67043190099994,11.6,-9.37087431300002));
#164384=CARTESIAN_POINT('Ctrl Pts',(5.66981928099994,15.2,-9.36796465500001));
#164385=CARTESIAN_POINT('Ctrl Pts',(5.66981928099994,11.6,-9.36796465500001));
#164386=CARTESIAN_POINT('Ctrl Pts',(5.66920539599994,15.2,-9.36506082500001));
#164387=CARTESIAN_POINT('Ctrl Pts',(5.66920539599994,11.6,-9.36506082500001));
#164388=CARTESIAN_POINT('Ctrl Pts',(5.66859025199995,15.2,-9.36216282900002));
#164389=CARTESIAN_POINT('Ctrl Pts',(5.66859025199995,11.6,-9.36216282900002));
#164390=CARTESIAN_POINT('Ctrl Pts',(5.66797386299994,15.2,-9.35927067500002));
#164391=CARTESIAN_POINT('Ctrl Pts',(5.66797386299994,11.6,-9.35927067500002));
#164392=CARTESIAN_POINT('Ctrl Pts',(5.66735623499994,15.2,-9.35638437200002));
#164393=CARTESIAN_POINT('Ctrl Pts',(5.66735623499994,11.6,-9.35638437200002));
#164394=CARTESIAN_POINT('Ctrl Pts',(5.66673737799994,15.2,-9.35350392700002));
#164395=CARTESIAN_POINT('Ctrl Pts',(5.66673737799994,11.6,-9.35350392700002));
#164396=CARTESIAN_POINT('Ctrl Pts',(5.66611730199994,15.2,-9.35062934800002));
#164397=CARTESIAN_POINT('Ctrl Pts',(5.66611730199994,11.6,-9.35062934800002));
#164398=CARTESIAN_POINT('Ctrl Pts',(5.66549601799994,15.2,-9.34776064300002));
#164399=CARTESIAN_POINT('Ctrl Pts',(5.66549601799994,11.6,-9.34776064300002));
#164400=CARTESIAN_POINT('Ctrl Pts',(5.66487353399994,15.2,-9.34489782000002));
#164401=CARTESIAN_POINT('Ctrl Pts',(5.66487353399994,11.6,-9.34489782000002));
#164402=CARTESIAN_POINT('Ctrl Pts',(5.66424986199994,15.2,-9.34204088700002));
#164403=CARTESIAN_POINT('Ctrl Pts',(5.66424986199994,11.6,-9.34204088700002));
#164404=CARTESIAN_POINT('Ctrl Pts',(5.66362500799994,15.2,-9.33918985300001));
#164405=CARTESIAN_POINT('Ctrl Pts',(5.66362500799994,11.6,-9.33918985300001));
#164406=CARTESIAN_POINT('Ctrl Pts',(5.66299898499994,15.2,-9.33634472400002));
#164407=CARTESIAN_POINT('Ctrl Pts',(5.66299898499994,11.6,-9.33634472400002));
#164408=CARTESIAN_POINT('Ctrl Pts',(5.66237180199994,15.2,-9.33350551000002));
#164409=CARTESIAN_POINT('Ctrl Pts',(5.66237180199994,11.6,-9.33350551000002));
#164410=CARTESIAN_POINT('Ctrl Pts',(5.66174346799994,15.2,-9.33067221700002));
#164411=CARTESIAN_POINT('Ctrl Pts',(5.66174346799994,11.6,-9.33067221700002));
#164412=CARTESIAN_POINT('Ctrl Pts',(5.66111399299994,15.2,-9.32784485400001));
#164413=CARTESIAN_POINT('Ctrl Pts',(5.66111399299994,11.6,-9.32784485400001));
#164414=CARTESIAN_POINT('Ctrl Pts',(5.66048338799994,15.2,-9.32502343000002));
#164415=CARTESIAN_POINT('Ctrl Pts',(5.66048338799994,11.6,-9.32502343000002));
#164416=CARTESIAN_POINT('Ctrl Pts',(5.65985166199994,15.2,-9.32220795200001));
#164417=CARTESIAN_POINT('Ctrl Pts',(5.65985166199994,11.6,-9.32220795200001));
#164418=CARTESIAN_POINT('Ctrl Pts',(5.65921882599994,15.2,-9.31939842900002));
#164419=CARTESIAN_POINT('Ctrl Pts',(5.65921882599994,11.6,-9.31939842900002));
#164420=CARTESIAN_POINT('Ctrl Pts',(5.65858488799994,15.2,-9.31659486700001));
#164421=CARTESIAN_POINT('Ctrl Pts',(5.65858488799994,11.6,-9.31659486700001));
#164422=CARTESIAN_POINT('Ctrl Pts',(5.65794985999994,15.2,-9.31379727700002));
#164423=CARTESIAN_POINT('Ctrl Pts',(5.65794985999994,11.6,-9.31379727700002));
#164424=CARTESIAN_POINT('Ctrl Pts',(5.65731374999994,15.2,-9.31100566400002));
#164425=CARTESIAN_POINT('Ctrl Pts',(5.65731374999994,11.6,-9.31100566400002));
#164426=CARTESIAN_POINT('Ctrl Pts',(5.65667657099994,15.2,-9.30822003900002));
#164427=CARTESIAN_POINT('Ctrl Pts',(5.65667657099994,11.6,-9.30822003900002));
#164428=CARTESIAN_POINT('Ctrl Pts',(5.65603833099994,15.2,-9.30544040900001));
#164429=CARTESIAN_POINT('Ctrl Pts',(5.65603833099994,11.6,-9.30544040900001));
#164430=CARTESIAN_POINT('Ctrl Pts',(5.65539903999994,15.2,-9.30266678100002));
#164431=CARTESIAN_POINT('Ctrl Pts',(5.65539903999994,11.6,-9.30266678100002));
#164432=CARTESIAN_POINT('Ctrl Pts',(5.65475870899995,15.2,-9.29989916500002));
#164433=CARTESIAN_POINT('Ctrl Pts',(5.65475870899995,11.6,-9.29989916500002));
#164434=CARTESIAN_POINT('Ctrl Pts',(5.65411734799994,15.2,-9.29713756800002));
#164435=CARTESIAN_POINT('Ctrl Pts',(5.65411734799994,11.6,-9.29713756800002));
#164436=CARTESIAN_POINT('Ctrl Pts',(5.65347496699995,15.2,-9.29438199800002));
#164437=CARTESIAN_POINT('Ctrl Pts',(5.65347496699995,11.6,-9.29438199800002));
#164438=CARTESIAN_POINT('Ctrl Pts',(5.65283157699994,15.2,-9.29163246400002));
#164439=CARTESIAN_POINT('Ctrl Pts',(5.65283157699994,11.6,-9.29163246400002));
#164440=CARTESIAN_POINT('Ctrl Pts',(5.65218718599994,15.2,-9.28888897500002));
#164441=CARTESIAN_POINT('Ctrl Pts',(5.65218718599994,11.6,-9.28888897500002));
#164442=CARTESIAN_POINT('Ctrl Pts',(5.65154180699994,15.2,-9.28615153700001));
#164443=CARTESIAN_POINT('Ctrl Pts',(5.65154180699994,11.6,-9.28615153700001));
#164444=CARTESIAN_POINT('Ctrl Pts',(5.65089544999994,15.2,-9.28342016000002));
#164445=CARTESIAN_POINT('Ctrl Pts',(5.65089544999994,11.6,-9.28342016000002));
#164446=CARTESIAN_POINT('Ctrl Pts',(5.65024812399994,15.2,-9.28069485100002));
#164447=CARTESIAN_POINT('Ctrl Pts',(5.65024812399994,11.6,-9.28069485100002));
#164448=CARTESIAN_POINT('Ctrl Pts',(5.64959983999994,15.2,-9.27797561900002));
#164449=CARTESIAN_POINT('Ctrl Pts',(5.64959983999994,11.6,-9.27797561900002));
#164450=CARTESIAN_POINT('Ctrl Pts',(5.64895060899994,15.2,-9.27526247200002));
#164451=CARTESIAN_POINT('Ctrl Pts',(5.64895060899994,11.6,-9.27526247200002));
#164452=CARTESIAN_POINT('Ctrl Pts',(5.64830044099994,15.2,-9.27255541800001));
#164453=CARTESIAN_POINT('Ctrl Pts',(5.64830044099994,11.6,-9.27255541800001));
#164454=CARTESIAN_POINT('Ctrl Pts',(5.64764934599994,15.2,-9.26985446700002));
#164455=CARTESIAN_POINT('Ctrl Pts',(5.64764934599994,11.6,-9.26985446700002));
#164456=CARTESIAN_POINT('Ctrl Pts',(5.64699733599995,15.2,-9.26715962500002));
#164457=CARTESIAN_POINT('Ctrl Pts',(5.64699733599995,11.6,-9.26715962500002));
#164458=CARTESIAN_POINT('Ctrl Pts',(5.64634441999995,15.2,-9.26447090200002));
#164459=CARTESIAN_POINT('Ctrl Pts',(5.64634441999995,11.6,-9.26447090200002));
#164460=CARTESIAN_POINT('Ctrl Pts',(5.64569060899994,15.2,-9.26178830500002));
#164461=CARTESIAN_POINT('Ctrl Pts',(5.64569060899994,11.6,-9.26178830500002));
#164462=CARTESIAN_POINT('Ctrl Pts',(5.64503591399995,15.2,-9.25911184300002));
#164463=CARTESIAN_POINT('Ctrl Pts',(5.64503591399995,11.6,-9.25911184300002));
#164464=CARTESIAN_POINT('Ctrl Pts',(5.64438034599994,15.2,-9.25644152500002));
#164465=CARTESIAN_POINT('Ctrl Pts',(5.64438034599994,11.6,-9.25644152500002));
#164466=CARTESIAN_POINT('Ctrl Pts',(5.64372391599995,15.2,-9.25377735800001));
#164467=CARTESIAN_POINT('Ctrl Pts',(5.64372391599995,11.6,-9.25377735800001));
#164468=CARTESIAN_POINT('Ctrl Pts',(5.64306663299995,15.2,-9.25111935200002));
#164469=CARTESIAN_POINT('Ctrl Pts',(5.64306663299995,11.6,-9.25111935200002));
#164470=CARTESIAN_POINT('Ctrl Pts',(5.64240850899995,15.2,-9.24846751300001));
#164471=CARTESIAN_POINT('Ctrl Pts',(5.64240850899995,11.6,-9.24846751300001));
#164472=CARTESIAN_POINT('Ctrl Pts',(5.64174955499994,15.2,-9.24582185200002));
#164473=CARTESIAN_POINT('Ctrl Pts',(5.64174955499994,11.6,-9.24582185200002));
#164474=CARTESIAN_POINT('Ctrl Pts',(5.64108978099994,15.2,-9.24318237600002));
#164475=CARTESIAN_POINT('Ctrl Pts',(5.64108978099994,11.6,-9.24318237600002));
#164476=CARTESIAN_POINT('Ctrl Pts',(5.64042919799995,15.2,-9.24054909400001));
#164477=CARTESIAN_POINT('Ctrl Pts',(5.64042919799995,11.6,-9.24054909400001));
#164478=CARTESIAN_POINT('Ctrl Pts',(5.63976781599995,15.2,-9.23792201400002));
#164479=CARTESIAN_POINT('Ctrl Pts',(5.63976781599995,11.6,-9.23792201400002));
#164480=CARTESIAN_POINT('Ctrl Pts',(5.63910564999994,15.2,-9.23530114400002));
#164481=CARTESIAN_POINT('Ctrl Pts',(5.63910564999994,11.6,-9.23530114400002));
#164482=CARTESIAN_POINT('Ctrl Pts',(5.63844270699994,15.2,-9.23268649500002));
#164483=CARTESIAN_POINT('Ctrl Pts',(5.63844270699994,11.6,-9.23268649500002));
#164484=CARTESIAN_POINT('Ctrl Pts',(5.63777899799994,15.2,-9.23007807200002));
#164485=CARTESIAN_POINT('Ctrl Pts',(5.63777899799994,11.6,-9.23007807200002));
#164486=CARTESIAN_POINT('Ctrl Pts',(5.63711453599995,15.2,-9.22747588500001));
#164487=CARTESIAN_POINT('Ctrl Pts',(5.63711453599995,11.6,-9.22747588500001));
#164488=CARTESIAN_POINT('Ctrl Pts',(5.63644933199994,15.2,-9.22487994300001));
#164489=CARTESIAN_POINT('Ctrl Pts',(5.63644933199994,11.6,-9.22487994300001));
#164490=CARTESIAN_POINT('Ctrl Pts',(5.63578339499994,15.2,-9.22229025500001));
#164491=CARTESIAN_POINT('Ctrl Pts',(5.63578339499994,11.6,-9.22229025500001));
#164492=CARTESIAN_POINT('Ctrl Pts',(5.63511673699994,15.2,-9.21970682700002));
#164493=CARTESIAN_POINT('Ctrl Pts',(5.63511673699994,11.6,-9.21970682700002));
#164494=CARTESIAN_POINT('Ctrl Pts',(5.63444937099995,15.2,-9.21712967000002));
#164495=CARTESIAN_POINT('Ctrl Pts',(5.63444937099995,11.6,-9.21712967000002));
#164496=CARTESIAN_POINT('Ctrl Pts',(5.63378130699995,15.2,-9.21455879300002));
#164497=CARTESIAN_POINT('Ctrl Pts',(5.63378130699995,11.6,-9.21455879300002));
#164498=CARTESIAN_POINT('Ctrl Pts',(5.63311255499994,15.2,-9.21199420300002));
#164499=CARTESIAN_POINT('Ctrl Pts',(5.63311255499994,11.6,-9.21199420300002));
#164500=CARTESIAN_POINT('Ctrl Pts',(5.63244312799994,15.2,-9.20943590800002));
#164501=CARTESIAN_POINT('Ctrl Pts',(5.63244312799994,11.6,-9.20943590800002));
#164502=CARTESIAN_POINT('Ctrl Pts',(5.63177303699995,15.2,-9.20688391800002));
#164503=CARTESIAN_POINT('Ctrl Pts',(5.63177303699995,11.6,-9.20688391800002));
#164504=CARTESIAN_POINT('Ctrl Pts',(5.63110229299995,15.2,-9.20433824100002));
#164505=CARTESIAN_POINT('Ctrl Pts',(5.63110229299995,11.6,-9.20433824100002));
#164506=CARTESIAN_POINT('Ctrl Pts',(5.63043090699994,15.2,-9.20179888700002));
#164507=CARTESIAN_POINT('Ctrl Pts',(5.63043090699994,11.6,-9.20179888700002));
#164508=CARTESIAN_POINT('Ctrl Pts',(5.62975889099994,15.2,-9.19926586300001));
#164509=CARTESIAN_POINT('Ctrl Pts',(5.62975889099994,11.6,-9.19926586300001));
#164510=CARTESIAN_POINT('Ctrl Pts',(5.62908625599994,15.2,-9.19673917800001));
#164511=CARTESIAN_POINT('Ctrl Pts',(5.62908625599994,11.6,-9.19673917800001));
#164512=CARTESIAN_POINT('Ctrl Pts',(5.62841301499994,15.2,-9.19421884100002));
#164513=CARTESIAN_POINT('Ctrl Pts',(5.62841301499994,11.6,-9.19421884100002));
#164514=CARTESIAN_POINT('Ctrl Pts',(5.62773917699994,15.2,-9.19170486000001));
#164515=CARTESIAN_POINT('Ctrl Pts',(5.62773917699994,11.6,-9.19170486000001));
#164516=CARTESIAN_POINT('Ctrl Pts',(5.62706475599994,15.2,-9.18919724500002));
#164517=CARTESIAN_POINT('Ctrl Pts',(5.62706475599994,11.6,-9.18919724500002));
#164518=CARTESIAN_POINT('Ctrl Pts',(5.62638976199994,15.2,-9.18669600400002));
#164519=CARTESIAN_POINT('Ctrl Pts',(5.62638976199994,11.6,-9.18669600400002));
#164520=CARTESIAN_POINT('Ctrl Pts',(5.62571420699994,15.2,-9.18420114600002));
#164521=CARTESIAN_POINT('Ctrl Pts',(5.62571420699994,11.6,-9.18420114600002));
#164522=CARTESIAN_POINT('Ctrl Pts',(5.62503810399994,15.2,-9.18171268000001));
#164523=CARTESIAN_POINT('Ctrl Pts',(5.62503810399994,11.6,-9.18171268000001));
#164524=CARTESIAN_POINT('Ctrl Pts',(5.62436146299994,15.2,-9.17923061400002));
#164525=CARTESIAN_POINT('Ctrl Pts',(5.62436146299994,11.6,-9.17923061400002));
#164526=CARTESIAN_POINT('Ctrl Pts',(5.62368429599994,15.2,-9.17675495600001));
#164527=CARTESIAN_POINT('Ctrl Pts',(5.62368429599994,11.6,-9.17675495600001));
#164528=CARTESIAN_POINT('Ctrl Pts',(5.62300661499994,15.2,-9.17428571700002));
#164529=CARTESIAN_POINT('Ctrl Pts',(5.62300661499994,11.6,-9.17428571700002));
#164530=CARTESIAN_POINT('Ctrl Pts',(5.62232843199994,15.2,-9.17182290400002));
#164531=CARTESIAN_POINT('Ctrl Pts',(5.62232843199994,11.6,-9.17182290400002));
#164532=CARTESIAN_POINT('Ctrl Pts',(5.62164975999995,15.2,-9.16936652700001));
#164533=CARTESIAN_POINT('Ctrl Pts',(5.62164975999995,11.6,-9.16936652700001));
#164534=CARTESIAN_POINT('Ctrl Pts',(5.62097060899994,15.2,-9.16691659500002));
#164535=CARTESIAN_POINT('Ctrl Pts',(5.62097060899994,11.6,-9.16691659500002));
#164536=CARTESIAN_POINT('Ctrl Pts',(5.62029099199994,15.2,-9.16447311600002));
#164537=CARTESIAN_POINT('Ctrl Pts',(5.62029099199994,11.6,-9.16447311600002));
#164538=CARTESIAN_POINT('Ctrl Pts',(5.61961091999994,15.2,-9.16203609900002));
#164539=CARTESIAN_POINT('Ctrl Pts',(5.61961091999994,11.6,-9.16203609900002));
#164540=CARTESIAN_POINT('Ctrl Pts',(5.61893040599994,15.2,-9.15960555200002));
#164541=CARTESIAN_POINT('Ctrl Pts',(5.61893040599994,11.6,-9.15960555200002));
#164542=CARTESIAN_POINT('Ctrl Pts',(5.61824946299994,15.2,-9.15718148600002));
#164543=CARTESIAN_POINT('Ctrl Pts',(5.61824946299994,11.6,-9.15718148600002));
#164544=CARTESIAN_POINT('Ctrl Pts',(5.61756810099994,15.2,-9.15476390900002));
#164545=CARTESIAN_POINT('Ctrl Pts',(5.61756810099994,11.6,-9.15476390900002));
#164546=CARTESIAN_POINT('Ctrl Pts',(5.61688633399994,15.2,-9.15235283000002));
#164547=CARTESIAN_POINT('Ctrl Pts',(5.61688633399994,11.6,-9.15235283000002));
#164548=CARTESIAN_POINT('Ctrl Pts',(5.61620417199994,15.2,-9.14994825800001));
#164549=CARTESIAN_POINT('Ctrl Pts',(5.61620417199994,11.6,-9.14994825800001));
#164550=CARTESIAN_POINT('Ctrl Pts',(5.61552162899994,15.2,-9.14755020100002));
#164551=CARTESIAN_POINT('Ctrl Pts',(5.61552162899994,11.6,-9.14755020100002));
#164552=CARTESIAN_POINT('Ctrl Pts',(5.61483871699994,15.2,-9.14515867000001));
#164553=CARTESIAN_POINT('Ctrl Pts',(5.61483871699994,11.6,-9.14515867000001));
#164554=CARTESIAN_POINT('Ctrl Pts',(5.61415544799994,15.2,-9.14277367100001));
#164555=CARTESIAN_POINT('Ctrl Pts',(5.61415544799994,11.6,-9.14277367100001));
#164556=CARTESIAN_POINT('Ctrl Pts',(5.61347183399994,15.2,-9.14039521600002));
#164557=CARTESIAN_POINT('Ctrl Pts',(5.61347183399994,11.6,-9.14039521600002));
#164558=CARTESIAN_POINT('Ctrl Pts',(5.61278788899994,15.2,-9.13802331300002));
#164559=CARTESIAN_POINT('Ctrl Pts',(5.61278788899994,11.6,-9.13802331300002));
#164560=CARTESIAN_POINT('Ctrl Pts',(5.61210362299994,15.2,-9.13565797100001));
#164561=CARTESIAN_POINT('Ctrl Pts',(5.61210362299994,11.6,-9.13565797100001));
#164562=CARTESIAN_POINT('Ctrl Pts',(5.61141904999994,15.2,-9.13329919800002));
#164563=CARTESIAN_POINT('Ctrl Pts',(5.61141904999994,11.6,-9.13329919800002));
#164564=CARTESIAN_POINT('Ctrl Pts',(5.61073418199994,15.2,-9.13094700500002));
#164565=CARTESIAN_POINT('Ctrl Pts',(5.61073418199994,11.6,-9.13094700500002));
#164566=CARTESIAN_POINT('Ctrl Pts',(5.61004903199994,15.2,-9.12860140000002));
#164567=CARTESIAN_POINT('Ctrl Pts',(5.61004903199994,11.6,-9.12860140000002));
#164568=CARTESIAN_POINT('Ctrl Pts',(5.60936361399994,15.2,-9.12626239100002));
#164569=CARTESIAN_POINT('Ctrl Pts',(5.60936361399994,11.6,-9.12626239100002));
#164570=CARTESIAN_POINT('Ctrl Pts',(5.60867793699994,15.2,-9.12392999000001));
#164571=CARTESIAN_POINT('Ctrl Pts',(5.60867793699994,11.6,-9.12392999000001));
#164572=CARTESIAN_POINT('Ctrl Pts',(5.60799201599995,15.2,-9.12160420400001));
#164573=CARTESIAN_POINT('Ctrl Pts',(5.60799201599995,11.6,-9.12160420400001));
#164574=CARTESIAN_POINT('Ctrl Pts',(5.60730586399995,15.2,-9.11928504400001));
#164575=CARTESIAN_POINT('Ctrl Pts',(5.60730586399995,11.6,-9.11928504400001));
#164576=CARTESIAN_POINT('Ctrl Pts',(5.60661949299995,15.2,-9.11697251700001));
#164577=CARTESIAN_POINT('Ctrl Pts',(5.60661949299995,11.6,-9.11697251700001));
#164578=CARTESIAN_POINT('Ctrl Pts',(5.60593291599995,15.2,-9.11466663300001));
#164579=CARTESIAN_POINT('Ctrl Pts',(5.60593291599995,11.6,-9.11466663300001));
#164580=CARTESIAN_POINT('Ctrl Pts',(5.60524614599994,15.2,-9.11236740200002));
#164581=CARTESIAN_POINT('Ctrl Pts',(5.60524614599994,11.6,-9.11236740200002));
#164582=CARTESIAN_POINT('Ctrl Pts',(5.60455919499995,15.2,-9.11007483200001));
#164583=CARTESIAN_POINT('Ctrl Pts',(5.60455919499995,11.6,-9.11007483200001));
#164584=CARTESIAN_POINT('Ctrl Pts',(5.60387207799995,15.2,-9.10778893300002));
#164585=CARTESIAN_POINT('Ctrl Pts',(5.60387207799995,11.6,-9.10778893300002));
#164586=CARTESIAN_POINT('Ctrl Pts',(5.60318480499994,15.2,-9.10550971500001));
#164587=CARTESIAN_POINT('Ctrl Pts',(5.60318480499994,11.6,-9.10550971500001));
#164588=CARTESIAN_POINT('Ctrl Pts',(5.60249739199995,15.2,-9.10323718600001));
#164589=CARTESIAN_POINT('Ctrl Pts',(5.60249739199995,11.6,-9.10323718600001));
#164590=CARTESIAN_POINT('Ctrl Pts',(5.60180984999994,15.2,-9.10097135500001));
#164591=CARTESIAN_POINT('Ctrl Pts',(5.60180984999994,11.6,-9.10097135500001));
#164592=CARTESIAN_POINT('Ctrl Pts',(5.60112219399994,15.2,-9.09871223400001));
#164593=CARTESIAN_POINT('Ctrl Pts',(5.60112219399994,11.6,-9.09871223400001));
#164594=CARTESIAN_POINT('Ctrl Pts',(5.60043443499994,15.2,-9.09645983000001));
#164595=CARTESIAN_POINT('Ctrl Pts',(5.60043443499994,11.6,-9.09645983000001));
#164596=CARTESIAN_POINT('Ctrl Pts',(5.59974658699995,15.2,-9.09421415200002));
#164597=CARTESIAN_POINT('Ctrl Pts',(5.59974658699995,11.6,-9.09421415200002));
#164598=CARTESIAN_POINT('Ctrl Pts',(5.59905866399995,15.2,-9.09197521100002));
#164599=CARTESIAN_POINT('Ctrl Pts',(5.59905866399995,11.6,-9.09197521100002));
#164600=CARTESIAN_POINT('Ctrl Pts',(5.59837067799994,15.2,-9.08974301600002));
#164601=CARTESIAN_POINT('Ctrl Pts',(5.59837067799994,11.6,-9.08974301600002));
#164602=CARTESIAN_POINT('Ctrl Pts',(5.59768264499994,15.2,-9.08751757600001));
#164603=CARTESIAN_POINT('Ctrl Pts',(5.59768264499994,11.6,-9.08751757600001));
#164604=CARTESIAN_POINT('Ctrl Pts',(5.59699457499995,15.2,-9.08529890000001));
#164605=CARTESIAN_POINT('Ctrl Pts',(5.59699457499995,11.6,-9.08529890000001));
#164606=CARTESIAN_POINT('Ctrl Pts',(5.59630648299994,15.2,-9.08308699800001));
#164607=CARTESIAN_POINT('Ctrl Pts',(5.59630648299994,11.6,-9.08308699800001));
#164608=CARTESIAN_POINT('Ctrl Pts',(5.59561838299994,15.2,-9.08088187900002));
#164609=CARTESIAN_POINT('Ctrl Pts',(5.59561838299994,11.6,-9.08088187900002));
#164610=CARTESIAN_POINT('Ctrl Pts',(5.59493028699994,15.2,-9.07868355500002));
#164611=CARTESIAN_POINT('Ctrl Pts',(5.59493028699994,11.6,-9.07868355500002));
#164612=CARTESIAN_POINT('Ctrl Pts',(5.59424220999994,15.2,-9.07649203200002));
#164613=CARTESIAN_POINT('Ctrl Pts',(5.59424220999994,11.6,-9.07649203200002));
#164614=CARTESIAN_POINT('Ctrl Pts',(5.59355416599995,15.2,-9.07430732100002));
#164615=CARTESIAN_POINT('Ctrl Pts',(5.59355416599995,11.6,-9.07430732100002));
#164616=CARTESIAN_POINT('Ctrl Pts',(5.59286616599994,15.2,-9.07212943200001));
#164617=CARTESIAN_POINT('Ctrl Pts',(5.59286616599994,11.6,-9.07212943200001));
#164618=CARTESIAN_POINT('Ctrl Pts',(5.59217822699994,15.2,-9.06995837400002));
#164619=CARTESIAN_POINT('Ctrl Pts',(5.59217822699994,11.6,-9.06995837400002));
#164620=CARTESIAN_POINT('Ctrl Pts',(5.59149036099994,15.2,-9.06779415800001));
#164621=CARTESIAN_POINT('Ctrl Pts',(5.59149036099994,11.6,-9.06779415800001));
#164622=CARTESIAN_POINT('Ctrl Pts',(5.59080258099995,15.2,-9.06563679100002));
#164623=CARTESIAN_POINT('Ctrl Pts',(5.59080258099995,11.6,-9.06563679100002));
#164624=CARTESIAN_POINT('Ctrl Pts',(5.59011490299994,15.2,-9.06348628400002));
#164625=CARTESIAN_POINT('Ctrl Pts',(5.59011490299994,11.6,-9.06348628400002));
#164626=CARTESIAN_POINT('Ctrl Pts',(5.58942733899994,15.2,-9.06134264800002));
#164627=CARTESIAN_POINT('Ctrl Pts',(5.58942733899994,11.6,-9.06134264800002));
#164628=CARTESIAN_POINT('Ctrl Pts',(5.58873990499994,15.2,-9.05920589100001));
#164629=CARTESIAN_POINT('Ctrl Pts',(5.58873990499994,11.6,-9.05920589100001));
#164630=CARTESIAN_POINT('Ctrl Pts',(5.58805261299995,15.2,-9.05707602300001));
#164631=CARTESIAN_POINT('Ctrl Pts',(5.58805261299995,11.6,-9.05707602300001));
#164632=CARTESIAN_POINT('Ctrl Pts',(5.58736547799994,15.2,-9.05495305400001));
#164633=CARTESIAN_POINT('Ctrl Pts',(5.58736547799994,11.6,-9.05495305400001));
#164634=CARTESIAN_POINT('Ctrl Pts',(5.58667851399995,15.2,-9.05283699300002));
#164635=CARTESIAN_POINT('Ctrl Pts',(5.58667851399995,11.6,-9.05283699300002));
#164636=CARTESIAN_POINT('Ctrl Pts',(5.58599173399994,15.2,-9.05072785100002));
#164637=CARTESIAN_POINT('Ctrl Pts',(5.58599173399994,11.6,-9.05072785100002));
#164638=CARTESIAN_POINT('Ctrl Pts',(5.58530515499994,15.2,-9.04862563700001));
#164639=CARTESIAN_POINT('Ctrl Pts',(5.58530515499994,11.6,-9.04862563700001));
#164640=CARTESIAN_POINT('Ctrl Pts',(5.58461878799994,15.2,-9.04653036000001));
#164641=CARTESIAN_POINT('Ctrl Pts',(5.58461878799994,11.6,-9.04653036000001));
#164642=CARTESIAN_POINT('Ctrl Pts',(5.58393265099995,15.2,-9.04444203100002));
#164643=CARTESIAN_POINT('Ctrl Pts',(5.58393265099995,11.6,-9.04444203100002));
#164644=CARTESIAN_POINT('Ctrl Pts',(5.58324675399994,15.2,-9.04236066000001));
#164645=CARTESIAN_POINT('Ctrl Pts',(5.58324675399994,11.6,-9.04236066000001));
#164646=CARTESIAN_POINT('Ctrl Pts',(5.58256111399994,15.2,-9.04028625700001));
#164647=CARTESIAN_POINT('Ctrl Pts',(5.58256111399994,11.6,-9.04028625700001));
#164648=CARTESIAN_POINT('Ctrl Pts',(5.58187574599994,15.2,-9.03821883000001));
#164649=CARTESIAN_POINT('Ctrl Pts',(5.58187574599994,11.6,-9.03821883000001));
#164650=CARTESIAN_POINT('Ctrl Pts',(5.58119066299994,15.2,-9.03615839100001));
#164651=CARTESIAN_POINT('Ctrl Pts',(5.58119066299994,11.6,-9.03615839100001));
#164652=CARTESIAN_POINT('Ctrl Pts',(5.58050587999994,15.2,-9.03410495000001));
#164653=CARTESIAN_POINT('Ctrl Pts',(5.58050587999994,11.6,-9.03410495000001));
#164654=CARTESIAN_POINT('Ctrl Pts',(5.57982141099994,15.2,-9.03205851500001));
#164655=CARTESIAN_POINT('Ctrl Pts',(5.57982141099994,11.6,-9.03205851500001));
#164656=CARTESIAN_POINT('Ctrl Pts',(5.57913727299994,15.2,-9.03001909700002));
#164657=CARTESIAN_POINT('Ctrl Pts',(5.57913727299994,11.6,-9.03001909700002));
#164658=CARTESIAN_POINT('Ctrl Pts',(5.57845347799995,15.2,-9.02798670600001));
#164659=CARTESIAN_POINT('Ctrl Pts',(5.57845347799995,11.6,-9.02798670600001));
#164660=CARTESIAN_POINT('Ctrl Pts',(5.57777004199995,15.2,-9.02596135200002));
#164661=CARTESIAN_POINT('Ctrl Pts',(5.57777004199995,11.6,-9.02596135200002));
#164662=CARTESIAN_POINT('Ctrl Pts',(5.57708697999994,15.2,-9.02394304600002));
#164663=CARTESIAN_POINT('Ctrl Pts',(5.57708697999994,11.6,-9.02394304600002));
#164664=CARTESIAN_POINT('Ctrl Pts',(5.57640430699994,15.2,-9.02193179800001));
#164665=CARTESIAN_POINT('Ctrl Pts',(5.57640430699994,11.6,-9.02193179800001));
#164666=CARTESIAN_POINT('Ctrl Pts',(5.57572203699994,15.2,-9.01992761500002));
#164667=CARTESIAN_POINT('Ctrl Pts',(5.57572203699994,11.6,-9.01992761500002));
#164668=CARTESIAN_POINT('Ctrl Pts',(5.57504018499994,15.2,-9.01793051000002));
#164669=CARTESIAN_POINT('Ctrl Pts',(5.57504018499994,11.6,-9.01793051000002));
#164670=CARTESIAN_POINT('Ctrl Pts',(5.57435876799994,15.2,-9.01594049300002));
#164671=CARTESIAN_POINT('Ctrl Pts',(5.57435876799994,11.6,-9.01594049300002));
#164672=CARTESIAN_POINT('Ctrl Pts',(5.57367779799995,15.2,-9.01395757400002));
#164673=CARTESIAN_POINT('Ctrl Pts',(5.57367779799995,11.6,-9.01395757400002));
#164674=CARTESIAN_POINT('Ctrl Pts',(5.57299729299994,15.2,-9.01198176200002));
#164675=CARTESIAN_POINT('Ctrl Pts',(5.57299729299994,11.6,-9.01198176200002));
#164676=CARTESIAN_POINT('Ctrl Pts',(5.57231726599994,15.2,-9.01001306800002));
#164677=CARTESIAN_POINT('Ctrl Pts',(5.57231726599994,11.6,-9.01001306800002));
#164678=CARTESIAN_POINT('Ctrl Pts',(5.57163773399994,15.2,-9.00805150300002));
#164679=CARTESIAN_POINT('Ctrl Pts',(5.57163773399994,11.6,-9.00805150300002));
#164680=CARTESIAN_POINT('Ctrl Pts',(5.57095871099994,15.2,-9.00609707600001));
#164681=CARTESIAN_POINT('Ctrl Pts',(5.57095871099994,11.6,-9.00609707600001));
#164682=CARTESIAN_POINT('Ctrl Pts',(5.57028021399995,15.2,-9.00414979800002));
#164683=CARTESIAN_POINT('Ctrl Pts',(5.57028021399995,11.6,-9.00414979800002));
#164684=CARTESIAN_POINT('Ctrl Pts',(5.56960225599994,15.2,-9.00220967900001));
#164685=CARTESIAN_POINT('Ctrl Pts',(5.56960225599994,11.6,-9.00220967900001));
#164686=CARTESIAN_POINT('Ctrl Pts',(5.56892485499994,15.2,-9.00027672900002));
#164687=CARTESIAN_POINT('Ctrl Pts',(5.56892485499994,11.6,-9.00027672900002));
#164688=CARTESIAN_POINT('Ctrl Pts',(5.56824802499994,15.2,-8.99835095900002));
#164689=CARTESIAN_POINT('Ctrl Pts',(5.56824802499994,11.6,-8.99835095900002));
#164690=CARTESIAN_POINT('Ctrl Pts',(5.56757178199994,15.2,-8.99643237900002));
#164691=CARTESIAN_POINT('Ctrl Pts',(5.56757178199994,11.6,-8.99643237900002));
#164692=CARTESIAN_POINT('Ctrl Pts',(5.56689614199994,15.2,-8.99452099900002));
#164693=CARTESIAN_POINT('Ctrl Pts',(5.56689614199994,11.6,-8.99452099900002));
#164694=CARTESIAN_POINT('Ctrl Pts',(5.56622111999994,15.2,-8.99261683100002));
#164695=CARTESIAN_POINT('Ctrl Pts',(5.56622111999994,11.6,-8.99261683100002));
#164696=CARTESIAN_POINT('Ctrl Pts',(5.56554673199994,15.2,-8.99071988300001));
#164697=CARTESIAN_POINT('Ctrl Pts',(5.56554673199994,11.6,-8.99071988300001));
#164698=CARTESIAN_POINT('Ctrl Pts',(5.56487299499994,15.2,-8.98883016700001));
#164699=CARTESIAN_POINT('Ctrl Pts',(5.56487299499994,11.6,-8.98883016700001));
#164700=CARTESIAN_POINT('Ctrl Pts',(5.56419992299994,15.2,-8.98694769400001));
#164701=CARTESIAN_POINT('Ctrl Pts',(5.56419992299994,11.6,-8.98694769400001));
#164702=CARTESIAN_POINT('Ctrl Pts',(5.56352753399994,15.2,-8.98507247300002));
#164703=CARTESIAN_POINT('Ctrl Pts',(5.56352753399994,11.6,-8.98507247300002));
#164704=CARTESIAN_POINT('Ctrl Pts',(5.56285584299995,15.2,-8.98320451500001));
#164705=CARTESIAN_POINT('Ctrl Pts',(5.56285584299995,11.6,-8.98320451500001));
#164706=CARTESIAN_POINT('Ctrl Pts',(5.56218486399994,15.2,-8.98134383100002));
#164707=CARTESIAN_POINT('Ctrl Pts',(5.56218486399994,11.6,-8.98134383100002));
#164708=CARTESIAN_POINT('Ctrl Pts',(5.56151461599995,15.2,-8.97949043200001));
#164709=CARTESIAN_POINT('Ctrl Pts',(5.56151461599995,11.6,-8.97949043200001));
#164710=CARTESIAN_POINT('Ctrl Pts',(5.56084511599994,15.2,-8.97764432800002));
#164711=CARTESIAN_POINT('Ctrl Pts',(5.56084511599994,11.6,-8.97764432800002));
#164712=CARTESIAN_POINT('Ctrl Pts',(5.56017637699994,15.2,-8.97580552900001));
#164713=CARTESIAN_POINT('Ctrl Pts',(5.56017637699994,11.6,-8.97580552900001));
#164714=CARTESIAN_POINT('Ctrl Pts',(5.55950841699994,15.2,-8.97397404700002));
#164715=CARTESIAN_POINT('Ctrl Pts',(5.55950841699994,11.6,-8.97397404700002));
#164716=CARTESIAN_POINT('Ctrl Pts',(5.55884125299994,15.2,-8.97214989100002));
#164717=CARTESIAN_POINT('Ctrl Pts',(5.55884125299994,11.6,-8.97214989100002));
#164718=CARTESIAN_POINT('Ctrl Pts',(5.55817490099995,15.2,-8.97033307400001));
#164719=CARTESIAN_POINT('Ctrl Pts',(5.55817490099995,11.6,-8.97033307400001));
#164720=CARTESIAN_POINT('Ctrl Pts',(5.55750937599995,15.2,-8.96852360500001));
#164721=CARTESIAN_POINT('Ctrl Pts',(5.55750937599995,11.6,-8.96852360500001));
#164722=CARTESIAN_POINT('Ctrl Pts',(5.55684469699995,15.2,-8.96672149500001));
#164723=CARTESIAN_POINT('Ctrl Pts',(5.55684469699995,11.6,-8.96672149500001));
#164724=CARTESIAN_POINT('Ctrl Pts',(5.55618087999994,15.2,-8.96492675500001));
#164725=CARTESIAN_POINT('Ctrl Pts',(5.55618087999994,11.6,-8.96492675500001));
#164726=CARTESIAN_POINT('Ctrl Pts',(5.55551793999995,15.2,-8.96313939600001));
#164727=CARTESIAN_POINT('Ctrl Pts',(5.55551793999995,11.6,-8.96313939600001));
#164728=CARTESIAN_POINT('Ctrl Pts',(5.55485589499994,15.2,-8.96135942900001));
#164729=CARTESIAN_POINT('Ctrl Pts',(5.55485589499994,11.6,-8.96135942900001));
#164730=CARTESIAN_POINT('Ctrl Pts',(5.55419476299994,15.2,-8.95958686400002));
#164731=CARTESIAN_POINT('Ctrl Pts',(5.55419476299994,11.6,-8.95958686400002));
#164732=CARTESIAN_POINT('Ctrl Pts',(5.55353455899994,15.2,-8.95782171400001));
#164733=CARTESIAN_POINT('Ctrl Pts',(5.55353455899994,11.6,-8.95782171400001));
#164734=CARTESIAN_POINT('Ctrl Pts',(5.55287530099994,15.2,-8.95606398600002));
#164735=CARTESIAN_POINT('Ctrl Pts',(5.55287530099994,11.6,-8.95606398600002));
#164736=CARTESIAN_POINT('Ctrl Pts',(5.55221700599994,15.2,-8.95431369500002));
#164737=CARTESIAN_POINT('Ctrl Pts',(5.55221700599994,11.6,-8.95431369500002));
#164738=CARTESIAN_POINT('Ctrl Pts',(5.55155968999995,15.2,-8.95257085100001));
#164739=CARTESIAN_POINT('Ctrl Pts',(5.55155968999995,11.6,-8.95257085100001));
#164740=CARTESIAN_POINT('Ctrl Pts',(5.55090337199994,15.2,-8.95083546300001));
#164741=CARTESIAN_POINT('Ctrl Pts',(5.55090337199994,11.6,-8.95083546300001));
#164742=CARTESIAN_POINT('Ctrl Pts',(5.55024806799994,15.2,-8.94910754400002));
#164743=CARTESIAN_POINT('Ctrl Pts',(5.55024806799994,11.6,-8.94910754400002));
#164744=CARTESIAN_POINT('Ctrl Pts',(5.54959379599994,15.2,-8.94738710500001));
#164745=CARTESIAN_POINT('Ctrl Pts',(5.54959379599994,11.6,-8.94738710500001));
#164746=CARTESIAN_POINT('Ctrl Pts',(5.54894057199995,15.2,-8.94567415600001));
#164747=CARTESIAN_POINT('Ctrl Pts',(5.54894057199995,11.6,-8.94567415600001));
#164748=CARTESIAN_POINT('Ctrl Pts',(5.54828841499994,15.2,-8.94396870900002));
#164749=CARTESIAN_POINT('Ctrl Pts',(5.54828841499994,11.6,-8.94396870900002));
#164750=CARTESIAN_POINT('Ctrl Pts',(5.54763734099994,15.2,-8.94227077600002));
#164751=CARTESIAN_POINT('Ctrl Pts',(5.54763734099994,11.6,-8.94227077600002));
#164752=CARTESIAN_POINT('Ctrl Pts',(5.54698736999995,15.2,-8.94058036600001));
#164753=CARTESIAN_POINT('Ctrl Pts',(5.54698736999995,11.6,-8.94058036600001));
#164754=CARTESIAN_POINT('Ctrl Pts',(5.54633851699994,15.2,-8.93889749100002));
#164755=CARTESIAN_POINT('Ctrl Pts',(5.54633851699994,11.6,-8.93889749100002));
#164756=CARTESIAN_POINT('Ctrl Pts',(5.54569080099995,15.2,-8.93722216300001));
#164757=CARTESIAN_POINT('Ctrl Pts',(5.54569080099995,11.6,-8.93722216300001));
#164758=CARTESIAN_POINT('Ctrl Pts',(5.54504424099994,15.2,-8.93555439300001));
#164759=CARTESIAN_POINT('Ctrl Pts',(5.54504424099994,11.6,-8.93555439300001));
#164760=CARTESIAN_POINT('Ctrl Pts',(5.54439885199995,15.2,-8.93389419200001));
#164761=CARTESIAN_POINT('Ctrl Pts',(5.54439885199995,11.6,-8.93389419200001));
#164762=CARTESIAN_POINT('Ctrl Pts',(5.54375465499994,15.2,-8.93224157200001));
#164763=CARTESIAN_POINT('Ctrl Pts',(5.54375465499994,11.6,-8.93224157200001));
#164764=CARTESIAN_POINT('Ctrl Pts',(5.54311166499994,15.2,-8.93059654400002));
#164765=CARTESIAN_POINT('Ctrl Pts',(5.54311166499994,11.6,-8.93059654400002));
#164766=CARTESIAN_POINT('Ctrl Pts',(5.54246990199994,15.2,-8.92895911900002));
#164767=CARTESIAN_POINT('Ctrl Pts',(5.54246990199994,11.6,-8.92895911900002));
#164768=CARTESIAN_POINT('Ctrl Pts',(5.54182938399994,15.2,-8.92732930800002));
#164769=CARTESIAN_POINT('Ctrl Pts',(5.54182938399994,11.6,-8.92732930800002));
#164770=CARTESIAN_POINT('Ctrl Pts',(5.54119012799994,15.2,-8.92570712500002));
#164771=CARTESIAN_POINT('Ctrl Pts',(5.54119012799994,11.6,-8.92570712500002));
#164772=CARTESIAN_POINT('Ctrl Pts',(5.54055215399995,15.2,-8.92409257800002));
#164773=CARTESIAN_POINT('Ctrl Pts',(5.54055215399995,11.6,-8.92409257800002));
#164774=CARTESIAN_POINT('Ctrl Pts',(5.53991547999994,15.2,-8.92248568200002));
#164775=CARTESIAN_POINT('Ctrl Pts',(5.53991547999994,11.6,-8.92248568200002));
#164776=CARTESIAN_POINT('Ctrl Pts',(5.53928012499994,15.2,-8.92088644500001));
#164777=CARTESIAN_POINT('Ctrl Pts',(5.53928012499994,11.6,-8.92088644500001));
#164778=CARTESIAN_POINT('Ctrl Pts',(5.53864610499994,15.2,-8.91929488200002));
#164779=CARTESIAN_POINT('Ctrl Pts',(5.53864610499994,11.6,-8.91929488200002));
#164780=CARTESIAN_POINT('Ctrl Pts',(5.53801344099995,15.2,-8.91771100200001));
#164781=CARTESIAN_POINT('Ctrl Pts',(5.53801344099995,11.6,-8.91771100200001));
#164782=CARTESIAN_POINT('Ctrl Pts',(5.53738214999995,15.2,-8.91613481900002));
#164783=CARTESIAN_POINT('Ctrl Pts',(5.53738214999995,11.6,-8.91613481900002));
#164784=CARTESIAN_POINT('Ctrl Pts',(5.53675225199994,15.2,-8.91456634100001));
#164785=CARTESIAN_POINT('Ctrl Pts',(5.53675225199994,11.6,-8.91456634100001));
#164786=CARTESIAN_POINT('Ctrl Pts',(5.53612376599995,15.2,-8.91300558400001));
#164787=CARTESIAN_POINT('Ctrl Pts',(5.53612376599995,11.6,-8.91300558400001));
#164788=CARTESIAN_POINT('Ctrl Pts',(5.53549670999995,15.2,-8.91145255800001));
#164789=CARTESIAN_POINT('Ctrl Pts',(5.53549670999995,11.6,-8.91145255800001));
#164790=CARTESIAN_POINT('Ctrl Pts',(5.53487110399995,15.2,-8.90990727500002));
#164791=CARTESIAN_POINT('Ctrl Pts',(5.53487110399995,11.6,-8.90990727500002));
#164792=CARTESIAN_POINT('Ctrl Pts',(5.53424696599994,15.2,-8.90836974500001));
#164793=CARTESIAN_POINT('Ctrl Pts',(5.53424696599994,11.6,-8.90836974500001));
#164794=CARTESIAN_POINT('Ctrl Pts',(5.53362431699994,15.2,-8.90683998300002));
#164795=CARTESIAN_POINT('Ctrl Pts',(5.53362431699994,11.6,-8.90683998300002));
#164796=CARTESIAN_POINT('Ctrl Pts',(5.53300317299994,15.2,-8.90531799900002));
#164797=CARTESIAN_POINT('Ctrl Pts',(5.53300317299994,11.6,-8.90531799900002));
#164798=CARTESIAN_POINT('Ctrl Pts',(5.53238355599994,15.2,-8.90380380500002));
#164799=CARTESIAN_POINT('Ctrl Pts',(5.53238355599994,11.6,-8.90380380500002));
#164800=CARTESIAN_POINT('Ctrl Pts',(5.53176548499994,15.2,-8.90229741300002));
#164801=CARTESIAN_POINT('Ctrl Pts',(5.53176548499994,11.6,-8.90229741300002));
#164802=CARTESIAN_POINT('Ctrl Pts',(5.53114897799994,15.2,-8.90079883600002));
#164803=CARTESIAN_POINT('Ctrl Pts',(5.53114897799994,11.6,-8.90079883600002));
#164804=CARTESIAN_POINT('Ctrl Pts',(5.53053405599995,15.2,-8.89930808400001));
#164805=CARTESIAN_POINT('Ctrl Pts',(5.53053405599995,11.6,-8.89930808400001));
#164806=CARTESIAN_POINT('Ctrl Pts',(5.52992073899994,15.2,-8.89782517100001));
#164807=CARTESIAN_POINT('Ctrl Pts',(5.52992073899994,11.6,-8.89782517100001));
#164808=CARTESIAN_POINT('Ctrl Pts',(5.52930904599994,15.2,-8.89635010900001));
#164809=CARTESIAN_POINT('Ctrl Pts',(5.52930904599994,11.6,-8.89635010900001));
#164810=CARTESIAN_POINT('Ctrl Pts',(5.52869899599994,15.2,-8.89488290900001));
#164811=CARTESIAN_POINT('Ctrl Pts',(5.52869899599994,11.6,-8.89488290900001));
#164812=CARTESIAN_POINT('Ctrl Pts',(5.52809060999994,15.2,-8.89342358300001));
#164813=CARTESIAN_POINT('Ctrl Pts',(5.52809060999994,11.6,-8.89342358300001));
#164814=CARTESIAN_POINT('Ctrl Pts',(5.52748390799994,15.2,-8.89197214500001));
#164815=CARTESIAN_POINT('Ctrl Pts',(5.52748390799994,11.6,-8.89197214500001));
#164816=CARTESIAN_POINT('Ctrl Pts',(5.52687890999994,15.2,-8.89052860700002));
#164817=CARTESIAN_POINT('Ctrl Pts',(5.52687890999994,11.6,-8.89052860700002));
#164818=CARTESIAN_POINT('Ctrl Pts',(5.52627563499994,15.2,-8.88909298000002));
#164819=CARTESIAN_POINT('Ctrl Pts',(5.52627563499994,11.6,-8.88909298000002));
#164820=CARTESIAN_POINT('Ctrl Pts',(5.52567410499995,15.2,-8.88766527600002));
#164821=CARTESIAN_POINT('Ctrl Pts',(5.52567410499995,11.6,-8.88766527600002));
#164822=CARTESIAN_POINT('Ctrl Pts',(5.52507433899994,15.2,-8.88624550900002));
#164823=CARTESIAN_POINT('Ctrl Pts',(5.52507433899994,11.6,-8.88624550900002));
#164824=CARTESIAN_POINT('Ctrl Pts',(5.52447635799994,15.2,-8.88483369000001));
#164825=CARTESIAN_POINT('Ctrl Pts',(5.52447635799994,11.6,-8.88483369000001));
#164826=CARTESIAN_POINT('Ctrl Pts',(5.52388018299995,15.2,-8.88342983300002));
#164827=CARTESIAN_POINT('Ctrl Pts',(5.52388018299995,11.6,-8.88342983300002));
#164828=CARTESIAN_POINT('Ctrl Pts',(5.52328583399994,15.2,-8.88203395000002));
#164829=CARTESIAN_POINT('Ctrl Pts',(5.52328583399994,11.6,-8.88203395000002));
#164830=CARTESIAN_POINT('Ctrl Pts',(5.52269333099994,15.2,-8.88064605200002));
#164831=CARTESIAN_POINT('Ctrl Pts',(5.52269333099994,11.6,-8.88064605200002));
#164832=CARTESIAN_POINT('Ctrl Pts',(5.52210269599994,15.2,-8.87926615300002));
#164833=CARTESIAN_POINT('Ctrl Pts',(5.52210269599994,11.6,-8.87926615300002));
#164834=CARTESIAN_POINT('Ctrl Pts',(5.52151394899995,15.2,-8.87789426600002));
#164835=CARTESIAN_POINT('Ctrl Pts',(5.52151394899995,11.6,-8.87789426600002));
#164836=CARTESIAN_POINT('Ctrl Pts',(5.52092711099994,15.2,-8.87653040200002));
#164837=CARTESIAN_POINT('Ctrl Pts',(5.52092711099994,11.6,-8.87653040200002));
#164838=CARTESIAN_POINT('Ctrl Pts',(5.52034220399994,15.2,-8.87517457500002));
#164839=CARTESIAN_POINT('Ctrl Pts',(5.52034220399994,11.6,-8.87517457500002));
#164840=CARTESIAN_POINT('Ctrl Pts',(5.51975924799994,15.2,-8.87382679700002));
#164841=CARTESIAN_POINT('Ctrl Pts',(5.51975924799994,11.6,-8.87382679700002));
#164842=CARTESIAN_POINT('Ctrl Pts',(5.51917826499994,15.2,-8.87248708200002));
#164843=CARTESIAN_POINT('Ctrl Pts',(5.51917826499994,11.6,-8.87248708200002));
#164844=CARTESIAN_POINT('Ctrl Pts',(5.51859927599994,15.2,-8.87115544200002));
#164845=CARTESIAN_POINT('Ctrl Pts',(5.51859927599994,11.6,-8.87115544200002));
#164846=CARTESIAN_POINT('Ctrl Pts',(5.51802230199995,15.2,-8.86983188900002));
#164847=CARTESIAN_POINT('Ctrl Pts',(5.51802230199995,11.6,-8.86983188900002));
#164848=CARTESIAN_POINT('Ctrl Pts',(5.51744736599994,15.2,-8.86851643800001));
#164849=CARTESIAN_POINT('Ctrl Pts',(5.51744736599994,11.6,-8.86851643800001));
#164850=CARTESIAN_POINT('Ctrl Pts',(5.51687448799995,15.2,-8.86720909900001));
#164851=CARTESIAN_POINT('Ctrl Pts',(5.51687448799995,11.6,-8.86720909900001));
#164852=CARTESIAN_POINT('Ctrl Pts',(5.51630369099994,15.2,-8.86590988700002));
#164853=CARTESIAN_POINT('Ctrl Pts',(5.51630369099994,11.6,-8.86590988700002));
#164854=CARTESIAN_POINT('Ctrl Pts',(5.51573499599994,15.2,-8.86461881500002));
#164855=CARTESIAN_POINT('Ctrl Pts',(5.51573499599994,11.6,-8.86461881500002));
#164856=CARTESIAN_POINT('Ctrl Pts',(5.51516842399995,15.2,-8.86333589600002));
#164857=CARTESIAN_POINT('Ctrl Pts',(5.51516842399995,11.6,-8.86333589600002));
#164858=CARTESIAN_POINT('Ctrl Pts',(5.51460399899995,15.2,-8.86206114100002));
#164859=CARTESIAN_POINT('Ctrl Pts',(5.51460399899995,11.6,-8.86206114100002));
#164860=CARTESIAN_POINT('Ctrl Pts',(5.51404174199994,15.2,-8.86079456700001));
#164861=CARTESIAN_POINT('Ctrl Pts',(5.51404174199994,11.6,-8.86079456700001));
#164862=CARTESIAN_POINT('Ctrl Pts',(5.51348167599994,15.2,-8.85953618500002));
#164863=CARTESIAN_POINT('Ctrl Pts',(5.51348167599994,11.6,-8.85953618500002));
#164864=CARTESIAN_POINT('Ctrl Pts',(5.51292382199994,15.2,-8.85828600700002));
#164865=CARTESIAN_POINT('Ctrl Pts',(5.51292382199994,11.6,-8.85828600700002));
#164866=CARTESIAN_POINT('Ctrl Pts',(5.51236820399994,15.2,-8.85704404900002));
#164867=CARTESIAN_POINT('Ctrl Pts',(5.51236820399994,11.6,-8.85704404900002));
#164868=CARTESIAN_POINT('Ctrl Pts',(5.51181484299994,15.2,-8.85581032200001));
#164869=CARTESIAN_POINT('Ctrl Pts',(5.51181484299994,11.6,-8.85581032200001));
#164870=CARTESIAN_POINT('Ctrl Pts',(5.51126376199995,15.2,-8.85458484100001));
#164871=CARTESIAN_POINT('Ctrl Pts',(5.51126376199995,11.6,-8.85458484100001));
#164872=CARTESIAN_POINT('Ctrl Pts',(5.51071498499994,15.2,-8.85336761800002));
#164873=CARTESIAN_POINT('Ctrl Pts',(5.51071498499994,11.6,-8.85336761800002));
#164874=CARTESIAN_POINT('Ctrl Pts',(5.51016853299994,15.2,-8.85215866800002));
#164875=CARTESIAN_POINT('Ctrl Pts',(5.51016853299994,11.6,-8.85215866800002));
#164876=CARTESIAN_POINT('Ctrl Pts',(5.50962442999994,15.2,-8.85095800400002));
#164877=CARTESIAN_POINT('Ctrl Pts',(5.50962442999994,11.6,-8.85095800400002));
#164878=CARTESIAN_POINT('Ctrl Pts',(5.50908269899995,15.2,-8.84976563800001));
#164879=CARTESIAN_POINT('Ctrl Pts',(5.50908269899995,11.6,-8.84976563800001));
#164880=CARTESIAN_POINT('Ctrl Pts',(5.50854336299994,15.2,-8.84858158600002));
#164881=CARTESIAN_POINT('Ctrl Pts',(5.50854336299994,11.6,-8.84858158600002));
#164882=CARTESIAN_POINT('Ctrl Pts',(5.50800644599994,15.2,-8.84740586100002));
#164883=CARTESIAN_POINT('Ctrl Pts',(5.50800644599994,11.6,-8.84740586100002));
#164884=CARTESIAN_POINT('Ctrl Pts',(5.50747196999994,15.2,-8.84623847500002));
#164885=CARTESIAN_POINT('Ctrl Pts',(5.50747196999994,11.6,-8.84623847500002));
#164886=CARTESIAN_POINT('Ctrl Pts',(5.50693995899994,15.2,-8.84507944500001));
#164887=CARTESIAN_POINT('Ctrl Pts',(5.50693995899994,11.6,-8.84507944500001));
#164888=CARTESIAN_POINT('Ctrl Pts',(5.50641043699994,15.2,-8.84392878200002));
#164889=CARTESIAN_POINT('Ctrl Pts',(5.50641043699994,11.6,-8.84392878200002));
#164890=CARTESIAN_POINT('Ctrl Pts',(5.50588342799994,15.2,-8.84278649900001));
#164891=CARTESIAN_POINT('Ctrl Pts',(5.50588342799994,11.6,-8.84278649900001));
#164892=CARTESIAN_POINT('Ctrl Pts',(5.50535895399995,15.2,-8.84165261300002));
#164893=CARTESIAN_POINT('Ctrl Pts',(5.50535895399995,11.6,-8.84165261300002));
#164894=CARTESIAN_POINT('Ctrl Pts',(5.50483704099994,15.2,-8.84052713600001));
#164895=CARTESIAN_POINT('Ctrl Pts',(5.50483704099994,11.6,-8.84052713600001));
#164896=CARTESIAN_POINT('Ctrl Pts',(5.50431771199994,15.2,-8.83941008400001));
#164897=CARTESIAN_POINT('Ctrl Pts',(5.50431771199994,11.6,-8.83941008400001));
#164898=CARTESIAN_POINT('Ctrl Pts',(5.50380099099995,15.2,-8.83830146800002));
#164899=CARTESIAN_POINT('Ctrl Pts',(5.50380099099995,11.6,-8.83830146800002));
#164900=CARTESIAN_POINT('Ctrl Pts',(5.50328690399994,15.2,-8.83720130400001));
#164901=CARTESIAN_POINT('Ctrl Pts',(5.50328690399994,11.6,-8.83720130400001));
#164902=CARTESIAN_POINT('Ctrl Pts',(5.50277547299994,15.2,-8.83610960600001));
#164903=CARTESIAN_POINT('Ctrl Pts',(5.50277547299994,11.6,-8.83610960600001));
#164904=CARTESIAN_POINT('Ctrl Pts',(5.50226672399994,15.2,-8.83502638900002));
#164905=CARTESIAN_POINT('Ctrl Pts',(5.50226672399994,11.6,-8.83502638900002));
#164906=CARTESIAN_POINT('Ctrl Pts',(5.50176068099995,15.2,-8.83395166600002));
#164907=CARTESIAN_POINT('Ctrl Pts',(5.50176068099995,11.6,-8.83395166600002));
#164908=CARTESIAN_POINT('Ctrl Pts',(5.50125736899994,15.2,-8.83288545100001));
#164909=CARTESIAN_POINT('Ctrl Pts',(5.50125736899994,11.6,-8.83288545100001));
#164910=CARTESIAN_POINT('Ctrl Pts',(5.50075681299995,15.2,-8.83182776000002));
#164911=CARTESIAN_POINT('Ctrl Pts',(5.50075681299995,11.6,-8.83182776000002));
#164912=CARTESIAN_POINT('Ctrl Pts',(5.50025903799994,15.2,-8.83077860500002));
#164913=CARTESIAN_POINT('Ctrl Pts',(5.50025903799994,11.6,-8.83077860500002));
#164914=CARTESIAN_POINT('Ctrl Pts',(5.49976406799994,15.2,-8.82973800300002));
#164915=CARTESIAN_POINT('Ctrl Pts',(5.49976406799994,11.6,-8.82973800300002));
#164916=CARTESIAN_POINT('Ctrl Pts',(5.49927192999994,15.2,-8.82870596800002));
#164917=CARTESIAN_POINT('Ctrl Pts',(5.49927192999994,11.6,-8.82870596800002));
#164918=CARTESIAN_POINT('Ctrl Pts',(5.49878264899994,15.2,-8.82768251300002));
#164919=CARTESIAN_POINT('Ctrl Pts',(5.49878264899994,11.6,-8.82768251300002));
#164920=CARTESIAN_POINT('Ctrl Pts',(5.49829624999994,15.2,-8.82666765400002));
#164921=CARTESIAN_POINT('Ctrl Pts',(5.49829624999994,11.6,-8.82666765400002));
#164922=CARTESIAN_POINT('Ctrl Pts',(5.49781275699995,15.2,-8.82566140400002));
#164923=CARTESIAN_POINT('Ctrl Pts',(5.49781275699995,11.6,-8.82566140400002));
#164924=CARTESIAN_POINT('Ctrl Pts',(5.49733219899994,15.2,-8.82466378100002));
#164925=CARTESIAN_POINT('Ctrl Pts',(5.49733219899994,11.6,-8.82466378100002));
#164926=CARTESIAN_POINT('Ctrl Pts',(5.49685459999994,15.2,-8.82367479800001));
#164927=CARTESIAN_POINT('Ctrl Pts',(5.49685459999994,11.6,-8.82367479800001));
#164928=CARTESIAN_POINT('Ctrl Pts',(5.49637998599994,15.2,-8.82269446900001));
#164929=CARTESIAN_POINT('Ctrl Pts',(5.49637998599994,11.6,-8.82269446900001));
#164930=CARTESIAN_POINT('Ctrl Pts',(5.49590838399994,15.2,-8.82172281000001));
#164931=CARTESIAN_POINT('Ctrl Pts',(5.49590838399994,11.6,-8.82172281000001));
#164932=CARTESIAN_POINT('Ctrl Pts',(5.49543981999994,15.2,-8.82075983600001));
#164933=CARTESIAN_POINT('Ctrl Pts',(5.49543981999994,11.6,-8.82075983600001));
#164934=CARTESIAN_POINT('Ctrl Pts',(5.49497431799994,15.2,-8.81980556200002));
#164935=CARTESIAN_POINT('Ctrl Pts',(5.49497431799994,11.6,-8.81980556200002));
#164936=CARTESIAN_POINT('Ctrl Pts',(5.49451190799994,15.2,-8.81886000300002));
#164937=CARTESIAN_POINT('Ctrl Pts',(5.49451190799994,11.6,-8.81886000300002));
#164938=CARTESIAN_POINT('Ctrl Pts',(5.49405261599994,15.2,-8.81792317300001));
#164939=CARTESIAN_POINT('Ctrl Pts',(5.49405261599994,11.6,-8.81792317300001));
#164940=CARTESIAN_POINT('Ctrl Pts',(5.49359646699994,15.2,-8.81699508900001));
#164941=CARTESIAN_POINT('Ctrl Pts',(5.49359646699994,11.6,-8.81699508900001));
#164942=CARTESIAN_POINT('Ctrl Pts',(5.49314348999994,15.2,-8.81607576600001));
#164943=CARTESIAN_POINT('Ctrl Pts',(5.49314348999994,11.6,-8.81607576600001));
#164944=CARTESIAN_POINT('Ctrl Pts',(5.49269370999994,15.2,-8.81516521800001));
#164945=CARTESIAN_POINT('Ctrl Pts',(5.49269370999994,11.6,-8.81516521800001));
#164946=CARTESIAN_POINT('Ctrl Pts',(5.49224715599994,15.2,-8.81426346200002));
#164947=CARTESIAN_POINT('Ctrl Pts',(5.49224715599994,11.6,-8.81426346200002));
#164948=CARTESIAN_POINT('Ctrl Pts',(5.49180385399994,15.2,-8.81337051400001));
#164949=CARTESIAN_POINT('Ctrl Pts',(5.49180385399994,11.6,-8.81337051400001));
#164950=CARTESIAN_POINT('Ctrl Pts',(5.49136383199994,15.2,-8.81248638700002));
#164951=CARTESIAN_POINT('Ctrl Pts',(5.49136383199994,11.6,-8.81248638700002));
#164952=CARTESIAN_POINT('Ctrl Pts',(5.49092711899994,15.2,-8.81161109800002));
#164953=CARTESIAN_POINT('Ctrl Pts',(5.49092711899994,11.6,-8.81161109800002));
#164954=CARTESIAN_POINT('Ctrl Pts',(5.49049374099994,15.2,-8.81074466400002));
#164955=CARTESIAN_POINT('Ctrl Pts',(5.49049374099994,11.6,-8.81074466400002));
#164956=CARTESIAN_POINT('Ctrl Pts',(5.49006372599994,15.2,-8.80988709800001));
#164957=CARTESIAN_POINT('Ctrl Pts',(5.49006372599994,11.6,-8.80988709800001));
#164958=CARTESIAN_POINT('Ctrl Pts',(5.48963710299994,15.2,-8.80903841800002));
#164959=CARTESIAN_POINT('Ctrl Pts',(5.48963710299994,11.6,-8.80903841800002));
#164960=CARTESIAN_POINT('Ctrl Pts',(5.48921389899995,15.2,-8.80819864000001));
#164961=CARTESIAN_POINT('Ctrl Pts',(5.48921389899995,11.6,-8.80819864000001));
#164962=CARTESIAN_POINT('Ctrl Pts',(5.48879414499994,15.2,-8.80736777800001));
#164963=CARTESIAN_POINT('Ctrl Pts',(5.48879414499994,11.6,-8.80736777800001));
#164964=CARTESIAN_POINT('Ctrl Pts',(5.48838026299994,15.2,-8.80655058300002));
#164965=CARTESIAN_POINT('Ctrl Pts',(5.48838026299994,11.6,-8.80655058300002));
#164966=CARTESIAN_POINT('Ctrl Pts',(5.48805240199994,15.2,-8.80590483000002));
#164967=CARTESIAN_POINT('Ctrl Pts',(5.48805240199994,11.6,-8.80590483000002));
#164968=CARTESIAN_POINT('Ctrl Pts',(5.48780866099994,15.2,-8.80542564300002));
#164969=CARTESIAN_POINT('Ctrl Pts',(5.48780866099994,11.6,-8.80542564300002));
#164970=CARTESIAN_POINT('Ctrl Pts',(5.48764764299994,15.2,-8.80510947800002));
#164971=CARTESIAN_POINT('Ctrl Pts',(5.48764764299994,11.6,-8.80510947800002));
#164972=CARTESIAN_POINT('Ctrl Pts',(5.48756847899995,15.2,-8.80495412800002));
#164973=CARTESIAN_POINT('Ctrl Pts',(5.48756847899995,11.6,-8.80495412800002));
#164974=CARTESIAN_POINT('',(5.48756847908246,12.2,-8.80495412746575));
#164975=CARTESIAN_POINT('',(5.48756847908246,15.2,-8.80495412746575));
#164976=CARTESIAN_POINT('',(5.48756847899995,12.2,-8.80495412700002));
#164977=CARTESIAN_POINT('Ctrl Pts',(5.75020264099994,12.2,-9.95917514500001));
#164978=CARTESIAN_POINT('Ctrl Pts',(5.74993549095141,12.2,-9.95536156930721));
#164979=CARTESIAN_POINT('Ctrl Pts',(5.74966449014381,12.2,-9.95155489458726));
#164980=CARTESIAN_POINT('Ctrl Pts',(5.74938964875891,12.2,-9.94775512191045));
#164981=CARTESIAN_POINT('Ctrl Pts',(5.74911480737401,12.2,-9.94395534923364));
#164982=CARTESIAN_POINT('Ctrl Pts',(5.748836121958,12.2,-9.94016247888491));
#164983=CARTESIAN_POINT('Ctrl Pts',(5.74855360478793,12.2,-9.93637652429085));
#164984=CARTESIAN_POINT('Ctrl Pts',(5.74817691519361,12.2,-9.93132858437359));
#164985=CARTESIAN_POINT('Ctrl Pts',(5.74779341201749,12.2,-9.92629293960405));
#164986=CARTESIAN_POINT('Ctrl Pts',(5.747403168218,12.2,-9.9212696688311));
#164987=CARTESIAN_POINT('Ctrl Pts',(5.74711048539497,12.2,-9.91750221609359));
#164988=CARTESIAN_POINT('Ctrl Pts',(5.7468140126724,12.2,-9.91374172466357));
#164989=CARTESIAN_POINT('Ctrl Pts',(5.74651378172497,12.2,-9.90998822975829));
#164990=CARTESIAN_POINT('Ctrl Pts',(5.74611347375871,12.2,-9.90498356943));
#164991=CARTESIAN_POINT('Ctrl Pts',(5.74570648514168,12.2,-9.89999134467815));
#164992=CARTESIAN_POINT('Ctrl Pts',(5.74529287317401,12.2,-9.89501162118579));
#164993=CARTESIAN_POINT('Ctrl Pts',(5.74498266422643,12.2,-9.89127682890576));
#164994=CARTESIAN_POINT('Ctrl Pts',(5.74466873069324,12.2,-9.88754906896338));
#164995=CARTESIAN_POINT('Ctrl Pts',(5.74435109968848,12.2,-9.8838283690385));
#164996=CARTESIAN_POINT('Ctrl Pts',(5.74403346868372,12.2,-9.88010766911362));
#164997=CARTESIAN_POINT('Ctrl Pts',(5.74371213961966,12.2,-9.87639403032744));
#164998=CARTESIAN_POINT('Ctrl Pts',(5.74338714271448,12.2,-9.87268748404606));
#164999=CARTESIAN_POINT('Ctrl Pts',(5.7430621458093,12.2,-9.86898093776469));
#165000=CARTESIAN_POINT('Ctrl Pts',(5.74273348185456,12.2,-9.86528148464913));
#165001=CARTESIAN_POINT('Ctrl Pts',(5.74240117749164,12.2,-9.86158915378329));
#165002=CARTESIAN_POINT('Ctrl Pts',(5.74206887312871,12.2,-9.85789682291745));
#165003=CARTESIAN_POINT('Ctrl Pts',(5.74173293017427,12.2,-9.85421161373463));
#165004=CARTESIAN_POINT('Ctrl Pts',(5.74139337527026,12.2,-9.85053355740933));
#165005=CARTESIAN_POINT('Ctrl Pts',(5.74105382036624,12.2,-9.84685550108403));
#165006=CARTESIAN_POINT('Ctrl Pts',(5.74071065452133,12.2,-9.84318459710962));
#165007=CARTESIAN_POINT('Ctrl Pts',(5.74036390605869,12.2,-9.83952087472554));
#165008=CARTESIAN_POINT('Ctrl Pts',(5.74001715759605,12.2,-9.83585715234146));
#165009=CARTESIAN_POINT('Ctrl Pts',(5.73966682674711,12.2,-9.83220061396391));
#165010=CARTESIAN_POINT('Ctrl Pts',(5.73931294284378,12.2,-9.82855128680386));
#165011=CARTESIAN_POINT('Ctrl Pts',(5.73895905887616,12.2,-9.82490195898085));
#165012=CARTESIAN_POINT('Ctrl Pts',(5.73860162262422,12.2,-9.82125984485151));
#165013=CARTESIAN_POINT('Ctrl Pts',(5.73824066165461,12.2,-9.81762497344923));
#165014=CARTESIAN_POINT('Ctrl Pts',(5.73787970075058,12.2,-9.81399010270727));
#165015=CARTESIAN_POINT('Ctrl Pts',(5.73751521619673,12.2,-9.81036247540663));
#165016=CARTESIAN_POINT('Ctrl Pts',(5.73714723725147,12.2,-9.80674212208046));
#165017=CARTESIAN_POINT('Ctrl Pts',(5.73677925830621,12.2,-9.8031217687543));
#165018=CARTESIAN_POINT('Ctrl Pts',(5.73640778463773,12.2,-9.79950868903204));
#165019=CARTESIAN_POINT('Ctrl Pts',(5.73603284673296,12.2,-9.79590291327169));
#165020=CARTESIAN_POINT('Ctrl Pts',(5.73565790882819,12.2,-9.79229713751133));
#165021=CARTESIAN_POINT('Ctrl Pts',(5.73527950715483,12.2,-9.7886986664391));
#165022=CARTESIAN_POINT('Ctrl Pts',(5.73489767029198,12.2,-9.78510752971989));
#165023=CARTESIAN_POINT('Ctrl Pts',(5.73451583342913,12.2,-9.78151639300068));
#165024=CARTESIAN_POINT('Ctrl Pts',(5.73413056262785,12.2,-9.77793259222727));
#165025=CARTESIAN_POINT('Ctrl Pts',(5.73374188676728,12.2,-9.77435615689825));
#165026=CARTESIAN_POINT('Ctrl Pts',(5.73322365223943,12.2,-9.76958757602641));
#165027=CARTESIAN_POINT('Ctrl Pts',(5.73269936597196,12.2,-9.76483208952835));
#165028=CARTESIAN_POINT('Ctrl Pts',(5.7321691006649,12.2,-9.76008977010407));
#165029=CARTESIAN_POINT('Ctrl Pts',(5.73177140172072,12.2,-9.75653303085893));
#165030=CARTESIAN_POINT('Ctrl Pts',(5.73137033871861,12.2,-9.75298369825459));
#165031=CARTESIAN_POINT('Ctrl Pts',(5.7309659437333,12.2,-9.74944180396662));
#165032=CARTESIAN_POINT('Ctrl Pts',(5.73056154874799,12.2,-9.74589990967865));
#165033=CARTESIAN_POINT('Ctrl Pts',(5.7301538203795,12.2,-9.74236545357371));
#165034=CARTESIAN_POINT('Ctrl Pts',(5.72974279001971,12.2,-9.73883846536786));
#165035=CARTESIAN_POINT('Ctrl Pts',(5.72933175965994,12.2,-9.73531147716201));
#165036=CARTESIAN_POINT('Ctrl Pts',(5.72891742873604,12.2,-9.73179195886157));
#165037=CARTESIAN_POINT('Ctrl Pts',(5.72849982685573,12.2,-9.72827993989619));
#165038=CARTESIAN_POINT('Ctrl Pts',(5.72808222497542,12.2,-9.7247679209308));
#165039=CARTESIAN_POINT('Ctrl Pts',(5.72766135342657,12.2,-9.72126340180294));
#165040=CARTESIAN_POINT('Ctrl Pts',(5.72723724210909,12.2,-9.71776641401231));
#165041=CARTESIAN_POINT('Ctrl Pts',(5.72681313071456,12.2,-9.71426942558641));
#165042=CARTESIAN_POINT('Ctrl Pts',(5.72638578060245,12.2,-9.71077996896257));
#165043=CARTESIAN_POINT('Ctrl Pts',(5.72595522362277,12.2,-9.70729807449925));
#165044=CARTESIAN_POINT('Ctrl Pts',(5.72552466672131,12.2,-9.70381618066846));
#165045=CARTESIAN_POINT('Ctrl Pts',(5.72509090265336,12.2,-9.70034184847893));
#165046=CARTESIAN_POINT('Ctrl Pts',(5.72465396371062,12.2,-9.69687511114721));
#165047=CARTESIAN_POINT('Ctrl Pts',(5.72421702476789,12.2,-9.6934083738155));
#165048=CARTESIAN_POINT('Ctrl Pts',(5.72377691046882,12.2,-9.68994923025373));
#165049=CARTESIAN_POINT('Ctrl Pts',(5.72333365402456,12.2,-9.6864977119885));
#165050=CARTESIAN_POINT('Ctrl Pts',(5.72289039758031,12.2,-9.68304619372326));
#165051=CARTESIAN_POINT('Ctrl Pts',(5.7224439979194,12.2,-9.67960230077719));
#165052=CARTESIAN_POINT('Ctrl Pts',(5.72199448851704,12.2,-9.67616606546975));
#165053=CARTESIAN_POINT('Ctrl Pts',(5.72154497911468,12.2,-9.67272983016231));
#165054=CARTESIAN_POINT('Ctrl Pts',(5.72109235938276,12.2,-9.66930125219935));
#165055=CARTESIAN_POINT('Ctrl Pts',(5.72063666206625,12.2,-9.66588036286464));
#165056=CARTESIAN_POINT('Ctrl Pts',(5.72018096474975,12.2,-9.66245947352993));
#165057=CARTESIAN_POINT('Ctrl Pts',(5.71972219096677,12.2,-9.65904627233633));
#165058=CARTESIAN_POINT('Ctrl Pts',(5.71926037260897,12.2,-9.6556407925007));
#165059=CARTESIAN_POINT('Ctrl Pts',(5.71879855416727,12.2,-9.6522353120464));
#165060=CARTESIAN_POINT('Ctrl Pts',(5.7183336908497,12.2,-9.64883755190257));
#165061=CARTESIAN_POINT('Ctrl Pts',(5.71786581736463,12.2,-9.64544754449428));
#165062=CARTESIAN_POINT('Ctrl Pts',(5.71739794396455,12.2,-9.64205753770183));
#165063=CARTESIAN_POINT('Ctrl Pts',(5.71692705951506,12.2,-9.63867528334222));
#165064=CARTESIAN_POINT('Ctrl Pts',(5.71645319767492,12.2,-9.63530081383882));
#165065=CARTESIAN_POINT('Ctrl Pts',(5.71597933583479,12.2,-9.63192634433543));
#165066=CARTESIAN_POINT('Ctrl Pts',(5.71550249743045,12.2,-9.62855965891125));
#165067=CARTESIAN_POINT('Ctrl Pts',(5.71502271465595,12.2,-9.62520079061731));
#165068=CARTESIAN_POINT('Ctrl Pts',(5.71454293188147,12.2,-9.62184192232337));
#165069=CARTESIAN_POINT('Ctrl Pts',(5.71406020613232,12.2,-9.61849087154515));
#165070=CARTESIAN_POINT('Ctrl Pts',(5.7135745712333,12.2,-9.61514766879162));
#165071=CARTESIAN_POINT('Ctrl Pts',(5.71308893633428,12.2,-9.61180446603809));
#165072=CARTESIAN_POINT('Ctrl Pts',(5.71260039151871,12.2,-9.60846911215924));
#165073=CARTESIAN_POINT('Ctrl Pts',(5.71210897303681,12.2,-9.60514163986278));
#165074=CARTESIAN_POINT('Ctrl Pts',(5.71161755455492,12.2,-9.60181416756632));
#165075=CARTESIAN_POINT('Ctrl Pts',(5.71112326031923,12.2,-9.59849457665347));
#165076=CARTESIAN_POINT('Ctrl Pts',(5.71062612639612,12.2,-9.59518289919077));
#165077=CARTESIAN_POINT('Ctrl Pts',(5.71012899247301,12.2,-9.59187122172807));
#165078=CARTESIAN_POINT('Ctrl Pts',(5.70962901765759,12.2,-9.58856745801645));
#165079=CARTESIAN_POINT('Ctrl Pts',(5.7091262388429,12.2,-9.58527164076012));
#165080=CARTESIAN_POINT('Ctrl Pts',(5.7084558670291,12.2,-9.58087721735253));
#165081=CARTESIAN_POINT('Ctrl Pts',(5.70778050840926,12.2,-9.57649692019346));
#165082=CARTESIAN_POINT('Ctrl Pts',(5.7071002464833,12.2,-9.57213082739995));
#165083=CARTESIAN_POINT('Ctrl Pts',(5.70641998455734,12.2,-9.56776473460644));
#165084=CARTESIAN_POINT('Ctrl Pts',(5.70573481950302,12.2,-9.56341284618682));
#165085=CARTESIAN_POINT('Ctrl Pts',(5.70504483635381,12.2,-9.55907523950742));
#165086=CARTESIAN_POINT('Ctrl Pts',(5.70418235755832,12.2,-9.55365323204467));
#165087=CARTESIAN_POINT('Ctrl Pts',(5.70331234901849,12.2,-9.54825353962462));
#165088=CARTESIAN_POINT('Ctrl Pts',(5.70243498015639,12.2,-9.54287631694498));
#165089=CARTESIAN_POINT('Ctrl Pts',(5.70173308495194,12.2,-9.53857453809792));
#165090=CARTESIAN_POINT('Ctrl Pts',(5.70102647892484,12.2,-9.53428713773839));
#165091=CARTESIAN_POINT('Ctrl Pts',(5.70031524727496,12.2,-9.53001419628329));
#165092=CARTESIAN_POINT('Ctrl Pts',(5.69960401562509,12.2,-9.52574125482819));
#165093=CARTESIAN_POINT('Ctrl Pts',(5.69888816083579,12.2,-9.521482772297));
#165094=CARTESIAN_POINT('Ctrl Pts',(5.69816776840717,12.2,-9.51723882628941));
#165095=CARTESIAN_POINT('Ctrl Pts',(5.69744737607672,12.2,-9.51299488086007));
#165096=CARTESIAN_POINT('Ctrl Pts',(5.69672244777469,12.2,-9.50876547254694));
#165097=CARTESIAN_POINT('Ctrl Pts',(5.69599307077546,12.2,-9.50455068226116));
#165098=CARTESIAN_POINT('Ctrl Pts',(5.69526369367684,12.2,-9.50033589140112));
#165099=CARTESIAN_POINT('Ctrl Pts',(5.69452986885327,12.2,-9.49613571580055));
#165100=CARTESIAN_POINT('Ctrl Pts',(5.6937916858126,12.2,-9.49195023707397));
#165101=CARTESIAN_POINT('Ctrl Pts',(5.6930535028725,12.2,-9.48776475891764));
#165102=CARTESIAN_POINT('Ctrl Pts',(5.69231096271908,12.2,-9.48359397742607));
#165103=CARTESIAN_POINT('Ctrl Pts',(5.69156415383597,12.2,-9.47943797259818));
#165104=CARTESIAN_POINT('Ctrl Pts',(5.69081734485111,12.2,-9.47528196720405));
#165105=CARTESIAN_POINT('Ctrl Pts',(5.69006626980294,12.2,-9.47114073837547));
#165106=CARTESIAN_POINT('Ctrl Pts',(5.68931101739035,12.2,-9.46701436616794));
#165107=CARTESIAN_POINT('Ctrl Pts',(5.68855576508067,12.2,-9.46288799452263));
#165108=CARTESIAN_POINT('Ctrl Pts',(5.68779633758298,12.2,-9.45877648133163));
#165109=CARTESIAN_POINT('Ctrl Pts',(5.68703282731234,12.2,-9.45467990461));
#165110=CARTESIAN_POINT('Ctrl Pts',(5.68626931693766,12.2,-9.45058332733022));
#165111=CARTESIAN_POINT('Ctrl Pts',(5.68550172393193,12.2,-9.44650168901607));
#165112=CARTESIAN_POINT('Ctrl Pts',(5.68473014094518,12.2,-9.44243506968432));
#165113=CARTESIAN_POINT('Ctrl Pts',(5.68395855806355,12.2,-9.43836845090665));
#165114=CARTESIAN_POINT('Ctrl Pts',(5.68318298680181,12.2,-9.43431685210317));
#165115=CARTESIAN_POINT('Ctrl Pts',(5.68240352110471,12.2,-9.4302803531191));
#165116=CARTESIAN_POINT('Ctrl Pts',(5.68142918890369,12.2,-9.42523472897653));
#165117=CARTESIAN_POINT('Ctrl Pts',(5.68044877128079,12.2,-9.4202127011227));
#165118=CARTESIAN_POINT('Ctrl Pts',(5.6794624575311,12.2,-9.41521442959366));
#165119=CARTESIAN_POINT('Ctrl Pts',(5.67867340648834,12.2,-9.41121581215252));
#165120=CARTESIAN_POINT('Ctrl Pts',(5.67788058069513,12.2,-9.40723239801877));
#165121=CARTESIAN_POINT('Ctrl Pts',(5.67708407898481,12.2,-9.40326427069237));
#165122=CARTESIAN_POINT('Ctrl Pts',(5.67628757738301,12.2,-9.39929614390663));
#165123=CARTESIAN_POINT('Ctrl Pts',(5.6754873989153,12.2,-9.39534330348174));
#165124=CARTESIAN_POINT('Ctrl Pts',(5.67468364264804,12.2,-9.39140583263541));
#165125=CARTESIAN_POINT('Ctrl Pts',(5.67387988627127,12.2,-9.38746836125259));
#165126=CARTESIAN_POINT('Ctrl Pts',(5.67307255126396,12.2,-9.38354625975568));
#165127=CARTESIAN_POINT('Ctrl Pts',(5.67226173821607,12.2,-9.37963961174729));
#165128=CARTESIAN_POINT('Ctrl Pts',(5.67145092527866,12.2,-9.37573296427118));
#165129=CARTESIAN_POINT('Ctrl Pts',(5.67063663376646,12.2,-9.37184176999892));
#165130=CARTESIAN_POINT('Ctrl Pts',(5.66981896483365,12.2,-9.36796611259197));
#165131=CARTESIAN_POINT('Ctrl Pts',(5.66900129578943,12.2,-9.36409045465695));
#165132=CARTESIAN_POINT('Ctrl Pts',(5.66818025001711,12.2,-9.36023033455114));
#165133=CARTESIAN_POINT('Ctrl Pts',(5.66735592774996,12.2,-9.35638583650828));
#165134=CARTESIAN_POINT('Ctrl Pts',(5.66653160548281,12.2,-9.35254133846543));
#165135=CARTESIAN_POINT('Ctrl Pts',(5.66570400652639,12.2,-9.34871246181329));
#165136=CARTESIAN_POINT('Ctrl Pts',(5.66487323681413,12.2,-9.34489929188485));
#165137=CARTESIAN_POINT('Ctrl Pts',(5.66404246721504,12.2,-9.34108612247595));
#165138=CARTESIAN_POINT('Ctrl Pts',(5.66320852447201,12.2,-9.33728866048565));
#165139=CARTESIAN_POINT('Ctrl Pts',(5.66237151425886,12.2,-9.33350699027752));
#165140=CARTESIAN_POINT('Ctrl Pts',(5.66153450393166,12.2,-9.32972531955415));
#165141=CARTESIAN_POINT('Ctrl Pts',(5.66069442466114,12.2,-9.32595944014791));
#165142=CARTESIAN_POINT('Ctrl Pts',(5.65985138433712,12.2,-9.32220944011183));
#165143=CARTESIAN_POINT('Ctrl Pts',(5.65900834412796,12.2,-9.31845944058668));
#165144=CARTESIAN_POINT('Ctrl Pts',(5.65816234087474,12.2,-9.31472531863448));
#165145=CARTESIAN_POINT('Ctrl Pts',(5.65731348277766,12.2,-9.31100716127073));
#165146=CARTESIAN_POINT('Ctrl Pts',(5.65646462456492,12.2,-9.30728900340038));
#165147=CARTESIAN_POINT('Ctrl Pts',(5.65561291168768,12.2,-9.30358681077383));
#165148=CARTESIAN_POINT('Ctrl Pts',(5.65475845137595,12.2,-9.29990066922349));
#165149=CARTESIAN_POINT('Ctrl Pts',(5.65390399118066,12.2,-9.29621452817539));
#165150=CARTESIAN_POINT('Ctrl Pts',(5.65304678436365,12.2,-9.29254443822894));
#165151=CARTESIAN_POINT('Ctrl Pts',(5.65218693904522,12.2,-9.28889048808215));
#165152=CARTESIAN_POINT('Ctrl Pts',(5.65132709360964,12.2,-9.2852365374375));
#165153=CARTESIAN_POINT('Ctrl Pts',(5.65046461205152,12.2,-9.28159872526146));
#165154=CARTESIAN_POINT('Ctrl Pts',(5.64959960317088,12.2,-9.27797713995404));
#165155=CARTESIAN_POINT('Ctrl Pts',(5.64873459440811,12.2,-9.27435555514005));
#165156=CARTESIAN_POINT('Ctrl Pts',(5.64786705917053,12.2,-9.27075019752202));
#165157=CARTESIAN_POINT('Ctrl Pts',(5.64699710964284,12.2,-9.26716115524584));
#165158=CARTESIAN_POINT('Ctrl Pts',(5.64612715999663,12.2,-9.26357211248064));
#165159=CARTESIAN_POINT('Ctrl Pts',(5.6452547946818,12.2,-9.25999938506602));
#165160=CARTESIAN_POINT('Ctrl Pts',(5.64438013041176,12.2,-9.25644306248437));
#165161=CARTESIAN_POINT('Ctrl Pts',(5.64350546626089,12.2,-9.25288674038728));
#165162=CARTESIAN_POINT('Ctrl Pts',(5.64262850091326,12.2,-9.24934682233412));
#165163=CARTESIAN_POINT('Ctrl Pts',(5.64174935015203,12.2,-9.24582339884272));
#165164=CARTESIAN_POINT('Ctrl Pts',(5.64087019927102,12.2,-9.24229997487124));
#165165=CARTESIAN_POINT('Ctrl Pts',(5.63998886083485,12.2,-9.23879304451469));
#165166=CARTESIAN_POINT('Ctrl Pts',(5.63910545578269,12.2,-9.23530269919758));
#165167=CARTESIAN_POINT('Ctrl Pts',(5.63822205085089,12.2,-9.23181235435604));
#165168=CARTESIAN_POINT('Ctrl Pts',(5.63733657501396,12.2,-9.22833859259261));
#165169=CARTESIAN_POINT('Ctrl Pts',(5.63644914892005,12.2,-9.22488150704019));
#165170=CARTESIAN_POINT('Ctrl Pts',(5.63556172270521,12.2,-9.22142442101673));
#165171=CARTESIAN_POINT('Ctrl Pts',(5.63467234446241,12.2,-9.2179840087782));
#165172=CARTESIAN_POINT('Ctrl Pts',(5.63378113502495,12.2,-9.21456036475828));
#165173=CARTESIAN_POINT('Ctrl Pts',(5.63288992558749,12.2,-9.21113672073835));
#165174=CARTESIAN_POINT('Ctrl Pts',(5.63199688446648,12.2,-9.20772984107595));
#165175=CARTESIAN_POINT('Ctrl Pts',(5.63110213236199,12.2,-9.20433982117068));
#165176=CARTESIAN_POINT('Ctrl Pts',(5.63020738037941,12.2,-9.20094980172732));
#165177=CARTESIAN_POINT('Ctrl Pts',(5.62931091711177,12.2,-9.19757664075982));
#165178=CARTESIAN_POINT('Ctrl Pts',(5.62841286579223,12.2,-9.1942204300189));
#165179=CARTESIAN_POINT('Ctrl Pts',(5.62751481435033,12.2,-9.1908642188207));
#165180=CARTESIAN_POINT('Ctrl Pts',(5.62661517393243,12.2,-9.18752495868332));
#165181=CARTESIAN_POINT('Ctrl Pts',(5.62571406982762,12.2,-9.18420274344844));
#165182=CARTESIAN_POINT('Ctrl Pts',(5.62481296584558,12.2,-9.18088052866621));
#165183=CARTESIAN_POINT('Ctrl Pts',(5.62391039745263,12.2,-9.17757535724846));
#165184=CARTESIAN_POINT('Ctrl Pts',(5.62300648958216,12.2,-9.1742873237939));
#165185=CARTESIAN_POINT('Ctrl Pts',(5.62210258158854,12.2,-9.17099928989134));
#165186=CARTESIAN_POINT('Ctrl Pts',(5.62119733622986,12.2,-9.16772839441348));
#165187=CARTESIAN_POINT('Ctrl Pts',(5.62029087813507,12.2,-9.16447473101957));
#165188=CARTESIAN_POINT('Ctrl Pts',(5.6193844201638,12.2,-9.16122106806898));
#165189=CARTESIAN_POINT('Ctrl Pts',(5.61847675104986,12.2,-9.15798463650121));
#165190=CARTESIAN_POINT('Ctrl Pts',(5.6175679997909,12.2,-9.15476553376329));
#165191=CARTESIAN_POINT('Ctrl Pts',(5.61643206062433,12.2,-9.15074165501192));
#165192=CARTESIAN_POINT('Ctrl Pts',(5.61529442920214,12.2,-9.14674485083891));
#165193=CARTESIAN_POINT('Ctrl Pts',(5.6141553618411,12.2,-9.14277530722639));
#165194=CARTESIAN_POINT('Ctrl Pts',(5.61301629448007,12.2,-9.13880576361387));
#165195=CARTESIAN_POINT('Ctrl Pts',(5.61187579130575,12.2,-9.13486348257548));
#165196=CARTESIAN_POINT('Ctrl Pts',(5.6107341115089,12.2,-9.13094865200209));
#165197=CARTESIAN_POINT('Ctrl Pts',(5.60959243171206,12.2,-9.12703382142869));
#165198=CARTESIAN_POINT('Ctrl Pts',(5.60844957668883,12.2,-9.12314644026103));
#165199=CARTESIAN_POINT('Ctrl Pts',(5.60730580925828,12.2,-9.11928670227493));
#165200=CARTESIAN_POINT('Ctrl Pts',(5.60616204182773,12.2,-9.11542696428883));
#165201=CARTESIAN_POINT('Ctrl Pts',(5.60501736224439,12.2,-9.11159486614996));
#165202=CARTESIAN_POINT('Ctrl Pts',(5.60387203904995,12.2,-9.10779060323329));
#165203=CARTESIAN_POINT('Ctrl Pts',(5.60272671585551,12.2,-9.10398634031662));
#165204=CARTESIAN_POINT('Ctrl Pts',(5.60158074997676,12.2,-9.10020991180933));
#165205=CARTESIAN_POINT('Ctrl Pts',(5.60043441274932,12.2,-9.09646151151457));
#165206=CARTESIAN_POINT('Ctrl Pts',(5.59928807552188,12.2,-9.09271311121981));
#165207=CARTESIAN_POINT('Ctrl Pts',(5.59814136906938,12.2,-9.08899274026274));
#165208=CARTESIAN_POINT('Ctrl Pts',(5.59699456941661,12.2,-9.08530059325031));
#165209=CARTESIAN_POINT('Ctrl Pts',(5.59584776976382,12.2,-9.0816084462379));
#165210=CARTESIAN_POINT('Ctrl Pts',(5.59470087836385,12.2,-9.07794452493311));
#165211=CARTESIAN_POINT('Ctrl Pts',(5.59355417697495,12.2,-9.07430902625401));
#165212=CARTESIAN_POINT('Ctrl Pts',(5.59240747558606,12.2,-9.0706735275749));
#165213=CARTESIAN_POINT('Ctrl Pts',(5.59126096451302,12.2,-9.067066452667));
#165214=CARTESIAN_POINT('Ctrl Pts',(5.59011493140024,12.2,-9.06348800130964));
#165215=CARTESIAN_POINT('Ctrl Pts',(5.58896889828746,12.2,-9.05990954995228));
#165216=CARTESIAN_POINT('Ctrl Pts',(5.58782334446681,12.2,-9.05635972338149));
#165217=CARTESIAN_POINT('Ctrl Pts',(5.58667855988354,12.2,-9.05283872227274));
#165218=CARTESIAN_POINT('Ctrl Pts',(5.58553377530027,12.2,-9.04931772116399));
#165219=CARTESIAN_POINT('Ctrl Pts',(5.58438976336147,12.2,-9.04582554527794));
#165220=CARTESIAN_POINT('Ctrl Pts',(5.58324681808378,12.2,-9.04236240153031));
#165221=CARTESIAN_POINT('Ctrl Pts',(5.58210387293066,12.2,-9.03889925816016));
#165222=CARTESIAN_POINT('Ctrl Pts',(5.58096199755268,12.2,-9.03546514535989));
#165223=CARTESIAN_POINT('Ctrl Pts',(5.57982149385745,12.2,-9.03206026968698));
#165224=CARTESIAN_POINT('Ctrl Pts',(5.5786809900379,12.2,-9.02865539364294));
#165225=CARTESIAN_POINT('Ctrl Pts',(5.57754185839329,12.2,-9.02527975585112));
#165226=CARTESIAN_POINT('Ctrl Pts',(5.57640440790705,12.2,-9.02193356473764));
#165227=CARTESIAN_POINT('Ctrl Pts',(5.57526695742081,12.2,-9.01858737362414));
#165228=CARTESIAN_POINT('Ctrl Pts',(5.574131187305,12.2,-9.01527062885344));
#165229=CARTESIAN_POINT('Ctrl Pts',(5.5729974126649,12.2,-9.01198354188163));
#165230=CARTESIAN_POINT('Ctrl Pts',(5.57186363802479,12.2,-9.00869645490982));
#165231=CARTESIAN_POINT('Ctrl Pts',(5.57073185890172,12.2,-9.00543902751277));
#165232=CARTESIAN_POINT('Ctrl Pts',(5.56960239529048,12.2,-9.00221147146953));
#165233=CARTESIAN_POINT('Ctrl Pts',(5.56847293167925,12.2,-8.99898391542628));
#165234=CARTESIAN_POINT('Ctrl Pts',(5.56734578462364,12.2,-8.99578623151997));
#165235=CARTESIAN_POINT('Ctrl Pts',(5.56622127858183,12.2,-8.99261863624062));
#165236=CARTESIAN_POINT('Ctrl Pts',(5.5648718713807,12.2,-8.98881752204349));
#165237=CARTESIAN_POINT('Ctrl Pts',(5.56352627083102,12.2,-8.98505973376448));
#165238=CARTESIAN_POINT('Ctrl Pts',(5.56218504687946,12.2,-8.98134565264645));
#165239=CARTESIAN_POINT('Ctrl Pts',(5.56084382280607,12.2,-8.97763157119106));
#165240=CARTESIAN_POINT('Ctrl Pts',(5.55950698194974,12.2,-8.97396119534822));
#165241=CARTESIAN_POINT('Ctrl Pts',(5.5581751077107,12.2,-8.97033491081915));
#165242=CARTESIAN_POINT('Ctrl Pts',(5.55684323359264,12.2,-8.96670862661947));
#165243=CARTESIAN_POINT('Ctrl Pts',(5.55551632823354,12.2,-8.9631264309225));
#165244=CARTESIAN_POINT('Ctrl Pts',(5.55419499502554,12.2,-8.95958871770155));
#165245=CARTESIAN_POINT('Ctrl Pts',(5.55287366181754,12.2,-8.9560510044806));
#165246=CARTESIAN_POINT('Ctrl Pts',(5.55155789924552,12.2,-8.95255777049525));
#165247=CARTESIAN_POINT('Ctrl Pts',(5.55024832612601,12.2,-8.94910941436748));
#165248=CARTESIAN_POINT('Ctrl Pts',(5.54893875288755,12.2,-8.9456610579265));
#165249=CARTESIAN_POINT('Ctrl Pts',(5.54763536709289,12.2,-8.94225757884833));
#165250=CARTESIAN_POINT('Ctrl Pts',(5.54633880112452,12.2,-8.93889937741686));
#165251=CARTESIAN_POINT('Ctrl Pts',(5.54504223527394,12.2,-8.93554117629043));
#165252=CARTESIAN_POINT('Ctrl Pts',(5.54375249127834,12.2,-8.93222825632291));
#165253=CARTESIAN_POINT('Ctrl Pts',(5.5424702132416,12.2,-8.92896102252493));
#165254=CARTESIAN_POINT('Ctrl Pts',(5.54097422212106,12.2,-8.92514924956277));
#165255=CARTESIAN_POINT('Ctrl Pts',(5.5394883948182,12.2,-8.92139966416064));
#165256=CARTESIAN_POINT('Ctrl Pts',(5.53801378415268,12.2,-8.91771292589435));
#165257=CARTESIAN_POINT('Ctrl Pts',(5.53674983221926,12.2,-8.91455286468728));
#165258=CARTESIAN_POINT('Ctrl Pts',(5.53549412207964,12.2,-8.91143897676351));
#165259=CARTESIAN_POINT('Ctrl Pts',(5.53424733820826,12.2,-8.90837168695826));
#165260=CARTESIAN_POINT('Ctrl Pts',(5.53300055433687,12.2,-8.90530439715301));
#165261=CARTESIAN_POINT('Ctrl Pts',(5.53176269308149,12.2,-8.90228370678589));
#165262=CARTESIAN_POINT('Ctrl Pts',(5.53053445737548,12.2,-8.89931004405742));
#165263=CARTESIAN_POINT('Ctrl Pts',(5.52930622155789,12.2,-8.89633638105884));
#165264=CARTESIAN_POINT('Ctrl Pts',(5.52808761036701,12.2,-8.89340974786119));
#165265=CARTESIAN_POINT('Ctrl Pts',(5.52687934065807,12.2,-8.89053058447987));
#165266=CARTESIAN_POINT('Ctrl Pts',(5.52567107105887,12.2,-8.88765142136008));
#165267=CARTESIAN_POINT('Ctrl Pts',(5.52447314397346,12.2,-8.88481972509045));
#165268=CARTESIAN_POINT('Ctrl Pts',(5.52328629551659,12.2,-8.88203594627492));
#165269=CARTESIAN_POINT('Ctrl Pts',(5.52190163891169,12.2,-8.87878820415491));
#165270=CARTESIAN_POINT('Ctrl Pts',(5.52053206005894,12.2,-8.87560567919259));
#165271=CARTESIAN_POINT('Ctrl Pts',(5.51917876338774,12.2,-8.87248910049163));
#165272=CARTESIAN_POINT('Ctrl Pts',(5.51801879487263,12.2,-8.86981774745804));
#165273=CARTESIAN_POINT('Ctrl Pts',(5.51687078998367,12.2,-8.86719484213975));
#165274=CARTESIAN_POINT('Ctrl Pts',(5.51573552677492,12.2,-8.86462085323326));
#165275=CARTESIAN_POINT('Ctrl Pts',(5.51460026356616,12.2,-8.86204686432676));
#165276=CARTESIAN_POINT('Ctrl Pts',(5.51347774372312,12.2,-8.8595217898928));
#165277=CARTESIAN_POINT('Ctrl Pts',(5.5123687683739,12.2,-8.85704610702288));
#165278=CARTESIAN_POINT('Ctrl Pts',(5.51125979292394,12.2,-8.85457042392808));
#165279=CARTESIAN_POINT('Ctrl Pts',(5.51016436078168,12.2,-8.85214413192536));
#165280=CARTESIAN_POINT('Ctrl Pts',(5.50908329764042,12.2,-8.84976771621591));
#165281=CARTESIAN_POINT('Ctrl Pts',(5.50800223459734,12.2,-8.84739130072232));
#165282=CARTESIAN_POINT('Ctrl Pts',(5.50693554074929,12.2,-8.84506476471805));
#165283=CARTESIAN_POINT('Ctrl Pts',(5.50588406178277,12.2,-8.84278859820723));
#165284=CARTESIAN_POINT('Ctrl Pts',(5.50483258281625,12.2,-8.8405124316964));
#165285=CARTESIAN_POINT('Ctrl Pts',(5.5037963193359,12.2,-8.83828663894189));
#165286=CARTESIAN_POINT('Ctrl Pts',(5.50277614353892,12.2,-8.83611172635201));
#165287=CARTESIAN_POINT('Ctrl Pts',(5.50175596764927,12.2,-8.83393681356456));
#165288=CARTESIAN_POINT('Ctrl Pts',(5.50075187959496,12.2,-8.83181277937513));
#165289=CARTESIAN_POINT('Ctrl Pts',(5.49976477587566,12.2,-8.82974014451569));
#165290=CARTESIAN_POINT('Ctrl Pts',(5.49877767224603,12.2,-8.82766750984452));
#165291=CARTESIAN_POINT('Ctrl Pts',(5.49780755475439,12.2,-8.82564627083567));
#165292=CARTESIAN_POINT('Ctrl Pts',(5.49685534620643,12.2,-8.82367696140948));
#165293=CARTESIAN_POINT('Ctrl Pts',(5.49590313765847,12.2,-8.82170765198329));
#165294=CARTESIAN_POINT('Ctrl Pts',(5.49496883830079,12.2,-8.81979027085299));
#165295=CARTESIAN_POINT('Ctrl Pts',(5.49405340183321,12.2,-8.81792535958511));
#165296=CARTESIAN_POINT('Ctrl Pts',(5.49313796536564,12.2,-8.81606044831723));
#165297=CARTESIAN_POINT('Ctrl Pts',(5.49224138970664,12.2,-8.81424800979806));
#165298=CARTESIAN_POINT('Ctrl Pts',(5.49136465932048,12.2,-8.81248859669171));
#165299=CARTESIAN_POINT('Ctrl Pts',(5.49005377132756,12.2,-8.80985792077118));
#165300=CARTESIAN_POINT('Ctrl Pts',(5.48878723733333,12.2,-8.8073457972827));
#165301=CARTESIAN_POINT('Ctrl Pts',(5.48756847899995,12.2,-8.80495412800002));
#165302=CARTESIAN_POINT('Ctrl Pts',(5.48756847899995,15.2,-8.80495412800002));
#165303=CARTESIAN_POINT('Ctrl Pts',(5.48837968052293,15.2,-8.80654601517849));
#165304=CARTESIAN_POINT('Ctrl Pts',(5.48921205180367,15.2,-8.8081912649178));
#165305=CARTESIAN_POINT('Ctrl Pts',(5.49006457388987,15.2,-8.80988931929729));
#165306=CARTESIAN_POINT('Ctrl Pts',(5.49092120726851,15.2,-8.81159556255332));
#165307=CARTESIAN_POINT('Ctrl Pts',(5.49179818705027,15.2,-8.81335511472471));
#165308=CARTESIAN_POINT('Ctrl Pts',(5.49269451656167,15.2,-8.81516741616703));
#165309=CARTESIAN_POINT('Ctrl Pts',(5.49359084599165,15.2,-8.81697971744475));
#165310=CARTESIAN_POINT('Ctrl Pts',(5.49450652408385,15.2,-8.81884476556958));
#165311=CARTESIAN_POINT('Ctrl Pts',(5.49544058554991,15.2,-8.82076201099992));
#165312=CARTESIAN_POINT('Ctrl Pts',(5.49637464701597,15.2,-8.82267925643024));
#165313=CARTESIAN_POINT('Ctrl Pts',(5.49732708885225,15.2,-8.82464869965497));
#165314=CARTESIAN_POINT('Ctrl Pts',(5.4982969764478,15.2,-8.82666980609621));
#165315=CARTESIAN_POINT('Ctrl Pts',(5.49926686413145,15.2,-8.82869091272103));
#165316=CARTESIAN_POINT('Ctrl Pts',(5.50025419422016,15.2,-8.83076367841218));
#165317=CARTESIAN_POINT('Ctrl Pts',(5.50125805810934,15.2,-8.83288758219811));
#165318=CARTESIAN_POINT('Ctrl Pts',(5.50226192190734,15.2,-8.83501148579112));
#165319=CARTESIAN_POINT('Ctrl Pts',(5.50328231821661,15.2,-8.83718652736323));
#165320=CARTESIAN_POINT('Ctrl Pts',(5.50431836401705,15.2,-8.8394121930426));
#165321=CARTESIAN_POINT('Ctrl Pts',(5.5053544098175,15.2,-8.84163785872197));
#165322=CARTESIAN_POINT('Ctrl Pts',(5.50640610323126,15.2,-8.84391415024339));
#165323=CARTESIAN_POINT('Ctrl Pts',(5.50747258619186,15.2,-8.84624056382335));
#165324=CARTESIAN_POINT('Ctrl Pts',(5.50853906924934,15.2,-8.84856697761463));
#165325=CARTESIAN_POINT('Ctrl Pts',(5.50962034108367,15.2,-8.85094351569548));
#165326=CARTESIAN_POINT('Ctrl Pts',(5.5107155663943,15.2,-8.85336968649773));
#165327=CARTESIAN_POINT('Ctrl Pts',(5.51181079160544,15.2,-8.85579585707959));
#165328=CARTESIAN_POINT('Ctrl Pts',(5.51291997050134,15.2,-8.85827166115236));
#165329=CARTESIAN_POINT('Ctrl Pts',(5.51404228979448,15.2,-8.86079661514608));
#165330=CARTESIAN_POINT('Ctrl Pts',(5.51553871555263,15.2,-8.86416322054752));
#165331=CARTESIAN_POINT('Ctrl Pts',(5.51705850066996,15.2,-8.86761720947481));
#165332=CARTESIAN_POINT('Ctrl Pts',(5.51859977976712,15.2,-8.87115746377614));
#165333=CARTESIAN_POINT('Ctrl Pts',(5.51975573906372,15.2,-8.87381265444185));
#165334=CARTESIAN_POINT('Ctrl Pts',(5.52092378940405,15.2,-8.87651637193557));
#165335=CARTESIAN_POINT('Ctrl Pts',(5.52210316794403,15.2,-8.87926815583349));
#165336=CARTESIAN_POINT('Ctrl Pts',(5.52328254659114,15.2,-8.88201993998135));
#165337=CARTESIAN_POINT('Ctrl Pts',(5.52447325341468,15.2,-8.88481979146023));
#165338=CARTESIAN_POINT('Ctrl Pts',(5.52567454614754,15.2,-8.88766726053533));
#165339=CARTESIAN_POINT('Ctrl Pts',(5.52687583877127,15.2,-8.89051472935179));
#165340=CARTESIAN_POINT('Ctrl Pts',(5.52808771721051,15.2,-8.89340981469033));
#165341=CARTESIAN_POINT('Ctrl Pts',(5.52930945683322,15.2,-8.89635207466882));
#165342=CARTESIAN_POINT('Ctrl Pts',(5.53053119645593,15.2,-8.89929433464731));
#165343=CARTESIAN_POINT('Ctrl Pts',(5.53176279711951,15.2,-8.90228377044705));
#165344=CARTESIAN_POINT('Ctrl Pts',(5.53300355465734,15.2,-8.90531994633465));
#165345=CARTESIAN_POINT('Ctrl Pts',(5.53424431230788,15.2,-8.90835612249804));
#165346=CARTESIAN_POINT('Ctrl Pts',(5.53549422414293,15.2,-8.911439038534));
#165347=CARTESIAN_POINT('Ctrl Pts',(5.53675260512876,15.2,-8.91456827154103));
#165348=CARTESIAN_POINT('Ctrl Pts',(5.53801098600029,15.2,-8.91769750426382));
#165349=CARTESIAN_POINT('Ctrl Pts',(5.53927783420707,15.2,-8.92087304989906));
#165350=CARTESIAN_POINT('Ctrl Pts',(5.54055247907776,15.2,-8.92409449086736));
#165351=CARTESIAN_POINT('Ctrl Pts',(5.54182712394848,15.2,-8.92731593183566));
#165352=CARTESIAN_POINT('Ctrl Pts',(5.54310956692685,15.2,-8.93058326810029));
#165353=CARTESIAN_POINT('Ctrl Pts',(5.54439914987968,15.2,-8.93389608706124));
#165354=CARTESIAN_POINT('Ctrl Pts',(5.5456887328325,15.2,-8.93720890602218));
#165355=CARTESIAN_POINT('Ctrl Pts',(5.54698545768903,15.2,-8.94056720898073));
#165356=CARTESIAN_POINT('Ctrl Pts',(5.54828868564122,15.2,-8.94397058710398));
#165357=CARTESIAN_POINT('Ctrl Pts',(5.54959191371179,15.2,-8.94737396553636));
#165358=CARTESIAN_POINT('Ctrl Pts',(5.55090164269138,15.2,-8.9508224233232));
#165359=CARTESIAN_POINT('Ctrl Pts',(5.55221725084666,15.2,-8.95431555693216));
#165360=CARTESIAN_POINT('Ctrl Pts',(5.55353285888243,15.2,-8.95780869022383));
#165361=CARTESIAN_POINT('Ctrl Pts',(5.55485434506653,15.2,-8.96134650319564));
#165362=CARTESIAN_POINT('Ctrl Pts',(5.55618109927433,15.2,-8.96492860024832));
#165363=CARTESIAN_POINT('Ctrl Pts',(5.55750785348214,15.2,-8.968510697301));
#165364=CARTESIAN_POINT('Ctrl Pts',(5.55883987556145,15.2,-8.97213707871123));
#165365=CARTESIAN_POINT('Ctrl Pts',(5.56017657159591,15.2,-8.97580735782489));
#165366=CARTESIAN_POINT('Ctrl Pts',(5.56151326775177,15.2,-8.97947763727193));
#165367=CARTESIAN_POINT('Ctrl Pts',(5.56285463546433,15.2,-8.98319181465183));
#165368=CARTESIAN_POINT('Ctrl Pts',(5.5642000938551,15.2,-8.98694950738022));
#165369=CARTESIAN_POINT('Ctrl Pts',(5.56532130911965,15.2,-8.99008091781654));
#165370=CARTESIAN_POINT('Ctrl Pts',(5.56644536587487,15.2,-8.99324254762608));
#165371=CARTESIAN_POINT('Ctrl Pts',(5.56757193288896,15.2,-8.99643417943408));
#165372=CARTESIAN_POINT('Ctrl Pts',(5.56869849990304,15.2,-8.99962581124207));
#165373=CARTESIAN_POINT('Ctrl Pts',(5.56982757803107,15.2,-9.0028474442895));
#165374=CARTESIAN_POINT('Ctrl Pts',(5.57095884261458,15.2,-9.0060988636669));
#165375=CARTESIAN_POINT('Ctrl Pts',(5.57209010707476,15.2,-9.00935028268989));
#165376=CARTESIAN_POINT('Ctrl Pts',(5.57322355935868,15.2,-9.01263148874131));
#165377=CARTESIAN_POINT('Ctrl Pts',(5.57435887965144,15.2,-9.01594226705857));
#165378=CARTESIAN_POINT('Ctrl Pts',(5.57549420006795,15.2,-9.0192530457367));
#165379=CARTESIAN_POINT('Ctrl Pts',(5.57663138910113,15.2,-9.02259339834494));
#165380=CARTESIAN_POINT('Ctrl Pts',(5.57777013535099,15.2,-9.02596311355086));
#165381=CARTESIAN_POINT('Ctrl Pts',(5.57890888160086,15.2,-9.02933282875677));
#165382=CARTESIAN_POINT('Ctrl Pts',(5.58004918481604,15.2,-9.03273190783283));
#165383=CARTESIAN_POINT('Ctrl Pts',(5.5811907378591,15.2,-9.03616014008542));
#165384=CARTESIAN_POINT('Ctrl Pts',(5.58233229090214,15.2,-9.039588372338));
#165385=CARTESIAN_POINT('Ctrl Pts',(5.58347509396963,15.2,-9.04304575989028));
#165386=CARTESIAN_POINT('Ctrl Pts',(5.58461884535848,15.2,-9.04653209676378));
#165387=CARTESIAN_POINT('Ctrl Pts',(5.58576259674732,15.2,-9.0500184336373));
#165388=CARTESIAN_POINT('Ctrl Pts',(5.58690729834731,15.2,-9.05353371799764));
#165389=CARTESIAN_POINT('Ctrl Pts',(5.58805265216671,15.2,-9.05707774751));
#165390=CARTESIAN_POINT('Ctrl Pts',(5.58919800598611,15.2,-9.06062177702235));
#165391=CARTESIAN_POINT('Ctrl Pts',(5.59034401286633,15.2,-9.06419455234836));
#165392=CARTESIAN_POINT('Ctrl Pts',(5.59149038252432,15.2,-9.06779587028132));
#165393=CARTESIAN_POINT('Ctrl Pts',(5.59263675218231,15.2,-9.07139718821428));
#165394=CARTESIAN_POINT('Ctrl Pts',(5.59378348292216,15.2,-9.07502705063882));
#165395=CARTESIAN_POINT('Ctrl Pts',(5.59493029174161,15.2,-9.0786852552916));
#165396=CARTESIAN_POINT('Ctrl Pts',(5.59607710056105,15.2,-9.08234345994438));
#165397=CARTESIAN_POINT('Ctrl Pts',(5.59722398550091,15.2,-9.08603001015168));
#165398=CARTESIAN_POINT('Ctrl Pts',(5.59837066620057,15.2,-9.08974470475198));
#165399=CARTESIAN_POINT('Ctrl Pts',(5.59951734690023,15.2,-9.09345939935228));
#165400=CARTESIAN_POINT('Ctrl Pts',(5.60066382501381,15.2,-9.0972022406897));
#165401=CARTESIAN_POINT('Ctrl Pts',(5.60180982154156,15.2,-9.10097303270505));
#165402=CARTESIAN_POINT('Ctrl Pts',(5.60295581806932,15.2,-9.10474382472042));
#165403=CARTESIAN_POINT('Ctrl Pts',(5.60410133522485,15.2,-9.10854256793226));
#165404=CARTESIAN_POINT('Ctrl Pts',(5.60524610084981,15.2,-9.11236906751703));
#165405=CARTESIAN_POINT('Ctrl Pts',(5.60661981954985,15.2,-9.11696086685194));
#165406=CARTESIAN_POINT('Ctrl Pts',(5.60799245627496,15.2,-9.12159263445863));
#165407=CARTESIAN_POINT('Ctrl Pts',(5.60936354922522,15.2,-9.12626404270386));
#165408=CARTESIAN_POINT('Ctrl Pts',(5.61050612672528,15.2,-9.13015688304965));
#165409=CARTESIAN_POINT('Ctrl Pts',(5.61164763461081,15.2,-9.1340772502355));
#165410=CARTESIAN_POINT('Ctrl Pts',(5.61278780878266,15.2,-9.13802495323947));
#165411=CARTESIAN_POINT('Ctrl Pts',(5.6139279829545,15.2,-9.14197265624343));
#165412=CARTESIAN_POINT('Ctrl Pts',(5.61506682437216,15.2,-9.14594769726104));
#165413=CARTESIAN_POINT('Ctrl Pts',(5.61620407673328,15.2,-9.14994988677494));
#165414=CARTESIAN_POINT('Ctrl Pts',(5.61711387867176,15.2,-9.15315163856056));
#165415=CARTESIAN_POINT('Ctrl Pts',(5.61802266210177,15.2,-9.15637076496482));
#165416=CARTESIAN_POINT('Ctrl Pts',(5.61893029887335,15.2,-9.15960717275411));
#165417=CARTESIAN_POINT('Ctrl Pts',(5.61983793552126,15.2,-9.16284358010244));
#165418=CARTESIAN_POINT('Ctrl Pts',(5.62074442628866,15.2,-9.16609726676974));
#165419=CARTESIAN_POINT('Ctrl Pts',(5.62164964027433,15.2,-9.16936813823939));
#165420=CARTESIAN_POINT('Ctrl Pts',(5.62255485438335,15.2,-9.17263901015471));
#165421=CARTESIAN_POINT('Ctrl Pts',(5.62345879426513,15.2,-9.1759270681057));
#165422=CARTESIAN_POINT('Ctrl Pts',(5.62436133164751,15.2,-9.17923221656534));
#165423=CARTESIAN_POINT('Ctrl Pts',(5.62526386890692,15.2,-9.18253736457467));
#165424=CARTESIAN_POINT('Ctrl Pts',(5.62616500398872,15.2,-9.18585960212066));
#165425=CARTESIAN_POINT('Ctrl Pts',(5.62706461269306,15.2,-9.18919883823546));
#165426=CARTESIAN_POINT('Ctrl Pts',(5.62796422151997,15.2,-9.19253807480525));
#165427=CARTESIAN_POINT('Ctrl Pts',(5.62886230363652,15.2,-9.19589430955233));
#165428=CARTESIAN_POINT('Ctrl Pts',(5.62975873639669,15.2,-9.1992674482395));
#165429=CARTESIAN_POINT('Ctrl Pts',(5.63065516903472,15.2,-9.20264058646709));
#165430=CARTESIAN_POINT('Ctrl Pts',(5.63154995122204,15.2,-9.20603062856788));
#165431=CARTESIAN_POINT('Ctrl Pts',(5.63244296192693,15.2,-9.20943748395493));
#165432=CARTESIAN_POINT('Ctrl Pts',(5.63333597275349,15.2,-9.21284433980616));
#165433=CARTESIAN_POINT('Ctrl Pts',(5.63422721194373,15.2,-9.21626800593721));
#165434=CARTESIAN_POINT('Ctrl Pts',(5.63511656004764,15.2,-9.2197083950147));
#165435=CARTESIAN_POINT('Ctrl Pts',(5.63600590803037,15.2,-9.22314878362344));
#165436=CARTESIAN_POINT('Ctrl Pts',(5.63689336363277,15.2,-9.22660589165509));
#165437=CARTESIAN_POINT('Ctrl Pts',(5.63777880960479,15.2,-9.23007963048765));
#165438=CARTESIAN_POINT('Ctrl Pts',(5.63866425569746,15.2,-9.23355336979351));
#165439=CARTESIAN_POINT('Ctrl Pts',(5.63954768970464,15.2,-9.23704373748347));
#165440=CARTESIAN_POINT('Ctrl Pts',(5.64042899836365,15.2,-9.2405506447868));
#165441=CARTESIAN_POINT('Ctrl Pts',(5.64131030690258,15.2,-9.24405755161229));
#165442=CARTESIAN_POINT('Ctrl Pts',(5.64218948594748,15.2,-9.24758099778171));
#165443=CARTESIAN_POINT('Ctrl Pts',(5.64306642259824,15.2,-9.25112089321286));
#165444=CARTESIAN_POINT('Ctrl Pts',(5.64394335936849,15.2,-9.25466078912631));
#165445=CARTESIAN_POINT('Ctrl Pts',(5.64481805183794,15.2,-9.25821713354139));
#165446=CARTESIAN_POINT('Ctrl Pts',(5.64569038800055,15.2,-9.26178983875239));
#165447=CARTESIAN_POINT('Ctrl Pts',(5.6465627240443,15.2,-9.2653625434766));
#165448=CARTESIAN_POINT('Ctrl Pts',(5.647432701751,15.2,-9.26895160764578));
#165449=CARTESIAN_POINT('Ctrl Pts',(5.64830020912478,15.2,-9.27255694312716));
#165450=CARTESIAN_POINT('Ctrl Pts',(5.64916771661676,15.2,-9.27616227909976));
#165451=CARTESIAN_POINT('Ctrl Pts',(5.6500327534974,15.2,-9.27978388704058));
#165452=CARTESIAN_POINT('Ctrl Pts',(5.65089520776662,15.2,-9.28342167701661));
#165453=CARTESIAN_POINT('Ctrl Pts',(5.65175766203585,15.2,-9.28705946699264));
#165454=CARTESIAN_POINT('Ctrl Pts',(5.65261753520755,15.2,-9.29071343906502));
#165455=CARTESIAN_POINT('Ctrl Pts',(5.6534747148651,15.2,-9.29438350760002));
#165456=CARTESIAN_POINT('Ctrl Pts',(5.65433189440586,15.2,-9.29805357563497));
#165457=CARTESIAN_POINT('Ctrl Pts',(5.65518638215678,15.2,-9.30173973875276));
#165458=CARTESIAN_POINT('Ctrl Pts',(5.65603806825771,15.2,-9.30544190952244));
#165459=CARTESIAN_POINT('Ctrl Pts',(5.65688975447467,15.2,-9.30914408079652));
#165460=CARTESIAN_POINT('Ctrl Pts',(5.65773863933691,15.2,-9.31286225991089));
#165461=CARTESIAN_POINT('Ctrl Pts',(5.65858461560494,15.2,-9.31659636056049));
#165462=CARTESIAN_POINT('Ctrl Pts',(5.6594305917577,15.2,-9.32033046070131));
#165463=CARTESIAN_POINT('Ctrl Pts',(5.66027365826084,15.2,-9.32408048162337));
#165464=CARTESIAN_POINT('Ctrl Pts',(5.66111371041459,15.2,-9.32784633842558));
#165465=CARTESIAN_POINT('Ctrl Pts',(5.66195376268279,15.2,-9.33161219574089));
#165466=CARTESIAN_POINT('Ctrl Pts',(5.66279079897299,15.2,-9.33539388832526));
#165467=CARTESIAN_POINT('Ctrl Pts',(5.66362471583761,15.2,-9.33919132983441));
#165468=CARTESIAN_POINT('Ctrl Pts',(5.6644586325886,15.2,-9.34298877082616));
#165469=CARTESIAN_POINT('Ctrl Pts',(5.66528942769695,15.2,-9.34680196139004));
#165470=CARTESIAN_POINT('Ctrl Pts',(5.66611699990727,15.2,-9.3506308161871));
#165471=CARTESIAN_POINT('Ctrl Pts',(5.66694457223036,15.2,-9.35445967150584));
#165472=CARTESIAN_POINT('Ctrl Pts',(5.66776891981696,15.2,-9.35830419055702));
#165473=CARTESIAN_POINT('Ctrl Pts',(5.66858994075038,15.2,-9.362164289824));
#165474=CARTESIAN_POINT('Ctrl Pts',(5.66941096157194,15.2,-9.36602438856505));
#165475=CARTESIAN_POINT('Ctrl Pts',(5.67022865635459,15.2,-9.36990006707155));
#165476=CARTESIAN_POINT('Ctrl Pts',(5.67104292260678,15.2,-9.37379124016874));
#165477=CARTESIAN_POINT('Ctrl Pts',(5.67185718896992,15.2,-9.37768241379611));
#165478=CARTESIAN_POINT('Ctrl Pts',(5.67266802737214,15.2,-9.38158908264483));
#165479=CARTESIAN_POINT('Ctrl Pts',(5.67347533708259,15.2,-9.38551116330407));
#165480=CARTESIAN_POINT('Ctrl Pts',(5.67428264668304,15.2,-9.38943324342893));
#165481=CARTESIAN_POINT('Ctrl Pts',(5.6750864278175,15.2,-9.39337073562006));
#165482=CARTESIAN_POINT('Ctrl Pts',(5.67588658141914,15.2,-9.39732355512869));
#165483=CARTESIAN_POINT('Ctrl Pts',(5.67668673512979,15.2,-9.4012763751759));
#165484=CARTESIAN_POINT('Ctrl Pts',(5.67748326098175,15.2,-9.40524452292172));
#165485=CARTESIAN_POINT('Ctrl Pts',(5.67827606252496,15.2,-9.40922791624995));
#165486=CARTESIAN_POINT('Ctrl Pts',(5.67906886406817,15.2,-9.41321130957817));
#165487=CARTESIAN_POINT('Ctrl Pts',(5.67985793877206,15.2,-9.41720994765537));
#165488=CARTESIAN_POINT('Ctrl Pts',(5.68064319187001,15.2,-9.42122374893122));
#165489=CARTESIAN_POINT('Ctrl Pts',(5.68142844486097,15.2,-9.42523754966019));
#165490=CARTESIAN_POINT('Ctrl Pts',(5.68220987585667,15.2,-9.42926651283173));
#165491=CARTESIAN_POINT('Ctrl Pts',(5.6829873887411,15.2,-9.43331055696387));
#165492=CARTESIAN_POINT('Ctrl Pts',(5.68376490173146,15.2,-9.43735460164701));
#165493=CARTESIAN_POINT('Ctrl Pts',(5.68453849650092,15.2,-9.44141372589803));
#165494=CARTESIAN_POINT('Ctrl Pts',(5.68530807887578,15.2,-9.44548784989941));
#165495=CARTESIAN_POINT('Ctrl Pts',(5.6860776611458,15.2,-9.4495619733457));
#165496=CARTESIAN_POINT('Ctrl Pts',(5.68684322995243,15.2,-9.45365109599273));
#165497=CARTESIAN_POINT('Ctrl Pts',(5.68760469294601,15.2,-9.45775513615626));
#165498=CARTESIAN_POINT('Ctrl Pts',(5.68836615604333,15.2,-9.46185917687895));
#165499=CARTESIAN_POINT('Ctrl Pts',(5.68912351394759,15.2,-9.4659781349918));
#165500=CARTESIAN_POINT('Ctrl Pts',(5.68987667235922,15.2,-9.47011193059154));
#165501=CARTESIAN_POINT('Ctrl Pts',(5.69062983066824,15.2,-9.47424572562805));
#165502=CARTESIAN_POINT('Ctrl Pts',(5.69137878963853,15.2,-9.47839435699274));
#165503=CARTESIAN_POINT('Ctrl Pts',(5.69212345868904,15.2,-9.4825577451514));
#165504=CARTESIAN_POINT('Ctrl Pts',(5.69286812784101,15.2,-9.48672113387734));
#165505=CARTESIAN_POINT('Ctrl Pts',(5.6936085065036,15.2,-9.49089927927175));
#165506=CARTESIAN_POINT('Ctrl Pts',(5.69434450487675,15.2,-9.49509210133452));
#165507=CARTESIAN_POINT('Ctrl Pts',(5.69508050314962,15.2,-9.499284922826));
#165508=CARTESIAN_POINT('Ctrl Pts',(5.69581212078937,15.2,-9.5034924197479));
#165509=CARTESIAN_POINT('Ctrl Pts',(5.69653926787776,15.2,-9.50771451411239));
#165510=CARTESIAN_POINT('Ctrl Pts',(5.69744820181254,15.2,-9.51299213249944));
#165511=CARTESIAN_POINT('Ctrl Pts',(5.69835015177435,15.2,-9.51829255963091));
#165512=CARTESIAN_POINT('Ctrl Pts',(5.69924494323307,15.2,-9.52361563789364));
#165513=CARTESIAN_POINT('Ctrl Pts',(5.69996077643905,15.2,-9.52787410073591));
#165514=CARTESIAN_POINT('Ctrl Pts',(5.70067203001115,15.2,-9.53214706225213));
#165515=CARTESIAN_POINT('Ctrl Pts',(5.70137861454935,15.2,-9.53643444287558));
#165516=CARTESIAN_POINT('Ctrl Pts',(5.70208519899128,15.2,-9.54072182291489));
#165517=CARTESIAN_POINT('Ctrl Pts',(5.70278711590663,15.2,-9.54502362000108));
#165518=CARTESIAN_POINT('Ctrl Pts',(5.70348427894044,15.2,-9.54933975964041));
#165519=CARTESIAN_POINT('Ctrl Pts',(5.70418144206923,15.2,-9.55365589986781));
#165520=CARTESIAN_POINT('Ctrl Pts',(5.70487385056064,15.2,-9.557986379362));
#165521=CARTESIAN_POINT('Ctrl Pts',(5.70556141909779,15.2,-9.56233112215528));
#165522=CARTESIAN_POINT('Ctrl Pts',(5.70624898754126,15.2,-9.56667586435658));
#165523=CARTESIAN_POINT('Ctrl Pts',(5.70693171676072,15.2,-9.57103486862725));
#165524=CARTESIAN_POINT('Ctrl Pts',(5.70760952237247,15.2,-9.57540805860162));
#165525=CARTESIAN_POINT('Ctrl Pts',(5.70828732807658,15.2,-9.57978124917183));
#165526=CARTESIAN_POINT('Ctrl Pts',(5.70896020769989,15.2,-9.58416862314304));
#165527=CARTESIAN_POINT('Ctrl Pts',(5.70962808151709,15.2,-9.58857010473629));
#165528=CARTESIAN_POINT('Ctrl Pts',(5.71012898683448,15.2,-9.59187121563138));
#165529=CARTESIAN_POINT('Ctrl Pts',(5.71062707536524,15.2,-9.59518026310242));
#165530=CARTESIAN_POINT('Ctrl Pts',(5.71112231218285,15.2,-9.59849721245529));
#165531=CARTESIAN_POINT('Ctrl Pts',(5.71161754900046,15.2,-9.60181416180816));
#165532=CARTESIAN_POINT('Ctrl Pts',(5.71210993339743,15.2,-9.6051390145586));
#165533=CARTESIAN_POINT('Ctrl Pts',(5.71259943217156,15.2,-9.60847173739516));
#165534=CARTESIAN_POINT('Ctrl Pts',(5.71308893094569,15.2,-9.61180446023171));
#165535=CARTESIAN_POINT('Ctrl Pts',(5.71357554332836,15.2,-9.61514505440941));
#165536=CARTESIAN_POINT('Ctrl Pts',(5.71405923514452,15.2,-9.61849348574501));
#165537=CARTESIAN_POINT('Ctrl Pts',(5.71454292704854,15.2,-9.62184191768891));
#165538=CARTESIAN_POINT('Ctrl Pts',(5.71502369871842,15.2,-9.62519818791));
#165539=CARTESIAN_POINT('Ctrl Pts',(5.71550151516246,15.2,-9.62856226473333));
#165540=CARTESIAN_POINT('Ctrl Pts',(5.71629787569999,15.2,-9.63416905801289));
#165541=CARTESIAN_POINT('Ctrl Pts',(5.71708602842116,15.2,-9.63979753358412));
#165542=CARTESIAN_POINT('Ctrl Pts',(5.71786581736463,15.2,-9.64544754449428));
#165543=CARTESIAN_POINT('Ctrl Pts',(5.7183336908497,15.2,-9.64883755190256));
#165544=CARTESIAN_POINT('Ctrl Pts',(5.71879855416727,15.2,-9.65223531204639));
#165545=CARTESIAN_POINT('Ctrl Pts',(5.71926037260897,15.2,-9.6556407925007));
#165546=CARTESIAN_POINT('Ctrl Pts',(5.71972219096677,15.2,-9.65904627233634));
#165547=CARTESIAN_POINT('Ctrl Pts',(5.72018096474975,15.2,-9.66245947352992));
#165548=CARTESIAN_POINT('Ctrl Pts',(5.72063666206625,15.2,-9.66588036286463));
#165549=CARTESIAN_POINT('Ctrl Pts',(5.72109235938276,15.2,-9.66930125219934));
#165550=CARTESIAN_POINT('Ctrl Pts',(5.72154497911468,15.2,-9.6727298301623));
#165551=CARTESIAN_POINT('Ctrl Pts',(5.72199448851704,15.2,-9.67616606546974));
#165552=CARTESIAN_POINT('Ctrl Pts',(5.7224439979194,15.2,-9.67960230077718));
#165553=CARTESIAN_POINT('Ctrl Pts',(5.72289039758031,15.2,-9.68304619372326));
#165554=CARTESIAN_POINT('Ctrl Pts',(5.72333365402456,15.2,-9.68649771198849));
#165555=CARTESIAN_POINT('Ctrl Pts',(5.72377691046882,15.2,-9.68994923025373));
#165556=CARTESIAN_POINT('Ctrl Pts',(5.72421702476789,15.2,-9.69340837381549));
#165557=CARTESIAN_POINT('Ctrl Pts',(5.72465396371062,15.2,-9.69687511114722));
#165558=CARTESIAN_POINT('Ctrl Pts',(5.72509090265336,15.2,-9.70034184847895));
#165559=CARTESIAN_POINT('Ctrl Pts',(5.72552466672131,15.2,-9.70381618066846));
#165560=CARTESIAN_POINT('Ctrl Pts',(5.72595522362277,15.2,-9.70729807449925));
#165561=CARTESIAN_POINT('Ctrl Pts',(5.72638578060245,15.2,-9.71077996896258));
#165562=CARTESIAN_POINT('Ctrl Pts',(5.72681313071456,15.2,-9.71426942558639));
#165563=CARTESIAN_POINT('Ctrl Pts',(5.72723724210909,15.2,-9.71776641401231));
#165564=CARTESIAN_POINT('Ctrl Pts',(5.72766135342657,15.2,-9.72126340180294));
#165565=CARTESIAN_POINT('Ctrl Pts',(5.72808222497542,15.2,-9.7247679209308));
#165566=CARTESIAN_POINT('Ctrl Pts',(5.72849982685573,15.2,-9.72827993989619));
#165567=CARTESIAN_POINT('Ctrl Pts',(5.72905662933753,15.2,-9.73296263163737));
#165568=CARTESIAN_POINT('Ctrl Pts',(5.72960761765509,15.2,-9.73765865660929));
#165569=CARTESIAN_POINT('Ctrl Pts',(5.73015271872202,15.2,-9.7423679413901));
#165570=CARTESIAN_POINT('Ctrl Pts',(5.73056154454078,15.2,-9.74589990513612));
#165571=CARTESIAN_POINT('Ctrl Pts',(5.73096705657645,15.2,-9.74943932625664));
#165572=CARTESIAN_POINT('Ctrl Pts',(5.73136922689563,15.2,-9.75298617600176));
#165573=CARTESIAN_POINT('Ctrl Pts',(5.73177139728787,15.2,-9.75653302639121));
#165574=CARTESIAN_POINT('Ctrl Pts',(5.73217022414583,15.2,-9.76008730432445));
#165575=CARTESIAN_POINT('Ctrl Pts',(5.73256567761951,15.2,-9.76364897830141));
#165576=CARTESIAN_POINT('Ctrl Pts',(5.73296113102135,15.2,-9.76721065163135));
#165577=CARTESIAN_POINT('Ctrl Pts',(5.73335321090669,15.2,-9.77077972156922));
#165578=CARTESIAN_POINT('Ctrl Pts',(5.73374188676727,15.2,-9.77435615689825));
#165579=CARTESIAN_POINT('Ctrl Pts',(5.73413056262785,15.2,-9.77793259222727));
#165580=CARTESIAN_POINT('Ctrl Pts',(5.73451583342913,15.2,-9.78151639300068));
#165581=CARTESIAN_POINT('Ctrl Pts',(5.73489767029198,15.2,-9.78510752971989));
#165582=CARTESIAN_POINT('Ctrl Pts',(5.73527950715483,15.2,-9.7886986664391));
#165583=CARTESIAN_POINT('Ctrl Pts',(5.7356579088282,15.2,-9.79229713751135));
#165584=CARTESIAN_POINT('Ctrl Pts',(5.73603284673296,15.2,-9.79590291327169));
#165585=CARTESIAN_POINT('Ctrl Pts',(5.73640778463773,15.2,-9.79950868903203));
#165586=CARTESIAN_POINT('Ctrl Pts',(5.73677925830621,15.2,-9.80312176875431));
#165587=CARTESIAN_POINT('Ctrl Pts',(5.73714723725147,15.2,-9.80674212208047));
#165588=CARTESIAN_POINT('Ctrl Pts',(5.73751521619673,15.2,-9.81036247540663));
#165589=CARTESIAN_POINT('Ctrl Pts',(5.73787970075058,15.2,-9.81399010270728));
#165590=CARTESIAN_POINT('Ctrl Pts',(5.73824066165461,15.2,-9.81762497344923));
#165591=CARTESIAN_POINT('Ctrl Pts',(5.73860162262422,15.2,-9.82125984485152));
#165592=CARTESIAN_POINT('Ctrl Pts',(5.73895905887616,15.2,-9.82490195898083));
#165593=CARTESIAN_POINT('Ctrl Pts',(5.73931294284378,15.2,-9.82855128680385));
#165594=CARTESIAN_POINT('Ctrl Pts',(5.73966682674711,15.2,-9.83220061396391));
#165595=CARTESIAN_POINT('Ctrl Pts',(5.74001715759605,15.2,-9.83585715234145));
#165596=CARTESIAN_POINT('Ctrl Pts',(5.74036390605869,15.2,-9.83952087472554));
#165597=CARTESIAN_POINT('Ctrl Pts',(5.74071065452133,15.2,-9.84318459710964));
#165598=CARTESIAN_POINT('Ctrl Pts',(5.74105382036624,15.2,-9.84685550108401));
#165599=CARTESIAN_POINT('Ctrl Pts',(5.74139337527025,15.2,-9.85053355740932));
#165600=CARTESIAN_POINT('Ctrl Pts',(5.74173293017427,15.2,-9.85421161373463));
#165601=CARTESIAN_POINT('Ctrl Pts',(5.74206887312871,15.2,-9.85789682291744));
#165602=CARTESIAN_POINT('Ctrl Pts',(5.74240117749164,15.2,-9.86158915378329));
#165603=CARTESIAN_POINT('Ctrl Pts',(5.74273348185456,15.2,-9.86528148464913));
#165604=CARTESIAN_POINT('Ctrl Pts',(5.7430621458093,15.2,-9.86898093776469));
#165605=CARTESIAN_POINT('Ctrl Pts',(5.74338714271448,15.2,-9.87268748404607));
#165606=CARTESIAN_POINT('Ctrl Pts',(5.74371213961966,15.2,-9.87639403032745));
#165607=CARTESIAN_POINT('Ctrl Pts',(5.74403346868372,15.2,-9.88010766911364));
#165608=CARTESIAN_POINT('Ctrl Pts',(5.74435109968848,15.2,-9.88382836903851));
#165609=CARTESIAN_POINT('Ctrl Pts',(5.74466873069324,15.2,-9.88754906896337));
#165610=CARTESIAN_POINT('Ctrl Pts',(5.74498266422643,15.2,-9.89127682890577));
#165611=CARTESIAN_POINT('Ctrl Pts',(5.74529287317401,15.2,-9.89501162118579));
#165612=CARTESIAN_POINT('Ctrl Pts',(5.74560308217794,15.2,-9.89874641414431));
#165613=CARTESIAN_POINT('Ctrl Pts',(5.74590956548914,15.2,-9.90248823862143));
#165614=CARTESIAN_POINT('Ctrl Pts',(5.7462122990743,15.2,-9.90623706808388));
#165615=CARTESIAN_POINT('Ctrl Pts',(5.74661594376283,15.2,-9.91123550623208));
#165616=CARTESIAN_POINT('Ctrl Pts',(5.74701292447168,15.2,-9.91624639874254));
#165617=CARTESIAN_POINT('Ctrl Pts',(5.74740316821801,15.2,-9.9212696688311));
#165618=CARTESIAN_POINT('Ctrl Pts',(5.74769585104103,15.2,-9.92503712156862));
#165619=CARTESIAN_POINT('Ctrl Pts',(5.74798474299045,15.2,-9.92881153501771));
#165620=CARTESIAN_POINT('Ctrl Pts',(5.74826981149478,15.2,-9.93259287498512));
#165621=CARTESIAN_POINT('Ctrl Pts',(5.74855487999911,15.2,-9.93637421495252));
#165622=CARTESIAN_POINT('Ctrl Pts',(5.74883612434905,15.2,-9.94016247957813));
#165623=CARTESIAN_POINT('Ctrl Pts',(5.7491135267145,15.2,-9.9439576491893));
#165624=CARTESIAN_POINT('Ctrl Pts',(5.74948339656868,15.2,-9.94901787579716));
#165625=CARTESIAN_POINT('Ctrl Pts',(5.74984644090288,15.2,-9.95409037694775));
#165626=CARTESIAN_POINT('Ctrl Pts',(5.75020264099994,15.2,-9.95917514500001));
#165627=CARTESIAN_POINT('Ctrl Pts',(4.57383771099994,15.2,-9.31239140100002));
#165628=CARTESIAN_POINT('Ctrl Pts',(4.57383771099994,11.6,-9.31239140100002));
#165629=CARTESIAN_POINT('Ctrl Pts',(4.57392774199994,15.2,-9.31254071600002));
#165630=CARTESIAN_POINT('Ctrl Pts',(4.57392774199994,11.6,-9.31254071600002));
#165631=CARTESIAN_POINT('Ctrl Pts',(4.57411102199994,15.2,-9.31284451800002));
#165632=CARTESIAN_POINT('Ctrl Pts',(4.57411102199994,11.6,-9.31284451800002));
#165633=CARTESIAN_POINT('Ctrl Pts',(4.57438896199994,15.2,-9.31330471200001));
#165634=CARTESIAN_POINT('Ctrl Pts',(4.57438896199994,11.6,-9.31330471200001));
#165635=CARTESIAN_POINT('Ctrl Pts',(4.57476383499994,15.2,-9.31392435700002));
#165636=CARTESIAN_POINT('Ctrl Pts',(4.57476383499994,11.6,-9.31392435700002));
#165637=CARTESIAN_POINT('Ctrl Pts',(4.57523877599994,15.2,-9.31470764300002));
#165638=CARTESIAN_POINT('Ctrl Pts',(4.57523877599994,11.6,-9.31470764300002));
#165639=CARTESIAN_POINT('Ctrl Pts',(4.57572221399994,15.2,-9.31550314000001));
#165640=CARTESIAN_POINT('Ctrl Pts',(4.57572221399994,11.6,-9.31550314000001));
#165641=CARTESIAN_POINT('Ctrl Pts',(4.57621139799994,15.2,-9.31630627600001));
#165642=CARTESIAN_POINT('Ctrl Pts',(4.57621139799994,11.6,-9.31630627600001));
#165643=CARTESIAN_POINT('Ctrl Pts',(4.57670632999994,15.2,-9.31711702100002));
#165644=CARTESIAN_POINT('Ctrl Pts',(4.57670632999994,11.6,-9.31711702100002));
#165645=CARTESIAN_POINT('Ctrl Pts',(4.57720701299994,15.2,-9.31793534100001));
#165646=CARTESIAN_POINT('Ctrl Pts',(4.57720701299994,11.6,-9.31793534100001));
#165647=CARTESIAN_POINT('Ctrl Pts',(4.57771344599994,15.2,-9.31876120400002));
#165648=CARTESIAN_POINT('Ctrl Pts',(4.57771344599994,11.6,-9.31876120400002));
#165649=CARTESIAN_POINT('Ctrl Pts',(4.57822563299994,15.2,-9.31959457900001));
#165650=CARTESIAN_POINT('Ctrl Pts',(4.57822563299994,11.6,-9.31959457900001));
#165651=CARTESIAN_POINT('Ctrl Pts',(4.57874357399994,15.2,-9.32043543300002));
#165652=CARTESIAN_POINT('Ctrl Pts',(4.57874357399994,11.6,-9.32043543300002));
#165653=CARTESIAN_POINT('Ctrl Pts',(4.57926726999994,15.2,-9.32128373600002));
#165654=CARTESIAN_POINT('Ctrl Pts',(4.57926726999994,11.6,-9.32128373600002));
#165655=CARTESIAN_POINT('Ctrl Pts',(4.57979672299994,15.2,-9.32213945400001));
#165656=CARTESIAN_POINT('Ctrl Pts',(4.57979672299994,11.6,-9.32213945400001));
#165657=CARTESIAN_POINT('Ctrl Pts',(4.58033193499994,15.2,-9.32300255700002));
#165658=CARTESIAN_POINT('Ctrl Pts',(4.58033193499994,11.6,-9.32300255700002));
#165659=CARTESIAN_POINT('Ctrl Pts',(4.58087290499994,15.2,-9.32387301400002));
#165660=CARTESIAN_POINT('Ctrl Pts',(4.58087290499994,11.6,-9.32387301400002));
#165661=CARTESIAN_POINT('Ctrl Pts',(4.58141963599994,15.2,-9.32475079300002));
#165662=CARTESIAN_POINT('Ctrl Pts',(4.58141963599994,11.6,-9.32475079300002));
#165663=CARTESIAN_POINT('Ctrl Pts',(4.58197212899994,15.2,-9.32563586400001));
#165664=CARTESIAN_POINT('Ctrl Pts',(4.58197212899994,11.6,-9.32563586400001));
#165665=CARTESIAN_POINT('Ctrl Pts',(4.58253038599994,15.2,-9.32652819500002));
#165666=CARTESIAN_POINT('Ctrl Pts',(4.58253038599994,11.6,-9.32652819500002));
#165667=CARTESIAN_POINT('Ctrl Pts',(4.58309440599994,15.2,-9.32742775700002));
#165668=CARTESIAN_POINT('Ctrl Pts',(4.58309440599994,11.6,-9.32742775700002));
#165669=CARTESIAN_POINT('Ctrl Pts',(4.58366419299994,15.2,-9.32833451700001));
#165670=CARTESIAN_POINT('Ctrl Pts',(4.58366419299994,11.6,-9.32833451700001));
#165671=CARTESIAN_POINT('Ctrl Pts',(4.58423974599994,15.2,-9.32924844800001));
#165672=CARTESIAN_POINT('Ctrl Pts',(4.58423974599994,11.6,-9.32924844800001));
#165673=CARTESIAN_POINT('Ctrl Pts',(4.58482106699994,15.2,-9.33016951700001));
#165674=CARTESIAN_POINT('Ctrl Pts',(4.58482106699994,11.6,-9.33016951700001));
#165675=CARTESIAN_POINT('Ctrl Pts',(4.58540815599994,15.2,-9.33109769500001));
#165676=CARTESIAN_POINT('Ctrl Pts',(4.58540815599994,11.6,-9.33109769500001));
#165677=CARTESIAN_POINT('Ctrl Pts',(4.58600101699994,15.2,-9.33203295200002));
#165678=CARTESIAN_POINT('Ctrl Pts',(4.58600101699994,11.6,-9.33203295200002));
#165679=CARTESIAN_POINT('Ctrl Pts',(4.58659964899994,15.2,-9.33297525800001));
#165680=CARTESIAN_POINT('Ctrl Pts',(4.58659964899994,11.6,-9.33297525800001));
#165681=CARTESIAN_POINT('Ctrl Pts',(4.58720405199994,15.2,-9.33392458500002));
#165682=CARTESIAN_POINT('Ctrl Pts',(4.58720405199994,11.6,-9.33392458500002));
#165683=CARTESIAN_POINT('Ctrl Pts',(4.58781422999994,15.2,-9.33488090000001));
#165684=CARTESIAN_POINT('Ctrl Pts',(4.58781422999994,11.6,-9.33488090000001));
#165685=CARTESIAN_POINT('Ctrl Pts',(4.58843018199994,15.2,-9.33584417600001));
#165686=CARTESIAN_POINT('Ctrl Pts',(4.58843018199994,11.6,-9.33584417600001));
#165687=CARTESIAN_POINT('Ctrl Pts',(4.58905190799995,15.2,-9.33681438400002));
#165688=CARTESIAN_POINT('Ctrl Pts',(4.58905190799995,11.6,-9.33681438400002));
#165689=CARTESIAN_POINT('Ctrl Pts',(4.58967941299994,15.2,-9.33779149400002));
#165690=CARTESIAN_POINT('Ctrl Pts',(4.58967941299994,11.6,-9.33779149400002));
#165691=CARTESIAN_POINT('Ctrl Pts',(4.59031269299994,15.2,-9.33877547700002));
#165692=CARTESIAN_POINT('Ctrl Pts',(4.59031269299994,11.6,-9.33877547700002));
#165693=CARTESIAN_POINT('Ctrl Pts',(4.59095175299994,15.2,-9.33976630400002));
#165694=CARTESIAN_POINT('Ctrl Pts',(4.59095175299994,11.6,-9.33976630400002));
#165695=CARTESIAN_POINT('Ctrl Pts',(4.59159659199994,15.2,-9.34076394900002));
#165696=CARTESIAN_POINT('Ctrl Pts',(4.59159659199994,11.6,-9.34076394900002));
#165697=CARTESIAN_POINT('Ctrl Pts',(4.59224721199994,15.2,-9.34176837800001));
#165698=CARTESIAN_POINT('Ctrl Pts',(4.59224721199994,11.6,-9.34176837800001));
#165699=CARTESIAN_POINT('Ctrl Pts',(4.59290361199994,15.2,-9.34277956800001));
#165700=CARTESIAN_POINT('Ctrl Pts',(4.59290361199994,11.6,-9.34277956800001));
#165701=CARTESIAN_POINT('Ctrl Pts',(4.59356579399994,15.2,-9.34379748800002));
#165702=CARTESIAN_POINT('Ctrl Pts',(4.59356579399994,11.6,-9.34379748800002));
#165703=CARTESIAN_POINT('Ctrl Pts',(4.59423375999994,15.2,-9.34482211000002));
#165704=CARTESIAN_POINT('Ctrl Pts',(4.59423375999994,11.6,-9.34482211000002));
#165705=CARTESIAN_POINT('Ctrl Pts',(4.59490750999994,15.2,-9.34585340600002));
#165706=CARTESIAN_POINT('Ctrl Pts',(4.59490750999994,11.6,-9.34585340600002));
#165707=CARTESIAN_POINT('Ctrl Pts',(4.59558704399994,15.2,-9.34689134800001));
#165708=CARTESIAN_POINT('Ctrl Pts',(4.59558704399994,11.6,-9.34689134800001));
#165709=CARTESIAN_POINT('Ctrl Pts',(4.59627236399994,15.2,-9.34793590900002));
#165710=CARTESIAN_POINT('Ctrl Pts',(4.59627236399994,11.6,-9.34793590900002));
#165711=CARTESIAN_POINT('Ctrl Pts',(4.59696346899994,15.2,-9.34898706000002));
#165712=CARTESIAN_POINT('Ctrl Pts',(4.59696346899994,11.6,-9.34898706000002));
#165713=CARTESIAN_POINT('Ctrl Pts',(4.59766036299994,15.2,-9.35004477400001));
#165714=CARTESIAN_POINT('Ctrl Pts',(4.59766036299994,11.6,-9.35004477400001));
#165715=CARTESIAN_POINT('Ctrl Pts',(4.59836304399994,15.2,-9.35110902400002));
#165716=CARTESIAN_POINT('Ctrl Pts',(4.59836304399994,11.6,-9.35110902400002));
#165717=CARTESIAN_POINT('Ctrl Pts',(4.59907151299994,15.2,-9.35217978300001));
#165718=CARTESIAN_POINT('Ctrl Pts',(4.59907151299994,11.6,-9.35217978300001));
#165719=CARTESIAN_POINT('Ctrl Pts',(4.59978577199994,15.2,-9.35325702300002));
#165720=CARTESIAN_POINT('Ctrl Pts',(4.59978577199994,11.6,-9.35325702300002));
#165721=CARTESIAN_POINT('Ctrl Pts',(4.60050582099994,15.2,-9.35434071600002));
#165722=CARTESIAN_POINT('Ctrl Pts',(4.60050582099994,11.6,-9.35434071600002));
#165723=CARTESIAN_POINT('Ctrl Pts',(4.60123166099994,15.2,-9.35543083800002));
#165724=CARTESIAN_POINT('Ctrl Pts',(4.60123166099994,11.6,-9.35543083800002));
#165725=CARTESIAN_POINT('Ctrl Pts',(4.60196329199994,15.2,-9.35652735800002));
#165726=CARTESIAN_POINT('Ctrl Pts',(4.60196329199994,11.6,-9.35652735800002));
#165727=CARTESIAN_POINT('Ctrl Pts',(4.60270071599994,15.2,-9.35763025300002));
#165728=CARTESIAN_POINT('Ctrl Pts',(4.60270071599994,11.6,-9.35763025300002));
#165729=CARTESIAN_POINT('Ctrl Pts',(4.60344393199994,15.2,-9.35873949500002));
#165730=CARTESIAN_POINT('Ctrl Pts',(4.60344393199994,11.6,-9.35873949500002));
#165731=CARTESIAN_POINT('Ctrl Pts',(4.60419294099994,15.2,-9.35985505600001));
#165732=CARTESIAN_POINT('Ctrl Pts',(4.60419294099994,11.6,-9.35985505600001));
#165733=CARTESIAN_POINT('Ctrl Pts',(4.60494774599994,15.2,-9.36097691200001));
#165734=CARTESIAN_POINT('Ctrl Pts',(4.60494774599994,11.6,-9.36097691200001));
#165735=CARTESIAN_POINT('Ctrl Pts',(4.60570834399994,15.2,-9.36210503600002));
#165736=CARTESIAN_POINT('Ctrl Pts',(4.60570834399994,11.6,-9.36210503600002));
#165737=CARTESIAN_POINT('Ctrl Pts',(4.60647473799994,15.2,-9.36323940100002));
#165738=CARTESIAN_POINT('Ctrl Pts',(4.60647473799994,11.6,-9.36323940100002));
#165739=CARTESIAN_POINT('Ctrl Pts',(4.60724692799994,15.2,-9.36437998200002));
#165740=CARTESIAN_POINT('Ctrl Pts',(4.60724692799994,11.6,-9.36437998200002));
#165741=CARTESIAN_POINT('Ctrl Pts',(4.60802491399994,15.2,-9.36552675100002));
#165742=CARTESIAN_POINT('Ctrl Pts',(4.60802491399994,11.6,-9.36552675100002));
#165743=CARTESIAN_POINT('Ctrl Pts',(4.60880869699994,15.2,-9.36667968600002));
#165744=CARTESIAN_POINT('Ctrl Pts',(4.60880869699994,11.6,-9.36667968600002));
#165745=CARTESIAN_POINT('Ctrl Pts',(4.60959827699994,15.2,-9.36783875800002));
#165746=CARTESIAN_POINT('Ctrl Pts',(4.60959827699994,11.6,-9.36783875800002));
#165747=CARTESIAN_POINT('Ctrl Pts',(4.61039365599994,15.2,-9.36900394200002));
#165748=CARTESIAN_POINT('Ctrl Pts',(4.61039365599994,11.6,-9.36900394200002));
#165749=CARTESIAN_POINT('Ctrl Pts',(4.61119483299994,15.2,-9.37017521400002));
#165750=CARTESIAN_POINT('Ctrl Pts',(4.61119483299994,11.6,-9.37017521400002));
#165751=CARTESIAN_POINT('Ctrl Pts',(4.61200180799994,15.2,-9.37135254700001));
#165752=CARTESIAN_POINT('Ctrl Pts',(4.61200180799994,11.6,-9.37135254700001));
#165753=CARTESIAN_POINT('Ctrl Pts',(4.61281458299994,15.2,-9.37253591500001));
#165754=CARTESIAN_POINT('Ctrl Pts',(4.61281458299994,11.6,-9.37253591500001));
#165755=CARTESIAN_POINT('Ctrl Pts',(4.61363315799994,15.2,-9.37372529500001));
#165756=CARTESIAN_POINT('Ctrl Pts',(4.61363315799994,11.6,-9.37372529500001));
#165757=CARTESIAN_POINT('Ctrl Pts',(4.61445753499994,15.2,-9.37492066200001));
#165758=CARTESIAN_POINT('Ctrl Pts',(4.61445753499994,11.6,-9.37492066200001));
#165759=CARTESIAN_POINT('Ctrl Pts',(4.61528770999994,15.2,-9.37612198900002));
#165760=CARTESIAN_POINT('Ctrl Pts',(4.61528770999994,11.6,-9.37612198900002));
#165761=CARTESIAN_POINT('Ctrl Pts',(4.61612368799994,15.2,-9.37732925100002));
#165762=CARTESIAN_POINT('Ctrl Pts',(4.61612368799994,11.6,-9.37732925100002));
#165763=CARTESIAN_POINT('Ctrl Pts',(4.61696546699994,15.2,-9.37854242500002));
#165764=CARTESIAN_POINT('Ctrl Pts',(4.61696546699994,11.6,-9.37854242500002));
#165765=CARTESIAN_POINT('Ctrl Pts',(4.61781304699994,15.2,-9.37976148600002));
#165766=CARTESIAN_POINT('Ctrl Pts',(4.61781304699994,11.6,-9.37976148600002));
#165767=CARTESIAN_POINT('Ctrl Pts',(4.61866642999994,15.2,-9.38098640900002));
#165768=CARTESIAN_POINT('Ctrl Pts',(4.61866642999994,11.6,-9.38098640900002));
#165769=CARTESIAN_POINT('Ctrl Pts',(4.61952561499994,15.2,-9.38221716900001));
#165770=CARTESIAN_POINT('Ctrl Pts',(4.61952561499994,11.6,-9.38221716900001));
#165771=CARTESIAN_POINT('Ctrl Pts',(4.62039060399994,15.2,-9.38345374300001));
#165772=CARTESIAN_POINT('Ctrl Pts',(4.62039060399994,11.6,-9.38345374300001));
#165773=CARTESIAN_POINT('Ctrl Pts',(4.62126139499994,15.2,-9.38469610600002));
#165774=CARTESIAN_POINT('Ctrl Pts',(4.62126139499994,11.6,-9.38469610600002));
#165775=CARTESIAN_POINT('Ctrl Pts',(4.62213798999994,15.2,-9.38594423300002));
#165776=CARTESIAN_POINT('Ctrl Pts',(4.62213798999994,11.6,-9.38594423300002));
#165777=CARTESIAN_POINT('Ctrl Pts',(4.62302038999994,15.2,-9.38719810100002));
#165778=CARTESIAN_POINT('Ctrl Pts',(4.62302038999994,11.6,-9.38719810100002));
#165779=CARTESIAN_POINT('Ctrl Pts',(4.62390859299994,15.2,-9.38845768500002));
#165780=CARTESIAN_POINT('Ctrl Pts',(4.62390859299994,11.6,-9.38845768500002));
#165781=CARTESIAN_POINT('Ctrl Pts',(4.62480259899994,15.2,-9.38972296200001));
#165782=CARTESIAN_POINT('Ctrl Pts',(4.62480259899994,11.6,-9.38972296200001));
#165783=CARTESIAN_POINT('Ctrl Pts',(4.62570241199994,15.2,-9.39099390800001));
#165784=CARTESIAN_POINT('Ctrl Pts',(4.62570241199994,11.6,-9.39099390800001));
#165785=CARTESIAN_POINT('Ctrl Pts',(4.62660802799994,15.2,-9.39227050000002));
#165786=CARTESIAN_POINT('Ctrl Pts',(4.62660802799994,11.6,-9.39227050000002));
#165787=CARTESIAN_POINT('Ctrl Pts',(4.62751944999994,15.2,-9.39355271300002));
#165788=CARTESIAN_POINT('Ctrl Pts',(4.62751944999994,11.6,-9.39355271300002));
#165789=CARTESIAN_POINT('Ctrl Pts',(4.62843667699994,15.2,-9.39484052400001));
#165790=CARTESIAN_POINT('Ctrl Pts',(4.62843667699994,11.6,-9.39484052400001));
#165791=CARTESIAN_POINT('Ctrl Pts',(4.62935970899994,15.2,-9.39613391000002));
#165792=CARTESIAN_POINT('Ctrl Pts',(4.62935970899994,11.6,-9.39613391000002));
#165793=CARTESIAN_POINT('Ctrl Pts',(4.63028854799994,15.2,-9.39743284700001));
#165794=CARTESIAN_POINT('Ctrl Pts',(4.63028854799994,11.6,-9.39743284700001));
#165795=CARTESIAN_POINT('Ctrl Pts',(4.63122319099994,15.2,-9.39873731300001));
#165796=CARTESIAN_POINT('Ctrl Pts',(4.63122319099994,11.6,-9.39873731300001));
#165797=CARTESIAN_POINT('Ctrl Pts',(4.63216364099994,15.2,-9.40004728300002));
#165798=CARTESIAN_POINT('Ctrl Pts',(4.63216364099994,11.6,-9.40004728300002));
#165799=CARTESIAN_POINT('Ctrl Pts',(4.63310989699994,15.2,-9.40136273600002));
#165800=CARTESIAN_POINT('Ctrl Pts',(4.63310989699994,11.6,-9.40136273600002));
#165801=CARTESIAN_POINT('Ctrl Pts',(4.63406195899994,15.2,-9.40268364800002));
#165802=CARTESIAN_POINT('Ctrl Pts',(4.63406195899994,11.6,-9.40268364800002));
#165803=CARTESIAN_POINT('Ctrl Pts',(4.63501982699994,15.2,-9.40400999500002));
#165804=CARTESIAN_POINT('Ctrl Pts',(4.63501982699994,11.6,-9.40400999500002));
#165805=CARTESIAN_POINT('Ctrl Pts',(4.63598349999994,15.2,-9.40534175600002));
#165806=CARTESIAN_POINT('Ctrl Pts',(4.63598349999994,11.6,-9.40534175600002));
#165807=CARTESIAN_POINT('Ctrl Pts',(4.63695298199994,15.2,-9.40667890700002));
#165808=CARTESIAN_POINT('Ctrl Pts',(4.63695298199994,11.6,-9.40667890700002));
#165809=CARTESIAN_POINT('Ctrl Pts',(4.63792826799994,15.2,-9.40802142600001));
#165810=CARTESIAN_POINT('Ctrl Pts',(4.63792826799994,11.6,-9.40802142600001));
#165811=CARTESIAN_POINT('Ctrl Pts',(4.63890936299994,15.2,-9.40936929100002));
#165812=CARTESIAN_POINT('Ctrl Pts',(4.63890936299994,11.6,-9.40936929100002));
#165813=CARTESIAN_POINT('Ctrl Pts',(4.63989626199994,15.2,-9.41072247900001));
#165814=CARTESIAN_POINT('Ctrl Pts',(4.63989626199994,11.6,-9.41072247900001));
#165815=CARTESIAN_POINT('Ctrl Pts',(4.64088896899994,15.2,-9.41208096700001));
#165816=CARTESIAN_POINT('Ctrl Pts',(4.64088896899994,11.6,-9.41208096700001));
#165817=CARTESIAN_POINT('Ctrl Pts',(4.64188748399994,15.2,-9.41344473400001));
#165818=CARTESIAN_POINT('Ctrl Pts',(4.64188748399994,11.6,-9.41344473400001));
#165819=CARTESIAN_POINT('Ctrl Pts',(4.64289180299994,15.2,-9.41481375700001));
#165820=CARTESIAN_POINT('Ctrl Pts',(4.64289180299994,11.6,-9.41481375700001));
#165821=CARTESIAN_POINT('Ctrl Pts',(4.64390192999994,15.2,-9.41618801400002));
#165822=CARTESIAN_POINT('Ctrl Pts',(4.64390192999994,11.6,-9.41618801400002));
#165823=CARTESIAN_POINT('Ctrl Pts',(4.64491786299994,15.2,-9.41756748400002));
#165824=CARTESIAN_POINT('Ctrl Pts',(4.64491786299994,11.6,-9.41756748400002));
#165825=CARTESIAN_POINT('Ctrl Pts',(4.64593960299994,15.2,-9.41895214200001));
#165826=CARTESIAN_POINT('Ctrl Pts',(4.64593960299994,11.6,-9.41895214200001));
#165827=CARTESIAN_POINT('Ctrl Pts',(4.64696714999994,15.2,-9.42034197000002));
#165828=CARTESIAN_POINT('Ctrl Pts',(4.64696714999994,11.6,-9.42034197000002));
#165829=CARTESIAN_POINT('Ctrl Pts',(4.64800050299994,15.2,-9.42173694400001));
#165830=CARTESIAN_POINT('Ctrl Pts',(4.64800050299994,11.6,-9.42173694400001));
#165831=CARTESIAN_POINT('Ctrl Pts',(4.64903966199994,15.2,-9.42313704200001));
#165832=CARTESIAN_POINT('Ctrl Pts',(4.64903966199994,11.6,-9.42313704200001));
#165833=CARTESIAN_POINT('Ctrl Pts',(4.65008462699994,15.2,-9.42454224400001));
#165834=CARTESIAN_POINT('Ctrl Pts',(4.65008462699994,11.6,-9.42454224400001));
#165835=CARTESIAN_POINT('Ctrl Pts',(4.65113539899994,15.2,-9.42595252700002));
#165836=CARTESIAN_POINT('Ctrl Pts',(4.65113539899994,11.6,-9.42595252700002));
#165837=CARTESIAN_POINT('Ctrl Pts',(4.65219197599995,15.2,-9.42736787100002));
#165838=CARTESIAN_POINT('Ctrl Pts',(4.65219197599995,11.6,-9.42736787100002));
#165839=CARTESIAN_POINT('Ctrl Pts',(4.65325435999994,15.2,-9.42878825300001));
#165840=CARTESIAN_POINT('Ctrl Pts',(4.65325435999994,11.6,-9.42878825300001));
#165841=CARTESIAN_POINT('Ctrl Pts',(4.65432254899994,15.2,-9.43021365300002));
#165842=CARTESIAN_POINT('Ctrl Pts',(4.65432254899994,11.6,-9.43021365300002));
#165843=CARTESIAN_POINT('Ctrl Pts',(4.65539654399994,15.2,-9.43164405000001));
#165844=CARTESIAN_POINT('Ctrl Pts',(4.65539654399994,11.6,-9.43164405000001));
#165845=CARTESIAN_POINT('Ctrl Pts',(4.65647634499994,15.2,-9.43307942000001));
#165846=CARTESIAN_POINT('Ctrl Pts',(4.65647634499994,11.6,-9.43307942000001));
#165847=CARTESIAN_POINT('Ctrl Pts',(4.65756194999994,15.2,-9.43451974600002));
#165848=CARTESIAN_POINT('Ctrl Pts',(4.65756194999994,11.6,-9.43451974600002));
#165849=CARTESIAN_POINT('Ctrl Pts',(4.65865336199994,15.2,-9.43596500400002));
#165850=CARTESIAN_POINT('Ctrl Pts',(4.65865336199994,11.6,-9.43596500400002));
#165851=CARTESIAN_POINT('Ctrl Pts',(4.65975057699994,15.2,-9.43741517400002));
#165852=CARTESIAN_POINT('Ctrl Pts',(4.65975057699994,11.6,-9.43741517400002));
#165853=CARTESIAN_POINT('Ctrl Pts',(4.66085359799994,15.2,-9.43887023600002));
#165854=CARTESIAN_POINT('Ctrl Pts',(4.66085359799994,11.6,-9.43887023600002));
#165855=CARTESIAN_POINT('Ctrl Pts',(4.66196242299994,15.2,-9.44033016800002));
#165856=CARTESIAN_POINT('Ctrl Pts',(4.66196242299994,11.6,-9.44033016800002));
#165857=CARTESIAN_POINT('Ctrl Pts',(4.66307705199994,15.2,-9.44179494900002));
#165858=CARTESIAN_POINT('Ctrl Pts',(4.66307705199994,11.6,-9.44179494900002));
#165859=CARTESIAN_POINT('Ctrl Pts',(4.66419748599994,15.2,-9.44326456000002));
#165860=CARTESIAN_POINT('Ctrl Pts',(4.66419748599994,11.6,-9.44326456000002));
#165861=CARTESIAN_POINT('Ctrl Pts',(4.66532372199994,15.2,-9.44473898000001));
#165862=CARTESIAN_POINT('Ctrl Pts',(4.66532372199994,11.6,-9.44473898000001));
#165863=CARTESIAN_POINT('Ctrl Pts',(4.66645576299995,15.2,-9.44621818800002));
#165864=CARTESIAN_POINT('Ctrl Pts',(4.66645576299995,11.6,-9.44621818800002));
#165865=CARTESIAN_POINT('Ctrl Pts',(4.66759360699994,15.2,-9.44770216300002));
#165866=CARTESIAN_POINT('Ctrl Pts',(4.66759360699994,11.6,-9.44770216300002));
#165867=CARTESIAN_POINT('Ctrl Pts',(4.66873725299994,15.2,-9.44919088600002));
#165868=CARTESIAN_POINT('Ctrl Pts',(4.66873725299994,11.6,-9.44919088600002));
#165869=CARTESIAN_POINT('Ctrl Pts',(4.66988670199994,15.2,-9.45068433600002));
#165870=CARTESIAN_POINT('Ctrl Pts',(4.66988670199994,11.6,-9.45068433600002));
#165871=CARTESIAN_POINT('Ctrl Pts',(4.67104195499994,15.2,-9.45218249400002));
#165872=CARTESIAN_POINT('Ctrl Pts',(4.67104195499994,11.6,-9.45218249400002));
#165873=CARTESIAN_POINT('Ctrl Pts',(4.67220300799994,15.2,-9.45368533800002));
#165874=CARTESIAN_POINT('Ctrl Pts',(4.67220300799994,11.6,-9.45368533800002));
#165875=CARTESIAN_POINT('Ctrl Pts',(4.67336986399994,15.2,-9.45519284900002));
#165876=CARTESIAN_POINT('Ctrl Pts',(4.67336986399994,11.6,-9.45519284900002));
#165877=CARTESIAN_POINT('Ctrl Pts',(4.67454251999994,15.2,-9.45670500700002));
#165878=CARTESIAN_POINT('Ctrl Pts',(4.67454251999994,11.6,-9.45670500700002));
#165879=CARTESIAN_POINT('Ctrl Pts',(4.67572097799994,15.2,-9.45822179200002));
#165880=CARTESIAN_POINT('Ctrl Pts',(4.67572097799994,11.6,-9.45822179200002));
#165881=CARTESIAN_POINT('Ctrl Pts',(4.67690523599994,15.2,-9.45974318300001));
#165882=CARTESIAN_POINT('Ctrl Pts',(4.67690523599994,11.6,-9.45974318300001));
#165883=CARTESIAN_POINT('Ctrl Pts',(4.67809529399994,15.2,-9.46126916300001));
#165884=CARTESIAN_POINT('Ctrl Pts',(4.67809529399994,11.6,-9.46126916300001));
#165885=CARTESIAN_POINT('Ctrl Pts',(4.67929115299994,15.2,-9.46279970900001));
#165886=CARTESIAN_POINT('Ctrl Pts',(4.67929115299994,11.6,-9.46279970900001));
#165887=CARTESIAN_POINT('Ctrl Pts',(4.68049280999994,15.2,-9.46433480500002));
#165888=CARTESIAN_POINT('Ctrl Pts',(4.68049280999994,11.6,-9.46433480500002));
#165889=CARTESIAN_POINT('Ctrl Pts',(4.68170026699995,15.2,-9.46587442800002));
#165890=CARTESIAN_POINT('Ctrl Pts',(4.68170026699995,11.6,-9.46587442800002));
#165891=CARTESIAN_POINT('Ctrl Pts',(4.68291352099994,15.2,-9.46741856000001));
#165892=CARTESIAN_POINT('Ctrl Pts',(4.68291352099994,11.6,-9.46741856000001));
#165893=CARTESIAN_POINT('Ctrl Pts',(4.68413257499994,15.2,-9.46896718200002));
#165894=CARTESIAN_POINT('Ctrl Pts',(4.68413257499994,11.6,-9.46896718200002));
#165895=CARTESIAN_POINT('Ctrl Pts',(4.68535742699994,15.2,-9.47052027400002));
#165896=CARTESIAN_POINT('Ctrl Pts',(4.68535742699994,11.6,-9.47052027400002));
#165897=CARTESIAN_POINT('Ctrl Pts',(4.68658807499994,15.2,-9.47207781700002));
#165898=CARTESIAN_POINT('Ctrl Pts',(4.68658807499994,11.6,-9.47207781700002));
#165899=CARTESIAN_POINT('Ctrl Pts',(4.68782451899994,15.2,-9.47363979200002));
#165900=CARTESIAN_POINT('Ctrl Pts',(4.68782451899994,11.6,-9.47363979200002));
#165901=CARTESIAN_POINT('Ctrl Pts',(4.68906676199994,15.2,-9.47520617900001));
#165902=CARTESIAN_POINT('Ctrl Pts',(4.68906676199994,11.6,-9.47520617900001));
#165903=CARTESIAN_POINT('Ctrl Pts',(4.69031479799994,15.2,-9.47677695900002));
#165904=CARTESIAN_POINT('Ctrl Pts',(4.69031479799994,11.6,-9.47677695900002));
#165905=CARTESIAN_POINT('Ctrl Pts',(4.69156863099994,15.2,-9.47835211400001));
#165906=CARTESIAN_POINT('Ctrl Pts',(4.69156863099994,11.6,-9.47835211400001));
#165907=CARTESIAN_POINT('Ctrl Pts',(4.69282825799994,15.2,-9.47993162400002));
#165908=CARTESIAN_POINT('Ctrl Pts',(4.69282825799994,11.6,-9.47993162400002));
#165909=CARTESIAN_POINT('Ctrl Pts',(4.69409367999994,15.2,-9.48151547000002));
#165910=CARTESIAN_POINT('Ctrl Pts',(4.69409367999994,11.6,-9.48151547000002));
#165911=CARTESIAN_POINT('Ctrl Pts',(4.69536489499994,15.2,-9.48310363400001));
#165912=CARTESIAN_POINT('Ctrl Pts',(4.69536489499994,11.6,-9.48310363400001));
#165913=CARTESIAN_POINT('Ctrl Pts',(4.69664190399994,15.2,-9.48469609800001));
#165914=CARTESIAN_POINT('Ctrl Pts',(4.69664190399994,11.6,-9.48469609800001));
#165915=CARTESIAN_POINT('Ctrl Pts',(4.69792470499994,15.2,-9.48629284000001));
#165916=CARTESIAN_POINT('Ctrl Pts',(4.69792470499994,11.6,-9.48629284000001));
#165917=CARTESIAN_POINT('Ctrl Pts',(4.69921329899994,15.2,-9.48789384500002));
#165918=CARTESIAN_POINT('Ctrl Pts',(4.69921329899994,11.6,-9.48789384500002));
#165919=CARTESIAN_POINT('Ctrl Pts',(4.70050768499994,15.2,-9.48949909200002));
#165920=CARTESIAN_POINT('Ctrl Pts',(4.70050768499994,11.6,-9.48949909200002));
#165921=CARTESIAN_POINT('Ctrl Pts',(4.70180786099994,15.2,-9.49110856300001));
#165922=CARTESIAN_POINT('Ctrl Pts',(4.70180786099994,11.6,-9.49110856300001));
#165923=CARTESIAN_POINT('Ctrl Pts',(4.70311382699994,15.2,-9.49272224000002));
#165924=CARTESIAN_POINT('Ctrl Pts',(4.70311382699994,11.6,-9.49272224000002));
#165925=CARTESIAN_POINT('Ctrl Pts',(4.70442558399994,15.2,-9.49434010500001));
#165926=CARTESIAN_POINT('Ctrl Pts',(4.70442558399994,11.6,-9.49434010500001));
#165927=CARTESIAN_POINT('Ctrl Pts',(4.70574312999995,15.2,-9.49596213800002));
#165928=CARTESIAN_POINT('Ctrl Pts',(4.70574312999995,11.6,-9.49596213800002));
#165929=CARTESIAN_POINT('Ctrl Pts',(4.70706646299994,15.2,-9.49758832300001));
#165930=CARTESIAN_POINT('Ctrl Pts',(4.70706646299994,11.6,-9.49758832300001));
#165931=CARTESIAN_POINT('Ctrl Pts',(4.70839558499994,15.2,-9.49921863900002));
#165932=CARTESIAN_POINT('Ctrl Pts',(4.70839558499994,11.6,-9.49921863900002));
#165933=CARTESIAN_POINT('Ctrl Pts',(4.70973049599994,15.2,-9.50085307000002));
#165934=CARTESIAN_POINT('Ctrl Pts',(4.70973049599994,11.6,-9.50085307000002));
#165935=CARTESIAN_POINT('Ctrl Pts',(4.71107119199994,15.2,-9.50249159800002));
#165936=CARTESIAN_POINT('Ctrl Pts',(4.71107119199994,11.6,-9.50249159800002));
#165937=CARTESIAN_POINT('Ctrl Pts',(4.71241767399994,15.2,-9.50413420300002));
#165938=CARTESIAN_POINT('Ctrl Pts',(4.71241767399994,11.6,-9.50413420300002));
#165939=CARTESIAN_POINT('Ctrl Pts',(4.71376994199994,15.2,-9.50578086900002));
#165940=CARTESIAN_POINT('Ctrl Pts',(4.71376994199994,11.6,-9.50578086900002));
#165941=CARTESIAN_POINT('Ctrl Pts',(4.71512799299994,15.2,-9.50743157700002));
#165942=CARTESIAN_POINT('Ctrl Pts',(4.71512799299994,11.6,-9.50743157700002));
#165943=CARTESIAN_POINT('Ctrl Pts',(4.71649182999994,15.2,-9.50908630800001));
#165944=CARTESIAN_POINT('Ctrl Pts',(4.71649182999994,11.6,-9.50908630800001));
#165945=CARTESIAN_POINT('Ctrl Pts',(4.71786144899994,15.2,-9.51074504700001));
#165946=CARTESIAN_POINT('Ctrl Pts',(4.71786144899994,11.6,-9.51074504700001));
#165947=CARTESIAN_POINT('Ctrl Pts',(4.71923685099994,15.2,-9.51240777300002));
#165948=CARTESIAN_POINT('Ctrl Pts',(4.71923685099994,11.6,-9.51240777300002));
#165949=CARTESIAN_POINT('Ctrl Pts',(4.72061803499994,15.2,-9.51407447200001));
#165950=CARTESIAN_POINT('Ctrl Pts',(4.72061803499994,11.6,-9.51407447200001));
#165951=CARTESIAN_POINT('Ctrl Pts',(4.72200500099994,15.2,-9.51574512200001));
#165952=CARTESIAN_POINT('Ctrl Pts',(4.72200500099994,11.6,-9.51574512200001));
#165953=CARTESIAN_POINT('Ctrl Pts',(4.72339774699994,15.2,-9.51741970900001));
#165954=CARTESIAN_POINT('Ctrl Pts',(4.72339774699994,11.6,-9.51741970900001));
#165955=CARTESIAN_POINT('Ctrl Pts',(4.72479627199994,15.2,-9.51909821400001));
#165956=CARTESIAN_POINT('Ctrl Pts',(4.72479627199994,11.6,-9.51909821400001));
#165957=CARTESIAN_POINT('Ctrl Pts',(4.72620057599995,15.2,-9.52078061900002));
#165958=CARTESIAN_POINT('Ctrl Pts',(4.72620057599995,11.6,-9.52078061900002));
#165959=CARTESIAN_POINT('Ctrl Pts',(4.72761065899994,15.2,-9.52246690800001));
#165960=CARTESIAN_POINT('Ctrl Pts',(4.72761065899994,11.6,-9.52246690800001));
#165961=CARTESIAN_POINT('Ctrl Pts',(4.72902651799994,15.2,-9.52415706400001));
#165962=CARTESIAN_POINT('Ctrl Pts',(4.72902651799994,11.6,-9.52415706400001));
#165963=CARTESIAN_POINT('Ctrl Pts',(4.73044815599994,15.2,-9.52585106600001));
#165964=CARTESIAN_POINT('Ctrl Pts',(4.73044815599994,11.6,-9.52585106600001));
#165965=CARTESIAN_POINT('Ctrl Pts',(4.73187556799994,15.2,-9.52754890000002));
#165966=CARTESIAN_POINT('Ctrl Pts',(4.73187556799994,11.6,-9.52754890000002));
#165967=CARTESIAN_POINT('Ctrl Pts',(4.73330875499994,15.2,-9.52925054800002));
#165968=CARTESIAN_POINT('Ctrl Pts',(4.73330875499994,11.6,-9.52925054800002));
#165969=CARTESIAN_POINT('Ctrl Pts',(4.73474771699994,15.2,-9.53095599300001));
#165970=CARTESIAN_POINT('Ctrl Pts',(4.73474771699994,11.6,-9.53095599300001));
#165971=CARTESIAN_POINT('Ctrl Pts',(4.73619245199994,15.2,-9.53266521700002));
#165972=CARTESIAN_POINT('Ctrl Pts',(4.73619245199994,11.6,-9.53266521700002));
#165973=CARTESIAN_POINT('Ctrl Pts',(4.73764295999994,15.2,-9.53437820500002));
#165974=CARTESIAN_POINT('Ctrl Pts',(4.73764295999994,11.6,-9.53437820500002));
#165975=CARTESIAN_POINT('Ctrl Pts',(4.73909923899994,15.2,-9.53609493800002));
#165976=CARTESIAN_POINT('Ctrl Pts',(4.73909923899994,11.6,-9.53609493800002));
#165977=CARTESIAN_POINT('Ctrl Pts',(4.74056128899994,15.2,-9.53781539900002));
#165978=CARTESIAN_POINT('Ctrl Pts',(4.74056128899994,11.6,-9.53781539900002));
#165979=CARTESIAN_POINT('Ctrl Pts',(4.74202910999994,15.2,-9.53953957200002));
#165980=CARTESIAN_POINT('Ctrl Pts',(4.74202910999994,11.6,-9.53953957200002));
#165981=CARTESIAN_POINT('Ctrl Pts',(4.74350269999994,15.2,-9.54126744100002));
#165982=CARTESIAN_POINT('Ctrl Pts',(4.74350269999994,11.6,-9.54126744100002));
#165983=CARTESIAN_POINT('Ctrl Pts',(4.74498205799994,15.2,-9.54299898700001));
#165984=CARTESIAN_POINT('Ctrl Pts',(4.74498205799994,11.6,-9.54299898700001));
#165985=CARTESIAN_POINT('Ctrl Pts',(4.74646718399994,15.2,-9.54473419300001));
#165986=CARTESIAN_POINT('Ctrl Pts',(4.74646718399994,11.6,-9.54473419300001));
#165987=CARTESIAN_POINT('Ctrl Pts',(4.74795807699994,15.2,-9.54647304600002));
#165988=CARTESIAN_POINT('Ctrl Pts',(4.74795807699994,11.6,-9.54647304600002));
#165989=CARTESIAN_POINT('Ctrl Pts',(4.74945473399994,15.2,-9.54821552600002));
#165990=CARTESIAN_POINT('Ctrl Pts',(4.74945473399994,11.6,-9.54821552600002));
#165991=CARTESIAN_POINT('Ctrl Pts',(4.75095715699994,15.2,-9.54996161800001));
#165992=CARTESIAN_POINT('Ctrl Pts',(4.75095715699994,11.6,-9.54996161800001));
#165993=CARTESIAN_POINT('Ctrl Pts',(4.75246534399994,15.2,-9.55171130300002));
#165994=CARTESIAN_POINT('Ctrl Pts',(4.75246534399994,11.6,-9.55171130300002));
#165995=CARTESIAN_POINT('Ctrl Pts',(4.75397929399994,15.2,-9.55346456800001));
#165996=CARTESIAN_POINT('Ctrl Pts',(4.75397929399994,11.6,-9.55346456800001));
#165997=CARTESIAN_POINT('Ctrl Pts',(4.75549900499994,15.2,-9.55522139300001));
#165998=CARTESIAN_POINT('Ctrl Pts',(4.75549900499994,11.6,-9.55522139300001));
#165999=CARTESIAN_POINT('Ctrl Pts',(4.75702447799994,15.2,-9.55698176500002));
#166000=CARTESIAN_POINT('Ctrl Pts',(4.75702447799994,11.6,-9.55698176500002));
#166001=CARTESIAN_POINT('Ctrl Pts',(4.75855571099994,15.2,-9.55874566600002));
#166002=CARTESIAN_POINT('Ctrl Pts',(4.75855571099994,11.6,-9.55874566600002));
#166003=CARTESIAN_POINT('Ctrl Pts',(4.76009270299994,15.2,-9.56051308000001));
#166004=CARTESIAN_POINT('Ctrl Pts',(4.76009270299994,11.6,-9.56051308000001));
#166005=CARTESIAN_POINT('Ctrl Pts',(4.76163545499994,15.2,-9.56228399000001));
#166006=CARTESIAN_POINT('Ctrl Pts',(4.76163545499994,11.6,-9.56228399000001));
#166007=CARTESIAN_POINT('Ctrl Pts',(4.76318396199994,15.2,-9.56405838000002));
#166008=CARTESIAN_POINT('Ctrl Pts',(4.76318396199994,11.6,-9.56405838000002));
#166009=CARTESIAN_POINT('Ctrl Pts',(4.76473822699994,15.2,-9.56583623400002));
#166010=CARTESIAN_POINT('Ctrl Pts',(4.76473822699994,11.6,-9.56583623400002));
#166011=CARTESIAN_POINT('Ctrl Pts',(4.76629824599994,15.2,-9.56761753600002));
#166012=CARTESIAN_POINT('Ctrl Pts',(4.76629824599994,11.6,-9.56761753600002));
#166013=CARTESIAN_POINT('Ctrl Pts',(4.76786401999994,15.2,-9.56940227100001));
#166014=CARTESIAN_POINT('Ctrl Pts',(4.76786401999994,11.6,-9.56940227100001));
#166015=CARTESIAN_POINT('Ctrl Pts',(4.76943554699994,15.2,-9.57119042200001));
#166016=CARTESIAN_POINT('Ctrl Pts',(4.76943554699994,11.6,-9.57119042200001));
#166017=CARTESIAN_POINT('Ctrl Pts',(4.77101282699994,15.2,-9.57298197200002));
#166018=CARTESIAN_POINT('Ctrl Pts',(4.77101282699994,11.6,-9.57298197200002));
#166019=CARTESIAN_POINT('Ctrl Pts',(4.77259585799994,15.2,-9.57477690600001));
#166020=CARTESIAN_POINT('Ctrl Pts',(4.77259585799994,11.6,-9.57477690600001));
#166021=CARTESIAN_POINT('Ctrl Pts',(4.77418463899994,15.2,-9.57657520900002));
#166022=CARTESIAN_POINT('Ctrl Pts',(4.77418463899994,11.6,-9.57657520900002));
#166023=CARTESIAN_POINT('Ctrl Pts',(4.77577916999994,15.2,-9.57837686300002));
#166024=CARTESIAN_POINT('Ctrl Pts',(4.77577916999994,11.6,-9.57837686300002));
#166025=CARTESIAN_POINT('Ctrl Pts',(4.77737944799994,15.2,-9.58018185500002));
#166026=CARTESIAN_POINT('Ctrl Pts',(4.77737944799994,11.6,-9.58018185500002));
#166027=CARTESIAN_POINT('Ctrl Pts',(4.77898547399994,15.2,-9.58199016600001));
#166028=CARTESIAN_POINT('Ctrl Pts',(4.77898547399994,11.6,-9.58199016600001));
#166029=CARTESIAN_POINT('Ctrl Pts',(4.78059724599994,15.2,-9.58380178400001));
#166030=CARTESIAN_POINT('Ctrl Pts',(4.78059724599994,11.6,-9.58380178400001));
#166031=CARTESIAN_POINT('Ctrl Pts',(4.78221476399994,15.2,-9.58561669000002));
#166032=CARTESIAN_POINT('Ctrl Pts',(4.78221476399994,11.6,-9.58561669000002));
#166033=CARTESIAN_POINT('Ctrl Pts',(4.78383802499994,15.2,-9.58743487100002));
#166034=CARTESIAN_POINT('Ctrl Pts',(4.78383802499994,11.6,-9.58743487100002));
#166035=CARTESIAN_POINT('Ctrl Pts',(4.78546702799994,15.2,-9.58925631000002));
#166036=CARTESIAN_POINT('Ctrl Pts',(4.78546702799994,11.6,-9.58925631000002));
#166037=CARTESIAN_POINT('Ctrl Pts',(4.78710177399994,15.2,-9.59108099200002));
#166038=CARTESIAN_POINT('Ctrl Pts',(4.78710177399994,11.6,-9.59108099200002));
#166039=CARTESIAN_POINT('Ctrl Pts',(4.78874226099994,15.2,-9.59290890100002));
#166040=CARTESIAN_POINT('Ctrl Pts',(4.78874226099994,11.6,-9.59290890100002));
#166041=CARTESIAN_POINT('Ctrl Pts',(4.79038848599994,15.2,-9.59474002200002));
#166042=CARTESIAN_POINT('Ctrl Pts',(4.79038848599994,11.6,-9.59474002200002));
#166043=CARTESIAN_POINT('Ctrl Pts',(4.79204045099995,15.2,-9.59657434000002));
#166044=CARTESIAN_POINT('Ctrl Pts',(4.79204045099995,11.6,-9.59657434000002));
#166045=CARTESIAN_POINT('Ctrl Pts',(4.79369815299994,15.2,-9.59841183800001));
#166046=CARTESIAN_POINT('Ctrl Pts',(4.79369815299994,11.6,-9.59841183800001));
#166047=CARTESIAN_POINT('Ctrl Pts',(4.79536159199994,15.2,-9.60025250200001));
#166048=CARTESIAN_POINT('Ctrl Pts',(4.79536159199994,11.6,-9.60025250200001));
#166049=CARTESIAN_POINT('Ctrl Pts',(4.79703076399994,15.2,-9.60209631800002));
#166050=CARTESIAN_POINT('Ctrl Pts',(4.79703076399994,11.6,-9.60209631800002));
#166051=CARTESIAN_POINT('Ctrl Pts',(4.79870567099994,15.2,-9.60394326800002));
#166052=CARTESIAN_POINT('Ctrl Pts',(4.79870567099994,11.6,-9.60394326800002));
#166053=CARTESIAN_POINT('Ctrl Pts',(4.80038631199994,15.2,-9.60579333900002));
#166054=CARTESIAN_POINT('Ctrl Pts',(4.80038631199994,11.6,-9.60579333900002));
#166055=CARTESIAN_POINT('Ctrl Pts',(4.80207268399994,15.2,-9.60764651500002));
#166056=CARTESIAN_POINT('Ctrl Pts',(4.80207268399994,11.6,-9.60764651500002));
#166057=CARTESIAN_POINT('Ctrl Pts',(4.80376478599994,15.2,-9.60950278000002));
#166058=CARTESIAN_POINT('Ctrl Pts',(4.80376478599994,11.6,-9.60950278000002));
#166059=CARTESIAN_POINT('Ctrl Pts',(4.80546261699994,15.2,-9.61136212100002));
#166060=CARTESIAN_POINT('Ctrl Pts',(4.80546261699994,11.6,-9.61136212100002));
#166061=CARTESIAN_POINT('Ctrl Pts',(4.80716617699994,15.2,-9.61322452200001));
#166062=CARTESIAN_POINT('Ctrl Pts',(4.80716617699994,11.6,-9.61322452200001));
#166063=CARTESIAN_POINT('Ctrl Pts',(4.80887546399994,15.2,-9.61508996800001));
#166064=CARTESIAN_POINT('Ctrl Pts',(4.80887546399994,11.6,-9.61508996800001));
#166065=CARTESIAN_POINT('Ctrl Pts',(4.81059047599994,15.2,-9.61695844400002));
#166066=CARTESIAN_POINT('Ctrl Pts',(4.81059047599994,11.6,-9.61695844400002));
#166067=CARTESIAN_POINT('Ctrl Pts',(4.81231121399994,15.2,-9.61882993500002));
#166068=CARTESIAN_POINT('Ctrl Pts',(4.81231121399994,11.6,-9.61882993500002));
#166069=CARTESIAN_POINT('Ctrl Pts',(4.81403767399994,15.2,-9.62070442600002));
#166070=CARTESIAN_POINT('Ctrl Pts',(4.81403767399994,11.6,-9.62070442600002));
#166071=CARTESIAN_POINT('Ctrl Pts',(4.81576985699994,15.2,-9.62258190400001));
#166072=CARTESIAN_POINT('Ctrl Pts',(4.81576985699994,11.6,-9.62258190400001));
#166073=CARTESIAN_POINT('Ctrl Pts',(4.81750775999994,15.2,-9.62446235200002));
#166074=CARTESIAN_POINT('Ctrl Pts',(4.81750775999994,11.6,-9.62446235200002));
#166075=CARTESIAN_POINT('Ctrl Pts',(4.81925138399994,15.2,-9.62634575600001));
#166076=CARTESIAN_POINT('Ctrl Pts',(4.81925138399994,11.6,-9.62634575600001));
#166077=CARTESIAN_POINT('Ctrl Pts',(4.82100072499994,15.2,-9.62823210100002));
#166078=CARTESIAN_POINT('Ctrl Pts',(4.82100072499994,11.6,-9.62823210100002));
#166079=CARTESIAN_POINT('Ctrl Pts',(4.82275578399994,15.2,-9.63012137400002));
#166080=CARTESIAN_POINT('Ctrl Pts',(4.82275578399994,11.6,-9.63012137400002));
#166081=CARTESIAN_POINT('Ctrl Pts',(4.82451655899994,15.2,-9.63201355900001));
#166082=CARTESIAN_POINT('Ctrl Pts',(4.82451655899994,11.6,-9.63201355900001));
#166083=CARTESIAN_POINT('Ctrl Pts',(4.82628304799994,15.2,-9.63390864100001));
#166084=CARTESIAN_POINT('Ctrl Pts',(4.82628304799994,11.6,-9.63390864100001));
#166085=CARTESIAN_POINT('Ctrl Pts',(4.82805525099994,15.2,-9.63580660800002));
#166086=CARTESIAN_POINT('Ctrl Pts',(4.82805525099994,11.6,-9.63580660800002));
#166087=CARTESIAN_POINT('Ctrl Pts',(4.82983316599994,15.2,-9.63770744200002));
#166088=CARTESIAN_POINT('Ctrl Pts',(4.82983316599994,11.6,-9.63770744200002));
#166089=CARTESIAN_POINT('Ctrl Pts',(4.83161679299994,15.2,-9.63961113100002));
#166090=CARTESIAN_POINT('Ctrl Pts',(4.83161679299994,11.6,-9.63961113100002));
#166091=CARTESIAN_POINT('Ctrl Pts',(4.83340612799994,15.2,-9.64151766000001));
#166092=CARTESIAN_POINT('Ctrl Pts',(4.83340612799994,11.6,-9.64151766000001));
#166093=CARTESIAN_POINT('Ctrl Pts',(4.83520117199994,15.2,-9.64342701400002));
#166094=CARTESIAN_POINT('Ctrl Pts',(4.83520117199994,11.6,-9.64342701400002));
#166095=CARTESIAN_POINT('Ctrl Pts',(4.83700192299994,15.2,-9.64533918000001));
#166096=CARTESIAN_POINT('Ctrl Pts',(4.83700192299994,11.6,-9.64533918000001));
#166097=CARTESIAN_POINT('Ctrl Pts',(4.83880837899994,15.2,-9.64725414200002));
#166098=CARTESIAN_POINT('Ctrl Pts',(4.83880837899994,11.6,-9.64725414200002));
#166099=CARTESIAN_POINT('Ctrl Pts',(4.84062053999994,15.2,-9.64917188800002));
#166100=CARTESIAN_POINT('Ctrl Pts',(4.84062053999994,11.6,-9.64917188800002));
#166101=CARTESIAN_POINT('Ctrl Pts',(4.84243840399994,15.2,-9.65109240200002));
#166102=CARTESIAN_POINT('Ctrl Pts',(4.84243840399994,11.6,-9.65109240200002));
#166103=CARTESIAN_POINT('Ctrl Pts',(4.84426196999994,15.2,-9.65301567000001));
#166104=CARTESIAN_POINT('Ctrl Pts',(4.84426196999994,11.6,-9.65301567000001));
#166105=CARTESIAN_POINT('Ctrl Pts',(4.84609123599994,15.2,-9.65494167900001));
#166106=CARTESIAN_POINT('Ctrl Pts',(4.84609123599994,11.6,-9.65494167900001));
#166107=CARTESIAN_POINT('Ctrl Pts',(4.84792620099994,15.2,-9.65687041400001));
#166108=CARTESIAN_POINT('Ctrl Pts',(4.84792620099994,11.6,-9.65687041400001));
#166109=CARTESIAN_POINT('Ctrl Pts',(4.84976686399994,15.2,-9.65880186000001));
#166110=CARTESIAN_POINT('Ctrl Pts',(4.84976686399994,11.6,-9.65880186000001));
#166111=CARTESIAN_POINT('Ctrl Pts',(4.85161322299994,15.2,-9.66073600600001));
#166112=CARTESIAN_POINT('Ctrl Pts',(4.85161322299994,11.6,-9.66073600600001));
#166113=CARTESIAN_POINT('Ctrl Pts',(4.85346527699994,15.2,-9.66267283500001));
#166114=CARTESIAN_POINT('Ctrl Pts',(4.85346527699994,11.6,-9.66267283500001));
#166115=CARTESIAN_POINT('Ctrl Pts',(4.85532302399994,15.2,-9.66461233400001));
#166116=CARTESIAN_POINT('Ctrl Pts',(4.85532302399994,11.6,-9.66461233400001));
#166117=CARTESIAN_POINT('Ctrl Pts',(4.85718646499994,15.2,-9.66655449000001));
#166118=CARTESIAN_POINT('Ctrl Pts',(4.85718646499994,11.6,-9.66655449000001));
#166119=CARTESIAN_POINT('Ctrl Pts',(4.85905559499994,15.2,-9.66849928700001));
#166120=CARTESIAN_POINT('Ctrl Pts',(4.85905559499994,11.6,-9.66849928700001));
#166121=CARTESIAN_POINT('Ctrl Pts',(4.86093041599994,15.2,-9.67044671400001));
#166122=CARTESIAN_POINT('Ctrl Pts',(4.86093041599994,11.6,-9.67044671400001));
#166123=CARTESIAN_POINT('Ctrl Pts',(4.86281092399994,15.2,-9.67239675600001));
#166124=CARTESIAN_POINT('Ctrl Pts',(4.86281092399994,11.6,-9.67239675600001));
#166125=CARTESIAN_POINT('Ctrl Pts',(4.86469711899994,15.2,-9.67434939900001));
#166126=CARTESIAN_POINT('Ctrl Pts',(4.86469711899994,11.6,-9.67434939900001));
#166127=CARTESIAN_POINT('Ctrl Pts',(4.86658899899994,15.2,-9.67630462800001));
#166128=CARTESIAN_POINT('Ctrl Pts',(4.86658899899994,11.6,-9.67630462800001));
#166129=CARTESIAN_POINT('Ctrl Pts',(4.86848656299994,15.2,-9.67826243200001));
#166130=CARTESIAN_POINT('Ctrl Pts',(4.86848656299994,11.6,-9.67826243200001));
#166131=CARTESIAN_POINT('Ctrl Pts',(4.87038980999994,15.2,-9.68022279600001));
#166132=CARTESIAN_POINT('Ctrl Pts',(4.87038980999994,11.6,-9.68022279600001));
#166133=CARTESIAN_POINT('Ctrl Pts',(4.87229873699994,15.2,-9.68218570600001));
#166134=CARTESIAN_POINT('Ctrl Pts',(4.87229873699994,11.6,-9.68218570600001));
#166135=CARTESIAN_POINT('Ctrl Pts',(4.87421334399994,15.2,-9.68415114900001));
#166136=CARTESIAN_POINT('Ctrl Pts',(4.87421334399994,11.6,-9.68415114900001));
#166137=CARTESIAN_POINT('Ctrl Pts',(4.87613362999994,15.2,-9.68611911100002));
#166138=CARTESIAN_POINT('Ctrl Pts',(4.87613362999994,11.6,-9.68611911100002));
#166139=CARTESIAN_POINT('Ctrl Pts',(4.87805959199994,15.2,-9.68808957900001));
#166140=CARTESIAN_POINT('Ctrl Pts',(4.87805959199994,11.6,-9.68808957900001));
#166141=CARTESIAN_POINT('Ctrl Pts',(4.87999122899994,15.2,-9.69006253800002));
#166142=CARTESIAN_POINT('Ctrl Pts',(4.87999122899994,11.6,-9.69006253800002));
#166143=CARTESIAN_POINT('Ctrl Pts',(4.88192853999994,15.2,-9.69203797700001));
#166144=CARTESIAN_POINT('Ctrl Pts',(4.88192853999994,11.6,-9.69203797700001));
#166145=CARTESIAN_POINT('Ctrl Pts',(4.88387152299994,15.2,-9.69401588200001));
#166146=CARTESIAN_POINT('Ctrl Pts',(4.88387152299994,11.6,-9.69401588200001));
#166147=CARTESIAN_POINT('Ctrl Pts',(4.88582017699994,15.2,-9.69599623800001));
#166148=CARTESIAN_POINT('Ctrl Pts',(4.88582017699994,11.6,-9.69599623800001));
#166149=CARTESIAN_POINT('Ctrl Pts',(4.88777449999994,15.2,-9.69797903400002));
#166150=CARTESIAN_POINT('Ctrl Pts',(4.88777449999994,11.6,-9.69797903400002));
#166151=CARTESIAN_POINT('Ctrl Pts',(4.88973449199994,15.2,-9.69996425500001));
#166152=CARTESIAN_POINT('Ctrl Pts',(4.88973449199994,11.6,-9.69996425500001));
#166153=CARTESIAN_POINT('Ctrl Pts',(4.89170014899994,15.2,-9.70195188700002));
#166154=CARTESIAN_POINT('Ctrl Pts',(4.89170014899994,11.6,-9.70195188700002));
#166155=CARTESIAN_POINT('Ctrl Pts',(4.89367147099994,15.2,-9.70394192000001));
#166156=CARTESIAN_POINT('Ctrl Pts',(4.89367147099994,11.6,-9.70394192000001));
#166157=CARTESIAN_POINT('Ctrl Pts',(4.89564845699994,15.2,-9.70593433700001));
#166158=CARTESIAN_POINT('Ctrl Pts',(4.89564845699994,11.6,-9.70593433700001));
#166159=CARTESIAN_POINT('Ctrl Pts',(4.89763110499994,15.2,-9.70792912700001));
#166160=CARTESIAN_POINT('Ctrl Pts',(4.89763110499994,11.6,-9.70792912700001));
#166161=CARTESIAN_POINT('Ctrl Pts',(4.89961941299994,15.2,-9.70992627700001));
#166162=CARTESIAN_POINT('Ctrl Pts',(4.89961941299994,11.6,-9.70992627700001));
#166163=CARTESIAN_POINT('Ctrl Pts',(4.90161337899994,15.2,-9.71192577200001));
#166164=CARTESIAN_POINT('Ctrl Pts',(4.90161337899994,11.6,-9.71192577200001));
#166165=CARTESIAN_POINT('Ctrl Pts',(4.90361300299994,15.2,-9.71392760200001));
#166166=CARTESIAN_POINT('Ctrl Pts',(4.90361300299994,11.6,-9.71392760200001));
#166167=CARTESIAN_POINT('Ctrl Pts',(4.90561828399994,15.2,-9.71593175000001));
#166168=CARTESIAN_POINT('Ctrl Pts',(4.90561828399994,11.6,-9.71593175000001));
#166169=CARTESIAN_POINT('Ctrl Pts',(4.90762921799994,15.2,-9.71793820800001));
#166170=CARTESIAN_POINT('Ctrl Pts',(4.90762921799994,11.6,-9.71793820800001));
#166171=CARTESIAN_POINT('Ctrl Pts',(4.90964580399994,15.2,-9.71994695800001));
#166172=CARTESIAN_POINT('Ctrl Pts',(4.90964580399994,11.6,-9.71994695800001));
#166173=CARTESIAN_POINT('Ctrl Pts',(4.91166804199994,15.2,-9.72195799000001));
#166174=CARTESIAN_POINT('Ctrl Pts',(4.91166804199994,11.6,-9.72195799000001));
#166175=CARTESIAN_POINT('Ctrl Pts',(4.91369592899994,15.2,-9.72397129100001));
#166176=CARTESIAN_POINT('Ctrl Pts',(4.91369592899994,11.6,-9.72397129100001));
#166177=CARTESIAN_POINT('Ctrl Pts',(4.91572946499994,15.2,-9.72598684700001));
#166178=CARTESIAN_POINT('Ctrl Pts',(4.91572946499994,11.6,-9.72598684700001));
#166179=CARTESIAN_POINT('Ctrl Pts',(4.91776864699994,15.2,-9.72800464600001));
#166180=CARTESIAN_POINT('Ctrl Pts',(4.91776864699994,11.6,-9.72800464600001));
#166181=CARTESIAN_POINT('Ctrl Pts',(4.91981347399994,15.2,-9.73002467500001));
#166182=CARTESIAN_POINT('Ctrl Pts',(4.91981347399994,11.6,-9.73002467500001));
#166183=CARTESIAN_POINT('Ctrl Pts',(4.92186394399994,15.2,-9.73204692000001));
#166184=CARTESIAN_POINT('Ctrl Pts',(4.92186394399994,11.6,-9.73204692000001));
#166185=CARTESIAN_POINT('Ctrl Pts',(4.92392005599994,15.2,-9.73407137100001));
#166186=CARTESIAN_POINT('Ctrl Pts',(4.92392005599994,11.6,-9.73407137100001));
#166187=CARTESIAN_POINT('Ctrl Pts',(4.92598180799994,15.2,-9.73609801300001));
#166188=CARTESIAN_POINT('Ctrl Pts',(4.92598180799994,11.6,-9.73609801300001));
#166189=CARTESIAN_POINT('Ctrl Pts',(4.92804919799995,15.2,-9.73812683200001));
#166190=CARTESIAN_POINT('Ctrl Pts',(4.92804919799995,11.6,-9.73812683200001));
#166191=CARTESIAN_POINT('Ctrl Pts',(4.93012222499994,15.2,-9.74015782000001));
#166192=CARTESIAN_POINT('Ctrl Pts',(4.93012222499994,11.6,-9.74015782000001));
#166193=CARTESIAN_POINT('Ctrl Pts',(4.93220088799994,15.2,-9.74219096100001));
#166194=CARTESIAN_POINT('Ctrl Pts',(4.93220088799994,11.6,-9.74219096100001));
#166195=CARTESIAN_POINT('Ctrl Pts',(4.93428518399994,15.2,-9.74422624200001));
#166196=CARTESIAN_POINT('Ctrl Pts',(4.93428518399994,11.6,-9.74422624200001));
#166197=CARTESIAN_POINT('Ctrl Pts',(4.93637511199994,15.2,-9.74626365200001));
#166198=CARTESIAN_POINT('Ctrl Pts',(4.93637511199994,11.6,-9.74626365200001));
#166199=CARTESIAN_POINT('Ctrl Pts',(4.93847067099994,15.2,-9.74830317800001));
#166200=CARTESIAN_POINT('Ctrl Pts',(4.93847067099994,11.6,-9.74830317800001));
#166201=CARTESIAN_POINT('Ctrl Pts',(4.94057185799994,15.2,-9.75034480800001));
#166202=CARTESIAN_POINT('Ctrl Pts',(4.94057185799994,11.6,-9.75034480800001));
#166203=CARTESIAN_POINT('Ctrl Pts',(4.94267867199994,15.2,-9.75238852900001));
#166204=CARTESIAN_POINT('Ctrl Pts',(4.94267867199994,11.6,-9.75238852900001));
#166205=CARTESIAN_POINT('Ctrl Pts',(4.94479111299994,15.2,-9.75443432800001));
#166206=CARTESIAN_POINT('Ctrl Pts',(4.94479111299994,11.6,-9.75443432800001));
#166207=CARTESIAN_POINT('Ctrl Pts',(4.94690917699994,15.2,-9.75648219400002));
#166208=CARTESIAN_POINT('Ctrl Pts',(4.94690917699994,11.6,-9.75648219400002));
#166209=CARTESIAN_POINT('Ctrl Pts',(4.94903286299994,15.2,-9.75853211300001));
#166210=CARTESIAN_POINT('Ctrl Pts',(4.94903286299994,11.6,-9.75853211300001));
#166211=CARTESIAN_POINT('Ctrl Pts',(4.95116216899994,15.2,-9.76058407400001));
#166212=CARTESIAN_POINT('Ctrl Pts',(4.95116216899994,11.6,-9.76058407400001));
#166213=CARTESIAN_POINT('Ctrl Pts',(4.95329709499994,15.2,-9.76263806400001));
#166214=CARTESIAN_POINT('Ctrl Pts',(4.95329709499994,11.6,-9.76263806400001));
#166215=CARTESIAN_POINT('Ctrl Pts',(4.95543763799994,15.2,-9.76469407000001));
#166216=CARTESIAN_POINT('Ctrl Pts',(4.95543763799994,11.6,-9.76469407000001));
#166217=CARTESIAN_POINT('Ctrl Pts',(4.95758379699994,15.2,-9.76675208100001));
#166218=CARTESIAN_POINT('Ctrl Pts',(4.95758379699994,11.6,-9.76675208100001));
#166219=CARTESIAN_POINT('Ctrl Pts',(4.95973556799994,15.2,-9.76881208600001));
#166220=CARTESIAN_POINT('Ctrl Pts',(4.95973556799994,11.6,-9.76881208600001));
#166221=CARTESIAN_POINT('Ctrl Pts',(4.96189295299994,15.2,-9.77087406900001));
#166222=CARTESIAN_POINT('Ctrl Pts',(4.96189295299994,11.6,-9.77087406900001));
#166223=CARTESIAN_POINT('Ctrl Pts',(4.96405594799994,15.2,-9.77293802000001));
#166224=CARTESIAN_POINT('Ctrl Pts',(4.96405594799994,11.6,-9.77293802000001));
#166225=CARTESIAN_POINT('Ctrl Pts',(4.96622455099994,15.2,-9.77500392900001));
#166226=CARTESIAN_POINT('Ctrl Pts',(4.96622455099994,11.6,-9.77500392900001));
#166227=CARTESIAN_POINT('Ctrl Pts',(4.96839876099994,15.2,-9.77707177900001));
#166228=CARTESIAN_POINT('Ctrl Pts',(4.96839876099994,11.6,-9.77707177900001));
#166229=CARTESIAN_POINT('Ctrl Pts',(4.97057857799994,15.2,-9.77914156200001));
#166230=CARTESIAN_POINT('Ctrl Pts',(4.97057857799994,11.6,-9.77914156200001));
#166231=CARTESIAN_POINT('Ctrl Pts',(4.97276399699994,15.2,-9.78121326400001));
#166232=CARTESIAN_POINT('Ctrl Pts',(4.97276399699994,11.6,-9.78121326400001));
#166233=CARTESIAN_POINT('Ctrl Pts',(4.97495501799994,15.2,-9.78328687400001));
#166234=CARTESIAN_POINT('Ctrl Pts',(4.97495501799994,11.6,-9.78328687400001));
#166235=CARTESIAN_POINT('Ctrl Pts',(4.97715163999994,15.2,-9.78536237900001));
#166236=CARTESIAN_POINT('Ctrl Pts',(4.97715163999994,11.6,-9.78536237900001));
#166237=CARTESIAN_POINT('Ctrl Pts',(4.97935386099994,15.2,-9.78743976800001));
#166238=CARTESIAN_POINT('Ctrl Pts',(4.97935386099994,11.6,-9.78743976800001));
#166239=CARTESIAN_POINT('Ctrl Pts',(4.98156167699994,15.2,-9.78951902800001));
#166240=CARTESIAN_POINT('Ctrl Pts',(4.98156167699994,11.6,-9.78951902800001));
#166241=CARTESIAN_POINT('Ctrl Pts',(4.98377508799994,15.2,-9.79160014900001));
#166242=CARTESIAN_POINT('Ctrl Pts',(4.98377508799994,11.6,-9.79160014900001));
#166243=CARTESIAN_POINT('Ctrl Pts',(4.98599409399994,15.2,-9.79368311700001));
#166244=CARTESIAN_POINT('Ctrl Pts',(4.98599409399994,11.6,-9.79368311700001));
#166245=CARTESIAN_POINT('Ctrl Pts',(4.98821868999994,15.2,-9.79576792000001));
#166246=CARTESIAN_POINT('Ctrl Pts',(4.98821868999994,11.6,-9.79576792000001));
#166247=CARTESIAN_POINT('Ctrl Pts',(4.99044887699994,15.2,-9.79785454800002));
#166248=CARTESIAN_POINT('Ctrl Pts',(4.99044887699994,11.6,-9.79785454800002));
#166249=CARTESIAN_POINT('Ctrl Pts',(4.99268465099994,15.2,-9.79994298800001));
#166250=CARTESIAN_POINT('Ctrl Pts',(4.99268465099994,11.6,-9.79994298800001));
#166251=CARTESIAN_POINT('Ctrl Pts',(4.99492601099994,15.2,-9.80203322800001));
#166252=CARTESIAN_POINT('Ctrl Pts',(4.99492601099994,11.6,-9.80203322800001));
#166253=CARTESIAN_POINT('Ctrl Pts',(4.99717295499994,15.2,-9.80412525800001));
#166254=CARTESIAN_POINT('Ctrl Pts',(4.99717295499994,11.6,-9.80412525800001));
#166255=CARTESIAN_POINT('Ctrl Pts',(4.99942548199994,15.2,-9.80621906400001));
#166256=CARTESIAN_POINT('Ctrl Pts',(4.99942548199994,11.6,-9.80621906400001));
#166257=CARTESIAN_POINT('Ctrl Pts',(5.00168359099994,15.2,-9.80831463600001));
#166258=CARTESIAN_POINT('Ctrl Pts',(5.00168359099994,11.6,-9.80831463600001));
#166259=CARTESIAN_POINT('Ctrl Pts',(5.00394727799994,15.2,-9.81041196200001));
#166260=CARTESIAN_POINT('Ctrl Pts',(5.00394727799994,11.6,-9.81041196200001));
#166261=CARTESIAN_POINT('Ctrl Pts',(5.00621654199994,15.2,-9.81251102900002));
#166262=CARTESIAN_POINT('Ctrl Pts',(5.00621654199994,11.6,-9.81251102900002));
#166263=CARTESIAN_POINT('Ctrl Pts',(5.00849138299994,15.2,-9.81461182600001));
#166264=CARTESIAN_POINT('Ctrl Pts',(5.00849138299994,11.6,-9.81461182600001));
#166265=CARTESIAN_POINT('Ctrl Pts',(5.01077179499994,15.2,-9.81671434300001));
#166266=CARTESIAN_POINT('Ctrl Pts',(5.01077179499994,11.6,-9.81671434300001));
#166267=CARTESIAN_POINT('Ctrl Pts',(5.01305778099994,15.2,-9.81881856700001));
#166268=CARTESIAN_POINT('Ctrl Pts',(5.01305778099994,11.6,-9.81881856700001));
#166269=CARTESIAN_POINT('Ctrl Pts',(5.01534933699994,15.2,-9.82092448700001));
#166270=CARTESIAN_POINT('Ctrl Pts',(5.01534933699994,11.6,-9.82092448700001));
#166271=CARTESIAN_POINT('Ctrl Pts',(5.01764645999994,15.2,-9.82303209000001));
#166272=CARTESIAN_POINT('Ctrl Pts',(5.01764645999994,11.6,-9.82303209000001));
#166273=CARTESIAN_POINT('Ctrl Pts',(5.01994914999995,15.2,-9.82514136700001));
#166274=CARTESIAN_POINT('Ctrl Pts',(5.01994914999995,11.6,-9.82514136700001));
#166275=CARTESIAN_POINT('Ctrl Pts',(5.02225740499994,15.2,-9.82725230400001));
#166276=CARTESIAN_POINT('Ctrl Pts',(5.02225740499994,11.6,-9.82725230400001));
#166277=CARTESIAN_POINT('Ctrl Pts',(5.02457122199995,15.2,-9.82936489100001));
#166278=CARTESIAN_POINT('Ctrl Pts',(5.02457122199995,11.6,-9.82936489100001));
#166279=CARTESIAN_POINT('Ctrl Pts',(5.02689059999994,15.2,-9.83147911700001));
#166280=CARTESIAN_POINT('Ctrl Pts',(5.02689059999994,11.6,-9.83147911700001));
#166281=CARTESIAN_POINT('Ctrl Pts',(5.02921553699994,15.2,-9.83359496900001));
#166282=CARTESIAN_POINT('Ctrl Pts',(5.02921553699994,11.6,-9.83359496900001));
#166283=CARTESIAN_POINT('Ctrl Pts',(5.03154603199994,15.2,-9.83571243800001));
#166284=CARTESIAN_POINT('Ctrl Pts',(5.03154603199994,11.6,-9.83571243800001));
#166285=CARTESIAN_POINT('Ctrl Pts',(5.03388208199994,15.2,-9.83783151100001));
#166286=CARTESIAN_POINT('Ctrl Pts',(5.03388208199994,11.6,-9.83783151100001));
#166287=CARTESIAN_POINT('Ctrl Pts',(5.03622368499994,15.2,-9.83995217600001));
#166288=CARTESIAN_POINT('Ctrl Pts',(5.03622368499994,11.6,-9.83995217600001));
#166289=CARTESIAN_POINT('Ctrl Pts',(5.03857083999994,15.2,-9.84207442400001));
#166290=CARTESIAN_POINT('Ctrl Pts',(5.03857083999994,11.6,-9.84207442400001));
#166291=CARTESIAN_POINT('Ctrl Pts',(5.04092354399994,15.2,-9.84419824200001));
#166292=CARTESIAN_POINT('Ctrl Pts',(5.04092354399994,11.6,-9.84419824200001));
#166293=CARTESIAN_POINT('Ctrl Pts',(5.04328179699994,15.2,-9.84632361900001));
#166294=CARTESIAN_POINT('Ctrl Pts',(5.04328179699994,11.6,-9.84632361900001));
#166295=CARTESIAN_POINT('Ctrl Pts',(5.04564559499994,15.2,-9.84845054500001));
#166296=CARTESIAN_POINT('Ctrl Pts',(5.04564559499994,11.6,-9.84845054500001));
#166297=CARTESIAN_POINT('Ctrl Pts',(5.04801493799994,15.2,-9.85057900700001));
#166298=CARTESIAN_POINT('Ctrl Pts',(5.04801493799994,11.6,-9.85057900700001));
#166299=CARTESIAN_POINT('Ctrl Pts',(5.05038982199994,15.2,-9.85270899400001));
#166300=CARTESIAN_POINT('Ctrl Pts',(5.05038982199994,11.6,-9.85270899400001));
#166301=CARTESIAN_POINT('Ctrl Pts',(5.05277024799994,15.2,-9.85484049700001));
#166302=CARTESIAN_POINT('Ctrl Pts',(5.05277024799994,11.6,-9.85484049700001));
#166303=CARTESIAN_POINT('Ctrl Pts',(5.05515621199994,15.2,-9.85697350200001));
#166304=CARTESIAN_POINT('Ctrl Pts',(5.05515621199994,11.6,-9.85697350200001));
#166305=CARTESIAN_POINT('Ctrl Pts',(5.05754771099994,15.2,-9.85910800100001));
#166306=CARTESIAN_POINT('Ctrl Pts',(5.05754771099994,11.6,-9.85910800100001));
#166307=CARTESIAN_POINT('Ctrl Pts',(5.05994474599994,15.2,-9.86124398100001));
#166308=CARTESIAN_POINT('Ctrl Pts',(5.05994474599994,11.6,-9.86124398100001));
#166309=CARTESIAN_POINT('Ctrl Pts',(5.06234731399994,15.2,-9.86338143100001));
#166310=CARTESIAN_POINT('Ctrl Pts',(5.06234731399994,11.6,-9.86338143100001));
#166311=CARTESIAN_POINT('Ctrl Pts',(5.06475541199994,15.2,-9.86552034000001));
#166312=CARTESIAN_POINT('Ctrl Pts',(5.06475541199994,11.6,-9.86552034000001));
#166313=CARTESIAN_POINT('Ctrl Pts',(5.06716903899994,15.2,-9.86766069800001));
#166314=CARTESIAN_POINT('Ctrl Pts',(5.06716903899994,11.6,-9.86766069800001));
#166315=CARTESIAN_POINT('Ctrl Pts',(5.06958819299994,15.2,-9.86980249300001));
#166316=CARTESIAN_POINT('Ctrl Pts',(5.06958819299994,11.6,-9.86980249300001));
#166317=CARTESIAN_POINT('Ctrl Pts',(5.07201287199995,15.2,-9.87194571400001));
#166318=CARTESIAN_POINT('Ctrl Pts',(5.07201287199995,11.6,-9.87194571400001));
#166319=CARTESIAN_POINT('Ctrl Pts',(5.07444307399994,15.2,-9.87409035100001));
#166320=CARTESIAN_POINT('Ctrl Pts',(5.07444307399994,11.6,-9.87409035100001));
#166321=CARTESIAN_POINT('Ctrl Pts',(5.07687879599994,15.2,-9.87623639300001));
#166322=CARTESIAN_POINT('Ctrl Pts',(5.07687879599994,11.6,-9.87623639300001));
#166323=CARTESIAN_POINT('Ctrl Pts',(5.07932003899994,15.2,-9.87838382800001));
#166324=CARTESIAN_POINT('Ctrl Pts',(5.07932003899994,11.6,-9.87838382800001));
#166325=CARTESIAN_POINT('Ctrl Pts',(5.08176679799995,15.2,-9.88053264700001));
#166326=CARTESIAN_POINT('Ctrl Pts',(5.08176679799995,11.6,-9.88053264700001));
#166327=CARTESIAN_POINT('Ctrl Pts',(5.08421907399994,15.2,-9.88268283800001));
#166328=CARTESIAN_POINT('Ctrl Pts',(5.08421907399994,11.6,-9.88268283800001));
#166329=CARTESIAN_POINT('Ctrl Pts',(5.08667686199994,15.2,-9.88483438900001));
#166330=CARTESIAN_POINT('Ctrl Pts',(5.08667686199994,11.6,-9.88483438900001));
#166331=CARTESIAN_POINT('Ctrl Pts',(5.08914016199994,15.2,-9.88698729200001));
#166332=CARTESIAN_POINT('Ctrl Pts',(5.08914016199994,11.6,-9.88698729200001));
#166333=CARTESIAN_POINT('Ctrl Pts',(5.09160897099994,15.2,-9.88914153400001));
#166334=CARTESIAN_POINT('Ctrl Pts',(5.09160897099994,11.6,-9.88914153400001));
#166335=CARTESIAN_POINT('Ctrl Pts',(5.09408328699994,15.2,-9.89129710500001));
#166336=CARTESIAN_POINT('Ctrl Pts',(5.09408328699994,11.6,-9.89129710500001));
#166337=CARTESIAN_POINT('Ctrl Pts',(5.09656310899994,15.2,-9.89345399400001));
#166338=CARTESIAN_POINT('Ctrl Pts',(5.09656310899994,11.6,-9.89345399400001));
#166339=CARTESIAN_POINT('Ctrl Pts',(5.09904843499994,15.2,-9.89561219200001));
#166340=CARTESIAN_POINT('Ctrl Pts',(5.09904843499994,11.6,-9.89561219200001));
#166341=CARTESIAN_POINT('Ctrl Pts',(5.10153926199994,15.2,-9.89777168700001));
#166342=CARTESIAN_POINT('Ctrl Pts',(5.10153926199994,11.6,-9.89777168700001));
#166343=CARTESIAN_POINT('Ctrl Pts',(5.10403558799994,15.2,-9.89993246800001));
#166344=CARTESIAN_POINT('Ctrl Pts',(5.10403558799994,11.6,-9.89993246800001));
#166345=CARTESIAN_POINT('Ctrl Pts',(5.10653741199994,15.2,-9.90209452500001));
#166346=CARTESIAN_POINT('Ctrl Pts',(5.10653741199994,11.6,-9.90209452500001));
#166347=CARTESIAN_POINT('Ctrl Pts',(5.10904473099994,15.2,-9.90425784600001));
#166348=CARTESIAN_POINT('Ctrl Pts',(5.10904473099994,11.6,-9.90425784600001));
#166349=CARTESIAN_POINT('Ctrl Pts',(5.11155754399994,15.2,-9.90642242300001));
#166350=CARTESIAN_POINT('Ctrl Pts',(5.11155754399994,11.6,-9.90642242300001));
#166351=CARTESIAN_POINT('Ctrl Pts',(5.11407584799994,15.2,-9.90858824500001));
#166352=CARTESIAN_POINT('Ctrl Pts',(5.11407584799994,11.6,-9.90858824500001));
#166353=CARTESIAN_POINT('Ctrl Pts',(5.11659964299994,15.2,-9.91075529900001));
#166354=CARTESIAN_POINT('Ctrl Pts',(5.11659964299994,11.6,-9.91075529900001));
#166355=CARTESIAN_POINT('Ctrl Pts',(5.11912892399994,15.2,-9.91292357700001));
#166356=CARTESIAN_POINT('Ctrl Pts',(5.11912892399994,11.6,-9.91292357700001));
#166357=CARTESIAN_POINT('Ctrl Pts',(5.12166368999995,15.2,-9.91509306700001));
#166358=CARTESIAN_POINT('Ctrl Pts',(5.12166368999995,11.6,-9.91509306700001));
#166359=CARTESIAN_POINT('Ctrl Pts',(5.12420394099994,15.2,-9.91726376000001));
#166360=CARTESIAN_POINT('Ctrl Pts',(5.12420394099994,11.6,-9.91726376000001));
#166361=CARTESIAN_POINT('Ctrl Pts',(5.12674967199994,15.2,-9.91943564400001));
#166362=CARTESIAN_POINT('Ctrl Pts',(5.12674967199994,11.6,-9.91943564400001));
#166363=CARTESIAN_POINT('Ctrl Pts',(5.12930088299994,15.2,-9.92160871000001));
#166364=CARTESIAN_POINT('Ctrl Pts',(5.12930088299994,11.6,-9.92160871000001));
#166365=CARTESIAN_POINT('Ctrl Pts',(5.13185757099994,15.2,-9.92378294700002));
#166366=CARTESIAN_POINT('Ctrl Pts',(5.13185757099994,11.6,-9.92378294700002));
#166367=CARTESIAN_POINT('Ctrl Pts',(5.13441973599994,15.2,-9.92595834500001));
#166368=CARTESIAN_POINT('Ctrl Pts',(5.13441973599994,11.6,-9.92595834500001));
#166369=CARTESIAN_POINT('Ctrl Pts',(5.13698737199995,15.2,-9.92813489200001));
#166370=CARTESIAN_POINT('Ctrl Pts',(5.13698737199995,11.6,-9.92813489200001));
#166371=CARTESIAN_POINT('Ctrl Pts',(5.13956047999995,15.2,-9.93031258000001));
#166372=CARTESIAN_POINT('Ctrl Pts',(5.13956047999995,11.6,-9.93031258000001));
#166373=CARTESIAN_POINT('Ctrl Pts',(5.14213905699994,15.2,-9.93249139700001));
#166374=CARTESIAN_POINT('Ctrl Pts',(5.14213905699994,11.6,-9.93249139700001));
#166375=CARTESIAN_POINT('Ctrl Pts',(5.14472310199994,15.2,-9.93467133400001));
#166376=CARTESIAN_POINT('Ctrl Pts',(5.14472310199994,11.6,-9.93467133400001));
#166377=CARTESIAN_POINT('Ctrl Pts',(5.14731261099994,15.2,-9.93685238100001));
#166378=CARTESIAN_POINT('Ctrl Pts',(5.14731261099994,11.6,-9.93685238100001));
#166379=CARTESIAN_POINT('Ctrl Pts',(5.14990758299994,15.2,-9.93903452600001));
#166380=CARTESIAN_POINT('Ctrl Pts',(5.14990758299994,11.6,-9.93903452600001));
#166381=CARTESIAN_POINT('Ctrl Pts',(5.15250801599994,15.2,-9.94121776100001));
#166382=CARTESIAN_POINT('Ctrl Pts',(5.15250801599994,11.6,-9.94121776100001));
#166383=CARTESIAN_POINT('Ctrl Pts',(5.15511390699994,15.2,-9.94340207300001));
#166384=CARTESIAN_POINT('Ctrl Pts',(5.15511390699994,11.6,-9.94340207300001));
#166385=CARTESIAN_POINT('Ctrl Pts',(5.15772525599994,15.2,-9.94558745400001));
#166386=CARTESIAN_POINT('Ctrl Pts',(5.15772525599994,11.6,-9.94558745400001));
#166387=CARTESIAN_POINT('Ctrl Pts',(5.16034205999994,15.2,-9.94777389300001));
#166388=CARTESIAN_POINT('Ctrl Pts',(5.16034205999994,11.6,-9.94777389300001));
#166389=CARTESIAN_POINT('Ctrl Pts',(5.16296431499994,15.2,-9.94996138100001));
#166390=CARTESIAN_POINT('Ctrl Pts',(5.16296431499994,11.6,-9.94996138100001));
#166391=CARTESIAN_POINT('Ctrl Pts',(5.16559202199994,15.2,-9.95214990500001));
#166392=CARTESIAN_POINT('Ctrl Pts',(5.16559202199994,11.6,-9.95214990500001));
#166393=CARTESIAN_POINT('Ctrl Pts',(5.16822517599994,15.2,-9.95433945900001));
#166394=CARTESIAN_POINT('Ctrl Pts',(5.16822517599994,11.6,-9.95433945900001));
#166395=CARTESIAN_POINT('Ctrl Pts',(5.17086377599994,15.2,-9.95653003000001));
#166396=CARTESIAN_POINT('Ctrl Pts',(5.17086377599994,11.6,-9.95653003000001));
#166397=CARTESIAN_POINT('Ctrl Pts',(5.17350782199994,15.2,-9.95872160800001));
#166398=CARTESIAN_POINT('Ctrl Pts',(5.17350782199994,11.6,-9.95872160800001));
#166399=CARTESIAN_POINT('Ctrl Pts',(5.17615730899994,15.2,-9.96091418600001));
#166400=CARTESIAN_POINT('Ctrl Pts',(5.17615730899994,11.6,-9.96091418600001));
#166401=CARTESIAN_POINT('Ctrl Pts',(5.17881223599994,15.2,-9.96310775100001));
#166402=CARTESIAN_POINT('Ctrl Pts',(5.17881223599994,11.6,-9.96310775100001));
#166403=CARTESIAN_POINT('Ctrl Pts',(5.18147259999994,15.2,-9.96530229200001));
#166404=CARTESIAN_POINT('Ctrl Pts',(5.18147259999994,11.6,-9.96530229200001));
#166405=CARTESIAN_POINT('Ctrl Pts',(5.18413840099995,15.2,-9.96749780400001));
#166406=CARTESIAN_POINT('Ctrl Pts',(5.18413840099995,11.6,-9.96749780400001));
#166407=CARTESIAN_POINT('Ctrl Pts',(5.18680963499994,15.2,-9.96969427100001));
#166408=CARTESIAN_POINT('Ctrl Pts',(5.18680963499994,11.6,-9.96969427100001));
#166409=CARTESIAN_POINT('Ctrl Pts',(5.18948629999994,15.2,-9.97189168800001));
#166410=CARTESIAN_POINT('Ctrl Pts',(5.18948629999994,11.6,-9.97189168800001));
#166411=CARTESIAN_POINT('Ctrl Pts',(5.19216839499994,15.2,-9.97409004200001));
#166412=CARTESIAN_POINT('Ctrl Pts',(5.19216839499994,11.6,-9.97409004200001));
#166413=CARTESIAN_POINT('Ctrl Pts',(5.19485591699994,15.2,-9.97628932500001));
#166414=CARTESIAN_POINT('Ctrl Pts',(5.19485591699994,11.6,-9.97628932500001));
#166415=CARTESIAN_POINT('Ctrl Pts',(5.19754886399994,15.2,-9.97848952600001));
#166416=CARTESIAN_POINT('Ctrl Pts',(5.19754886399994,11.6,-9.97848952600001));
#166417=CARTESIAN_POINT('Ctrl Pts',(5.20024723299994,15.2,-9.98069063500001));
#166418=CARTESIAN_POINT('Ctrl Pts',(5.20024723299994,11.6,-9.98069063500001));
#166419=CARTESIAN_POINT('Ctrl Pts',(5.20295102399994,15.2,-9.98289264400001));
#166420=CARTESIAN_POINT('Ctrl Pts',(5.20295102399994,11.6,-9.98289264400001));
#166421=CARTESIAN_POINT('Ctrl Pts',(5.20566023399994,15.2,-9.98509554200002));
#166422=CARTESIAN_POINT('Ctrl Pts',(5.20566023399994,11.6,-9.98509554200002));
#166423=CARTESIAN_POINT('Ctrl Pts',(5.20837485899994,15.2,-9.98729931800001));
#166424=CARTESIAN_POINT('Ctrl Pts',(5.20837485899994,11.6,-9.98729931800001));
#166425=CARTESIAN_POINT('Ctrl Pts',(5.21109489899994,15.2,-9.98950396400001));
#166426=CARTESIAN_POINT('Ctrl Pts',(5.21109489899994,11.6,-9.98950396400001));
#166427=CARTESIAN_POINT('Ctrl Pts',(5.21382035099994,15.2,-9.99170947000001));
#166428=CARTESIAN_POINT('Ctrl Pts',(5.21382035099994,11.6,-9.99170947000001));
#166429=CARTESIAN_POINT('Ctrl Pts',(5.21655121299994,15.2,-9.99391582500001));
#166430=CARTESIAN_POINT('Ctrl Pts',(5.21655121299994,11.6,-9.99391582500001));
#166431=CARTESIAN_POINT('Ctrl Pts',(5.21928748199994,15.2,-9.99612302200001));
#166432=CARTESIAN_POINT('Ctrl Pts',(5.21928748199994,11.6,-9.99612302200001));
#166433=CARTESIAN_POINT('Ctrl Pts',(5.22202915799994,15.2,-9.99833104900001));
#166434=CARTESIAN_POINT('Ctrl Pts',(5.22202915799994,11.6,-9.99833104900001));
#166435=CARTESIAN_POINT('Ctrl Pts',(5.22477623599994,15.2,-10.000539896));
#166436=CARTESIAN_POINT('Ctrl Pts',(5.22477623599994,11.6,-10.000539896));
#166437=CARTESIAN_POINT('Ctrl Pts',(5.22752871599994,15.2,-10.002749554));
#166438=CARTESIAN_POINT('Ctrl Pts',(5.22752871599994,11.6,-10.002749554));
#166439=CARTESIAN_POINT('Ctrl Pts',(5.23028659499994,15.2,-10.004960015));
#166440=CARTESIAN_POINT('Ctrl Pts',(5.23028659499994,11.6,-10.004960015));
#166441=CARTESIAN_POINT('Ctrl Pts',(5.23304987099994,15.2,-10.007171267));
#166442=CARTESIAN_POINT('Ctrl Pts',(5.23304987099994,11.6,-10.007171267));
#166443=CARTESIAN_POINT('Ctrl Pts',(5.23581854099994,15.2,-10.009383302));
#166444=CARTESIAN_POINT('Ctrl Pts',(5.23581854099994,11.6,-10.009383302));
#166445=CARTESIAN_POINT('Ctrl Pts',(5.23859260399994,15.2,-10.01159611));
#166446=CARTESIAN_POINT('Ctrl Pts',(5.23859260399994,11.6,-10.01159611));
#166447=CARTESIAN_POINT('Ctrl Pts',(5.24137205699994,15.2,-10.013809682));
#166448=CARTESIAN_POINT('Ctrl Pts',(5.24137205699994,11.6,-10.013809682));
#166449=CARTESIAN_POINT('Ctrl Pts',(5.24415689799994,15.2,-10.016024008));
#166450=CARTESIAN_POINT('Ctrl Pts',(5.24415689799994,11.6,-10.016024008));
#166451=CARTESIAN_POINT('Ctrl Pts',(5.24694712499994,15.2,-10.018239077));
#166452=CARTESIAN_POINT('Ctrl Pts',(5.24694712499994,11.6,-10.018239077));
#166453=CARTESIAN_POINT('Ctrl Pts',(5.24974273599994,15.2,-10.020454881));
#166454=CARTESIAN_POINT('Ctrl Pts',(5.24974273599994,11.6,-10.020454881));
#166455=CARTESIAN_POINT('Ctrl Pts',(5.25254372799994,15.2,-10.022671411));
#166456=CARTESIAN_POINT('Ctrl Pts',(5.25254372799994,11.6,-10.022671411));
#166457=CARTESIAN_POINT('Ctrl Pts',(5.25535009899994,15.2,-10.024888657));
#166458=CARTESIAN_POINT('Ctrl Pts',(5.25535009899994,11.6,-10.024888657));
#166459=CARTESIAN_POINT('Ctrl Pts',(5.25816184699995,15.2,-10.02710661));
#166460=CARTESIAN_POINT('Ctrl Pts',(5.25816184699995,11.6,-10.02710661));
#166461=CARTESIAN_POINT('Ctrl Pts',(5.26097896999994,15.2,-10.029325259));
#166462=CARTESIAN_POINT('Ctrl Pts',(5.26097896999994,11.6,-10.029325259));
#166463=CARTESIAN_POINT('Ctrl Pts',(5.26380146599994,15.2,-10.031544597));
#166464=CARTESIAN_POINT('Ctrl Pts',(5.26380146599994,11.6,-10.031544597));
#166465=CARTESIAN_POINT('Ctrl Pts',(5.26662933099994,15.2,-10.033764612));
#166466=CARTESIAN_POINT('Ctrl Pts',(5.26662933099994,11.6,-10.033764612));
#166467=CARTESIAN_POINT('Ctrl Pts',(5.26946256499994,15.2,-10.035985297));
#166468=CARTESIAN_POINT('Ctrl Pts',(5.26946256499994,11.6,-10.035985297));
#166469=CARTESIAN_POINT('Ctrl Pts',(5.27230116399994,15.2,-10.038206641));
#166470=CARTESIAN_POINT('Ctrl Pts',(5.27230116399994,11.6,-10.038206641));
#166471=CARTESIAN_POINT('Ctrl Pts',(5.27514512699994,15.2,-10.040428636));
#166472=CARTESIAN_POINT('Ctrl Pts',(5.27514512699994,11.6,-10.040428636));
#166473=CARTESIAN_POINT('Ctrl Pts',(5.27799445099994,15.2,-10.042651271));
#166474=CARTESIAN_POINT('Ctrl Pts',(5.27799445099994,11.6,-10.042651271));
#166475=CARTESIAN_POINT('Ctrl Pts',(5.28084913499994,15.2,-10.04487454));
#166476=CARTESIAN_POINT('Ctrl Pts',(5.28084913499994,11.6,-10.04487454));
#166477=CARTESIAN_POINT('Ctrl Pts',(5.28370917499994,15.2,-10.047098429));
#166478=CARTESIAN_POINT('Ctrl Pts',(5.28370917499994,11.6,-10.047098429));
#166479=CARTESIAN_POINT('Ctrl Pts',(5.28657456899994,15.2,-10.049322933));
#166480=CARTESIAN_POINT('Ctrl Pts',(5.28657456899994,11.6,-10.049322933));
#166481=CARTESIAN_POINT('Ctrl Pts',(5.28944531599994,15.2,-10.05154804));
#166482=CARTESIAN_POINT('Ctrl Pts',(5.28944531599994,11.6,-10.05154804));
#166483=CARTESIAN_POINT('Ctrl Pts',(5.29232141299994,15.2,-10.053773742));
#166484=CARTESIAN_POINT('Ctrl Pts',(5.29232141299994,11.6,-10.053773742));
#166485=CARTESIAN_POINT('Ctrl Pts',(5.29520285699994,15.2,-10.05600003));
#166486=CARTESIAN_POINT('Ctrl Pts',(5.29520285699994,11.6,-10.05600003));
#166487=CARTESIAN_POINT('Ctrl Pts',(5.29808964699994,15.2,-10.058226894));
#166488=CARTESIAN_POINT('Ctrl Pts',(5.29808964699994,11.6,-10.058226894));
#166489=CARTESIAN_POINT('Ctrl Pts',(5.30098177999994,15.2,-10.060454326));
#166490=CARTESIAN_POINT('Ctrl Pts',(5.30098177999994,11.6,-10.060454326));
#166491=CARTESIAN_POINT('Ctrl Pts',(5.30387925399994,15.2,-10.062682315));
#166492=CARTESIAN_POINT('Ctrl Pts',(5.30387925399994,11.6,-10.062682315));
#166493=CARTESIAN_POINT('Ctrl Pts',(5.30678206599994,15.2,-10.064910853));
#166494=CARTESIAN_POINT('Ctrl Pts',(5.30678206599994,11.6,-10.064910853));
#166495=CARTESIAN_POINT('Ctrl Pts',(5.30969021499994,15.2,-10.067139933));
#166496=CARTESIAN_POINT('Ctrl Pts',(5.30969021499994,11.6,-10.067139933));
#166497=CARTESIAN_POINT('Ctrl Pts',(5.31260369799995,15.2,-10.069369542));
#166498=CARTESIAN_POINT('Ctrl Pts',(5.31260369799995,11.6,-10.069369542));
#166499=CARTESIAN_POINT('Ctrl Pts',(5.31552251199994,15.2,-10.071599674));
#166500=CARTESIAN_POINT('Ctrl Pts',(5.31552251199994,11.6,-10.071599674));
#166501=CARTESIAN_POINT('Ctrl Pts',(5.31844665599994,15.2,-10.073830318));
#166502=CARTESIAN_POINT('Ctrl Pts',(5.31844665599994,11.6,-10.073830318));
#166503=CARTESIAN_POINT('Ctrl Pts',(5.32137612699994,15.2,-10.076061466));
#166504=CARTESIAN_POINT('Ctrl Pts',(5.32137612699994,11.6,-10.076061466));
#166505=CARTESIAN_POINT('Ctrl Pts',(5.32431092299994,15.2,-10.078293108));
#166506=CARTESIAN_POINT('Ctrl Pts',(5.32431092299994,11.6,-10.078293108));
#166507=CARTESIAN_POINT('Ctrl Pts',(5.32725104099994,15.2,-10.080525236));
#166508=CARTESIAN_POINT('Ctrl Pts',(5.32725104099994,11.6,-10.080525236));
#166509=CARTESIAN_POINT('Ctrl Pts',(5.33019647899994,15.2,-10.08275784));
#166510=CARTESIAN_POINT('Ctrl Pts',(5.33019647899994,11.6,-10.08275784));
#166511=CARTESIAN_POINT('Ctrl Pts',(5.33314723499994,15.2,-10.084990912));
#166512=CARTESIAN_POINT('Ctrl Pts',(5.33314723499994,11.6,-10.084990912));
#166513=CARTESIAN_POINT('Ctrl Pts',(5.33610330699994,15.2,-10.087224444));
#166514=CARTESIAN_POINT('Ctrl Pts',(5.33610330699994,11.6,-10.087224444));
#166515=CARTESIAN_POINT('Ctrl Pts',(5.33906469099994,15.2,-10.089458425));
#166516=CARTESIAN_POINT('Ctrl Pts',(5.33906469099994,11.6,-10.089458425));
#166517=CARTESIAN_POINT('Ctrl Pts',(5.34203138799994,15.2,-10.091692847));
#166518=CARTESIAN_POINT('Ctrl Pts',(5.34203138799994,11.6,-10.091692847));
#166519=CARTESIAN_POINT('Ctrl Pts',(5.34500339199994,15.2,-10.093927703));
#166520=CARTESIAN_POINT('Ctrl Pts',(5.34500339199994,11.6,-10.093927703));
#166521=CARTESIAN_POINT('Ctrl Pts',(5.34798070299994,15.2,-10.096162981));
#166522=CARTESIAN_POINT('Ctrl Pts',(5.34798070299994,11.6,-10.096162981));
#166523=CARTESIAN_POINT('Ctrl Pts',(5.35096331799994,15.2,-10.098398674));
#166524=CARTESIAN_POINT('Ctrl Pts',(5.35096331799994,11.6,-10.098398674));
#166525=CARTESIAN_POINT('Ctrl Pts',(5.35395123399994,15.2,-10.100634772));
#166526=CARTESIAN_POINT('Ctrl Pts',(5.35395123399994,11.6,-10.100634772));
#166527=CARTESIAN_POINT('Ctrl Pts',(5.35694444999994,15.2,-10.102871266));
#166528=CARTESIAN_POINT('Ctrl Pts',(5.35694444999994,11.6,-10.102871266));
#166529=CARTESIAN_POINT('Ctrl Pts',(5.35994296099994,15.2,-10.105108146));
#166530=CARTESIAN_POINT('Ctrl Pts',(5.35994296099994,11.6,-10.105108146));
#166531=CARTESIAN_POINT('Ctrl Pts',(5.36294676699994,15.2,-10.107345404));
#166532=CARTESIAN_POINT('Ctrl Pts',(5.36294676699994,11.6,-10.107345404));
#166533=CARTESIAN_POINT('Ctrl Pts',(5.36595586499995,15.2,-10.109583032));
#166534=CARTESIAN_POINT('Ctrl Pts',(5.36595586499995,11.6,-10.109583032));
#166535=CARTESIAN_POINT('Ctrl Pts',(5.36897025299995,15.2,-10.111821023));
#166536=CARTESIAN_POINT('Ctrl Pts',(5.36897025299995,11.6,-10.111821023));
#166537=CARTESIAN_POINT('Ctrl Pts',(5.37198992799994,15.2,-10.114059367));
#166538=CARTESIAN_POINT('Ctrl Pts',(5.37198992799994,11.6,-10.114059367));
#166539=CARTESIAN_POINT('Ctrl Pts',(5.37501488899994,15.2,-10.116298058));
#166540=CARTESIAN_POINT('Ctrl Pts',(5.37501488899994,11.6,-10.116298058));
#166541=CARTESIAN_POINT('Ctrl Pts',(5.37804513399994,15.2,-10.118537086));
#166542=CARTESIAN_POINT('Ctrl Pts',(5.37804513399994,11.6,-10.118537086));
#166543=CARTESIAN_POINT('Ctrl Pts',(5.38108065899994,15.2,-10.120776443));
#166544=CARTESIAN_POINT('Ctrl Pts',(5.38108065899994,11.6,-10.120776443));
#166545=CARTESIAN_POINT('Ctrl Pts',(5.38412146299994,15.2,-10.123016119));
#166546=CARTESIAN_POINT('Ctrl Pts',(5.38412146299994,11.6,-10.123016119));
#166547=CARTESIAN_POINT('Ctrl Pts',(5.38716754099994,15.2,-10.125256102));
#166548=CARTESIAN_POINT('Ctrl Pts',(5.38716754099994,11.6,-10.125256102));
#166549=CARTESIAN_POINT('Ctrl Pts',(5.39021889199994,15.2,-10.127496383));
#166550=CARTESIAN_POINT('Ctrl Pts',(5.39021889199994,11.6,-10.127496383));
#166551=CARTESIAN_POINT('Ctrl Pts',(5.39327551199994,15.2,-10.129736951));
#166552=CARTESIAN_POINT('Ctrl Pts',(5.39327551199994,11.6,-10.129736951));
#166553=CARTESIAN_POINT('Ctrl Pts',(5.39633739999994,15.2,-10.131977796));
#166554=CARTESIAN_POINT('Ctrl Pts',(5.39633739999994,11.6,-10.131977796));
#166555=CARTESIAN_POINT('Ctrl Pts',(5.39940455199994,15.2,-10.13421891));
#166556=CARTESIAN_POINT('Ctrl Pts',(5.39940455199994,11.6,-10.13421891));
#166557=CARTESIAN_POINT('Ctrl Pts',(5.40247696699994,15.2,-10.136460289));
#166558=CARTESIAN_POINT('Ctrl Pts',(5.40247696699994,11.6,-10.136460289));
#166559=CARTESIAN_POINT('Ctrl Pts',(5.40555464399994,15.2,-10.138701926));
#166560=CARTESIAN_POINT('Ctrl Pts',(5.40555464399994,11.6,-10.138701926));
#166561=CARTESIAN_POINT('Ctrl Pts',(5.40863758099994,15.2,-10.140943823));
#166562=CARTESIAN_POINT('Ctrl Pts',(5.40863758099994,11.6,-10.140943823));
#166563=CARTESIAN_POINT('Ctrl Pts',(5.41110813999994,15.2,-10.142737544));
#166564=CARTESIAN_POINT('Ctrl Pts',(5.41110813999994,11.6,-10.142737544));
#166565=CARTESIAN_POINT('Ctrl Pts',(5.41296342599994,15.2,-10.14408295));
#166566=CARTESIAN_POINT('Ctrl Pts',(5.41296342599994,11.6,-10.14408295));
#166567=CARTESIAN_POINT('Ctrl Pts',(5.41420133599994,15.2,-10.144979939));
#166568=CARTESIAN_POINT('Ctrl Pts',(5.41420133599994,11.6,-10.144979939));
#166569=CARTESIAN_POINT('Ctrl Pts',(5.41482055299994,15.2,-10.145428447));
#166570=CARTESIAN_POINT('Ctrl Pts',(5.41482055299994,11.6,-10.145428447));
#166571=CARTESIAN_POINT('Ctrl Pts',(4.57383771099994,15.2,-9.31239140100002));
#166572=CARTESIAN_POINT('Ctrl Pts',(4.57476026769951,15.2,-9.31392144680197));
#166573=CARTESIAN_POINT('Ctrl Pts',(4.57571693070584,15.2,-9.31549767344764));
#166574=CARTESIAN_POINT('Ctrl Pts',(4.57670776760804,15.2,-9.31711891458905));
#166575=CARTESIAN_POINT('Ctrl Pts',(4.57770338282661,15.2,-9.31874797417473));
#166576=CARTESIAN_POINT('Ctrl Pts',(4.57873349763143,15.2,-9.32042248430923));
#166577=CARTESIAN_POINT('Ctrl Pts',(4.57979816282796,15.2,-9.32214130040799));
#166578=CARTESIAN_POINT('Ctrl Pts',(4.58086282792779,15.2,-9.32386011635063));
#166579=CARTESIAN_POINT('Ctrl Pts',(4.58196204049941,15.2,-9.32562323961556));
#166580=CARTESIAN_POINT('Ctrl Pts',(4.58309584770821,15.2,-9.32742955654993));
#166581=CARTESIAN_POINT('Ctrl Pts',(4.58422965491702,15.2,-9.32923587348429));
#166582=CARTESIAN_POINT('Ctrl Pts',(4.5853980563192,15.1999999999999,-9.33108538508538));
#166583=CARTESIAN_POINT('Ctrl Pts',(4.58660109166692,15.2,-9.33297701302539));
#166584=CARTESIAN_POINT('Ctrl Pts',(4.58780412712392,15.2,-9.33486864113721));
#166585=CARTESIAN_POINT('Ctrl Pts',(4.58904179768353,15.2,-9.33680238271311));
#166586=CARTESIAN_POINT('Ctrl Pts',(4.59031413808858,15.2,-9.33877718824021));
#166587=CARTESIAN_POINT('Ctrl Pts',(4.59158647837806,15.2,-9.34075199358794));
#166588=CARTESIAN_POINT('Ctrl Pts',(4.59289349004307,15.2,-9.34276786523282));
#166589=CARTESIAN_POINT('Ctrl Pts',(4.5942352060005,15.2,-9.34482377850088));
#166590=CARTESIAN_POINT('Ctrl Pts',(4.59557692195793,15.2,-9.34687969176897));
#166591=CARTESIAN_POINT('Ctrl Pts',(4.59695334073424,15.2,-9.34897564678802));
#166592=CARTESIAN_POINT('Ctrl Pts',(4.59836449093146,15.2,-9.35111065112542));
#166593=CARTESIAN_POINT('Ctrl Pts',(4.59977564125686,15.2,-9.35324565565676));
#166594=CARTESIAN_POINT('Ctrl Pts',(4.60122152409488,15.2,-9.35541970753459));
#166595=CARTESIAN_POINT('Ctrl Pts',(4.60270216417795,15.2,-9.35763183999108));
#166596=CARTESIAN_POINT('Ctrl Pts',(4.60418280412651,15.2,-9.35984397224663));
#166597=CARTESIAN_POINT('Ctrl Pts',(4.60569820106435,15.2,-9.36209418342296));
#166598=CARTESIAN_POINT('Ctrl Pts',(4.60724837709285,15.2,-9.36438152917477));
#166599=CARTESIAN_POINT('Ctrl Pts',(4.60879855312135,15.2,-9.36666887492659));
#166600=CARTESIAN_POINT('Ctrl Pts',(4.61038350778881,15.2,-9.36899335881716));
#166601=CARTESIAN_POINT('Ctrl Pts',(4.61200325789508,15.2,-9.37135405564644));
#166602=CARTESIAN_POINT('Ctrl Pts',(4.61362300800136,15.2,-9.37371475247571));
#166603=CARTESIAN_POINT('Ctrl Pts',(4.61527755797951,15.2,-9.3761116657423));
#166604=CARTESIAN_POINT('Ctrl Pts',(4.61696691708242,15.2,-9.37854389648485));
#166605=CARTESIAN_POINT('Ctrl Pts',(4.61865627633879,15.2,-9.38097612744834));
#166606=CARTESIAN_POINT('Ctrl Pts',(4.62038044630684,15.2,-9.38344367723195));
#166607=CARTESIAN_POINT('Ctrl Pts',(4.6221394413209,15.2,-9.38594566836979));
#166608=CARTESIAN_POINT('Ctrl Pts',(4.62389843617517,15.2,-9.38844765928039));
#166609=CARTESIAN_POINT('Ctrl Pts',(4.62569225239894,15.2,-9.39098409241392));
#166610=CARTESIAN_POINT('Ctrl Pts',(4.62752090125739,15.2,-9.39355411249879));
#166611=CARTESIAN_POINT('Ctrl Pts',(4.62965432503633,15.2,-9.39655246942013));
#166612=CARTESIAN_POINT('Ctrl Pts',(4.63183515898931,15.2,-9.39959654241051));
#166613=CARTESIAN_POINT('Ctrl Pts',(4.63406341059595,15.2,-9.4026850069196));
#166614=CARTESIAN_POINT('Ctrl Pts',(4.63597334044536,15.2,-9.40533226207569));
#166615=CARTESIAN_POINT('Ctrl Pts',(4.63791810759892,15.2,-9.40801213163555));
#166616=CARTESIAN_POINT('Ctrl Pts',(4.63989771385881,15.2,-9.41072380386897));
#166617=CARTESIAN_POINT('Ctrl Pts',(4.64187732011871,15.2,-9.4134354761024));
#166618=CARTESIAN_POINT('Ctrl Pts',(4.64389176767837,15.2,-9.41617895175048));
#166619=CARTESIAN_POINT('Ctrl Pts',(4.64594105451818,15.2,-9.41895343414755));
#166620=CARTESIAN_POINT('Ctrl Pts',(4.64799034154416,15.2,-9.42172791679664));
#166621=CARTESIAN_POINT('Ctrl Pts',(4.65007446671518,15.2,-9.42453340810711));
#166622=CARTESIAN_POINT('Ctrl Pts',(4.65219342783218,15.2,-9.42736913067964));
#166623=CARTESIAN_POINT('Ctrl Pts',(4.65431238875671,15.2,-9.43020485299459));
#166624=CARTESIAN_POINT('Ctrl Pts',(4.6564661859602,15.2,-9.43307080742409));
#166625=CARTESIAN_POINT('Ctrl Pts',(4.65865481280723,15.2,-9.43596623199865));
#166626=CARTESIAN_POINT('Ctrl Pts',(4.66084343965424,15.2,-9.43886165657323));
#166627=CARTESIAN_POINT('Ctrl Pts',(4.66306689596317,15.2,-9.4417865522873));
#166628=CARTESIAN_POINT('Ctrl Pts',(4.66532517296207,15.2,-9.44474017667803));
#166629=CARTESIAN_POINT('Ctrl Pts',(4.66758345016611,15.2,-9.44769380133706));
#166630=CARTESIAN_POINT('Ctrl Pts',(4.66987654967998,15.2,-9.45067615296685));
#166631=CARTESIAN_POINT('Ctrl Pts',(4.67220445892517,15.2,-9.45368650503292));
#166632=CARTESIAN_POINT('Ctrl Pts',(4.6745323679589,15.2,-9.45669685682556));
#166633=CARTESIAN_POINT('Ctrl Pts',(4.67689508671199,15.2,-9.45973520780302));
#166634=CARTESIAN_POINT('Ctrl Pts',(4.67929260254154,15.2,-9.46280084644163));
#166635=CARTESIAN_POINT('Ctrl Pts',(4.68169011837109,15.2,-9.46586648508024));
#166636=CARTESIAN_POINT('Ctrl Pts',(4.68412243150472,15.2,-9.46895940989898));
#166637=CARTESIAN_POINT('Ctrl Pts',(4.68658952378631,15.2,-9.47207892468993));
#166638=CARTESIAN_POINT('Ctrl Pts',(4.689056616292,15.2,-9.47519843976424));
#166639=CARTESIAN_POINT('Ctrl Pts',(4.69155849149409,15.2,-9.47834454267108));
#166640=CARTESIAN_POINT('Ctrl Pts',(4.69409512855138,15.2,-9.48151654984572));
#166641=CARTESIAN_POINT('Ctrl Pts',(4.69620899265059,15.2,-9.48415988901386));
#166642=CARTESIAN_POINT('Ctrl Pts',(4.69834699793628,15.2,-9.48682121918228));
#166643=CARTESIAN_POINT('Ctrl Pts',(4.70050913279937,15.2,-9.48950014835038));
#166644=CARTESIAN_POINT('Ctrl Pts',(4.70267126742678,15.2,-9.49217907722649));
#166645=CARTESIAN_POINT('Ctrl Pts',(4.70485753088146,15.2,-9.49487560747001));
#166646=CARTESIAN_POINT('Ctrl Pts',(4.70706790994411,15.2,-9.49758935543668));
#166647=CARTESIAN_POINT('Ctrl Pts',(4.70927828924768,15.2,-9.50030310369916));
#166648=CARTESIAN_POINT('Ctrl Pts',(4.71151278833977,15.2,-9.50303407011418));
#166649=CARTESIAN_POINT('Ctrl Pts',(4.71377138750447,15.2,-9.50578187914056));
#166650=CARTESIAN_POINT('Ctrl Pts',(4.71648170664982,15.2,-9.50907925015195));
#166651=CARTESIAN_POINT('Ctrl Pts',(4.71922673423483,15.2,-9.51240087193117));
#166652=CARTESIAN_POINT('Ctrl Pts',(4.7220064462772,15.2,-9.51574610653197));
#166653=CARTESIAN_POINT('Ctrl Pts',(4.72432287285293,15.2,-9.51853380188071));
#166654=CARTESIAN_POINT('Ctrl Pts',(4.72666338229611,15.2,-9.52133789668977));
#166655=CARTESIAN_POINT('Ctrl Pts',(4.72902796299251,15.2,-9.52415802592718));
#166656=CARTESIAN_POINT('Ctrl Pts',(4.73139254368892,15.2,-9.52697815516461));
#166657=CARTESIAN_POINT('Ctrl Pts',(4.73378119318574,15.2,-9.52981431736618));
#166658=CARTESIAN_POINT('Ctrl Pts',(4.7361938955488,15.2,-9.53266615833967));
#166659=CARTESIAN_POINT('Ctrl Pts',(4.73860659764888,15.2,-9.53551799900231));
#166660=CARTESIAN_POINT('Ctrl Pts',(4.74104335202599,15.2,-9.53838551687173));
#166661=CARTESIAN_POINT('Ctrl Pts',(4.74350414168635,15.2,-9.54126835988957));
#166662=CARTESIAN_POINT('Ctrl Pts',(4.74596493161494,15.2,-9.54415120322165));
#166663=CARTESIAN_POINT('Ctrl Pts',(4.7484497562237,15.2,-9.54704937064239));
#166664=CARTESIAN_POINT('Ctrl Pts',(4.75095859768007,15.2,-9.54996251591894));
#166665=CARTESIAN_POINT('Ctrl Pts',(4.75346743913642,15.2,-9.55287566119547));
#166666=CARTESIAN_POINT('Ctrl Pts',(4.75600029617711,15.2,-9.55580378354579));
#166667=CARTESIAN_POINT('Ctrl Pts',(4.75855715046982,15.2,-9.55874654390009));
#166668=CARTESIAN_POINT('Ctrl Pts',(4.76213674653536,15.2,-9.56286640846026));
#166669=CARTESIAN_POINT('Ctrl Pts',(4.76576337720379,15.2,-9.56701495697939));
#166670=CARTESIAN_POINT('Ctrl Pts',(4.76943698523321,15.2,-9.57119127176664));
#166671=CARTESIAN_POINT('Ctrl Pts',(4.77206099092766,15.2,-9.57417435371108));
#166672=CARTESIAN_POINT('Ctrl Pts',(4.77470896504431,15.2,-9.57717160112774));
#166673=CARTESIAN_POINT('Ctrl Pts',(4.77738088497488,15.2,-9.58018268480831));
#166674=CARTESIAN_POINT('Ctrl Pts',(4.78005280490545,15.2,-9.58319376848888));
#166675=CARTESIAN_POINT('Ctrl Pts',(4.78274867295005,15.2,-9.58621868871556));
#166676=CARTESIAN_POINT('Ctrl Pts',(4.78546846372637,15.2,-9.58925712074331));
#166677=CARTESIAN_POINT('Ctrl Pts',(4.78818825450268,15.2,-9.59229555277104));
#166678=CARTESIAN_POINT('Ctrl Pts',(4.79093197017425,15.2,-9.5953474966443));
#166679=CARTESIAN_POINT('Ctrl Pts',(4.7936995873977,15.2,-9.59841262970052));
#166680=CARTESIAN_POINT('Ctrl Pts',(4.79646720462116,15.2,-9.60147776275676));
#166681=CARTESIAN_POINT('Ctrl Pts',(4.79925872182179,15.2,-9.60455608865711));
#166682=CARTESIAN_POINT('Ctrl Pts',(4.80207411668416,15.2,-9.60764728747723));
#166683=CARTESIAN_POINT('Ctrl Pts',(4.80432643238992,15.2,-9.61012024633116));
#166684=CARTESIAN_POINT('Ctrl Pts',(4.80659402907221,15.2,-9.61260144555096));
#166685=CARTESIAN_POINT('Ctrl Pts',(4.80887689494432,15.2,-9.61509072513948));
#166686=CARTESIAN_POINT('Ctrl Pts',(4.81115976112746,15.2,-9.61758000506716));
#166687=CARTESIAN_POINT('Ctrl Pts',(4.81345789653985,15.2,-9.62007736431503));
#166688=CARTESIAN_POINT('Ctrl Pts',(4.81577128722248,15.2,-9.62258264672987));
#166689=CARTESIAN_POINT('Ctrl Pts',(4.81808467758992,15.2,-9.62508792880336));
#166690=CARTESIAN_POINT('Ctrl Pts',(4.82041332369872,15.2,-9.62760113152524));
#166691=CARTESIAN_POINT('Ctrl Pts',(4.82275721261667,15.2,-9.63012210159614));
#166692=CARTESIAN_POINT('Ctrl Pts',(4.82510110185397,15.2,-9.63264307201052));
#166693=CARTESIAN_POINT('Ctrl Pts',(4.82746023271683,15.2,-9.63517180841028));
#166694=CARTESIAN_POINT('Ctrl Pts',(4.82983459396817,15.2,-9.63770815572671));
#166695=CARTESIAN_POINT('Ctrl Pts',(4.832208954896,15.2,-9.64024450269757));
#166696=CARTESIAN_POINT('Ctrl Pts',(4.83459854451597,15.2,-9.64278846171439));
#166697=CARTESIAN_POINT('Ctrl Pts',(4.83700334887337,15.2,-9.64533987861616));
#166698=CARTESIAN_POINT('Ctrl Pts',(4.83940815355843,15.2,-9.64789129586556));
#166699=CARTESIAN_POINT('Ctrl Pts',(4.84182817370882,15.2,-9.65045017198234));
#166700=CARTESIAN_POINT('Ctrl Pts',(4.84426339500821,15.2,-9.65301635523332));
#166701=CARTESIAN_POINT('Ctrl Pts',(4.84669861630759,15.2,-9.65558253848429));
#166702=CARTESIAN_POINT('Ctrl Pts',(4.84914903850876,15.2,-9.65815602873055));
#166703=CARTESIAN_POINT('Ctrl Pts',(4.85161464714468,15.2,-9.66073667720525));
#166704=CARTESIAN_POINT('Ctrl Pts',(4.85408025544467,15.2,-9.66331732532834));
#166705=CARTESIAN_POINT('Ctrl Pts',(4.85656105066872,15.2,-9.6659051301097));
#166706=CARTESIAN_POINT('Ctrl Pts',(4.85905701769819,15.2,-9.66849994446489));
#166707=CARTESIAN_POINT('Ctrl Pts',(4.86155298506772,15.2,-9.67109475917362));
#166708=CARTESIAN_POINT('Ctrl Pts',(4.86406412438483,15.2,-9.67369658477809));
#166709=CARTESIAN_POINT('Ctrl Pts',(4.86659042041294,15.2,-9.67630527214317));
#166710=CARTESIAN_POINT('Ctrl Pts',(4.86974829027598,15.2,-9.67956613117182));
#166711=CARTESIAN_POINT('Ctrl Pts',(4.87292984304499,15.2,-9.68283771485622));
#166712=CARTESIAN_POINT('Ctrl Pts',(4.8761350494358,15.2,-9.68611973791261));
#166713=CARTESIAN_POINT('Ctrl Pts',(4.87869921433883,15.2,-9.68874535614309));
#166714=CARTESIAN_POINT('Ctrl Pts',(4.88127851644015,15.2,-9.69137765576307));
#166715=CARTESIAN_POINT('Ctrl Pts',(4.88387294073979,15.2,-9.69401649478152));
#166716=CARTESIAN_POINT('Ctrl Pts',(4.88646736539291,15.2,-9.69665533415952));
#166717=CARTESIAN_POINT('Ctrl Pts',(4.88907691291499,15.2,-9.69930071231338));
#166718=CARTESIAN_POINT('Ctrl Pts',(4.89170156567069,15.2,-9.70195248762522));
#166719=CARTESIAN_POINT('Ctrl Pts',(4.89498238143651,15.2,-9.70526720658438));
#166720=CARTESIAN_POINT('Ctrl Pts',(4.89828680232771,15.2,-9.708591920502));
#166721=CARTESIAN_POINT('Ctrl Pts',(4.90161479392686,15.2,-9.7119263561278));
#166722=CARTESIAN_POINT('Ctrl Pts',(4.90427718698853,15.2,-9.71459390441036));
#166723=CARTESIAN_POINT('Ctrl Pts',(4.90695466801434,15.2,-9.71726767529121));
#166724=CARTESIAN_POINT('Ctrl Pts',(4.90964721697305,15.2,-9.71994752847316));
#166725=CARTESIAN_POINT('Ctrl Pts',(4.91233976629863,15.2,-9.72262738202025));
#166726=CARTESIAN_POINT('Ctrl Pts',(4.9150473860368,15.2,-9.72531331995113));
#166727=CARTESIAN_POINT('Ctrl Pts',(4.91777005868672,15.2,-9.72800520393178));
#166728=CARTESIAN_POINT('Ctrl Pts',(4.92049273096567,15.2,-9.73069708754565));
#166729=CARTESIAN_POINT('Ctrl Pts',(4.92323045634267,15.2,-9.73339491785597));
#166730=CARTESIAN_POINT('Ctrl Pts',(4.92598321728332,15.2,-9.73609855707902));
#166731=CARTESIAN_POINT('Ctrl Pts',(4.92873597859904,15.2,-9.73880219667045));
#166732=CARTESIAN_POINT('Ctrl Pts',(4.9315037762229,15.2,-9.74151164834323));
#166733=CARTESIAN_POINT('Ctrl Pts',(4.93428659240377,15.2,-9.74422677462734));
#166734=CARTESIAN_POINT('Ctrl Pts',(4.93776511244029,15.2,-9.74762068229751));
#166735=CARTESIAN_POINT('Ctrl Pts',(4.941267098748,15.2,-9.75102345940662));
#166736=CARTESIAN_POINT('Ctrl Pts',(4.94479251923602,15.2,-9.7544348451712));
#166737=CARTESIAN_POINT('Ctrl Pts',(4.94831793972405,15.2,-9.7578462309358));
#166738=CARTESIAN_POINT('Ctrl Pts',(4.9518667911208,15.2,-9.76126622572552));
#166739=CARTESIAN_POINT('Ctrl Pts',(4.95543904244214,15.2,-9.76469457169842));
#166740=CARTESIAN_POINT('Ctrl Pts',(4.95829684326559,15.2,-9.76743724825253));
#166741=CARTESIAN_POINT('Ctrl Pts',(4.96116961839593,15.2,-9.77018527115238));
#166742=CARTESIAN_POINT('Ctrl Pts',(4.96405735000625,15.2,-9.77293850943978));
#166743=CARTESIAN_POINT('Ctrl Pts',(4.96694508201002,15.2,-9.77569174810231));
#166744=CARTESIAN_POINT('Ctrl Pts',(4.96984777119694,15.2,-9.77845020128403));
#166745=CARTESIAN_POINT('Ctrl Pts',(4.97276539796859,15.2,-9.78121374143516));
#166746=CARTESIAN_POINT('Ctrl Pts',(4.97641243123438,15.2,-9.7846681664358));
#166747=CARTESIAN_POINT('Ctrl Pts',(4.98008280670335,15.2,-9.78813053885881));
#166748=CARTESIAN_POINT('Ctrl Pts',(4.98377648719136,15.2,-9.79160061122055));
#166749=CARTESIAN_POINT('Ctrl Pts',(4.9867314313402,15.2,-9.794376668883));
#166750=CARTESIAN_POINT('Ctrl Pts',(4.98970129165934,15.2,-9.79715765257257));
#166751=CARTESIAN_POINT('Ctrl Pts',(4.99268604724769,15.2,-9.79994343778897));
#166752=CARTESIAN_POINT('Ctrl Pts',(4.99567080324272,15.2,-9.80272922338492));
#166753=CARTESIAN_POINT('Ctrl Pts',(4.99867045525731,15.2,-9.80551981066045));
#166754=CARTESIAN_POINT('Ctrl Pts',(5.00168498596239,15.2,-9.80831507489729));
#166755=CARTESIAN_POINT('Ctrl Pts',(5.00469951625674,15.2,-9.81111033875329));
#166756=CARTESIAN_POINT('Ctrl Pts',(5.00772892316488,15.2,-9.81391027710032));
#166757=CARTESIAN_POINT('Ctrl Pts',(5.01077318819283,15.2,-9.81671476953744));
#166758=CARTESIAN_POINT('Ctrl Pts',(5.01381745363556,15.2,-9.81951926235666));
#166759=CARTESIAN_POINT('Ctrl Pts',(5.01687657826893,15.2,-9.82232830744308));
#166760=CARTESIAN_POINT('Ctrl Pts',(5.01995054149299,15.2,-9.82514178226337));
#166761=CARTESIAN_POINT('Ctrl Pts',(5.02379299531365,15.2,-9.82865862559708));
#166762=CARTESIAN_POINT('Ctrl Pts',(5.02765863386107,15.2,-9.83218238931079));
#166763=CARTESIAN_POINT('Ctrl Pts',(5.03154742120973,15.2,-9.83571283941819));
#166764=CARTESIAN_POINT('Ctrl Pts',(5.03465845083434,15.2,-9.83853719927321));
#166765=CARTESIAN_POINT('Ctrl Pts',(5.03778429343989,15.2,-9.84136583625865));
#166766=CARTESIAN_POINT('Ctrl Pts',(5.04092493095995,15.2,-9.84419863152679));
#166767=CARTESIAN_POINT('Ctrl Pts',(5.04406556890792,15.2,-9.84703142718091));
#166768=CARTESIAN_POINT('Ctrl Pts',(5.04722100104379,15.2,-9.84986838097997));
#166769=CARTESIAN_POINT('Ctrl Pts',(5.05039120771752,15.2,-9.85270937319062));
#166770=CARTESIAN_POINT('Ctrl Pts',(5.05356141395932,15.2,-9.85555036501418));
#166771=CARTESIAN_POINT('Ctrl Pts',(5.05674639388866,15.2,-9.85839539606642));
#166772=CARTESIAN_POINT('Ctrl Pts',(5.05994612878567,15.2,-9.86124434808662));
#166773=CARTESIAN_POINT('Ctrl Pts',(5.06314586411864,15.2,-9.86409330049499));
#166774=CARTESIAN_POINT('Ctrl Pts',(5.06636035255929,15.2,-9.86694617341931));
#166775=CARTESIAN_POINT('Ctrl Pts',(5.06958957451402,15.2,-9.8698028497419));
#166776=CARTESIAN_POINT('Ctrl Pts',(5.07281879602876,15.2,-9.87265952567528));
#166777=CARTESIAN_POINT('Ctrl Pts',(5.07606275000721,15.2,-9.87552000557456));
#166778=CARTESIAN_POINT('Ctrl Pts',(5.0793214175171,15.2,-9.87838417350671));
#166779=CARTESIAN_POINT('Ctrl Pts',(5.08258008547098,15.2,-9.8812483418291));
#166780=CARTESIAN_POINT('Ctrl Pts',(5.08585346667739,15.2,-9.88411619788519));
#166781=CARTESIAN_POINT('Ctrl Pts',(5.08914153926046,15.2,-9.88698762677695));
#166782=CARTESIAN_POINT('Ctrl Pts',(5.09242961139553,15.2,-9.88985905527749));
#166783=CARTESIAN_POINT('Ctrl Pts',(5.09573237493298,15.2,-9.89273405530115));
#166784=CARTESIAN_POINT('Ctrl Pts',(5.09904980971583,15.2,-9.89561251578771));
#166785=CARTESIAN_POINT('Ctrl Pts',(5.10236724495068,15.2,-9.89849097666645));
#166786=CARTESIAN_POINT('Ctrl Pts',(5.10569934985637,15.2,-9.90137289553997));
#166787=CARTESIAN_POINT('Ctrl Pts',(5.10904610448321,15.2,-9.904258159975));
#166788=CARTESIAN_POINT('Ctrl Pts',(5.11239285911007,15.2,-9.90714342441002));
#166789=CARTESIAN_POINT('Ctrl Pts',(5.11575426434694,15.2,-9.91003203617322));
#166790=CARTESIAN_POINT('Ctrl Pts',(5.11913029581021,15.2,-9.91292388049782));
#166791=CARTESIAN_POINT('Ctrl Pts',(5.12166231917767,15.2,-9.91509276354427));
#166792=CARTESIAN_POINT('Ctrl Pts',(5.12420257155736,15.2,-9.9172634657072));
#166793=CARTESIAN_POINT('Ctrl Pts',(5.12675104246803,15.2,-9.91943593990367));
#166794=CARTESIAN_POINT('Ctrl Pts',(5.1292995133787,15.2,-9.92160841410014));
#166795=CARTESIAN_POINT('Ctrl Pts',(5.13185620388874,15.2,-9.92378266093279));
#166796=CARTESIAN_POINT('Ctrl Pts',(5.13442110408793,15.2,-9.92595863252054));
#166797=CARTESIAN_POINT('Ctrl Pts',(5.13698600428713,15.2,-9.9281346041083));
#166798=CARTESIAN_POINT('Ctrl Pts',(5.139559113277,15.2,-9.93031230086252));
#166799=CARTESIAN_POINT('Ctrl Pts',(5.14214042397488,15.2,-9.93249167699166));
#166800=CARTESIAN_POINT('Ctrl Pts',(5.14472173467275,15.2,-9.9346710531208));
#166801=CARTESIAN_POINT('Ctrl Pts',(5.14731124576196,15.2,-9.93685210917488));
#166802=CARTESIAN_POINT('Ctrl Pts',(5.14990894795854,15.2,-9.93903479822045));
#166803=CARTESIAN_POINT('Ctrl Pts',(5.15250665015513,15.2,-9.94121748726602));
#166804=CARTESIAN_POINT('Ctrl Pts',(5.15511254299286,15.2,-9.94340180889749));
#166805=CARTESIAN_POINT('Ctrl Pts',(5.15772661923588,15.2,-9.94558771809377));
#166806=CARTESIAN_POINT('Ctrl Pts',(5.16034069547889,15.2,-9.94777362729005));
#166807=CARTESIAN_POINT('Ctrl Pts',(5.16296295305647,15.2,-9.94996112383586));
#166808=CARTESIAN_POINT('Ctrl Pts',(5.1655933832098,15.2,-9.95215016196446));
#166809=CARTESIAN_POINT('Ctrl Pts',(5.16822381384098,15.2,-9.95433920049074));
#166810=CARTESIAN_POINT('Ctrl Pts',(5.17086241622444,15.2,-9.95652978094242));
#166811=CARTESIAN_POINT('Ctrl Pts',(5.17350918286022,15.2,-9.95872185842788));
#166812=CARTESIAN_POINT('Ctrl Pts',(5.17615594901517,15.2,-9.9609139355151));
#166813=CARTESIAN_POINT('Ctrl Pts',(5.17881087726968,15.2,-9.96310750935224));
#166814=CARTESIAN_POINT('Ctrl Pts',(5.18147395950697,15.2,-9.96530253489762));
#166815=CARTESIAN_POINT('Ctrl Pts',(5.18413704174425,15.2,-9.96749756044298));
#166816=CARTESIAN_POINT('Ctrl Pts',(5.18680827773747,15.2,-9.96969403773854));
#166817=CARTESIAN_POINT('Ctrl Pts',(5.18948765748565,15.2,-9.97189192229367));
#166818=CARTESIAN_POINT('Ctrl Pts',(5.19216703723384,15.2,-9.9740898068488));
#166819=CARTESIAN_POINT('Ctrl Pts',(5.19485456173318,15.2,-9.97628909883465));
#166820=CARTESIAN_POINT('Ctrl Pts',(5.19755021952244,15.2,-9.97848975301467));
#166821=CARTESIAN_POINT('Ctrl Pts',(5.2011444302346,15.2,-9.98142395885457));
#166822=CARTESIAN_POINT('Ctrl Pts',(5.20475310328501,15.2,-9.98436058880345));
#166823=CARTESIAN_POINT('Ctrl Pts',(5.20837621331727,15.2,-9.98729953596386));
#166824=CARTESIAN_POINT('Ctrl Pts',(5.21109354559466,15.2,-9.98950374613394));
#166825=CARTESIAN_POINT('Ctrl Pts',(5.2138189997966,15.2,-9.99170926057063));
#166826=CARTESIAN_POINT('Ctrl Pts',(5.21655256507298,15.2,-9.9939160356989));
#166827=CARTESIAN_POINT('Ctrl Pts',(5.21928613034937,15.2,-9.99612281082715));
#166828=CARTESIAN_POINT('Ctrl Pts',(5.22202780768977,15.2,-9.9983308470389));
#166829=CARTESIAN_POINT('Ctrl Pts',(5.22477758647739,15.2,-10.0005400987603));
#166830=CARTESIAN_POINT('Ctrl Pts',(5.22752736526501,15.2,-10.0027493504818));
#166831=CARTESIAN_POINT('Ctrl Pts',(5.23028524676868,15.2,-10.0049598200516));
#166832=CARTESIAN_POINT('Ctrl Pts',(5.23305121951404,15.2,-10.0071714627313));
#166833=CARTESIAN_POINT('Ctrl Pts',(5.23581719225941,15.2,-10.009383105411));
#166834=CARTESIAN_POINT('Ctrl Pts',(5.23859125696523,15.2,-10.0115959222059));
#166835=CARTESIAN_POINT('Ctrl Pts',(5.24137340369677,15.2,-10.0138098702504));
#166836=CARTESIAN_POINT('Ctrl Pts',(5.24415555042832,15.2,-10.0160238182948));
#166837=CARTESIAN_POINT('Ctrl Pts',(5.2469457794593,15.2,-10.0182388958809));
#166838=CARTESIAN_POINT('Ctrl Pts',(5.2497440806482,15.2,-10.0204550620086));
#166839=CARTESIAN_POINT('Ctrl Pts',(5.25254238234546,15.2,-10.0226712285388));
#166840=CARTESIAN_POINT('Ctrl Pts',(5.25534875561998,15.2,-10.0248884839444));
#166841=CARTESIAN_POINT('Ctrl Pts',(5.25816319136344,15.2,-10.0271067845169));
#166842=CARTESIAN_POINT('Ctrl Pts',(5.26097762659562,15.2,-10.0293250846865));
#166843=CARTESIAN_POINT('Ctrl Pts',(5.26380012429403,15.2,-10.0315444305393));
#166844=CARTESIAN_POINT('Ctrl Pts',(5.26663067352522,15.2,-10.0337647797087));
#166845=CARTESIAN_POINT('Ctrl Pts',(5.2694612227564,15.2,-10.0359851288781));
#166846=CARTESIAN_POINT('Ctrl Pts',(5.27229982402627,15.2,-10.0382064818227));
#166847=CARTESIAN_POINT('Ctrl Pts',(5.27514646726914,15.2,-10.0404287960437));
#166848=CARTESIAN_POINT('Ctrl Pts',(5.27799311051202,15.2,-10.0426511102647));
#166849=CARTESIAN_POINT('Ctrl Pts',(5.28084779672167,15.2,-10.0448743869687));
#166850=CARTESIAN_POINT('Ctrl Pts',(5.28371051350562,15.2,-10.0470985826897));
#166851=CARTESIAN_POINT('Ctrl Pts',(5.28657323028958,15.2,-10.0493227784106));
#166852=CARTESIAN_POINT('Ctrl Pts',(5.28944397922486,15.2,-10.0515478941217));
#166853=CARTESIAN_POINT('Ctrl Pts',(5.2923227494529,15.2,-10.0537738882491));
#166854=CARTESIAN_POINT('Ctrl Pts',(5.2961611101056,15.2,-10.0567418806885));
#166855=CARTESIAN_POINT('Ctrl Pts',(5.30001373151003,15.2,-10.0597114351726));
#166856=CARTESIAN_POINT('Ctrl Pts',(5.3038805888328,15.2,-10.0626824525012));
#166857=CARTESIAN_POINT('Ctrl Pts',(5.30678073156146,15.2,-10.0649107152953));
#166858=CARTESIAN_POINT('Ctrl Pts',(5.30968888252856,15.2,-10.0671398029896));
#166859=CARTESIAN_POINT('Ctrl Pts',(5.31260503076921,15.2,-10.0693696727104));
#166860=CARTESIAN_POINT('Ctrl Pts',(5.31552117900986,15.2,-10.0715995424311));
#166861=CARTESIAN_POINT('Ctrl Pts',(5.31844532504048,15.2,-10.0738301953356));
#166862=CARTESIAN_POINT('Ctrl Pts',(5.32137745823889,15.2,-10.0760615895146));
#166863=CARTESIAN_POINT('Ctrl Pts',(5.3243095914373,15.2,-10.0782929836937));
#166864=CARTESIAN_POINT('Ctrl Pts',(5.32724971145315,15.2,-10.0805251195045));
#166865=CARTESIAN_POINT('Ctrl Pts',(5.33019780817868,15.2,-10.0827579567566));
#166866=CARTESIAN_POINT('Ctrl Pts',(5.33314590490421,15.2,-10.0849907940088));
#166867=CARTESIAN_POINT('Ctrl Pts',(5.33610197836251,15.2,-10.0872243339776));
#166868=CARTESIAN_POINT('Ctrl Pts',(5.33906601854541,15.2,-10.0894585347713));
#166869=CARTESIAN_POINT('Ctrl Pts',(5.34203005926677,15.2,-10.0916927359709));
#166870=CARTESIAN_POINT('Ctrl Pts',(5.34500206646536,15.2,-10.0939276000957));
#166871=CARTESIAN_POINT('Ctrl Pts',(5.34798202964953,15.2,-10.0961630852123));
#166872=CARTESIAN_POINT('Ctrl Pts',(5.35096199229233,15.2,-10.0983985699229));
#166873=CARTESIAN_POINT('Ctrl Pts',(5.35394991103786,15.2,-10.1006346766689));
#166874=CARTESIAN_POINT('Ctrl Pts',(5.35694577437126,15.2,-10.1028713629494));
#166875=CARTESIAN_POINT('Ctrl Pts',(5.35994163770466,15.2,-10.10510804923));
#166876=CARTESIAN_POINT('Ctrl Pts',(5.36294544513703,15.2,-10.1073453142585));
#166877=CARTESIAN_POINT('Ctrl Pts',(5.36595718781997,15.2,-10.1095831229689));
#166878=CARTESIAN_POINT('Ctrl Pts',(5.3689689305029,15.2,-10.1118209316793));
#166879=CARTESIAN_POINT('Ctrl Pts',(5.37198860734323,15.2,-10.114059283598));
#166880=CARTESIAN_POINT('Ctrl Pts',(5.37501620998321,15.2,-10.1162981422667));
#166881=CARTESIAN_POINT('Ctrl Pts',(5.3780438126232,15.2,-10.1185370009353));
#166882=CARTESIAN_POINT('Ctrl Pts',(5.38107934056289,15.2,-10.1207763669873));
#166883=CARTESIAN_POINT('Ctrl Pts',(5.38412278120162,15.2,-10.1230161955309));
#166884=CARTESIAN_POINT('Ctrl Pts',(5.38716622184035,15.2,-10.1252560240745));
#166885=CARTESIAN_POINT('Ctrl Pts',(5.39021757455064,15.2,-10.1274963140527));
#166886=CARTESIAN_POINT('Ctrl Pts',(5.39327682838308,15.2,-10.1297370198332));
#166887=CARTESIAN_POINT('Ctrl Pts',(5.39633608221551,15.2,-10.1319777256136));
#166888=CARTESIAN_POINT('Ctrl Pts',(5.39940323605899,15.2,-10.1342188453762));
#166889=CARTESIAN_POINT('Ctrl Pts',(5.4024782818212,15.2,-10.1364603530864));
#166890=CARTESIAN_POINT('Ctrl Pts',(5.4065783432099,15.2,-10.1394490303047));
#166891=CARTESIAN_POINT('Ctrl Pts',(5.4106924385417,15.2,-10.1424383928519));
#166892=CARTESIAN_POINT('Ctrl Pts',(5.41482055299994,15.2,-10.145428447));
#166893=CARTESIAN_POINT('Ctrl Pts',(4.57383771099994,12.2,-9.31239140100002));
#166894=CARTESIAN_POINT('Ctrl Pts',(4.57476026769951,12.2,-9.31392144680197));
#166895=CARTESIAN_POINT('Ctrl Pts',(4.57571693070584,12.2,-9.31549767344764));
#166896=CARTESIAN_POINT('Ctrl Pts',(4.57670776760804,12.2,-9.31711891458905));
#166897=CARTESIAN_POINT('Ctrl Pts',(4.57770338282661,12.2,-9.31874797417473));
#166898=CARTESIAN_POINT('Ctrl Pts',(4.57873349763143,12.2,-9.32042248430923));
#166899=CARTESIAN_POINT('Ctrl Pts',(4.57979816282796,12.2,-9.32214130040799));
#166900=CARTESIAN_POINT('Ctrl Pts',(4.58086282792779,12.2,-9.32386011635063));
#166901=CARTESIAN_POINT('Ctrl Pts',(4.58196204049941,12.2,-9.32562323961556));
#166902=CARTESIAN_POINT('Ctrl Pts',(4.58309584770821,12.2,-9.32742955654993));
#166903=CARTESIAN_POINT('Ctrl Pts',(4.58422965491702,12.2,-9.32923587348429));
#166904=CARTESIAN_POINT('Ctrl Pts',(4.5853980563192,12.2,-9.33108538508538));
#166905=CARTESIAN_POINT('Ctrl Pts',(4.58660109166692,12.2,-9.33297701302539));
#166906=CARTESIAN_POINT('Ctrl Pts',(4.58780412712392,12.2,-9.33486864113721));
#166907=CARTESIAN_POINT('Ctrl Pts',(4.58904179768353,12.2,-9.33680238271311));
#166908=CARTESIAN_POINT('Ctrl Pts',(4.59031413808858,12.2,-9.33877718824021));
#166909=CARTESIAN_POINT('Ctrl Pts',(4.59158647837806,12.2,-9.34075199358794));
#166910=CARTESIAN_POINT('Ctrl Pts',(4.59289349004307,12.2,-9.34276786523282));
#166911=CARTESIAN_POINT('Ctrl Pts',(4.5942352060005,12.2,-9.34482377850088));
#166912=CARTESIAN_POINT('Ctrl Pts',(4.59557692195793,12.2,-9.34687969176897));
#166913=CARTESIAN_POINT('Ctrl Pts',(4.59695334073424,12.2,-9.34897564678802));
#166914=CARTESIAN_POINT('Ctrl Pts',(4.59836449093146,12.2,-9.35111065112542));
#166915=CARTESIAN_POINT('Ctrl Pts',(4.59977564125686,12.2,-9.35324565565676));
#166916=CARTESIAN_POINT('Ctrl Pts',(4.60122152409488,12.2,-9.35541970753459));
#166917=CARTESIAN_POINT('Ctrl Pts',(4.60270216417795,12.2,-9.35763183999108));
#166918=CARTESIAN_POINT('Ctrl Pts',(4.60418280412651,12.2,-9.35984397224663));
#166919=CARTESIAN_POINT('Ctrl Pts',(4.60569820106435,12.2,-9.36209418342296));
#166920=CARTESIAN_POINT('Ctrl Pts',(4.60724837709285,12.2,-9.36438152917477));
#166921=CARTESIAN_POINT('Ctrl Pts',(4.60879855312135,12.2,-9.36666887492659));
#166922=CARTESIAN_POINT('Ctrl Pts',(4.61038350778881,12.2,-9.36899335881716));
#166923=CARTESIAN_POINT('Ctrl Pts',(4.61200325789508,12.2,-9.37135405564644));
#166924=CARTESIAN_POINT('Ctrl Pts',(4.61362300800136,12.2,-9.37371475247571));
#166925=CARTESIAN_POINT('Ctrl Pts',(4.6152775579795,12.2,-9.3761116657423));
#166926=CARTESIAN_POINT('Ctrl Pts',(4.61696691708242,12.2,-9.37854389648485));
#166927=CARTESIAN_POINT('Ctrl Pts',(4.61865627633879,12.2,-9.38097612744834));
#166928=CARTESIAN_POINT('Ctrl Pts',(4.62038044630684,12.2,-9.38344367723194));
#166929=CARTESIAN_POINT('Ctrl Pts',(4.6221394413209,12.2,-9.38594566836979));
#166930=CARTESIAN_POINT('Ctrl Pts',(4.62389843617516,12.2,-9.38844765928039));
#166931=CARTESIAN_POINT('Ctrl Pts',(4.62569225239893,12.2,-9.39098409241391));
#166932=CARTESIAN_POINT('Ctrl Pts',(4.62752090125738,12.2,-9.39355411249878));
#166933=CARTESIAN_POINT('Ctrl Pts',(4.62965432503632,12.2,-9.39655246942012));
#166934=CARTESIAN_POINT('Ctrl Pts',(4.63183515898931,12.2,-9.39959654241051));
#166935=CARTESIAN_POINT('Ctrl Pts',(4.63406341059595,12.2,-9.4026850069196));
#166936=CARTESIAN_POINT('Ctrl Pts',(4.63597334044536,12.2,-9.40533226207569));
#166937=CARTESIAN_POINT('Ctrl Pts',(4.63791810759893,12.2,-9.40801213163557));
#166938=CARTESIAN_POINT('Ctrl Pts',(4.63989771385882,12.2,-9.41072380386899));
#166939=CARTESIAN_POINT('Ctrl Pts',(4.64187732011872,12.2,-9.41343547610242));
#166940=CARTESIAN_POINT('Ctrl Pts',(4.64389176767837,12.2,-9.41617895175048));
#166941=CARTESIAN_POINT('Ctrl Pts',(4.64594105451818,12.2,-9.41895343414755));
#166942=CARTESIAN_POINT('Ctrl Pts',(4.64799034154415,12.2,-9.42172791679664));
#166943=CARTESIAN_POINT('Ctrl Pts',(4.65007446671519,12.2,-9.42453340810711));
#166944=CARTESIAN_POINT('Ctrl Pts',(4.65219342783218,12.2,-9.42736913067964));
#166945=CARTESIAN_POINT('Ctrl Pts',(4.65431238875671,12.2,-9.43020485299459));
#166946=CARTESIAN_POINT('Ctrl Pts',(4.6564661859602,12.2,-9.43307080742409));
#166947=CARTESIAN_POINT('Ctrl Pts',(4.65865481280723,12.2,-9.43596623199865));
#166948=CARTESIAN_POINT('Ctrl Pts',(4.66084343965424,12.2,-9.43886165657323));
#166949=CARTESIAN_POINT('Ctrl Pts',(4.66306689596317,12.2,-9.4417865522873));
#166950=CARTESIAN_POINT('Ctrl Pts',(4.66532517296207,12.2,-9.44474017667803));
#166951=CARTESIAN_POINT('Ctrl Pts',(4.66758345016611,12.2,-9.44769380133706));
#166952=CARTESIAN_POINT('Ctrl Pts',(4.66987654967998,12.2,-9.45067615296685));
#166953=CARTESIAN_POINT('Ctrl Pts',(4.67220445892517,12.2,-9.45368650503292));
#166954=CARTESIAN_POINT('Ctrl Pts',(4.6745323679589,12.2,-9.45669685682556));
#166955=CARTESIAN_POINT('Ctrl Pts',(4.67689508671198,12.2,-9.45973520780301));
#166956=CARTESIAN_POINT('Ctrl Pts',(4.67929260254153,12.2,-9.46280084644161));
#166957=CARTESIAN_POINT('Ctrl Pts',(4.68169011837108,12.2,-9.46586648508022));
#166958=CARTESIAN_POINT('Ctrl Pts',(4.68412243150472,12.2,-9.46895940989898));
#166959=CARTESIAN_POINT('Ctrl Pts',(4.68658952378631,12.2,-9.47207892468993));
#166960=CARTESIAN_POINT('Ctrl Pts',(4.68864543409567,12.2,-9.47467852044351));
#166961=CARTESIAN_POINT('Ctrl Pts',(4.69072549915812,12.2,-9.4772965804064));
#166962=CARTESIAN_POINT('Ctrl Pts',(4.69282970658743,12.2,-9.47993270783602));
#166963=CARTESIAN_POINT('Ctrl Pts',(4.69493391401673,12.2,-9.48256883526565));
#166964=CARTESIAN_POINT('Ctrl Pts',(4.69706226372717,12.2,-9.48522303139291));
#166965=CARTESIAN_POINT('Ctrl Pts',(4.69921474685093,12.2,-9.48789490535034));
#166966=CARTESIAN_POINT('Ctrl Pts',(4.70136722997468,12.2,-9.49056677930778));
#166967=CARTESIAN_POINT('Ctrl Pts',(4.70354384427209,12.2,-9.49325633018069));
#166968=CARTESIAN_POINT('Ctrl Pts',(4.70574457678203,12.2,-9.49596317595684));
#166969=CARTESIAN_POINT('Ctrl Pts',(4.70794530929197,12.2,-9.49867002173299));
#166970=CARTESIAN_POINT('Ctrl Pts',(4.71017016234989,12.2,-9.50139416148887));
#166971=CARTESIAN_POINT('Ctrl Pts',(4.71241912047488,12.2,-9.50413521822497));
#166972=CARTESIAN_POINT('Ctrl Pts',(4.71466807859987,12.2,-9.50687627496106));
#166973=CARTESIAN_POINT('Ctrl Pts',(4.71694114156841,12.2,-9.50963424783884));
#166974=CARTESIAN_POINT('Ctrl Pts',(4.71923829650947,12.2,-9.51240876618482));
#166975=CARTESIAN_POINT('Ctrl Pts',(4.72153545145053,12.2,-9.51518328453081));
#166976=CARTESIAN_POINT('Ctrl Pts',(4.72385669858549,12.2,-9.51797434746616));
#166977=CARTESIAN_POINT('Ctrl Pts',(4.72620202087842,12.2,-9.52078159017534));
#166978=CARTESIAN_POINT('Ctrl Pts',(4.72854734317134,12.2,-9.52358883288451));
#166979=CARTESIAN_POINT('Ctrl Pts',(4.73091674152754,12.2,-9.5264122556905));
#166980=CARTESIAN_POINT('Ctrl Pts',(4.73331019888989,12.2,-9.52925149742742));
#166981=CARTESIAN_POINT('Ctrl Pts',(4.73570365625225,12.2,-9.53209073916435));
#166982=CARTESIAN_POINT('Ctrl Pts',(4.73812117286532,12.2,-9.53494580107768));
#166983=CARTESIAN_POINT('Ctrl Pts',(4.74056273201673,12.2,-9.53781632733326));
#166984=CARTESIAN_POINT('Ctrl Pts',(4.74300429116814,12.2,-9.54068685358883));
#166985=CARTESIAN_POINT('Ctrl Pts',(4.74546989343469,12.2,-9.54357284476711));
#166986=CARTESIAN_POINT('Ctrl Pts',(4.7479595183672,12.2,-9.54647395317112));
#166987=CARTESIAN_POINT('Ctrl Pts',(4.75044914329972,12.2,-9.54937506157513));
#166988=CARTESIAN_POINT('Ctrl Pts',(4.75296279254097,12.2,-9.55229128474327));
#166989=CARTESIAN_POINT('Ctrl Pts',(4.75550044580681,12.2,-9.55522228009169));
#166990=CARTESIAN_POINT('Ctrl Pts',(4.75803809879606,12.2,-9.55815327512063));
#166991=CARTESIAN_POINT('Ctrl Pts',(4.76059975812328,12.2,-9.56109904482553));
#166992=CARTESIAN_POINT('Ctrl Pts',(4.76318540110335,12.2,-9.56405924561279));
#166993=CARTESIAN_POINT('Ctrl Pts',(4.76628817318676,12.2,-9.56761148713828));
#166994=CARTESIAN_POINT('Ctrl Pts',(4.76942548359022,12.2,-9.57118451397422));
#166995=CARTESIAN_POINT('Ctrl Pts',(4.77259729568122,12.2,-9.57477774842089));
#166996=CARTESIAN_POINT('Ctrl Pts',(4.77524047227967,12.2,-9.57777211029659));
#166997=CARTESIAN_POINT('Ctrl Pts',(4.7779076078581,12.2,-9.58078050513585));
#166998=CARTESIAN_POINT('Ctrl Pts',(4.78059868265102,12.2,-9.5838026062477));
#166999=CARTESIAN_POINT('Ctrl Pts',(4.78328975744394,12.2,-9.58682470735954));
#167000=CARTESIAN_POINT('Ctrl Pts',(4.78600476912389,12.2,-9.58986051461742));
#167001=CARTESIAN_POINT('Ctrl Pts',(4.78874369585958,12.2,-9.59290970435399));
#167002=CARTESIAN_POINT('Ctrl Pts',(4.79148262259527,12.2,-9.59595889409057));
#167003=CARTESIAN_POINT('Ctrl Pts',(4.79424546551801,12.2,-9.59902146576233));
#167004=CARTESIAN_POINT('Ctrl Pts',(4.79703219808939,12.2,-9.60209710194394));
#167005=CARTESIAN_POINT('Ctrl Pts',(4.79926158396424,12.2,-9.60455761068807));
#167006=CARTESIAN_POINT('Ctrl Pts',(4.80150626298157,12.2,-9.60702647992004));
#167007=CARTESIAN_POINT('Ctrl Pts',(4.80376621807361,12.2,-9.60950354877256));
#167008=CARTESIAN_POINT('Ctrl Pts',(4.80602617347356,12.2,-9.61198061796259));
#167009=CARTESIAN_POINT('Ctrl Pts',(4.80830140771829,12.2,-9.6144658881857));
#167010=CARTESIAN_POINT('Ctrl Pts',(4.81059190779221,12.2,-9.6169591981135));
#167011=CARTESIAN_POINT('Ctrl Pts',(4.81345503272857,12.2,-9.6200758353534));
#167012=CARTESIAN_POINT('Ctrl Pts',(4.81634200971201,12.2,-9.62320503612101));
#167013=CARTESIAN_POINT('Ctrl Pts',(4.81925281367229,12.2,-9.62634649167755));
#167014=CARTESIAN_POINT('Ctrl Pts',(4.82158145665014,12.2,-9.62885965591734));
#167015=CARTESIAN_POINT('Ctrl Pts',(4.82392534859546,12.2,-9.63138066453388));
#167016=CARTESIAN_POINT('Ctrl Pts',(4.82628447629051,12.2,-9.63390936199334));
#167017=CARTESIAN_POINT('Ctrl Pts',(4.82864360430698,12.2,-9.63643805979733));
#167018=CARTESIAN_POINT('Ctrl Pts',(4.83101796937634,12.2,-9.638974445925));
#167019=CARTESIAN_POINT('Ctrl Pts',(4.83340755557171,12.2,-9.64151836663583));
#167020=CARTESIAN_POINT('Ctrl Pts',(4.8357971414415,12.2,-9.64406228700005));
#167021=CARTESIAN_POINT('Ctrl Pts',(4.83820194925935,12.2,-9.64661374168387));
#167022=CARTESIAN_POINT('Ctrl Pts',(4.84062196556053,12.2,-9.64917257980754));
#167023=CARTESIAN_POINT('Ctrl Pts',(4.84304198219142,12.2,-9.65173141827984));
#167024=CARTESIAN_POINT('Ctrl Pts',(4.84547720705748,12.2,-9.65429763929749));
#167025=CARTESIAN_POINT('Ctrl Pts',(4.84792762569202,12.2,-9.65687109199377));
#167026=CARTESIAN_POINT('Ctrl Pts',(4.85037804399269,12.2,-9.65944454433941));
#167027=CARTESIAN_POINT('Ctrl Pts',(4.85284365539239,12.2,-9.66202522954351));
#167028=CARTESIAN_POINT('Ctrl Pts',(4.85532444708999,12.2,-9.66461299784952));
#167029=CARTESIAN_POINT('Ctrl Pts',(4.8578052391256,12.2,-9.66720076650812));
#167030=CARTESIAN_POINT('Ctrl Pts',(4.86030121057858,12.2,-9.66979561792327));
#167031=CARTESIAN_POINT('Ctrl Pts',(4.86281234593865,12.2,-9.67239740645441));
#167032=CARTESIAN_POINT('Ctrl Pts',(4.86532348095657,12.2,-9.67499919463106));
#167033=CARTESIAN_POINT('Ctrl Pts',(4.86784978065201,12.2,-9.67760791779519));
#167034=CARTESIAN_POINT('Ctrl Pts',(4.87039122960937,12.2,-9.68022343208069));
#167035=CARTESIAN_POINT('Ctrl Pts',(4.87293267891299,12.2,-9.68283894672254));
#167036=CARTESIAN_POINT('Ctrl Pts',(4.87548927804419,12.2,-9.68546125174097));
#167037=CARTESIAN_POINT('Ctrl Pts',(4.87806101075164,12.2,-9.68809020178511));
#167038=CARTESIAN_POINT('Ctrl Pts',(4.88063274310869,12.2,-9.69071915147105));
#167039=CARTESIAN_POINT('Ctrl Pts',(4.88321960949983,12.2,-9.69335474786243));
#167040=CARTESIAN_POINT('Ctrl Pts',(4.88582159384114,12.2,-9.69599684753468));
#167041=CARTESIAN_POINT('Ctrl Pts',(4.88842357853696,12.2,-9.6986389475669));
#167042=CARTESIAN_POINT('Ctrl Pts',(4.89104068168142,12.2,-9.70128755079418));
#167043=CARTESIAN_POINT('Ctrl Pts',(4.89367288699155,12.2,-9.70394251604998));
#167044=CARTESIAN_POINT('Ctrl Pts',(4.89630509230166,12.2,-9.70659748130578));
#167045=CARTESIAN_POINT('Ctrl Pts',(4.89895240050244,12.2,-9.70925880748178));
#167046=CARTESIAN_POINT('Ctrl Pts',(4.90161479392686,12.2,-9.7119263561278));
#167047=CARTESIAN_POINT('Ctrl Pts',(4.90427718698853,12.2,-9.71459390441036));
#167048=CARTESIAN_POINT('Ctrl Pts',(4.90695466801434,12.2,-9.71726767529121));
#167049=CARTESIAN_POINT('Ctrl Pts',(4.90964721697305,12.2,-9.71994752847316));
#167050=CARTESIAN_POINT('Ctrl Pts',(4.91233976629863,12.2,-9.72262738202025));
#167051=CARTESIAN_POINT('Ctrl Pts',(4.9150473860368,12.2,-9.72531331995113));
#167052=CARTESIAN_POINT('Ctrl Pts',(4.91777005868672,12.2,-9.72800520393178));
#167053=CARTESIAN_POINT('Ctrl Pts',(4.92049273096567,12.2,-9.73069708754566));
#167054=CARTESIAN_POINT('Ctrl Pts',(4.92323045634267,12.2,-9.73339491785597));
#167055=CARTESIAN_POINT('Ctrl Pts',(4.92598321728332,12.2,-9.73609855707902));
#167056=CARTESIAN_POINT('Ctrl Pts',(4.92873597859904,12.2,-9.73880219667045));
#167057=CARTESIAN_POINT('Ctrl Pts',(4.9315037762229,12.2,-9.74151164834323));
#167058=CARTESIAN_POINT('Ctrl Pts',(4.93428659240377,12.2,-9.74422677462734));
#167059=CARTESIAN_POINT('Ctrl Pts',(4.93706940820549,12.2,-9.74694190054151));
#167060=CARTESIAN_POINT('Ctrl Pts',(4.93986724227323,12.2,-9.74966270318374));
#167061=CARTESIAN_POINT('Ctrl Pts',(4.94268007848674,12.2,-9.75238904829383));
#167062=CARTESIAN_POINT('Ctrl Pts',(4.94619612404108,12.2,-9.75579697996004));
#167063=CARTESIAN_POINT('Ctrl Pts',(4.94973560847935,12.2,-9.75921357279315));
#167064=CARTESIAN_POINT('Ctrl Pts',(4.95329849903368,12.2,-9.76263856779271));
#167065=CARTESIAN_POINT('Ctrl Pts',(4.95614881163249,12.2,-9.76537856394169));
#167066=CARTESIAN_POINT('Ctrl Pts',(4.95901410263243,12.2,-9.76812393955583));
#167067=CARTESIAN_POINT('Ctrl Pts',(4.96189435593458,12.2,-9.77087456139916));
#167068=CARTESIAN_POINT('Ctrl Pts',(4.96477460884431,12.2,-9.77362518286772));
#167069=CARTESIAN_POINT('Ctrl Pts',(4.9676698214871,12.2,-9.77638105316425));
#167070=CARTESIAN_POINT('Ctrl Pts',(4.97057997830379,12.2,-9.77914204154933));
#167071=CARTESIAN_POINT('Ctrl Pts',(4.97421767462202,12.2,-9.78259327731281));
#167072=CARTESIAN_POINT('Ctrl Pts',(4.97787871967697,12.2,-9.78605251049038));
#167073=CARTESIAN_POINT('Ctrl Pts',(4.98156307550907,12.2,-9.78951949298997));
#167074=CARTESIAN_POINT('Ctrl Pts',(4.98524743134117,12.2,-9.79298647548955));
#167075=CARTESIAN_POINT('Ctrl Pts',(4.98895510245724,12.2,-9.7964612059838));
#167076=CARTESIAN_POINT('Ctrl Pts',(4.99268604724769,12.2,-9.79994343778897));
#167077=CARTESIAN_POINT('Ctrl Pts',(4.99567080324272,12.2,-9.80272922338492));
#167078=CARTESIAN_POINT('Ctrl Pts',(4.99867045525731,12.2,-9.80551981066045));
#167079=CARTESIAN_POINT('Ctrl Pts',(5.00168498596239,12.2,-9.80831507489729));
#167080=CARTESIAN_POINT('Ctrl Pts',(5.00469951625674,12.2,-9.81111033875329));
#167081=CARTESIAN_POINT('Ctrl Pts',(5.00772892316488,12.2,-9.81391027710032));
#167082=CARTESIAN_POINT('Ctrl Pts',(5.01077318819283,12.2,-9.81671476953744));
#167083=CARTESIAN_POINT('Ctrl Pts',(5.01381745363556,12.2,-9.81951926235666));
#167084=CARTESIAN_POINT('Ctrl Pts',(5.01687657826894,12.2,-9.82232830744308));
#167085=CARTESIAN_POINT('Ctrl Pts',(5.019950541493,12.2,-9.82514178226338));
#167086=CARTESIAN_POINT('Ctrl Pts',(5.02302450429823,12.2,-9.82795525670034));
#167087=CARTESIAN_POINT('Ctrl Pts',(5.02611330502179,12.2,-9.83077316011948));
#167088=CARTESIAN_POINT('Ctrl Pts',(5.02921692603295,12.2,-9.83359537280717));
#167089=CARTESIAN_POINT('Ctrl Pts',(5.03232054746697,12.2,-9.83641758587938));
#167090=CARTESIAN_POINT('Ctrl Pts',(5.03543898819278,12.2,-9.83924410726024));
#167091=CARTESIAN_POINT('Ctrl Pts',(5.03857222753117,12.2,-9.84207481674811));
#167092=CARTESIAN_POINT('Ctrl Pts',(5.04170546644265,12.2,-9.8449055258503));
#167093=CARTESIAN_POINT('Ctrl Pts',(5.04485350520118,12.2,-9.8477404231461));
#167094=CARTESIAN_POINT('Ctrl Pts',(5.04801632277444,12.2,-9.85057938780249));
#167095=CARTESIAN_POINT('Ctrl Pts',(5.05117914077863,12.2,-9.85341835284568));
#167096=CARTESIAN_POINT('Ctrl Pts',(5.0543567388913,12.2,-9.85626138643381));
#167097=CARTESIAN_POINT('Ctrl Pts',(5.05754909496873,12.2,-9.85910837126861));
#167098=CARTESIAN_POINT('Ctrl Pts',(5.06153953984804,12.2,-9.86266710211814));
#167099=CARTESIAN_POINT('Ctrl Pts',(5.06555304729059,12.2,-9.86623200453327));
#167100=CARTESIAN_POINT('Ctrl Pts',(5.06958957451401,12.2,-9.8698028497419));
#167101=CARTESIAN_POINT('Ctrl Pts',(5.07281879602875,12.2,-9.87265952567528));
#167102=CARTESIAN_POINT('Ctrl Pts',(5.07606275000722,12.2,-9.87552000557456));
#167103=CARTESIAN_POINT('Ctrl Pts',(5.0793214175171,12.2,-9.87838417350671));
#167104=CARTESIAN_POINT('Ctrl Pts',(5.08258008547098,12.2,-9.8812483418291));
#167105=CARTESIAN_POINT('Ctrl Pts',(5.08585346667739,12.2,-9.88411619788519));
#167106=CARTESIAN_POINT('Ctrl Pts',(5.08914153926046,12.2,-9.88698762677695));
#167107=CARTESIAN_POINT('Ctrl Pts',(5.0932516297653,12.2,-9.89057691269605));
#167108=CARTESIAN_POINT('Ctrl Pts',(5.09738467640395,12.2,-9.89417178020187));
#167109=CARTESIAN_POINT('Ctrl Pts',(5.10154063703015,12.2,-9.89777200874382));
#167110=CARTESIAN_POINT('Ctrl Pts',(5.10486540525931,12.2,-9.90065219134192));
#167111=CARTESIAN_POINT('Ctrl Pts',(5.10820483866885,12.2,-9.90353580266432));
#167112=CARTESIAN_POINT('Ctrl Pts',(5.1115589162265,12.2,-9.90642273376132));
#167113=CARTESIAN_POINT('Ctrl Pts',(5.11491299424114,12.2,-9.90930966525166));
#167114=CARTESIAN_POINT('Ctrl Pts',(5.11828171662183,12.2,-9.91219991338946));
#167115=CARTESIAN_POINT('Ctrl Pts',(5.12166506121053,12.2,-9.91509336772697));
#167116=CARTESIAN_POINT('Ctrl Pts',(5.12420256942157,12.2,-9.91726345828299));
#167117=CARTESIAN_POINT('Ctrl Pts',(5.1267483029788,12.2,-9.91943535220047));
#167118=CARTESIAN_POINT('Ctrl Pts',(5.12930225227257,12.2,-9.92160900275636));
#167119=CARTESIAN_POINT('Ctrl Pts',(5.13185620156634,12.2,-9.92378265331226));
#167120=CARTESIAN_POINT('Ctrl Pts',(5.13441836786396,12.2,-9.92595806039197));
#167121=CARTESIAN_POINT('Ctrl Pts',(5.13698873968652,12.2,-9.92813517697939));
#167122=CARTESIAN_POINT('Ctrl Pts',(5.13955911150909,12.2,-9.93031229356681));
#167123=CARTESIAN_POINT('Ctrl Pts',(5.14213769076441,12.2,-9.9324911200041));
#167124=CARTESIAN_POINT('Ctrl Pts',(5.14472446746098,12.2,-9.93467161100799));
#167125=CARTESIAN_POINT('Ctrl Pts',(5.14731124462747,12.2,-9.93685210240799));
#167126=CARTESIAN_POINT('Ctrl Pts',(5.14990621883794,12.2,-9.93903425782513));
#167127=CARTESIAN_POINT('Ctrl Pts',(5.15250938109238,12.2,-9.94121803076773));
#167128=CARTESIAN_POINT('Ctrl Pts',(5.15511254287392,12.2,-9.94340180331361));
#167129=CARTESIAN_POINT('Ctrl Pts',(5.15772389388682,12.2,-9.9455871930265));
#167130=CARTESIAN_POINT('Ctrl Pts',(5.16034342329846,12.2,-9.94777415563981));
#167131=CARTESIAN_POINT('Ctrl Pts',(5.16296295271009,12.2,-9.94996111825313));
#167132=CARTESIAN_POINT('Ctrl Pts',(5.16559066093239,12.2,-9.95214965205152));
#167133=CARTESIAN_POINT('Ctrl Pts',(5.16822653779567,12.2,-9.95433971351375));
#167134=CARTESIAN_POINT('Ctrl Pts',(5.17086241465894,12.2,-9.95652977497597));
#167135=CARTESIAN_POINT('Ctrl Pts',(5.17350646224624,12.2,-9.95872136234635));
#167136=CARTESIAN_POINT('Ctrl Pts',(5.17615866898321,12.2,-9.96091443276667));
#167137=CARTESIAN_POINT('Ctrl Pts',(5.17881087572018,12.2,-9.96310750318699));
#167138=CARTESIAN_POINT('Ctrl Pts',(5.18147124182349,12.2,-9.96530205405724));
#167139=CARTESIAN_POINT('Ctrl Pts',(5.18413975897583,12.2,-9.96749804260233));
#167140=CARTESIAN_POINT('Ctrl Pts',(5.18680827612816,12.2,-9.96969403114742));
#167141=CARTESIAN_POINT('Ctrl Pts',(5.18948494291156,12.2,-9.97189145606147));
#167142=CARTESIAN_POINT('Ctrl Pts',(5.19216975123886,12.2,-9.9740902737996));
#167143=CARTESIAN_POINT('Ctrl Pts',(5.19574949600042,12.2,-9.97702203105007));
#167144=CARTESIAN_POINT('Ctrl Pts',(5.19934371189465,12.2,-9.97995626288546));
#167145=CARTESIAN_POINT('Ctrl Pts',(5.2029523790367,12.2,-9.98289286649009));
#167146=CARTESIAN_POINT('Ctrl Pts',(5.20565887914739,12.2,-9.98509531899352));
#167147=CARTESIAN_POINT('Ctrl Pts',(5.20837350631548,12.2,-9.98729910394679));
#167148=CARTESIAN_POINT('Ctrl Pts',(5.21109625200821,12.2,-9.98950417899167));
#167149=CARTESIAN_POINT('Ctrl Pts',(5.21381899770095,12.2,-9.99170925403654));
#167150=CARTESIAN_POINT('Ctrl Pts',(5.21654986121836,12.2,-9.99391561827304));
#167151=CARTESIAN_POINT('Ctrl Pts',(5.21928883340981,12.2,-9.99612322927606));
#167152=CARTESIAN_POINT('Ctrl Pts',(5.22202780560126,12.2,-9.99833084027908));
#167153=CARTESIAN_POINT('Ctrl Pts',(5.22477488589697,12.2,-10.0005396955924));
#167154=CARTESIAN_POINT('Ctrl Pts',(5.22753006522524,12.2,-10.0027497542891));
#167155=CARTESIAN_POINT('Ctrl Pts',(5.23028524455351,12.2,-10.0049598129857));
#167156=CARTESIAN_POINT('Ctrl Pts',(5.23304852239753,12.2,-10.0071710741482));
#167157=CARTESIAN_POINT('Ctrl Pts',(5.23581988862907,12.2,-10.009383494776));
#167158=CARTESIAN_POINT('Ctrl Pts',(5.23859125536407,12.2,-10.0115959158057));
#167159=CARTESIAN_POINT('Ctrl Pts',(5.24137071086803,12.2,-10.0138094972275));
#167160=CARTESIAN_POINT('Ctrl Pts',(5.24415824510758,12.2,-10.0160241942578));
#167161=CARTESIAN_POINT('Ctrl Pts',(5.24787495658297,12.2,-10.018977122961));
#167162=CARTESIAN_POINT('Ctrl Pts',(5.2516060308065,12.2,-10.0219320355112));
#167163=CARTESIAN_POINT('Ctrl Pts',(5.25535144294384,12.2,-10.0248888334916));
#167164=CARTESIAN_POINT('Ctrl Pts',(5.25816050217442,12.2,-10.0271064320776));
#167165=CARTESIAN_POINT('Ctrl Pts',(5.26097762743775,12.2,-10.0293250901802));
#167166=CARTESIAN_POINT('Ctrl Pts',(5.26380280766734,12.2,-10.0315447658078));
#167167=CARTESIAN_POINT('Ctrl Pts',(5.26662798841017,12.2,-10.0337644418386));
#167168=CARTESIAN_POINT('Ctrl Pts',(5.26946122435527,12.2,-10.035985135178));
#167169=CARTESIAN_POINT('Ctrl Pts',(5.27230250560263,12.2,-10.0382068042093));
#167170=CARTESIAN_POINT('Ctrl Pts',(5.27609087973883,12.2,-10.0411690289118));
#167171=CARTESIAN_POINT('Ctrl Pts',(5.27989355796704,12.2,-10.0441329885297));
#167172=CARTESIAN_POINT('Ctrl Pts',(5.28371051350562,12.2,-10.0470985826897));
#167173=CARTESIAN_POINT('Ctrl Pts',(5.28657323028958,12.2,-10.0493227784106));
#167174=CARTESIAN_POINT('Ctrl Pts',(5.28944397922486,12.2,-10.0515478941217));
#167175=CARTESIAN_POINT('Ctrl Pts',(5.2923227494529,12.2,-10.0537738882491));
#167176=CARTESIAN_POINT('Ctrl Pts',(5.29520151968094,12.2,-10.0559998823764));
#167177=CARTESIAN_POINT('Ctrl Pts',(5.2980883114251,12.2,-10.0582267551621));
#167178=CARTESIAN_POINT('Ctrl Pts',(5.3009831146105,12.2,-10.0604544647894));
#167179=CARTESIAN_POINT('Ctrl Pts',(5.30387791832178,12.2,-10.0626821748214));
#167180=CARTESIAN_POINT('Ctrl Pts',(5.30678073296032,12.2,-10.0649107217619));
#167181=CARTESIAN_POINT('Ctrl Pts',(5.30969154913446,12.2,-10.0671400657943));
#167182=CARTESIAN_POINT('Ctrl Pts',(5.31260236477979,12.2,-10.0693694094218));
#167183=CARTESIAN_POINT('Ctrl Pts',(5.31552118099209,12.2,-10.0715995491345));
#167184=CARTESIAN_POINT('Ctrl Pts',(5.31844798832456,12.2,-10.073830444415));
#167185=CARTESIAN_POINT('Ctrl Pts',(5.32137479565703,12.2,-10.0760613396954));
#167186=CARTESIAN_POINT('Ctrl Pts',(5.32430959359368,12.2,-10.0782929900911));
#167187=CARTESIAN_POINT('Ctrl Pts',(5.32725237132079,12.2,-10.08052535526));
#167188=CARTESIAN_POINT('Ctrl Pts',(5.33019514904789,12.2,-10.082757720429));
#167189=CARTESIAN_POINT('Ctrl Pts',(5.33314590727405,12.2,-10.0849908006478));
#167190=CARTESIAN_POINT('Ctrl Pts',(5.33610463504155,12.2,-10.087224556275));
#167191=CARTESIAN_POINT('Ctrl Pts',(5.34004960575655,12.2,-10.0902028973818));
#167192=CARTESIAN_POINT('Ctrl Pts',(5.34400874576488,12.2,-10.0931824386609));
#167193=CARTESIAN_POINT('Ctrl Pts',(5.34798202964953,12.2,-10.0961630852123));
#167194=CARTESIAN_POINT('Ctrl Pts',(5.35096199229234,12.2,-10.0983985699229));
#167195=CARTESIAN_POINT('Ctrl Pts',(5.35394991103786,12.2,-10.1006346766689));
#167196=CARTESIAN_POINT('Ctrl Pts',(5.35694577437126,12.2,-10.1028713629494));
#167197=CARTESIAN_POINT('Ctrl Pts',(5.35994163770465,12.2,-10.10510804923));
#167198=CARTESIAN_POINT('Ctrl Pts',(5.36294544513703,12.2,-10.1073453142585));
#167199=CARTESIAN_POINT('Ctrl Pts',(5.36595718781997,12.2,-10.1095831229689));
#167200=CARTESIAN_POINT('Ctrl Pts',(5.3689689305029,12.2,-10.1118209316793));
#167201=CARTESIAN_POINT('Ctrl Pts',(5.37198860734323,12.2,-10.114059283598));
#167202=CARTESIAN_POINT('Ctrl Pts',(5.37501620998322,12.2,-10.1162981422667));
#167203=CARTESIAN_POINT('Ctrl Pts',(5.3780438126232,12.2,-10.1185370009353));
#167204=CARTESIAN_POINT('Ctrl Pts',(5.38107934056289,12.2,-10.1207763669873));
#167205=CARTESIAN_POINT('Ctrl Pts',(5.38412278120162,12.2,-10.1230161955309));
#167206=CARTESIAN_POINT('Ctrl Pts',(5.38716622184035,12.2,-10.1252560240745));
#167207=CARTESIAN_POINT('Ctrl Pts',(5.39021757455064,12.2,-10.1274963140527));
#167208=CARTESIAN_POINT('Ctrl Pts',(5.39327682838308,12.2,-10.1297370198332));
#167209=CARTESIAN_POINT('Ctrl Pts',(5.39735583386349,12.2,-10.1327246278118));
#167210=CARTESIAN_POINT('Ctrl Pts',(5.40144888316411,12.2,-10.1357129685643));
#167211=CARTESIAN_POINT('Ctrl Pts',(5.40555595936562,12.2,-10.1387019911788));
#167212=CARTESIAN_POINT('Ctrl Pts',(5.40863626623696,12.2,-10.140943757936));
#167213=CARTESIAN_POINT('Ctrl Pts',(5.41172446743749,12.2,-10.1431859065926));
#167214=CARTESIAN_POINT('Ctrl Pts',(5.41482055299994,12.2,-10.145428447));
#167215=CARTESIAN_POINT('Origin',(-5.66257110645729E-14,15.2,-1.77635683940025E-14));
#167216=CARTESIAN_POINT('',(5.85257411399994,15.2,-8.56667970900002));
#167217=CARTESIAN_POINT('',(5.85257411399994,12.2,-8.56667970900002));
#167218=CARTESIAN_POINT('',(5.85257411399994,15.2,-8.56667970900002));
#167219=CARTESIAN_POINT('Origin',(-5.66257110645729E-14,12.2,-1.77635683940025E-14));
#167220=CARTESIAN_POINT('Origin',(-5.66257110645729E-14,15.2,-1.77635683940025E-14));
#167221=CARTESIAN_POINT('Origin',(-5.66257110645729E-14,15.2,-1.77635683940025E-14));
#167222=CARTESIAN_POINT('',(6.80355049614186,15.2,-9.27155330252674));
#167223=CARTESIAN_POINT('',(7.10901226899994,15.2,-9.03946594400002));
#167224=CARTESIAN_POINT('Origin',(-5.66257110645729E-14,15.2,-1.77635683940025E-14));
#167225=CARTESIAN_POINT('',(7.10901226899994,12.2,-9.03946594400002));
#167226=CARTESIAN_POINT('',(7.10901226899994,15.2,-9.03946594400002));
#167227=CARTESIAN_POINT('',(6.80355049614186,12.2,-9.27155330252674));
#167228=CARTESIAN_POINT('Origin',(-5.66257110645729E-14,12.2,-1.77635683940025E-14));
#167229=CARTESIAN_POINT('',(6.80355049599994,15.2,-9.27155330200002));
#167230=CARTESIAN_POINT('Ctrl Pts',(5.85257411399994,15.2,-8.56667970900002));
#167231=CARTESIAN_POINT('Ctrl Pts',(5.85257411399994,11.6,-8.56667970900002));
#167232=CARTESIAN_POINT('Ctrl Pts',(5.85268447799995,15.2,-8.56681469200002));
#167233=CARTESIAN_POINT('Ctrl Pts',(5.85268447799995,11.6,-8.56681469200002));
#167234=CARTESIAN_POINT('Ctrl Pts',(5.85290912899994,15.2,-8.56708931900002));
#167235=CARTESIAN_POINT('Ctrl Pts',(5.85290912899994,11.6,-8.56708931900002));
#167236=CARTESIAN_POINT('Ctrl Pts',(5.85324973299994,15.2,-8.56750527300001));
#167237=CARTESIAN_POINT('Ctrl Pts',(5.85324973299994,11.6,-8.56750527300001));
#167238=CARTESIAN_POINT('Ctrl Pts',(5.85370897499994,15.2,-8.56806526200002));
#167239=CARTESIAN_POINT('Ctrl Pts',(5.85370897499994,11.6,-8.56806526200002));
#167240=CARTESIAN_POINT('Ctrl Pts',(5.85429055399994,15.2,-8.56877298400001));
#167241=CARTESIAN_POINT('Ctrl Pts',(5.85429055399994,11.6,-8.56877298400001));
#167242=CARTESIAN_POINT('Ctrl Pts',(5.85488228099995,15.2,-8.56949158200001));
#167243=CARTESIAN_POINT('Ctrl Pts',(5.85488228099995,11.6,-8.56949158200001));
#167244=CARTESIAN_POINT('Ctrl Pts',(5.85548078499994,15.2,-8.57021692600001));
#167245=CARTESIAN_POINT('Ctrl Pts',(5.85548078499994,11.6,-8.57021692600001));
#167246=CARTESIAN_POINT('Ctrl Pts',(5.85608606099995,15.2,-8.57094898200002));
#167247=CARTESIAN_POINT('Ctrl Pts',(5.85608606099995,11.6,-8.57094898200002));
#167248=CARTESIAN_POINT('Ctrl Pts',(5.85669810699994,15.2,-8.57168771800002));
#167249=CARTESIAN_POINT('Ctrl Pts',(5.85669810699994,11.6,-8.57168771800002));
#167250=CARTESIAN_POINT('Ctrl Pts',(5.85731691799994,15.2,-8.57243310300002));
#167251=CARTESIAN_POINT('Ctrl Pts',(5.85731691799994,11.6,-8.57243310300002));
#167252=CARTESIAN_POINT('Ctrl Pts',(5.85794249299994,15.2,-8.57318510400002));
#167253=CARTESIAN_POINT('Ctrl Pts',(5.85794249299994,11.6,-8.57318510400002));
#167254=CARTESIAN_POINT('Ctrl Pts',(5.85857482799995,15.2,-8.57394368900002));
#167255=CARTESIAN_POINT('Ctrl Pts',(5.85857482799995,11.6,-8.57394368900002));
#167256=CARTESIAN_POINT('Ctrl Pts',(5.85921391899995,15.2,-8.57470882600002));
#167257=CARTESIAN_POINT('Ctrl Pts',(5.85921391899995,11.6,-8.57470882600002));
#167258=CARTESIAN_POINT('Ctrl Pts',(5.85985976499994,15.2,-8.57548048600002));
#167259=CARTESIAN_POINT('Ctrl Pts',(5.85985976499994,11.6,-8.57548048600002));
#167260=CARTESIAN_POINT('Ctrl Pts',(5.86051236099995,15.2,-8.57625863500001));
#167261=CARTESIAN_POINT('Ctrl Pts',(5.86051236099995,11.6,-8.57625863500001));
#167262=CARTESIAN_POINT('Ctrl Pts',(5.86117170399994,15.2,-8.57704324400002));
#167263=CARTESIAN_POINT('Ctrl Pts',(5.86117170399994,11.6,-8.57704324400002));
#167264=CARTESIAN_POINT('Ctrl Pts',(5.86183779199994,15.2,-8.57783428100002));
#167265=CARTESIAN_POINT('Ctrl Pts',(5.86183779199994,11.6,-8.57783428100002));
#167266=CARTESIAN_POINT('Ctrl Pts',(5.86251061899994,15.2,-8.57863171400002));
#167267=CARTESIAN_POINT('Ctrl Pts',(5.86251061899994,11.6,-8.57863171400002));
#167268=CARTESIAN_POINT('Ctrl Pts',(5.86319018499994,15.2,-8.57943551500002));
#167269=CARTESIAN_POINT('Ctrl Pts',(5.86319018499994,11.6,-8.57943551500002));
#167270=CARTESIAN_POINT('Ctrl Pts',(5.86387648599994,15.2,-8.58024565100001));
#167271=CARTESIAN_POINT('Ctrl Pts',(5.86387648599994,11.6,-8.58024565100001));
#167272=CARTESIAN_POINT('Ctrl Pts',(5.86456951799994,15.2,-8.58106209400002));
#167273=CARTESIAN_POINT('Ctrl Pts',(5.86456951799994,11.6,-8.58106209400002));
#167274=CARTESIAN_POINT('Ctrl Pts',(5.86526927899994,15.2,-8.58188481300001));
#167275=CARTESIAN_POINT('Ctrl Pts',(5.86526927899994,11.6,-8.58188481300001));
#167276=CARTESIAN_POINT('Ctrl Pts',(5.86597576599994,15.2,-8.58271377600002));
#167277=CARTESIAN_POINT('Ctrl Pts',(5.86597576599994,11.6,-8.58271377600002));
#167278=CARTESIAN_POINT('Ctrl Pts',(5.86668897299995,15.2,-8.58354895500002));
#167279=CARTESIAN_POINT('Ctrl Pts',(5.86668897299995,11.6,-8.58354895500002));
#167280=CARTESIAN_POINT('Ctrl Pts',(5.86740889999994,15.2,-8.58439031900001));
#167281=CARTESIAN_POINT('Ctrl Pts',(5.86740889999994,11.6,-8.58439031900001));
#167282=CARTESIAN_POINT('Ctrl Pts',(5.86813554199995,15.2,-8.58523784000001));
#167283=CARTESIAN_POINT('Ctrl Pts',(5.86813554199995,11.6,-8.58523784000001));
#167284=CARTESIAN_POINT('Ctrl Pts',(5.86886889699994,15.2,-8.58609148700002));
#167285=CARTESIAN_POINT('Ctrl Pts',(5.86886889699994,11.6,-8.58609148700002));
#167286=CARTESIAN_POINT('Ctrl Pts',(5.86960896099994,15.2,-8.58695123200001));
#167287=CARTESIAN_POINT('Ctrl Pts',(5.86960896099994,11.6,-8.58695123200001));
#167288=CARTESIAN_POINT('Ctrl Pts',(5.87035573299994,15.2,-8.58781704500002));
#167289=CARTESIAN_POINT('Ctrl Pts',(5.87035573299994,11.6,-8.58781704500002));
#167290=CARTESIAN_POINT('Ctrl Pts',(5.87110920599994,15.2,-8.58868889600001));
#167291=CARTESIAN_POINT('Ctrl Pts',(5.87110920599994,11.6,-8.58868889600001));
#167292=CARTESIAN_POINT('Ctrl Pts',(5.87186938099994,15.2,-8.58956675700002));
#167293=CARTESIAN_POINT('Ctrl Pts',(5.87186938099994,11.6,-8.58956675700002));
#167294=CARTESIAN_POINT('Ctrl Pts',(5.87263625099995,15.2,-8.59045059900001));
#167295=CARTESIAN_POINT('Ctrl Pts',(5.87263625099995,11.6,-8.59045059900001));
#167296=CARTESIAN_POINT('Ctrl Pts',(5.87340981499994,15.2,-8.59134039400002));
#167297=CARTESIAN_POINT('Ctrl Pts',(5.87340981499994,11.6,-8.59134039400002));
#167298=CARTESIAN_POINT('Ctrl Pts',(5.87419006999994,15.2,-8.59223611300001));
#167299=CARTESIAN_POINT('Ctrl Pts',(5.87419006999994,11.6,-8.59223611300001));
#167300=CARTESIAN_POINT('Ctrl Pts',(5.87497701299994,15.2,-8.59313772700002));
#167301=CARTESIAN_POINT('Ctrl Pts',(5.87497701299994,11.6,-8.59313772700002));
#167302=CARTESIAN_POINT('Ctrl Pts',(5.87577063899994,15.2,-8.59404520900002));
#167303=CARTESIAN_POINT('Ctrl Pts',(5.87577063899994,11.6,-8.59404520900002));
#167304=CARTESIAN_POINT('Ctrl Pts',(5.87657094599994,15.2,-8.59495852900002));
#167305=CARTESIAN_POINT('Ctrl Pts',(5.87657094599994,11.6,-8.59495852900002));
#167306=CARTESIAN_POINT('Ctrl Pts',(5.87737793199994,15.2,-8.59587766000002));
#167307=CARTESIAN_POINT('Ctrl Pts',(5.87737793199994,11.6,-8.59587766000002));
#167308=CARTESIAN_POINT('Ctrl Pts',(5.87819159199994,15.2,-8.59680257500001));
#167309=CARTESIAN_POINT('Ctrl Pts',(5.87819159199994,11.6,-8.59680257500001));
#167310=CARTESIAN_POINT('Ctrl Pts',(5.87901192399994,15.2,-8.59773324500001));
#167311=CARTESIAN_POINT('Ctrl Pts',(5.87901192399994,11.6,-8.59773324500001));
#167312=CARTESIAN_POINT('Ctrl Pts',(5.87983892499994,15.2,-8.59866964200002));
#167313=CARTESIAN_POINT('Ctrl Pts',(5.87983892499994,11.6,-8.59866964200002));
#167314=CARTESIAN_POINT('Ctrl Pts',(5.88067259099994,15.2,-8.59961174000002));
#167315=CARTESIAN_POINT('Ctrl Pts',(5.88067259099994,11.6,-8.59961174000002));
#167316=CARTESIAN_POINT('Ctrl Pts',(5.88151291899995,15.2,-8.60055951000002));
#167317=CARTESIAN_POINT('Ctrl Pts',(5.88151291899995,11.6,-8.60055951000002));
#167318=CARTESIAN_POINT('Ctrl Pts',(5.88235990599995,15.2,-8.60151292500002));
#167319=CARTESIAN_POINT('Ctrl Pts',(5.88235990599995,11.6,-8.60151292500002));
#167320=CARTESIAN_POINT('Ctrl Pts',(5.88321354999994,15.2,-8.60247195900002));
#167321=CARTESIAN_POINT('Ctrl Pts',(5.88321354999994,11.6,-8.60247195900002));
#167322=CARTESIAN_POINT('Ctrl Pts',(5.88407384499994,15.2,-8.60343658400001));
#167323=CARTESIAN_POINT('Ctrl Pts',(5.88407384499994,11.6,-8.60343658400001));
#167324=CARTESIAN_POINT('Ctrl Pts',(5.88494079099994,15.2,-8.60440677400002));
#167325=CARTESIAN_POINT('Ctrl Pts',(5.88494079099994,11.6,-8.60440677400002));
#167326=CARTESIAN_POINT('Ctrl Pts',(5.88581438299995,15.2,-8.60538250100002));
#167327=CARTESIAN_POINT('Ctrl Pts',(5.88581438299995,11.6,-8.60538250100002));
#167328=CARTESIAN_POINT('Ctrl Pts',(5.88669461899994,15.2,-8.60636373900002));
#167329=CARTESIAN_POINT('Ctrl Pts',(5.88669461899994,11.6,-8.60636373900002));
#167330=CARTESIAN_POINT('Ctrl Pts',(5.88758149499994,15.2,-8.60735046100002));
#167331=CARTESIAN_POINT('Ctrl Pts',(5.88758149499994,11.6,-8.60735046100002));
#167332=CARTESIAN_POINT('Ctrl Pts',(5.88847500799995,15.2,-8.60834264100001));
#167333=CARTESIAN_POINT('Ctrl Pts',(5.88847500799995,11.6,-8.60834264100001));
#167334=CARTESIAN_POINT('Ctrl Pts',(5.88937515499994,15.2,-8.60934025300002));
#167335=CARTESIAN_POINT('Ctrl Pts',(5.88937515499994,11.6,-8.60934025300002));
#167336=CARTESIAN_POINT('Ctrl Pts',(5.89028193299994,15.2,-8.61034327100001));
#167337=CARTESIAN_POINT('Ctrl Pts',(5.89028193299994,11.6,-8.61034327100001));
#167338=CARTESIAN_POINT('Ctrl Pts',(5.89119533899994,15.2,-8.61135166700001));
#167339=CARTESIAN_POINT('Ctrl Pts',(5.89119533899994,11.6,-8.61135166700001));
#167340=CARTESIAN_POINT('Ctrl Pts',(5.89211536799994,15.2,-8.61236541700002));
#167341=CARTESIAN_POINT('Ctrl Pts',(5.89211536799994,11.6,-8.61236541700002));
#167342=CARTESIAN_POINT('Ctrl Pts',(5.89304201999994,15.2,-8.61338449400002));
#167343=CARTESIAN_POINT('Ctrl Pts',(5.89304201999994,11.6,-8.61338449400002));
#167344=CARTESIAN_POINT('Ctrl Pts',(5.89397528899994,15.2,-8.61440887300001));
#167345=CARTESIAN_POINT('Ctrl Pts',(5.89397528899994,11.6,-8.61440887300001));
#167346=CARTESIAN_POINT('Ctrl Pts',(5.89491517399994,15.2,-8.61543852800001));
#167347=CARTESIAN_POINT('Ctrl Pts',(5.89491517399994,11.6,-8.61543852800001));
#167348=CARTESIAN_POINT('Ctrl Pts',(5.89586167099994,15.2,-8.61647343400002));
#167349=CARTESIAN_POINT('Ctrl Pts',(5.89586167099994,11.6,-8.61647343400002));
#167350=CARTESIAN_POINT('Ctrl Pts',(5.89681477699994,15.2,-8.61751356400001));
#167351=CARTESIAN_POINT('Ctrl Pts',(5.89681477699994,11.6,-8.61751356400001));
#167352=CARTESIAN_POINT('Ctrl Pts',(5.89777448799994,15.2,-8.61855889400001));
#167353=CARTESIAN_POINT('Ctrl Pts',(5.89777448799994,11.6,-8.61855889400001));
#167354=CARTESIAN_POINT('Ctrl Pts',(5.89874080199994,15.2,-8.61960939900002));
#167355=CARTESIAN_POINT('Ctrl Pts',(5.89874080199994,11.6,-8.61960939900002));
#167356=CARTESIAN_POINT('Ctrl Pts',(5.89971371499994,15.2,-8.62066505300002));
#167357=CARTESIAN_POINT('Ctrl Pts',(5.89971371499994,11.6,-8.62066505300002));
#167358=CARTESIAN_POINT('Ctrl Pts',(5.90069322499994,15.2,-8.62172583100002));
#167359=CARTESIAN_POINT('Ctrl Pts',(5.90069322499994,11.6,-8.62172583100002));
#167360=CARTESIAN_POINT('Ctrl Pts',(5.90167932799995,15.2,-8.62279170800001));
#167361=CARTESIAN_POINT('Ctrl Pts',(5.90167932799995,11.6,-8.62279170800001));
#167362=CARTESIAN_POINT('Ctrl Pts',(5.90267202099994,15.2,-8.62386266200001));
#167363=CARTESIAN_POINT('Ctrl Pts',(5.90267202099994,11.6,-8.62386266200001));
#167364=CARTESIAN_POINT('Ctrl Pts',(5.90367129999994,15.2,-8.62493866400002));
#167365=CARTESIAN_POINT('Ctrl Pts',(5.90367129999994,11.6,-8.62493866400002));
#167366=CARTESIAN_POINT('Ctrl Pts',(5.90467716299995,15.2,-8.62601969300002));
#167367=CARTESIAN_POINT('Ctrl Pts',(5.90467716299995,11.6,-8.62601969300002));
#167368=CARTESIAN_POINT('Ctrl Pts',(5.90568960799994,15.2,-8.62710572200001));
#167369=CARTESIAN_POINT('Ctrl Pts',(5.90568960799994,11.6,-8.62710572200001));
#167370=CARTESIAN_POINT('Ctrl Pts',(5.90670862899994,15.2,-8.62819672800001));
#167371=CARTESIAN_POINT('Ctrl Pts',(5.90670862899994,11.6,-8.62819672800001));
#167372=CARTESIAN_POINT('Ctrl Pts',(5.90773422399995,15.2,-8.62929268600002));
#167373=CARTESIAN_POINT('Ctrl Pts',(5.90773422399995,11.6,-8.62929268600002));
#167374=CARTESIAN_POINT('Ctrl Pts',(5.90876639199994,15.2,-8.63039357200002));
#167375=CARTESIAN_POINT('Ctrl Pts',(5.90876639199994,11.6,-8.63039357200002));
#167376=CARTESIAN_POINT('Ctrl Pts',(5.90980512599995,15.2,-8.63149936300001));
#167377=CARTESIAN_POINT('Ctrl Pts',(5.90980512599995,11.6,-8.63149936300001));
#167378=CARTESIAN_POINT('Ctrl Pts',(5.91085042599994,15.2,-8.63261003400002));
#167379=CARTESIAN_POINT('Ctrl Pts',(5.91085042599994,11.6,-8.63261003400002));
#167380=CARTESIAN_POINT('Ctrl Pts',(5.91190228799994,15.2,-8.63372556000002));
#167381=CARTESIAN_POINT('Ctrl Pts',(5.91190228799994,11.6,-8.63372556000002));
#167382=CARTESIAN_POINT('Ctrl Pts',(5.91296070699994,15.2,-8.63484591900002));
#167383=CARTESIAN_POINT('Ctrl Pts',(5.91296070699994,11.6,-8.63484591900002));
#167384=CARTESIAN_POINT('Ctrl Pts',(5.91402568199995,15.2,-8.63597108700001));
#167385=CARTESIAN_POINT('Ctrl Pts',(5.91402568199995,11.6,-8.63597108700001));
#167386=CARTESIAN_POINT('Ctrl Pts',(5.91509720999994,15.2,-8.63710104100001));
#167387=CARTESIAN_POINT('Ctrl Pts',(5.91509720999994,11.6,-8.63710104100001));
#167388=CARTESIAN_POINT('Ctrl Pts',(5.91617528699994,15.2,-8.63823575600002));
#167389=CARTESIAN_POINT('Ctrl Pts',(5.91617528699994,11.6,-8.63823575600002));
#167390=CARTESIAN_POINT('Ctrl Pts',(5.91725990899994,15.2,-8.63937520900001));
#167391=CARTESIAN_POINT('Ctrl Pts',(5.91725990899994,11.6,-8.63937520900001));
#167392=CARTESIAN_POINT('Ctrl Pts',(5.91835107499994,15.2,-8.64051937700001));
#167393=CARTESIAN_POINT('Ctrl Pts',(5.91835107499994,11.6,-8.64051937700001));
#167394=CARTESIAN_POINT('Ctrl Pts',(5.91944877999994,15.2,-8.64166823700002));
#167395=CARTESIAN_POINT('Ctrl Pts',(5.91944877999994,11.6,-8.64166823700002));
#167396=CARTESIAN_POINT('Ctrl Pts',(5.92055302199994,15.2,-8.64282176500001));
#167397=CARTESIAN_POINT('Ctrl Pts',(5.92055302199994,11.6,-8.64282176500001));
#167398=CARTESIAN_POINT('Ctrl Pts',(5.92166379799995,15.2,-8.64397994000001));
#167399=CARTESIAN_POINT('Ctrl Pts',(5.92166379799995,11.6,-8.64397994000001));
#167400=CARTESIAN_POINT('Ctrl Pts',(5.92278110299994,15.2,-8.64514273600001));
#167401=CARTESIAN_POINT('Ctrl Pts',(5.92278110299994,11.6,-8.64514273600001));
#167402=CARTESIAN_POINT('Ctrl Pts',(5.92390493499994,15.2,-8.64631013400002));
#167403=CARTESIAN_POINT('Ctrl Pts',(5.92390493499994,11.6,-8.64631013400002));
#167404=CARTESIAN_POINT('Ctrl Pts',(5.92503529199995,15.2,-8.64748210700002));
#167405=CARTESIAN_POINT('Ctrl Pts',(5.92503529199995,11.6,-8.64748210700002));
#167406=CARTESIAN_POINT('Ctrl Pts',(5.92617216899994,15.2,-8.64865863600001));
#167407=CARTESIAN_POINT('Ctrl Pts',(5.92617216899994,11.6,-8.64865863600001));
#167408=CARTESIAN_POINT('Ctrl Pts',(5.92731556399994,15.2,-8.64983969600001));
#167409=CARTESIAN_POINT('Ctrl Pts',(5.92731556399994,11.6,-8.64983969600001));
#167410=CARTESIAN_POINT('Ctrl Pts',(5.92846547399994,15.2,-8.65102526600002));
#167411=CARTESIAN_POINT('Ctrl Pts',(5.92846547399994,11.6,-8.65102526600002));
#167412=CARTESIAN_POINT('Ctrl Pts',(5.92962189399994,15.2,-8.65221532200002));
#167413=CARTESIAN_POINT('Ctrl Pts',(5.92962189399994,11.6,-8.65221532200002));
#167414=CARTESIAN_POINT('Ctrl Pts',(5.93078482299994,15.2,-8.65340984300002));
#167415=CARTESIAN_POINT('Ctrl Pts',(5.93078482299994,11.6,-8.65340984300002));
#167416=CARTESIAN_POINT('Ctrl Pts',(5.93195425599994,15.2,-8.65460880700001));
#167417=CARTESIAN_POINT('Ctrl Pts',(5.93195425599994,11.6,-8.65460880700001));
#167418=CARTESIAN_POINT('Ctrl Pts',(5.93313019299995,15.2,-8.65581219100001));
#167419=CARTESIAN_POINT('Ctrl Pts',(5.93313019299995,11.6,-8.65581219100001));
#167420=CARTESIAN_POINT('Ctrl Pts',(5.93431262699994,15.2,-8.65701997400001));
#167421=CARTESIAN_POINT('Ctrl Pts',(5.93431262699994,11.6,-8.65701997400001));
#167422=CARTESIAN_POINT('Ctrl Pts',(5.93550155699995,15.2,-8.65823213200001));
#167423=CARTESIAN_POINT('Ctrl Pts',(5.93550155699995,11.6,-8.65823213200001));
#167424=CARTESIAN_POINT('Ctrl Pts',(5.93669697899994,15.2,-8.65944864500002));
#167425=CARTESIAN_POINT('Ctrl Pts',(5.93669697899994,11.6,-8.65944864500002));
#167426=CARTESIAN_POINT('Ctrl Pts',(5.93789889099994,15.2,-8.66066949100002));
#167427=CARTESIAN_POINT('Ctrl Pts',(5.93789889099994,11.6,-8.66066949100002));
#167428=CARTESIAN_POINT('Ctrl Pts',(5.93910728799995,15.2,-8.66189464800001));
#167429=CARTESIAN_POINT('Ctrl Pts',(5.93910728799995,11.6,-8.66189464800001));
#167430=CARTESIAN_POINT('Ctrl Pts',(5.94032216899994,15.2,-8.66312409300001));
#167431=CARTESIAN_POINT('Ctrl Pts',(5.94032216899994,11.6,-8.66312409300001));
#167432=CARTESIAN_POINT('Ctrl Pts',(5.94154352899994,15.2,-8.66435780700002));
#167433=CARTESIAN_POINT('Ctrl Pts',(5.94154352899994,11.6,-8.66435780700002));
#167434=CARTESIAN_POINT('Ctrl Pts',(5.94277136499994,15.2,-8.66559576600002));
#167435=CARTESIAN_POINT('Ctrl Pts',(5.94277136499994,11.6,-8.66559576600002));
#167436=CARTESIAN_POINT('Ctrl Pts',(5.94400567599994,15.2,-8.66683795100002));
#167437=CARTESIAN_POINT('Ctrl Pts',(5.94400567599994,11.6,-8.66683795100002));
#167438=CARTESIAN_POINT('Ctrl Pts',(5.94524645699994,15.2,-8.66808434000001));
#167439=CARTESIAN_POINT('Ctrl Pts',(5.94524645699994,11.6,-8.66808434000001));
#167440=CARTESIAN_POINT('Ctrl Pts',(5.94649370399994,15.2,-8.66933491000001));
#167441=CARTESIAN_POINT('Ctrl Pts',(5.94649370399994,11.6,-8.66933491000001));
#167442=CARTESIAN_POINT('Ctrl Pts',(5.94774741599994,15.2,-8.67058964200002));
#167443=CARTESIAN_POINT('Ctrl Pts',(5.94774741599994,11.6,-8.67058964200002));
#167444=CARTESIAN_POINT('Ctrl Pts',(5.94900758799994,15.2,-8.67184851400001));
#167445=CARTESIAN_POINT('Ctrl Pts',(5.94900758799994,11.6,-8.67184851400001));
#167446=CARTESIAN_POINT('Ctrl Pts',(5.95027421799994,15.2,-8.67311150500001));
#167447=CARTESIAN_POINT('Ctrl Pts',(5.95027421799994,11.6,-8.67311150500001));
#167448=CARTESIAN_POINT('Ctrl Pts',(5.95154730199994,15.2,-8.67437859500002));
#167449=CARTESIAN_POINT('Ctrl Pts',(5.95154730199994,11.6,-8.67437859500002));
#167450=CARTESIAN_POINT('Ctrl Pts',(5.95282683699994,15.2,-8.67564976200002));
#167451=CARTESIAN_POINT('Ctrl Pts',(5.95282683699994,11.6,-8.67564976200002));
#167452=CARTESIAN_POINT('Ctrl Pts',(5.95411282099994,15.2,-8.67692498600002));
#167453=CARTESIAN_POINT('Ctrl Pts',(5.95411282099994,11.6,-8.67692498600002));
#167454=CARTESIAN_POINT('Ctrl Pts',(5.95540524899994,15.2,-8.67820424500002));
#167455=CARTESIAN_POINT('Ctrl Pts',(5.95540524899994,11.6,-8.67820424500002));
#167456=CARTESIAN_POINT('Ctrl Pts',(5.95670411999994,15.2,-8.67948752000002));
#167457=CARTESIAN_POINT('Ctrl Pts',(5.95670411999994,11.6,-8.67948752000002));
#167458=CARTESIAN_POINT('Ctrl Pts',(5.95800942899994,15.2,-8.68077479000002));
#167459=CARTESIAN_POINT('Ctrl Pts',(5.95800942899994,11.6,-8.68077479000002));
#167460=CARTESIAN_POINT('Ctrl Pts',(5.95932117299995,15.2,-8.68206603400001));
#167461=CARTESIAN_POINT('Ctrl Pts',(5.95932117299995,11.6,-8.68206603400001));
#167462=CARTESIAN_POINT('Ctrl Pts',(5.96063934899995,15.2,-8.68336123200002));
#167463=CARTESIAN_POINT('Ctrl Pts',(5.96063934899995,11.6,-8.68336123200002));
#167464=CARTESIAN_POINT('Ctrl Pts',(5.96196395499994,15.2,-8.68466036400001));
#167465=CARTESIAN_POINT('Ctrl Pts',(5.96196395499994,11.6,-8.68466036400001));
#167466=CARTESIAN_POINT('Ctrl Pts',(5.96329498499995,15.2,-8.68596340900002));
#167467=CARTESIAN_POINT('Ctrl Pts',(5.96329498499995,11.6,-8.68596340900002));
#167468=CARTESIAN_POINT('Ctrl Pts',(5.96463243999994,15.2,-8.68727034800001));
#167469=CARTESIAN_POINT('Ctrl Pts',(5.96463243999994,11.6,-8.68727034800001));
#167470=CARTESIAN_POINT('Ctrl Pts',(5.96597631299995,15.2,-8.68858116100002));
#167471=CARTESIAN_POINT('Ctrl Pts',(5.96597631299995,11.6,-8.68858116100002));
#167472=CARTESIAN_POINT('Ctrl Pts',(5.96732660299994,15.2,-8.68989582500001));
#167473=CARTESIAN_POINT('Ctrl Pts',(5.96732660299994,11.6,-8.68989582500001));
#167474=CARTESIAN_POINT('Ctrl Pts',(5.96868330599994,15.2,-8.69121432500001));
#167475=CARTESIAN_POINT('Ctrl Pts',(5.96868330599994,11.6,-8.69121432500001));
#167476=CARTESIAN_POINT('Ctrl Pts',(5.97004641899994,15.2,-8.69253663700002));
#167477=CARTESIAN_POINT('Ctrl Pts',(5.97004641899994,11.6,-8.69253663700002));
#167478=CARTESIAN_POINT('Ctrl Pts',(5.97141593799994,15.2,-8.69386274300001));
#167479=CARTESIAN_POINT('Ctrl Pts',(5.97141593799994,11.6,-8.69386274300001));
#167480=CARTESIAN_POINT('Ctrl Pts',(5.97279186099994,15.2,-8.69519262200001));
#167481=CARTESIAN_POINT('Ctrl Pts',(5.97279186099994,11.6,-8.69519262200001));
#167482=CARTESIAN_POINT('Ctrl Pts',(5.97417418499995,15.2,-8.69652625600001));
#167483=CARTESIAN_POINT('Ctrl Pts',(5.97417418499995,11.6,-8.69652625600001));
#167484=CARTESIAN_POINT('Ctrl Pts',(5.97556290599995,15.2,-8.69786362500001));
#167485=CARTESIAN_POINT('Ctrl Pts',(5.97556290599995,11.6,-8.69786362500001));
#167486=CARTESIAN_POINT('Ctrl Pts',(5.97695801999994,15.2,-8.69920470900002));
#167487=CARTESIAN_POINT('Ctrl Pts',(5.97695801999994,11.6,-8.69920470900002));
#167488=CARTESIAN_POINT('Ctrl Pts',(5.97835952599994,15.2,-8.70054948900002));
#167489=CARTESIAN_POINT('Ctrl Pts',(5.97835952599994,11.6,-8.70054948900002));
#167490=CARTESIAN_POINT('Ctrl Pts',(5.97976741899994,15.2,-8.70189794500002));
#167491=CARTESIAN_POINT('Ctrl Pts',(5.97976741899994,11.6,-8.70189794500002));
#167492=CARTESIAN_POINT('Ctrl Pts',(5.98118169699994,15.2,-8.70325005800002));
#167493=CARTESIAN_POINT('Ctrl Pts',(5.98118169699994,11.6,-8.70325005800002));
#167494=CARTESIAN_POINT('Ctrl Pts',(5.98260235599994,15.2,-8.70460581000001));
#167495=CARTESIAN_POINT('Ctrl Pts',(5.98260235599994,11.6,-8.70460581000001));
#167496=CARTESIAN_POINT('Ctrl Pts',(5.98402939199994,15.2,-8.70596518000001));
#167497=CARTESIAN_POINT('Ctrl Pts',(5.98402939199994,11.6,-8.70596518000001));
#167498=CARTESIAN_POINT('Ctrl Pts',(5.98546280499994,15.2,-8.70732814900002));
#167499=CARTESIAN_POINT('Ctrl Pts',(5.98546280499994,11.6,-8.70732814900002));
#167500=CARTESIAN_POINT('Ctrl Pts',(5.98690258799994,15.2,-8.70869469900001));
#167501=CARTESIAN_POINT('Ctrl Pts',(5.98690258799994,11.6,-8.70869469900001));
#167502=CARTESIAN_POINT('Ctrl Pts',(5.98834873999994,15.2,-8.71006481000002));
#167503=CARTESIAN_POINT('Ctrl Pts',(5.98834873999994,11.6,-8.71006481000002));
#167504=CARTESIAN_POINT('Ctrl Pts',(5.98980125799994,15.2,-8.71143846400001));
#167505=CARTESIAN_POINT('Ctrl Pts',(5.98980125799994,11.6,-8.71143846400001));
#167506=CARTESIAN_POINT('Ctrl Pts',(5.99126013699995,15.2,-8.71281564200002));
#167507=CARTESIAN_POINT('Ctrl Pts',(5.99126013699995,11.6,-8.71281564200002));
#167508=CARTESIAN_POINT('Ctrl Pts',(5.99272537499995,15.2,-8.71419632500002));
#167509=CARTESIAN_POINT('Ctrl Pts',(5.99272537499995,11.6,-8.71419632500002));
#167510=CARTESIAN_POINT('Ctrl Pts',(5.99419696899995,15.2,-8.71558049400001));
#167511=CARTESIAN_POINT('Ctrl Pts',(5.99419696899995,11.6,-8.71558049400001));
#167512=CARTESIAN_POINT('Ctrl Pts',(5.99567491499994,15.2,-8.71696813100002));
#167513=CARTESIAN_POINT('Ctrl Pts',(5.99567491499994,11.6,-8.71696813100002));
#167514=CARTESIAN_POINT('Ctrl Pts',(5.99715921199994,15.2,-8.71835921700002));
#167515=CARTESIAN_POINT('Ctrl Pts',(5.99715921199994,11.6,-8.71835921700002));
#167516=CARTESIAN_POINT('Ctrl Pts',(5.99864985299994,15.2,-8.71975373400002));
#167517=CARTESIAN_POINT('Ctrl Pts',(5.99864985299994,11.6,-8.71975373400002));
#167518=CARTESIAN_POINT('Ctrl Pts',(6.00014683699994,15.2,-8.72115166300001));
#167519=CARTESIAN_POINT('Ctrl Pts',(6.00014683699994,11.6,-8.72115166300001));
#167520=CARTESIAN_POINT('Ctrl Pts',(6.00165016199994,15.2,-8.72255298400002));
#167521=CARTESIAN_POINT('Ctrl Pts',(6.00165016199994,11.6,-8.72255298400002));
#167522=CARTESIAN_POINT('Ctrl Pts',(6.00315982299994,15.2,-8.72395768300001));
#167523=CARTESIAN_POINT('Ctrl Pts',(6.00315982299994,11.6,-8.72395768300001));
#167524=CARTESIAN_POINT('Ctrl Pts',(6.00467581699994,15.2,-8.72536573700001));
#167525=CARTESIAN_POINT('Ctrl Pts',(6.00467581699994,11.6,-8.72536573700001));
#167526=CARTESIAN_POINT('Ctrl Pts',(6.00619813999994,15.2,-8.72677713200002));
#167527=CARTESIAN_POINT('Ctrl Pts',(6.00619813999994,11.6,-8.72677713200002));
#167528=CARTESIAN_POINT('Ctrl Pts',(6.00772679099994,15.2,-8.72819184600001));
#167529=CARTESIAN_POINT('Ctrl Pts',(6.00772679099994,11.6,-8.72819184600001));
#167530=CARTESIAN_POINT('Ctrl Pts',(6.00926176599994,15.2,-8.72960986400001));
#167531=CARTESIAN_POINT('Ctrl Pts',(6.00926176599994,11.6,-8.72960986400001));
#167532=CARTESIAN_POINT('Ctrl Pts',(6.01080305999994,15.2,-8.73103116600002));
#167533=CARTESIAN_POINT('Ctrl Pts',(6.01080305999994,11.6,-8.73103116600002));
#167534=CARTESIAN_POINT('Ctrl Pts',(6.01235067299994,15.2,-8.73245573400002));
#167535=CARTESIAN_POINT('Ctrl Pts',(6.01235067299994,11.6,-8.73245573400002));
#167536=CARTESIAN_POINT('Ctrl Pts',(6.01390459799994,15.2,-8.73388355100002));
#167537=CARTESIAN_POINT('Ctrl Pts',(6.01390459799994,11.6,-8.73388355100002));
#167538=CARTESIAN_POINT('Ctrl Pts',(6.01546483399994,15.2,-8.73531460000001));
#167539=CARTESIAN_POINT('Ctrl Pts',(6.01546483399994,11.6,-8.73531460000001));
#167540=CARTESIAN_POINT('Ctrl Pts',(6.01703137899994,15.2,-8.73674886200002));
#167541=CARTESIAN_POINT('Ctrl Pts',(6.01703137899994,11.6,-8.73674886200002));
#167542=CARTESIAN_POINT('Ctrl Pts',(6.01860422799994,15.2,-8.73818631900001));
#167543=CARTESIAN_POINT('Ctrl Pts',(6.01860422799994,11.6,-8.73818631900001));
#167544=CARTESIAN_POINT('Ctrl Pts',(6.02018337599994,15.2,-8.73962695300002));
#167545=CARTESIAN_POINT('Ctrl Pts',(6.02018337599994,11.6,-8.73962695300002));
#167546=CARTESIAN_POINT('Ctrl Pts',(6.02176882399994,15.2,-8.74107074900002));
#167547=CARTESIAN_POINT('Ctrl Pts',(6.02176882399994,11.6,-8.74107074900002));
#167548=CARTESIAN_POINT('Ctrl Pts',(6.02336056599994,15.2,-8.74251768600002));
#167549=CARTESIAN_POINT('Ctrl Pts',(6.02336056599994,11.6,-8.74251768600002));
#167550=CARTESIAN_POINT('Ctrl Pts',(6.02495859899994,15.2,-8.74396774900001));
#167551=CARTESIAN_POINT('Ctrl Pts',(6.02495859899994,11.6,-8.74396774900001));
#167552=CARTESIAN_POINT('Ctrl Pts',(6.02656291999994,15.2,-8.74542091800001));
#167553=CARTESIAN_POINT('Ctrl Pts',(6.02656291999994,11.6,-8.74542091800001));
#167554=CARTESIAN_POINT('Ctrl Pts',(6.02817352699994,15.2,-8.74687718000001));
#167555=CARTESIAN_POINT('Ctrl Pts',(6.02817352699994,11.6,-8.74687718000001));
#167556=CARTESIAN_POINT('Ctrl Pts',(6.02979041499994,15.2,-8.74833651300002));
#167557=CARTESIAN_POINT('Ctrl Pts',(6.02979041499994,11.6,-8.74833651300002));
#167558=CARTESIAN_POINT('Ctrl Pts',(6.03141358199994,15.2,-8.74979890200001));
#167559=CARTESIAN_POINT('Ctrl Pts',(6.03141358199994,11.6,-8.74979890200001));
#167560=CARTESIAN_POINT('Ctrl Pts',(6.03304302299994,15.2,-8.75126433100002));
#167561=CARTESIAN_POINT('Ctrl Pts',(6.03304302299994,11.6,-8.75126433100002));
#167562=CARTESIAN_POINT('Ctrl Pts',(6.03467873699994,15.2,-8.75273277900002));
#167563=CARTESIAN_POINT('Ctrl Pts',(6.03467873699994,11.6,-8.75273277900002));
#167564=CARTESIAN_POINT('Ctrl Pts',(6.03632071899994,15.2,-8.75420423200002));
#167565=CARTESIAN_POINT('Ctrl Pts',(6.03632071899994,11.6,-8.75420423200002));
#167566=CARTESIAN_POINT('Ctrl Pts',(6.03796896799994,15.2,-8.75567867300001));
#167567=CARTESIAN_POINT('Ctrl Pts',(6.03796896799994,11.6,-8.75567867300001));
#167568=CARTESIAN_POINT('Ctrl Pts',(6.03962347799994,15.2,-8.75715608400002));
#167569=CARTESIAN_POINT('Ctrl Pts',(6.03962347799994,11.6,-8.75715608400002));
#167570=CARTESIAN_POINT('Ctrl Pts',(6.04128424699995,15.2,-8.75863644800001));
#167571=CARTESIAN_POINT('Ctrl Pts',(6.04128424699995,11.6,-8.75863644800001));
#167572=CARTESIAN_POINT('Ctrl Pts',(6.04295127299994,15.2,-8.76011974800001));
#167573=CARTESIAN_POINT('Ctrl Pts',(6.04295127299994,11.6,-8.76011974800001));
#167574=CARTESIAN_POINT('Ctrl Pts',(6.04462455099994,15.2,-8.76160596800002));
#167575=CARTESIAN_POINT('Ctrl Pts',(6.04462455099994,11.6,-8.76160596800002));
#167576=CARTESIAN_POINT('Ctrl Pts',(6.04630407799994,15.2,-8.76309509100002));
#167577=CARTESIAN_POINT('Ctrl Pts',(6.04630407799994,11.6,-8.76309509100002));
#167578=CARTESIAN_POINT('Ctrl Pts',(6.04798985099994,15.2,-8.76458710000002));
#167579=CARTESIAN_POINT('Ctrl Pts',(6.04798985099994,11.6,-8.76458710000002));
#167580=CARTESIAN_POINT('Ctrl Pts',(6.04968186699994,15.2,-8.76608197700002));
#167581=CARTESIAN_POINT('Ctrl Pts',(6.04968186699994,11.6,-8.76608197700002));
#167582=CARTESIAN_POINT('Ctrl Pts',(6.05138012199994,15.2,-8.76757970900002));
#167583=CARTESIAN_POINT('Ctrl Pts',(6.05138012199994,11.6,-8.76757970900002));
#167584=CARTESIAN_POINT('Ctrl Pts',(6.05308461499994,15.2,-8.76908027600001));
#167585=CARTESIAN_POINT('Ctrl Pts',(6.05308461499994,11.6,-8.76908027600001));
#167586=CARTESIAN_POINT('Ctrl Pts',(6.05479533999994,15.2,-8.77058366200002));
#167587=CARTESIAN_POINT('Ctrl Pts',(6.05479533999994,11.6,-8.77058366200002));
#167588=CARTESIAN_POINT('Ctrl Pts',(6.05651229499995,15.2,-8.77208985200001));
#167589=CARTESIAN_POINT('Ctrl Pts',(6.05651229499995,11.6,-8.77208985200001));
#167590=CARTESIAN_POINT('Ctrl Pts',(6.05823547599995,15.2,-8.77359882900001));
#167591=CARTESIAN_POINT('Ctrl Pts',(6.05823547599995,11.6,-8.77359882900001));
#167592=CARTESIAN_POINT('Ctrl Pts',(6.05996488099994,15.2,-8.77511057700002));
#167593=CARTESIAN_POINT('Ctrl Pts',(6.05996488099994,11.6,-8.77511057700002));
#167594=CARTESIAN_POINT('Ctrl Pts',(6.06170050599994,15.2,-8.77662507800002));
#167595=CARTESIAN_POINT('Ctrl Pts',(6.06170050599994,11.6,-8.77662507800002));
#167596=CARTESIAN_POINT('Ctrl Pts',(6.06344234899994,15.2,-8.77814231800001));
#167597=CARTESIAN_POINT('Ctrl Pts',(6.06344234899994,11.6,-8.77814231800001));
#167598=CARTESIAN_POINT('Ctrl Pts',(6.06519040399994,15.2,-8.77966227900002));
#167599=CARTESIAN_POINT('Ctrl Pts',(6.06519040399994,11.6,-8.77966227900002));
#167600=CARTESIAN_POINT('Ctrl Pts',(6.06694466899994,15.2,-8.78118494600002));
#167601=CARTESIAN_POINT('Ctrl Pts',(6.06694466899994,11.6,-8.78118494600002));
#167602=CARTESIAN_POINT('Ctrl Pts',(6.06870514199994,15.2,-8.78271030200001));
#167603=CARTESIAN_POINT('Ctrl Pts',(6.06870514199994,11.6,-8.78271030200001));
#167604=CARTESIAN_POINT('Ctrl Pts',(6.07047181899994,15.2,-8.78423833100002));
#167605=CARTESIAN_POINT('Ctrl Pts',(6.07047181899994,11.6,-8.78423833100002));
#167606=CARTESIAN_POINT('Ctrl Pts',(6.07224469599994,15.2,-8.78576901800002));
#167607=CARTESIAN_POINT('Ctrl Pts',(6.07224469599994,11.6,-8.78576901800002));
#167608=CARTESIAN_POINT('Ctrl Pts',(6.07402377099994,15.2,-8.78730234600001));
#167609=CARTESIAN_POINT('Ctrl Pts',(6.07402377099994,11.6,-8.78730234600001));
#167610=CARTESIAN_POINT('Ctrl Pts',(6.07580903899994,15.2,-8.78883830000002));
#167611=CARTESIAN_POINT('Ctrl Pts',(6.07580903899994,11.6,-8.78883830000002));
#167612=CARTESIAN_POINT('Ctrl Pts',(6.07760049799994,15.2,-8.79037686400002));
#167613=CARTESIAN_POINT('Ctrl Pts',(6.07760049799994,11.6,-8.79037686400002));
#167614=CARTESIAN_POINT('Ctrl Pts',(6.07939814499994,15.2,-8.79191802100001));
#167615=CARTESIAN_POINT('Ctrl Pts',(6.07939814499994,11.6,-8.79191802100001));
#167616=CARTESIAN_POINT('Ctrl Pts',(6.08120197499994,15.2,-8.79346175700002));
#167617=CARTESIAN_POINT('Ctrl Pts',(6.08120197499994,11.6,-8.79346175700002));
#167618=CARTESIAN_POINT('Ctrl Pts',(6.08301198699994,15.2,-8.79500805500001));
#167619=CARTESIAN_POINT('Ctrl Pts',(6.08301198699994,11.6,-8.79500805500001));
#167620=CARTESIAN_POINT('Ctrl Pts',(6.08482817699994,15.2,-8.79655689900002));
#167621=CARTESIAN_POINT('Ctrl Pts',(6.08482817699994,11.6,-8.79655689900002));
#167622=CARTESIAN_POINT('Ctrl Pts',(6.08665053999994,15.2,-8.79810827400001));
#167623=CARTESIAN_POINT('Ctrl Pts',(6.08665053999994,11.6,-8.79810827400001));
#167624=CARTESIAN_POINT('Ctrl Pts',(6.08847907499994,15.2,-8.79966216600002));
#167625=CARTESIAN_POINT('Ctrl Pts',(6.08847907499994,11.6,-8.79966216600002));
#167626=CARTESIAN_POINT('Ctrl Pts',(6.09031377799995,15.2,-8.80121855700001));
#167627=CARTESIAN_POINT('Ctrl Pts',(6.09031377799995,11.6,-8.80121855700001));
#167628=CARTESIAN_POINT('Ctrl Pts',(6.09215464499994,15.2,-8.80277743400002));
#167629=CARTESIAN_POINT('Ctrl Pts',(6.09215464499994,11.6,-8.80277743400002));
#167630=CARTESIAN_POINT('Ctrl Pts',(6.09400167399994,15.2,-8.80433877800002));
#167631=CARTESIAN_POINT('Ctrl Pts',(6.09400167399994,11.6,-8.80433877800002));
#167632=CARTESIAN_POINT('Ctrl Pts',(6.09585485999994,15.2,-8.80590257700002));
#167633=CARTESIAN_POINT('Ctrl Pts',(6.09585485999994,11.6,-8.80590257700002));
#167634=CARTESIAN_POINT('Ctrl Pts',(6.09771420199994,15.2,-8.80746881400002));
#167635=CARTESIAN_POINT('Ctrl Pts',(6.09771420199994,11.6,-8.80746881400002));
#167636=CARTESIAN_POINT('Ctrl Pts',(6.09957969399994,15.2,-8.80903747400002));
#167637=CARTESIAN_POINT('Ctrl Pts',(6.09957969399994,11.6,-8.80903747400002));
#167638=CARTESIAN_POINT('Ctrl Pts',(6.10145133499994,15.2,-8.81060854200001));
#167639=CARTESIAN_POINT('Ctrl Pts',(6.10145133499994,11.6,-8.81060854200001));
#167640=CARTESIAN_POINT('Ctrl Pts',(6.10332912099994,15.2,-8.81218200200001));
#167641=CARTESIAN_POINT('Ctrl Pts',(6.10332912099994,11.6,-8.81218200200001));
#167642=CARTESIAN_POINT('Ctrl Pts',(6.10521304799994,15.2,-8.81375784000002));
#167643=CARTESIAN_POINT('Ctrl Pts',(6.10521304799994,11.6,-8.81375784000002));
#167644=CARTESIAN_POINT('Ctrl Pts',(6.10710311299994,15.2,-8.81533604100002));
#167645=CARTESIAN_POINT('Ctrl Pts',(6.10710311299994,11.6,-8.81533604100002));
#167646=CARTESIAN_POINT('Ctrl Pts',(6.10899931399994,15.2,-8.81691658800002));
#167647=CARTESIAN_POINT('Ctrl Pts',(6.10899931399994,11.6,-8.81691658800002));
#167648=CARTESIAN_POINT('Ctrl Pts',(6.11090164599994,15.2,-8.81849946800001));
#167649=CARTESIAN_POINT('Ctrl Pts',(6.11090164599994,11.6,-8.81849946800001));
#167650=CARTESIAN_POINT('Ctrl Pts',(6.11281010699994,15.2,-8.82008466500002));
#167651=CARTESIAN_POINT('Ctrl Pts',(6.11281010699994,11.6,-8.82008466500002));
#167652=CARTESIAN_POINT('Ctrl Pts',(6.11472469299994,15.2,-8.82167216400001));
#167653=CARTESIAN_POINT('Ctrl Pts',(6.11472469299994,11.6,-8.82167216400001));
#167654=CARTESIAN_POINT('Ctrl Pts',(6.11664539999994,15.2,-8.82326195200001));
#167655=CARTESIAN_POINT('Ctrl Pts',(6.11664539999994,11.6,-8.82326195200001));
#167656=CARTESIAN_POINT('Ctrl Pts',(6.11857222599994,15.2,-8.82485401100002));
#167657=CARTESIAN_POINT('Ctrl Pts',(6.11857222599994,11.6,-8.82485401100002));
#167658=CARTESIAN_POINT('Ctrl Pts',(6.12050516699994,15.2,-8.82644832800001));
#167659=CARTESIAN_POINT('Ctrl Pts',(6.12050516699994,11.6,-8.82644832800001));
#167660=CARTESIAN_POINT('Ctrl Pts',(6.12244422199994,15.2,-8.82804488900002));
#167661=CARTESIAN_POINT('Ctrl Pts',(6.12244422199994,11.6,-8.82804488900002));
#167662=CARTESIAN_POINT('Ctrl Pts',(6.12438938299994,15.2,-8.82964367800002));
#167663=CARTESIAN_POINT('Ctrl Pts',(6.12438938299994,11.6,-8.82964367800002));
#167664=CARTESIAN_POINT('Ctrl Pts',(6.12634064999994,15.2,-8.83124468000002));
#167665=CARTESIAN_POINT('Ctrl Pts',(6.12634064999994,11.6,-8.83124468000002));
#167666=CARTESIAN_POINT('Ctrl Pts',(6.12829801999994,15.2,-8.83284788100001));
#167667=CARTESIAN_POINT('Ctrl Pts',(6.12829801999994,11.6,-8.83284788100001));
#167668=CARTESIAN_POINT('Ctrl Pts',(6.13026148799994,15.2,-8.83445326700001));
#167669=CARTESIAN_POINT('Ctrl Pts',(6.13026148799994,11.6,-8.83445326700001));
#167670=CARTESIAN_POINT('Ctrl Pts',(6.13223105199994,15.2,-8.83606082300001));
#167671=CARTESIAN_POINT('Ctrl Pts',(6.13223105199994,11.6,-8.83606082300001));
#167672=CARTESIAN_POINT('Ctrl Pts',(6.13420670699994,15.2,-8.83767053400002));
#167673=CARTESIAN_POINT('Ctrl Pts',(6.13420670699994,11.6,-8.83767053400002));
#167674=CARTESIAN_POINT('Ctrl Pts',(6.13618845099994,15.2,-8.83928238600001));
#167675=CARTESIAN_POINT('Ctrl Pts',(6.13618845099994,11.6,-8.83928238600001));
#167676=CARTESIAN_POINT('Ctrl Pts',(6.13817627999994,15.2,-8.84089636400001));
#167677=CARTESIAN_POINT('Ctrl Pts',(6.13817627999994,11.6,-8.84089636400001));
#167678=CARTESIAN_POINT('Ctrl Pts',(6.14017019199994,15.2,-8.84251245500002));
#167679=CARTESIAN_POINT('Ctrl Pts',(6.14017019199994,11.6,-8.84251245500002));
#167680=CARTESIAN_POINT('Ctrl Pts',(6.14217018299994,15.2,-8.84413064300002));
#167681=CARTESIAN_POINT('Ctrl Pts',(6.14217018299994,11.6,-8.84413064300002));
#167682=CARTESIAN_POINT('Ctrl Pts',(6.14417624999994,15.2,-8.84575091500002));
#167683=CARTESIAN_POINT('Ctrl Pts',(6.14417624999994,11.6,-8.84575091500002));
#167684=CARTESIAN_POINT('Ctrl Pts',(6.14618838899994,15.2,-8.84737325500002));
#167685=CARTESIAN_POINT('Ctrl Pts',(6.14618838899994,11.6,-8.84737325500002));
#167686=CARTESIAN_POINT('Ctrl Pts',(6.14820659699994,15.2,-8.84899765100002));
#167687=CARTESIAN_POINT('Ctrl Pts',(6.14820659699994,11.6,-8.84899765100002));
#167688=CARTESIAN_POINT('Ctrl Pts',(6.15023086899994,15.2,-8.85062408700002));
#167689=CARTESIAN_POINT('Ctrl Pts',(6.15023086899994,11.6,-8.85062408700002));
#167690=CARTESIAN_POINT('Ctrl Pts',(6.15226120499995,15.2,-8.85225255100002));
#167691=CARTESIAN_POINT('Ctrl Pts',(6.15226120499995,11.6,-8.85225255100002));
#167692=CARTESIAN_POINT('Ctrl Pts',(6.15429759899994,15.2,-8.85388302700001));
#167693=CARTESIAN_POINT('Ctrl Pts',(6.15429759899994,11.6,-8.85388302700001));
#167694=CARTESIAN_POINT('Ctrl Pts',(6.15634004999994,15.2,-8.85551550100002));
#167695=CARTESIAN_POINT('Ctrl Pts',(6.15634004999994,11.6,-8.85551550100002));
#167696=CARTESIAN_POINT('Ctrl Pts',(6.15838855099994,15.2,-8.85714995900001));
#167697=CARTESIAN_POINT('Ctrl Pts',(6.15838855099994,11.6,-8.85714995900001));
#167698=CARTESIAN_POINT('Ctrl Pts',(6.16044310199994,15.2,-8.85878638800002));
#167699=CARTESIAN_POINT('Ctrl Pts',(6.16044310199994,11.6,-8.85878638800002));
#167700=CARTESIAN_POINT('Ctrl Pts',(6.16250369999994,15.2,-8.86042477400002));
#167701=CARTESIAN_POINT('Ctrl Pts',(6.16250369999994,11.6,-8.86042477400002));
#167702=CARTESIAN_POINT('Ctrl Pts',(6.16457033899994,15.2,-8.86206510100001));
#167703=CARTESIAN_POINT('Ctrl Pts',(6.16457033899994,11.6,-8.86206510100001));
#167704=CARTESIAN_POINT('Ctrl Pts',(6.16664301799994,15.2,-8.86370735900002));
#167705=CARTESIAN_POINT('Ctrl Pts',(6.16664301799994,11.6,-8.86370735900002));
#167706=CARTESIAN_POINT('Ctrl Pts',(6.16872173199994,15.2,-8.86535153000001));
#167707=CARTESIAN_POINT('Ctrl Pts',(6.16872173199994,11.6,-8.86535153000001));
#167708=CARTESIAN_POINT('Ctrl Pts',(6.17080647799994,15.2,-8.86699760300001));
#167709=CARTESIAN_POINT('Ctrl Pts',(6.17080647799994,11.6,-8.86699760300001));
#167710=CARTESIAN_POINT('Ctrl Pts',(6.17289725299995,15.2,-8.86864556300001));
#167711=CARTESIAN_POINT('Ctrl Pts',(6.17289725299995,11.6,-8.86864556300001));
#167712=CARTESIAN_POINT('Ctrl Pts',(6.17499405399994,15.2,-8.87029539700002));
#167713=CARTESIAN_POINT('Ctrl Pts',(6.17499405399994,11.6,-8.87029539700002));
#167714=CARTESIAN_POINT('Ctrl Pts',(6.17709687799994,15.2,-8.87194709200001));
#167715=CARTESIAN_POINT('Ctrl Pts',(6.17709687799994,11.6,-8.87194709200001));
#167716=CARTESIAN_POINT('Ctrl Pts',(6.17920571999994,15.2,-8.87360063200001));
#167717=CARTESIAN_POINT('Ctrl Pts',(6.17920571999994,11.6,-8.87360063200001));
#167718=CARTESIAN_POINT('Ctrl Pts',(6.18132057899994,15.2,-8.87525600500001));
#167719=CARTESIAN_POINT('Ctrl Pts',(6.18132057899994,11.6,-8.87525600500001));
#167720=CARTESIAN_POINT('Ctrl Pts',(6.18344144899994,15.2,-8.87691319600002));
#167721=CARTESIAN_POINT('Ctrl Pts',(6.18344144899994,11.6,-8.87691319600002));
#167722=CARTESIAN_POINT('Ctrl Pts',(6.18556832799994,15.2,-8.87857219500002));
#167723=CARTESIAN_POINT('Ctrl Pts',(6.18556832799994,11.6,-8.87857219500002));
#167724=CARTESIAN_POINT('Ctrl Pts',(6.18770121399994,15.2,-8.88023298500002));
#167725=CARTESIAN_POINT('Ctrl Pts',(6.18770121399994,11.6,-8.88023298500002));
#167726=CARTESIAN_POINT('Ctrl Pts',(6.18984009999994,15.2,-8.88189555400002));
#167727=CARTESIAN_POINT('Ctrl Pts',(6.18984009999994,11.6,-8.88189555400002));
#167728=CARTESIAN_POINT('Ctrl Pts',(6.19198498599994,15.2,-8.88355988700001));
#167729=CARTESIAN_POINT('Ctrl Pts',(6.19198498599994,11.6,-8.88355988700001));
#167730=CARTESIAN_POINT('Ctrl Pts',(6.19413586799994,15.2,-8.88522597300001));
#167731=CARTESIAN_POINT('Ctrl Pts',(6.19413586799994,11.6,-8.88522597300001));
#167732=CARTESIAN_POINT('Ctrl Pts',(6.19629274299994,15.2,-8.88689379800002));
#167733=CARTESIAN_POINT('Ctrl Pts',(6.19629274299994,11.6,-8.88689379800002));
#167734=CARTESIAN_POINT('Ctrl Pts',(6.19845560599994,15.2,-8.88856334700002));
#167735=CARTESIAN_POINT('Ctrl Pts',(6.19845560599994,11.6,-8.88856334700002));
#167736=CARTESIAN_POINT('Ctrl Pts',(6.20062445399994,15.2,-8.89023460900002));
#167737=CARTESIAN_POINT('Ctrl Pts',(6.20062445399994,11.6,-8.89023460900002));
#167738=CARTESIAN_POINT('Ctrl Pts',(6.20279928499994,15.2,-8.89190757000001));
#167739=CARTESIAN_POINT('Ctrl Pts',(6.20279928499994,11.6,-8.89190757000001));
#167740=CARTESIAN_POINT('Ctrl Pts',(6.20498009499994,15.2,-8.89358221500002));
#167741=CARTESIAN_POINT('Ctrl Pts',(6.20498009499994,11.6,-8.89358221500002));
#167742=CARTESIAN_POINT('Ctrl Pts',(6.20716688099994,15.2,-8.89525853400002));
#167743=CARTESIAN_POINT('Ctrl Pts',(6.20716688099994,11.6,-8.89525853400002));
#167744=CARTESIAN_POINT('Ctrl Pts',(6.20935963799995,15.2,-8.89693651100002));
#167745=CARTESIAN_POINT('Ctrl Pts',(6.20935963799995,11.6,-8.89693651100002));
#167746=CARTESIAN_POINT('Ctrl Pts',(6.21155836399994,15.2,-8.89861613500001));
#167747=CARTESIAN_POINT('Ctrl Pts',(6.21155836399994,11.6,-8.89861613500001));
#167748=CARTESIAN_POINT('Ctrl Pts',(6.21376305499994,15.2,-8.90029739200001));
#167749=CARTESIAN_POINT('Ctrl Pts',(6.21376305499994,11.6,-8.90029739200001));
#167750=CARTESIAN_POINT('Ctrl Pts',(6.21597370899994,15.2,-8.90198026900002));
#167751=CARTESIAN_POINT('Ctrl Pts',(6.21597370899994,11.6,-8.90198026900002));
#167752=CARTESIAN_POINT('Ctrl Pts',(6.21819032199994,15.2,-8.90366475300001));
#167753=CARTESIAN_POINT('Ctrl Pts',(6.21819032199994,11.6,-8.90366475300001));
#167754=CARTESIAN_POINT('Ctrl Pts',(6.22041288899994,15.2,-8.90535083100002));
#167755=CARTESIAN_POINT('Ctrl Pts',(6.22041288899994,11.6,-8.90535083100002));
#167756=CARTESIAN_POINT('Ctrl Pts',(6.22264140799994,15.2,-8.90703849100002));
#167757=CARTESIAN_POINT('Ctrl Pts',(6.22264140799994,11.6,-8.90703849100002));
#167758=CARTESIAN_POINT('Ctrl Pts',(6.22487587699994,15.2,-8.90872771900002));
#167759=CARTESIAN_POINT('Ctrl Pts',(6.22487587699994,11.6,-8.90872771900002));
#167760=CARTESIAN_POINT('Ctrl Pts',(6.22711629099994,15.2,-8.91041850200001));
#167761=CARTESIAN_POINT('Ctrl Pts',(6.22711629099994,11.6,-8.91041850200001));
#167762=CARTESIAN_POINT('Ctrl Pts',(6.22936264599994,15.2,-8.91211082700002));
#167763=CARTESIAN_POINT('Ctrl Pts',(6.22936264599994,11.6,-8.91211082700002));
#167764=CARTESIAN_POINT('Ctrl Pts',(6.23161493899994,15.2,-8.91380468300002));
#167765=CARTESIAN_POINT('Ctrl Pts',(6.23161493899994,11.6,-8.91380468300002));
#167766=CARTESIAN_POINT('Ctrl Pts',(6.23387316899994,15.2,-8.91550005600001));
#167767=CARTESIAN_POINT('Ctrl Pts',(6.23387316899994,11.6,-8.91550005600001));
#167768=CARTESIAN_POINT('Ctrl Pts',(6.23613732999994,15.2,-8.91719693300002));
#167769=CARTESIAN_POINT('Ctrl Pts',(6.23613732999994,11.6,-8.91719693300002));
#167770=CARTESIAN_POINT('Ctrl Pts',(6.23840741799994,15.2,-8.91889530200002));
#167771=CARTESIAN_POINT('Ctrl Pts',(6.23840741799994,11.6,-8.91889530200002));
#167772=CARTESIAN_POINT('Ctrl Pts',(6.24068343299994,15.2,-8.92059515000001));
#167773=CARTESIAN_POINT('Ctrl Pts',(6.24068343299994,11.6,-8.92059515000001));
#167774=CARTESIAN_POINT('Ctrl Pts',(6.24296536899994,15.2,-8.92229646500001));
#167775=CARTESIAN_POINT('Ctrl Pts',(6.24296536899994,11.6,-8.92229646500001));
#167776=CARTESIAN_POINT('Ctrl Pts',(6.24525322299994,15.2,-8.92399923300001));
#167777=CARTESIAN_POINT('Ctrl Pts',(6.24525322299994,11.6,-8.92399923300001));
#167778=CARTESIAN_POINT('Ctrl Pts',(6.24754699199994,15.2,-8.92570344200001));
#167779=CARTESIAN_POINT('Ctrl Pts',(6.24754699199994,11.6,-8.92570344200001));
#167780=CARTESIAN_POINT('Ctrl Pts',(6.24984667299994,15.2,-8.92740908100001));
#167781=CARTESIAN_POINT('Ctrl Pts',(6.24984667299994,11.6,-8.92740908100001));
#167782=CARTESIAN_POINT('Ctrl Pts',(6.25215226099994,15.2,-8.92911613600001));
#167783=CARTESIAN_POINT('Ctrl Pts',(6.25215226099994,11.6,-8.92911613600001));
#167784=CARTESIAN_POINT('Ctrl Pts',(6.25446375499994,15.2,-8.93082459400001));
#167785=CARTESIAN_POINT('Ctrl Pts',(6.25446375499994,11.6,-8.93082459400001));
#167786=CARTESIAN_POINT('Ctrl Pts',(6.25678114899994,15.2,-8.93253444400001));
#167787=CARTESIAN_POINT('Ctrl Pts',(6.25678114899994,11.6,-8.93253444400001));
#167788=CARTESIAN_POINT('Ctrl Pts',(6.25910444299994,15.2,-8.93424567300002));
#167789=CARTESIAN_POINT('Ctrl Pts',(6.25910444299994,11.6,-8.93424567300002));
#167790=CARTESIAN_POINT('Ctrl Pts',(6.26143362999994,15.2,-8.93595826800002));
#167791=CARTESIAN_POINT('Ctrl Pts',(6.26143362999994,11.6,-8.93595826800002));
#167792=CARTESIAN_POINT('Ctrl Pts',(6.26376870799994,15.2,-8.93767221800001));
#167793=CARTESIAN_POINT('Ctrl Pts',(6.26376870799994,11.6,-8.93767221800001));
#167794=CARTESIAN_POINT('Ctrl Pts',(6.26610967499994,15.2,-8.93938751000002));
#167795=CARTESIAN_POINT('Ctrl Pts',(6.26610967499994,11.6,-8.93938751000002));
#167796=CARTESIAN_POINT('Ctrl Pts',(6.26845652499994,15.2,-8.94110413200002));
#167797=CARTESIAN_POINT('Ctrl Pts',(6.26845652499994,11.6,-8.94110413200002));
#167798=CARTESIAN_POINT('Ctrl Pts',(6.27080925699994,15.2,-8.94282207100002));
#167799=CARTESIAN_POINT('Ctrl Pts',(6.27080925699994,11.6,-8.94282207100002));
#167800=CARTESIAN_POINT('Ctrl Pts',(6.27316786699994,15.2,-8.94454131600002));
#167801=CARTESIAN_POINT('Ctrl Pts',(6.27316786699994,11.6,-8.94454131600002));
#167802=CARTESIAN_POINT('Ctrl Pts',(6.27553235099994,15.2,-8.94626185400002));
#167803=CARTESIAN_POINT('Ctrl Pts',(6.27553235099994,11.6,-8.94626185400002));
#167804=CARTESIAN_POINT('Ctrl Pts',(6.27790270499994,15.2,-8.94798367200002));
#167805=CARTESIAN_POINT('Ctrl Pts',(6.27790270499994,11.6,-8.94798367200002));
#167806=CARTESIAN_POINT('Ctrl Pts',(6.28027892799994,15.2,-8.94970676000002));
#167807=CARTESIAN_POINT('Ctrl Pts',(6.28027892799994,11.6,-8.94970676000002));
#167808=CARTESIAN_POINT('Ctrl Pts',(6.28266101299994,15.2,-8.95143110400002));
#167809=CARTESIAN_POINT('Ctrl Pts',(6.28266101299994,11.6,-8.95143110400002));
#167810=CARTESIAN_POINT('Ctrl Pts',(6.28504895899994,15.2,-8.95315669400001));
#167811=CARTESIAN_POINT('Ctrl Pts',(6.28504895899994,11.6,-8.95315669400001));
#167812=CARTESIAN_POINT('Ctrl Pts',(6.28744276399994,15.2,-8.95488351500001));
#167813=CARTESIAN_POINT('Ctrl Pts',(6.28744276399994,11.6,-8.95488351500001));
#167814=CARTESIAN_POINT('Ctrl Pts',(6.28984242199994,15.2,-8.95661155900001));
#167815=CARTESIAN_POINT('Ctrl Pts',(6.28984242199994,11.6,-8.95661155900001));
#167816=CARTESIAN_POINT('Ctrl Pts',(6.29224792999994,15.2,-8.95834081000002));
#167817=CARTESIAN_POINT('Ctrl Pts',(6.29224792999994,11.6,-8.95834081000002));
#167818=CARTESIAN_POINT('Ctrl Pts',(6.29465928599994,15.2,-8.96007125900002));
#167819=CARTESIAN_POINT('Ctrl Pts',(6.29465928599994,11.6,-8.96007125900002));
#167820=CARTESIAN_POINT('Ctrl Pts',(6.29707648499994,15.2,-8.96180289200002));
#167821=CARTESIAN_POINT('Ctrl Pts',(6.29707648499994,11.6,-8.96180289200002));
#167822=CARTESIAN_POINT('Ctrl Pts',(6.29949952399994,15.2,-8.96353569800001));
#167823=CARTESIAN_POINT('Ctrl Pts',(6.29949952399994,11.6,-8.96353569800001));
#167824=CARTESIAN_POINT('Ctrl Pts',(6.30192839999994,15.2,-8.96526966600002));
#167825=CARTESIAN_POINT('Ctrl Pts',(6.30192839999994,11.6,-8.96526966600002));
#167826=CARTESIAN_POINT('Ctrl Pts',(6.30436310999994,15.2,-8.96700478300002));
#167827=CARTESIAN_POINT('Ctrl Pts',(6.30436310999994,11.6,-8.96700478300002));
#167828=CARTESIAN_POINT('Ctrl Pts',(6.30680364899994,15.2,-8.96874103900002));
#167829=CARTESIAN_POINT('Ctrl Pts',(6.30680364899994,11.6,-8.96874103900002));
#167830=CARTESIAN_POINT('Ctrl Pts',(6.30925001499994,15.2,-8.97047842000001));
#167831=CARTESIAN_POINT('Ctrl Pts',(6.30925001499994,11.6,-8.97047842000001));
#167832=CARTESIAN_POINT('Ctrl Pts',(6.31170220399994,15.2,-8.97221691500001));
#167833=CARTESIAN_POINT('Ctrl Pts',(6.31170220399994,11.6,-8.97221691500001));
#167834=CARTESIAN_POINT('Ctrl Pts',(6.31416021399994,15.2,-8.97395651300002));
#167835=CARTESIAN_POINT('Ctrl Pts',(6.31416021399994,11.6,-8.97395651300002));
#167836=CARTESIAN_POINT('Ctrl Pts',(6.31662403899994,15.2,-8.97569720100002));
#167837=CARTESIAN_POINT('Ctrl Pts',(6.31662403899994,11.6,-8.97569720100002));
#167838=CARTESIAN_POINT('Ctrl Pts',(6.31909367699994,15.2,-8.97743896900002));
#167839=CARTESIAN_POINT('Ctrl Pts',(6.31909367699994,11.6,-8.97743896900002));
#167840=CARTESIAN_POINT('Ctrl Pts',(6.32156912499994,15.2,-8.97918180400002));
#167841=CARTESIAN_POINT('Ctrl Pts',(6.32156912499994,11.6,-8.97918180400002));
#167842=CARTESIAN_POINT('Ctrl Pts',(6.32405037899994,15.2,-8.98092569600001));
#167843=CARTESIAN_POINT('Ctrl Pts',(6.32405037899994,11.6,-8.98092569600001));
#167844=CARTESIAN_POINT('Ctrl Pts',(6.32653743599994,15.2,-8.98267063100001));
#167845=CARTESIAN_POINT('Ctrl Pts',(6.32653743599994,11.6,-8.98267063100001));
#167846=CARTESIAN_POINT('Ctrl Pts',(6.32903029199994,15.2,-8.98441660100002));
#167847=CARTESIAN_POINT('Ctrl Pts',(6.32903029199994,11.6,-8.98441660100002));
#167848=CARTESIAN_POINT('Ctrl Pts',(6.33152894299994,15.2,-8.98616359100001));
#167849=CARTESIAN_POINT('Ctrl Pts',(6.33152894299994,11.6,-8.98616359100001));
#167850=CARTESIAN_POINT('Ctrl Pts',(6.33403338799994,15.2,-8.98791159100002));
#167851=CARTESIAN_POINT('Ctrl Pts',(6.33403338799994,11.6,-8.98791159100002));
#167852=CARTESIAN_POINT('Ctrl Pts',(6.33654362099994,15.2,-8.98966059000001));
#167853=CARTESIAN_POINT('Ctrl Pts',(6.33654362099994,11.6,-8.98966059000001));
#167854=CARTESIAN_POINT('Ctrl Pts',(6.33905963999994,15.2,-8.99141057600002));
#167855=CARTESIAN_POINT('Ctrl Pts',(6.33905963999994,11.6,-8.99141057600002));
#167856=CARTESIAN_POINT('Ctrl Pts',(6.34158143999994,15.2,-8.99316153900001));
#167857=CARTESIAN_POINT('Ctrl Pts',(6.34158143999994,11.6,-8.99316153900001));
#167858=CARTESIAN_POINT('Ctrl Pts',(6.34410901999994,15.2,-8.99491346500002));
#167859=CARTESIAN_POINT('Ctrl Pts',(6.34410901999994,11.6,-8.99491346500002));
#167860=CARTESIAN_POINT('Ctrl Pts',(6.34664237499994,15.2,-8.99666634500001));
#167861=CARTESIAN_POINT('Ctrl Pts',(6.34664237499994,11.6,-8.99666634500001));
#167862=CARTESIAN_POINT('Ctrl Pts',(6.34918150099994,15.2,-8.99842016600001));
#167863=CARTESIAN_POINT('Ctrl Pts',(6.34918150099994,11.6,-8.99842016600001));
#167864=CARTESIAN_POINT('Ctrl Pts',(6.35172639699994,15.2,-9.00017491800002));
#167865=CARTESIAN_POINT('Ctrl Pts',(6.35172639699994,11.6,-9.00017491800002));
#167866=CARTESIAN_POINT('Ctrl Pts',(6.35427705599994,15.2,-9.00193058900001));
#167867=CARTESIAN_POINT('Ctrl Pts',(6.35427705599994,11.6,-9.00193058900001));
#167868=CARTESIAN_POINT('Ctrl Pts',(6.35683347799994,15.2,-9.00368716800001));
#167869=CARTESIAN_POINT('Ctrl Pts',(6.35683347799994,11.6,-9.00368716800001));
#167870=CARTESIAN_POINT('Ctrl Pts',(6.35939565699994,15.2,-9.00544464400001));
#167871=CARTESIAN_POINT('Ctrl Pts',(6.35939565699994,11.6,-9.00544464400001));
#167872=CARTESIAN_POINT('Ctrl Pts',(6.36196359199994,15.2,-9.00720300600002));
#167873=CARTESIAN_POINT('Ctrl Pts',(6.36196359199994,11.6,-9.00720300600002));
#167874=CARTESIAN_POINT('Ctrl Pts',(6.36453727799994,15.2,-9.00896224300002));
#167875=CARTESIAN_POINT('Ctrl Pts',(6.36453727799994,11.6,-9.00896224300002));
#167876=CARTESIAN_POINT('Ctrl Pts',(6.36711671099994,15.2,-9.01072234300001));
#167877=CARTESIAN_POINT('Ctrl Pts',(6.36711671099994,11.6,-9.01072234300001));
#167878=CARTESIAN_POINT('Ctrl Pts',(6.36970188799994,15.2,-9.01248329400002));
#167879=CARTESIAN_POINT('Ctrl Pts',(6.36970188799994,11.6,-9.01248329400002));
#167880=CARTESIAN_POINT('Ctrl Pts',(6.37229280699994,15.2,-9.01424508800002));
#167881=CARTESIAN_POINT('Ctrl Pts',(6.37229280699994,11.6,-9.01424508800002));
#167882=CARTESIAN_POINT('Ctrl Pts',(6.37488946299994,15.2,-9.01600771300001));
#167883=CARTESIAN_POINT('Ctrl Pts',(6.37488946299994,11.6,-9.01600771300001));
#167884=CARTESIAN_POINT('Ctrl Pts',(6.37749185299994,15.2,-9.01777115600002));
#167885=CARTESIAN_POINT('Ctrl Pts',(6.37749185299994,11.6,-9.01777115600002));
#167886=CARTESIAN_POINT('Ctrl Pts',(6.38009997299994,15.2,-9.01953540700001));
#167887=CARTESIAN_POINT('Ctrl Pts',(6.38009997299994,11.6,-9.01953540700001));
#167888=CARTESIAN_POINT('Ctrl Pts',(6.38271382099994,15.2,-9.02130045600002));
#167889=CARTESIAN_POINT('Ctrl Pts',(6.38271382099994,11.6,-9.02130045600002));
#167890=CARTESIAN_POINT('Ctrl Pts',(6.38533339199994,15.2,-9.02306629200002));
#167891=CARTESIAN_POINT('Ctrl Pts',(6.38533339199994,11.6,-9.02306629200002));
#167892=CARTESIAN_POINT('Ctrl Pts',(6.38795868399994,15.2,-9.02483290300001));
#167893=CARTESIAN_POINT('Ctrl Pts',(6.38795868399994,11.6,-9.02483290300001));
#167894=CARTESIAN_POINT('Ctrl Pts',(6.39058969199994,15.2,-9.02660027900002));
#167895=CARTESIAN_POINT('Ctrl Pts',(6.39058969199994,11.6,-9.02660027900002));
#167896=CARTESIAN_POINT('Ctrl Pts',(6.39322641399994,15.2,-9.02836840800001));
#167897=CARTESIAN_POINT('Ctrl Pts',(6.39322641399994,11.6,-9.02836840800001));
#167898=CARTESIAN_POINT('Ctrl Pts',(6.39586884499994,15.2,-9.03013728200002));
#167899=CARTESIAN_POINT('Ctrl Pts',(6.39586884499994,11.6,-9.03013728200002));
#167900=CARTESIAN_POINT('Ctrl Pts',(6.39851698299994,15.2,-9.03190688700001));
#167901=CARTESIAN_POINT('Ctrl Pts',(6.39851698299994,11.6,-9.03190688700001));
#167902=CARTESIAN_POINT('Ctrl Pts',(6.40117082299994,15.2,-9.03367721300001));
#167903=CARTESIAN_POINT('Ctrl Pts',(6.40117082299994,11.6,-9.03367721300001));
#167904=CARTESIAN_POINT('Ctrl Pts',(6.40383036299994,15.2,-9.03544825000001));
#167905=CARTESIAN_POINT('Ctrl Pts',(6.40383036299994,11.6,-9.03544825000001));
#167906=CARTESIAN_POINT('Ctrl Pts',(6.40649559999994,15.2,-9.03721998700002));
#167907=CARTESIAN_POINT('Ctrl Pts',(6.40649559999994,11.6,-9.03721998700002));
#167908=CARTESIAN_POINT('Ctrl Pts',(6.40916652899994,15.2,-9.03899241300002));
#167909=CARTESIAN_POINT('Ctrl Pts',(6.40916652899994,11.6,-9.03899241300002));
#167910=CARTESIAN_POINT('Ctrl Pts',(6.41184314599994,15.2,-9.04076551800001));
#167911=CARTESIAN_POINT('Ctrl Pts',(6.41184314599994,11.6,-9.04076551800001));
#167912=CARTESIAN_POINT('Ctrl Pts',(6.41452544999994,15.2,-9.04253929100001));
#167913=CARTESIAN_POINT('Ctrl Pts',(6.41452544999994,11.6,-9.04253929100001));
#167914=CARTESIAN_POINT('Ctrl Pts',(6.41721343599994,15.2,-9.04431372100002));
#167915=CARTESIAN_POINT('Ctrl Pts',(6.41721343599994,11.6,-9.04431372100002));
#167916=CARTESIAN_POINT('Ctrl Pts',(6.41990709999994,15.2,-9.04608879800002));
#167917=CARTESIAN_POINT('Ctrl Pts',(6.41990709999994,11.6,-9.04608879800002));
#167918=CARTESIAN_POINT('Ctrl Pts',(6.42260643999994,15.2,-9.04786451100002));
#167919=CARTESIAN_POINT('Ctrl Pts',(6.42260643999994,11.6,-9.04786451100002));
#167920=CARTESIAN_POINT('Ctrl Pts',(6.42531145199994,15.2,-9.04964084900002));
#167921=CARTESIAN_POINT('Ctrl Pts',(6.42531145199994,11.6,-9.04964084900002));
#167922=CARTESIAN_POINT('Ctrl Pts',(6.42802213199994,15.2,-9.05141780400001));
#167923=CARTESIAN_POINT('Ctrl Pts',(6.42802213199994,11.6,-9.05141780400001));
#167924=CARTESIAN_POINT('Ctrl Pts',(6.43073847599994,15.2,-9.05319536200002));
#167925=CARTESIAN_POINT('Ctrl Pts',(6.43073847599994,11.6,-9.05319536200002));
#167926=CARTESIAN_POINT('Ctrl Pts',(6.43346048199994,15.2,-9.05497351500001));
#167927=CARTESIAN_POINT('Ctrl Pts',(6.43346048199994,11.6,-9.05497351500001));
#167928=CARTESIAN_POINT('Ctrl Pts',(6.43618814599995,15.2,-9.05675225100002));
#167929=CARTESIAN_POINT('Ctrl Pts',(6.43618814599995,11.6,-9.05675225100002));
#167930=CARTESIAN_POINT('Ctrl Pts',(6.43892146399994,15.2,-9.05853156000001));
#167931=CARTESIAN_POINT('Ctrl Pts',(6.43892146399994,11.6,-9.05853156000001));
#167932=CARTESIAN_POINT('Ctrl Pts',(6.44166043299994,15.2,-9.06031143300002));
#167933=CARTESIAN_POINT('Ctrl Pts',(6.44166043299994,11.6,-9.06031143300002));
#167934=CARTESIAN_POINT('Ctrl Pts',(6.44440504999994,15.2,-9.06209185800002));
#167935=CARTESIAN_POINT('Ctrl Pts',(6.44440504999994,11.6,-9.06209185800002));
#167936=CARTESIAN_POINT('Ctrl Pts',(6.44715531099994,15.2,-9.06387282500001));
#167937=CARTESIAN_POINT('Ctrl Pts',(6.44715531099994,11.6,-9.06387282500001));
#167938=CARTESIAN_POINT('Ctrl Pts',(6.44991121199994,15.2,-9.06565432300001));
#167939=CARTESIAN_POINT('Ctrl Pts',(6.44991121199994,11.6,-9.06565432300001));
#167940=CARTESIAN_POINT('Ctrl Pts',(6.45267274999994,15.2,-9.06743634400001));
#167941=CARTESIAN_POINT('Ctrl Pts',(6.45267274999994,11.6,-9.06743634400001));
#167942=CARTESIAN_POINT('Ctrl Pts',(6.45543992299994,15.2,-9.06921887500001));
#167943=CARTESIAN_POINT('Ctrl Pts',(6.45543992299994,11.6,-9.06921887500001));
#167944=CARTESIAN_POINT('Ctrl Pts',(6.45821272399994,15.2,-9.07100190800002));
#167945=CARTESIAN_POINT('Ctrl Pts',(6.45821272399994,11.6,-9.07100190800002));
#167946=CARTESIAN_POINT('Ctrl Pts',(6.46099115299994,15.2,-9.07278543100002));
#167947=CARTESIAN_POINT('Ctrl Pts',(6.46099115299994,11.6,-9.07278543100002));
#167948=CARTESIAN_POINT('Ctrl Pts',(6.46377520499994,15.2,-9.07456943400001));
#167949=CARTESIAN_POINT('Ctrl Pts',(6.46377520499994,11.6,-9.07456943400001));
#167950=CARTESIAN_POINT('Ctrl Pts',(6.46656487599994,15.2,-9.07635390800002));
#167951=CARTESIAN_POINT('Ctrl Pts',(6.46656487599994,11.6,-9.07635390800002));
#167952=CARTESIAN_POINT('Ctrl Pts',(6.46936016299994,15.2,-9.07813884200002));
#167953=CARTESIAN_POINT('Ctrl Pts',(6.46936016299994,11.6,-9.07813884200002));
#167954=CARTESIAN_POINT('Ctrl Pts',(6.47216106399994,15.2,-9.07992422500002));
#167955=CARTESIAN_POINT('Ctrl Pts',(6.47216106399994,11.6,-9.07992422500002));
#167956=CARTESIAN_POINT('Ctrl Pts',(6.47496757199994,15.2,-9.08171004900002));
#167957=CARTESIAN_POINT('Ctrl Pts',(6.47496757199994,11.6,-9.08171004900002));
#167958=CARTESIAN_POINT('Ctrl Pts',(6.47777968799994,15.2,-9.08349630400001));
#167959=CARTESIAN_POINT('Ctrl Pts',(6.47777968799994,11.6,-9.08349630400001));
#167960=CARTESIAN_POINT('Ctrl Pts',(6.48059740499994,15.2,-9.08528297600002));
#167961=CARTESIAN_POINT('Ctrl Pts',(6.48059740499994,11.6,-9.08528297600002));
#167962=CARTESIAN_POINT('Ctrl Pts',(6.48342072099994,15.2,-9.08707005900002));
#167963=CARTESIAN_POINT('Ctrl Pts',(6.48342072099994,11.6,-9.08707005900002));
#167964=CARTESIAN_POINT('Ctrl Pts',(6.48624963199994,15.2,-9.08885754100002));
#167965=CARTESIAN_POINT('Ctrl Pts',(6.48624963199994,11.6,-9.08885754100002));
#167966=CARTESIAN_POINT('Ctrl Pts',(6.48908413499994,15.2,-9.09064541400002));
#167967=CARTESIAN_POINT('Ctrl Pts',(6.48908413499994,11.6,-9.09064541400002));
#167968=CARTESIAN_POINT('Ctrl Pts',(6.49192422599994,15.2,-9.09243366500002));
#167969=CARTESIAN_POINT('Ctrl Pts',(6.49192422599994,11.6,-9.09243366500002));
#167970=CARTESIAN_POINT('Ctrl Pts',(6.49476990199994,15.2,-9.09422228700001));
#167971=CARTESIAN_POINT('Ctrl Pts',(6.49476990199994,11.6,-9.09422228700001));
#167972=CARTESIAN_POINT('Ctrl Pts',(6.49762115899994,15.2,-9.09601126700002));
#167973=CARTESIAN_POINT('Ctrl Pts',(6.49762115899994,11.6,-9.09601126700002));
#167974=CARTESIAN_POINT('Ctrl Pts',(6.50047799399994,15.2,-9.09780059800001));
#167975=CARTESIAN_POINT('Ctrl Pts',(6.50047799399994,11.6,-9.09780059800001));
#167976=CARTESIAN_POINT('Ctrl Pts',(6.50334040299994,15.2,-9.09959026900001));
#167977=CARTESIAN_POINT('Ctrl Pts',(6.50334040299994,11.6,-9.09959026900001));
#167978=CARTESIAN_POINT('Ctrl Pts',(6.50620838199995,15.2,-9.10138026900002));
#167979=CARTESIAN_POINT('Ctrl Pts',(6.50620838199995,11.6,-9.10138026900002));
#167980=CARTESIAN_POINT('Ctrl Pts',(6.50908192999994,15.2,-9.10317059000001));
#167981=CARTESIAN_POINT('Ctrl Pts',(6.50908192999994,11.6,-9.10317059000001));
#167982=CARTESIAN_POINT('Ctrl Pts',(6.51196104099995,15.2,-9.10496122100002));
#167983=CARTESIAN_POINT('Ctrl Pts',(6.51196104099995,11.6,-9.10496122100002));
#167984=CARTESIAN_POINT('Ctrl Pts',(6.51484571099994,15.2,-9.10675215300002));
#167985=CARTESIAN_POINT('Ctrl Pts',(6.51484571099994,11.6,-9.10675215300002));
#167986=CARTESIAN_POINT('Ctrl Pts',(6.51773593899994,15.2,-9.10854337500002));
#167987=CARTESIAN_POINT('Ctrl Pts',(6.51773593899994,11.6,-9.10854337500002));
#167988=CARTESIAN_POINT('Ctrl Pts',(6.52063172099994,15.2,-9.11033487800001));
#167989=CARTESIAN_POINT('Ctrl Pts',(6.52063172099994,11.6,-9.11033487800001));
#167990=CARTESIAN_POINT('Ctrl Pts',(6.52353305099994,15.2,-9.11212665200001));
#167991=CARTESIAN_POINT('Ctrl Pts',(6.52353305099994,11.6,-9.11212665200001));
#167992=CARTESIAN_POINT('Ctrl Pts',(6.52643992799994,15.2,-9.11391868900001));
#167993=CARTESIAN_POINT('Ctrl Pts',(6.52643992799994,11.6,-9.11391868900001));
#167994=CARTESIAN_POINT('Ctrl Pts',(6.52935234699994,15.2,-9.11571097500002));
#167995=CARTESIAN_POINT('Ctrl Pts',(6.52935234699994,11.6,-9.11571097500002));
#167996=CARTESIAN_POINT('Ctrl Pts',(6.53227030599994,15.2,-9.11750350600002));
#167997=CARTESIAN_POINT('Ctrl Pts',(6.53227030599994,11.6,-9.11750350600002));
#167998=CARTESIAN_POINT('Ctrl Pts',(6.53519379999994,15.2,-9.11929626800001));
#167999=CARTESIAN_POINT('Ctrl Pts',(6.53519379999994,11.6,-9.11929626800001));
#168000=CARTESIAN_POINT('Ctrl Pts',(6.53812282699994,15.2,-9.12108925300002));
#168001=CARTESIAN_POINT('Ctrl Pts',(6.53812282699994,11.6,-9.12108925300002));
#168002=CARTESIAN_POINT('Ctrl Pts',(6.54105738299994,15.2,-9.12288245200001));
#168003=CARTESIAN_POINT('Ctrl Pts',(6.54105738299994,11.6,-9.12288245200001));
#168004=CARTESIAN_POINT('Ctrl Pts',(6.54399746299994,15.2,-9.12467585300002));
#168005=CARTESIAN_POINT('Ctrl Pts',(6.54399746299994,11.6,-9.12467585300002));
#168006=CARTESIAN_POINT('Ctrl Pts',(6.54694306499994,15.2,-9.12646944900001));
#168007=CARTESIAN_POINT('Ctrl Pts',(6.54694306499994,11.6,-9.12646944900001));
#168008=CARTESIAN_POINT('Ctrl Pts',(6.54989418399994,15.2,-9.12826322900001));
#168009=CARTESIAN_POINT('Ctrl Pts',(6.54989418399994,11.6,-9.12826322900001));
#168010=CARTESIAN_POINT('Ctrl Pts',(6.55285081899994,15.2,-9.13005718400001));
#168011=CARTESIAN_POINT('Ctrl Pts',(6.55285081899994,11.6,-9.13005718400001));
#168012=CARTESIAN_POINT('Ctrl Pts',(6.55581296599994,15.2,-9.13185130500001));
#168013=CARTESIAN_POINT('Ctrl Pts',(6.55581296599994,11.6,-9.13185130500001));
#168014=CARTESIAN_POINT('Ctrl Pts',(6.55878061899994,15.2,-9.13364558100002));
#168015=CARTESIAN_POINT('Ctrl Pts',(6.55878061899994,11.6,-9.13364558100002));
#168016=CARTESIAN_POINT('Ctrl Pts',(6.56175377599994,15.2,-9.13544000400002));
#168017=CARTESIAN_POINT('Ctrl Pts',(6.56175377599994,11.6,-9.13544000400002));
#168018=CARTESIAN_POINT('Ctrl Pts',(6.56473243399994,15.2,-9.13723456500002));
#168019=CARTESIAN_POINT('Ctrl Pts',(6.56473243399994,11.6,-9.13723456500002));
#168020=CARTESIAN_POINT('Ctrl Pts',(6.56771658899994,15.2,-9.13902925200002));
#168021=CARTESIAN_POINT('Ctrl Pts',(6.56771658899994,11.6,-9.13902925200002));
#168022=CARTESIAN_POINT('Ctrl Pts',(6.57070623699994,15.2,-9.14082405700002));
#168023=CARTESIAN_POINT('Ctrl Pts',(6.57070623699994,11.6,-9.14082405700002));
#168024=CARTESIAN_POINT('Ctrl Pts',(6.57370137599994,15.2,-9.14261897200002));
#168025=CARTESIAN_POINT('Ctrl Pts',(6.57370137599994,11.6,-9.14261897200002));
#168026=CARTESIAN_POINT('Ctrl Pts',(6.57670199999994,15.2,-9.14441398600001));
#168027=CARTESIAN_POINT('Ctrl Pts',(6.57670199999994,11.6,-9.14441398600001));
#168028=CARTESIAN_POINT('Ctrl Pts',(6.57970810799994,15.2,-9.14620908900002));
#168029=CARTESIAN_POINT('Ctrl Pts',(6.57970810799994,11.6,-9.14620908900002));
#168030=CARTESIAN_POINT('Ctrl Pts',(6.58271969499994,15.2,-9.14800427400002));
#168031=CARTESIAN_POINT('Ctrl Pts',(6.58271969499994,11.6,-9.14800427400002));
#168032=CARTESIAN_POINT('Ctrl Pts',(6.58573675799994,15.2,-9.14979953100002));
#168033=CARTESIAN_POINT('Ctrl Pts',(6.58573675799994,11.6,-9.14979953100002));
#168034=CARTESIAN_POINT('Ctrl Pts',(6.58875929299994,15.2,-9.15159484900002));
#168035=CARTESIAN_POINT('Ctrl Pts',(6.58875929299994,11.6,-9.15159484900002));
#168036=CARTESIAN_POINT('Ctrl Pts',(6.59178729699994,15.2,-9.15339022000002));
#168037=CARTESIAN_POINT('Ctrl Pts',(6.59178729699994,11.6,-9.15339022000002));
#168038=CARTESIAN_POINT('Ctrl Pts',(6.59482076499994,15.2,-9.15518563400001));
#168039=CARTESIAN_POINT('Ctrl Pts',(6.59482076499994,11.6,-9.15518563400001));
#168040=CARTESIAN_POINT('Ctrl Pts',(6.59785969599994,15.2,-9.15698108300001));
#168041=CARTESIAN_POINT('Ctrl Pts',(6.59785969599994,11.6,-9.15698108300001));
#168042=CARTESIAN_POINT('Ctrl Pts',(6.60090408599994,15.2,-9.15877655700001));
#168043=CARTESIAN_POINT('Ctrl Pts',(6.60090408599994,11.6,-9.15877655700001));
#168044=CARTESIAN_POINT('Ctrl Pts',(6.60395392899995,15.2,-9.16057204700002));
#168045=CARTESIAN_POINT('Ctrl Pts',(6.60395392899995,11.6,-9.16057204700002));
#168046=CARTESIAN_POINT('Ctrl Pts',(6.60700922399994,15.2,-9.16236754400002));
#168047=CARTESIAN_POINT('Ctrl Pts',(6.60700922399994,11.6,-9.16236754400002));
#168048=CARTESIAN_POINT('Ctrl Pts',(6.61006996599995,15.2,-9.16416303900002));
#168049=CARTESIAN_POINT('Ctrl Pts',(6.61006996599995,11.6,-9.16416303900002));
#168050=CARTESIAN_POINT('Ctrl Pts',(6.61313615199994,15.2,-9.16595852100002));
#168051=CARTESIAN_POINT('Ctrl Pts',(6.61313615199994,11.6,-9.16595852100002));
#168052=CARTESIAN_POINT('Ctrl Pts',(6.61620777899994,15.2,-9.16775398400001));
#168053=CARTESIAN_POINT('Ctrl Pts',(6.61620777899994,11.6,-9.16775398400001));
#168054=CARTESIAN_POINT('Ctrl Pts',(6.61928484299994,15.2,-9.16954941700002));
#168055=CARTESIAN_POINT('Ctrl Pts',(6.61928484299994,11.6,-9.16954941700002));
#168056=CARTESIAN_POINT('Ctrl Pts',(6.62236733999994,15.2,-9.17134481100002));
#168057=CARTESIAN_POINT('Ctrl Pts',(6.62236733999994,11.6,-9.17134481100002));
#168058=CARTESIAN_POINT('Ctrl Pts',(6.62545526699994,15.2,-9.17314015600001));
#168059=CARTESIAN_POINT('Ctrl Pts',(6.62545526699994,11.6,-9.17314015600001));
#168060=CARTESIAN_POINT('Ctrl Pts',(6.62854862099994,15.2,-9.17493544700001));
#168061=CARTESIAN_POINT('Ctrl Pts',(6.62854862099994,11.6,-9.17493544700001));
#168062=CARTESIAN_POINT('Ctrl Pts',(6.63164739699994,15.2,-9.17673067000001));
#168063=CARTESIAN_POINT('Ctrl Pts',(6.63164739699994,11.6,-9.17673067000001));
#168064=CARTESIAN_POINT('Ctrl Pts',(6.63475159199994,15.2,-9.17852581800001));
#168065=CARTESIAN_POINT('Ctrl Pts',(6.63475159199994,11.6,-9.17852581800001));
#168066=CARTESIAN_POINT('Ctrl Pts',(6.63786120299994,15.2,-9.18032088200002));
#168067=CARTESIAN_POINT('Ctrl Pts',(6.63786120299994,11.6,-9.18032088200002));
#168068=CARTESIAN_POINT('Ctrl Pts',(6.64097622599994,15.2,-9.18211585500002));
#168069=CARTESIAN_POINT('Ctrl Pts',(6.64097622599994,11.6,-9.18211585500002));
#168070=CARTESIAN_POINT('Ctrl Pts',(6.64409665799995,15.2,-9.18391072500001));
#168071=CARTESIAN_POINT('Ctrl Pts',(6.64409665799995,11.6,-9.18391072500001));
#168072=CARTESIAN_POINT('Ctrl Pts',(6.64722249499994,15.2,-9.18570548400002));
#168073=CARTESIAN_POINT('Ctrl Pts',(6.64722249499994,11.6,-9.18570548400002));
#168074=CARTESIAN_POINT('Ctrl Pts',(6.65035373299995,15.2,-9.18750012300002));
#168075=CARTESIAN_POINT('Ctrl Pts',(6.65035373299995,11.6,-9.18750012300002));
#168076=CARTESIAN_POINT('Ctrl Pts',(6.65349036899994,15.2,-9.18929463500002));
#168077=CARTESIAN_POINT('Ctrl Pts',(6.65349036899994,11.6,-9.18929463500002));
#168078=CARTESIAN_POINT('Ctrl Pts',(6.65663239999994,15.2,-9.19108900900002));
#168079=CARTESIAN_POINT('Ctrl Pts',(6.65663239999994,11.6,-9.19108900900002));
#168080=CARTESIAN_POINT('Ctrl Pts',(6.65977982099994,15.2,-9.19288323700002));
#168081=CARTESIAN_POINT('Ctrl Pts',(6.65977982099994,11.6,-9.19288323700002));
#168082=CARTESIAN_POINT('Ctrl Pts',(6.66293262999995,15.2,-9.19467731100001));
#168083=CARTESIAN_POINT('Ctrl Pts',(6.66293262999995,11.6,-9.19467731100001));
#168084=CARTESIAN_POINT('Ctrl Pts',(6.66609082299995,15.2,-9.19647121900002));
#168085=CARTESIAN_POINT('Ctrl Pts',(6.66609082299995,11.6,-9.19647121900002));
#168086=CARTESIAN_POINT('Ctrl Pts',(6.66925439499994,15.2,-9.19826495600002));
#168087=CARTESIAN_POINT('Ctrl Pts',(6.66925439499994,11.6,-9.19826495600002));
#168088=CARTESIAN_POINT('Ctrl Pts',(6.67242334399995,15.2,-9.20005851000001));
#168089=CARTESIAN_POINT('Ctrl Pts',(6.67242334399995,11.6,-9.20005851000001));
#168090=CARTESIAN_POINT('Ctrl Pts',(6.67559766699994,15.2,-9.20185187500002));
#168091=CARTESIAN_POINT('Ctrl Pts',(6.67559766699994,11.6,-9.20185187500002));
#168092=CARTESIAN_POINT('Ctrl Pts',(6.67877735899994,15.2,-9.20364504200002));
#168093=CARTESIAN_POINT('Ctrl Pts',(6.67877735899994,11.6,-9.20364504200002));
#168094=CARTESIAN_POINT('Ctrl Pts',(6.68196241599994,15.2,-9.20543800000001));
#168095=CARTESIAN_POINT('Ctrl Pts',(6.68196241599994,11.6,-9.20543800000001));
#168096=CARTESIAN_POINT('Ctrl Pts',(6.68515283699994,15.2,-9.20723074200002));
#168097=CARTESIAN_POINT('Ctrl Pts',(6.68515283699994,11.6,-9.20723074200002));
#168098=CARTESIAN_POINT('Ctrl Pts',(6.68834861499994,15.2,-9.20902325900002));
#168099=CARTESIAN_POINT('Ctrl Pts',(6.68834861499994,11.6,-9.20902325900002));
#168100=CARTESIAN_POINT('Ctrl Pts',(6.69154974999994,15.2,-9.21081554300001));
#168101=CARTESIAN_POINT('Ctrl Pts',(6.69154974999994,11.6,-9.21081554300001));
#168102=CARTESIAN_POINT('Ctrl Pts',(6.69475623599994,15.2,-9.21260758400001));
#168103=CARTESIAN_POINT('Ctrl Pts',(6.69475623599994,11.6,-9.21260758400001));
#168104=CARTESIAN_POINT('Ctrl Pts',(6.69796806999994,15.2,-9.21439937500002));
#168105=CARTESIAN_POINT('Ctrl Pts',(6.69796806999994,11.6,-9.21439937500002));
#168106=CARTESIAN_POINT('Ctrl Pts',(6.70118524799994,15.2,-9.21619090500002));
#168107=CARTESIAN_POINT('Ctrl Pts',(6.70118524799994,11.6,-9.21619090500002));
#168108=CARTESIAN_POINT('Ctrl Pts',(6.70440776799994,15.2,-9.21798216800001));
#168109=CARTESIAN_POINT('Ctrl Pts',(6.70440776799994,11.6,-9.21798216800001));
#168110=CARTESIAN_POINT('Ctrl Pts',(6.70763562499994,15.2,-9.21977315400002));
#168111=CARTESIAN_POINT('Ctrl Pts',(6.70763562499994,11.6,-9.21977315400002));
#168112=CARTESIAN_POINT('Ctrl Pts',(6.71086881499994,15.2,-9.22156385400001));
#168113=CARTESIAN_POINT('Ctrl Pts',(6.71086881499994,11.6,-9.22156385400001));
#168114=CARTESIAN_POINT('Ctrl Pts',(6.71410733699994,15.2,-9.22335426000001));
#168115=CARTESIAN_POINT('Ctrl Pts',(6.71410733699994,11.6,-9.22335426000001));
#168116=CARTESIAN_POINT('Ctrl Pts',(6.71735118499994,15.2,-9.22514436400002));
#168117=CARTESIAN_POINT('Ctrl Pts',(6.71735118499994,11.6,-9.22514436400002));
#168118=CARTESIAN_POINT('Ctrl Pts',(6.72060035499995,15.2,-9.22693415700002));
#168119=CARTESIAN_POINT('Ctrl Pts',(6.72060035499995,11.6,-9.22693415700002));
#168120=CARTESIAN_POINT('Ctrl Pts',(6.72385484599994,15.2,-9.22872363200002));
#168121=CARTESIAN_POINT('Ctrl Pts',(6.72385484599994,11.6,-9.22872363200002));
#168122=CARTESIAN_POINT('Ctrl Pts',(6.72711465299995,15.2,-9.23051277900001));
#168123=CARTESIAN_POINT('Ctrl Pts',(6.72711465299995,11.6,-9.23051277900001));
#168124=CARTESIAN_POINT('Ctrl Pts',(6.73037977199994,15.2,-9.23230159000001));
#168125=CARTESIAN_POINT('Ctrl Pts',(6.73037977199994,11.6,-9.23230159000001));
#168126=CARTESIAN_POINT('Ctrl Pts',(6.73365020099994,15.2,-9.23409005700002));
#168127=CARTESIAN_POINT('Ctrl Pts',(6.73365020099994,11.6,-9.23409005700002));
#168128=CARTESIAN_POINT('Ctrl Pts',(6.73692593399994,15.2,-9.23587817000002));
#168129=CARTESIAN_POINT('Ctrl Pts',(6.73692593399994,11.6,-9.23587817000002));
#168130=CARTESIAN_POINT('Ctrl Pts',(6.74020696799994,15.2,-9.23766592000002));
#168131=CARTESIAN_POINT('Ctrl Pts',(6.74020696799994,11.6,-9.23766592000002));
#168132=CARTESIAN_POINT('Ctrl Pts',(6.74349330199994,15.2,-9.23945330000001));
#168133=CARTESIAN_POINT('Ctrl Pts',(6.74349330199994,11.6,-9.23945330000001));
#168134=CARTESIAN_POINT('Ctrl Pts',(6.74678492799995,15.2,-9.24124030000002));
#168135=CARTESIAN_POINT('Ctrl Pts',(6.74678492799995,11.6,-9.24124030000002));
#168136=CARTESIAN_POINT('Ctrl Pts',(6.75008184499994,15.2,-9.24302691400002));
#168137=CARTESIAN_POINT('Ctrl Pts',(6.75008184499994,11.6,-9.24302691400002));
#168138=CARTESIAN_POINT('Ctrl Pts',(6.75338404999994,15.2,-9.24481313200002));
#168139=CARTESIAN_POINT('Ctrl Pts',(6.75338404999994,11.6,-9.24481313200002));
#168140=CARTESIAN_POINT('Ctrl Pts',(6.75669153899995,15.2,-9.24659894800002));
#168141=CARTESIAN_POINT('Ctrl Pts',(6.75669153899995,11.6,-9.24659894800002));
#168142=CARTESIAN_POINT('Ctrl Pts',(6.76000430999994,15.2,-9.24838435500002));
#168143=CARTESIAN_POINT('Ctrl Pts',(6.76000430999994,11.6,-9.24838435500002));
#168144=CARTESIAN_POINT('Ctrl Pts',(6.76332235699994,15.2,-9.25016934500002));
#168145=CARTESIAN_POINT('Ctrl Pts',(6.76332235699994,11.6,-9.25016934500002));
#168146=CARTESIAN_POINT('Ctrl Pts',(6.76664567999994,15.2,-9.25195390800001));
#168147=CARTESIAN_POINT('Ctrl Pts',(6.76664567999994,11.6,-9.25195390800001));
#168148=CARTESIAN_POINT('Ctrl Pts',(6.76997427099994,15.2,-9.25373803600002));
#168149=CARTESIAN_POINT('Ctrl Pts',(6.76997427099994,11.6,-9.25373803600002));
#168150=CARTESIAN_POINT('Ctrl Pts',(6.77330812799994,15.2,-9.25552171800001));
#168151=CARTESIAN_POINT('Ctrl Pts',(6.77330812799994,11.6,-9.25552171800001));
#168152=CARTESIAN_POINT('Ctrl Pts',(6.77664724599994,15.2,-9.25730494300002));
#168153=CARTESIAN_POINT('Ctrl Pts',(6.77664724599994,11.6,-9.25730494300002));
#168154=CARTESIAN_POINT('Ctrl Pts',(6.77999162099994,15.2,-9.25908770200002));
#168155=CARTESIAN_POINT('Ctrl Pts',(6.77999162099994,11.6,-9.25908770200002));
#168156=CARTESIAN_POINT('Ctrl Pts',(6.78334124799994,15.2,-9.26086998700002));
#168157=CARTESIAN_POINT('Ctrl Pts',(6.78334124799994,11.6,-9.26086998700002));
#168158=CARTESIAN_POINT('Ctrl Pts',(6.78669612399994,15.2,-9.26265178800002));
#168159=CARTESIAN_POINT('Ctrl Pts',(6.78669612399994,11.6,-9.26265178800002));
#168160=CARTESIAN_POINT('Ctrl Pts',(6.79005624699994,15.2,-9.26443310200002));
#168161=CARTESIAN_POINT('Ctrl Pts',(6.79005624699994,11.6,-9.26443310200002));
#168162=CARTESIAN_POINT('Ctrl Pts',(6.79342161599994,15.2,-9.26621392500002));
#168163=CARTESIAN_POINT('Ctrl Pts',(6.79342161599994,11.6,-9.26621392500002));
#168164=CARTESIAN_POINT('Ctrl Pts',(6.79679222899994,15.2,-9.26799425300001));
#168165=CARTESIAN_POINT('Ctrl Pts',(6.79679222899994,11.6,-9.26799425300001));
#168166=CARTESIAN_POINT('Ctrl Pts',(6.79949291499995,15.2,-9.26941812000001));
#168167=CARTESIAN_POINT('Ctrl Pts',(6.79949291499995,11.6,-9.26941812000001));
#168168=CARTESIAN_POINT('Ctrl Pts',(6.80152078799994,15.2,-9.27048579800001));
#168169=CARTESIAN_POINT('Ctrl Pts',(6.80152078799994,11.6,-9.27048579800001));
#168170=CARTESIAN_POINT('Ctrl Pts',(6.80287375199994,15.2,-9.27119748400001));
#168171=CARTESIAN_POINT('Ctrl Pts',(6.80287375199994,11.6,-9.27119748400001));
#168172=CARTESIAN_POINT('Ctrl Pts',(6.80355049599994,15.2,-9.27155330300002));
#168173=CARTESIAN_POINT('Ctrl Pts',(6.80355049599994,11.6,-9.27155330300002));
#168174=CARTESIAN_POINT('Ctrl Pts',(5.85257411399994,15.2,-8.56667970900002));
#168175=CARTESIAN_POINT('Ctrl Pts',(5.85268447799995,15.2,-8.56681469200002));
#168176=CARTESIAN_POINT('Ctrl Pts',(5.85290912899994,15.2,-8.56708931800001));
#168177=CARTESIAN_POINT('Ctrl Pts',(5.85324973299994,15.2,-8.56750527300001));
#168178=CARTESIAN_POINT('Ctrl Pts',(5.85370897399994,15.2,-8.56806526100002));
#168179=CARTESIAN_POINT('Ctrl Pts',(5.85429055399994,15.2,-8.56877298400001));
#168180=CARTESIAN_POINT('Ctrl Pts',(5.85488228099995,15.2,-8.56949158200001));
#168181=CARTESIAN_POINT('Ctrl Pts',(5.85548078499994,15.2,-8.57021692600001));
#168182=CARTESIAN_POINT('Ctrl Pts',(5.85608606099995,15.2,-8.57094898200002));
#168183=CARTESIAN_POINT('Ctrl Pts',(5.85669810699994,15.2,-8.57168771800002));
#168184=CARTESIAN_POINT('Ctrl Pts',(5.85731691799994,15.2,-8.57243310300002));
#168185=CARTESIAN_POINT('Ctrl Pts',(5.85794249299994,15.2,-8.57318510400002));
#168186=CARTESIAN_POINT('Ctrl Pts',(5.85857482799995,15.2,-8.57394368900002));
#168187=CARTESIAN_POINT('Ctrl Pts',(5.85921391899995,15.2,-8.57470882600002));
#168188=CARTESIAN_POINT('Ctrl Pts',(5.85985976499994,15.2,-8.57548048600002));
#168189=CARTESIAN_POINT('Ctrl Pts',(5.86051236099995,15.2,-8.57625863500001));
#168190=CARTESIAN_POINT('Ctrl Pts',(5.86117170399994,15.2,-8.57704324400002));
#168191=CARTESIAN_POINT('Ctrl Pts',(5.86183779199994,15.2,-8.57783428100002));
#168192=CARTESIAN_POINT('Ctrl Pts',(5.86251061899994,15.2,-8.57863171400002));
#168193=CARTESIAN_POINT('Ctrl Pts',(5.86319018499994,15.2,-8.57943551500002));
#168194=CARTESIAN_POINT('Ctrl Pts',(5.86387648599994,15.2,-8.58024565100001));
#168195=CARTESIAN_POINT('Ctrl Pts',(5.86456951799994,15.2,-8.58106209400002));
#168196=CARTESIAN_POINT('Ctrl Pts',(5.86526927899994,15.2,-8.58188481300001));
#168197=CARTESIAN_POINT('Ctrl Pts',(5.86597576599994,15.2,-8.58271377600002));
#168198=CARTESIAN_POINT('Ctrl Pts',(5.86668897299995,15.2,-8.58354895500002));
#168199=CARTESIAN_POINT('Ctrl Pts',(5.86740889999994,15.2,-8.58439031900001));
#168200=CARTESIAN_POINT('Ctrl Pts',(5.86813554199995,15.2,-8.58523784000001));
#168201=CARTESIAN_POINT('Ctrl Pts',(5.86886889699994,15.2,-8.58609148700002));
#168202=CARTESIAN_POINT('Ctrl Pts',(5.86960896099994,15.2,-8.58695123200001));
#168203=CARTESIAN_POINT('Ctrl Pts',(5.87035573299994,15.2,-8.58781704500002));
#168204=CARTESIAN_POINT('Ctrl Pts',(5.87110920599994,15.2,-8.58868889600001));
#168205=CARTESIAN_POINT('Ctrl Pts',(5.87186938099994,15.2,-8.58956675700002));
#168206=CARTESIAN_POINT('Ctrl Pts',(5.87263625099995,15.2,-8.59045059900001));
#168207=CARTESIAN_POINT('Ctrl Pts',(5.87340981499994,15.2,-8.59134039400002));
#168208=CARTESIAN_POINT('Ctrl Pts',(5.87419006999994,15.2,-8.59223611300001));
#168209=CARTESIAN_POINT('Ctrl Pts',(5.87497701299994,15.2,-8.59313772700002));
#168210=CARTESIAN_POINT('Ctrl Pts',(5.87577063899994,15.2,-8.59404520900002));
#168211=CARTESIAN_POINT('Ctrl Pts',(5.87657094599994,15.2,-8.59495852900002));
#168212=CARTESIAN_POINT('Ctrl Pts',(5.87737793199994,15.2,-8.59587766000002));
#168213=CARTESIAN_POINT('Ctrl Pts',(5.87819159199994,15.2,-8.59680257500001));
#168214=CARTESIAN_POINT('Ctrl Pts',(5.87901192399994,15.2,-8.59773324500001));
#168215=CARTESIAN_POINT('Ctrl Pts',(5.87983892499994,15.2,-8.59866964200002));
#168216=CARTESIAN_POINT('Ctrl Pts',(5.88067259099994,15.2,-8.59961174000002));
#168217=CARTESIAN_POINT('Ctrl Pts',(5.88151291899995,15.2,-8.60055951000002));
#168218=CARTESIAN_POINT('Ctrl Pts',(5.88235990599995,15.2,-8.60151292500002));
#168219=CARTESIAN_POINT('Ctrl Pts',(5.88321354999994,15.2,-8.60247195900002));
#168220=CARTESIAN_POINT('Ctrl Pts',(5.88407384499994,15.2,-8.60343658400001));
#168221=CARTESIAN_POINT('Ctrl Pts',(5.88494079099994,15.2,-8.60440677400002));
#168222=CARTESIAN_POINT('Ctrl Pts',(5.88581438299995,15.2,-8.60538250100002));
#168223=CARTESIAN_POINT('Ctrl Pts',(5.88669461899994,15.2,-8.60636373900002));
#168224=CARTESIAN_POINT('Ctrl Pts',(5.88758149499994,15.2,-8.60735046100002));
#168225=CARTESIAN_POINT('Ctrl Pts',(5.88847500799995,15.2,-8.60834264100001));
#168226=CARTESIAN_POINT('Ctrl Pts',(5.88937515499994,15.2,-8.60934025300002));
#168227=CARTESIAN_POINT('Ctrl Pts',(5.89028193299994,15.2,-8.61034327100001));
#168228=CARTESIAN_POINT('Ctrl Pts',(5.89119533899994,15.2,-8.61135166700001));
#168229=CARTESIAN_POINT('Ctrl Pts',(5.89211536799994,15.2,-8.61236541700002));
#168230=CARTESIAN_POINT('Ctrl Pts',(5.89304201999994,15.2,-8.61338449400002));
#168231=CARTESIAN_POINT('Ctrl Pts',(5.89397528899994,15.2,-8.61440887300001));
#168232=CARTESIAN_POINT('Ctrl Pts',(5.89491517399994,15.2,-8.61543852800001));
#168233=CARTESIAN_POINT('Ctrl Pts',(5.89586167099994,15.2,-8.61647343400002));
#168234=CARTESIAN_POINT('Ctrl Pts',(5.89681477699994,15.2,-8.61751356400001));
#168235=CARTESIAN_POINT('Ctrl Pts',(5.89777448799994,15.2,-8.61855889400001));
#168236=CARTESIAN_POINT('Ctrl Pts',(5.89874080199994,15.2,-8.61960939900002));
#168237=CARTESIAN_POINT('Ctrl Pts',(5.89971371499994,15.2,-8.62066505300002));
#168238=CARTESIAN_POINT('Ctrl Pts',(5.90069322499994,15.2,-8.62172583100002));
#168239=CARTESIAN_POINT('Ctrl Pts',(5.90167932799995,15.2,-8.62279170800001));
#168240=CARTESIAN_POINT('Ctrl Pts',(5.90267202099994,15.2,-8.62386266200001));
#168241=CARTESIAN_POINT('Ctrl Pts',(5.90367129999994,15.2,-8.62493866400002));
#168242=CARTESIAN_POINT('Ctrl Pts',(5.90467716299995,15.2,-8.62601969300002));
#168243=CARTESIAN_POINT('Ctrl Pts',(5.90568960799994,15.2,-8.62710572200001));
#168244=CARTESIAN_POINT('Ctrl Pts',(5.90670862899994,15.2,-8.62819672800001));
#168245=CARTESIAN_POINT('Ctrl Pts',(5.90773422399995,15.2,-8.62929268600002));
#168246=CARTESIAN_POINT('Ctrl Pts',(5.90876639199994,15.2,-8.63039357200002));
#168247=CARTESIAN_POINT('Ctrl Pts',(5.90980512599995,15.2,-8.63149936300001));
#168248=CARTESIAN_POINT('Ctrl Pts',(5.91085042599994,15.2,-8.63261003400002));
#168249=CARTESIAN_POINT('Ctrl Pts',(5.91190228799994,15.2,-8.63372556000002));
#168250=CARTESIAN_POINT('Ctrl Pts',(5.91296070699994,15.2,-8.63484591900002));
#168251=CARTESIAN_POINT('Ctrl Pts',(5.91402568199995,15.2,-8.63597108700001));
#168252=CARTESIAN_POINT('Ctrl Pts',(5.91509720999994,15.2,-8.63710104100001));
#168253=CARTESIAN_POINT('Ctrl Pts',(5.91617528699994,15.2,-8.63823575600002));
#168254=CARTESIAN_POINT('Ctrl Pts',(5.91725990899994,15.2,-8.63937520900001));
#168255=CARTESIAN_POINT('Ctrl Pts',(5.91835107499994,15.2,-8.64051937700001));
#168256=CARTESIAN_POINT('Ctrl Pts',(5.91944877999994,15.2,-8.64166823700002));
#168257=CARTESIAN_POINT('Ctrl Pts',(5.92055302199994,15.2,-8.64282176500001));
#168258=CARTESIAN_POINT('Ctrl Pts',(5.92166379799995,15.2,-8.64397994000001));
#168259=CARTESIAN_POINT('Ctrl Pts',(5.92278110299994,15.2,-8.64514273600001));
#168260=CARTESIAN_POINT('Ctrl Pts',(5.92390493499994,15.2,-8.64631013400002));
#168261=CARTESIAN_POINT('Ctrl Pts',(5.92503529199995,15.2,-8.64748210700002));
#168262=CARTESIAN_POINT('Ctrl Pts',(5.92617216899994,15.2,-8.64865863600001));
#168263=CARTESIAN_POINT('Ctrl Pts',(5.92731556399994,15.2,-8.64983969600001));
#168264=CARTESIAN_POINT('Ctrl Pts',(5.92846547399994,15.2,-8.65102526600002));
#168265=CARTESIAN_POINT('Ctrl Pts',(5.92962189399994,15.2,-8.65221532200002));
#168266=CARTESIAN_POINT('Ctrl Pts',(5.93078482299994,15.2,-8.65340984300002));
#168267=CARTESIAN_POINT('Ctrl Pts',(5.93195425599994,15.2,-8.65460880700001));
#168268=CARTESIAN_POINT('Ctrl Pts',(5.93313019299995,15.2,-8.65581219100001));
#168269=CARTESIAN_POINT('Ctrl Pts',(5.93431262699994,15.2,-8.65701997400001));
#168270=CARTESIAN_POINT('Ctrl Pts',(5.93550155699995,15.2,-8.65823213200001));
#168271=CARTESIAN_POINT('Ctrl Pts',(5.93669697899994,15.2,-8.65944864500002));
#168272=CARTESIAN_POINT('Ctrl Pts',(5.93789889099994,15.2,-8.66066949100002));
#168273=CARTESIAN_POINT('Ctrl Pts',(5.93910728799995,15.2,-8.66189464800001));
#168274=CARTESIAN_POINT('Ctrl Pts',(5.94032216899994,15.2,-8.66312409300001));
#168275=CARTESIAN_POINT('Ctrl Pts',(5.94154352899994,15.2,-8.66435780700002));
#168276=CARTESIAN_POINT('Ctrl Pts',(5.94277136499994,15.2,-8.66559576600002));
#168277=CARTESIAN_POINT('Ctrl Pts',(5.94400567599994,15.2,-8.66683795100002));
#168278=CARTESIAN_POINT('Ctrl Pts',(5.94524645699994,15.2,-8.66808434000001));
#168279=CARTESIAN_POINT('Ctrl Pts',(5.94649370399994,15.2,-8.66933491000001));
#168280=CARTESIAN_POINT('Ctrl Pts',(5.94774741599994,15.2,-8.67058964200002));
#168281=CARTESIAN_POINT('Ctrl Pts',(5.94900758799994,15.2,-8.67184851400001));
#168282=CARTESIAN_POINT('Ctrl Pts',(5.95027421799994,15.2,-8.67311150500001));
#168283=CARTESIAN_POINT('Ctrl Pts',(5.95154730199994,15.2,-8.67437859500002));
#168284=CARTESIAN_POINT('Ctrl Pts',(5.95282683699994,15.2,-8.67564976200002));
#168285=CARTESIAN_POINT('Ctrl Pts',(5.95411282099994,15.2,-8.67692498600002));
#168286=CARTESIAN_POINT('Ctrl Pts',(5.95540524899994,15.2,-8.67820424500002));
#168287=CARTESIAN_POINT('Ctrl Pts',(5.95670411999994,15.2,-8.67948752000002));
#168288=CARTESIAN_POINT('Ctrl Pts',(5.95800942899994,15.2,-8.68077479000002));
#168289=CARTESIAN_POINT('Ctrl Pts',(5.95932117299995,15.2,-8.68206603400001));
#168290=CARTESIAN_POINT('Ctrl Pts',(5.96063934899995,15.2,-8.68336123200002));
#168291=CARTESIAN_POINT('Ctrl Pts',(5.96196395499994,15.2,-8.68466036400001));
#168292=CARTESIAN_POINT('Ctrl Pts',(5.96329498499995,15.2,-8.68596340900002));
#168293=CARTESIAN_POINT('Ctrl Pts',(5.96463243999994,15.2,-8.68727034800001));
#168294=CARTESIAN_POINT('Ctrl Pts',(5.96597631299995,15.2,-8.68858116100002));
#168295=CARTESIAN_POINT('Ctrl Pts',(5.96732660299994,15.2,-8.68989582500001));
#168296=CARTESIAN_POINT('Ctrl Pts',(5.96868330599994,15.2,-8.69121432500001));
#168297=CARTESIAN_POINT('Ctrl Pts',(5.97004641899994,15.2,-8.69253663700002));
#168298=CARTESIAN_POINT('Ctrl Pts',(5.97141593799994,15.2,-8.69386274300001));
#168299=CARTESIAN_POINT('Ctrl Pts',(5.97279186099994,15.2,-8.69519262200001));
#168300=CARTESIAN_POINT('Ctrl Pts',(5.97417418499995,15.2,-8.69652625600001));
#168301=CARTESIAN_POINT('Ctrl Pts',(5.97556290599995,15.2,-8.69786362500001));
#168302=CARTESIAN_POINT('Ctrl Pts',(5.97695801999994,15.2,-8.69920470900002));
#168303=CARTESIAN_POINT('Ctrl Pts',(5.97835952599994,15.2,-8.70054948900002));
#168304=CARTESIAN_POINT('Ctrl Pts',(5.97976741899994,15.2,-8.70189794500002));
#168305=CARTESIAN_POINT('Ctrl Pts',(5.98118169699994,15.2,-8.70325005800002));
#168306=CARTESIAN_POINT('Ctrl Pts',(5.98260235599994,15.2,-8.70460581000001));
#168307=CARTESIAN_POINT('Ctrl Pts',(5.98402939199994,15.2,-8.70596518000001));
#168308=CARTESIAN_POINT('Ctrl Pts',(5.98546280499994,15.2,-8.70732814900002));
#168309=CARTESIAN_POINT('Ctrl Pts',(5.98690258799994,15.2,-8.70869469900001));
#168310=CARTESIAN_POINT('Ctrl Pts',(5.98834873999994,15.2,-8.71006481000002));
#168311=CARTESIAN_POINT('Ctrl Pts',(5.98980125799994,15.2,-8.71143846400001));
#168312=CARTESIAN_POINT('Ctrl Pts',(5.99126013699995,15.2,-8.71281564200002));
#168313=CARTESIAN_POINT('Ctrl Pts',(5.99272537499995,15.2,-8.71419632500002));
#168314=CARTESIAN_POINT('Ctrl Pts',(5.99419696899995,15.2,-8.71558049400001));
#168315=CARTESIAN_POINT('Ctrl Pts',(5.99567491499994,15.2,-8.71696813100002));
#168316=CARTESIAN_POINT('Ctrl Pts',(5.99715921199994,15.2,-8.71835921700002));
#168317=CARTESIAN_POINT('Ctrl Pts',(5.99864985299994,15.2,-8.71975373400002));
#168318=CARTESIAN_POINT('Ctrl Pts',(6.00014683699994,15.2,-8.72115166300001));
#168319=CARTESIAN_POINT('Ctrl Pts',(6.00165016199994,15.2,-8.72255298400002));
#168320=CARTESIAN_POINT('Ctrl Pts',(6.00315982299994,15.2,-8.72395768300001));
#168321=CARTESIAN_POINT('Ctrl Pts',(6.00467581699994,15.2,-8.72536573700001));
#168322=CARTESIAN_POINT('Ctrl Pts',(6.00619813999994,15.2,-8.72677713200002));
#168323=CARTESIAN_POINT('Ctrl Pts',(6.00772679099994,15.2,-8.72819184600001));
#168324=CARTESIAN_POINT('Ctrl Pts',(6.00926176599994,15.2,-8.72960986400001));
#168325=CARTESIAN_POINT('Ctrl Pts',(6.01080305999994,15.2,-8.73103116600002));
#168326=CARTESIAN_POINT('Ctrl Pts',(6.01235067299994,15.2,-8.73245573400002));
#168327=CARTESIAN_POINT('Ctrl Pts',(6.01390459799994,15.2,-8.73388355100002));
#168328=CARTESIAN_POINT('Ctrl Pts',(6.01546483399994,15.2,-8.73531460000001));
#168329=CARTESIAN_POINT('Ctrl Pts',(6.01703137899994,15.2,-8.73674886200002));
#168330=CARTESIAN_POINT('Ctrl Pts',(6.01860422799994,15.2,-8.73818631900001));
#168331=CARTESIAN_POINT('Ctrl Pts',(6.02018337599994,15.2,-8.73962695300002));
#168332=CARTESIAN_POINT('Ctrl Pts',(6.02176882399994,15.2,-8.74107074900002));
#168333=CARTESIAN_POINT('Ctrl Pts',(6.02336056599994,15.2,-8.74251768600002));
#168334=CARTESIAN_POINT('Ctrl Pts',(6.02495859899994,15.2,-8.74396774900001));
#168335=CARTESIAN_POINT('Ctrl Pts',(6.02656291999994,15.2,-8.74542091800001));
#168336=CARTESIAN_POINT('Ctrl Pts',(6.02817352699994,15.2,-8.74687718000001));
#168337=CARTESIAN_POINT('Ctrl Pts',(6.02979041499994,15.2,-8.74833651300002));
#168338=CARTESIAN_POINT('Ctrl Pts',(6.03141358199994,15.2,-8.74979890200001));
#168339=CARTESIAN_POINT('Ctrl Pts',(6.03304302299994,15.2,-8.75126433100002));
#168340=CARTESIAN_POINT('Ctrl Pts',(6.03467873699994,15.2,-8.75273277900002));
#168341=CARTESIAN_POINT('Ctrl Pts',(6.03632071899994,15.2,-8.75420423200002));
#168342=CARTESIAN_POINT('Ctrl Pts',(6.03796896799994,15.2,-8.75567867300001));
#168343=CARTESIAN_POINT('Ctrl Pts',(6.03962347799994,15.2,-8.75715608400002));
#168344=CARTESIAN_POINT('Ctrl Pts',(6.04128424699995,15.2,-8.75863644800001));
#168345=CARTESIAN_POINT('Ctrl Pts',(6.04295127299994,15.2,-8.76011974800001));
#168346=CARTESIAN_POINT('Ctrl Pts',(6.04462455099994,15.2,-8.76160596800002));
#168347=CARTESIAN_POINT('Ctrl Pts',(6.04630407799994,15.2,-8.76309509100002));
#168348=CARTESIAN_POINT('Ctrl Pts',(6.04798985099994,15.2,-8.76458710000002));
#168349=CARTESIAN_POINT('Ctrl Pts',(6.04968186699994,15.2,-8.76608197700002));
#168350=CARTESIAN_POINT('Ctrl Pts',(6.05138012199994,15.2,-8.76757970900002));
#168351=CARTESIAN_POINT('Ctrl Pts',(6.05308461499994,15.2,-8.76908027600001));
#168352=CARTESIAN_POINT('Ctrl Pts',(6.05479533999994,15.2,-8.77058366200002));
#168353=CARTESIAN_POINT('Ctrl Pts',(6.05651229499995,15.2,-8.77208985200001));
#168354=CARTESIAN_POINT('Ctrl Pts',(6.05823547599995,15.2,-8.77359882900001));
#168355=CARTESIAN_POINT('Ctrl Pts',(6.05996488099994,15.2,-8.77511057700002));
#168356=CARTESIAN_POINT('Ctrl Pts',(6.06170050599994,15.2,-8.77662507800002));
#168357=CARTESIAN_POINT('Ctrl Pts',(6.06344234899994,15.2,-8.77814231800001));
#168358=CARTESIAN_POINT('Ctrl Pts',(6.06519040399994,15.2,-8.77966227900002));
#168359=CARTESIAN_POINT('Ctrl Pts',(6.06694466899994,15.2,-8.78118494600002));
#168360=CARTESIAN_POINT('Ctrl Pts',(6.06870514199994,15.2,-8.78271030200001));
#168361=CARTESIAN_POINT('Ctrl Pts',(6.07047181899994,15.2,-8.78423833100002));
#168362=CARTESIAN_POINT('Ctrl Pts',(6.07224469599994,15.2,-8.78576901800002));
#168363=CARTESIAN_POINT('Ctrl Pts',(6.07402377099994,15.2,-8.78730234600001));
#168364=CARTESIAN_POINT('Ctrl Pts',(6.07580903899994,15.2,-8.78883830000002));
#168365=CARTESIAN_POINT('Ctrl Pts',(6.07760049799994,15.2,-8.79037686400002));
#168366=CARTESIAN_POINT('Ctrl Pts',(6.07939814499994,15.2,-8.79191802100001));
#168367=CARTESIAN_POINT('Ctrl Pts',(6.08120197499994,15.2,-8.79346175700002));
#168368=CARTESIAN_POINT('Ctrl Pts',(6.08301198699994,15.2,-8.79500805500001));
#168369=CARTESIAN_POINT('Ctrl Pts',(6.08482817699994,15.2,-8.79655689900002));
#168370=CARTESIAN_POINT('Ctrl Pts',(6.08665053999994,15.2,-8.79810827400001));
#168371=CARTESIAN_POINT('Ctrl Pts',(6.08847907499994,15.2,-8.79966216600002));
#168372=CARTESIAN_POINT('Ctrl Pts',(6.09031377799995,15.2,-8.80121855700001));
#168373=CARTESIAN_POINT('Ctrl Pts',(6.09215464499994,15.2,-8.80277743400002));
#168374=CARTESIAN_POINT('Ctrl Pts',(6.09400167399994,15.2,-8.80433877800002));
#168375=CARTESIAN_POINT('Ctrl Pts',(6.09585485999994,15.2,-8.80590257700002));
#168376=CARTESIAN_POINT('Ctrl Pts',(6.09771420199994,15.2,-8.80746881400002));
#168377=CARTESIAN_POINT('Ctrl Pts',(6.09957969399994,15.2,-8.80903747400002));
#168378=CARTESIAN_POINT('Ctrl Pts',(6.10145133499994,15.2,-8.81060854200001));
#168379=CARTESIAN_POINT('Ctrl Pts',(6.10332912099994,15.2,-8.81218200200001));
#168380=CARTESIAN_POINT('Ctrl Pts',(6.10521304799994,15.2,-8.81375784000002));
#168381=CARTESIAN_POINT('Ctrl Pts',(6.10710311299994,15.2,-8.81533604100002));
#168382=CARTESIAN_POINT('Ctrl Pts',(6.10899931399994,15.2,-8.81691658800002));
#168383=CARTESIAN_POINT('Ctrl Pts',(6.11090164599994,15.2,-8.81849946800001));
#168384=CARTESIAN_POINT('Ctrl Pts',(6.11281010699994,15.2,-8.82008466500002));
#168385=CARTESIAN_POINT('Ctrl Pts',(6.11472469299994,15.2,-8.82167216400001));
#168386=CARTESIAN_POINT('Ctrl Pts',(6.11664539999994,15.2,-8.82326195200001));
#168387=CARTESIAN_POINT('Ctrl Pts',(6.11857222599994,15.2,-8.82485401100002));
#168388=CARTESIAN_POINT('Ctrl Pts',(6.12050516699994,15.2,-8.82644832800001));
#168389=CARTESIAN_POINT('Ctrl Pts',(6.12244422199994,15.2,-8.82804488900002));
#168390=CARTESIAN_POINT('Ctrl Pts',(6.12438938299994,15.2,-8.82964367800002));
#168391=CARTESIAN_POINT('Ctrl Pts',(6.12634064999994,15.2,-8.83124468000002));
#168392=CARTESIAN_POINT('Ctrl Pts',(6.12829801999994,15.2,-8.83284788100001));
#168393=CARTESIAN_POINT('Ctrl Pts',(6.13026148799994,15.2,-8.83445326700001));
#168394=CARTESIAN_POINT('Ctrl Pts',(6.13223105199994,15.2,-8.83606082300001));
#168395=CARTESIAN_POINT('Ctrl Pts',(6.13420670699994,15.2,-8.83767053400002));
#168396=CARTESIAN_POINT('Ctrl Pts',(6.13618845099994,15.2,-8.83928238600001));
#168397=CARTESIAN_POINT('Ctrl Pts',(6.13817627999994,15.2,-8.84089636400001));
#168398=CARTESIAN_POINT('Ctrl Pts',(6.14017019199994,15.2,-8.84251245500002));
#168399=CARTESIAN_POINT('Ctrl Pts',(6.14217018299994,15.2,-8.84413064300002));
#168400=CARTESIAN_POINT('Ctrl Pts',(6.14417624999994,15.2,-8.84575091500002));
#168401=CARTESIAN_POINT('Ctrl Pts',(6.14618838899994,15.2,-8.84737325500002));
#168402=CARTESIAN_POINT('Ctrl Pts',(6.14820659699994,15.2,-8.84899765100002));
#168403=CARTESIAN_POINT('Ctrl Pts',(6.15023086899994,15.2,-8.85062408700002));
#168404=CARTESIAN_POINT('Ctrl Pts',(6.15226120499995,15.2,-8.85225255100002));
#168405=CARTESIAN_POINT('Ctrl Pts',(6.15429759899994,15.2,-8.85388302700001));
#168406=CARTESIAN_POINT('Ctrl Pts',(6.15634004999994,15.2,-8.85551550100002));
#168407=CARTESIAN_POINT('Ctrl Pts',(6.15838855099994,15.2,-8.85714995900001));
#168408=CARTESIAN_POINT('Ctrl Pts',(6.16044310199994,15.2,-8.85878638800002));
#168409=CARTESIAN_POINT('Ctrl Pts',(6.16250369999994,15.2,-8.86042477400002));
#168410=CARTESIAN_POINT('Ctrl Pts',(6.16457033899994,15.2,-8.86206510100001));
#168411=CARTESIAN_POINT('Ctrl Pts',(6.16664301799994,15.2,-8.86370735900002));
#168412=CARTESIAN_POINT('Ctrl Pts',(6.16872173199994,15.2,-8.86535153000001));
#168413=CARTESIAN_POINT('Ctrl Pts',(6.17080647799994,15.2,-8.86699760300001));
#168414=CARTESIAN_POINT('Ctrl Pts',(6.17289725299995,15.2,-8.86864556300001));
#168415=CARTESIAN_POINT('Ctrl Pts',(6.17499405399994,15.2,-8.87029539700002));
#168416=CARTESIAN_POINT('Ctrl Pts',(6.17709687799994,15.2,-8.87194709200001));
#168417=CARTESIAN_POINT('Ctrl Pts',(6.17920571999994,15.2,-8.87360063200001));
#168418=CARTESIAN_POINT('Ctrl Pts',(6.18132057899994,15.2,-8.87525600500001));
#168419=CARTESIAN_POINT('Ctrl Pts',(6.18344144899994,15.2,-8.87691319600002));
#168420=CARTESIAN_POINT('Ctrl Pts',(6.18556832799994,15.2,-8.87857219500002));
#168421=CARTESIAN_POINT('Ctrl Pts',(6.18770121399994,15.2,-8.88023298500002));
#168422=CARTESIAN_POINT('Ctrl Pts',(6.18984009999994,15.2,-8.88189555400002));
#168423=CARTESIAN_POINT('Ctrl Pts',(6.19198498599994,15.2,-8.88355988700001));
#168424=CARTESIAN_POINT('Ctrl Pts',(6.19413586799994,15.2,-8.88522597300001));
#168425=CARTESIAN_POINT('Ctrl Pts',(6.19629274299994,15.2,-8.88689379800002));
#168426=CARTESIAN_POINT('Ctrl Pts',(6.19845560599994,15.2,-8.88856334700002));
#168427=CARTESIAN_POINT('Ctrl Pts',(6.20062445399994,15.2,-8.89023460900002));
#168428=CARTESIAN_POINT('Ctrl Pts',(6.20279928499994,15.2,-8.89190757000001));
#168429=CARTESIAN_POINT('Ctrl Pts',(6.20498009499994,15.2,-8.89358221500002));
#168430=CARTESIAN_POINT('Ctrl Pts',(6.20716688099994,15.2,-8.89525853400002));
#168431=CARTESIAN_POINT('Ctrl Pts',(6.20935963799995,15.2,-8.89693651100002));
#168432=CARTESIAN_POINT('Ctrl Pts',(6.21155836399994,15.2,-8.89861613500001));
#168433=CARTESIAN_POINT('Ctrl Pts',(6.21376305499994,15.2,-8.90029739200001));
#168434=CARTESIAN_POINT('Ctrl Pts',(6.21597370899994,15.2,-8.90198026900002));
#168435=CARTESIAN_POINT('Ctrl Pts',(6.21819032199994,15.2,-8.90366475300001));
#168436=CARTESIAN_POINT('Ctrl Pts',(6.22041288899994,15.2,-8.90535083100002));
#168437=CARTESIAN_POINT('Ctrl Pts',(6.22264140799994,15.2,-8.90703849100002));
#168438=CARTESIAN_POINT('Ctrl Pts',(6.22487587699994,15.2,-8.90872771900002));
#168439=CARTESIAN_POINT('Ctrl Pts',(6.22711629099994,15.2,-8.91041850200001));
#168440=CARTESIAN_POINT('Ctrl Pts',(6.22936264599994,15.2,-8.91211082700002));
#168441=CARTESIAN_POINT('Ctrl Pts',(6.23161493899994,15.2,-8.91380468300002));
#168442=CARTESIAN_POINT('Ctrl Pts',(6.23387316899994,15.2,-8.91550005600001));
#168443=CARTESIAN_POINT('Ctrl Pts',(6.23613732999994,15.2,-8.91719693300002));
#168444=CARTESIAN_POINT('Ctrl Pts',(6.23840741799994,15.2,-8.91889530200002));
#168445=CARTESIAN_POINT('Ctrl Pts',(6.24068343299994,15.2,-8.92059515000001));
#168446=CARTESIAN_POINT('Ctrl Pts',(6.24296536899994,15.2,-8.92229646500001));
#168447=CARTESIAN_POINT('Ctrl Pts',(6.24525322299994,15.2,-8.92399923300001));
#168448=CARTESIAN_POINT('Ctrl Pts',(6.24754699199994,15.2,-8.92570344200001));
#168449=CARTESIAN_POINT('Ctrl Pts',(6.24984667299994,15.2,-8.92740908100001));
#168450=CARTESIAN_POINT('Ctrl Pts',(6.25215226099994,15.2,-8.92911613600001));
#168451=CARTESIAN_POINT('Ctrl Pts',(6.25446375499994,15.2,-8.93082459400001));
#168452=CARTESIAN_POINT('Ctrl Pts',(6.25678114899994,15.2,-8.93253444400001));
#168453=CARTESIAN_POINT('Ctrl Pts',(6.25910444299994,15.2,-8.93424567300002));
#168454=CARTESIAN_POINT('Ctrl Pts',(6.26143362999994,15.2,-8.93595826800002));
#168455=CARTESIAN_POINT('Ctrl Pts',(6.26376870799994,15.2,-8.93767221800001));
#168456=CARTESIAN_POINT('Ctrl Pts',(6.26610967499994,15.2,-8.93938751000002));
#168457=CARTESIAN_POINT('Ctrl Pts',(6.26845652499994,15.2,-8.94110413200002));
#168458=CARTESIAN_POINT('Ctrl Pts',(6.27080925699994,15.2,-8.94282207100002));
#168459=CARTESIAN_POINT('Ctrl Pts',(6.27316786699994,15.2,-8.94454131600002));
#168460=CARTESIAN_POINT('Ctrl Pts',(6.27553235099994,15.2,-8.94626185400002));
#168461=CARTESIAN_POINT('Ctrl Pts',(6.27790270499994,15.2,-8.94798367200002));
#168462=CARTESIAN_POINT('Ctrl Pts',(6.28027892799994,15.2,-8.94970676000002));
#168463=CARTESIAN_POINT('Ctrl Pts',(6.28266101299994,15.2,-8.95143110400002));
#168464=CARTESIAN_POINT('Ctrl Pts',(6.28504895899994,15.2,-8.95315669400001));
#168465=CARTESIAN_POINT('Ctrl Pts',(6.28744276399994,15.2,-8.95488351500001));
#168466=CARTESIAN_POINT('Ctrl Pts',(6.28984242199994,15.2,-8.95661155900001));
#168467=CARTESIAN_POINT('Ctrl Pts',(6.29224792999994,15.2,-8.95834081000002));
#168468=CARTESIAN_POINT('Ctrl Pts',(6.29465928599994,15.2,-8.96007125900002));
#168469=CARTESIAN_POINT('Ctrl Pts',(6.29707648499994,15.2,-8.96180289200002));
#168470=CARTESIAN_POINT('Ctrl Pts',(6.29949952399994,15.2,-8.96353569800001));
#168471=CARTESIAN_POINT('Ctrl Pts',(6.30192839999994,15.2,-8.96526966600002));
#168472=CARTESIAN_POINT('Ctrl Pts',(6.30436310999994,15.2,-8.96700478300002));
#168473=CARTESIAN_POINT('Ctrl Pts',(6.30680364899994,15.2,-8.96874103900002));
#168474=CARTESIAN_POINT('Ctrl Pts',(6.30925001499994,15.2,-8.97047842000001));
#168475=CARTESIAN_POINT('Ctrl Pts',(6.31170220399994,15.2,-8.97221691500001));
#168476=CARTESIAN_POINT('Ctrl Pts',(6.31416021399994,15.2,-8.97395651300002));
#168477=CARTESIAN_POINT('Ctrl Pts',(6.31662403899994,15.2,-8.97569720100002));
#168478=CARTESIAN_POINT('Ctrl Pts',(6.31909367699994,15.2,-8.97743896900002));
#168479=CARTESIAN_POINT('Ctrl Pts',(6.32156912499994,15.2,-8.97918180400002));
#168480=CARTESIAN_POINT('Ctrl Pts',(6.32405037899994,15.2,-8.98092569600001));
#168481=CARTESIAN_POINT('Ctrl Pts',(6.32653743599994,15.2,-8.98267063100001));
#168482=CARTESIAN_POINT('Ctrl Pts',(6.32903029199994,15.2,-8.98441660100002));
#168483=CARTESIAN_POINT('Ctrl Pts',(6.33152894299994,15.2,-8.98616359100001));
#168484=CARTESIAN_POINT('Ctrl Pts',(6.33403338799994,15.2,-8.98791159100002));
#168485=CARTESIAN_POINT('Ctrl Pts',(6.33654362099994,15.2,-8.98966059000001));
#168486=CARTESIAN_POINT('Ctrl Pts',(6.33905963999994,15.2,-8.99141057600002));
#168487=CARTESIAN_POINT('Ctrl Pts',(6.34158143999994,15.2,-8.99316153900001));
#168488=CARTESIAN_POINT('Ctrl Pts',(6.34410901999994,15.2,-8.99491346500002));
#168489=CARTESIAN_POINT('Ctrl Pts',(6.34664237499994,15.2,-8.99666634500001));
#168490=CARTESIAN_POINT('Ctrl Pts',(6.34918150099994,15.2,-8.99842016600001));
#168491=CARTESIAN_POINT('Ctrl Pts',(6.35172639699994,15.2,-9.00017491800002));
#168492=CARTESIAN_POINT('Ctrl Pts',(6.35427705599994,15.2,-9.00193058900001));
#168493=CARTESIAN_POINT('Ctrl Pts',(6.35683347799994,15.2,-9.00368716800001));
#168494=CARTESIAN_POINT('Ctrl Pts',(6.35939565699994,15.2,-9.00544464400001));
#168495=CARTESIAN_POINT('Ctrl Pts',(6.36196359199994,15.2,-9.00720300600002));
#168496=CARTESIAN_POINT('Ctrl Pts',(6.36453727799994,15.2,-9.00896224300002));
#168497=CARTESIAN_POINT('Ctrl Pts',(6.36711671099994,15.2,-9.01072234300001));
#168498=CARTESIAN_POINT('Ctrl Pts',(6.36970188799994,15.2,-9.01248329400002));
#168499=CARTESIAN_POINT('Ctrl Pts',(6.37229280699994,15.2,-9.01424508800002));
#168500=CARTESIAN_POINT('Ctrl Pts',(6.37488946299994,15.2,-9.01600771300001));
#168501=CARTESIAN_POINT('Ctrl Pts',(6.37749185299994,15.2,-9.01777115600002));
#168502=CARTESIAN_POINT('Ctrl Pts',(6.38009997299994,15.2,-9.01953540700001));
#168503=CARTESIAN_POINT('Ctrl Pts',(6.38271382099994,15.2,-9.02130045600002));
#168504=CARTESIAN_POINT('Ctrl Pts',(6.38533339199994,15.2,-9.02306629200002));
#168505=CARTESIAN_POINT('Ctrl Pts',(6.38795868399994,15.2,-9.02483290300001));
#168506=CARTESIAN_POINT('Ctrl Pts',(6.39058969199994,15.2,-9.02660027900002));
#168507=CARTESIAN_POINT('Ctrl Pts',(6.39322641399994,15.2,-9.02836840800001));
#168508=CARTESIAN_POINT('Ctrl Pts',(6.39586884499994,15.2,-9.03013728200002));
#168509=CARTESIAN_POINT('Ctrl Pts',(6.39851698299994,15.2,-9.03190688700001));
#168510=CARTESIAN_POINT('Ctrl Pts',(6.40117082299994,15.2,-9.03367721300001));
#168511=CARTESIAN_POINT('Ctrl Pts',(6.40383036299994,15.2,-9.03544825000001));
#168512=CARTESIAN_POINT('Ctrl Pts',(6.40649559999994,15.2,-9.03721998700002));
#168513=CARTESIAN_POINT('Ctrl Pts',(6.40916652899994,15.2,-9.03899241300002));
#168514=CARTESIAN_POINT('Ctrl Pts',(6.41184314599994,15.2,-9.04076551800001));
#168515=CARTESIAN_POINT('Ctrl Pts',(6.41452544999994,15.2,-9.04253929100001));
#168516=CARTESIAN_POINT('Ctrl Pts',(6.41721343599994,15.2,-9.04431372100002));
#168517=CARTESIAN_POINT('Ctrl Pts',(6.41990709999994,15.2,-9.04608879800002));
#168518=CARTESIAN_POINT('Ctrl Pts',(6.42260643999994,15.2,-9.04786451100002));
#168519=CARTESIAN_POINT('Ctrl Pts',(6.42531145199994,15.2,-9.04964084900002));
#168520=CARTESIAN_POINT('Ctrl Pts',(6.42802213199994,15.2,-9.05141780400001));
#168521=CARTESIAN_POINT('Ctrl Pts',(6.43073847599994,15.2,-9.05319536200002));
#168522=CARTESIAN_POINT('Ctrl Pts',(6.43346048199994,15.2,-9.05497351500001));
#168523=CARTESIAN_POINT('Ctrl Pts',(6.43618814599995,15.2,-9.05675225100002));
#168524=CARTESIAN_POINT('Ctrl Pts',(6.43892146399994,15.2,-9.05853156000001));
#168525=CARTESIAN_POINT('Ctrl Pts',(6.44166043299994,15.2,-9.06031143300002));
#168526=CARTESIAN_POINT('Ctrl Pts',(6.44440504999994,15.2,-9.06209185800002));
#168527=CARTESIAN_POINT('Ctrl Pts',(6.44715531099994,15.2,-9.06387282500001));
#168528=CARTESIAN_POINT('Ctrl Pts',(6.44991121199994,15.2,-9.06565432300001));
#168529=CARTESIAN_POINT('Ctrl Pts',(6.45267274999994,15.2,-9.06743634400001));
#168530=CARTESIAN_POINT('Ctrl Pts',(6.45543992299994,15.2,-9.06921887500001));
#168531=CARTESIAN_POINT('Ctrl Pts',(6.45821272399994,15.2,-9.07100190800002));
#168532=CARTESIAN_POINT('Ctrl Pts',(6.46099115299994,15.2,-9.07278543100002));
#168533=CARTESIAN_POINT('Ctrl Pts',(6.46377520499994,15.2,-9.07456943400001));
#168534=CARTESIAN_POINT('Ctrl Pts',(6.46656487599994,15.2,-9.07635390800002));
#168535=CARTESIAN_POINT('Ctrl Pts',(6.46936016299994,15.2,-9.07813884200002));
#168536=CARTESIAN_POINT('Ctrl Pts',(6.47216106399994,15.2,-9.07992422500002));
#168537=CARTESIAN_POINT('Ctrl Pts',(6.47496757199994,15.2,-9.08171004900002));
#168538=CARTESIAN_POINT('Ctrl Pts',(6.47777968799994,15.2,-9.08349630400001));
#168539=CARTESIAN_POINT('Ctrl Pts',(6.48059740499994,15.2,-9.08528297600002));
#168540=CARTESIAN_POINT('Ctrl Pts',(6.48342072099994,15.2,-9.08707005900002));
#168541=CARTESIAN_POINT('Ctrl Pts',(6.48624963199994,15.2,-9.08885754100002));
#168542=CARTESIAN_POINT('Ctrl Pts',(6.48908413499994,15.2,-9.09064541400002));
#168543=CARTESIAN_POINT('Ctrl Pts',(6.49192422599994,15.2,-9.09243366500002));
#168544=CARTESIAN_POINT('Ctrl Pts',(6.49476990199994,15.2,-9.09422228700001));
#168545=CARTESIAN_POINT('Ctrl Pts',(6.49762115899994,15.2,-9.09601126700002));
#168546=CARTESIAN_POINT('Ctrl Pts',(6.50047799399994,15.2,-9.09780059800001));
#168547=CARTESIAN_POINT('Ctrl Pts',(6.50334040299994,15.2,-9.09959026900001));
#168548=CARTESIAN_POINT('Ctrl Pts',(6.50620838199995,15.2,-9.10138026900002));
#168549=CARTESIAN_POINT('Ctrl Pts',(6.50908192999994,15.2,-9.10317059000001));
#168550=CARTESIAN_POINT('Ctrl Pts',(6.51196104099995,15.2,-9.10496122100002));
#168551=CARTESIAN_POINT('Ctrl Pts',(6.51484571099994,15.2,-9.10675215300002));
#168552=CARTESIAN_POINT('Ctrl Pts',(6.51773593899994,15.2,-9.10854337500002));
#168553=CARTESIAN_POINT('Ctrl Pts',(6.52063172099994,15.2,-9.11033487800001));
#168554=CARTESIAN_POINT('Ctrl Pts',(6.52353305099994,15.2,-9.11212665200001));
#168555=CARTESIAN_POINT('Ctrl Pts',(6.52643992799994,15.2,-9.11391868900001));
#168556=CARTESIAN_POINT('Ctrl Pts',(6.52935234699994,15.2,-9.11571097500002));
#168557=CARTESIAN_POINT('Ctrl Pts',(6.53227030599994,15.2,-9.11750350600002));
#168558=CARTESIAN_POINT('Ctrl Pts',(6.53519379999994,15.2,-9.11929626800001));
#168559=CARTESIAN_POINT('Ctrl Pts',(6.53812282699994,15.2,-9.12108925300002));
#168560=CARTESIAN_POINT('Ctrl Pts',(6.54105738299994,15.2,-9.12288245200001));
#168561=CARTESIAN_POINT('Ctrl Pts',(6.54399746299994,15.2,-9.12467585300002));
#168562=CARTESIAN_POINT('Ctrl Pts',(6.54694306499994,15.2,-9.12646944900001));
#168563=CARTESIAN_POINT('Ctrl Pts',(6.54989418399994,15.2,-9.12826322900001));
#168564=CARTESIAN_POINT('Ctrl Pts',(6.55285081899994,15.2,-9.13005718400001));
#168565=CARTESIAN_POINT('Ctrl Pts',(6.55581296599994,15.2,-9.13185130500001));
#168566=CARTESIAN_POINT('Ctrl Pts',(6.55878061899994,15.2,-9.13364558100002));
#168567=CARTESIAN_POINT('Ctrl Pts',(6.56175377599994,15.2,-9.13544000400002));
#168568=CARTESIAN_POINT('Ctrl Pts',(6.56473243399994,15.2,-9.13723456500002));
#168569=CARTESIAN_POINT('Ctrl Pts',(6.56771658899994,15.2,-9.13902925200002));
#168570=CARTESIAN_POINT('Ctrl Pts',(6.57070623699994,15.2,-9.14082405700002));
#168571=CARTESIAN_POINT('Ctrl Pts',(6.57370137599994,15.2,-9.14261897200002));
#168572=CARTESIAN_POINT('Ctrl Pts',(6.57670199999994,15.2,-9.14441398600001));
#168573=CARTESIAN_POINT('Ctrl Pts',(6.57970810799994,15.2,-9.14620908900002));
#168574=CARTESIAN_POINT('Ctrl Pts',(6.58271969499994,15.2,-9.14800427400002));
#168575=CARTESIAN_POINT('Ctrl Pts',(6.58573675799994,15.2,-9.14979953100002));
#168576=CARTESIAN_POINT('Ctrl Pts',(6.58875929299994,15.2,-9.15159484900002));
#168577=CARTESIAN_POINT('Ctrl Pts',(6.59178729699994,15.2,-9.15339022000002));
#168578=CARTESIAN_POINT('Ctrl Pts',(6.59482076499994,15.2,-9.15518563400001));
#168579=CARTESIAN_POINT('Ctrl Pts',(6.59785969599994,15.2,-9.15698108300001));
#168580=CARTESIAN_POINT('Ctrl Pts',(6.60090408599994,15.2,-9.15877655700001));
#168581=CARTESIAN_POINT('Ctrl Pts',(6.60395392899995,15.2,-9.16057204700002));
#168582=CARTESIAN_POINT('Ctrl Pts',(6.60700922399994,15.2,-9.16236754400002));
#168583=CARTESIAN_POINT('Ctrl Pts',(6.61006996599995,15.2,-9.16416303900002));
#168584=CARTESIAN_POINT('Ctrl Pts',(6.61313615199994,15.2,-9.16595852100002));
#168585=CARTESIAN_POINT('Ctrl Pts',(6.61620777899994,15.2,-9.16775398400001));
#168586=CARTESIAN_POINT('Ctrl Pts',(6.61928484299994,15.2,-9.16954941700002));
#168587=CARTESIAN_POINT('Ctrl Pts',(6.62236733999994,15.2,-9.17134481100002));
#168588=CARTESIAN_POINT('Ctrl Pts',(6.62545526699994,15.2,-9.17314015600001));
#168589=CARTESIAN_POINT('Ctrl Pts',(6.62854862099994,15.2,-9.17493544700001));
#168590=CARTESIAN_POINT('Ctrl Pts',(6.63164739699994,15.2,-9.17673067000001));
#168591=CARTESIAN_POINT('Ctrl Pts',(6.63475159199994,15.2,-9.17852581800001));
#168592=CARTESIAN_POINT('Ctrl Pts',(6.63786120299994,15.2,-9.18032088200002));
#168593=CARTESIAN_POINT('Ctrl Pts',(6.64097622599994,15.2,-9.18211585500002));
#168594=CARTESIAN_POINT('Ctrl Pts',(6.64409665799995,15.2,-9.18391072500001));
#168595=CARTESIAN_POINT('Ctrl Pts',(6.64722249499994,15.2,-9.18570548400002));
#168596=CARTESIAN_POINT('Ctrl Pts',(6.65035373299995,15.2,-9.18750012300002));
#168597=CARTESIAN_POINT('Ctrl Pts',(6.65349036899994,15.2,-9.18929463500002));
#168598=CARTESIAN_POINT('Ctrl Pts',(6.65663239999994,15.2,-9.19108900900002));
#168599=CARTESIAN_POINT('Ctrl Pts',(6.65977982099994,15.2,-9.19288323700002));
#168600=CARTESIAN_POINT('Ctrl Pts',(6.66293262999995,15.2,-9.19467731100001));
#168601=CARTESIAN_POINT('Ctrl Pts',(6.66609082299995,15.2,-9.19647121900002));
#168602=CARTESIAN_POINT('Ctrl Pts',(6.66925439499994,15.2,-9.19826495600002));
#168603=CARTESIAN_POINT('Ctrl Pts',(6.67242334399995,15.2,-9.20005851000001));
#168604=CARTESIAN_POINT('Ctrl Pts',(6.67559766699994,15.2,-9.20185187500002));
#168605=CARTESIAN_POINT('Ctrl Pts',(6.67877735899994,15.2,-9.20364504200002));
#168606=CARTESIAN_POINT('Ctrl Pts',(6.68196241599994,15.2,-9.20543800000001));
#168607=CARTESIAN_POINT('Ctrl Pts',(6.68515283699994,15.2,-9.20723074200002));
#168608=CARTESIAN_POINT('Ctrl Pts',(6.68834861499994,15.2,-9.20902325900002));
#168609=CARTESIAN_POINT('Ctrl Pts',(6.69154974999994,15.2,-9.21081554300001));
#168610=CARTESIAN_POINT('Ctrl Pts',(6.69475623599994,15.2,-9.21260758400001));
#168611=CARTESIAN_POINT('Ctrl Pts',(6.69796806999994,15.2,-9.21439937500002));
#168612=CARTESIAN_POINT('Ctrl Pts',(6.70118524799994,15.2,-9.21619090500002));
#168613=CARTESIAN_POINT('Ctrl Pts',(6.70440776799994,15.2,-9.21798216800001));
#168614=CARTESIAN_POINT('Ctrl Pts',(6.70763562499994,15.2,-9.21977315400002));
#168615=CARTESIAN_POINT('Ctrl Pts',(6.71086881499994,15.2,-9.22156385400001));
#168616=CARTESIAN_POINT('Ctrl Pts',(6.71410733699994,15.2,-9.22335426000001));
#168617=CARTESIAN_POINT('Ctrl Pts',(6.71735118499994,15.2,-9.22514436400002));
#168618=CARTESIAN_POINT('Ctrl Pts',(6.72060035499995,15.2,-9.22693415700002));
#168619=CARTESIAN_POINT('Ctrl Pts',(6.72385484599994,15.2,-9.22872363200002));
#168620=CARTESIAN_POINT('Ctrl Pts',(6.72711465299995,15.2,-9.23051277900001));
#168621=CARTESIAN_POINT('Ctrl Pts',(6.73037977199994,15.2,-9.23230159000001));
#168622=CARTESIAN_POINT('Ctrl Pts',(6.73365020099994,15.2,-9.23409005700002));
#168623=CARTESIAN_POINT('Ctrl Pts',(6.73692593399994,15.2,-9.23587817000002));
#168624=CARTESIAN_POINT('Ctrl Pts',(6.74020696799994,15.2,-9.23766592000002));
#168625=CARTESIAN_POINT('Ctrl Pts',(6.74349330199994,15.2,-9.23945330000001));
#168626=CARTESIAN_POINT('Ctrl Pts',(6.74678492799995,15.2,-9.24124030000002));
#168627=CARTESIAN_POINT('Ctrl Pts',(6.75008184499994,15.2,-9.24302691400002));
#168628=CARTESIAN_POINT('Ctrl Pts',(6.75338404999994,15.2,-9.24481313200002));
#168629=CARTESIAN_POINT('Ctrl Pts',(6.75669153899995,15.2,-9.24659894800002));
#168630=CARTESIAN_POINT('Ctrl Pts',(6.76000430999994,15.2,-9.24838435500002));
#168631=CARTESIAN_POINT('Ctrl Pts',(6.76332235699994,15.2,-9.25016934500002));
#168632=CARTESIAN_POINT('Ctrl Pts',(6.76664567999994,15.2,-9.25195390800001));
#168633=CARTESIAN_POINT('Ctrl Pts',(6.76997427099994,15.2,-9.25373803600002));
#168634=CARTESIAN_POINT('Ctrl Pts',(6.77330812799994,15.2,-9.25552171800001));
#168635=CARTESIAN_POINT('Ctrl Pts',(6.77664724599994,15.2,-9.25730494300002));
#168636=CARTESIAN_POINT('Ctrl Pts',(6.77999162099994,15.2,-9.25908770200002));
#168637=CARTESIAN_POINT('Ctrl Pts',(6.78334124799994,15.2,-9.26086998700002));
#168638=CARTESIAN_POINT('Ctrl Pts',(6.78669612399994,15.2,-9.26265178800002));
#168639=CARTESIAN_POINT('Ctrl Pts',(6.79005624699994,15.2,-9.26443310200002));
#168640=CARTESIAN_POINT('Ctrl Pts',(6.79342161599994,15.2,-9.26621392500002));
#168641=CARTESIAN_POINT('Ctrl Pts',(6.79679222899994,15.2,-9.26799425300001));
#168642=CARTESIAN_POINT('Ctrl Pts',(6.79949291499995,15.2,-9.26941812000001));
#168643=CARTESIAN_POINT('Ctrl Pts',(6.80152078799994,15.2,-9.27048579800001));
#168644=CARTESIAN_POINT('Ctrl Pts',(6.80287375199994,15.2,-9.27119748400001));
#168645=CARTESIAN_POINT('Ctrl Pts',(6.80355049599994,15.2,-9.27155330300002));
#168646=CARTESIAN_POINT('Ctrl Pts',(5.85257411399994,12.2,-8.56667970900002));
#168647=CARTESIAN_POINT('Ctrl Pts',(5.85268447799995,12.2,-8.56681469200002));
#168648=CARTESIAN_POINT('Ctrl Pts',(5.85290912899994,12.2,-8.56708931800001));
#168649=CARTESIAN_POINT('Ctrl Pts',(5.85324973299994,12.2,-8.56750527300001));
#168650=CARTESIAN_POINT('Ctrl Pts',(5.85370897399994,12.2,-8.56806526100002));
#168651=CARTESIAN_POINT('Ctrl Pts',(5.85429055399994,12.2,-8.56877298400001));
#168652=CARTESIAN_POINT('Ctrl Pts',(5.85488228099995,12.2,-8.56949158200001));
#168653=CARTESIAN_POINT('Ctrl Pts',(5.85548078499994,12.2,-8.57021692600001));
#168654=CARTESIAN_POINT('Ctrl Pts',(5.85608606099995,12.2,-8.57094898200002));
#168655=CARTESIAN_POINT('Ctrl Pts',(5.85669810699994,12.2,-8.57168771800002));
#168656=CARTESIAN_POINT('Ctrl Pts',(5.85731691799994,12.2,-8.57243310300002));
#168657=CARTESIAN_POINT('Ctrl Pts',(5.85794249299994,12.2,-8.57318510400002));
#168658=CARTESIAN_POINT('Ctrl Pts',(5.85857482799995,12.2,-8.57394368900002));
#168659=CARTESIAN_POINT('Ctrl Pts',(5.85921391899995,12.2,-8.57470882600002));
#168660=CARTESIAN_POINT('Ctrl Pts',(5.85985976499994,12.2,-8.57548048600002));
#168661=CARTESIAN_POINT('Ctrl Pts',(5.86051236099995,12.2,-8.57625863500001));
#168662=CARTESIAN_POINT('Ctrl Pts',(5.86117170399994,12.2,-8.57704324400002));
#168663=CARTESIAN_POINT('Ctrl Pts',(5.86183779199994,12.2,-8.57783428100002));
#168664=CARTESIAN_POINT('Ctrl Pts',(5.86251061899994,12.2,-8.57863171400002));
#168665=CARTESIAN_POINT('Ctrl Pts',(5.86319018499994,12.2,-8.57943551500002));
#168666=CARTESIAN_POINT('Ctrl Pts',(5.86387648599994,12.2,-8.58024565100001));
#168667=CARTESIAN_POINT('Ctrl Pts',(5.86456951799994,12.2,-8.58106209400002));
#168668=CARTESIAN_POINT('Ctrl Pts',(5.86526927899994,12.2,-8.58188481300001));
#168669=CARTESIAN_POINT('Ctrl Pts',(5.86597576599994,12.2,-8.58271377600002));
#168670=CARTESIAN_POINT('Ctrl Pts',(5.86668897299995,12.2,-8.58354895500002));
#168671=CARTESIAN_POINT('Ctrl Pts',(5.86740889999994,12.2,-8.58439031900001));
#168672=CARTESIAN_POINT('Ctrl Pts',(5.86813554199995,12.2,-8.58523784000001));
#168673=CARTESIAN_POINT('Ctrl Pts',(5.86886889699994,12.2,-8.58609148700002));
#168674=CARTESIAN_POINT('Ctrl Pts',(5.86960896099994,12.2,-8.58695123200001));
#168675=CARTESIAN_POINT('Ctrl Pts',(5.87035573299994,12.2,-8.58781704500002));
#168676=CARTESIAN_POINT('Ctrl Pts',(5.87110920599994,12.2,-8.58868889600001));
#168677=CARTESIAN_POINT('Ctrl Pts',(5.87186938099994,12.2,-8.58956675700002));
#168678=CARTESIAN_POINT('Ctrl Pts',(5.87263625099995,12.2,-8.59045059900001));
#168679=CARTESIAN_POINT('Ctrl Pts',(5.87340981499994,12.2,-8.59134039400002));
#168680=CARTESIAN_POINT('Ctrl Pts',(5.87419006999994,12.2,-8.59223611300001));
#168681=CARTESIAN_POINT('Ctrl Pts',(5.87497701299994,12.2,-8.59313772700002));
#168682=CARTESIAN_POINT('Ctrl Pts',(5.87577063899994,12.2,-8.59404520900002));
#168683=CARTESIAN_POINT('Ctrl Pts',(5.87657094599994,12.2,-8.59495852900002));
#168684=CARTESIAN_POINT('Ctrl Pts',(5.87737793199994,12.2,-8.59587766000002));
#168685=CARTESIAN_POINT('Ctrl Pts',(5.87819159199994,12.2,-8.59680257500001));
#168686=CARTESIAN_POINT('Ctrl Pts',(5.87901192399994,12.2,-8.59773324500001));
#168687=CARTESIAN_POINT('Ctrl Pts',(5.87983892499994,12.2,-8.59866964200002));
#168688=CARTESIAN_POINT('Ctrl Pts',(5.88067259099994,12.2,-8.59961174000002));
#168689=CARTESIAN_POINT('Ctrl Pts',(5.88151291899995,12.2,-8.60055951000002));
#168690=CARTESIAN_POINT('Ctrl Pts',(5.88235990599995,12.2,-8.60151292500002));
#168691=CARTESIAN_POINT('Ctrl Pts',(5.88321354999994,12.2,-8.60247195900002));
#168692=CARTESIAN_POINT('Ctrl Pts',(5.88407384499994,12.2,-8.60343658400001));
#168693=CARTESIAN_POINT('Ctrl Pts',(5.88494079099994,12.2,-8.60440677400002));
#168694=CARTESIAN_POINT('Ctrl Pts',(5.88581438299995,12.2,-8.60538250100002));
#168695=CARTESIAN_POINT('Ctrl Pts',(5.88669461899994,12.2,-8.60636373900002));
#168696=CARTESIAN_POINT('Ctrl Pts',(5.88758149499994,12.2,-8.60735046100002));
#168697=CARTESIAN_POINT('Ctrl Pts',(5.88847500799995,12.2,-8.60834264100001));
#168698=CARTESIAN_POINT('Ctrl Pts',(5.88937515499994,12.2,-8.60934025300002));
#168699=CARTESIAN_POINT('Ctrl Pts',(5.89028193299994,12.2,-8.61034327100001));
#168700=CARTESIAN_POINT('Ctrl Pts',(5.89119533899994,12.2,-8.61135166700001));
#168701=CARTESIAN_POINT('Ctrl Pts',(5.89211536799994,12.2,-8.61236541700002));
#168702=CARTESIAN_POINT('Ctrl Pts',(5.89304201999994,12.2,-8.61338449400002));
#168703=CARTESIAN_POINT('Ctrl Pts',(5.89397528899994,12.2,-8.61440887300001));
#168704=CARTESIAN_POINT('Ctrl Pts',(5.89491517399994,12.2,-8.61543852800001));
#168705=CARTESIAN_POINT('Ctrl Pts',(5.89586167099994,12.2,-8.61647343400002));
#168706=CARTESIAN_POINT('Ctrl Pts',(5.89681477699994,12.2,-8.61751356400001));
#168707=CARTESIAN_POINT('Ctrl Pts',(5.89777448799994,12.2,-8.61855889400001));
#168708=CARTESIAN_POINT('Ctrl Pts',(5.89874080199994,12.2,-8.61960939900002));
#168709=CARTESIAN_POINT('Ctrl Pts',(5.89971371499994,12.2,-8.62066505300002));
#168710=CARTESIAN_POINT('Ctrl Pts',(5.90069322499994,12.2,-8.62172583100002));
#168711=CARTESIAN_POINT('Ctrl Pts',(5.90167932799995,12.2,-8.62279170800001));
#168712=CARTESIAN_POINT('Ctrl Pts',(5.90267202099994,12.2,-8.62386266200001));
#168713=CARTESIAN_POINT('Ctrl Pts',(5.90367129999994,12.2,-8.62493866400002));
#168714=CARTESIAN_POINT('Ctrl Pts',(5.90467716299995,12.2,-8.62601969300002));
#168715=CARTESIAN_POINT('Ctrl Pts',(5.90568960799994,12.2,-8.62710572200001));
#168716=CARTESIAN_POINT('Ctrl Pts',(5.90670862899994,12.2,-8.62819672800001));
#168717=CARTESIAN_POINT('Ctrl Pts',(5.90773422399995,12.2,-8.62929268600002));
#168718=CARTESIAN_POINT('Ctrl Pts',(5.90876639199994,12.2,-8.63039357200002));
#168719=CARTESIAN_POINT('Ctrl Pts',(5.90980512599995,12.2,-8.63149936300001));
#168720=CARTESIAN_POINT('Ctrl Pts',(5.91085042599994,12.2,-8.63261003400002));
#168721=CARTESIAN_POINT('Ctrl Pts',(5.91190228799994,12.2,-8.63372556000002));
#168722=CARTESIAN_POINT('Ctrl Pts',(5.91296070699994,12.2,-8.63484591900002));
#168723=CARTESIAN_POINT('Ctrl Pts',(5.91402568199995,12.2,-8.63597108700001));
#168724=CARTESIAN_POINT('Ctrl Pts',(5.91509720999994,12.2,-8.63710104100001));
#168725=CARTESIAN_POINT('Ctrl Pts',(5.91617528699994,12.2,-8.63823575600002));
#168726=CARTESIAN_POINT('Ctrl Pts',(5.91725990899994,12.2,-8.63937520900001));
#168727=CARTESIAN_POINT('Ctrl Pts',(5.91835107499994,12.2,-8.64051937700001));
#168728=CARTESIAN_POINT('Ctrl Pts',(5.91944877999994,12.2,-8.64166823700002));
#168729=CARTESIAN_POINT('Ctrl Pts',(5.92055302199994,12.2,-8.64282176500001));
#168730=CARTESIAN_POINT('Ctrl Pts',(5.92166379799995,12.2,-8.64397994000001));
#168731=CARTESIAN_POINT('Ctrl Pts',(5.92278110299994,12.2,-8.64514273600001));
#168732=CARTESIAN_POINT('Ctrl Pts',(5.92390493499994,12.2,-8.64631013400002));
#168733=CARTESIAN_POINT('Ctrl Pts',(5.92503529199995,12.2,-8.64748210700002));
#168734=CARTESIAN_POINT('Ctrl Pts',(5.92617216899994,12.2,-8.64865863600001));
#168735=CARTESIAN_POINT('Ctrl Pts',(5.92731556399994,12.2,-8.64983969600001));
#168736=CARTESIAN_POINT('Ctrl Pts',(5.92846547399994,12.2,-8.65102526600002));
#168737=CARTESIAN_POINT('Ctrl Pts',(5.92962189399994,12.2,-8.65221532200002));
#168738=CARTESIAN_POINT('Ctrl Pts',(5.93078482299994,12.2,-8.65340984300002));
#168739=CARTESIAN_POINT('Ctrl Pts',(5.93195425599994,12.2,-8.65460880700001));
#168740=CARTESIAN_POINT('Ctrl Pts',(5.93313019299995,12.2,-8.65581219100001));
#168741=CARTESIAN_POINT('Ctrl Pts',(5.93431262699994,12.2,-8.65701997400001));
#168742=CARTESIAN_POINT('Ctrl Pts',(5.93550155699995,12.2,-8.65823213200001));
#168743=CARTESIAN_POINT('Ctrl Pts',(5.93669697899994,12.2,-8.65944864500002));
#168744=CARTESIAN_POINT('Ctrl Pts',(5.93789889099994,12.2,-8.66066949100002));
#168745=CARTESIAN_POINT('Ctrl Pts',(5.93910728799995,12.2,-8.66189464800001));
#168746=CARTESIAN_POINT('Ctrl Pts',(5.94032216899994,12.2,-8.66312409300001));
#168747=CARTESIAN_POINT('Ctrl Pts',(5.94154352899994,12.2,-8.66435780700002));
#168748=CARTESIAN_POINT('Ctrl Pts',(5.94277136499994,12.2,-8.66559576600002));
#168749=CARTESIAN_POINT('Ctrl Pts',(5.94400567599994,12.2,-8.66683795100002));
#168750=CARTESIAN_POINT('Ctrl Pts',(5.94524645699994,12.2,-8.66808434000001));
#168751=CARTESIAN_POINT('Ctrl Pts',(5.94649370399994,12.2,-8.66933491000001));
#168752=CARTESIAN_POINT('Ctrl Pts',(5.94774741599994,12.2,-8.67058964200002));
#168753=CARTESIAN_POINT('Ctrl Pts',(5.94900758799994,12.2,-8.67184851400001));
#168754=CARTESIAN_POINT('Ctrl Pts',(5.95027421799994,12.2,-8.67311150500001));
#168755=CARTESIAN_POINT('Ctrl Pts',(5.95154730199994,12.2,-8.67437859500002));
#168756=CARTESIAN_POINT('Ctrl Pts',(5.95282683699994,12.2,-8.67564976200002));
#168757=CARTESIAN_POINT('Ctrl Pts',(5.95411282099994,12.2,-8.67692498600002));
#168758=CARTESIAN_POINT('Ctrl Pts',(5.95540524899994,12.2,-8.67820424500002));
#168759=CARTESIAN_POINT('Ctrl Pts',(5.95670411999994,12.2,-8.67948752000002));
#168760=CARTESIAN_POINT('Ctrl Pts',(5.95800942899994,12.2,-8.68077479000002));
#168761=CARTESIAN_POINT('Ctrl Pts',(5.95932117299995,12.2,-8.68206603400001));
#168762=CARTESIAN_POINT('Ctrl Pts',(5.96063934899995,12.2,-8.68336123200002));
#168763=CARTESIAN_POINT('Ctrl Pts',(5.96196395499994,12.2,-8.68466036400001));
#168764=CARTESIAN_POINT('Ctrl Pts',(5.96329498499995,12.2,-8.68596340900002));
#168765=CARTESIAN_POINT('Ctrl Pts',(5.96463243999994,12.2,-8.68727034800001));
#168766=CARTESIAN_POINT('Ctrl Pts',(5.96597631299995,12.2,-8.68858116100002));
#168767=CARTESIAN_POINT('Ctrl Pts',(5.96732660299994,12.2,-8.68989582500001));
#168768=CARTESIAN_POINT('Ctrl Pts',(5.96868330599994,12.2,-8.69121432500001));
#168769=CARTESIAN_POINT('Ctrl Pts',(5.97004641899994,12.2,-8.69253663700002));
#168770=CARTESIAN_POINT('Ctrl Pts',(5.97141593799994,12.2,-8.69386274300001));
#168771=CARTESIAN_POINT('Ctrl Pts',(5.97279186099994,12.2,-8.69519262200001));
#168772=CARTESIAN_POINT('Ctrl Pts',(5.97417418499995,12.2,-8.69652625600001));
#168773=CARTESIAN_POINT('Ctrl Pts',(5.97556290599995,12.2,-8.69786362500001));
#168774=CARTESIAN_POINT('Ctrl Pts',(5.97695801999994,12.2,-8.69920470900002));
#168775=CARTESIAN_POINT('Ctrl Pts',(5.97835952599994,12.2,-8.70054948900002));
#168776=CARTESIAN_POINT('Ctrl Pts',(5.97976741899994,12.2,-8.70189794500002));
#168777=CARTESIAN_POINT('Ctrl Pts',(5.98118169699994,12.2,-8.70325005800002));
#168778=CARTESIAN_POINT('Ctrl Pts',(5.98260235599994,12.2,-8.70460581000001));
#168779=CARTESIAN_POINT('Ctrl Pts',(5.98402939199994,12.2,-8.70596518000001));
#168780=CARTESIAN_POINT('Ctrl Pts',(5.98546280499994,12.2,-8.70732814900002));
#168781=CARTESIAN_POINT('Ctrl Pts',(5.98690258799994,12.2,-8.70869469900001));
#168782=CARTESIAN_POINT('Ctrl Pts',(5.98834873999994,12.2,-8.71006481000002));
#168783=CARTESIAN_POINT('Ctrl Pts',(5.98980125799994,12.2,-8.71143846400001));
#168784=CARTESIAN_POINT('Ctrl Pts',(5.99126013699995,12.2,-8.71281564200002));
#168785=CARTESIAN_POINT('Ctrl Pts',(5.99272537499995,12.2,-8.71419632500002));
#168786=CARTESIAN_POINT('Ctrl Pts',(5.99419696899995,12.2,-8.71558049400001));
#168787=CARTESIAN_POINT('Ctrl Pts',(5.99567491499994,12.2,-8.71696813100002));
#168788=CARTESIAN_POINT('Ctrl Pts',(5.99715921199994,12.2,-8.71835921700002));
#168789=CARTESIAN_POINT('Ctrl Pts',(5.99864985299994,12.2,-8.71975373400002));
#168790=CARTESIAN_POINT('Ctrl Pts',(6.00014683699994,12.2,-8.72115166300001));
#168791=CARTESIAN_POINT('Ctrl Pts',(6.00165016199994,12.2,-8.72255298400002));
#168792=CARTESIAN_POINT('Ctrl Pts',(6.00315982299994,12.2,-8.72395768300001));
#168793=CARTESIAN_POINT('Ctrl Pts',(6.00467581699994,12.2,-8.72536573700001));
#168794=CARTESIAN_POINT('Ctrl Pts',(6.00619813999994,12.2,-8.72677713200002));
#168795=CARTESIAN_POINT('Ctrl Pts',(6.00772679099994,12.2,-8.72819184600001));
#168796=CARTESIAN_POINT('Ctrl Pts',(6.00926176599994,12.2,-8.72960986400001));
#168797=CARTESIAN_POINT('Ctrl Pts',(6.01080305999994,12.2,-8.73103116600002));
#168798=CARTESIAN_POINT('Ctrl Pts',(6.01235067299994,12.2,-8.73245573400002));
#168799=CARTESIAN_POINT('Ctrl Pts',(6.01390459799994,12.2,-8.73388355100002));
#168800=CARTESIAN_POINT('Ctrl Pts',(6.01546483399994,12.2,-8.73531460000001));
#168801=CARTESIAN_POINT('Ctrl Pts',(6.01703137899994,12.2,-8.73674886200002));
#168802=CARTESIAN_POINT('Ctrl Pts',(6.01860422799994,12.2,-8.73818631900001));
#168803=CARTESIAN_POINT('Ctrl Pts',(6.02018337599994,12.2,-8.73962695300002));
#168804=CARTESIAN_POINT('Ctrl Pts',(6.02176882399994,12.2,-8.74107074900002));
#168805=CARTESIAN_POINT('Ctrl Pts',(6.02336056599994,12.2,-8.74251768600002));
#168806=CARTESIAN_POINT('Ctrl Pts',(6.02495859899994,12.2,-8.74396774900001));
#168807=CARTESIAN_POINT('Ctrl Pts',(6.02656291999994,12.2,-8.74542091800001));
#168808=CARTESIAN_POINT('Ctrl Pts',(6.02817352699994,12.2,-8.74687718000001));
#168809=CARTESIAN_POINT('Ctrl Pts',(6.02979041499994,12.2,-8.74833651300002));
#168810=CARTESIAN_POINT('Ctrl Pts',(6.03141358199994,12.2,-8.74979890200001));
#168811=CARTESIAN_POINT('Ctrl Pts',(6.03304302299994,12.2,-8.75126433100002));
#168812=CARTESIAN_POINT('Ctrl Pts',(6.03467873699994,12.2,-8.75273277900002));
#168813=CARTESIAN_POINT('Ctrl Pts',(6.03632071899994,12.2,-8.75420423200002));
#168814=CARTESIAN_POINT('Ctrl Pts',(6.03796896799994,12.2,-8.75567867300001));
#168815=CARTESIAN_POINT('Ctrl Pts',(6.03962347799994,12.2,-8.75715608400002));
#168816=CARTESIAN_POINT('Ctrl Pts',(6.04128424699995,12.2,-8.75863644800001));
#168817=CARTESIAN_POINT('Ctrl Pts',(6.04295127299994,12.2,-8.76011974800001));
#168818=CARTESIAN_POINT('Ctrl Pts',(6.04462455099994,12.2,-8.76160596800002));
#168819=CARTESIAN_POINT('Ctrl Pts',(6.04630407799994,12.2,-8.76309509100002));
#168820=CARTESIAN_POINT('Ctrl Pts',(6.04798985099994,12.2,-8.76458710000002));
#168821=CARTESIAN_POINT('Ctrl Pts',(6.04968186699994,12.2,-8.76608197700002));
#168822=CARTESIAN_POINT('Ctrl Pts',(6.05138012199994,12.2,-8.76757970900002));
#168823=CARTESIAN_POINT('Ctrl Pts',(6.05308461499994,12.2,-8.76908027600001));
#168824=CARTESIAN_POINT('Ctrl Pts',(6.05479533999994,12.2,-8.77058366200002));
#168825=CARTESIAN_POINT('Ctrl Pts',(6.05651229499995,12.2,-8.77208985200001));
#168826=CARTESIAN_POINT('Ctrl Pts',(6.05823547599995,12.2,-8.77359882900001));
#168827=CARTESIAN_POINT('Ctrl Pts',(6.05996488099994,12.2,-8.77511057700002));
#168828=CARTESIAN_POINT('Ctrl Pts',(6.06170050599994,12.2,-8.77662507800002));
#168829=CARTESIAN_POINT('Ctrl Pts',(6.06344234899994,12.2,-8.77814231800001));
#168830=CARTESIAN_POINT('Ctrl Pts',(6.06519040399994,12.2,-8.77966227900002));
#168831=CARTESIAN_POINT('Ctrl Pts',(6.06694466899994,12.2,-8.78118494600002));
#168832=CARTESIAN_POINT('Ctrl Pts',(6.06870514199994,12.2,-8.78271030200001));
#168833=CARTESIAN_POINT('Ctrl Pts',(6.07047181899994,12.2,-8.78423833100002));
#168834=CARTESIAN_POINT('Ctrl Pts',(6.07224469599994,12.2,-8.78576901800002));
#168835=CARTESIAN_POINT('Ctrl Pts',(6.07402377099994,12.2,-8.78730234600001));
#168836=CARTESIAN_POINT('Ctrl Pts',(6.07580903899994,12.2,-8.78883830000002));
#168837=CARTESIAN_POINT('Ctrl Pts',(6.07760049799994,12.2,-8.79037686400002));
#168838=CARTESIAN_POINT('Ctrl Pts',(6.07939814499994,12.2,-8.79191802100001));
#168839=CARTESIAN_POINT('Ctrl Pts',(6.08120197499994,12.2,-8.79346175700002));
#168840=CARTESIAN_POINT('Ctrl Pts',(6.08301198699994,12.2,-8.79500805500001));
#168841=CARTESIAN_POINT('Ctrl Pts',(6.08482817699994,12.2,-8.79655689900002));
#168842=CARTESIAN_POINT('Ctrl Pts',(6.08665053999994,12.2,-8.79810827400001));
#168843=CARTESIAN_POINT('Ctrl Pts',(6.08847907499994,12.2,-8.79966216600002));
#168844=CARTESIAN_POINT('Ctrl Pts',(6.09031377799995,12.2,-8.80121855700001));
#168845=CARTESIAN_POINT('Ctrl Pts',(6.09215464499994,12.2,-8.80277743400002));
#168846=CARTESIAN_POINT('Ctrl Pts',(6.09400167399994,12.2,-8.80433877800002));
#168847=CARTESIAN_POINT('Ctrl Pts',(6.09585485999994,12.2,-8.80590257700002));
#168848=CARTESIAN_POINT('Ctrl Pts',(6.09771420199994,12.2,-8.80746881400002));
#168849=CARTESIAN_POINT('Ctrl Pts',(6.09957969399994,12.2,-8.80903747400002));
#168850=CARTESIAN_POINT('Ctrl Pts',(6.10145133499994,12.2,-8.81060854200001));
#168851=CARTESIAN_POINT('Ctrl Pts',(6.10332912099994,12.2,-8.81218200200001));
#168852=CARTESIAN_POINT('Ctrl Pts',(6.10521304799994,12.2,-8.81375784000002));
#168853=CARTESIAN_POINT('Ctrl Pts',(6.10710311299994,12.2,-8.81533604100002));
#168854=CARTESIAN_POINT('Ctrl Pts',(6.10899931399994,12.2,-8.81691658800002));
#168855=CARTESIAN_POINT('Ctrl Pts',(6.11090164599994,12.2,-8.81849946800001));
#168856=CARTESIAN_POINT('Ctrl Pts',(6.11281010699994,12.2,-8.82008466500002));
#168857=CARTESIAN_POINT('Ctrl Pts',(6.11472469299994,12.2,-8.82167216400001));
#168858=CARTESIAN_POINT('Ctrl Pts',(6.11664539999994,12.2,-8.82326195200001));
#168859=CARTESIAN_POINT('Ctrl Pts',(6.11857222599994,12.2,-8.82485401100002));
#168860=CARTESIAN_POINT('Ctrl Pts',(6.12050516699994,12.2,-8.82644832800001));
#168861=CARTESIAN_POINT('Ctrl Pts',(6.12244422199994,12.2,-8.82804488900002));
#168862=CARTESIAN_POINT('Ctrl Pts',(6.12438938299994,12.2,-8.82964367800002));
#168863=CARTESIAN_POINT('Ctrl Pts',(6.12634064999994,12.2,-8.83124468000002));
#168864=CARTESIAN_POINT('Ctrl Pts',(6.12829801999994,12.2,-8.83284788100001));
#168865=CARTESIAN_POINT('Ctrl Pts',(6.13026148799994,12.2,-8.83445326700001));
#168866=CARTESIAN_POINT('Ctrl Pts',(6.13223105199994,12.2,-8.83606082300001));
#168867=CARTESIAN_POINT('Ctrl Pts',(6.13420670699994,12.2,-8.83767053400002));
#168868=CARTESIAN_POINT('Ctrl Pts',(6.13618845099994,12.2,-8.83928238600001));
#168869=CARTESIAN_POINT('Ctrl Pts',(6.13817627999994,12.2,-8.84089636400001));
#168870=CARTESIAN_POINT('Ctrl Pts',(6.14017019199994,12.2,-8.84251245500002));
#168871=CARTESIAN_POINT('Ctrl Pts',(6.14217018299994,12.2,-8.84413064300002));
#168872=CARTESIAN_POINT('Ctrl Pts',(6.14417624999994,12.2,-8.84575091500002));
#168873=CARTESIAN_POINT('Ctrl Pts',(6.14618838899994,12.2,-8.84737325500002));
#168874=CARTESIAN_POINT('Ctrl Pts',(6.14820659699994,12.2,-8.84899765100002));
#168875=CARTESIAN_POINT('Ctrl Pts',(6.15023086899994,12.2,-8.85062408700002));
#168876=CARTESIAN_POINT('Ctrl Pts',(6.15226120499995,12.2,-8.85225255100002));
#168877=CARTESIAN_POINT('Ctrl Pts',(6.15429759899994,12.2,-8.85388302700001));
#168878=CARTESIAN_POINT('Ctrl Pts',(6.15634004999994,12.2,-8.85551550100002));
#168879=CARTESIAN_POINT('Ctrl Pts',(6.15838855099994,12.2,-8.85714995900001));
#168880=CARTESIAN_POINT('Ctrl Pts',(6.16044310199994,12.2,-8.85878638800002));
#168881=CARTESIAN_POINT('Ctrl Pts',(6.16250369999994,12.2,-8.86042477400002));
#168882=CARTESIAN_POINT('Ctrl Pts',(6.16457033899994,12.2,-8.86206510100001));
#168883=CARTESIAN_POINT('Ctrl Pts',(6.16664301799994,12.2,-8.86370735900002));
#168884=CARTESIAN_POINT('Ctrl Pts',(6.16872173199994,12.2,-8.86535153000001));
#168885=CARTESIAN_POINT('Ctrl Pts',(6.17080647799994,12.2,-8.86699760300001));
#168886=CARTESIAN_POINT('Ctrl Pts',(6.17289725299995,12.2,-8.86864556300001));
#168887=CARTESIAN_POINT('Ctrl Pts',(6.17499405399994,12.2,-8.87029539700002));
#168888=CARTESIAN_POINT('Ctrl Pts',(6.17709687799994,12.2,-8.87194709200001));
#168889=CARTESIAN_POINT('Ctrl Pts',(6.17920571999994,12.2,-8.87360063200001));
#168890=CARTESIAN_POINT('Ctrl Pts',(6.18132057899994,12.2,-8.87525600500001));
#168891=CARTESIAN_POINT('Ctrl Pts',(6.18344144899994,12.2,-8.87691319600002));
#168892=CARTESIAN_POINT('Ctrl Pts',(6.18556832799994,12.2,-8.87857219500002));
#168893=CARTESIAN_POINT('Ctrl Pts',(6.18770121399994,12.2,-8.88023298500002));
#168894=CARTESIAN_POINT('Ctrl Pts',(6.18984009999994,12.2,-8.88189555400002));
#168895=CARTESIAN_POINT('Ctrl Pts',(6.19198498599994,12.2,-8.88355988700001));
#168896=CARTESIAN_POINT('Ctrl Pts',(6.19413586799994,12.2,-8.88522597300001));
#168897=CARTESIAN_POINT('Ctrl Pts',(6.19629274299994,12.2,-8.88689379800002));
#168898=CARTESIAN_POINT('Ctrl Pts',(6.19845560599994,12.2,-8.88856334700002));
#168899=CARTESIAN_POINT('Ctrl Pts',(6.20062445399994,12.2,-8.89023460900002));
#168900=CARTESIAN_POINT('Ctrl Pts',(6.20279928499994,12.2,-8.89190757000001));
#168901=CARTESIAN_POINT('Ctrl Pts',(6.20498009499994,12.2,-8.89358221500002));
#168902=CARTESIAN_POINT('Ctrl Pts',(6.20716688099994,12.2,-8.89525853400002));
#168903=CARTESIAN_POINT('Ctrl Pts',(6.20935963799995,12.2,-8.89693651100002));
#168904=CARTESIAN_POINT('Ctrl Pts',(6.21155836399994,12.2,-8.89861613500001));
#168905=CARTESIAN_POINT('Ctrl Pts',(6.21376305499994,12.2,-8.90029739200001));
#168906=CARTESIAN_POINT('Ctrl Pts',(6.21597370899994,12.2,-8.90198026900002));
#168907=CARTESIAN_POINT('Ctrl Pts',(6.21819032199994,12.2,-8.90366475300001));
#168908=CARTESIAN_POINT('Ctrl Pts',(6.22041288899994,12.2,-8.90535083100002));
#168909=CARTESIAN_POINT('Ctrl Pts',(6.22264140799994,12.2,-8.90703849100002));
#168910=CARTESIAN_POINT('Ctrl Pts',(6.22487587699994,12.2,-8.90872771900002));
#168911=CARTESIAN_POINT('Ctrl Pts',(6.22711629099994,12.2,-8.91041850200001));
#168912=CARTESIAN_POINT('Ctrl Pts',(6.22936264599994,12.2,-8.91211082700002));
#168913=CARTESIAN_POINT('Ctrl Pts',(6.23161493899994,12.2,-8.91380468300002));
#168914=CARTESIAN_POINT('Ctrl Pts',(6.23387316899994,12.2,-8.91550005600001));
#168915=CARTESIAN_POINT('Ctrl Pts',(6.23613732999994,12.2,-8.91719693300002));
#168916=CARTESIAN_POINT('Ctrl Pts',(6.23840741799994,12.2,-8.91889530200002));
#168917=CARTESIAN_POINT('Ctrl Pts',(6.24068343299994,12.2,-8.92059515000001));
#168918=CARTESIAN_POINT('Ctrl Pts',(6.24296536899994,12.2,-8.92229646500001));
#168919=CARTESIAN_POINT('Ctrl Pts',(6.24525322299994,12.2,-8.92399923300001));
#168920=CARTESIAN_POINT('Ctrl Pts',(6.24754699199994,12.2,-8.92570344200001));
#168921=CARTESIAN_POINT('Ctrl Pts',(6.24984667299994,12.2,-8.92740908100001));
#168922=CARTESIAN_POINT('Ctrl Pts',(6.25215226099994,12.2,-8.92911613600001));
#168923=CARTESIAN_POINT('Ctrl Pts',(6.25446375499994,12.2,-8.93082459400001));
#168924=CARTESIAN_POINT('Ctrl Pts',(6.25678114899994,12.2,-8.93253444400001));
#168925=CARTESIAN_POINT('Ctrl Pts',(6.25910444299994,12.2,-8.93424567300002));
#168926=CARTESIAN_POINT('Ctrl Pts',(6.26143362999994,12.2,-8.93595826800002));
#168927=CARTESIAN_POINT('Ctrl Pts',(6.26376870799994,12.2,-8.93767221800001));
#168928=CARTESIAN_POINT('Ctrl Pts',(6.26610967499994,12.2,-8.93938751000002));
#168929=CARTESIAN_POINT('Ctrl Pts',(6.26845652499994,12.2,-8.94110413200002));
#168930=CARTESIAN_POINT('Ctrl Pts',(6.27080925699994,12.2,-8.94282207100002));
#168931=CARTESIAN_POINT('Ctrl Pts',(6.27316786699994,12.2,-8.94454131600002));
#168932=CARTESIAN_POINT('Ctrl Pts',(6.27553235099994,12.2,-8.94626185400002));
#168933=CARTESIAN_POINT('Ctrl Pts',(6.27790270499994,12.2,-8.94798367200002));
#168934=CARTESIAN_POINT('Ctrl Pts',(6.28027892799994,12.2,-8.94970676000002));
#168935=CARTESIAN_POINT('Ctrl Pts',(6.28266101299994,12.2,-8.95143110400002));
#168936=CARTESIAN_POINT('Ctrl Pts',(6.28504895899994,12.2,-8.95315669400001));
#168937=CARTESIAN_POINT('Ctrl Pts',(6.28744276399994,12.2,-8.95488351500001));
#168938=CARTESIAN_POINT('Ctrl Pts',(6.28984242199994,12.2,-8.95661155900001));
#168939=CARTESIAN_POINT('Ctrl Pts',(6.29224792999994,12.2,-8.95834081000002));
#168940=CARTESIAN_POINT('Ctrl Pts',(6.29465928599994,12.2,-8.96007125900002));
#168941=CARTESIAN_POINT('Ctrl Pts',(6.29707648499994,12.2,-8.96180289200002));
#168942=CARTESIAN_POINT('Ctrl Pts',(6.29949952399994,12.2,-8.96353569800001));
#168943=CARTESIAN_POINT('Ctrl Pts',(6.30192839999994,12.2,-8.96526966600002));
#168944=CARTESIAN_POINT('Ctrl Pts',(6.30436310999994,12.2,-8.96700478300002));
#168945=CARTESIAN_POINT('Ctrl Pts',(6.30680364899994,12.2,-8.96874103900002));
#168946=CARTESIAN_POINT('Ctrl Pts',(6.30925001499994,12.2,-8.97047842000001));
#168947=CARTESIAN_POINT('Ctrl Pts',(6.31170220399994,12.2,-8.97221691500001));
#168948=CARTESIAN_POINT('Ctrl Pts',(6.31416021399994,12.2,-8.97395651300002));
#168949=CARTESIAN_POINT('Ctrl Pts',(6.31662403899994,12.2,-8.97569720100002));
#168950=CARTESIAN_POINT('Ctrl Pts',(6.31909367699994,12.2,-8.97743896900002));
#168951=CARTESIAN_POINT('Ctrl Pts',(6.32156912499994,12.2,-8.97918180400002));
#168952=CARTESIAN_POINT('Ctrl Pts',(6.32405037899994,12.2,-8.98092569600001));
#168953=CARTESIAN_POINT('Ctrl Pts',(6.32653743599994,12.2,-8.98267063100001));
#168954=CARTESIAN_POINT('Ctrl Pts',(6.32903029199994,12.2,-8.98441660100002));
#168955=CARTESIAN_POINT('Ctrl Pts',(6.33152894299994,12.2,-8.98616359100001));
#168956=CARTESIAN_POINT('Ctrl Pts',(6.33403338799994,12.2,-8.98791159100002));
#168957=CARTESIAN_POINT('Ctrl Pts',(6.33654362099994,12.2,-8.98966059000001));
#168958=CARTESIAN_POINT('Ctrl Pts',(6.33905963999994,12.2,-8.99141057600002));
#168959=CARTESIAN_POINT('Ctrl Pts',(6.34158143999994,12.2,-8.99316153900001));
#168960=CARTESIAN_POINT('Ctrl Pts',(6.34410901999994,12.2,-8.99491346500002));
#168961=CARTESIAN_POINT('Ctrl Pts',(6.34664237499994,12.2,-8.99666634500001));
#168962=CARTESIAN_POINT('Ctrl Pts',(6.34918150099994,12.2,-8.99842016600001));
#168963=CARTESIAN_POINT('Ctrl Pts',(6.35172639699994,12.2,-9.00017491800002));
#168964=CARTESIAN_POINT('Ctrl Pts',(6.35427705599994,12.2,-9.00193058900001));
#168965=CARTESIAN_POINT('Ctrl Pts',(6.35683347799994,12.2,-9.00368716800001));
#168966=CARTESIAN_POINT('Ctrl Pts',(6.35939565699994,12.2,-9.00544464400001));
#168967=CARTESIAN_POINT('Ctrl Pts',(6.36196359199994,12.2,-9.00720300600002));
#168968=CARTESIAN_POINT('Ctrl Pts',(6.36453727799994,12.2,-9.00896224300002));
#168969=CARTESIAN_POINT('Ctrl Pts',(6.36711671099994,12.2,-9.01072234300001));
#168970=CARTESIAN_POINT('Ctrl Pts',(6.36970188799994,12.2,-9.01248329400002));
#168971=CARTESIAN_POINT('Ctrl Pts',(6.37229280699994,12.2,-9.01424508800002));
#168972=CARTESIAN_POINT('Ctrl Pts',(6.37488946299994,12.2,-9.01600771300001));
#168973=CARTESIAN_POINT('Ctrl Pts',(6.37749185299994,12.2,-9.01777115600002));
#168974=CARTESIAN_POINT('Ctrl Pts',(6.38009997299994,12.2,-9.01953540700001));
#168975=CARTESIAN_POINT('Ctrl Pts',(6.38271382099994,12.2,-9.02130045600002));
#168976=CARTESIAN_POINT('Ctrl Pts',(6.38533339199994,12.2,-9.02306629200002));
#168977=CARTESIAN_POINT('Ctrl Pts',(6.38795868399994,12.2,-9.02483290300001));
#168978=CARTESIAN_POINT('Ctrl Pts',(6.39058969199994,12.2,-9.02660027900002));
#168979=CARTESIAN_POINT('Ctrl Pts',(6.39322641399994,12.2,-9.02836840800001));
#168980=CARTESIAN_POINT('Ctrl Pts',(6.39586884499994,12.2,-9.03013728200002));
#168981=CARTESIAN_POINT('Ctrl Pts',(6.39851698299994,12.2,-9.03190688700001));
#168982=CARTESIAN_POINT('Ctrl Pts',(6.40117082299994,12.2,-9.03367721300001));
#168983=CARTESIAN_POINT('Ctrl Pts',(6.40383036299994,12.2,-9.03544825000001));
#168984=CARTESIAN_POINT('Ctrl Pts',(6.40649559999994,12.2,-9.03721998700002));
#168985=CARTESIAN_POINT('Ctrl Pts',(6.40916652899994,12.2,-9.03899241300002));
#168986=CARTESIAN_POINT('Ctrl Pts',(6.41184314599994,12.2,-9.04076551800001));
#168987=CARTESIAN_POINT('Ctrl Pts',(6.41452544999994,12.2,-9.04253929100001));
#168988=CARTESIAN_POINT('Ctrl Pts',(6.41721343599994,12.2,-9.04431372100002));
#168989=CARTESIAN_POINT('Ctrl Pts',(6.41990709999994,12.2,-9.04608879800002));
#168990=CARTESIAN_POINT('Ctrl Pts',(6.42260643999994,12.2,-9.04786451100002));
#168991=CARTESIAN_POINT('Ctrl Pts',(6.42531145199994,12.2,-9.04964084900002));
#168992=CARTESIAN_POINT('Ctrl Pts',(6.42802213199994,12.2,-9.05141780400001));
#168993=CARTESIAN_POINT('Ctrl Pts',(6.43073847599994,12.2,-9.05319536200002));
#168994=CARTESIAN_POINT('Ctrl Pts',(6.43346048199994,12.2,-9.05497351500001));
#168995=CARTESIAN_POINT('Ctrl Pts',(6.43618814599995,12.2,-9.05675225100002));
#168996=CARTESIAN_POINT('Ctrl Pts',(6.43892146399994,12.2,-9.05853156000001));
#168997=CARTESIAN_POINT('Ctrl Pts',(6.44166043299994,12.2,-9.06031143300002));
#168998=CARTESIAN_POINT('Ctrl Pts',(6.44440504999994,12.2,-9.06209185800002));
#168999=CARTESIAN_POINT('Ctrl Pts',(6.44715531099994,12.2,-9.06387282500001));
#169000=CARTESIAN_POINT('Ctrl Pts',(6.44991121199994,12.2,-9.06565432300001));
#169001=CARTESIAN_POINT('Ctrl Pts',(6.45267274999994,12.2,-9.06743634400001));
#169002=CARTESIAN_POINT('Ctrl Pts',(6.45543992299994,12.2,-9.06921887500001));
#169003=CARTESIAN_POINT('Ctrl Pts',(6.45821272399994,12.2,-9.07100190800002));
#169004=CARTESIAN_POINT('Ctrl Pts',(6.46099115299994,12.2,-9.07278543100002));
#169005=CARTESIAN_POINT('Ctrl Pts',(6.46377520499994,12.2,-9.07456943400001));
#169006=CARTESIAN_POINT('Ctrl Pts',(6.46656487599994,12.2,-9.07635390800002));
#169007=CARTESIAN_POINT('Ctrl Pts',(6.46936016299994,12.2,-9.07813884200002));
#169008=CARTESIAN_POINT('Ctrl Pts',(6.47216106399994,12.2,-9.07992422500002));
#169009=CARTESIAN_POINT('Ctrl Pts',(6.47496757199994,12.2,-9.08171004900002));
#169010=CARTESIAN_POINT('Ctrl Pts',(6.47777968799994,12.2,-9.08349630400001));
#169011=CARTESIAN_POINT('Ctrl Pts',(6.48059740499994,12.2,-9.08528297600002));
#169012=CARTESIAN_POINT('Ctrl Pts',(6.48342072099994,12.2,-9.08707005900002));
#169013=CARTESIAN_POINT('Ctrl Pts',(6.48624963199994,12.2,-9.08885754100002));
#169014=CARTESIAN_POINT('Ctrl Pts',(6.48908413499994,12.2,-9.09064541400002));
#169015=CARTESIAN_POINT('Ctrl Pts',(6.49192422599994,12.2,-9.09243366500002));
#169016=CARTESIAN_POINT('Ctrl Pts',(6.49476990199994,12.2,-9.09422228700001));
#169017=CARTESIAN_POINT('Ctrl Pts',(6.49762115899994,12.2,-9.09601126700002));
#169018=CARTESIAN_POINT('Ctrl Pts',(6.50047799399994,12.2,-9.09780059800001));
#169019=CARTESIAN_POINT('Ctrl Pts',(6.50334040299994,12.2,-9.09959026900001));
#169020=CARTESIAN_POINT('Ctrl Pts',(6.50620838199995,12.2,-9.10138026900002));
#169021=CARTESIAN_POINT('Ctrl Pts',(6.50908192999994,12.2,-9.10317059000001));
#169022=CARTESIAN_POINT('Ctrl Pts',(6.51196104099995,12.2,-9.10496122100002));
#169023=CARTESIAN_POINT('Ctrl Pts',(6.51484571099994,12.2,-9.10675215300002));
#169024=CARTESIAN_POINT('Ctrl Pts',(6.51773593899994,12.2,-9.10854337500002));
#169025=CARTESIAN_POINT('Ctrl Pts',(6.52063172099994,12.2,-9.11033487800001));
#169026=CARTESIAN_POINT('Ctrl Pts',(6.52353305099994,12.2,-9.11212665200001));
#169027=CARTESIAN_POINT('Ctrl Pts',(6.52643992799994,12.2,-9.11391868900001));
#169028=CARTESIAN_POINT('Ctrl Pts',(6.52935234699994,12.2,-9.11571097500002));
#169029=CARTESIAN_POINT('Ctrl Pts',(6.53227030599994,12.2,-9.11750350600002));
#169030=CARTESIAN_POINT('Ctrl Pts',(6.53519379999994,12.2,-9.11929626800001));
#169031=CARTESIAN_POINT('Ctrl Pts',(6.53812282699994,12.2,-9.12108925300002));
#169032=CARTESIAN_POINT('Ctrl Pts',(6.54105738299994,12.2,-9.12288245200001));
#169033=CARTESIAN_POINT('Ctrl Pts',(6.54399746299994,12.2,-9.12467585300002));
#169034=CARTESIAN_POINT('Ctrl Pts',(6.54694306499994,12.2,-9.12646944900001));
#169035=CARTESIAN_POINT('Ctrl Pts',(6.54989418399994,12.2,-9.12826322900001));
#169036=CARTESIAN_POINT('Ctrl Pts',(6.55285081899994,12.2,-9.13005718400001));
#169037=CARTESIAN_POINT('Ctrl Pts',(6.55581296599994,12.2,-9.13185130500001));
#169038=CARTESIAN_POINT('Ctrl Pts',(6.55878061899994,12.2,-9.13364558100002));
#169039=CARTESIAN_POINT('Ctrl Pts',(6.56175377599994,12.2,-9.13544000400002));
#169040=CARTESIAN_POINT('Ctrl Pts',(6.56473243399994,12.2,-9.13723456500002));
#169041=CARTESIAN_POINT('Ctrl Pts',(6.56771658899994,12.2,-9.13902925200002));
#169042=CARTESIAN_POINT('Ctrl Pts',(6.57070623699994,12.2,-9.14082405700002));
#169043=CARTESIAN_POINT('Ctrl Pts',(6.57370137599994,12.2,-9.14261897200002));
#169044=CARTESIAN_POINT('Ctrl Pts',(6.57670199999994,12.2,-9.14441398600001));
#169045=CARTESIAN_POINT('Ctrl Pts',(6.57970810799994,12.2,-9.14620908900002));
#169046=CARTESIAN_POINT('Ctrl Pts',(6.58271969499994,12.2,-9.14800427400002));
#169047=CARTESIAN_POINT('Ctrl Pts',(6.58573675799994,12.2,-9.14979953100002));
#169048=CARTESIAN_POINT('Ctrl Pts',(6.58875929299994,12.2,-9.15159484900002));
#169049=CARTESIAN_POINT('Ctrl Pts',(6.59178729699994,12.2,-9.15339022000002));
#169050=CARTESIAN_POINT('Ctrl Pts',(6.59482076499994,12.2,-9.15518563400001));
#169051=CARTESIAN_POINT('Ctrl Pts',(6.59785969599994,12.2,-9.15698108300001));
#169052=CARTESIAN_POINT('Ctrl Pts',(6.60090408599994,12.2,-9.15877655700001));
#169053=CARTESIAN_POINT('Ctrl Pts',(6.60395392899995,12.2,-9.16057204700002));
#169054=CARTESIAN_POINT('Ctrl Pts',(6.60700922399994,12.2,-9.16236754400002));
#169055=CARTESIAN_POINT('Ctrl Pts',(6.61006996599995,12.2,-9.16416303900002));
#169056=CARTESIAN_POINT('Ctrl Pts',(6.61313615199994,12.2,-9.16595852100002));
#169057=CARTESIAN_POINT('Ctrl Pts',(6.61620777899994,12.2,-9.16775398400001));
#169058=CARTESIAN_POINT('Ctrl Pts',(6.61928484299994,12.2,-9.16954941700002));
#169059=CARTESIAN_POINT('Ctrl Pts',(6.62236733999994,12.2,-9.17134481100002));
#169060=CARTESIAN_POINT('Ctrl Pts',(6.62545526699994,12.2,-9.17314015600001));
#169061=CARTESIAN_POINT('Ctrl Pts',(6.62854862099994,12.2,-9.17493544700001));
#169062=CARTESIAN_POINT('Ctrl Pts',(6.63164739699994,12.2,-9.17673067000001));
#169063=CARTESIAN_POINT('Ctrl Pts',(6.63475159199994,12.2,-9.17852581800001));
#169064=CARTESIAN_POINT('Ctrl Pts',(6.63786120299994,12.2,-9.18032088200002));
#169065=CARTESIAN_POINT('Ctrl Pts',(6.64097622599994,12.2,-9.18211585500002));
#169066=CARTESIAN_POINT('Ctrl Pts',(6.64409665799995,12.2,-9.18391072500001));
#169067=CARTESIAN_POINT('Ctrl Pts',(6.64722249499994,12.2,-9.18570548400002));
#169068=CARTESIAN_POINT('Ctrl Pts',(6.65035373299995,12.2,-9.18750012300002));
#169069=CARTESIAN_POINT('Ctrl Pts',(6.65349036899994,12.2,-9.18929463500002));
#169070=CARTESIAN_POINT('Ctrl Pts',(6.65663239999994,12.2,-9.19108900900002));
#169071=CARTESIAN_POINT('Ctrl Pts',(6.65977982099994,12.2,-9.19288323700002));
#169072=CARTESIAN_POINT('Ctrl Pts',(6.66293262999995,12.2,-9.19467731100001));
#169073=CARTESIAN_POINT('Ctrl Pts',(6.66609082299995,12.2,-9.19647121900002));
#169074=CARTESIAN_POINT('Ctrl Pts',(6.66925439499994,12.2,-9.19826495600002));
#169075=CARTESIAN_POINT('Ctrl Pts',(6.67242334399995,12.2,-9.20005851000001));
#169076=CARTESIAN_POINT('Ctrl Pts',(6.67559766699994,12.2,-9.20185187500002));
#169077=CARTESIAN_POINT('Ctrl Pts',(6.67877735899994,12.2,-9.20364504200002));
#169078=CARTESIAN_POINT('Ctrl Pts',(6.68196241599994,12.2,-9.20543800000001));
#169079=CARTESIAN_POINT('Ctrl Pts',(6.68515283699994,12.2,-9.20723074200002));
#169080=CARTESIAN_POINT('Ctrl Pts',(6.68834861499994,12.2,-9.20902325900002));
#169081=CARTESIAN_POINT('Ctrl Pts',(6.69154974999994,12.2,-9.21081554300001));
#169082=CARTESIAN_POINT('Ctrl Pts',(6.69475623599994,12.2,-9.21260758400001));
#169083=CARTESIAN_POINT('Ctrl Pts',(6.69796806999994,12.2,-9.21439937500002));
#169084=CARTESIAN_POINT('Ctrl Pts',(6.70118524799994,12.2,-9.21619090500002));
#169085=CARTESIAN_POINT('Ctrl Pts',(6.70440776799994,12.2,-9.21798216800001));
#169086=CARTESIAN_POINT('Ctrl Pts',(6.70763562499994,12.2,-9.21977315400002));
#169087=CARTESIAN_POINT('Ctrl Pts',(6.71086881499994,12.2,-9.22156385400001));
#169088=CARTESIAN_POINT('Ctrl Pts',(6.71410733699994,12.2,-9.22335426000001));
#169089=CARTESIAN_POINT('Ctrl Pts',(6.71735118499994,12.2,-9.22514436400002));
#169090=CARTESIAN_POINT('Ctrl Pts',(6.72060035499995,12.2,-9.22693415700002));
#169091=CARTESIAN_POINT('Ctrl Pts',(6.72385484599994,12.2,-9.22872363200002));
#169092=CARTESIAN_POINT('Ctrl Pts',(6.72711465299995,12.2,-9.23051277900001));
#169093=CARTESIAN_POINT('Ctrl Pts',(6.73037977199994,12.2,-9.23230159000001));
#169094=CARTESIAN_POINT('Ctrl Pts',(6.73365020099994,12.2,-9.23409005700002));
#169095=CARTESIAN_POINT('Ctrl Pts',(6.73692593399994,12.2,-9.23587817000002));
#169096=CARTESIAN_POINT('Ctrl Pts',(6.74020696799994,12.2,-9.23766592000002));
#169097=CARTESIAN_POINT('Ctrl Pts',(6.74349330199994,12.2,-9.23945330000001));
#169098=CARTESIAN_POINT('Ctrl Pts',(6.74678492799995,12.2,-9.24124030000002));
#169099=CARTESIAN_POINT('Ctrl Pts',(6.75008184499994,12.2,-9.24302691400002));
#169100=CARTESIAN_POINT('Ctrl Pts',(6.75338404999994,12.2,-9.24481313200002));
#169101=CARTESIAN_POINT('Ctrl Pts',(6.75669153899995,12.2,-9.24659894800002));
#169102=CARTESIAN_POINT('Ctrl Pts',(6.76000430999994,12.2,-9.24838435500002));
#169103=CARTESIAN_POINT('Ctrl Pts',(6.76332235699994,12.2,-9.25016934500002));
#169104=CARTESIAN_POINT('Ctrl Pts',(6.76664567999994,12.2,-9.25195390800001));
#169105=CARTESIAN_POINT('Ctrl Pts',(6.76997427099994,12.2,-9.25373803600002));
#169106=CARTESIAN_POINT('Ctrl Pts',(6.77330812799994,12.2,-9.25552171800001));
#169107=CARTESIAN_POINT('Ctrl Pts',(6.77664724599994,12.2,-9.25730494300002));
#169108=CARTESIAN_POINT('Ctrl Pts',(6.77999162099994,12.2,-9.25908770200002));
#169109=CARTESIAN_POINT('Ctrl Pts',(6.78334124799994,12.2,-9.26086998700002));
#169110=CARTESIAN_POINT('Ctrl Pts',(6.78669612399994,12.2,-9.26265178800002));
#169111=CARTESIAN_POINT('Ctrl Pts',(6.79005624699994,12.2,-9.26443310200002));
#169112=CARTESIAN_POINT('Ctrl Pts',(6.79342161599994,12.2,-9.26621392500002));
#169113=CARTESIAN_POINT('Ctrl Pts',(6.79679222899994,12.2,-9.26799425300001));
#169114=CARTESIAN_POINT('Ctrl Pts',(6.79949291499995,12.2,-9.26941812000001));
#169115=CARTESIAN_POINT('Ctrl Pts',(6.80152078799994,12.2,-9.27048579800001));
#169116=CARTESIAN_POINT('Ctrl Pts',(6.80287375199994,12.2,-9.27119748400001));
#169117=CARTESIAN_POINT('Ctrl Pts',(6.80355049599994,12.2,-9.27155330300002));
#169118=CARTESIAN_POINT('Ctrl Pts',(7.10901226899994,15.2,-9.03946594400002));
#169119=CARTESIAN_POINT('Ctrl Pts',(7.10901226899994,11.6,-9.03946594400002));
#169120=CARTESIAN_POINT('Ctrl Pts',(7.10885083699995,15.2,-9.03871859500001));
#169121=CARTESIAN_POINT('Ctrl Pts',(7.10885083699995,11.6,-9.03871859500001));
#169122=CARTESIAN_POINT('Ctrl Pts',(7.10852778299994,15.2,-9.03722439200001));
#169123=CARTESIAN_POINT('Ctrl Pts',(7.10852778299994,11.6,-9.03722439200001));
#169124=CARTESIAN_POINT('Ctrl Pts',(7.10804263899995,15.2,-9.03498456100002));
#169125=CARTESIAN_POINT('Ctrl Pts',(7.10804263899995,11.6,-9.03498456100002));
#169126=CARTESIAN_POINT('Ctrl Pts',(7.10739465099994,15.2,-9.03200107200002));
#169127=CARTESIAN_POINT('Ctrl Pts',(7.10739465099994,11.6,-9.03200107200002));
#169128=CARTESIAN_POINT('Ctrl Pts',(7.10658278299994,15.2,-9.02827662900001));
#169129=CARTESIAN_POINT('Ctrl Pts',(7.10658278299994,11.6,-9.02827662900001));
#169130=CARTESIAN_POINT('Ctrl Pts',(7.10576903499994,15.2,-9.02455710700002));
#169131=CARTESIAN_POINT('Ctrl Pts',(7.10576903499994,11.6,-9.02455710700002));
#169132=CARTESIAN_POINT('Ctrl Pts',(7.10495340799994,15.2,-9.02084250500002));
#169133=CARTESIAN_POINT('Ctrl Pts',(7.10495340799994,11.6,-9.02084250500002));
#169134=CARTESIAN_POINT('Ctrl Pts',(7.10413590299994,15.2,-9.01713282900002));
#169135=CARTESIAN_POINT('Ctrl Pts',(7.10413590299994,11.6,-9.01713282900002));
#169136=CARTESIAN_POINT('Ctrl Pts',(7.10331652799994,15.2,-9.01342808000001));
#169137=CARTESIAN_POINT('Ctrl Pts',(7.10331652799994,11.6,-9.01342808000001));
#169138=CARTESIAN_POINT('Ctrl Pts',(7.10249528699994,15.2,-9.00972826500002));
#169139=CARTESIAN_POINT('Ctrl Pts',(7.10249528699994,11.6,-9.00972826500002));
#169140=CARTESIAN_POINT('Ctrl Pts',(7.10167218799994,15.2,-9.00603338900002));
#169141=CARTESIAN_POINT('Ctrl Pts',(7.10167218799994,11.6,-9.00603338900002));
#169142=CARTESIAN_POINT('Ctrl Pts',(7.10084723999994,15.2,-9.00234345900002));
#169143=CARTESIAN_POINT('Ctrl Pts',(7.10084723999994,11.6,-9.00234345900002));
#169144=CARTESIAN_POINT('Ctrl Pts',(7.10002044999994,15.2,-8.99865848200001));
#169145=CARTESIAN_POINT('Ctrl Pts',(7.10002044999994,11.6,-8.99865848200001));
#169146=CARTESIAN_POINT('Ctrl Pts',(7.09919182999994,15.2,-8.99497846600001));
#169147=CARTESIAN_POINT('Ctrl Pts',(7.09919182999994,11.6,-8.99497846600001));
#169148=CARTESIAN_POINT('Ctrl Pts',(7.09836138399995,15.2,-8.99130341500002));
#169149=CARTESIAN_POINT('Ctrl Pts',(7.09836138399995,11.6,-8.99130341500002));
#169150=CARTESIAN_POINT('Ctrl Pts',(7.09752912199995,15.2,-8.98763333900002));
#169151=CARTESIAN_POINT('Ctrl Pts',(7.09752912199995,11.6,-8.98763333900002));
#169152=CARTESIAN_POINT('Ctrl Pts',(7.09669504999995,15.2,-8.98396824000002));
#169153=CARTESIAN_POINT('Ctrl Pts',(7.09669504999995,11.6,-8.98396824000002));
#169154=CARTESIAN_POINT('Ctrl Pts',(7.09585917499994,15.2,-8.98030812400001));
#169155=CARTESIAN_POINT('Ctrl Pts',(7.09585917499994,11.6,-8.98030812400001));
#169156=CARTESIAN_POINT('Ctrl Pts',(7.09502150299994,15.2,-8.97665299700002));
#169157=CARTESIAN_POINT('Ctrl Pts',(7.09502150299994,11.6,-8.97665299700002));
#169158=CARTESIAN_POINT('Ctrl Pts',(7.09418203899994,15.2,-8.97300286300002));
#169159=CARTESIAN_POINT('Ctrl Pts',(7.09418203899994,11.6,-8.97300286300002));
#169160=CARTESIAN_POINT('Ctrl Pts',(7.09334079199994,15.2,-8.96935772800001));
#169161=CARTESIAN_POINT('Ctrl Pts',(7.09334079199994,11.6,-8.96935772800001));
#169162=CARTESIAN_POINT('Ctrl Pts',(7.09249776599994,15.2,-8.96571759800001));
#169163=CARTESIAN_POINT('Ctrl Pts',(7.09249776599994,11.6,-8.96571759800001));
#169164=CARTESIAN_POINT('Ctrl Pts',(7.09165297099994,15.2,-8.96208247700002));
#169165=CARTESIAN_POINT('Ctrl Pts',(7.09165297099994,11.6,-8.96208247700002));
#169166=CARTESIAN_POINT('Ctrl Pts',(7.09080641499994,15.2,-8.95845237400002));
#169167=CARTESIAN_POINT('Ctrl Pts',(7.09080641499994,11.6,-8.95845237400002));
#169168=CARTESIAN_POINT('Ctrl Pts',(7.08995810299994,15.2,-8.95482729200002));
#169169=CARTESIAN_POINT('Ctrl Pts',(7.08995810299994,11.6,-8.95482729200002));
#169170=CARTESIAN_POINT('Ctrl Pts',(7.08910804199994,15.2,-8.95120723800002));
#169171=CARTESIAN_POINT('Ctrl Pts',(7.08910804199994,11.6,-8.95120723800002));
#169172=CARTESIAN_POINT('Ctrl Pts',(7.08825624299994,15.2,-8.94759221800001));
#169173=CARTESIAN_POINT('Ctrl Pts',(7.08825624299994,11.6,-8.94759221800001));
#169174=CARTESIAN_POINT('Ctrl Pts',(7.08740270999995,15.2,-8.94398223900001));
#169175=CARTESIAN_POINT('Ctrl Pts',(7.08740270999995,11.6,-8.94398223900001));
#169176=CARTESIAN_POINT('Ctrl Pts',(7.08654745099994,15.2,-8.94037730400001));
#169177=CARTESIAN_POINT('Ctrl Pts',(7.08654745099994,11.6,-8.94037730400001));
#169178=CARTESIAN_POINT('Ctrl Pts',(7.08569047499994,15.2,-8.93677742100002));
#169179=CARTESIAN_POINT('Ctrl Pts',(7.08569047499994,11.6,-8.93677742100002));
#169180=CARTESIAN_POINT('Ctrl Pts',(7.08483178599994,15.2,-8.93318259300001));
#169181=CARTESIAN_POINT('Ctrl Pts',(7.08483178599994,11.6,-8.93318259300001));
#169182=CARTESIAN_POINT('Ctrl Pts',(7.08397139199994,15.2,-8.92959282900001));
#169183=CARTESIAN_POINT('Ctrl Pts',(7.08397139199994,11.6,-8.92959282900001));
#169184=CARTESIAN_POINT('Ctrl Pts',(7.08310930199994,15.2,-8.92600813100002));
#169185=CARTESIAN_POINT('Ctrl Pts',(7.08310930199994,11.6,-8.92600813100002));
#169186=CARTESIAN_POINT('Ctrl Pts',(7.08224552099994,15.2,-8.92242850800002));
#169187=CARTESIAN_POINT('Ctrl Pts',(7.08224552099994,11.6,-8.92242850800002));
#169188=CARTESIAN_POINT('Ctrl Pts',(7.08138005899994,15.2,-8.91885396400001));
#169189=CARTESIAN_POINT('Ctrl Pts',(7.08138005899994,11.6,-8.91885396400001));
#169190=CARTESIAN_POINT('Ctrl Pts',(7.08051291999994,15.2,-8.91528450500001));
#169191=CARTESIAN_POINT('Ctrl Pts',(7.08051291999994,11.6,-8.91528450500001));
#169192=CARTESIAN_POINT('Ctrl Pts',(7.07964411499994,15.2,-8.91172013700002));
#169193=CARTESIAN_POINT('Ctrl Pts',(7.07964411499994,11.6,-8.91172013700002));
#169194=CARTESIAN_POINT('Ctrl Pts',(7.07877364899994,15.2,-8.90816086600001));
#169195=CARTESIAN_POINT('Ctrl Pts',(7.07877364899994,11.6,-8.90816086600001));
#169196=CARTESIAN_POINT('Ctrl Pts',(7.07790152999995,15.2,-8.90460669800002));
#169197=CARTESIAN_POINT('Ctrl Pts',(7.07790152999995,11.6,-8.90460669800002));
#169198=CARTESIAN_POINT('Ctrl Pts',(7.07702776499994,15.2,-8.90105763700002));
#169199=CARTESIAN_POINT('Ctrl Pts',(7.07702776499994,11.6,-8.90105763700002));
#169200=CARTESIAN_POINT('Ctrl Pts',(7.07615236299994,15.2,-8.89751369100001));
#169201=CARTESIAN_POINT('Ctrl Pts',(7.07615236299994,11.6,-8.89751369100001));
#169202=CARTESIAN_POINT('Ctrl Pts',(7.07527532899995,15.2,-8.89397486500001));
#169203=CARTESIAN_POINT('Ctrl Pts',(7.07527532899995,11.6,-8.89397486500001));
#169204=CARTESIAN_POINT('Ctrl Pts',(7.07439667399994,15.2,-8.89044116400001));
#169205=CARTESIAN_POINT('Ctrl Pts',(7.07439667399994,11.6,-8.89044116400001));
#169206=CARTESIAN_POINT('Ctrl Pts',(7.07351640099994,15.2,-8.88691259500002));
#169207=CARTESIAN_POINT('Ctrl Pts',(7.07351640099994,11.6,-8.88691259500002));
#169208=CARTESIAN_POINT('Ctrl Pts',(7.07263452099994,15.2,-8.88338916200002));
#169209=CARTESIAN_POINT('Ctrl Pts',(7.07263452099994,11.6,-8.88338916200002));
#169210=CARTESIAN_POINT('Ctrl Pts',(7.07175103999995,15.2,-8.87987087200001));
#169211=CARTESIAN_POINT('Ctrl Pts',(7.07175103999995,11.6,-8.87987087200001));
#169212=CARTESIAN_POINT('Ctrl Pts',(7.07086596699994,15.2,-8.87635773100002));
#169213=CARTESIAN_POINT('Ctrl Pts',(7.07086596699994,11.6,-8.87635773100002));
#169214=CARTESIAN_POINT('Ctrl Pts',(7.06997930699995,15.2,-8.87284974500002));
#169215=CARTESIAN_POINT('Ctrl Pts',(7.06997930699995,11.6,-8.87284974500002));
#169216=CARTESIAN_POINT('Ctrl Pts',(7.06909106899994,15.2,-8.86934691900001));
#169217=CARTESIAN_POINT('Ctrl Pts',(7.06909106899994,11.6,-8.86934691900001));
#169218=CARTESIAN_POINT('Ctrl Pts',(7.06820126099994,15.2,-8.86584925900002));
#169219=CARTESIAN_POINT('Ctrl Pts',(7.06820126099994,11.6,-8.86584925900002));
#169220=CARTESIAN_POINT('Ctrl Pts',(7.06730988999994,15.2,-8.86235676900002));
#169221=CARTESIAN_POINT('Ctrl Pts',(7.06730988999994,11.6,-8.86235676900002));
#169222=CARTESIAN_POINT('Ctrl Pts',(7.06641696399994,15.2,-8.85886945800002));
#169223=CARTESIAN_POINT('Ctrl Pts',(7.06641696399994,11.6,-8.85886945800002));
#169224=CARTESIAN_POINT('Ctrl Pts',(7.06552248999994,15.2,-8.85538733200002));
#169225=CARTESIAN_POINT('Ctrl Pts',(7.06552248999994,11.6,-8.85538733200002));
#169226=CARTESIAN_POINT('Ctrl Pts',(7.06462647799994,15.2,-8.85191039400001));
#169227=CARTESIAN_POINT('Ctrl Pts',(7.06462647799994,11.6,-8.85191039400001));
#169228=CARTESIAN_POINT('Ctrl Pts',(7.06372893199994,15.2,-8.84843865100001));
#169229=CARTESIAN_POINT('Ctrl Pts',(7.06372893199994,11.6,-8.84843865100001));
#169230=CARTESIAN_POINT('Ctrl Pts',(7.06282986099994,15.2,-8.84497210900001));
#169231=CARTESIAN_POINT('Ctrl Pts',(7.06282986099994,11.6,-8.84497210900001));
#169232=CARTESIAN_POINT('Ctrl Pts',(7.06192927499995,15.2,-8.84151077400002));
#169233=CARTESIAN_POINT('Ctrl Pts',(7.06192927499995,11.6,-8.84151077400002));
#169234=CARTESIAN_POINT('Ctrl Pts',(7.06102717799994,15.2,-8.83805465100002));
#169235=CARTESIAN_POINT('Ctrl Pts',(7.06102717799994,11.6,-8.83805465100002));
#169236=CARTESIAN_POINT('Ctrl Pts',(7.06012358099994,15.2,-8.83460374700002));
#169237=CARTESIAN_POINT('Ctrl Pts',(7.06012358099994,11.6,-8.83460374700002));
#169238=CARTESIAN_POINT('Ctrl Pts',(7.05921848999994,15.2,-8.83115806600001));
#169239=CARTESIAN_POINT('Ctrl Pts',(7.05921848999994,11.6,-8.83115806600001));
#169240=CARTESIAN_POINT('Ctrl Pts',(7.05831191399994,15.2,-8.82771761700001));
#169241=CARTESIAN_POINT('Ctrl Pts',(7.05831191399994,11.6,-8.82771761700001));
#169242=CARTESIAN_POINT('Ctrl Pts',(7.05740385899994,15.2,-8.82428240200002));
#169243=CARTESIAN_POINT('Ctrl Pts',(7.05740385899994,11.6,-8.82428240200002));
#169244=CARTESIAN_POINT('Ctrl Pts',(7.05649433399994,15.2,-8.82085243000001));
#169245=CARTESIAN_POINT('Ctrl Pts',(7.05649433399994,11.6,-8.82085243000001));
#169246=CARTESIAN_POINT('Ctrl Pts',(7.05558334699995,15.2,-8.81742770600002));
#169247=CARTESIAN_POINT('Ctrl Pts',(7.05558334699995,11.6,-8.81742770600002));
#169248=CARTESIAN_POINT('Ctrl Pts',(7.05467090599995,15.2,-8.81400823500002));
#169249=CARTESIAN_POINT('Ctrl Pts',(7.05467090599995,11.6,-8.81400823500002));
#169250=CARTESIAN_POINT('Ctrl Pts',(7.05375701899994,15.2,-8.81059402400002));
#169251=CARTESIAN_POINT('Ctrl Pts',(7.05375701899994,11.6,-8.81059402400002));
#169252=CARTESIAN_POINT('Ctrl Pts',(7.05284169299994,15.2,-8.80718507700001));
#169253=CARTESIAN_POINT('Ctrl Pts',(7.05284169299994,11.6,-8.80718507700001));
#169254=CARTESIAN_POINT('Ctrl Pts',(7.05192493599994,15.2,-8.80378140200002));
#169255=CARTESIAN_POINT('Ctrl Pts',(7.05192493599994,11.6,-8.80378140200002));
#169256=CARTESIAN_POINT('Ctrl Pts',(7.05100675599994,15.2,-8.80038300300001));
#169257=CARTESIAN_POINT('Ctrl Pts',(7.05100675599994,11.6,-8.80038300300001));
#169258=CARTESIAN_POINT('Ctrl Pts',(7.05008716199995,15.2,-8.79698988800002));
#169259=CARTESIAN_POINT('Ctrl Pts',(7.05008716199995,11.6,-8.79698988800002));
#169260=CARTESIAN_POINT('Ctrl Pts',(7.04916616099994,15.2,-8.79360206200002));
#169261=CARTESIAN_POINT('Ctrl Pts',(7.04916616099994,11.6,-8.79360206200002));
#169262=CARTESIAN_POINT('Ctrl Pts',(7.04824376099995,15.2,-8.79021953000001));
#169263=CARTESIAN_POINT('Ctrl Pts',(7.04824376099995,11.6,-8.79021953000001));
#169264=CARTESIAN_POINT('Ctrl Pts',(7.04731997099994,15.2,-8.78684229900001));
#169265=CARTESIAN_POINT('Ctrl Pts',(7.04731997099994,11.6,-8.78684229900001));
#169266=CARTESIAN_POINT('Ctrl Pts',(7.04639479699994,15.2,-8.78347037400001));
#169267=CARTESIAN_POINT('Ctrl Pts',(7.04639479699994,11.6,-8.78347037400001));
#169268=CARTESIAN_POINT('Ctrl Pts',(7.04546824999994,15.2,-8.78010376100002));
#169269=CARTESIAN_POINT('Ctrl Pts',(7.04546824999994,11.6,-8.78010376100002));
#169270=CARTESIAN_POINT('Ctrl Pts',(7.04454033599994,15.2,-8.77674246600002));
#169271=CARTESIAN_POINT('Ctrl Pts',(7.04454033599994,11.6,-8.77674246600002));
#169272=CARTESIAN_POINT('Ctrl Pts',(7.04361106199995,15.2,-8.77338649600001));
#169273=CARTESIAN_POINT('Ctrl Pts',(7.04361106199995,11.6,-8.77338649600001));
#169274=CARTESIAN_POINT('Ctrl Pts',(7.04268043899994,15.2,-8.77003585600002));
#169275=CARTESIAN_POINT('Ctrl Pts',(7.04268043899994,11.6,-8.77003585600002));
#169276=CARTESIAN_POINT('Ctrl Pts',(7.04174847399995,15.2,-8.76669055200002));
#169277=CARTESIAN_POINT('Ctrl Pts',(7.04174847399995,11.6,-8.76669055200002));
#169278=CARTESIAN_POINT('Ctrl Pts',(7.04081517499994,15.2,-8.76335058900001));
#169279=CARTESIAN_POINT('Ctrl Pts',(7.04081517499994,11.6,-8.76335058900001));
#169280=CARTESIAN_POINT('Ctrl Pts',(7.03988054999994,15.2,-8.76001597500002));
#169281=CARTESIAN_POINT('Ctrl Pts',(7.03988054999994,11.6,-8.76001597500002));
#169282=CARTESIAN_POINT('Ctrl Pts',(7.03894460699994,15.2,-8.75668671600002));
#169283=CARTESIAN_POINT('Ctrl Pts',(7.03894460699994,11.6,-8.75668671600002));
#169284=CARTESIAN_POINT('Ctrl Pts',(7.03800735599994,15.2,-8.75336281500001));
#169285=CARTESIAN_POINT('Ctrl Pts',(7.03800735599994,11.6,-8.75336281500001));
#169286=CARTESIAN_POINT('Ctrl Pts',(7.03706880199994,15.2,-8.75004428000001));
#169287=CARTESIAN_POINT('Ctrl Pts',(7.03706880199994,11.6,-8.75004428000001));
#169288=CARTESIAN_POINT('Ctrl Pts',(7.03612895599995,15.2,-8.74673111600002));
#169289=CARTESIAN_POINT('Ctrl Pts',(7.03612895599995,11.6,-8.74673111600002));
#169290=CARTESIAN_POINT('Ctrl Pts',(7.03518782499994,15.2,-8.74342333000002));
#169291=CARTESIAN_POINT('Ctrl Pts',(7.03518782499994,11.6,-8.74342333000002));
#169292=CARTESIAN_POINT('Ctrl Pts',(7.03424541799994,15.2,-8.74012092800001));
#169293=CARTESIAN_POINT('Ctrl Pts',(7.03424541799994,11.6,-8.74012092800001));
#169294=CARTESIAN_POINT('Ctrl Pts',(7.03330174299994,15.2,-8.73682391500001));
#169295=CARTESIAN_POINT('Ctrl Pts',(7.03330174299994,11.6,-8.73682391500001));
#169296=CARTESIAN_POINT('Ctrl Pts',(7.03235680899994,15.2,-8.73353229700001));
#169297=CARTESIAN_POINT('Ctrl Pts',(7.03235680899994,11.6,-8.73353229700001));
#169298=CARTESIAN_POINT('Ctrl Pts',(7.03141062299995,15.2,-8.73024608200001));
#169299=CARTESIAN_POINT('Ctrl Pts',(7.03141062299995,11.6,-8.73024608200001));
#169300=CARTESIAN_POINT('Ctrl Pts',(7.03046319299995,15.2,-8.72696527400001));
#169301=CARTESIAN_POINT('Ctrl Pts',(7.03046319299995,11.6,-8.72696527400001));
#169302=CARTESIAN_POINT('Ctrl Pts',(7.02951453099994,15.2,-8.72368987800002));
#169303=CARTESIAN_POINT('Ctrl Pts',(7.02951453099994,11.6,-8.72368987800002));
#169304=CARTESIAN_POINT('Ctrl Pts',(7.02856464099994,15.2,-8.72041990300002));
#169305=CARTESIAN_POINT('Ctrl Pts',(7.02856464099994,11.6,-8.72041990300002));
#169306=CARTESIAN_POINT('Ctrl Pts',(7.02761353399994,15.2,-8.71715535200002));
#169307=CARTESIAN_POINT('Ctrl Pts',(7.02761353399994,11.6,-8.71715535200002));
#169308=CARTESIAN_POINT('Ctrl Pts',(7.02666121799994,15.2,-8.71389623300002));
#169309=CARTESIAN_POINT('Ctrl Pts',(7.02666121799994,11.6,-8.71389623300002));
#169310=CARTESIAN_POINT('Ctrl Pts',(7.02570770099994,15.2,-8.71064255100002));
#169311=CARTESIAN_POINT('Ctrl Pts',(7.02570770099994,11.6,-8.71064255100002));
#169312=CARTESIAN_POINT('Ctrl Pts',(7.02475299199994,15.2,-8.70739431300001));
#169313=CARTESIAN_POINT('Ctrl Pts',(7.02475299199994,11.6,-8.70739431300001));
#169314=CARTESIAN_POINT('Ctrl Pts',(7.02379709999994,15.2,-8.70415152400002));
#169315=CARTESIAN_POINT('Ctrl Pts',(7.02379709999994,11.6,-8.70415152400002));
#169316=CARTESIAN_POINT('Ctrl Pts',(7.02284003299994,15.2,-8.70091419100002));
#169317=CARTESIAN_POINT('Ctrl Pts',(7.02284003299994,11.6,-8.70091419100002));
#169318=CARTESIAN_POINT('Ctrl Pts',(7.02188179799994,15.2,-8.69768231900002));
#169319=CARTESIAN_POINT('Ctrl Pts',(7.02188179799994,11.6,-8.69768231900002));
#169320=CARTESIAN_POINT('Ctrl Pts',(7.02092240599994,15.2,-8.69445591400002));
#169321=CARTESIAN_POINT('Ctrl Pts',(7.02092240599994,11.6,-8.69445591400002));
#169322=CARTESIAN_POINT('Ctrl Pts',(7.01996186499994,15.2,-8.69123498300001));
#169323=CARTESIAN_POINT('Ctrl Pts',(7.01996186499994,11.6,-8.69123498300001));
#169324=CARTESIAN_POINT('Ctrl Pts',(7.01900018299995,15.2,-8.68801953100002));
#169325=CARTESIAN_POINT('Ctrl Pts',(7.01900018299995,11.6,-8.68801953100002));
#169326=CARTESIAN_POINT('Ctrl Pts',(7.01803736899994,15.2,-8.68480956600001));
#169327=CARTESIAN_POINT('Ctrl Pts',(7.01803736899994,11.6,-8.68480956600001));
#169328=CARTESIAN_POINT('Ctrl Pts',(7.01707343299995,15.2,-8.68160509100001));
#169329=CARTESIAN_POINT('Ctrl Pts',(7.01707343299995,11.6,-8.68160509100001));
#169330=CARTESIAN_POINT('Ctrl Pts',(7.01610838099994,15.2,-8.67840611400002));
#169331=CARTESIAN_POINT('Ctrl Pts',(7.01610838099994,11.6,-8.67840611400002));
#169332=CARTESIAN_POINT('Ctrl Pts',(7.01514222399994,15.2,-8.67521264000001));
#169333=CARTESIAN_POINT('Ctrl Pts',(7.01514222399994,11.6,-8.67521264000001));
#169334=CARTESIAN_POINT('Ctrl Pts',(7.01417496999994,15.2,-8.67202467700002));
#169335=CARTESIAN_POINT('Ctrl Pts',(7.01417496999994,11.6,-8.67202467700002));
#169336=CARTESIAN_POINT('Ctrl Pts',(7.01320662599994,15.2,-8.66884222900002));
#169337=CARTESIAN_POINT('Ctrl Pts',(7.01320662599994,11.6,-8.66884222900002));
#169338=CARTESIAN_POINT('Ctrl Pts',(7.01223720399994,15.2,-8.66566530400002));
#169339=CARTESIAN_POINT('Ctrl Pts',(7.01223720399994,11.6,-8.66566530400002));
#169340=CARTESIAN_POINT('Ctrl Pts',(7.01126671099995,15.2,-8.66249390500002));
#169341=CARTESIAN_POINT('Ctrl Pts',(7.01126671099995,11.6,-8.66249390500002));
#169342=CARTESIAN_POINT('Ctrl Pts',(7.01029515599994,15.2,-8.65932804100002));
#169343=CARTESIAN_POINT('Ctrl Pts',(7.01029515599994,11.6,-8.65932804100002));
#169344=CARTESIAN_POINT('Ctrl Pts',(7.00932254799994,15.2,-8.65616771800001));
#169345=CARTESIAN_POINT('Ctrl Pts',(7.00932254799994,11.6,-8.65616771800001));
#169346=CARTESIAN_POINT('Ctrl Pts',(7.00834889699994,15.2,-8.65301294000002));
#169347=CARTESIAN_POINT('Ctrl Pts',(7.00834889699994,11.6,-8.65301294000002));
#169348=CARTESIAN_POINT('Ctrl Pts',(7.00737420899994,15.2,-8.64986371400001));
#169349=CARTESIAN_POINT('Ctrl Pts',(7.00737420899994,11.6,-8.64986371400001));
#169350=CARTESIAN_POINT('Ctrl Pts',(7.00639849599995,15.2,-8.64672004800001));
#169351=CARTESIAN_POINT('Ctrl Pts',(7.00639849599995,11.6,-8.64672004800001));
#169352=CARTESIAN_POINT('Ctrl Pts',(7.00542176599994,15.2,-8.64358194500002));
#169353=CARTESIAN_POINT('Ctrl Pts',(7.00542176599994,11.6,-8.64358194500002));
#169354=CARTESIAN_POINT('Ctrl Pts',(7.00444402699994,15.2,-8.64044941300002));
#169355=CARTESIAN_POINT('Ctrl Pts',(7.00444402699994,11.6,-8.64044941300002));
#169356=CARTESIAN_POINT('Ctrl Pts',(7.00346528799995,15.2,-8.63732245800002));
#169357=CARTESIAN_POINT('Ctrl Pts',(7.00346528799995,11.6,-8.63732245800002));
#169358=CARTESIAN_POINT('Ctrl Pts',(7.00248555899995,15.2,-8.63420108600002));
#169359=CARTESIAN_POINT('Ctrl Pts',(7.00248555899995,11.6,-8.63420108600002));
#169360=CARTESIAN_POINT('Ctrl Pts',(7.00150484899994,15.2,-8.63108530300002));
#169361=CARTESIAN_POINT('Ctrl Pts',(7.00150484899994,11.6,-8.63108530300002));
#169362=CARTESIAN_POINT('Ctrl Pts',(7.00052316699994,15.2,-8.62797511400002));
#169363=CARTESIAN_POINT('Ctrl Pts',(7.00052316699994,11.6,-8.62797511400002));
#169364=CARTESIAN_POINT('Ctrl Pts',(6.99954052099995,15.2,-8.62487052700001));
#169365=CARTESIAN_POINT('Ctrl Pts',(6.99954052099995,11.6,-8.62487052700001));
#169366=CARTESIAN_POINT('Ctrl Pts',(6.99855692199994,15.2,-8.62177154700002));
#169367=CARTESIAN_POINT('Ctrl Pts',(6.99855692199994,11.6,-8.62177154700002));
#169368=CARTESIAN_POINT('Ctrl Pts',(6.99757237899994,15.2,-8.61867818100002));
#169369=CARTESIAN_POINT('Ctrl Pts',(6.99757237899994,11.6,-8.61867818100002));
#169370=CARTESIAN_POINT('Ctrl Pts',(6.99658689799994,15.2,-8.61559043400002));
#169371=CARTESIAN_POINT('Ctrl Pts',(6.99658689799994,11.6,-8.61559043400002));
#169372=CARTESIAN_POINT('Ctrl Pts',(6.99560049199994,15.2,-8.61250831300002));
#169373=CARTESIAN_POINT('Ctrl Pts',(6.99560049199994,11.6,-8.61250831300002));
#169374=CARTESIAN_POINT('Ctrl Pts',(6.99461316799994,15.2,-8.60943182400002));
#169375=CARTESIAN_POINT('Ctrl Pts',(6.99461316799994,11.6,-8.60943182400002));
#169376=CARTESIAN_POINT('Ctrl Pts',(6.99362493699994,15.2,-8.60636097400001));
#169377=CARTESIAN_POINT('Ctrl Pts',(6.99362493699994,11.6,-8.60636097400001));
#169378=CARTESIAN_POINT('Ctrl Pts',(6.99263580599994,15.2,-8.60329576700002));
#169379=CARTESIAN_POINT('Ctrl Pts',(6.99263580599994,11.6,-8.60329576700002));
#169380=CARTESIAN_POINT('Ctrl Pts',(6.99164578499994,15.2,-8.60023621100002));
#169381=CARTESIAN_POINT('Ctrl Pts',(6.99164578499994,11.6,-8.60023621100002));
#169382=CARTESIAN_POINT('Ctrl Pts',(6.99065488599994,15.2,-8.59718231200001));
#169383=CARTESIAN_POINT('Ctrl Pts',(6.99065488599994,11.6,-8.59718231200001));
#169384=CARTESIAN_POINT('Ctrl Pts',(6.98966311399994,15.2,-8.59413407600002));
#169385=CARTESIAN_POINT('Ctrl Pts',(6.98966311399994,11.6,-8.59413407600002));
#169386=CARTESIAN_POINT('Ctrl Pts',(6.98867048099994,15.2,-8.59109150800002));
#169387=CARTESIAN_POINT('Ctrl Pts',(6.98867048099994,11.6,-8.59109150800002));
#169388=CARTESIAN_POINT('Ctrl Pts',(6.98767699599994,15.2,-8.58805461600002));
#169389=CARTESIAN_POINT('Ctrl Pts',(6.98767699599994,11.6,-8.58805461600002));
#169390=CARTESIAN_POINT('Ctrl Pts',(6.98668266799994,15.2,-8.58502340600002));
#169391=CARTESIAN_POINT('Ctrl Pts',(6.98668266799994,11.6,-8.58502340600002));
#169392=CARTESIAN_POINT('Ctrl Pts',(6.98568750699994,15.2,-8.58199788300002));
#169393=CARTESIAN_POINT('Ctrl Pts',(6.98568750699994,11.6,-8.58199788300002));
#169394=CARTESIAN_POINT('Ctrl Pts',(6.98469152199994,15.2,-8.57897805400002));
#169395=CARTESIAN_POINT('Ctrl Pts',(6.98469152199994,11.6,-8.57897805400002));
#169396=CARTESIAN_POINT('Ctrl Pts',(6.98369472199994,15.2,-8.57596392400002));
#169397=CARTESIAN_POINT('Ctrl Pts',(6.98369472199994,11.6,-8.57596392400002));
#169398=CARTESIAN_POINT('Ctrl Pts',(6.98269711799994,15.2,-8.57295550200002));
#169399=CARTESIAN_POINT('Ctrl Pts',(6.98269711799994,11.6,-8.57295550200002));
#169400=CARTESIAN_POINT('Ctrl Pts',(6.98169871799994,15.2,-8.56995279200002));
#169401=CARTESIAN_POINT('Ctrl Pts',(6.98169871799994,11.6,-8.56995279200002));
#169402=CARTESIAN_POINT('Ctrl Pts',(6.98069953199994,15.2,-8.56695580000002));
#169403=CARTESIAN_POINT('Ctrl Pts',(6.98069953199994,11.6,-8.56695580000002));
#169404=CARTESIAN_POINT('Ctrl Pts',(6.97969957099994,15.2,-8.56396453400002));
#169405=CARTESIAN_POINT('Ctrl Pts',(6.97969957099994,11.6,-8.56396453400002));
#169406=CARTESIAN_POINT('Ctrl Pts',(6.97869884199994,15.2,-8.56097899900002));
#169407=CARTESIAN_POINT('Ctrl Pts',(6.97869884199994,11.6,-8.56097899900002));
#169408=CARTESIAN_POINT('Ctrl Pts',(6.97769735699994,15.2,-8.55799920200001));
#169409=CARTESIAN_POINT('Ctrl Pts',(6.97769735699994,11.6,-8.55799920200001));
#169410=CARTESIAN_POINT('Ctrl Pts',(6.97669512399994,15.2,-8.55502514800002));
#169411=CARTESIAN_POINT('Ctrl Pts',(6.97669512399994,11.6,-8.55502514800002));
#169412=CARTESIAN_POINT('Ctrl Pts',(6.97569215299994,15.2,-8.55205684500002));
#169413=CARTESIAN_POINT('Ctrl Pts',(6.97569215299994,11.6,-8.55205684500002));
#169414=CARTESIAN_POINT('Ctrl Pts',(6.97468845399994,15.2,-8.54909429700001));
#169415=CARTESIAN_POINT('Ctrl Pts',(6.97468845399994,11.6,-8.54909429700001));
#169416=CARTESIAN_POINT('Ctrl Pts',(6.97368403699994,15.2,-8.54613751400001));
#169417=CARTESIAN_POINT('Ctrl Pts',(6.97368403699994,11.6,-8.54613751400001));
#169418=CARTESIAN_POINT('Ctrl Pts',(6.97267891199994,15.2,-8.54318649800001));
#169419=CARTESIAN_POINT('Ctrl Pts',(6.97267891199994,11.6,-8.54318649800001));
#169420=CARTESIAN_POINT('Ctrl Pts',(6.97167308699994,15.2,-8.54024125700001));
#169421=CARTESIAN_POINT('Ctrl Pts',(6.97167308699994,11.6,-8.54024125700001));
#169422=CARTESIAN_POINT('Ctrl Pts',(6.97066657399994,15.2,-8.53730179900002));
#169423=CARTESIAN_POINT('Ctrl Pts',(6.97066657399994,11.6,-8.53730179900002));
#169424=CARTESIAN_POINT('Ctrl Pts',(6.96965938299994,15.2,-8.53436812800001));
#169425=CARTESIAN_POINT('Ctrl Pts',(6.96965938299994,11.6,-8.53436812800001));
#169426=CARTESIAN_POINT('Ctrl Pts',(6.96865152099994,15.2,-8.53144025000002));
#169427=CARTESIAN_POINT('Ctrl Pts',(6.96865152099994,11.6,-8.53144025000002));
#169428=CARTESIAN_POINT('Ctrl Pts',(6.96764299999994,15.2,-8.52851817400002));
#169429=CARTESIAN_POINT('Ctrl Pts',(6.96764299999994,11.6,-8.52851817400002));
#169430=CARTESIAN_POINT('Ctrl Pts',(6.96663382999994,15.2,-8.52560190500002));
#169431=CARTESIAN_POINT('Ctrl Pts',(6.96663382999994,11.6,-8.52560190500002));
#169432=CARTESIAN_POINT('Ctrl Pts',(6.96562401999994,15.2,-8.52269144800001));
#169433=CARTESIAN_POINT('Ctrl Pts',(6.96562401999994,11.6,-8.52269144800001));
#169434=CARTESIAN_POINT('Ctrl Pts',(6.96461357999994,15.2,-8.51978681100002));
#169435=CARTESIAN_POINT('Ctrl Pts',(6.96461357999994,11.6,-8.51978681100002));
#169436=CARTESIAN_POINT('Ctrl Pts',(6.96360252099994,15.2,-8.51688800000002));
#169437=CARTESIAN_POINT('Ctrl Pts',(6.96360252099994,11.6,-8.51688800000002));
#169438=CARTESIAN_POINT('Ctrl Pts',(6.96259085299994,15.2,-8.51399502000002));
#169439=CARTESIAN_POINT('Ctrl Pts',(6.96259085299994,11.6,-8.51399502000002));
#169440=CARTESIAN_POINT('Ctrl Pts',(6.96157858499994,15.2,-8.51110787900001));
#169441=CARTESIAN_POINT('Ctrl Pts',(6.96157858499994,11.6,-8.51110787900001));
#169442=CARTESIAN_POINT('Ctrl Pts',(6.96056572699994,15.2,-8.50822658400002));
#169443=CARTESIAN_POINT('Ctrl Pts',(6.96056572699994,11.6,-8.50822658400002));
#169444=CARTESIAN_POINT('Ctrl Pts',(6.95955229099994,15.2,-8.50535113900002));
#169445=CARTESIAN_POINT('Ctrl Pts',(6.95955229099994,11.6,-8.50535113900002));
#169446=CARTESIAN_POINT('Ctrl Pts',(6.95853828499994,15.2,-8.50248155200001));
#169447=CARTESIAN_POINT('Ctrl Pts',(6.95853828499994,11.6,-8.50248155200001));
#169448=CARTESIAN_POINT('Ctrl Pts',(6.95752371999995,15.2,-8.49961782800002));
#169449=CARTESIAN_POINT('Ctrl Pts',(6.95752371999995,11.6,-8.49961782800002));
#169450=CARTESIAN_POINT('Ctrl Pts',(6.95650860599994,15.2,-8.49675997600002));
#169451=CARTESIAN_POINT('Ctrl Pts',(6.95650860599994,11.6,-8.49675997600002));
#169452=CARTESIAN_POINT('Ctrl Pts',(6.95549295399994,15.2,-8.49390799900002));
#169453=CARTESIAN_POINT('Ctrl Pts',(6.95549295399994,11.6,-8.49390799900002));
#169454=CARTESIAN_POINT('Ctrl Pts',(6.95447677299994,15.2,-8.49106190600001));
#169455=CARTESIAN_POINT('Ctrl Pts',(6.95447677299994,11.6,-8.49106190600001));
#169456=CARTESIAN_POINT('Ctrl Pts',(6.95346007499994,15.2,-8.48822170300001));
#169457=CARTESIAN_POINT('Ctrl Pts',(6.95346007499994,11.6,-8.48822170300001));
#169458=CARTESIAN_POINT('Ctrl Pts',(6.95244286799994,15.2,-8.48538739600002));
#169459=CARTESIAN_POINT('Ctrl Pts',(6.95244286799994,11.6,-8.48538739600002));
#169460=CARTESIAN_POINT('Ctrl Pts',(6.95142516299994,15.2,-8.48255899100002));
#169461=CARTESIAN_POINT('Ctrl Pts',(6.95142516299994,11.6,-8.48255899100002));
#169462=CARTESIAN_POINT('Ctrl Pts',(6.95040697199994,15.2,-8.47973649400002));
#169463=CARTESIAN_POINT('Ctrl Pts',(6.95040697199994,11.6,-8.47973649400002));
#169464=CARTESIAN_POINT('Ctrl Pts',(6.94938830399995,15.2,-8.47691991200002));
#169465=CARTESIAN_POINT('Ctrl Pts',(6.94938830399995,11.6,-8.47691991200002));
#169466=CARTESIAN_POINT('Ctrl Pts',(6.94836916999994,15.2,-8.47410925300002));
#169467=CARTESIAN_POINT('Ctrl Pts',(6.94836916999994,11.6,-8.47410925300002));
#169468=CARTESIAN_POINT('Ctrl Pts',(6.94734957799994,15.2,-8.47130452200001));
#169469=CARTESIAN_POINT('Ctrl Pts',(6.94734957799994,11.6,-8.47130452200001));
#169470=CARTESIAN_POINT('Ctrl Pts',(6.94632954299994,15.2,-8.46850572500001));
#169471=CARTESIAN_POINT('Ctrl Pts',(6.94632954299994,11.6,-8.46850572500001));
#169472=CARTESIAN_POINT('Ctrl Pts',(6.94530907199994,15.2,-8.46571286900001));
#169473=CARTESIAN_POINT('Ctrl Pts',(6.94530907199994,11.6,-8.46571286900001));
#169474=CARTESIAN_POINT('Ctrl Pts',(6.94428817599994,15.2,-8.46292596000002));
#169475=CARTESIAN_POINT('Ctrl Pts',(6.94428817599994,11.6,-8.46292596000002));
#169476=CARTESIAN_POINT('Ctrl Pts',(6.94326686599994,15.2,-8.46014500600001));
#169477=CARTESIAN_POINT('Ctrl Pts',(6.94326686599994,11.6,-8.46014500600001));
#169478=CARTESIAN_POINT('Ctrl Pts',(6.94224515399994,15.2,-8.45737001200002));
#169479=CARTESIAN_POINT('Ctrl Pts',(6.94224515399994,11.6,-8.45737001200002));
#169480=CARTESIAN_POINT('Ctrl Pts',(6.94122304799994,15.2,-8.45460098400002));
#169481=CARTESIAN_POINT('Ctrl Pts',(6.94122304799994,11.6,-8.45460098400002));
#169482=CARTESIAN_POINT('Ctrl Pts',(6.94020055999995,15.2,-8.45183793000002));
#169483=CARTESIAN_POINT('Ctrl Pts',(6.94020055999995,11.6,-8.45183793000002));
#169484=CARTESIAN_POINT('Ctrl Pts',(6.93917770099994,15.2,-8.44908085600002));
#169485=CARTESIAN_POINT('Ctrl Pts',(6.93917770099994,11.6,-8.44908085600002));
#169486=CARTESIAN_POINT('Ctrl Pts',(6.93815448099994,15.2,-8.44632976900002));
#169487=CARTESIAN_POINT('Ctrl Pts',(6.93815448099994,11.6,-8.44632976900002));
#169488=CARTESIAN_POINT('Ctrl Pts',(6.93713091199994,15.2,-8.44358467400001));
#169489=CARTESIAN_POINT('Ctrl Pts',(6.93713091199994,11.6,-8.44358467400001));
#169490=CARTESIAN_POINT('Ctrl Pts',(6.93610700299994,15.2,-8.44084557900001));
#169491=CARTESIAN_POINT('Ctrl Pts',(6.93610700299994,11.6,-8.44084557900001));
#169492=CARTESIAN_POINT('Ctrl Pts',(6.93508276499994,15.2,-8.43811248900002));
#169493=CARTESIAN_POINT('Ctrl Pts',(6.93508276499994,11.6,-8.43811248900002));
#169494=CARTESIAN_POINT('Ctrl Pts',(6.93405820999994,15.2,-8.43538541100001));
#169495=CARTESIAN_POINT('Ctrl Pts',(6.93405820999994,11.6,-8.43538541100001));
#169496=CARTESIAN_POINT('Ctrl Pts',(6.93303334799994,15.2,-8.43266435400002));
#169497=CARTESIAN_POINT('Ctrl Pts',(6.93303334799994,11.6,-8.43266435400002));
#169498=CARTESIAN_POINT('Ctrl Pts',(6.93200819099994,15.2,-8.42994932100002));
#169499=CARTESIAN_POINT('Ctrl Pts',(6.93200819099994,11.6,-8.42994932100002));
#169500=CARTESIAN_POINT('Ctrl Pts',(6.93098274699994,15.2,-8.42724032100002));
#169501=CARTESIAN_POINT('Ctrl Pts',(6.93098274699994,11.6,-8.42724032100002));
#169502=CARTESIAN_POINT('Ctrl Pts',(6.92995702999994,15.2,-8.42453735900002));
#169503=CARTESIAN_POINT('Ctrl Pts',(6.92995702999994,11.6,-8.42453735900002));
#169504=CARTESIAN_POINT('Ctrl Pts',(6.92893105099994,15.2,-8.42184044300001));
#169505=CARTESIAN_POINT('Ctrl Pts',(6.92893105099994,11.6,-8.42184044300001));
#169506=CARTESIAN_POINT('Ctrl Pts',(6.92790481799994,15.2,-8.41914957800002));
#169507=CARTESIAN_POINT('Ctrl Pts',(6.92790481799994,11.6,-8.41914957800002));
#169508=CARTESIAN_POINT('Ctrl Pts',(6.92687834499995,15.2,-8.41646477200002));
#169509=CARTESIAN_POINT('Ctrl Pts',(6.92687834499995,11.6,-8.41646477200002));
#169510=CARTESIAN_POINT('Ctrl Pts',(6.92585164099994,15.2,-8.41378603000001));
#169511=CARTESIAN_POINT('Ctrl Pts',(6.92585164099994,11.6,-8.41378603000001));
#169512=CARTESIAN_POINT('Ctrl Pts',(6.92482471899995,15.2,-8.41111336100001));
#169513=CARTESIAN_POINT('Ctrl Pts',(6.92482471899995,11.6,-8.41111336100001));
#169514=CARTESIAN_POINT('Ctrl Pts',(6.92379758999994,15.2,-8.40844676800002));
#169515=CARTESIAN_POINT('Ctrl Pts',(6.92379758999994,11.6,-8.40844676800002));
#169516=CARTESIAN_POINT('Ctrl Pts',(6.92277026199994,15.2,-8.40578626200001));
#169517=CARTESIAN_POINT('Ctrl Pts',(6.92277026199994,11.6,-8.40578626200001));
#169518=CARTESIAN_POINT('Ctrl Pts',(6.92174274999994,15.2,-8.40313184700002));
#169519=CARTESIAN_POINT('Ctrl Pts',(6.92174274999994,11.6,-8.40313184700002));
#169520=CARTESIAN_POINT('Ctrl Pts',(6.92071506399994,15.2,-8.40048352900002));
#169521=CARTESIAN_POINT('Ctrl Pts',(6.92071506399994,11.6,-8.40048352900002));
#169522=CARTESIAN_POINT('Ctrl Pts',(6.91968721499994,15.2,-8.39784131600002));
#169523=CARTESIAN_POINT('Ctrl Pts',(6.91968721499994,11.6,-8.39784131600002));
#169524=CARTESIAN_POINT('Ctrl Pts',(6.91865921499994,15.2,-8.39520521500001));
#169525=CARTESIAN_POINT('Ctrl Pts',(6.91865921499994,11.6,-8.39520521500001));
#169526=CARTESIAN_POINT('Ctrl Pts',(6.91763107299994,15.2,-8.39257523200001));
#169527=CARTESIAN_POINT('Ctrl Pts',(6.91763107299994,11.6,-8.39257523200001));
#169528=CARTESIAN_POINT('Ctrl Pts',(6.91660280299994,15.2,-8.38995137300002));
#169529=CARTESIAN_POINT('Ctrl Pts',(6.91660280299994,11.6,-8.38995137300002));
#169530=CARTESIAN_POINT('Ctrl Pts',(6.91557441499994,15.2,-8.38733364600002));
#169531=CARTESIAN_POINT('Ctrl Pts',(6.91557441499994,11.6,-8.38733364600002));
#169532=CARTESIAN_POINT('Ctrl Pts',(6.91454591999995,15.2,-8.38472205600001));
#169533=CARTESIAN_POINT('Ctrl Pts',(6.91454591999995,11.6,-8.38472205600001));
#169534=CARTESIAN_POINT('Ctrl Pts',(6.91351733199994,15.2,-8.38211661100001));
#169535=CARTESIAN_POINT('Ctrl Pts',(6.91351733199994,11.6,-8.38211661100001));
#169536=CARTESIAN_POINT('Ctrl Pts',(6.91248865999994,15.2,-8.37951731700001));
#169537=CARTESIAN_POINT('Ctrl Pts',(6.91248865999994,11.6,-8.37951731700001));
#169538=CARTESIAN_POINT('Ctrl Pts',(6.91145991499994,15.2,-8.37692418200002));
#169539=CARTESIAN_POINT('Ctrl Pts',(6.91145991499994,11.6,-8.37692418200002));
#169540=CARTESIAN_POINT('Ctrl Pts',(6.91043111099994,15.2,-8.37433721000002));
#169541=CARTESIAN_POINT('Ctrl Pts',(6.91043111099994,11.6,-8.37433721000002));
#169542=CARTESIAN_POINT('Ctrl Pts',(6.90940225899995,15.2,-8.37175641100002));
#169543=CARTESIAN_POINT('Ctrl Pts',(6.90940225899995,11.6,-8.37175641100002));
#169544=CARTESIAN_POINT('Ctrl Pts',(6.90837336899994,15.2,-8.36918179000002));
#169545=CARTESIAN_POINT('Ctrl Pts',(6.90837336899994,11.6,-8.36918179000002));
#169546=CARTESIAN_POINT('Ctrl Pts',(6.90734445199994,15.2,-8.36661335300001));
#169547=CARTESIAN_POINT('Ctrl Pts',(6.90734445199994,11.6,-8.36661335300001));
#169548=CARTESIAN_POINT('Ctrl Pts',(6.90631552399994,15.2,-8.36405110800002));
#169549=CARTESIAN_POINT('Ctrl Pts',(6.90631552399994,11.6,-8.36405110800002));
#169550=CARTESIAN_POINT('Ctrl Pts',(6.90528659299994,15.2,-8.36149506200002));
#169551=CARTESIAN_POINT('Ctrl Pts',(6.90528659299994,11.6,-8.36149506200002));
#169552=CARTESIAN_POINT('Ctrl Pts',(6.90425767199994,15.2,-8.35894522000002));
#169553=CARTESIAN_POINT('Ctrl Pts',(6.90425767199994,11.6,-8.35894522000002));
#169554=CARTESIAN_POINT('Ctrl Pts',(6.90322877199994,15.2,-8.35640159100001));
#169555=CARTESIAN_POINT('Ctrl Pts',(6.90322877199994,11.6,-8.35640159100001));
#169556=CARTESIAN_POINT('Ctrl Pts',(6.90219990499994,15.2,-8.35386418100001));
#169557=CARTESIAN_POINT('Ctrl Pts',(6.90219990499994,11.6,-8.35386418100001));
#169558=CARTESIAN_POINT('Ctrl Pts',(6.90117108399994,15.2,-8.35133299500002));
#169559=CARTESIAN_POINT('Ctrl Pts',(6.90117108399994,11.6,-8.35133299500002));
#169560=CARTESIAN_POINT('Ctrl Pts',(6.90014232099994,15.2,-8.34880804200001));
#169561=CARTESIAN_POINT('Ctrl Pts',(6.90014232099994,11.6,-8.34880804200001));
#169562=CARTESIAN_POINT('Ctrl Pts',(6.89911362499994,15.2,-8.34628932700002));
#169563=CARTESIAN_POINT('Ctrl Pts',(6.89911362499994,11.6,-8.34628932700002));
#169564=CARTESIAN_POINT('Ctrl Pts',(6.89808501099994,15.2,-8.34377685900002));
#169565=CARTESIAN_POINT('Ctrl Pts',(6.89808501099994,11.6,-8.34377685900002));
#169566=CARTESIAN_POINT('Ctrl Pts',(6.89705648999994,15.2,-8.34127064300001));
#169567=CARTESIAN_POINT('Ctrl Pts',(6.89705648999994,11.6,-8.34127064300001));
#169568=CARTESIAN_POINT('Ctrl Pts',(6.89602807299995,15.2,-8.33877068600002));
#169569=CARTESIAN_POINT('Ctrl Pts',(6.89602807299995,11.6,-8.33877068600002));
#169570=CARTESIAN_POINT('Ctrl Pts',(6.89499977499994,15.2,-8.33627699600001));
#169571=CARTESIAN_POINT('Ctrl Pts',(6.89499977499994,11.6,-8.33627699600001));
#169572=CARTESIAN_POINT('Ctrl Pts',(6.89397160499994,15.2,-8.33378957900001));
#169573=CARTESIAN_POINT('Ctrl Pts',(6.89397160499994,11.6,-8.33378957900001));
#169574=CARTESIAN_POINT('Ctrl Pts',(6.89294357699994,15.2,-8.33130844200002));
#169575=CARTESIAN_POINT('Ctrl Pts',(6.89294357699994,11.6,-8.33130844200002));
#169576=CARTESIAN_POINT('Ctrl Pts',(6.89191570099994,15.2,-8.32883359100002));
#169577=CARTESIAN_POINT('Ctrl Pts',(6.89191570099994,11.6,-8.32883359100002));
#169578=CARTESIAN_POINT('Ctrl Pts',(6.89088799199994,15.2,-8.32636503500002));
#169579=CARTESIAN_POINT('Ctrl Pts',(6.89088799199994,11.6,-8.32636503500002));
#169580=CARTESIAN_POINT('Ctrl Pts',(6.88986046099994,15.2,-8.32390277900002));
#169581=CARTESIAN_POINT('Ctrl Pts',(6.88986046099994,11.6,-8.32390277900002));
#169582=CARTESIAN_POINT('Ctrl Pts',(6.88883311899994,15.2,-8.32144682900001));
#169583=CARTESIAN_POINT('Ctrl Pts',(6.88883311899994,11.6,-8.32144682900001));
#169584=CARTESIAN_POINT('Ctrl Pts',(6.88780597999994,15.2,-8.31899719600001));
#169585=CARTESIAN_POINT('Ctrl Pts',(6.88780597999994,11.6,-8.31899719600001));
#169586=CARTESIAN_POINT('Ctrl Pts',(6.88677905699994,15.2,-8.31655388200002));
#169587=CARTESIAN_POINT('Ctrl Pts',(6.88677905699994,11.6,-8.31655388200002));
#169588=CARTESIAN_POINT('Ctrl Pts',(6.88575235999994,15.2,-8.31411689700002));
#169589=CARTESIAN_POINT('Ctrl Pts',(6.88575235999994,11.6,-8.31411689700002));
#169590=CARTESIAN_POINT('Ctrl Pts',(6.88472590399994,15.2,-8.31168624500001));
#169591=CARTESIAN_POINT('Ctrl Pts',(6.88472590399994,11.6,-8.31168624500001));
#169592=CARTESIAN_POINT('Ctrl Pts',(6.88369969899994,15.2,-8.30926193800002));
#169593=CARTESIAN_POINT('Ctrl Pts',(6.88369969899994,11.6,-8.30926193800002));
#169594=CARTESIAN_POINT('Ctrl Pts',(6.88267375899994,15.2,-8.30684397800002));
#169595=CARTESIAN_POINT('Ctrl Pts',(6.88267375899994,11.6,-8.30684397800002));
#169596=CARTESIAN_POINT('Ctrl Pts',(6.88164809599995,15.2,-8.30443237500001));
#169597=CARTESIAN_POINT('Ctrl Pts',(6.88164809599995,11.6,-8.30443237500001));
#169598=CARTESIAN_POINT('Ctrl Pts',(6.88062272399995,15.2,-8.30202713300002));
#169599=CARTESIAN_POINT('Ctrl Pts',(6.88062272399995,11.6,-8.30202713300002));
#169600=CARTESIAN_POINT('Ctrl Pts',(6.87959765299994,15.2,-8.29962826200001));
#169601=CARTESIAN_POINT('Ctrl Pts',(6.87959765299994,11.6,-8.29962826200001));
#169602=CARTESIAN_POINT('Ctrl Pts',(6.87857289699994,15.2,-8.29723576700001));
#169603=CARTESIAN_POINT('Ctrl Pts',(6.87857289699994,11.6,-8.29723576700001));
#169604=CARTESIAN_POINT('Ctrl Pts',(6.87754846999994,15.2,-8.29484965700001));
#169605=CARTESIAN_POINT('Ctrl Pts',(6.87754846999994,11.6,-8.29484965700001));
#169606=CARTESIAN_POINT('Ctrl Pts',(6.87652438199994,15.2,-8.29246993600002));
#169607=CARTESIAN_POINT('Ctrl Pts',(6.87652438199994,11.6,-8.29246993600002));
#169608=CARTESIAN_POINT('Ctrl Pts',(6.87550064899995,15.2,-8.29009661300002));
#169609=CARTESIAN_POINT('Ctrl Pts',(6.87550064899995,11.6,-8.29009661300002));
#169610=CARTESIAN_POINT('Ctrl Pts',(6.87447728099994,15.2,-8.28772969500001));
#169611=CARTESIAN_POINT('Ctrl Pts',(6.87447728099994,11.6,-8.28772969500001));
#169612=CARTESIAN_POINT('Ctrl Pts',(6.87345429199994,15.2,-8.28536918900001));
#169613=CARTESIAN_POINT('Ctrl Pts',(6.87345429199994,11.6,-8.28536918900001));
#169614=CARTESIAN_POINT('Ctrl Pts',(6.87243169499994,15.2,-8.28301510100001));
#169615=CARTESIAN_POINT('Ctrl Pts',(6.87243169499994,11.6,-8.28301510100001));
#169616=CARTESIAN_POINT('Ctrl Pts',(6.87140950299994,15.2,-8.28066743900001));
#169617=CARTESIAN_POINT('Ctrl Pts',(6.87140950299994,11.6,-8.28066743900001));
#169618=CARTESIAN_POINT('Ctrl Pts',(6.87038772899994,15.2,-8.27832621000002));
#169619=CARTESIAN_POINT('Ctrl Pts',(6.87038772899994,11.6,-8.27832621000002));
#169620=CARTESIAN_POINT('Ctrl Pts',(6.86936638499994,15.2,-8.27599142100001));
#169621=CARTESIAN_POINT('Ctrl Pts',(6.86936638499994,11.6,-8.27599142100001));
#169622=CARTESIAN_POINT('Ctrl Pts',(6.86834548499994,15.2,-8.27366307800002));
#169623=CARTESIAN_POINT('Ctrl Pts',(6.86834548499994,11.6,-8.27366307800002));
#169624=CARTESIAN_POINT('Ctrl Pts',(6.86732504299994,15.2,-8.27134119000002));
#169625=CARTESIAN_POINT('Ctrl Pts',(6.86732504299994,11.6,-8.27134119000002));
#169626=CARTESIAN_POINT('Ctrl Pts',(6.86630506999995,15.2,-8.26902576200002));
#169627=CARTESIAN_POINT('Ctrl Pts',(6.86630506999995,11.6,-8.26902576200002));
#169628=CARTESIAN_POINT('Ctrl Pts',(6.86528557999995,15.2,-8.26671680300001));
#169629=CARTESIAN_POINT('Ctrl Pts',(6.86528557999995,11.6,-8.26671680300001));
#169630=CARTESIAN_POINT('Ctrl Pts',(6.86426658699994,15.2,-8.26441431900001));
#169631=CARTESIAN_POINT('Ctrl Pts',(6.86426658699994,11.6,-8.26441431900001));
#169632=CARTESIAN_POINT('Ctrl Pts',(6.86324810299995,15.2,-8.26211831700002));
#169633=CARTESIAN_POINT('Ctrl Pts',(6.86324810299995,11.6,-8.26211831700002));
#169634=CARTESIAN_POINT('Ctrl Pts',(6.86223014199994,15.2,-8.25982880500002));
#169635=CARTESIAN_POINT('Ctrl Pts',(6.86223014199994,11.6,-8.25982880500002));
#169636=CARTESIAN_POINT('Ctrl Pts',(6.86121271699994,15.2,-8.25754578900002));
#169637=CARTESIAN_POINT('Ctrl Pts',(6.86121271699994,11.6,-8.25754578900002));
#169638=CARTESIAN_POINT('Ctrl Pts',(6.86019584299994,15.2,-8.25526927700002));
#169639=CARTESIAN_POINT('Ctrl Pts',(6.86019584299994,11.6,-8.25526927700002));
#169640=CARTESIAN_POINT('Ctrl Pts',(6.85917953099994,15.2,-8.25299927600001));
#169641=CARTESIAN_POINT('Ctrl Pts',(6.85917953099994,11.6,-8.25299927600001));
#169642=CARTESIAN_POINT('Ctrl Pts',(6.85816379599994,15.2,-8.25073579300001));
#169643=CARTESIAN_POINT('Ctrl Pts',(6.85816379599994,11.6,-8.25073579300001));
#169644=CARTESIAN_POINT('Ctrl Pts',(6.85714865199994,15.2,-8.24847883600001));
#169645=CARTESIAN_POINT('Ctrl Pts',(6.85714865199994,11.6,-8.24847883600001));
#169646=CARTESIAN_POINT('Ctrl Pts',(6.85613410999995,15.2,-8.24622841000001));
#169647=CARTESIAN_POINT('Ctrl Pts',(6.85613410999995,11.6,-8.24622841000001));
#169648=CARTESIAN_POINT('Ctrl Pts',(6.85512018599994,15.2,-8.24398452500001));
#169649=CARTESIAN_POINT('Ctrl Pts',(6.85512018599994,11.6,-8.24398452500001));
#169650=CARTESIAN_POINT('Ctrl Pts',(6.85410689299994,15.2,-8.24174718600002));
#169651=CARTESIAN_POINT('Ctrl Pts',(6.85410689299994,11.6,-8.24174718600002));
#169652=CARTESIAN_POINT('Ctrl Pts',(6.85309424499994,15.2,-8.23951640200002));
#169653=CARTESIAN_POINT('Ctrl Pts',(6.85309424499994,11.6,-8.23951640200002));
#169654=CARTESIAN_POINT('Ctrl Pts',(6.85208225499994,15.2,-8.23729217900001));
#169655=CARTESIAN_POINT('Ctrl Pts',(6.85208225499994,11.6,-8.23729217900001));
#169656=CARTESIAN_POINT('Ctrl Pts',(6.85107093599994,15.2,-8.23507452400002));
#169657=CARTESIAN_POINT('Ctrl Pts',(6.85107093599994,11.6,-8.23507452400002));
#169658=CARTESIAN_POINT('Ctrl Pts',(6.85006030399994,15.2,-8.23286344400002));
#169659=CARTESIAN_POINT('Ctrl Pts',(6.85006030399994,11.6,-8.23286344400002));
#169660=CARTESIAN_POINT('Ctrl Pts',(6.84905037099995,15.2,-8.23065895000001));
#169661=CARTESIAN_POINT('Ctrl Pts',(6.84905037099995,11.6,-8.23065895000001));
#169662=CARTESIAN_POINT('Ctrl Pts',(6.84804115199994,15.2,-8.22846104400002));
#169663=CARTESIAN_POINT('Ctrl Pts',(6.84804115199994,11.6,-8.22846104400002));
#169664=CARTESIAN_POINT('Ctrl Pts',(6.84703265999994,15.2,-8.22626973500002));
#169665=CARTESIAN_POINT('Ctrl Pts',(6.84703265999994,11.6,-8.22626973500002));
#169666=CARTESIAN_POINT('Ctrl Pts',(6.84602490999994,15.2,-8.22408503200002));
#169667=CARTESIAN_POINT('Ctrl Pts',(6.84602490999994,11.6,-8.22408503200002));
#169668=CARTESIAN_POINT('Ctrl Pts',(6.84501791499994,15.2,-8.22190694200001));
#169669=CARTESIAN_POINT('Ctrl Pts',(6.84501791499994,11.6,-8.22190694200001));
#169670=CARTESIAN_POINT('Ctrl Pts',(6.84401168999995,15.2,-8.21973547000002));
#169671=CARTESIAN_POINT('Ctrl Pts',(6.84401168999995,11.6,-8.21973547000002));
#169672=CARTESIAN_POINT('Ctrl Pts',(6.84300624899994,15.2,-8.21757062500001));
#169673=CARTESIAN_POINT('Ctrl Pts',(6.84300624899994,11.6,-8.21757062500001));
#169674=CARTESIAN_POINT('Ctrl Pts',(6.84200160499994,15.2,-8.21541241600002));
#169675=CARTESIAN_POINT('Ctrl Pts',(6.84200160499994,11.6,-8.21541241600002));
#169676=CARTESIAN_POINT('Ctrl Pts',(6.84099777399994,15.2,-8.21326084700001));
#169677=CARTESIAN_POINT('Ctrl Pts',(6.84099777399994,11.6,-8.21326084700001));
#169678=CARTESIAN_POINT('Ctrl Pts',(6.83999476999994,15.2,-8.21111592700002));
#169679=CARTESIAN_POINT('Ctrl Pts',(6.83999476999994,11.6,-8.21111592700002));
#169680=CARTESIAN_POINT('Ctrl Pts',(6.83899260499994,15.2,-8.20897766300002));
#169681=CARTESIAN_POINT('Ctrl Pts',(6.83899260499994,11.6,-8.20897766300002));
#169682=CARTESIAN_POINT('Ctrl Pts',(6.83799129699994,15.2,-8.20684606400001));
#169683=CARTESIAN_POINT('Ctrl Pts',(6.83799129699994,11.6,-8.20684606400001));
#169684=CARTESIAN_POINT('Ctrl Pts',(6.83699085699994,15.2,-8.20472113600001));
#169685=CARTESIAN_POINT('Ctrl Pts',(6.83699085699994,11.6,-8.20472113600001));
#169686=CARTESIAN_POINT('Ctrl Pts',(6.83599130199994,15.2,-8.20260288400002));
#169687=CARTESIAN_POINT('Ctrl Pts',(6.83599130199994,11.6,-8.20260288400002));
#169688=CARTESIAN_POINT('Ctrl Pts',(6.83499264499994,15.2,-8.20049132000002));
#169689=CARTESIAN_POINT('Ctrl Pts',(6.83499264499994,11.6,-8.20049132000002));
#169690=CARTESIAN_POINT('Ctrl Pts',(6.83399489999994,15.2,-8.19838644900001));
#169691=CARTESIAN_POINT('Ctrl Pts',(6.83399489999994,11.6,-8.19838644900001));
#169692=CARTESIAN_POINT('Ctrl Pts',(6.83299808299994,15.2,-8.19628827900001));
#169693=CARTESIAN_POINT('Ctrl Pts',(6.83299808299994,11.6,-8.19628827900001));
#169694=CARTESIAN_POINT('Ctrl Pts',(6.83200220999994,15.2,-8.19419681600002));
#169695=CARTESIAN_POINT('Ctrl Pts',(6.83200220999994,11.6,-8.19419681600002));
#169696=CARTESIAN_POINT('Ctrl Pts',(6.83100729199994,15.2,-8.19211207100001));
#169697=CARTESIAN_POINT('Ctrl Pts',(6.83100729199994,11.6,-8.19211207100001));
#169698=CARTESIAN_POINT('Ctrl Pts',(6.83001334499994,15.2,-8.19003404700002));
#169699=CARTESIAN_POINT('Ctrl Pts',(6.83001334499994,11.6,-8.19003404700002));
#169700=CARTESIAN_POINT('Ctrl Pts',(6.82902038699994,15.2,-8.18796275400001));
#169701=CARTESIAN_POINT('Ctrl Pts',(6.82902038699994,11.6,-8.18796275400001));
#169702=CARTESIAN_POINT('Ctrl Pts',(6.82802842799994,15.2,-8.18589820000001));
#169703=CARTESIAN_POINT('Ctrl Pts',(6.82802842799994,11.6,-8.18589820000001));
#169704=CARTESIAN_POINT('Ctrl Pts',(6.82703748599994,15.2,-8.18384039100001));
#169705=CARTESIAN_POINT('Ctrl Pts',(6.82703748599994,11.6,-8.18384039100001));
#169706=CARTESIAN_POINT('Ctrl Pts',(6.82604757499995,15.2,-8.18178933600001));
#169707=CARTESIAN_POINT('Ctrl Pts',(6.82604757499995,11.6,-8.18178933600001));
#169708=CARTESIAN_POINT('Ctrl Pts',(6.82505870999995,15.2,-8.17974504100001));
#169709=CARTESIAN_POINT('Ctrl Pts',(6.82505870999995,11.6,-8.17974504100001));
#169710=CARTESIAN_POINT('Ctrl Pts',(6.82407090599995,15.2,-8.17770751500002));
#169711=CARTESIAN_POINT('Ctrl Pts',(6.82407090599995,11.6,-8.17770751500002));
#169712=CARTESIAN_POINT('Ctrl Pts',(6.82308417899994,15.2,-8.17567676500002));
#169713=CARTESIAN_POINT('Ctrl Pts',(6.82308417899994,11.6,-8.17567676500002));
#169714=CARTESIAN_POINT('Ctrl Pts',(6.82209854199994,15.2,-8.17365279700002));
#169715=CARTESIAN_POINT('Ctrl Pts',(6.82209854199994,11.6,-8.17365279700002));
#169716=CARTESIAN_POINT('Ctrl Pts',(6.82111401199994,15.2,-8.17163562200001));
#169717=CARTESIAN_POINT('Ctrl Pts',(6.82111401199994,11.6,-8.17163562200001));
#169718=CARTESIAN_POINT('Ctrl Pts',(6.82013060499994,15.2,-8.16962524400001));
#169719=CARTESIAN_POINT('Ctrl Pts',(6.82013060499994,11.6,-8.16962524400001));
#169720=CARTESIAN_POINT('Ctrl Pts',(6.81914833299994,15.2,-8.16762167300002));
#169721=CARTESIAN_POINT('Ctrl Pts',(6.81914833299994,11.6,-8.16762167300002));
#169722=CARTESIAN_POINT('Ctrl Pts',(6.81816721399994,15.2,-8.16562491600001));
#169723=CARTESIAN_POINT('Ctrl Pts',(6.81816721399994,11.6,-8.16562491600001));
#169724=CARTESIAN_POINT('Ctrl Pts',(6.81718726299994,15.2,-8.16363498000002));
#169725=CARTESIAN_POINT('Ctrl Pts',(6.81718726299994,11.6,-8.16363498000002));
#169726=CARTESIAN_POINT('Ctrl Pts',(6.81620849499994,15.2,-8.16165187500001));
#169727=CARTESIAN_POINT('Ctrl Pts',(6.81620849499994,11.6,-8.16165187500001));
#169728=CARTESIAN_POINT('Ctrl Pts',(6.81523092699994,15.2,-8.15967560500001));
#169729=CARTESIAN_POINT('Ctrl Pts',(6.81523092699994,11.6,-8.15967560500001));
#169730=CARTESIAN_POINT('Ctrl Pts',(6.81425457199994,15.2,-8.15770618000002));
#169731=CARTESIAN_POINT('Ctrl Pts',(6.81425457199994,11.6,-8.15770618000002));
#169732=CARTESIAN_POINT('Ctrl Pts',(6.81327944699994,15.2,-8.15574360800002));
#169733=CARTESIAN_POINT('Ctrl Pts',(6.81327944699994,11.6,-8.15574360800002));
#169734=CARTESIAN_POINT('Ctrl Pts',(6.81230556799994,15.2,-8.15378789600001));
#169735=CARTESIAN_POINT('Ctrl Pts',(6.81230556799994,11.6,-8.15378789600001));
#169736=CARTESIAN_POINT('Ctrl Pts',(6.81133295099994,15.2,-8.15183905000002));
#169737=CARTESIAN_POINT('Ctrl Pts',(6.81133295099994,11.6,-8.15183905000002));
#169738=CARTESIAN_POINT('Ctrl Pts',(6.81036160899994,15.2,-8.14989708200001));
#169739=CARTESIAN_POINT('Ctrl Pts',(6.81036160899994,11.6,-8.14989708200001));
#169740=CARTESIAN_POINT('Ctrl Pts',(6.80939156199994,15.2,-8.14796199600002));
#169741=CARTESIAN_POINT('Ctrl Pts',(6.80939156199994,11.6,-8.14796199600002));
#169742=CARTESIAN_POINT('Ctrl Pts',(6.80842282199994,15.2,-8.14603380000002));
#169743=CARTESIAN_POINT('Ctrl Pts',(6.80842282199994,11.6,-8.14603380000002));
#169744=CARTESIAN_POINT('Ctrl Pts',(6.80745540699994,15.2,-8.14411250400001));
#169745=CARTESIAN_POINT('Ctrl Pts',(6.80745540699994,11.6,-8.14411250400001));
#169746=CARTESIAN_POINT('Ctrl Pts',(6.80648933299994,15.2,-8.14219811500001));
#169747=CARTESIAN_POINT('Ctrl Pts',(6.80648933299994,11.6,-8.14219811500001));
#169748=CARTESIAN_POINT('Ctrl Pts',(6.80552461599994,15.2,-8.14029063900002));
#169749=CARTESIAN_POINT('Ctrl Pts',(6.80552461599994,11.6,-8.14029063900002));
#169750=CARTESIAN_POINT('Ctrl Pts',(6.80456127099994,15.2,-8.13839008500001));
#169751=CARTESIAN_POINT('Ctrl Pts',(6.80456127099994,11.6,-8.13839008500001));
#169752=CARTESIAN_POINT('Ctrl Pts',(6.80359931599994,15.2,-8.13649646300002));
#169753=CARTESIAN_POINT('Ctrl Pts',(6.80359931599994,11.6,-8.13649646300002));
#169754=CARTESIAN_POINT('Ctrl Pts',(6.80263876599994,15.2,-8.13460977800002));
#169755=CARTESIAN_POINT('Ctrl Pts',(6.80263876599994,11.6,-8.13460977800002));
#169756=CARTESIAN_POINT('Ctrl Pts',(6.80167963599994,15.2,-8.13273003800001));
#169757=CARTESIAN_POINT('Ctrl Pts',(6.80167963599994,11.6,-8.13273003800001));
#169758=CARTESIAN_POINT('Ctrl Pts',(6.80072194599994,15.2,-8.13085725200001));
#169759=CARTESIAN_POINT('Ctrl Pts',(6.80072194599994,11.6,-8.13085725200001));
#169760=CARTESIAN_POINT('Ctrl Pts',(6.79976570799994,15.2,-8.12899142800001));
#169761=CARTESIAN_POINT('Ctrl Pts',(6.79976570799994,11.6,-8.12899142800001));
#169762=CARTESIAN_POINT('Ctrl Pts',(6.79881094199994,15.2,-8.12713257400001));
#169763=CARTESIAN_POINT('Ctrl Pts',(6.79881094199994,11.6,-8.12713257400001));
#169764=CARTESIAN_POINT('Ctrl Pts',(6.79785766299994,15.2,-8.12528069600001));
#169765=CARTESIAN_POINT('Ctrl Pts',(6.79785766299994,11.6,-8.12528069600001));
#169766=CARTESIAN_POINT('Ctrl Pts',(6.79690588799994,15.2,-8.12343580400002));
#169767=CARTESIAN_POINT('Ctrl Pts',(6.79690588799994,11.6,-8.12343580400002));
#169768=CARTESIAN_POINT('Ctrl Pts',(6.79595563299995,15.2,-8.12159790600001));
#169769=CARTESIAN_POINT('Ctrl Pts',(6.79595563299995,11.6,-8.12159790600001));
#169770=CARTESIAN_POINT('Ctrl Pts',(6.79500691399994,15.2,-8.11976700800002));
#169771=CARTESIAN_POINT('Ctrl Pts',(6.79500691399994,11.6,-8.11976700800002));
#169772=CARTESIAN_POINT('Ctrl Pts',(6.79405974999994,15.2,-8.11794312000002));
#169773=CARTESIAN_POINT('Ctrl Pts',(6.79405974999994,11.6,-8.11794312000002));
#169774=CARTESIAN_POINT('Ctrl Pts',(6.79311415699994,15.2,-8.11612625000001));
#169775=CARTESIAN_POINT('Ctrl Pts',(6.79311415699994,11.6,-8.11612625000001));
#169776=CARTESIAN_POINT('Ctrl Pts',(6.79217014999994,15.2,-8.11431640400002));
#169777=CARTESIAN_POINT('Ctrl Pts',(6.79217014999994,11.6,-8.11431640400002));
#169778=CARTESIAN_POINT('Ctrl Pts',(6.79122774799994,15.2,-8.11251359100002));
#169779=CARTESIAN_POINT('Ctrl Pts',(6.79122774799994,11.6,-8.11251359100002));
#169780=CARTESIAN_POINT('Ctrl Pts',(6.79028696699994,15.2,-8.11071782000001));
#169781=CARTESIAN_POINT('Ctrl Pts',(6.79028696699994,11.6,-8.11071782000001));
#169782=CARTESIAN_POINT('Ctrl Pts',(6.78934782399994,15.2,-8.10892909900002));
#169783=CARTESIAN_POINT('Ctrl Pts',(6.78934782399994,11.6,-8.10892909900002));
#169784=CARTESIAN_POINT('Ctrl Pts',(6.78841033799994,15.2,-8.10714743400002));
#169785=CARTESIAN_POINT('Ctrl Pts',(6.78841033799994,11.6,-8.10714743400002));
#169786=CARTESIAN_POINT('Ctrl Pts',(6.78747452299994,15.2,-8.10537283700001));
#169787=CARTESIAN_POINT('Ctrl Pts',(6.78747452299994,11.6,-8.10537283700001));
#169788=CARTESIAN_POINT('Ctrl Pts',(6.78654039799994,15.2,-8.10360531100002));
#169789=CARTESIAN_POINT('Ctrl Pts',(6.78654039799994,11.6,-8.10360531100002));
#169790=CARTESIAN_POINT('Ctrl Pts',(6.78560798099994,15.2,-8.10184486900001));
#169791=CARTESIAN_POINT('Ctrl Pts',(6.78560798099994,11.6,-8.10184486900001));
#169792=CARTESIAN_POINT('Ctrl Pts',(6.78467728799995,15.2,-8.10009151600001));
#169793=CARTESIAN_POINT('Ctrl Pts',(6.78467728799995,11.6,-8.10009151600001));
#169794=CARTESIAN_POINT('Ctrl Pts',(6.78374833699994,15.2,-8.09834526200002));
#169795=CARTESIAN_POINT('Ctrl Pts',(6.78374833699994,11.6,-8.09834526200002));
#169796=CARTESIAN_POINT('Ctrl Pts',(6.78282114499994,15.2,-8.09660611400002));
#169797=CARTESIAN_POINT('Ctrl Pts',(6.78282114499994,11.6,-8.09660611400002));
#169798=CARTESIAN_POINT('Ctrl Pts',(6.78189572999995,15.2,-8.09487408000002));
#169799=CARTESIAN_POINT('Ctrl Pts',(6.78189572999995,11.6,-8.09487408000002));
#169800=CARTESIAN_POINT('Ctrl Pts',(6.78097211099994,15.2,-8.09314916800002));
#169801=CARTESIAN_POINT('Ctrl Pts',(6.78097211099994,11.6,-8.09314916800002));
#169802=CARTESIAN_POINT('Ctrl Pts',(6.78005030299994,15.2,-8.09143138900002));
#169803=CARTESIAN_POINT('Ctrl Pts',(6.78005030299994,11.6,-8.09143138900002));
#169804=CARTESIAN_POINT('Ctrl Pts',(6.77913032499994,15.2,-8.08972074800002));
#169805=CARTESIAN_POINT('Ctrl Pts',(6.77913032499994,11.6,-8.08972074800002));
#169806=CARTESIAN_POINT('Ctrl Pts',(6.77821219499994,15.2,-8.08801725500001));
#169807=CARTESIAN_POINT('Ctrl Pts',(6.77821219499994,11.6,-8.08801725500001));
#169808=CARTESIAN_POINT('Ctrl Pts',(6.77729593099994,15.2,-8.08632091800002));
#169809=CARTESIAN_POINT('Ctrl Pts',(6.77729593099994,11.6,-8.08632091800002));
#169810=CARTESIAN_POINT('Ctrl Pts',(6.77638154999994,15.2,-8.08463174500002));
#169811=CARTESIAN_POINT('Ctrl Pts',(6.77638154999994,11.6,-8.08463174500002));
#169812=CARTESIAN_POINT('Ctrl Pts',(6.77546907099994,15.2,-8.08294974400001));
#169813=CARTESIAN_POINT('Ctrl Pts',(6.77546907099994,11.6,-8.08294974400001));
#169814=CARTESIAN_POINT('Ctrl Pts',(6.77455851199994,15.2,-8.08127492400001));
#169815=CARTESIAN_POINT('Ctrl Pts',(6.77455851199994,11.6,-8.08127492400001));
#169816=CARTESIAN_POINT('Ctrl Pts',(6.77364988999994,15.2,-8.07960729300002));
#169817=CARTESIAN_POINT('Ctrl Pts',(6.77364988999994,11.6,-8.07960729300002));
#169818=CARTESIAN_POINT('Ctrl Pts',(6.77274322499994,15.2,-8.07794686000002));
#169819=CARTESIAN_POINT('Ctrl Pts',(6.77274322499994,11.6,-8.07794686000002));
#169820=CARTESIAN_POINT('Ctrl Pts',(6.77183853299994,15.2,-8.07629363200002));
#169821=CARTESIAN_POINT('Ctrl Pts',(6.77183853299994,11.6,-8.07629363200002));
#169822=CARTESIAN_POINT('Ctrl Pts',(6.77093583499994,15.2,-8.07464761900002));
#169823=CARTESIAN_POINT('Ctrl Pts',(6.77093583499994,11.6,-8.07464761900002));
#169824=CARTESIAN_POINT('Ctrl Pts',(6.77003514699994,15.2,-8.07300882800002));
#169825=CARTESIAN_POINT('Ctrl Pts',(6.77003514699994,11.6,-8.07300882800002));
#169826=CARTESIAN_POINT('Ctrl Pts',(6.76913648999995,15.2,-8.07137726900002));
#169827=CARTESIAN_POINT('Ctrl Pts',(6.76913648999995,11.6,-8.07137726900002));
#169828=CARTESIAN_POINT('Ctrl Pts',(6.76823988099994,15.2,-8.06975294900001));
#169829=CARTESIAN_POINT('Ctrl Pts',(6.76823988099994,11.6,-8.06975294900001));
#169830=CARTESIAN_POINT('Ctrl Pts',(6.76734533799995,15.2,-8.06813587700002));
#169831=CARTESIAN_POINT('Ctrl Pts',(6.76734533799995,11.6,-8.06813587700002));
#169832=CARTESIAN_POINT('Ctrl Pts',(6.76645288099994,15.2,-8.06652606100002));
#169833=CARTESIAN_POINT('Ctrl Pts',(6.76645288099994,11.6,-8.06652606100002));
#169834=CARTESIAN_POINT('Ctrl Pts',(6.76556252799994,15.2,-8.06492351100001));
#169835=CARTESIAN_POINT('Ctrl Pts',(6.76556252799994,11.6,-8.06492351100001));
#169836=CARTESIAN_POINT('Ctrl Pts',(6.76467429899994,15.2,-8.06332823600002));
#169837=CARTESIAN_POINT('Ctrl Pts',(6.76467429899994,11.6,-8.06332823600002));
#169838=CARTESIAN_POINT('Ctrl Pts',(6.76378821099994,15.2,-8.06174024100001));
#169839=CARTESIAN_POINT('Ctrl Pts',(6.76378821099994,11.6,-8.06174024100001));
#169840=CARTESIAN_POINT('Ctrl Pts',(6.76290428599994,15.2,-8.06015953800001));
#169841=CARTESIAN_POINT('Ctrl Pts',(6.76290428599994,11.6,-8.06015953800001));
#169842=CARTESIAN_POINT('Ctrl Pts',(6.76202253899994,15.2,-8.05858613400002));
#169843=CARTESIAN_POINT('Ctrl Pts',(6.76202253899994,11.6,-8.05858613400002));
#169844=CARTESIAN_POINT('Ctrl Pts',(6.76114299199994,15.2,-8.05702003800001));
#169845=CARTESIAN_POINT('Ctrl Pts',(6.76114299199994,11.6,-8.05702003800001));
#169846=CARTESIAN_POINT('Ctrl Pts',(6.76026566399995,15.2,-8.05546125900002));
#169847=CARTESIAN_POINT('Ctrl Pts',(6.76026566399995,11.6,-8.05546125900002));
#169848=CARTESIAN_POINT('Ctrl Pts',(6.75939057299995,15.2,-8.05390980500002));
#169849=CARTESIAN_POINT('Ctrl Pts',(6.75939057299995,11.6,-8.05390980500002));
#169850=CARTESIAN_POINT('Ctrl Pts',(6.75851773999994,15.2,-8.05236568400002));
#169851=CARTESIAN_POINT('Ctrl Pts',(6.75851773999994,11.6,-8.05236568400002));
#169852=CARTESIAN_POINT('Ctrl Pts',(6.75764718299994,15.2,-8.05082890700002));
#169853=CARTESIAN_POINT('Ctrl Pts',(6.75764718299994,11.6,-8.05082890700002));
#169854=CARTESIAN_POINT('Ctrl Pts',(6.75677892299994,15.2,-8.04929948100002));
#169855=CARTESIAN_POINT('Ctrl Pts',(6.75677892299994,11.6,-8.04929948100002));
#169856=CARTESIAN_POINT('Ctrl Pts',(6.75591297799994,15.2,-8.04777741600001));
#169857=CARTESIAN_POINT('Ctrl Pts',(6.75591297799994,11.6,-8.04777741600001));
#169858=CARTESIAN_POINT('Ctrl Pts',(6.75504936899994,15.2,-8.04626271800002));
#169859=CARTESIAN_POINT('Ctrl Pts',(6.75504936899994,11.6,-8.04626271800002));
#169860=CARTESIAN_POINT('Ctrl Pts',(6.75418811399994,15.2,-8.04475539900002));
#169861=CARTESIAN_POINT('Ctrl Pts',(6.75418811399994,11.6,-8.04475539900002));
#169862=CARTESIAN_POINT('Ctrl Pts',(6.75332923499994,15.2,-8.04325546600002));
#169863=CARTESIAN_POINT('Ctrl Pts',(6.75332923499994,11.6,-8.04325546600002));
#169864=CARTESIAN_POINT('Ctrl Pts',(6.75247275099994,15.2,-8.04176292900001));
#169865=CARTESIAN_POINT('Ctrl Pts',(6.75247275099994,11.6,-8.04176292900001));
#169866=CARTESIAN_POINT('Ctrl Pts',(6.75161868199995,15.2,-8.04027779500002));
#169867=CARTESIAN_POINT('Ctrl Pts',(6.75161868199995,11.6,-8.04027779500002));
#169868=CARTESIAN_POINT('Ctrl Pts',(6.75076704799995,15.2,-8.03880007500002));
#169869=CARTESIAN_POINT('Ctrl Pts',(6.75076704799995,11.6,-8.03880007500002));
#169870=CARTESIAN_POINT('Ctrl Pts',(6.74991786899994,15.2,-8.03732977600001));
#169871=CARTESIAN_POINT('Ctrl Pts',(6.74991786899994,11.6,-8.03732977600001));
#169872=CARTESIAN_POINT('Ctrl Pts',(6.74907116499995,15.2,-8.03586690800002));
#169873=CARTESIAN_POINT('Ctrl Pts',(6.74907116499995,11.6,-8.03586690800002));
#169874=CARTESIAN_POINT('Ctrl Pts',(6.74822695699994,15.2,-8.03441148000001));
#169875=CARTESIAN_POINT('Ctrl Pts',(6.74822695699994,11.6,-8.03441148000001));
#169876=CARTESIAN_POINT('Ctrl Pts',(6.74738526499994,15.2,-8.03296350100002));
#169877=CARTESIAN_POINT('Ctrl Pts',(6.74738526499994,11.6,-8.03296350100002));
#169878=CARTESIAN_POINT('Ctrl Pts',(6.74654610999994,15.2,-8.03152298000001));
#169879=CARTESIAN_POINT('Ctrl Pts',(6.74654610999994,11.6,-8.03152298000001));
#169880=CARTESIAN_POINT('Ctrl Pts',(6.74570951199994,15.2,-8.03008992500001));
#169881=CARTESIAN_POINT('Ctrl Pts',(6.74570951199994,11.6,-8.03008992500001));
#169882=CARTESIAN_POINT('Ctrl Pts',(6.74487549099994,15.2,-8.02866434600002));
#169883=CARTESIAN_POINT('Ctrl Pts',(6.74487549099994,11.6,-8.02866434600002));
#169884=CARTESIAN_POINT('Ctrl Pts',(6.74404406899995,15.2,-8.02724625000002));
#169885=CARTESIAN_POINT('Ctrl Pts',(6.74404406899995,11.6,-8.02724625000002));
#169886=CARTESIAN_POINT('Ctrl Pts',(6.74321526699995,15.2,-8.02583564900001));
#169887=CARTESIAN_POINT('Ctrl Pts',(6.74321526699995,11.6,-8.02583564900001));
#169888=CARTESIAN_POINT('Ctrl Pts',(6.74238910499994,15.2,-8.02443255100002));
#169889=CARTESIAN_POINT('Ctrl Pts',(6.74238910499994,11.6,-8.02443255100002));
#169890=CARTESIAN_POINT('Ctrl Pts',(6.74156560399994,15.2,-8.02303696500001));
#169891=CARTESIAN_POINT('Ctrl Pts',(6.74156560399994,11.6,-8.02303696500001));
#169892=CARTESIAN_POINT('Ctrl Pts',(6.74074478399994,15.2,-8.02164890000002));
#169893=CARTESIAN_POINT('Ctrl Pts',(6.74074478399994,11.6,-8.02164890000002));
#169894=CARTESIAN_POINT('Ctrl Pts',(6.73992666899994,15.2,-8.02026836500002));
#169895=CARTESIAN_POINT('Ctrl Pts',(6.73992666899994,11.6,-8.02026836500002));
#169896=CARTESIAN_POINT('Ctrl Pts',(6.73911127899994,15.2,-8.01889537000001));
#169897=CARTESIAN_POINT('Ctrl Pts',(6.73911127899994,11.6,-8.01889537000001));
#169898=CARTESIAN_POINT('Ctrl Pts',(6.73829863399994,15.2,-8.01752992300001));
#169899=CARTESIAN_POINT('Ctrl Pts',(6.73829863399994,11.6,-8.01752992300001));
#169900=CARTESIAN_POINT('Ctrl Pts',(6.73748875699994,15.2,-8.01617203400001));
#169901=CARTESIAN_POINT('Ctrl Pts',(6.73748875699994,11.6,-8.01617203400001));
#169902=CARTESIAN_POINT('Ctrl Pts',(6.73668166999994,15.2,-8.01482171200002));
#169903=CARTESIAN_POINT('Ctrl Pts',(6.73668166999994,11.6,-8.01482171200002));
#169904=CARTESIAN_POINT('Ctrl Pts',(6.73587739199994,15.2,-8.01347896600002));
#169905=CARTESIAN_POINT('Ctrl Pts',(6.73587739199994,11.6,-8.01347896600002));
#169906=CARTESIAN_POINT('Ctrl Pts',(6.73507594699994,15.2,-8.01214380700002));
#169907=CARTESIAN_POINT('Ctrl Pts',(6.73507594699994,11.6,-8.01214380700002));
#169908=CARTESIAN_POINT('Ctrl Pts',(6.73427735599994,15.2,-8.01081624200001));
#169909=CARTESIAN_POINT('Ctrl Pts',(6.73427735599994,11.6,-8.01081624200001));
#169910=CARTESIAN_POINT('Ctrl Pts',(6.73348164099994,15.2,-8.00949628200001));
#169911=CARTESIAN_POINT('Ctrl Pts',(6.73348164099994,11.6,-8.00949628200001));
#169912=CARTESIAN_POINT('Ctrl Pts',(6.73268882399994,15.2,-8.00818393500002));
#169913=CARTESIAN_POINT('Ctrl Pts',(6.73268882399994,11.6,-8.00818393500002));
#169914=CARTESIAN_POINT('Ctrl Pts',(6.73189892699994,15.2,-8.00687921200002));
#169915=CARTESIAN_POINT('Ctrl Pts',(6.73189892699994,11.6,-8.00687921200002));
#169916=CARTESIAN_POINT('Ctrl Pts',(6.73111197299994,15.2,-8.00558212100002));
#169917=CARTESIAN_POINT('Ctrl Pts',(6.73111197299994,11.6,-8.00558212100002));
#169918=CARTESIAN_POINT('Ctrl Pts',(6.73032798299994,15.2,-8.00429267200002));
#169919=CARTESIAN_POINT('Ctrl Pts',(6.73032798299994,11.6,-8.00429267200002));
#169920=CARTESIAN_POINT('Ctrl Pts',(6.72954697899995,15.2,-8.00301087500002));
#169921=CARTESIAN_POINT('Ctrl Pts',(6.72954697899995,11.6,-8.00301087500002));
#169922=CARTESIAN_POINT('Ctrl Pts',(6.72876898499994,15.2,-8.00173673800002));
#169923=CARTESIAN_POINT('Ctrl Pts',(6.72876898499994,11.6,-8.00173673800002));
#169924=CARTESIAN_POINT('Ctrl Pts',(6.72799402199994,15.2,-8.00047027200002));
#169925=CARTESIAN_POINT('Ctrl Pts',(6.72799402199994,11.6,-8.00047027200002));
#169926=CARTESIAN_POINT('Ctrl Pts',(6.72722211399994,15.2,-7.99921148700002));
#169927=CARTESIAN_POINT('Ctrl Pts',(6.72722211399994,11.6,-7.99921148700002));
#169928=CARTESIAN_POINT('Ctrl Pts',(6.72645328299994,15.2,-7.99796039100002));
#169929=CARTESIAN_POINT('Ctrl Pts',(6.72645328299994,11.6,-7.99796039100002));
#169930=CARTESIAN_POINT('Ctrl Pts',(6.72568755199995,15.2,-7.99671699400001));
#169931=CARTESIAN_POINT('Ctrl Pts',(6.72568755199995,11.6,-7.99671699400001));
#169932=CARTESIAN_POINT('Ctrl Pts',(6.72492494399994,15.2,-7.99548130700002));
#169933=CARTESIAN_POINT('Ctrl Pts',(6.72492494399994,11.6,-7.99548130700002));
#169934=CARTESIAN_POINT('Ctrl Pts',(6.72416548199994,15.2,-7.99425333800002));
#169935=CARTESIAN_POINT('Ctrl Pts',(6.72416548199994,11.6,-7.99425333800002));
#169936=CARTESIAN_POINT('Ctrl Pts',(6.72340918899994,15.2,-7.99303309800001));
#169937=CARTESIAN_POINT('Ctrl Pts',(6.72340918899994,11.6,-7.99303309800001));
#169938=CARTESIAN_POINT('Ctrl Pts',(6.72265608899994,15.2,-7.99182059500002));
#169939=CARTESIAN_POINT('Ctrl Pts',(6.72265608899994,11.6,-7.99182059500002));
#169940=CARTESIAN_POINT('Ctrl Pts',(6.72190620499994,15.2,-7.99061584100001));
#169941=CARTESIAN_POINT('Ctrl Pts',(6.72190620499994,11.6,-7.99061584100001));
#169942=CARTESIAN_POINT('Ctrl Pts',(6.72115955899995,15.2,-7.98941884400002));
#169943=CARTESIAN_POINT('Ctrl Pts',(6.72115955899995,11.6,-7.98941884400002));
#169944=CARTESIAN_POINT('Ctrl Pts',(6.72041617599994,15.2,-7.98822961300001));
#169945=CARTESIAN_POINT('Ctrl Pts',(6.72041617599994,11.6,-7.98822961300001));
#169946=CARTESIAN_POINT('Ctrl Pts',(6.71967607999994,15.2,-7.98704816100001));
#169947=CARTESIAN_POINT('Ctrl Pts',(6.71967607999994,11.6,-7.98704816100001));
#169948=CARTESIAN_POINT('Ctrl Pts',(6.71893929399995,15.2,-7.98587449600002));
#169949=CARTESIAN_POINT('Ctrl Pts',(6.71893929399995,11.6,-7.98587449600002));
#169950=CARTESIAN_POINT('Ctrl Pts',(6.71820584199994,15.2,-7.98470862800002));
#169951=CARTESIAN_POINT('Ctrl Pts',(6.71820584199994,11.6,-7.98470862800002));
#169952=CARTESIAN_POINT('Ctrl Pts',(6.71747574699994,15.2,-7.98355056600002));
#169953=CARTESIAN_POINT('Ctrl Pts',(6.71747574699994,11.6,-7.98355056600002));
#169954=CARTESIAN_POINT('Ctrl Pts',(6.71674903499994,15.2,-7.98240032100002));
#169955=CARTESIAN_POINT('Ctrl Pts',(6.71674903499994,11.6,-7.98240032100002));
#169956=CARTESIAN_POINT('Ctrl Pts',(6.71602572899994,15.2,-7.98125790400002));
#169957=CARTESIAN_POINT('Ctrl Pts',(6.71602572899994,11.6,-7.98125790400002));
#169958=CARTESIAN_POINT('Ctrl Pts',(6.71530585299994,15.2,-7.98012332400001));
#169959=CARTESIAN_POINT('Ctrl Pts',(6.71530585299994,11.6,-7.98012332400001));
#169960=CARTESIAN_POINT('Ctrl Pts',(6.71458943199994,15.2,-7.97899659000001));
#169961=CARTESIAN_POINT('Ctrl Pts',(6.71458943199994,11.6,-7.97899659000001));
#169962=CARTESIAN_POINT('Ctrl Pts',(6.71387649099994,15.2,-7.97787771300002));
#169963=CARTESIAN_POINT('Ctrl Pts',(6.71387649099994,11.6,-7.97787771300002));
#169964=CARTESIAN_POINT('Ctrl Pts',(6.71316705499994,15.2,-7.97676670400002));
#169965=CARTESIAN_POINT('Ctrl Pts',(6.71316705499994,11.6,-7.97676670400002));
#169966=CARTESIAN_POINT('Ctrl Pts',(6.71246114699994,15.2,-7.97566357200001));
#169967=CARTESIAN_POINT('Ctrl Pts',(6.71246114699994,11.6,-7.97566357200001));
#169968=CARTESIAN_POINT('Ctrl Pts',(6.71175879199994,15.2,-7.97456832700002));
#169969=CARTESIAN_POINT('Ctrl Pts',(6.71175879199994,11.6,-7.97456832700002));
#169970=CARTESIAN_POINT('Ctrl Pts',(6.71106001699994,15.2,-7.97348098000001));
#169971=CARTESIAN_POINT('Ctrl Pts',(6.71106001699994,11.6,-7.97348098000001));
#169972=CARTESIAN_POINT('Ctrl Pts',(6.71036484499994,15.2,-7.97240154000002));
#169973=CARTESIAN_POINT('Ctrl Pts',(6.71036484499994,11.6,-7.97240154000002));
#169974=CARTESIAN_POINT('Ctrl Pts',(6.70967330099994,15.2,-7.97133002000002));
#169975=CARTESIAN_POINT('Ctrl Pts',(6.70967330099994,11.6,-7.97133002000002));
#169976=CARTESIAN_POINT('Ctrl Pts',(6.70898541199994,15.2,-7.97026642700001));
#169977=CARTESIAN_POINT('Ctrl Pts',(6.70898541199994,11.6,-7.97026642700001));
#169978=CARTESIAN_POINT('Ctrl Pts',(6.70830120299994,15.2,-7.96921077400001));
#169979=CARTESIAN_POINT('Ctrl Pts',(6.70830120299994,11.6,-7.96921077400001));
#169980=CARTESIAN_POINT('Ctrl Pts',(6.70762069999994,15.2,-7.96816306900002));
#169981=CARTESIAN_POINT('Ctrl Pts',(6.70762069999994,11.6,-7.96816306900002));
#169982=CARTESIAN_POINT('Ctrl Pts',(6.70694392699994,15.2,-7.96712332400002));
#169983=CARTESIAN_POINT('Ctrl Pts',(6.70694392699994,11.6,-7.96712332400002));
#169984=CARTESIAN_POINT('Ctrl Pts',(6.70627090999995,15.2,-7.96609155000001));
#169985=CARTESIAN_POINT('Ctrl Pts',(6.70627090999995,11.6,-7.96609155000001));
#169986=CARTESIAN_POINT('Ctrl Pts',(6.70560167699994,15.2,-7.96506775500001));
#169987=CARTESIAN_POINT('Ctrl Pts',(6.70560167699994,11.6,-7.96506775500001));
#169988=CARTESIAN_POINT('Ctrl Pts',(6.70493625199994,15.2,-7.96405195200002));
#169989=CARTESIAN_POINT('Ctrl Pts',(6.70493625199994,11.6,-7.96405195200002));
#169990=CARTESIAN_POINT('Ctrl Pts',(6.70427466299994,15.2,-7.96304415000002));
#169991=CARTESIAN_POINT('Ctrl Pts',(6.70427466299994,11.6,-7.96304415000002));
#169992=CARTESIAN_POINT('Ctrl Pts',(6.70361693399994,15.2,-7.96204436100002));
#169993=CARTESIAN_POINT('Ctrl Pts',(6.70361693399994,11.6,-7.96204436100002));
#169994=CARTESIAN_POINT('Ctrl Pts',(6.70296309299995,15.2,-7.96105259300001));
#169995=CARTESIAN_POINT('Ctrl Pts',(6.70296309299995,11.6,-7.96105259300001));
#169996=CARTESIAN_POINT('Ctrl Pts',(6.70231316599994,15.2,-7.96006886000002));
#169997=CARTESIAN_POINT('Ctrl Pts',(6.70231316599994,11.6,-7.96006886000002));
#169998=CARTESIAN_POINT('Ctrl Pts',(6.70166717899995,15.2,-7.95909317200002));
#169999=CARTESIAN_POINT('Ctrl Pts',(6.70166717899995,11.6,-7.95909317200002));
#170000=CARTESIAN_POINT('Ctrl Pts',(6.70102515999995,15.2,-7.95812553600002));
#170001=CARTESIAN_POINT('Ctrl Pts',(6.70102515999995,11.6,-7.95812553600002));
#170002=CARTESIAN_POINT('Ctrl Pts',(6.70038713599994,15.2,-7.95716596700001));
#170003=CARTESIAN_POINT('Ctrl Pts',(6.70038713599994,11.6,-7.95716596700001));
#170004=CARTESIAN_POINT('Ctrl Pts',(6.69975313299994,15.2,-7.95621447500002));
#170005=CARTESIAN_POINT('Ctrl Pts',(6.69975313299994,11.6,-7.95621447500002));
#170006=CARTESIAN_POINT('Ctrl Pts',(6.69912317899994,15.2,-7.95527107000002));
#170007=CARTESIAN_POINT('Ctrl Pts',(6.69912317899994,11.6,-7.95527107000002));
#170008=CARTESIAN_POINT('Ctrl Pts',(6.69849730099994,15.2,-7.95433576200002));
#170009=CARTESIAN_POINT('Ctrl Pts',(6.69849730099994,11.6,-7.95433576200002));
#170010=CARTESIAN_POINT('Ctrl Pts',(6.69787552599994,15.2,-7.95340856300002));
#170011=CARTESIAN_POINT('Ctrl Pts',(6.69787552599994,11.6,-7.95340856300002));
#170012=CARTESIAN_POINT('Ctrl Pts',(6.69725788299994,15.2,-7.95248948500002));
#170013=CARTESIAN_POINT('Ctrl Pts',(6.69725788299994,11.6,-7.95248948500002));
#170014=CARTESIAN_POINT('Ctrl Pts',(6.69664439799995,15.2,-7.95157853800001));
#170015=CARTESIAN_POINT('Ctrl Pts',(6.69664439799995,11.6,-7.95157853800001));
#170016=CARTESIAN_POINT('Ctrl Pts',(6.69603509999994,15.2,-7.95067573100001));
#170017=CARTESIAN_POINT('Ctrl Pts',(6.69603509999994,11.6,-7.95067573100001));
#170018=CARTESIAN_POINT('Ctrl Pts',(6.69543001599994,15.2,-7.94978107900001));
#170019=CARTESIAN_POINT('Ctrl Pts',(6.69543001599994,11.6,-7.94978107900001));
#170020=CARTESIAN_POINT('Ctrl Pts',(6.69482917499994,15.2,-7.94889459000002));
#170021=CARTESIAN_POINT('Ctrl Pts',(6.69482917499994,11.6,-7.94889459000002));
#170022=CARTESIAN_POINT('Ctrl Pts',(6.69423260499994,15.2,-7.94801627700001));
#170023=CARTESIAN_POINT('Ctrl Pts',(6.69423260499994,11.6,-7.94801627700001));
#170024=CARTESIAN_POINT('Ctrl Pts',(6.69364033499994,15.2,-7.94714614900002));
#170025=CARTESIAN_POINT('Ctrl Pts',(6.69364033499994,11.6,-7.94714614900002));
#170026=CARTESIAN_POINT('Ctrl Pts',(6.69305239199994,15.2,-7.94628422000001));
#170027=CARTESIAN_POINT('Ctrl Pts',(6.69305239199994,11.6,-7.94628422000001));
#170028=CARTESIAN_POINT('Ctrl Pts',(6.69246880599994,15.2,-7.94543049900001));
#170029=CARTESIAN_POINT('Ctrl Pts',(6.69246880599994,11.6,-7.94543049900001));
#170030=CARTESIAN_POINT('Ctrl Pts',(6.69188960599994,15.2,-7.94458500000002));
#170031=CARTESIAN_POINT('Ctrl Pts',(6.69188960599994,11.6,-7.94458500000002));
#170032=CARTESIAN_POINT('Ctrl Pts',(6.69131482099995,15.2,-7.94374773000002));
#170033=CARTESIAN_POINT('Ctrl Pts',(6.69131482099995,11.6,-7.94374773000002));
#170034=CARTESIAN_POINT('Ctrl Pts',(6.69074447799994,15.2,-7.94291870500002));
#170035=CARTESIAN_POINT('Ctrl Pts',(6.69074447799994,11.6,-7.94291870500002));
#170036=CARTESIAN_POINT('Ctrl Pts',(6.69017860899995,15.2,-7.94209793300002));
#170037=CARTESIAN_POINT('Ctrl Pts',(6.69017860899995,11.6,-7.94209793300002));
#170038=CARTESIAN_POINT('Ctrl Pts',(6.68961724099994,15.2,-7.94128542600002));
#170039=CARTESIAN_POINT('Ctrl Pts',(6.68961724099994,11.6,-7.94128542600002));
#170040=CARTESIAN_POINT('Ctrl Pts',(6.68906040599994,15.2,-7.94048119900002));
#170041=CARTESIAN_POINT('Ctrl Pts',(6.68906040599994,11.6,-7.94048119900002));
#170042=CARTESIAN_POINT('Ctrl Pts',(6.68850813299994,15.2,-7.93968525900001));
#170043=CARTESIAN_POINT('Ctrl Pts',(6.68850813299994,11.6,-7.93968525900001));
#170044=CARTESIAN_POINT('Ctrl Pts',(6.68796045099994,15.2,-7.93889762000001));
#170045=CARTESIAN_POINT('Ctrl Pts',(6.68796045099994,11.6,-7.93889762000001));
#170046=CARTESIAN_POINT('Ctrl Pts',(6.68741739099994,15.2,-7.93811829200001));
#170047=CARTESIAN_POINT('Ctrl Pts',(6.68741739099994,11.6,-7.93811829200001));
#170048=CARTESIAN_POINT('Ctrl Pts',(6.68687898199994,15.2,-7.93734729000001));
#170049=CARTESIAN_POINT('Ctrl Pts',(6.68687898199994,11.6,-7.93734729000001));
#170050=CARTESIAN_POINT('Ctrl Pts',(6.68634525499994,15.2,-7.93658462300002));
#170051=CARTESIAN_POINT('Ctrl Pts',(6.68634525499994,11.6,-7.93658462300002));
#170052=CARTESIAN_POINT('Ctrl Pts',(6.68581928699994,15.2,-7.93583464600002));
#170053=CARTESIAN_POINT('Ctrl Pts',(6.68581928699994,11.6,-7.93583464600002));
#170054=CARTESIAN_POINT('Ctrl Pts',(6.68540286299995,15.2,-7.93524212600002));
#170055=CARTESIAN_POINT('Ctrl Pts',(6.68540286299995,11.6,-7.93524212600002));
#170056=CARTESIAN_POINT('Ctrl Pts',(6.68509340699995,15.2,-7.93480250500001));
#170057=CARTESIAN_POINT('Ctrl Pts',(6.68509340699995,11.6,-7.93480250500001));
#170058=CARTESIAN_POINT('Ctrl Pts',(6.68488903399994,15.2,-7.93451247300001));
#170059=CARTESIAN_POINT('Ctrl Pts',(6.68488903399994,11.6,-7.93451247300001));
#170060=CARTESIAN_POINT('Ctrl Pts',(6.68478856699994,15.2,-7.93436996900001));
#170061=CARTESIAN_POINT('Ctrl Pts',(6.68478856699994,11.6,-7.93436996900001));
#170062=CARTESIAN_POINT('',(6.68478856699994,12.2,-7.93436996900001));
#170063=CARTESIAN_POINT('',(6.68478856699994,15.2,-7.93436996900001));
#170064=CARTESIAN_POINT('',(6.68478856699994,12.2,-7.93436996900001));
#170065=CARTESIAN_POINT('Ctrl Pts',(7.10901226899994,12.2,-9.03946594400002));
#170066=CARTESIAN_POINT('Ctrl Pts',(7.10885083699995,12.2,-9.03871859500001));
#170067=CARTESIAN_POINT('Ctrl Pts',(7.10852778299994,12.2,-9.03722439200001));
#170068=CARTESIAN_POINT('Ctrl Pts',(7.10804263899995,12.2,-9.03498456100002));
#170069=CARTESIAN_POINT('Ctrl Pts',(7.10739465099994,12.2,-9.03200107200002));
#170070=CARTESIAN_POINT('Ctrl Pts',(7.10658278299994,12.2,-9.02827662900001));
#170071=CARTESIAN_POINT('Ctrl Pts',(7.10576903499994,12.2,-9.02455710700002));
#170072=CARTESIAN_POINT('Ctrl Pts',(7.10495340799994,12.2,-9.02084250500002));
#170073=CARTESIAN_POINT('Ctrl Pts',(7.10413590299994,12.2,-9.01713282900002));
#170074=CARTESIAN_POINT('Ctrl Pts',(7.10331652799994,12.2,-9.01342808000001));
#170075=CARTESIAN_POINT('Ctrl Pts',(7.10249528699994,12.2,-9.00972826500002));
#170076=CARTESIAN_POINT('Ctrl Pts',(7.10167218799994,12.2,-9.00603338900002));
#170077=CARTESIAN_POINT('Ctrl Pts',(7.10084723999994,12.2,-9.00234345900002));
#170078=CARTESIAN_POINT('Ctrl Pts',(7.10002044999994,12.2,-8.99865848200001));
#170079=CARTESIAN_POINT('Ctrl Pts',(7.09919182999994,12.2,-8.99497846600001));
#170080=CARTESIAN_POINT('Ctrl Pts',(7.09836138399995,12.2,-8.99130341500002));
#170081=CARTESIAN_POINT('Ctrl Pts',(7.09752912199995,12.2,-8.98763333900002));
#170082=CARTESIAN_POINT('Ctrl Pts',(7.09669504999995,12.2,-8.98396824000002));
#170083=CARTESIAN_POINT('Ctrl Pts',(7.09585917499994,12.2,-8.98030812400001));
#170084=CARTESIAN_POINT('Ctrl Pts',(7.09502150299994,12.2,-8.97665299700002));
#170085=CARTESIAN_POINT('Ctrl Pts',(7.09418203899994,12.2,-8.97300286300002));
#170086=CARTESIAN_POINT('Ctrl Pts',(7.09334079199994,12.2,-8.96935772800001));
#170087=CARTESIAN_POINT('Ctrl Pts',(7.09249776599994,12.2,-8.96571759800001));
#170088=CARTESIAN_POINT('Ctrl Pts',(7.09165297099994,12.2,-8.96208247700002));
#170089=CARTESIAN_POINT('Ctrl Pts',(7.09080641499994,12.2,-8.95845237400002));
#170090=CARTESIAN_POINT('Ctrl Pts',(7.08995810299994,12.2,-8.95482729200002));
#170091=CARTESIAN_POINT('Ctrl Pts',(7.08910804199994,12.2,-8.95120723800002));
#170092=CARTESIAN_POINT('Ctrl Pts',(7.08825624299994,12.2,-8.94759221800001));
#170093=CARTESIAN_POINT('Ctrl Pts',(7.08740270999995,12.2,-8.94398223900001));
#170094=CARTESIAN_POINT('Ctrl Pts',(7.08654745099994,12.2,-8.94037730400001));
#170095=CARTESIAN_POINT('Ctrl Pts',(7.08569047499994,12.2,-8.93677742100002));
#170096=CARTESIAN_POINT('Ctrl Pts',(7.08483178599994,12.2,-8.93318259300001));
#170097=CARTESIAN_POINT('Ctrl Pts',(7.08397139199994,12.2,-8.92959282900001));
#170098=CARTESIAN_POINT('Ctrl Pts',(7.08310930199994,12.2,-8.92600813100002));
#170099=CARTESIAN_POINT('Ctrl Pts',(7.08224552099994,12.2,-8.92242850800002));
#170100=CARTESIAN_POINT('Ctrl Pts',(7.08138005899994,12.2,-8.91885396400001));
#170101=CARTESIAN_POINT('Ctrl Pts',(7.08051291999994,12.2,-8.91528450500001));
#170102=CARTESIAN_POINT('Ctrl Pts',(7.07964411499994,12.2,-8.91172013700002));
#170103=CARTESIAN_POINT('Ctrl Pts',(7.07877364899994,12.2,-8.90816086600001));
#170104=CARTESIAN_POINT('Ctrl Pts',(7.07790152999995,12.2,-8.90460669800002));
#170105=CARTESIAN_POINT('Ctrl Pts',(7.07702776499994,12.2,-8.90105763700002));
#170106=CARTESIAN_POINT('Ctrl Pts',(7.07615236299994,12.2,-8.89751369100001));
#170107=CARTESIAN_POINT('Ctrl Pts',(7.07527532899995,12.2,-8.89397486500001));
#170108=CARTESIAN_POINT('Ctrl Pts',(7.07439667399994,12.2,-8.89044116400001));
#170109=CARTESIAN_POINT('Ctrl Pts',(7.07351640099994,12.2,-8.88691259500002));
#170110=CARTESIAN_POINT('Ctrl Pts',(7.07263452099994,12.2,-8.88338916200002));
#170111=CARTESIAN_POINT('Ctrl Pts',(7.07175103999995,12.2,-8.87987087200001));
#170112=CARTESIAN_POINT('Ctrl Pts',(7.07086596699994,12.2,-8.87635773100002));
#170113=CARTESIAN_POINT('Ctrl Pts',(7.06997930699995,12.2,-8.87284974500002));
#170114=CARTESIAN_POINT('Ctrl Pts',(7.06909106899994,12.2,-8.86934691900001));
#170115=CARTESIAN_POINT('Ctrl Pts',(7.06820126099994,12.2,-8.86584925900002));
#170116=CARTESIAN_POINT('Ctrl Pts',(7.06730988999994,12.2,-8.86235676900002));
#170117=CARTESIAN_POINT('Ctrl Pts',(7.06641696399994,12.2,-8.85886945800002));
#170118=CARTESIAN_POINT('Ctrl Pts',(7.06552248999994,12.2,-8.85538733200002));
#170119=CARTESIAN_POINT('Ctrl Pts',(7.06462647799994,12.2,-8.85191039400001));
#170120=CARTESIAN_POINT('Ctrl Pts',(7.06372893199994,12.2,-8.84843865100001));
#170121=CARTESIAN_POINT('Ctrl Pts',(7.06282986099994,12.2,-8.84497210900001));
#170122=CARTESIAN_POINT('Ctrl Pts',(7.06192927499995,12.2,-8.84151077400002));
#170123=CARTESIAN_POINT('Ctrl Pts',(7.06102717799994,12.2,-8.83805465100002));
#170124=CARTESIAN_POINT('Ctrl Pts',(7.06012358099994,12.2,-8.83460374700002));
#170125=CARTESIAN_POINT('Ctrl Pts',(7.05921848999994,12.2,-8.83115806600001));
#170126=CARTESIAN_POINT('Ctrl Pts',(7.05831191399994,12.2,-8.82771761700001));
#170127=CARTESIAN_POINT('Ctrl Pts',(7.05740385899994,12.2,-8.82428240200002));
#170128=CARTESIAN_POINT('Ctrl Pts',(7.05649433399994,12.2,-8.82085243000001));
#170129=CARTESIAN_POINT('Ctrl Pts',(7.05558334699995,12.2,-8.81742770600002));
#170130=CARTESIAN_POINT('Ctrl Pts',(7.05467090599995,12.2,-8.81400823500002));
#170131=CARTESIAN_POINT('Ctrl Pts',(7.05375701899994,12.2,-8.81059402400002));
#170132=CARTESIAN_POINT('Ctrl Pts',(7.05284169299994,12.2,-8.80718507700001));
#170133=CARTESIAN_POINT('Ctrl Pts',(7.05192493599994,12.2,-8.80378140200002));
#170134=CARTESIAN_POINT('Ctrl Pts',(7.05100675599994,12.2,-8.80038300300001));
#170135=CARTESIAN_POINT('Ctrl Pts',(7.05008716199995,12.2,-8.79698988800002));
#170136=CARTESIAN_POINT('Ctrl Pts',(7.04916616099994,12.2,-8.79360206200002));
#170137=CARTESIAN_POINT('Ctrl Pts',(7.04824376099995,12.2,-8.79021953000001));
#170138=CARTESIAN_POINT('Ctrl Pts',(7.04731997099994,12.2,-8.78684229900001));
#170139=CARTESIAN_POINT('Ctrl Pts',(7.04639479699994,12.2,-8.78347037400001));
#170140=CARTESIAN_POINT('Ctrl Pts',(7.04546824999994,12.2,-8.78010376100002));
#170141=CARTESIAN_POINT('Ctrl Pts',(7.04454033599994,12.2,-8.77674246600002));
#170142=CARTESIAN_POINT('Ctrl Pts',(7.04361106199995,12.2,-8.77338649600001));
#170143=CARTESIAN_POINT('Ctrl Pts',(7.04268043899994,12.2,-8.77003585600002));
#170144=CARTESIAN_POINT('Ctrl Pts',(7.04174847399995,12.2,-8.76669055200002));
#170145=CARTESIAN_POINT('Ctrl Pts',(7.04081517499994,12.2,-8.76335058900001));
#170146=CARTESIAN_POINT('Ctrl Pts',(7.03988054999994,12.2,-8.76001597500002));
#170147=CARTESIAN_POINT('Ctrl Pts',(7.03894460699994,12.2,-8.75668671600002));
#170148=CARTESIAN_POINT('Ctrl Pts',(7.03800735599994,12.2,-8.75336281500001));
#170149=CARTESIAN_POINT('Ctrl Pts',(7.03706880199994,12.2,-8.75004428000001));
#170150=CARTESIAN_POINT('Ctrl Pts',(7.03612895599995,12.2,-8.74673111600002));
#170151=CARTESIAN_POINT('Ctrl Pts',(7.03518782499994,12.2,-8.74342333000002));
#170152=CARTESIAN_POINT('Ctrl Pts',(7.03424541799994,12.2,-8.74012092800001));
#170153=CARTESIAN_POINT('Ctrl Pts',(7.03330174299994,12.2,-8.73682391500001));
#170154=CARTESIAN_POINT('Ctrl Pts',(7.03235680899994,12.2,-8.73353229700001));
#170155=CARTESIAN_POINT('Ctrl Pts',(7.03141062299995,12.2,-8.73024608200001));
#170156=CARTESIAN_POINT('Ctrl Pts',(7.03046319299995,12.2,-8.72696527400001));
#170157=CARTESIAN_POINT('Ctrl Pts',(7.02951453099994,12.2,-8.72368987800002));
#170158=CARTESIAN_POINT('Ctrl Pts',(7.02856464099994,12.2,-8.72041990300002));
#170159=CARTESIAN_POINT('Ctrl Pts',(7.02761353399994,12.2,-8.71715535200002));
#170160=CARTESIAN_POINT('Ctrl Pts',(7.02666121799994,12.2,-8.71389623300002));
#170161=CARTESIAN_POINT('Ctrl Pts',(7.02570770099994,12.2,-8.71064255100002));
#170162=CARTESIAN_POINT('Ctrl Pts',(7.02475299199994,12.2,-8.70739431300001));
#170163=CARTESIAN_POINT('Ctrl Pts',(7.02379709999994,12.2,-8.70415152400002));
#170164=CARTESIAN_POINT('Ctrl Pts',(7.02284003299994,12.2,-8.70091419100002));
#170165=CARTESIAN_POINT('Ctrl Pts',(7.02188179799994,12.2,-8.69768231900002));
#170166=CARTESIAN_POINT('Ctrl Pts',(7.02092240599994,12.2,-8.69445591400002));
#170167=CARTESIAN_POINT('Ctrl Pts',(7.01996186499994,12.2,-8.69123498300001));
#170168=CARTESIAN_POINT('Ctrl Pts',(7.01900018299995,12.2,-8.68801953100002));
#170169=CARTESIAN_POINT('Ctrl Pts',(7.01803736899994,12.2,-8.68480956600001));
#170170=CARTESIAN_POINT('Ctrl Pts',(7.01707343299995,12.2,-8.68160509100001));
#170171=CARTESIAN_POINT('Ctrl Pts',(7.01610838099994,12.2,-8.67840611400002));
#170172=CARTESIAN_POINT('Ctrl Pts',(7.01514222399994,12.2,-8.67521264000001));
#170173=CARTESIAN_POINT('Ctrl Pts',(7.01417496999994,12.2,-8.67202467700002));
#170174=CARTESIAN_POINT('Ctrl Pts',(7.01320662599994,12.2,-8.66884222900002));
#170175=CARTESIAN_POINT('Ctrl Pts',(7.01223720399994,12.2,-8.66566530400002));
#170176=CARTESIAN_POINT('Ctrl Pts',(7.01126671099995,12.2,-8.66249390500002));
#170177=CARTESIAN_POINT('Ctrl Pts',(7.01029515599994,12.2,-8.65932804100002));
#170178=CARTESIAN_POINT('Ctrl Pts',(7.00932254799994,12.2,-8.65616771800001));
#170179=CARTESIAN_POINT('Ctrl Pts',(7.00834889699994,12.2,-8.65301294000002));
#170180=CARTESIAN_POINT('Ctrl Pts',(7.00737420899994,12.2,-8.64986371400001));
#170181=CARTESIAN_POINT('Ctrl Pts',(7.00639849599995,12.2,-8.64672004800001));
#170182=CARTESIAN_POINT('Ctrl Pts',(7.00542176599994,12.2,-8.64358194500002));
#170183=CARTESIAN_POINT('Ctrl Pts',(7.00444402699994,12.2,-8.64044941300002));
#170184=CARTESIAN_POINT('Ctrl Pts',(7.00346528799995,12.2,-8.63732245800002));
#170185=CARTESIAN_POINT('Ctrl Pts',(7.00248555899995,12.2,-8.63420108600002));
#170186=CARTESIAN_POINT('Ctrl Pts',(7.00150484899994,12.2,-8.63108530300002));
#170187=CARTESIAN_POINT('Ctrl Pts',(7.00052316699994,12.2,-8.62797511400002));
#170188=CARTESIAN_POINT('Ctrl Pts',(6.99954052099995,12.2,-8.62487052700001));
#170189=CARTESIAN_POINT('Ctrl Pts',(6.99855692199994,12.2,-8.62177154700002));
#170190=CARTESIAN_POINT('Ctrl Pts',(6.99757237899994,12.2,-8.61867818100002));
#170191=CARTESIAN_POINT('Ctrl Pts',(6.99658689799994,12.2,-8.61559043400002));
#170192=CARTESIAN_POINT('Ctrl Pts',(6.99560049199994,12.2,-8.61250831300002));
#170193=CARTESIAN_POINT('Ctrl Pts',(6.99461316799994,12.2,-8.60943182400002));
#170194=CARTESIAN_POINT('Ctrl Pts',(6.99362493699994,12.2,-8.60636097400001));
#170195=CARTESIAN_POINT('Ctrl Pts',(6.99263580599994,12.2,-8.60329576700002));
#170196=CARTESIAN_POINT('Ctrl Pts',(6.99164578499994,12.2,-8.60023621100002));
#170197=CARTESIAN_POINT('Ctrl Pts',(6.99065488599994,12.2,-8.59718231200001));
#170198=CARTESIAN_POINT('Ctrl Pts',(6.98966311399994,12.2,-8.59413407600002));
#170199=CARTESIAN_POINT('Ctrl Pts',(6.98867048099994,12.2,-8.59109150800002));
#170200=CARTESIAN_POINT('Ctrl Pts',(6.98767699599994,12.2,-8.58805461600002));
#170201=CARTESIAN_POINT('Ctrl Pts',(6.98668266799994,12.2,-8.58502340600002));
#170202=CARTESIAN_POINT('Ctrl Pts',(6.98568750699994,12.2,-8.58199788300002));
#170203=CARTESIAN_POINT('Ctrl Pts',(6.98469152199994,12.2,-8.57897805400002));
#170204=CARTESIAN_POINT('Ctrl Pts',(6.98369472199994,12.2,-8.57596392400002));
#170205=CARTESIAN_POINT('Ctrl Pts',(6.98269711799994,12.2,-8.57295550200002));
#170206=CARTESIAN_POINT('Ctrl Pts',(6.98169871799994,12.2,-8.56995279200002));
#170207=CARTESIAN_POINT('Ctrl Pts',(6.98069953199994,12.2,-8.56695580000002));
#170208=CARTESIAN_POINT('Ctrl Pts',(6.97969957099994,12.2,-8.56396453400002));
#170209=CARTESIAN_POINT('Ctrl Pts',(6.97869884199994,12.2,-8.56097899900002));
#170210=CARTESIAN_POINT('Ctrl Pts',(6.97769735699994,12.2,-8.55799920200001));
#170211=CARTESIAN_POINT('Ctrl Pts',(6.97669512399994,12.2,-8.55502514800002));
#170212=CARTESIAN_POINT('Ctrl Pts',(6.97569215299994,12.2,-8.55205684500002));
#170213=CARTESIAN_POINT('Ctrl Pts',(6.97468845399994,12.2,-8.54909429700001));
#170214=CARTESIAN_POINT('Ctrl Pts',(6.97368403699994,12.2,-8.54613751400001));
#170215=CARTESIAN_POINT('Ctrl Pts',(6.97267891199994,12.2,-8.54318649800001));
#170216=CARTESIAN_POINT('Ctrl Pts',(6.97167308699994,12.2,-8.54024125700001));
#170217=CARTESIAN_POINT('Ctrl Pts',(6.97066657399994,12.2,-8.53730179900002));
#170218=CARTESIAN_POINT('Ctrl Pts',(6.96965938299994,12.2,-8.53436812800001));
#170219=CARTESIAN_POINT('Ctrl Pts',(6.96865152099994,12.2,-8.53144025000002));
#170220=CARTESIAN_POINT('Ctrl Pts',(6.96764299999994,12.2,-8.52851817400002));
#170221=CARTESIAN_POINT('Ctrl Pts',(6.96663382999994,12.2,-8.52560190500002));
#170222=CARTESIAN_POINT('Ctrl Pts',(6.96562401999994,12.2,-8.52269144800001));
#170223=CARTESIAN_POINT('Ctrl Pts',(6.96461357999994,12.2,-8.51978681100002));
#170224=CARTESIAN_POINT('Ctrl Pts',(6.96360252099994,12.2,-8.51688800000002));
#170225=CARTESIAN_POINT('Ctrl Pts',(6.96259085299994,12.2,-8.51399502000002));
#170226=CARTESIAN_POINT('Ctrl Pts',(6.96157858499994,12.2,-8.51110787900001));
#170227=CARTESIAN_POINT('Ctrl Pts',(6.96056572699994,12.2,-8.50822658400002));
#170228=CARTESIAN_POINT('Ctrl Pts',(6.95955229099994,12.2,-8.50535113900002));
#170229=CARTESIAN_POINT('Ctrl Pts',(6.95853828499994,12.2,-8.50248155200001));
#170230=CARTESIAN_POINT('Ctrl Pts',(6.95752371999995,12.2,-8.49961782800002));
#170231=CARTESIAN_POINT('Ctrl Pts',(6.95650860599994,12.2,-8.49675997600002));
#170232=CARTESIAN_POINT('Ctrl Pts',(6.95549295399994,12.2,-8.49390799900002));
#170233=CARTESIAN_POINT('Ctrl Pts',(6.95447677299994,12.2,-8.49106190600001));
#170234=CARTESIAN_POINT('Ctrl Pts',(6.95346007499994,12.2,-8.48822170300001));
#170235=CARTESIAN_POINT('Ctrl Pts',(6.95244286799994,12.2,-8.48538739600002));
#170236=CARTESIAN_POINT('Ctrl Pts',(6.95142516299994,12.2,-8.48255899100002));
#170237=CARTESIAN_POINT('Ctrl Pts',(6.95040697199994,12.2,-8.47973649400002));
#170238=CARTESIAN_POINT('Ctrl Pts',(6.94938830399995,12.2,-8.47691991200002));
#170239=CARTESIAN_POINT('Ctrl Pts',(6.94836916999994,12.2,-8.47410925300002));
#170240=CARTESIAN_POINT('Ctrl Pts',(6.94734957799994,12.2,-8.47130452200001));
#170241=CARTESIAN_POINT('Ctrl Pts',(6.94632954299994,12.2,-8.46850572500001));
#170242=CARTESIAN_POINT('Ctrl Pts',(6.94530907199994,12.2,-8.46571286900001));
#170243=CARTESIAN_POINT('Ctrl Pts',(6.94428817599994,12.2,-8.46292596000002));
#170244=CARTESIAN_POINT('Ctrl Pts',(6.94326686599994,12.2,-8.46014500600001));
#170245=CARTESIAN_POINT('Ctrl Pts',(6.94224515399994,12.2,-8.45737001200002));
#170246=CARTESIAN_POINT('Ctrl Pts',(6.94122304799994,12.2,-8.45460098400002));
#170247=CARTESIAN_POINT('Ctrl Pts',(6.94020055999995,12.2,-8.45183793000002));
#170248=CARTESIAN_POINT('Ctrl Pts',(6.93917770099994,12.2,-8.44908085600002));
#170249=CARTESIAN_POINT('Ctrl Pts',(6.93815448099994,12.2,-8.44632976900002));
#170250=CARTESIAN_POINT('Ctrl Pts',(6.93713091199994,12.2,-8.44358467400001));
#170251=CARTESIAN_POINT('Ctrl Pts',(6.93610700299994,12.2,-8.44084557900001));
#170252=CARTESIAN_POINT('Ctrl Pts',(6.93508276499994,12.2,-8.43811248900002));
#170253=CARTESIAN_POINT('Ctrl Pts',(6.93405820999994,12.2,-8.43538541100001));
#170254=CARTESIAN_POINT('Ctrl Pts',(6.93303334799994,12.2,-8.43266435400002));
#170255=CARTESIAN_POINT('Ctrl Pts',(6.93200819099994,12.2,-8.42994932100002));
#170256=CARTESIAN_POINT('Ctrl Pts',(6.93098274699994,12.2,-8.42724032100002));
#170257=CARTESIAN_POINT('Ctrl Pts',(6.92995702999994,12.2,-8.42453735900002));
#170258=CARTESIAN_POINT('Ctrl Pts',(6.92893105099994,12.2,-8.42184044300001));
#170259=CARTESIAN_POINT('Ctrl Pts',(6.92790481799994,12.2,-8.41914957800002));
#170260=CARTESIAN_POINT('Ctrl Pts',(6.92687834499995,12.2,-8.41646477200002));
#170261=CARTESIAN_POINT('Ctrl Pts',(6.92585164099994,12.2,-8.41378603000001));
#170262=CARTESIAN_POINT('Ctrl Pts',(6.92482471899995,12.2,-8.41111336100001));
#170263=CARTESIAN_POINT('Ctrl Pts',(6.92379758999994,12.2,-8.40844676800002));
#170264=CARTESIAN_POINT('Ctrl Pts',(6.92277026199994,12.2,-8.40578626200001));
#170265=CARTESIAN_POINT('Ctrl Pts',(6.92174274999994,12.2,-8.40313184700002));
#170266=CARTESIAN_POINT('Ctrl Pts',(6.92071506399994,12.2,-8.40048352900002));
#170267=CARTESIAN_POINT('Ctrl Pts',(6.91968721499994,12.2,-8.39784131600002));
#170268=CARTESIAN_POINT('Ctrl Pts',(6.91865921499994,12.2,-8.39520521500001));
#170269=CARTESIAN_POINT('Ctrl Pts',(6.91763107299994,12.2,-8.39257523200001));
#170270=CARTESIAN_POINT('Ctrl Pts',(6.91660280299994,12.2,-8.38995137300002));
#170271=CARTESIAN_POINT('Ctrl Pts',(6.91557441499994,12.2,-8.38733364600002));
#170272=CARTESIAN_POINT('Ctrl Pts',(6.91454591999995,12.2,-8.38472205600001));
#170273=CARTESIAN_POINT('Ctrl Pts',(6.91351733199994,12.2,-8.38211661100001));
#170274=CARTESIAN_POINT('Ctrl Pts',(6.91248865999994,12.2,-8.37951731700001));
#170275=CARTESIAN_POINT('Ctrl Pts',(6.91145991499994,12.2,-8.37692418200002));
#170276=CARTESIAN_POINT('Ctrl Pts',(6.91043111099994,12.2,-8.37433721000002));
#170277=CARTESIAN_POINT('Ctrl Pts',(6.90940225899995,12.2,-8.37175641100002));
#170278=CARTESIAN_POINT('Ctrl Pts',(6.90837336899994,12.2,-8.36918179000002));
#170279=CARTESIAN_POINT('Ctrl Pts',(6.90734445199994,12.2,-8.36661335300001));
#170280=CARTESIAN_POINT('Ctrl Pts',(6.90631552399994,12.2,-8.36405110800002));
#170281=CARTESIAN_POINT('Ctrl Pts',(6.90528659299994,12.2,-8.36149506200002));
#170282=CARTESIAN_POINT('Ctrl Pts',(6.90425767199994,12.2,-8.35894522000002));
#170283=CARTESIAN_POINT('Ctrl Pts',(6.90322877199994,12.2,-8.35640159100001));
#170284=CARTESIAN_POINT('Ctrl Pts',(6.90219990499994,12.2,-8.35386418100001));
#170285=CARTESIAN_POINT('Ctrl Pts',(6.90117108399994,12.2,-8.35133299500002));
#170286=CARTESIAN_POINT('Ctrl Pts',(6.90014232099994,12.2,-8.34880804200001));
#170287=CARTESIAN_POINT('Ctrl Pts',(6.89911362499994,12.2,-8.34628932700002));
#170288=CARTESIAN_POINT('Ctrl Pts',(6.89808501099994,12.2,-8.34377685900002));
#170289=CARTESIAN_POINT('Ctrl Pts',(6.89705648999994,12.2,-8.34127064300001));
#170290=CARTESIAN_POINT('Ctrl Pts',(6.89602807299995,12.2,-8.33877068600002));
#170291=CARTESIAN_POINT('Ctrl Pts',(6.89499977499994,12.2,-8.33627699600001));
#170292=CARTESIAN_POINT('Ctrl Pts',(6.89397160499994,12.2,-8.33378957900001));
#170293=CARTESIAN_POINT('Ctrl Pts',(6.89294357699994,12.2,-8.33130844200002));
#170294=CARTESIAN_POINT('Ctrl Pts',(6.89191570099994,12.2,-8.32883359100002));
#170295=CARTESIAN_POINT('Ctrl Pts',(6.89088799199994,12.2,-8.32636503500002));
#170296=CARTESIAN_POINT('Ctrl Pts',(6.88986046099994,12.2,-8.32390277900002));
#170297=CARTESIAN_POINT('Ctrl Pts',(6.88883311899994,12.2,-8.32144682900001));
#170298=CARTESIAN_POINT('Ctrl Pts',(6.88780597999994,12.2,-8.31899719600001));
#170299=CARTESIAN_POINT('Ctrl Pts',(6.88677905699994,12.2,-8.31655388200002));
#170300=CARTESIAN_POINT('Ctrl Pts',(6.88575235999994,12.2,-8.31411689700002));
#170301=CARTESIAN_POINT('Ctrl Pts',(6.88472590399994,12.2,-8.31168624500001));
#170302=CARTESIAN_POINT('Ctrl Pts',(6.88369969899994,12.2,-8.30926193800002));
#170303=CARTESIAN_POINT('Ctrl Pts',(6.88267375899994,12.2,-8.30684397800002));
#170304=CARTESIAN_POINT('Ctrl Pts',(6.88164809599995,12.2,-8.30443237500001));
#170305=CARTESIAN_POINT('Ctrl Pts',(6.88062272399995,12.2,-8.30202713300002));
#170306=CARTESIAN_POINT('Ctrl Pts',(6.87959765299994,12.2,-8.29962826200001));
#170307=CARTESIAN_POINT('Ctrl Pts',(6.87857289699994,12.2,-8.29723576700001));
#170308=CARTESIAN_POINT('Ctrl Pts',(6.87754846999994,12.2,-8.29484965700001));
#170309=CARTESIAN_POINT('Ctrl Pts',(6.87652438199994,12.2,-8.29246993600002));
#170310=CARTESIAN_POINT('Ctrl Pts',(6.87550064899995,12.2,-8.29009661300002));
#170311=CARTESIAN_POINT('Ctrl Pts',(6.87447728099994,12.2,-8.28772969500001));
#170312=CARTESIAN_POINT('Ctrl Pts',(6.87345429199994,12.2,-8.28536918900001));
#170313=CARTESIAN_POINT('Ctrl Pts',(6.87243169499994,12.2,-8.28301510100001));
#170314=CARTESIAN_POINT('Ctrl Pts',(6.87140950299994,12.2,-8.28066743900001));
#170315=CARTESIAN_POINT('Ctrl Pts',(6.87038772899994,12.2,-8.27832621000002));
#170316=CARTESIAN_POINT('Ctrl Pts',(6.86936638499994,12.2,-8.27599142100001));
#170317=CARTESIAN_POINT('Ctrl Pts',(6.86834548499994,12.2,-8.27366307800002));
#170318=CARTESIAN_POINT('Ctrl Pts',(6.86732504299994,12.2,-8.27134119000002));
#170319=CARTESIAN_POINT('Ctrl Pts',(6.86630506999995,12.2,-8.26902576200002));
#170320=CARTESIAN_POINT('Ctrl Pts',(6.86528557999995,12.2,-8.26671680300001));
#170321=CARTESIAN_POINT('Ctrl Pts',(6.86426658699994,12.2,-8.26441431900001));
#170322=CARTESIAN_POINT('Ctrl Pts',(6.86324810299995,12.2,-8.26211831700002));
#170323=CARTESIAN_POINT('Ctrl Pts',(6.86223014199994,12.2,-8.25982880500002));
#170324=CARTESIAN_POINT('Ctrl Pts',(6.86121271699994,12.2,-8.25754578900002));
#170325=CARTESIAN_POINT('Ctrl Pts',(6.86019584299994,12.2,-8.25526927700002));
#170326=CARTESIAN_POINT('Ctrl Pts',(6.85917953099994,12.2,-8.25299927600001));
#170327=CARTESIAN_POINT('Ctrl Pts',(6.85816379599994,12.2,-8.25073579300001));
#170328=CARTESIAN_POINT('Ctrl Pts',(6.85714865199994,12.2,-8.24847883600001));
#170329=CARTESIAN_POINT('Ctrl Pts',(6.85613410999995,12.2,-8.24622841000001));
#170330=CARTESIAN_POINT('Ctrl Pts',(6.85512018599994,12.2,-8.24398452500001));
#170331=CARTESIAN_POINT('Ctrl Pts',(6.85410689299994,12.2,-8.24174718600002));
#170332=CARTESIAN_POINT('Ctrl Pts',(6.85309424499994,12.2,-8.23951640200002));
#170333=CARTESIAN_POINT('Ctrl Pts',(6.85208225499994,12.2,-8.23729217900001));
#170334=CARTESIAN_POINT('Ctrl Pts',(6.85107093599994,12.2,-8.23507452400002));
#170335=CARTESIAN_POINT('Ctrl Pts',(6.85006030399994,12.2,-8.23286344400002));
#170336=CARTESIAN_POINT('Ctrl Pts',(6.84905037099995,12.2,-8.23065895000001));
#170337=CARTESIAN_POINT('Ctrl Pts',(6.84804115199994,12.2,-8.22846104400002));
#170338=CARTESIAN_POINT('Ctrl Pts',(6.84703265999994,12.2,-8.22626973500002));
#170339=CARTESIAN_POINT('Ctrl Pts',(6.84602490999994,12.2,-8.22408503200002));
#170340=CARTESIAN_POINT('Ctrl Pts',(6.84501791499994,12.2,-8.22190694200001));
#170341=CARTESIAN_POINT('Ctrl Pts',(6.84401168999995,12.2,-8.21973547000002));
#170342=CARTESIAN_POINT('Ctrl Pts',(6.84300624899994,12.2,-8.21757062500001));
#170343=CARTESIAN_POINT('Ctrl Pts',(6.84200160499994,12.2,-8.21541241600002));
#170344=CARTESIAN_POINT('Ctrl Pts',(6.84099777399994,12.2,-8.21326084700001));
#170345=CARTESIAN_POINT('Ctrl Pts',(6.83999476999994,12.2,-8.21111592700002));
#170346=CARTESIAN_POINT('Ctrl Pts',(6.83899260499994,12.2,-8.20897766300002));
#170347=CARTESIAN_POINT('Ctrl Pts',(6.83799129699994,12.2,-8.20684606400001));
#170348=CARTESIAN_POINT('Ctrl Pts',(6.83699085699994,12.2,-8.20472113600001));
#170349=CARTESIAN_POINT('Ctrl Pts',(6.83599130199994,12.2,-8.20260288400002));
#170350=CARTESIAN_POINT('Ctrl Pts',(6.83499264499994,12.2,-8.20049132000002));
#170351=CARTESIAN_POINT('Ctrl Pts',(6.83399489999994,12.2,-8.19838644900001));
#170352=CARTESIAN_POINT('Ctrl Pts',(6.83299808299994,12.2,-8.19628827900001));
#170353=CARTESIAN_POINT('Ctrl Pts',(6.83200220999994,12.2,-8.19419681600002));
#170354=CARTESIAN_POINT('Ctrl Pts',(6.83100729199994,12.2,-8.19211207100001));
#170355=CARTESIAN_POINT('Ctrl Pts',(6.83001334499994,12.2,-8.19003404700002));
#170356=CARTESIAN_POINT('Ctrl Pts',(6.82902038699994,12.2,-8.18796275400001));
#170357=CARTESIAN_POINT('Ctrl Pts',(6.82802842799994,12.2,-8.18589820000001));
#170358=CARTESIAN_POINT('Ctrl Pts',(6.82703748599994,12.2,-8.18384039100001));
#170359=CARTESIAN_POINT('Ctrl Pts',(6.82604757499995,12.2,-8.18178933600001));
#170360=CARTESIAN_POINT('Ctrl Pts',(6.82505870999995,12.2,-8.17974504100001));
#170361=CARTESIAN_POINT('Ctrl Pts',(6.82407090599995,12.2,-8.17770751500002));
#170362=CARTESIAN_POINT('Ctrl Pts',(6.82308417899994,12.2,-8.17567676500002));
#170363=CARTESIAN_POINT('Ctrl Pts',(6.82209854199994,12.2,-8.17365279700002));
#170364=CARTESIAN_POINT('Ctrl Pts',(6.82111401199994,12.2,-8.17163562200001));
#170365=CARTESIAN_POINT('Ctrl Pts',(6.82013060499994,12.2,-8.16962524400001));
#170366=CARTESIAN_POINT('Ctrl Pts',(6.81914833299994,12.2,-8.16762167300002));
#170367=CARTESIAN_POINT('Ctrl Pts',(6.81816721399994,12.2,-8.16562491600001));
#170368=CARTESIAN_POINT('Ctrl Pts',(6.81718726299994,12.2,-8.16363498000002));
#170369=CARTESIAN_POINT('Ctrl Pts',(6.81620849499994,12.2,-8.16165187500001));
#170370=CARTESIAN_POINT('Ctrl Pts',(6.81523092699994,12.2,-8.15967560500001));
#170371=CARTESIAN_POINT('Ctrl Pts',(6.81425457199994,12.2,-8.15770618000002));
#170372=CARTESIAN_POINT('Ctrl Pts',(6.81327944699994,12.2,-8.15574360800002));
#170373=CARTESIAN_POINT('Ctrl Pts',(6.81230556799994,12.2,-8.15378789600001));
#170374=CARTESIAN_POINT('Ctrl Pts',(6.81133295099994,12.2,-8.15183905000002));
#170375=CARTESIAN_POINT('Ctrl Pts',(6.81036160899994,12.2,-8.14989708200001));
#170376=CARTESIAN_POINT('Ctrl Pts',(6.80939156199994,12.2,-8.14796199600002));
#170377=CARTESIAN_POINT('Ctrl Pts',(6.80842282199994,12.2,-8.14603380000002));
#170378=CARTESIAN_POINT('Ctrl Pts',(6.80745540699994,12.2,-8.14411250400001));
#170379=CARTESIAN_POINT('Ctrl Pts',(6.80648933299994,12.2,-8.14219811500001));
#170380=CARTESIAN_POINT('Ctrl Pts',(6.80552461599994,12.2,-8.14029063900002));
#170381=CARTESIAN_POINT('Ctrl Pts',(6.80456127099994,12.2,-8.13839008500001));
#170382=CARTESIAN_POINT('Ctrl Pts',(6.80359931599994,12.2,-8.13649646300002));
#170383=CARTESIAN_POINT('Ctrl Pts',(6.80263876599994,12.2,-8.13460977800002));
#170384=CARTESIAN_POINT('Ctrl Pts',(6.80167963599994,12.2,-8.13273003800001));
#170385=CARTESIAN_POINT('Ctrl Pts',(6.80072194599994,12.2,-8.13085725200001));
#170386=CARTESIAN_POINT('Ctrl Pts',(6.79976570799994,12.2,-8.12899142800001));
#170387=CARTESIAN_POINT('Ctrl Pts',(6.79881094199994,12.2,-8.12713257400001));
#170388=CARTESIAN_POINT('Ctrl Pts',(6.79785766299994,12.2,-8.12528069600001));
#170389=CARTESIAN_POINT('Ctrl Pts',(6.79690588799994,12.2,-8.12343580400002));
#170390=CARTESIAN_POINT('Ctrl Pts',(6.79595563299995,12.2,-8.12159790600001));
#170391=CARTESIAN_POINT('Ctrl Pts',(6.79500691399994,12.2,-8.11976700800002));
#170392=CARTESIAN_POINT('Ctrl Pts',(6.79405974999994,12.2,-8.11794312000002));
#170393=CARTESIAN_POINT('Ctrl Pts',(6.79311415699994,12.2,-8.11612625000001));
#170394=CARTESIAN_POINT('Ctrl Pts',(6.79217014999994,12.2,-8.11431640400002));
#170395=CARTESIAN_POINT('Ctrl Pts',(6.79122774799994,12.2,-8.11251359100002));
#170396=CARTESIAN_POINT('Ctrl Pts',(6.79028696699994,12.2,-8.11071782000001));
#170397=CARTESIAN_POINT('Ctrl Pts',(6.78934782399994,12.2,-8.10892909900002));
#170398=CARTESIAN_POINT('Ctrl Pts',(6.78841033799994,12.2,-8.10714743400002));
#170399=CARTESIAN_POINT('Ctrl Pts',(6.78747452299994,12.2,-8.10537283700001));
#170400=CARTESIAN_POINT('Ctrl Pts',(6.78654039799994,12.2,-8.10360531100002));
#170401=CARTESIAN_POINT('Ctrl Pts',(6.78560798099994,12.2,-8.10184486900001));
#170402=CARTESIAN_POINT('Ctrl Pts',(6.78467728799995,12.2,-8.10009151600001));
#170403=CARTESIAN_POINT('Ctrl Pts',(6.78374833699994,12.2,-8.09834526200002));
#170404=CARTESIAN_POINT('Ctrl Pts',(6.78282114499994,12.2,-8.09660611400002));
#170405=CARTESIAN_POINT('Ctrl Pts',(6.78189572999995,12.2,-8.09487408000002));
#170406=CARTESIAN_POINT('Ctrl Pts',(6.78097211099994,12.2,-8.09314916800002));
#170407=CARTESIAN_POINT('Ctrl Pts',(6.78005030299994,12.2,-8.09143138900002));
#170408=CARTESIAN_POINT('Ctrl Pts',(6.77913032499994,12.2,-8.08972074800002));
#170409=CARTESIAN_POINT('Ctrl Pts',(6.77821219499994,12.2,-8.08801725500001));
#170410=CARTESIAN_POINT('Ctrl Pts',(6.77729593099994,12.2,-8.08632091800002));
#170411=CARTESIAN_POINT('Ctrl Pts',(6.77638154999994,12.2,-8.08463174500002));
#170412=CARTESIAN_POINT('Ctrl Pts',(6.77546907099994,12.2,-8.08294974400001));
#170413=CARTESIAN_POINT('Ctrl Pts',(6.77455851199994,12.2,-8.08127492400001));
#170414=CARTESIAN_POINT('Ctrl Pts',(6.77364988999994,12.2,-8.07960729300002));
#170415=CARTESIAN_POINT('Ctrl Pts',(6.77274322499994,12.2,-8.07794686000002));
#170416=CARTESIAN_POINT('Ctrl Pts',(6.77183853299994,12.2,-8.07629363200002));
#170417=CARTESIAN_POINT('Ctrl Pts',(6.77093583499994,12.2,-8.07464761900002));
#170418=CARTESIAN_POINT('Ctrl Pts',(6.77003514699994,12.2,-8.07300882800002));
#170419=CARTESIAN_POINT('Ctrl Pts',(6.76913648999995,12.2,-8.07137726900002));
#170420=CARTESIAN_POINT('Ctrl Pts',(6.76823988099994,12.2,-8.06975294900001));
#170421=CARTESIAN_POINT('Ctrl Pts',(6.76734533799995,12.2,-8.06813587700002));
#170422=CARTESIAN_POINT('Ctrl Pts',(6.76645288099994,12.2,-8.06652606100002));
#170423=CARTESIAN_POINT('Ctrl Pts',(6.76556252799994,12.2,-8.06492351100001));
#170424=CARTESIAN_POINT('Ctrl Pts',(6.76467429899994,12.2,-8.06332823600002));
#170425=CARTESIAN_POINT('Ctrl Pts',(6.76378821099994,12.2,-8.06174024100001));
#170426=CARTESIAN_POINT('Ctrl Pts',(6.76290428599994,12.2,-8.06015953800001));
#170427=CARTESIAN_POINT('Ctrl Pts',(6.76202253899994,12.2,-8.05858613400002));
#170428=CARTESIAN_POINT('Ctrl Pts',(6.76114299199994,12.2,-8.05702003800001));
#170429=CARTESIAN_POINT('Ctrl Pts',(6.76026566399995,12.2,-8.05546125900002));
#170430=CARTESIAN_POINT('Ctrl Pts',(6.75939057299995,12.2,-8.05390980500002));
#170431=CARTESIAN_POINT('Ctrl Pts',(6.75851773999994,12.2,-8.05236568400002));
#170432=CARTESIAN_POINT('Ctrl Pts',(6.75764718299994,12.2,-8.05082890700002));
#170433=CARTESIAN_POINT('Ctrl Pts',(6.75677892299994,12.2,-8.04929948100002));
#170434=CARTESIAN_POINT('Ctrl Pts',(6.75591297799994,12.2,-8.04777741600001));
#170435=CARTESIAN_POINT('Ctrl Pts',(6.75504936899994,12.2,-8.04626271800002));
#170436=CARTESIAN_POINT('Ctrl Pts',(6.75418811399994,12.2,-8.04475539900002));
#170437=CARTESIAN_POINT('Ctrl Pts',(6.75332923499994,12.2,-8.04325546600002));
#170438=CARTESIAN_POINT('Ctrl Pts',(6.75247275099994,12.2,-8.04176292900001));
#170439=CARTESIAN_POINT('Ctrl Pts',(6.75161868199995,12.2,-8.04027779500002));
#170440=CARTESIAN_POINT('Ctrl Pts',(6.75076704799995,12.2,-8.03880007500002));
#170441=CARTESIAN_POINT('Ctrl Pts',(6.74991786899994,12.2,-8.03732977600001));
#170442=CARTESIAN_POINT('Ctrl Pts',(6.74907116499995,12.2,-8.03586690800002));
#170443=CARTESIAN_POINT('Ctrl Pts',(6.74822695699994,12.2,-8.03441148000001));
#170444=CARTESIAN_POINT('Ctrl Pts',(6.74738526499994,12.2,-8.03296350100002));
#170445=CARTESIAN_POINT('Ctrl Pts',(6.74654610999994,12.2,-8.03152298000001));
#170446=CARTESIAN_POINT('Ctrl Pts',(6.74570951199994,12.2,-8.03008992500001));
#170447=CARTESIAN_POINT('Ctrl Pts',(6.74487549099994,12.2,-8.02866434600002));
#170448=CARTESIAN_POINT('Ctrl Pts',(6.74404406899995,12.2,-8.02724625000002));
#170449=CARTESIAN_POINT('Ctrl Pts',(6.74321526699995,12.2,-8.02583564900001));
#170450=CARTESIAN_POINT('Ctrl Pts',(6.74238910499994,12.2,-8.02443255100002));
#170451=CARTESIAN_POINT('Ctrl Pts',(6.74156560399994,12.2,-8.02303696500001));
#170452=CARTESIAN_POINT('Ctrl Pts',(6.74074478399994,12.2,-8.02164890000002));
#170453=CARTESIAN_POINT('Ctrl Pts',(6.73992666899994,12.2,-8.02026836500002));
#170454=CARTESIAN_POINT('Ctrl Pts',(6.73911127899994,12.2,-8.01889537000001));
#170455=CARTESIAN_POINT('Ctrl Pts',(6.73829863399994,12.2,-8.01752992300001));
#170456=CARTESIAN_POINT('Ctrl Pts',(6.73748875699994,12.2,-8.01617203400001));
#170457=CARTESIAN_POINT('Ctrl Pts',(6.73668166999994,12.2,-8.01482171200002));
#170458=CARTESIAN_POINT('Ctrl Pts',(6.73587739199994,12.2,-8.01347896600002));
#170459=CARTESIAN_POINT('Ctrl Pts',(6.73507594699994,12.2,-8.01214380700002));
#170460=CARTESIAN_POINT('Ctrl Pts',(6.73427735599994,12.2,-8.01081624200001));
#170461=CARTESIAN_POINT('Ctrl Pts',(6.73348164099994,12.2,-8.00949628200001));
#170462=CARTESIAN_POINT('Ctrl Pts',(6.73268882399994,12.2,-8.00818393500002));
#170463=CARTESIAN_POINT('Ctrl Pts',(6.73189892699994,12.2,-8.00687921200002));
#170464=CARTESIAN_POINT('Ctrl Pts',(6.73111197299994,12.2,-8.00558212100002));
#170465=CARTESIAN_POINT('Ctrl Pts',(6.73032798299994,12.2,-8.00429267200002));
#170466=CARTESIAN_POINT('Ctrl Pts',(6.72954697899995,12.2,-8.00301087500002));
#170467=CARTESIAN_POINT('Ctrl Pts',(6.72876898499994,12.2,-8.00173673800002));
#170468=CARTESIAN_POINT('Ctrl Pts',(6.72799402199994,12.2,-8.00047027200002));
#170469=CARTESIAN_POINT('Ctrl Pts',(6.72722211399994,12.2,-7.99921148700002));
#170470=CARTESIAN_POINT('Ctrl Pts',(6.72645328299994,12.2,-7.99796039100002));
#170471=CARTESIAN_POINT('Ctrl Pts',(6.72568755199995,12.2,-7.99671699400001));
#170472=CARTESIAN_POINT('Ctrl Pts',(6.72492494399994,12.2,-7.99548130700002));
#170473=CARTESIAN_POINT('Ctrl Pts',(6.72416548199994,12.2,-7.99425333800002));
#170474=CARTESIAN_POINT('Ctrl Pts',(6.72340918899994,12.2,-7.99303309800001));
#170475=CARTESIAN_POINT('Ctrl Pts',(6.72265608899994,12.2,-7.99182059500002));
#170476=CARTESIAN_POINT('Ctrl Pts',(6.72190620499994,12.2,-7.99061584100001));
#170477=CARTESIAN_POINT('Ctrl Pts',(6.72115955899995,12.2,-7.98941884400002));
#170478=CARTESIAN_POINT('Ctrl Pts',(6.72041617599994,12.2,-7.98822961300001));
#170479=CARTESIAN_POINT('Ctrl Pts',(6.71967607999994,12.2,-7.98704816100001));
#170480=CARTESIAN_POINT('Ctrl Pts',(6.71893929399995,12.2,-7.98587449600002));
#170481=CARTESIAN_POINT('Ctrl Pts',(6.71820584199994,12.2,-7.98470862800002));
#170482=CARTESIAN_POINT('Ctrl Pts',(6.71747574699994,12.2,-7.98355056600002));
#170483=CARTESIAN_POINT('Ctrl Pts',(6.71674903499994,12.2,-7.98240032100002));
#170484=CARTESIAN_POINT('Ctrl Pts',(6.71602572899994,12.2,-7.98125790400002));
#170485=CARTESIAN_POINT('Ctrl Pts',(6.71530585299994,12.2,-7.98012332400001));
#170486=CARTESIAN_POINT('Ctrl Pts',(6.71458943199994,12.2,-7.97899659000001));
#170487=CARTESIAN_POINT('Ctrl Pts',(6.71387649099994,12.2,-7.97787771300002));
#170488=CARTESIAN_POINT('Ctrl Pts',(6.71316705499994,12.2,-7.97676670400002));
#170489=CARTESIAN_POINT('Ctrl Pts',(6.71246114699994,12.2,-7.97566357200001));
#170490=CARTESIAN_POINT('Ctrl Pts',(6.71175879199994,12.2,-7.97456832700002));
#170491=CARTESIAN_POINT('Ctrl Pts',(6.71106001699994,12.2,-7.97348098000001));
#170492=CARTESIAN_POINT('Ctrl Pts',(6.71036484499994,12.2,-7.97240154000002));
#170493=CARTESIAN_POINT('Ctrl Pts',(6.70967330099994,12.2,-7.97133002000002));
#170494=CARTESIAN_POINT('Ctrl Pts',(6.70898541199994,12.2,-7.97026642700001));
#170495=CARTESIAN_POINT('Ctrl Pts',(6.70830120299994,12.2,-7.96921077400001));
#170496=CARTESIAN_POINT('Ctrl Pts',(6.70762069999994,12.2,-7.96816306900002));
#170497=CARTESIAN_POINT('Ctrl Pts',(6.70694392699994,12.2,-7.96712332400002));
#170498=CARTESIAN_POINT('Ctrl Pts',(6.70627090999995,12.2,-7.96609155000001));
#170499=CARTESIAN_POINT('Ctrl Pts',(6.70560167699994,12.2,-7.96506775500001));
#170500=CARTESIAN_POINT('Ctrl Pts',(6.70493625199994,12.2,-7.96405195200002));
#170501=CARTESIAN_POINT('Ctrl Pts',(6.70427466299994,12.2,-7.96304415000002));
#170502=CARTESIAN_POINT('Ctrl Pts',(6.70361693399994,12.2,-7.96204436100002));
#170503=CARTESIAN_POINT('Ctrl Pts',(6.70296309299995,12.2,-7.96105259300001));
#170504=CARTESIAN_POINT('Ctrl Pts',(6.70231316599994,12.2,-7.96006886000002));
#170505=CARTESIAN_POINT('Ctrl Pts',(6.70166717899995,12.2,-7.95909317200002));
#170506=CARTESIAN_POINT('Ctrl Pts',(6.70102515999995,12.2,-7.95812553600002));
#170507=CARTESIAN_POINT('Ctrl Pts',(6.70038713599994,12.2,-7.95716596700001));
#170508=CARTESIAN_POINT('Ctrl Pts',(6.69975313299994,12.2,-7.95621447500002));
#170509=CARTESIAN_POINT('Ctrl Pts',(6.69912317899994,12.2,-7.95527107000002));
#170510=CARTESIAN_POINT('Ctrl Pts',(6.69849730099994,12.2,-7.95433576200002));
#170511=CARTESIAN_POINT('Ctrl Pts',(6.69787552599994,12.2,-7.95340856300002));
#170512=CARTESIAN_POINT('Ctrl Pts',(6.69725788299994,12.2,-7.95248948500002));
#170513=CARTESIAN_POINT('Ctrl Pts',(6.69664439799995,12.2,-7.95157853800001));
#170514=CARTESIAN_POINT('Ctrl Pts',(6.69603509999994,12.2,-7.95067573100001));
#170515=CARTESIAN_POINT('Ctrl Pts',(6.69543001599994,12.2,-7.94978107900001));
#170516=CARTESIAN_POINT('Ctrl Pts',(6.69482917499994,12.2,-7.94889459000002));
#170517=CARTESIAN_POINT('Ctrl Pts',(6.69423260499994,12.2,-7.94801627700001));
#170518=CARTESIAN_POINT('Ctrl Pts',(6.69364033499994,12.2,-7.94714614900002));
#170519=CARTESIAN_POINT('Ctrl Pts',(6.69305239199994,12.2,-7.94628422000001));
#170520=CARTESIAN_POINT('Ctrl Pts',(6.69246880599994,12.2,-7.94543049900001));
#170521=CARTESIAN_POINT('Ctrl Pts',(6.69188960599994,12.2,-7.94458500000002));
#170522=CARTESIAN_POINT('Ctrl Pts',(6.69131482099995,12.2,-7.94374773000002));
#170523=CARTESIAN_POINT('Ctrl Pts',(6.69074447799994,12.2,-7.94291870500002));
#170524=CARTESIAN_POINT('Ctrl Pts',(6.69017860899995,12.2,-7.94209793300002));
#170525=CARTESIAN_POINT('Ctrl Pts',(6.68961724099994,12.2,-7.94128542600002));
#170526=CARTESIAN_POINT('Ctrl Pts',(6.68906040599994,12.2,-7.94048119900002));
#170527=CARTESIAN_POINT('Ctrl Pts',(6.68850813299994,12.2,-7.93968525900001));
#170528=CARTESIAN_POINT('Ctrl Pts',(6.68796045099994,12.2,-7.93889762000001));
#170529=CARTESIAN_POINT('Ctrl Pts',(6.68741739099994,12.2,-7.93811829200001));
#170530=CARTESIAN_POINT('Ctrl Pts',(6.68687898199994,12.2,-7.93734729000001));
#170531=CARTESIAN_POINT('Ctrl Pts',(6.68634525499994,12.2,-7.93658462300002));
#170532=CARTESIAN_POINT('Ctrl Pts',(6.68581928699994,12.2,-7.93583464600002));
#170533=CARTESIAN_POINT('Ctrl Pts',(6.68540286299995,12.2,-7.93524212600002));
#170534=CARTESIAN_POINT('Ctrl Pts',(6.68509340699995,12.2,-7.93480250500001));
#170535=CARTESIAN_POINT('Ctrl Pts',(6.68488903399994,12.2,-7.93451247200001));
#170536=CARTESIAN_POINT('Ctrl Pts',(6.68478856699994,12.2,-7.93436996900001));
#170537=CARTESIAN_POINT('Ctrl Pts',(6.68478856699994,15.2,-7.93436996900001));
#170538=CARTESIAN_POINT('Ctrl Pts',(6.68488903399994,15.2,-7.93451247200001));
#170539=CARTESIAN_POINT('Ctrl Pts',(6.68509340699995,15.2,-7.93480250500001));
#170540=CARTESIAN_POINT('Ctrl Pts',(6.68540286299995,15.2,-7.93524212600002));
#170541=CARTESIAN_POINT('Ctrl Pts',(6.68581928699994,15.2,-7.93583464600002));
#170542=CARTESIAN_POINT('Ctrl Pts',(6.68634525499994,15.2,-7.93658462300002));
#170543=CARTESIAN_POINT('Ctrl Pts',(6.68687898199994,15.2,-7.93734729000001));
#170544=CARTESIAN_POINT('Ctrl Pts',(6.68741739099994,15.2,-7.93811829200001));
#170545=CARTESIAN_POINT('Ctrl Pts',(6.68796045099994,15.2,-7.93889762000001));
#170546=CARTESIAN_POINT('Ctrl Pts',(6.68850813299994,15.2,-7.93968525900001));
#170547=CARTESIAN_POINT('Ctrl Pts',(6.68906040599994,15.2,-7.94048119900002));
#170548=CARTESIAN_POINT('Ctrl Pts',(6.68961724099994,15.2,-7.94128542600002));
#170549=CARTESIAN_POINT('Ctrl Pts',(6.69017860899995,15.2,-7.94209793300002));
#170550=CARTESIAN_POINT('Ctrl Pts',(6.69074447799994,15.2,-7.94291870500002));
#170551=CARTESIAN_POINT('Ctrl Pts',(6.69131482099995,15.2,-7.94374773000002));
#170552=CARTESIAN_POINT('Ctrl Pts',(6.69188960599994,15.2,-7.94458500000002));
#170553=CARTESIAN_POINT('Ctrl Pts',(6.69246880599994,15.2,-7.94543049900001));
#170554=CARTESIAN_POINT('Ctrl Pts',(6.69305239199994,15.2,-7.94628422000001));
#170555=CARTESIAN_POINT('Ctrl Pts',(6.69364033499994,15.2,-7.94714614900002));
#170556=CARTESIAN_POINT('Ctrl Pts',(6.69423260499994,15.2,-7.94801627700001));
#170557=CARTESIAN_POINT('Ctrl Pts',(6.69482917499994,15.2,-7.94889459000002));
#170558=CARTESIAN_POINT('Ctrl Pts',(6.69543001599994,15.2,-7.94978107900001));
#170559=CARTESIAN_POINT('Ctrl Pts',(6.69603509999994,15.2,-7.95067573100001));
#170560=CARTESIAN_POINT('Ctrl Pts',(6.69664439799995,15.2,-7.95157853800001));
#170561=CARTESIAN_POINT('Ctrl Pts',(6.69725788299994,15.2,-7.95248948500002));
#170562=CARTESIAN_POINT('Ctrl Pts',(6.69787552599994,15.2,-7.95340856300002));
#170563=CARTESIAN_POINT('Ctrl Pts',(6.69849730099994,15.2,-7.95433576200002));
#170564=CARTESIAN_POINT('Ctrl Pts',(6.69912317899994,15.2,-7.95527107000002));
#170565=CARTESIAN_POINT('Ctrl Pts',(6.69975313299994,15.2,-7.95621447500002));
#170566=CARTESIAN_POINT('Ctrl Pts',(6.70038713599994,15.2,-7.95716596700001));
#170567=CARTESIAN_POINT('Ctrl Pts',(6.70102515999995,15.2,-7.95812553600002));
#170568=CARTESIAN_POINT('Ctrl Pts',(6.70166717899995,15.2,-7.95909317200002));
#170569=CARTESIAN_POINT('Ctrl Pts',(6.70231316599994,15.2,-7.96006886000002));
#170570=CARTESIAN_POINT('Ctrl Pts',(6.70296309299995,15.2,-7.96105259300001));
#170571=CARTESIAN_POINT('Ctrl Pts',(6.70361693399994,15.2,-7.96204436100002));
#170572=CARTESIAN_POINT('Ctrl Pts',(6.70427466299994,15.2,-7.96304415000002));
#170573=CARTESIAN_POINT('Ctrl Pts',(6.70493625199994,15.2,-7.96405195200002));
#170574=CARTESIAN_POINT('Ctrl Pts',(6.70560167699994,15.2,-7.96506775500001));
#170575=CARTESIAN_POINT('Ctrl Pts',(6.70627090999995,15.2,-7.96609155000001));
#170576=CARTESIAN_POINT('Ctrl Pts',(6.70694392699994,15.2,-7.96712332400002));
#170577=CARTESIAN_POINT('Ctrl Pts',(6.70762069999994,15.2,-7.96816306900002));
#170578=CARTESIAN_POINT('Ctrl Pts',(6.70830120299994,15.2,-7.96921077400001));
#170579=CARTESIAN_POINT('Ctrl Pts',(6.70898541199994,15.2,-7.97026642700001));
#170580=CARTESIAN_POINT('Ctrl Pts',(6.70967330099994,15.2,-7.97133002000002));
#170581=CARTESIAN_POINT('Ctrl Pts',(6.71036484499994,15.2,-7.97240154000002));
#170582=CARTESIAN_POINT('Ctrl Pts',(6.71106001699994,15.2,-7.97348098000001));
#170583=CARTESIAN_POINT('Ctrl Pts',(6.71175879199994,15.2,-7.97456832700002));
#170584=CARTESIAN_POINT('Ctrl Pts',(6.71246114699994,15.2,-7.97566357200001));
#170585=CARTESIAN_POINT('Ctrl Pts',(6.71316705499994,15.2,-7.97676670400002));
#170586=CARTESIAN_POINT('Ctrl Pts',(6.71387649099994,15.2,-7.97787771300002));
#170587=CARTESIAN_POINT('Ctrl Pts',(6.71458943199994,15.2,-7.97899659000001));
#170588=CARTESIAN_POINT('Ctrl Pts',(6.71530585299994,15.2,-7.98012332400001));
#170589=CARTESIAN_POINT('Ctrl Pts',(6.71602572899994,15.2,-7.98125790400002));
#170590=CARTESIAN_POINT('Ctrl Pts',(6.71674903499994,15.2,-7.98240032100002));
#170591=CARTESIAN_POINT('Ctrl Pts',(6.71747574699994,15.2,-7.98355056600002));
#170592=CARTESIAN_POINT('Ctrl Pts',(6.71820584199994,15.2,-7.98470862800002));
#170593=CARTESIAN_POINT('Ctrl Pts',(6.71893929399995,15.2,-7.98587449600002));
#170594=CARTESIAN_POINT('Ctrl Pts',(6.71967607999994,15.2,-7.98704816100001));
#170595=CARTESIAN_POINT('Ctrl Pts',(6.72041617599994,15.2,-7.98822961300001));
#170596=CARTESIAN_POINT('Ctrl Pts',(6.72115955899995,15.2,-7.98941884400002));
#170597=CARTESIAN_POINT('Ctrl Pts',(6.72190620499994,15.2,-7.99061584100001));
#170598=CARTESIAN_POINT('Ctrl Pts',(6.72265608899994,15.2,-7.99182059500002));
#170599=CARTESIAN_POINT('Ctrl Pts',(6.72340918899994,15.2,-7.99303309800001));
#170600=CARTESIAN_POINT('Ctrl Pts',(6.72416548199994,15.2,-7.99425333800002));
#170601=CARTESIAN_POINT('Ctrl Pts',(6.72492494399994,15.2,-7.99548130700002));
#170602=CARTESIAN_POINT('Ctrl Pts',(6.72568755199995,15.2,-7.99671699400001));
#170603=CARTESIAN_POINT('Ctrl Pts',(6.72645328299994,15.2,-7.99796039100002));
#170604=CARTESIAN_POINT('Ctrl Pts',(6.72722211399994,15.2,-7.99921148700002));
#170605=CARTESIAN_POINT('Ctrl Pts',(6.72799402199994,15.2,-8.00047027200002));
#170606=CARTESIAN_POINT('Ctrl Pts',(6.72876898499994,15.2,-8.00173673800002));
#170607=CARTESIAN_POINT('Ctrl Pts',(6.72954697899995,15.2,-8.00301087500002));
#170608=CARTESIAN_POINT('Ctrl Pts',(6.73032798299994,15.2,-8.00429267200002));
#170609=CARTESIAN_POINT('Ctrl Pts',(6.73111197299994,15.2,-8.00558212100002));
#170610=CARTESIAN_POINT('Ctrl Pts',(6.73189892699994,15.2,-8.00687921200002));
#170611=CARTESIAN_POINT('Ctrl Pts',(6.73268882399994,15.2,-8.00818393500002));
#170612=CARTESIAN_POINT('Ctrl Pts',(6.73348164099994,15.2,-8.00949628200001));
#170613=CARTESIAN_POINT('Ctrl Pts',(6.73427735599994,15.2,-8.01081624200001));
#170614=CARTESIAN_POINT('Ctrl Pts',(6.73507594699994,15.2,-8.01214380700002));
#170615=CARTESIAN_POINT('Ctrl Pts',(6.73587739199994,15.2,-8.01347896600002));
#170616=CARTESIAN_POINT('Ctrl Pts',(6.73668166999994,15.2,-8.01482171200002));
#170617=CARTESIAN_POINT('Ctrl Pts',(6.73748875699994,15.2,-8.01617203400001));
#170618=CARTESIAN_POINT('Ctrl Pts',(6.73829863399994,15.2,-8.01752992300001));
#170619=CARTESIAN_POINT('Ctrl Pts',(6.73911127899994,15.2,-8.01889537000001));
#170620=CARTESIAN_POINT('Ctrl Pts',(6.73992666899994,15.2,-8.02026836500002));
#170621=CARTESIAN_POINT('Ctrl Pts',(6.74074478399994,15.2,-8.02164890000002));
#170622=CARTESIAN_POINT('Ctrl Pts',(6.74156560399994,15.2,-8.02303696500001));
#170623=CARTESIAN_POINT('Ctrl Pts',(6.74238910499994,15.2,-8.02443255100002));
#170624=CARTESIAN_POINT('Ctrl Pts',(6.74321526699995,15.2,-8.02583564900001));
#170625=CARTESIAN_POINT('Ctrl Pts',(6.74404406899995,15.2,-8.02724625000002));
#170626=CARTESIAN_POINT('Ctrl Pts',(6.74487549099994,15.2,-8.02866434600002));
#170627=CARTESIAN_POINT('Ctrl Pts',(6.74570951199994,15.2,-8.03008992500001));
#170628=CARTESIAN_POINT('Ctrl Pts',(6.74654610999994,15.2,-8.03152298000001));
#170629=CARTESIAN_POINT('Ctrl Pts',(6.74738526499994,15.2,-8.03296350100002));
#170630=CARTESIAN_POINT('Ctrl Pts',(6.74822695699994,15.2,-8.03441148000001));
#170631=CARTESIAN_POINT('Ctrl Pts',(6.74907116499995,15.2,-8.03586690800002));
#170632=CARTESIAN_POINT('Ctrl Pts',(6.74991786899994,15.2,-8.03732977600001));
#170633=CARTESIAN_POINT('Ctrl Pts',(6.75076704799995,15.2,-8.03880007500002));
#170634=CARTESIAN_POINT('Ctrl Pts',(6.75161868199995,15.2,-8.04027779500002));
#170635=CARTESIAN_POINT('Ctrl Pts',(6.75247275099994,15.2,-8.04176292900001));
#170636=CARTESIAN_POINT('Ctrl Pts',(6.75332923499994,15.2,-8.04325546600002));
#170637=CARTESIAN_POINT('Ctrl Pts',(6.75418811399994,15.2,-8.04475539900002));
#170638=CARTESIAN_POINT('Ctrl Pts',(6.75504936899994,15.2,-8.04626271800002));
#170639=CARTESIAN_POINT('Ctrl Pts',(6.75591297799994,15.2,-8.04777741600001));
#170640=CARTESIAN_POINT('Ctrl Pts',(6.75677892299994,15.2,-8.04929948100002));
#170641=CARTESIAN_POINT('Ctrl Pts',(6.75764718299994,15.2,-8.05082890700002));
#170642=CARTESIAN_POINT('Ctrl Pts',(6.75851773999994,15.2,-8.05236568400002));
#170643=CARTESIAN_POINT('Ctrl Pts',(6.75939057299995,15.2,-8.05390980500002));
#170644=CARTESIAN_POINT('Ctrl Pts',(6.76026566399995,15.2,-8.05546125900002));
#170645=CARTESIAN_POINT('Ctrl Pts',(6.76114299199994,15.2,-8.05702003800001));
#170646=CARTESIAN_POINT('Ctrl Pts',(6.76202253899994,15.2,-8.05858613400002));
#170647=CARTESIAN_POINT('Ctrl Pts',(6.76290428599994,15.2,-8.06015953800001));
#170648=CARTESIAN_POINT('Ctrl Pts',(6.76378821099994,15.2,-8.06174024100001));
#170649=CARTESIAN_POINT('Ctrl Pts',(6.76467429899994,15.2,-8.06332823600002));
#170650=CARTESIAN_POINT('Ctrl Pts',(6.76556252799994,15.2,-8.06492351100001));
#170651=CARTESIAN_POINT('Ctrl Pts',(6.76645288099994,15.2,-8.06652606100002));
#170652=CARTESIAN_POINT('Ctrl Pts',(6.76734533799995,15.2,-8.06813587700002));
#170653=CARTESIAN_POINT('Ctrl Pts',(6.76823988099994,15.2,-8.06975294900001));
#170654=CARTESIAN_POINT('Ctrl Pts',(6.76913648999995,15.2,-8.07137726900002));
#170655=CARTESIAN_POINT('Ctrl Pts',(6.77003514699994,15.2,-8.07300882800002));
#170656=CARTESIAN_POINT('Ctrl Pts',(6.77093583499994,15.2,-8.07464761900002));
#170657=CARTESIAN_POINT('Ctrl Pts',(6.77183853299994,15.2,-8.07629363200002));
#170658=CARTESIAN_POINT('Ctrl Pts',(6.77274322499994,15.2,-8.07794686000002));
#170659=CARTESIAN_POINT('Ctrl Pts',(6.77364988999994,15.2,-8.07960729300002));
#170660=CARTESIAN_POINT('Ctrl Pts',(6.77455851199994,15.2,-8.08127492400001));
#170661=CARTESIAN_POINT('Ctrl Pts',(6.77546907099994,15.2,-8.08294974400001));
#170662=CARTESIAN_POINT('Ctrl Pts',(6.77638154999994,15.2,-8.08463174500002));
#170663=CARTESIAN_POINT('Ctrl Pts',(6.77729593099994,15.2,-8.08632091800002));
#170664=CARTESIAN_POINT('Ctrl Pts',(6.77821219499994,15.2,-8.08801725500001));
#170665=CARTESIAN_POINT('Ctrl Pts',(6.77913032499994,15.2,-8.08972074800002));
#170666=CARTESIAN_POINT('Ctrl Pts',(6.78005030299994,15.2,-8.09143138900002));
#170667=CARTESIAN_POINT('Ctrl Pts',(6.78097211099994,15.2,-8.09314916800002));
#170668=CARTESIAN_POINT('Ctrl Pts',(6.78189572999995,15.2,-8.09487408000002));
#170669=CARTESIAN_POINT('Ctrl Pts',(6.78282114499994,15.2,-8.09660611400002));
#170670=CARTESIAN_POINT('Ctrl Pts',(6.78374833699994,15.2,-8.09834526200002));
#170671=CARTESIAN_POINT('Ctrl Pts',(6.78467728799995,15.2,-8.10009151600001));
#170672=CARTESIAN_POINT('Ctrl Pts',(6.78560798099994,15.2,-8.10184486900001));
#170673=CARTESIAN_POINT('Ctrl Pts',(6.78654039799994,15.2,-8.10360531100002));
#170674=CARTESIAN_POINT('Ctrl Pts',(6.78747452299994,15.2,-8.10537283700001));
#170675=CARTESIAN_POINT('Ctrl Pts',(6.78841033799994,15.2,-8.10714743400002));
#170676=CARTESIAN_POINT('Ctrl Pts',(6.78934782399994,15.2,-8.10892909900002));
#170677=CARTESIAN_POINT('Ctrl Pts',(6.79028696699994,15.2,-8.11071782000001));
#170678=CARTESIAN_POINT('Ctrl Pts',(6.79122774799994,15.2,-8.11251359100002));
#170679=CARTESIAN_POINT('Ctrl Pts',(6.79217014999994,15.2,-8.11431640400002));
#170680=CARTESIAN_POINT('Ctrl Pts',(6.79311415699994,15.2,-8.11612625000001));
#170681=CARTESIAN_POINT('Ctrl Pts',(6.79405974999994,15.2,-8.11794312000002));
#170682=CARTESIAN_POINT('Ctrl Pts',(6.79500691399994,15.2,-8.11976700800002));
#170683=CARTESIAN_POINT('Ctrl Pts',(6.79595563299995,15.2,-8.12159790600001));
#170684=CARTESIAN_POINT('Ctrl Pts',(6.79690588799994,15.2,-8.12343580400002));
#170685=CARTESIAN_POINT('Ctrl Pts',(6.79785766299994,15.2,-8.12528069600001));
#170686=CARTESIAN_POINT('Ctrl Pts',(6.79881094199994,15.2,-8.12713257400001));
#170687=CARTESIAN_POINT('Ctrl Pts',(6.79976570799994,15.2,-8.12899142800001));
#170688=CARTESIAN_POINT('Ctrl Pts',(6.80072194599994,15.2,-8.13085725200001));
#170689=CARTESIAN_POINT('Ctrl Pts',(6.80167963599994,15.2,-8.13273003800001));
#170690=CARTESIAN_POINT('Ctrl Pts',(6.80263876599994,15.2,-8.13460977800002));
#170691=CARTESIAN_POINT('Ctrl Pts',(6.80359931599994,15.2,-8.13649646300002));
#170692=CARTESIAN_POINT('Ctrl Pts',(6.80456127099994,15.2,-8.13839008500001));
#170693=CARTESIAN_POINT('Ctrl Pts',(6.80552461599994,15.2,-8.14029063900002));
#170694=CARTESIAN_POINT('Ctrl Pts',(6.80648933299994,15.2,-8.14219811500001));
#170695=CARTESIAN_POINT('Ctrl Pts',(6.80745540699994,15.2,-8.14411250400001));
#170696=CARTESIAN_POINT('Ctrl Pts',(6.80842282199994,15.2,-8.14603380000002));
#170697=CARTESIAN_POINT('Ctrl Pts',(6.80939156199994,15.2,-8.14796199600002));
#170698=CARTESIAN_POINT('Ctrl Pts',(6.81036160899994,15.2,-8.14989708200001));
#170699=CARTESIAN_POINT('Ctrl Pts',(6.81133295099994,15.2,-8.15183905000002));
#170700=CARTESIAN_POINT('Ctrl Pts',(6.81230556799994,15.2,-8.15378789600001));
#170701=CARTESIAN_POINT('Ctrl Pts',(6.81327944699994,15.2,-8.15574360800002));
#170702=CARTESIAN_POINT('Ctrl Pts',(6.81425457199994,15.2,-8.15770618000002));
#170703=CARTESIAN_POINT('Ctrl Pts',(6.81523092699994,15.2,-8.15967560500001));
#170704=CARTESIAN_POINT('Ctrl Pts',(6.81620849499994,15.2,-8.16165187500001));
#170705=CARTESIAN_POINT('Ctrl Pts',(6.81718726299994,15.2,-8.16363498000002));
#170706=CARTESIAN_POINT('Ctrl Pts',(6.81816721399994,15.2,-8.16562491600001));
#170707=CARTESIAN_POINT('Ctrl Pts',(6.81914833299994,15.2,-8.16762167300002));
#170708=CARTESIAN_POINT('Ctrl Pts',(6.82013060499994,15.2,-8.16962524400001));
#170709=CARTESIAN_POINT('Ctrl Pts',(6.82111401199994,15.2,-8.17163562200001));
#170710=CARTESIAN_POINT('Ctrl Pts',(6.82209854199994,15.2,-8.17365279700002));
#170711=CARTESIAN_POINT('Ctrl Pts',(6.82308417899994,15.2,-8.17567676500002));
#170712=CARTESIAN_POINT('Ctrl Pts',(6.82407090599995,15.2,-8.17770751500002));
#170713=CARTESIAN_POINT('Ctrl Pts',(6.82505870999995,15.2,-8.17974504100001));
#170714=CARTESIAN_POINT('Ctrl Pts',(6.82604757499995,15.2,-8.18178933600001));
#170715=CARTESIAN_POINT('Ctrl Pts',(6.82703748599994,15.2,-8.18384039100001));
#170716=CARTESIAN_POINT('Ctrl Pts',(6.82802842799994,15.2,-8.18589820000001));
#170717=CARTESIAN_POINT('Ctrl Pts',(6.82902038699994,15.2,-8.18796275400001));
#170718=CARTESIAN_POINT('Ctrl Pts',(6.83001334499994,15.2,-8.19003404700002));
#170719=CARTESIAN_POINT('Ctrl Pts',(6.83100729199994,15.2,-8.19211207100001));
#170720=CARTESIAN_POINT('Ctrl Pts',(6.83200220999994,15.2,-8.19419681600002));
#170721=CARTESIAN_POINT('Ctrl Pts',(6.83299808299994,15.2,-8.19628827900001));
#170722=CARTESIAN_POINT('Ctrl Pts',(6.83399489999994,15.2,-8.19838644900001));
#170723=CARTESIAN_POINT('Ctrl Pts',(6.83499264499994,15.2,-8.20049132000002));
#170724=CARTESIAN_POINT('Ctrl Pts',(6.83599130199994,15.2,-8.20260288400002));
#170725=CARTESIAN_POINT('Ctrl Pts',(6.83699085699994,15.2,-8.20472113600001));
#170726=CARTESIAN_POINT('Ctrl Pts',(6.83799129699994,15.2,-8.20684606400001));
#170727=CARTESIAN_POINT('Ctrl Pts',(6.83899260499994,15.2,-8.20897766300002));
#170728=CARTESIAN_POINT('Ctrl Pts',(6.83999476999994,15.2,-8.21111592700002));
#170729=CARTESIAN_POINT('Ctrl Pts',(6.84099777399994,15.2,-8.21326084700001));
#170730=CARTESIAN_POINT('Ctrl Pts',(6.84200160499994,15.2,-8.21541241600002));
#170731=CARTESIAN_POINT('Ctrl Pts',(6.84300624899994,15.2,-8.21757062500001));
#170732=CARTESIAN_POINT('Ctrl Pts',(6.84401168999995,15.2,-8.21973547000002));
#170733=CARTESIAN_POINT('Ctrl Pts',(6.84501791499994,15.2,-8.22190694200001));
#170734=CARTESIAN_POINT('Ctrl Pts',(6.84602490999994,15.2,-8.22408503200002));
#170735=CARTESIAN_POINT('Ctrl Pts',(6.84703265999994,15.2,-8.22626973500002));
#170736=CARTESIAN_POINT('Ctrl Pts',(6.84804115199994,15.2,-8.22846104400002));
#170737=CARTESIAN_POINT('Ctrl Pts',(6.84905037099995,15.2,-8.23065895000001));
#170738=CARTESIAN_POINT('Ctrl Pts',(6.85006030399994,15.2,-8.23286344400002));
#170739=CARTESIAN_POINT('Ctrl Pts',(6.85107093599994,15.2,-8.23507452400002));
#170740=CARTESIAN_POINT('Ctrl Pts',(6.85208225499994,15.2,-8.23729217900001));
#170741=CARTESIAN_POINT('Ctrl Pts',(6.85309424499994,15.2,-8.23951640200002));
#170742=CARTESIAN_POINT('Ctrl Pts',(6.85410689299994,15.2,-8.24174718600002));
#170743=CARTESIAN_POINT('Ctrl Pts',(6.85512018599994,15.2,-8.24398452500001));
#170744=CARTESIAN_POINT('Ctrl Pts',(6.85613410999995,15.2,-8.24622841000001));
#170745=CARTESIAN_POINT('Ctrl Pts',(6.85714865199994,15.2,-8.24847883600001));
#170746=CARTESIAN_POINT('Ctrl Pts',(6.85816379599994,15.2,-8.25073579300001));
#170747=CARTESIAN_POINT('Ctrl Pts',(6.85917953099994,15.2,-8.25299927600001));
#170748=CARTESIAN_POINT('Ctrl Pts',(6.86019584299994,15.2,-8.25526927700002));
#170749=CARTESIAN_POINT('Ctrl Pts',(6.86121271699994,15.2,-8.25754578900002));
#170750=CARTESIAN_POINT('Ctrl Pts',(6.86223014199994,15.2,-8.25982880500002));
#170751=CARTESIAN_POINT('Ctrl Pts',(6.86324810299995,15.2,-8.26211831700002));
#170752=CARTESIAN_POINT('Ctrl Pts',(6.86426658699994,15.2,-8.26441431900001));
#170753=CARTESIAN_POINT('Ctrl Pts',(6.86528557999995,15.2,-8.26671680300001));
#170754=CARTESIAN_POINT('Ctrl Pts',(6.86630506999995,15.2,-8.26902576200002));
#170755=CARTESIAN_POINT('Ctrl Pts',(6.86732504299994,15.2,-8.27134119000002));
#170756=CARTESIAN_POINT('Ctrl Pts',(6.86834548499994,15.2,-8.27366307800002));
#170757=CARTESIAN_POINT('Ctrl Pts',(6.86936638499994,15.2,-8.27599142100001));
#170758=CARTESIAN_POINT('Ctrl Pts',(6.87038772899994,15.2,-8.27832621000002));
#170759=CARTESIAN_POINT('Ctrl Pts',(6.87140950299994,15.2,-8.28066743900001));
#170760=CARTESIAN_POINT('Ctrl Pts',(6.87243169499994,15.2,-8.28301510100001));
#170761=CARTESIAN_POINT('Ctrl Pts',(6.87345429199994,15.2,-8.28536918900001));
#170762=CARTESIAN_POINT('Ctrl Pts',(6.87447728099994,15.2,-8.28772969500001));
#170763=CARTESIAN_POINT('Ctrl Pts',(6.87550064899995,15.2,-8.29009661300002));
#170764=CARTESIAN_POINT('Ctrl Pts',(6.87652438199994,15.2,-8.29246993600002));
#170765=CARTESIAN_POINT('Ctrl Pts',(6.87754846999994,15.2,-8.29484965700001));
#170766=CARTESIAN_POINT('Ctrl Pts',(6.87857289699994,15.2,-8.29723576700001));
#170767=CARTESIAN_POINT('Ctrl Pts',(6.87959765299994,15.2,-8.29962826200001));
#170768=CARTESIAN_POINT('Ctrl Pts',(6.88062272399995,15.2,-8.30202713300002));
#170769=CARTESIAN_POINT('Ctrl Pts',(6.88164809599995,15.2,-8.30443237500001));
#170770=CARTESIAN_POINT('Ctrl Pts',(6.88267375899994,15.2,-8.30684397800002));
#170771=CARTESIAN_POINT('Ctrl Pts',(6.88369969899994,15.2,-8.30926193800002));
#170772=CARTESIAN_POINT('Ctrl Pts',(6.88472590399994,15.2,-8.31168624500001));
#170773=CARTESIAN_POINT('Ctrl Pts',(6.88575235999994,15.2,-8.31411689700002));
#170774=CARTESIAN_POINT('Ctrl Pts',(6.88677905699994,15.2,-8.31655388200002));
#170775=CARTESIAN_POINT('Ctrl Pts',(6.88780597999994,15.2,-8.31899719600001));
#170776=CARTESIAN_POINT('Ctrl Pts',(6.88883311899994,15.2,-8.32144682900001));
#170777=CARTESIAN_POINT('Ctrl Pts',(6.88986046099994,15.2,-8.32390277900002));
#170778=CARTESIAN_POINT('Ctrl Pts',(6.89088799199994,15.2,-8.32636503500002));
#170779=CARTESIAN_POINT('Ctrl Pts',(6.89191570099994,15.2,-8.32883359100002));
#170780=CARTESIAN_POINT('Ctrl Pts',(6.89294357699994,15.2,-8.33130844200002));
#170781=CARTESIAN_POINT('Ctrl Pts',(6.89397160499994,15.2,-8.33378957900001));
#170782=CARTESIAN_POINT('Ctrl Pts',(6.89499977499994,15.2,-8.33627699600001));
#170783=CARTESIAN_POINT('Ctrl Pts',(6.89602807299995,15.2,-8.33877068600002));
#170784=CARTESIAN_POINT('Ctrl Pts',(6.89705648999994,15.2,-8.34127064300001));
#170785=CARTESIAN_POINT('Ctrl Pts',(6.89808501099994,15.2,-8.34377685900002));
#170786=CARTESIAN_POINT('Ctrl Pts',(6.89911362499994,15.2,-8.34628932700002));
#170787=CARTESIAN_POINT('Ctrl Pts',(6.90014232099994,15.2,-8.34880804200001));
#170788=CARTESIAN_POINT('Ctrl Pts',(6.90117108399994,15.2,-8.35133299500002));
#170789=CARTESIAN_POINT('Ctrl Pts',(6.90219990499994,15.2,-8.35386418100001));
#170790=CARTESIAN_POINT('Ctrl Pts',(6.90322877199994,15.2,-8.35640159100001));
#170791=CARTESIAN_POINT('Ctrl Pts',(6.90425767199994,15.2,-8.35894522000002));
#170792=CARTESIAN_POINT('Ctrl Pts',(6.90528659299994,15.2,-8.36149506200002));
#170793=CARTESIAN_POINT('Ctrl Pts',(6.90631552399994,15.2,-8.36405110800002));
#170794=CARTESIAN_POINT('Ctrl Pts',(6.90734445199994,15.2,-8.36661335300001));
#170795=CARTESIAN_POINT('Ctrl Pts',(6.90837336899994,15.2,-8.36918179000002));
#170796=CARTESIAN_POINT('Ctrl Pts',(6.90940225899995,15.2,-8.37175641100002));
#170797=CARTESIAN_POINT('Ctrl Pts',(6.91043111099994,15.2,-8.37433721000002));
#170798=CARTESIAN_POINT('Ctrl Pts',(6.91145991499994,15.2,-8.37692418200002));
#170799=CARTESIAN_POINT('Ctrl Pts',(6.91248865999994,15.2,-8.37951731700001));
#170800=CARTESIAN_POINT('Ctrl Pts',(6.91351733199994,15.2,-8.38211661100001));
#170801=CARTESIAN_POINT('Ctrl Pts',(6.91454591999995,15.2,-8.38472205600001));
#170802=CARTESIAN_POINT('Ctrl Pts',(6.91557441499994,15.2,-8.38733364600002));
#170803=CARTESIAN_POINT('Ctrl Pts',(6.91660280299994,15.2,-8.38995137300002));
#170804=CARTESIAN_POINT('Ctrl Pts',(6.91763107299994,15.2,-8.39257523200001));
#170805=CARTESIAN_POINT('Ctrl Pts',(6.91865921499994,15.2,-8.39520521500001));
#170806=CARTESIAN_POINT('Ctrl Pts',(6.91968721499994,15.2,-8.39784131600002));
#170807=CARTESIAN_POINT('Ctrl Pts',(6.92071506399994,15.2,-8.40048352900002));
#170808=CARTESIAN_POINT('Ctrl Pts',(6.92174274999994,15.2,-8.40313184700002));
#170809=CARTESIAN_POINT('Ctrl Pts',(6.92277026199994,15.2,-8.40578626200001));
#170810=CARTESIAN_POINT('Ctrl Pts',(6.92379758999994,15.2,-8.40844676800002));
#170811=CARTESIAN_POINT('Ctrl Pts',(6.92482471899995,15.2,-8.41111336100001));
#170812=CARTESIAN_POINT('Ctrl Pts',(6.92585164099994,15.2,-8.41378603000001));
#170813=CARTESIAN_POINT('Ctrl Pts',(6.92687834499995,15.2,-8.41646477200002));
#170814=CARTESIAN_POINT('Ctrl Pts',(6.92790481799994,15.2,-8.41914957800002));
#170815=CARTESIAN_POINT('Ctrl Pts',(6.92893105099994,15.2,-8.42184044300001));
#170816=CARTESIAN_POINT('Ctrl Pts',(6.92995702999994,15.2,-8.42453735900002));
#170817=CARTESIAN_POINT('Ctrl Pts',(6.93098274699994,15.2,-8.42724032100002));
#170818=CARTESIAN_POINT('Ctrl Pts',(6.93200819099994,15.2,-8.42994932100002));
#170819=CARTESIAN_POINT('Ctrl Pts',(6.93303334799994,15.2,-8.43266435400002));
#170820=CARTESIAN_POINT('Ctrl Pts',(6.93405820999994,15.2,-8.43538541100001));
#170821=CARTESIAN_POINT('Ctrl Pts',(6.93508276499994,15.2,-8.43811248900002));
#170822=CARTESIAN_POINT('Ctrl Pts',(6.93610700299994,15.2,-8.44084557900001));
#170823=CARTESIAN_POINT('Ctrl Pts',(6.93713091199994,15.2,-8.44358467400001));
#170824=CARTESIAN_POINT('Ctrl Pts',(6.93815448099994,15.2,-8.44632976900002));
#170825=CARTESIAN_POINT('Ctrl Pts',(6.93917770099994,15.2,-8.44908085600002));
#170826=CARTESIAN_POINT('Ctrl Pts',(6.94020055999995,15.2,-8.45183793000002));
#170827=CARTESIAN_POINT('Ctrl Pts',(6.94122304799994,15.2,-8.45460098400002));
#170828=CARTESIAN_POINT('Ctrl Pts',(6.94224515399994,15.2,-8.45737001200002));
#170829=CARTESIAN_POINT('Ctrl Pts',(6.94326686599994,15.2,-8.46014500600001));
#170830=CARTESIAN_POINT('Ctrl Pts',(6.94428817599994,15.2,-8.46292596000002));
#170831=CARTESIAN_POINT('Ctrl Pts',(6.94530907199994,15.2,-8.46571286900001));
#170832=CARTESIAN_POINT('Ctrl Pts',(6.94632954299994,15.2,-8.46850572500001));
#170833=CARTESIAN_POINT('Ctrl Pts',(6.94734957799994,15.2,-8.47130452200001));
#170834=CARTESIAN_POINT('Ctrl Pts',(6.94836916999994,15.2,-8.47410925300002));
#170835=CARTESIAN_POINT('Ctrl Pts',(6.94938830399995,15.2,-8.47691991200002));
#170836=CARTESIAN_POINT('Ctrl Pts',(6.95040697199994,15.2,-8.47973649400002));
#170837=CARTESIAN_POINT('Ctrl Pts',(6.95142516299994,15.2,-8.48255899100002));
#170838=CARTESIAN_POINT('Ctrl Pts',(6.95244286799994,15.2,-8.48538739600002));
#170839=CARTESIAN_POINT('Ctrl Pts',(6.95346007499994,15.2,-8.48822170300001));
#170840=CARTESIAN_POINT('Ctrl Pts',(6.95447677299994,15.2,-8.49106190600001));
#170841=CARTESIAN_POINT('Ctrl Pts',(6.95549295399994,15.2,-8.49390799900002));
#170842=CARTESIAN_POINT('Ctrl Pts',(6.95650860599994,15.2,-8.49675997600002));
#170843=CARTESIAN_POINT('Ctrl Pts',(6.95752371999995,15.2,-8.49961782800002));
#170844=CARTESIAN_POINT('Ctrl Pts',(6.95853828499994,15.2,-8.50248155200001));
#170845=CARTESIAN_POINT('Ctrl Pts',(6.95955229099994,15.2,-8.50535113900002));
#170846=CARTESIAN_POINT('Ctrl Pts',(6.96056572699994,15.2,-8.50822658400002));
#170847=CARTESIAN_POINT('Ctrl Pts',(6.96157858499994,15.2,-8.51110787900001));
#170848=CARTESIAN_POINT('Ctrl Pts',(6.96259085299994,15.2,-8.51399502000002));
#170849=CARTESIAN_POINT('Ctrl Pts',(6.96360252099994,15.2,-8.51688800000002));
#170850=CARTESIAN_POINT('Ctrl Pts',(6.96461357999994,15.2,-8.51978681100002));
#170851=CARTESIAN_POINT('Ctrl Pts',(6.96562401999994,15.2,-8.52269144800001));
#170852=CARTESIAN_POINT('Ctrl Pts',(6.96663382999994,15.2,-8.52560190500002));
#170853=CARTESIAN_POINT('Ctrl Pts',(6.96764299999994,15.2,-8.52851817400002));
#170854=CARTESIAN_POINT('Ctrl Pts',(6.96865152099994,15.2,-8.53144025000002));
#170855=CARTESIAN_POINT('Ctrl Pts',(6.96965938299994,15.2,-8.53436812800001));
#170856=CARTESIAN_POINT('Ctrl Pts',(6.97066657399994,15.2,-8.53730179900002));
#170857=CARTESIAN_POINT('Ctrl Pts',(6.97167308699994,15.2,-8.54024125700001));
#170858=CARTESIAN_POINT('Ctrl Pts',(6.97267891199994,15.2,-8.54318649800001));
#170859=CARTESIAN_POINT('Ctrl Pts',(6.97368403699994,15.2,-8.54613751400001));
#170860=CARTESIAN_POINT('Ctrl Pts',(6.97468845399994,15.2,-8.54909429700001));
#170861=CARTESIAN_POINT('Ctrl Pts',(6.97569215299994,15.2,-8.55205684500002));
#170862=CARTESIAN_POINT('Ctrl Pts',(6.97669512399994,15.2,-8.55502514800002));
#170863=CARTESIAN_POINT('Ctrl Pts',(6.97769735699994,15.2,-8.55799920200001));
#170864=CARTESIAN_POINT('Ctrl Pts',(6.97869884199994,15.2,-8.56097899900002));
#170865=CARTESIAN_POINT('Ctrl Pts',(6.97969957099994,15.2,-8.56396453400002));
#170866=CARTESIAN_POINT('Ctrl Pts',(6.98069953199994,15.2,-8.56695580000002));
#170867=CARTESIAN_POINT('Ctrl Pts',(6.98169871799994,15.2,-8.56995279200002));
#170868=CARTESIAN_POINT('Ctrl Pts',(6.98269711799994,15.2,-8.57295550200002));
#170869=CARTESIAN_POINT('Ctrl Pts',(6.98369472199994,15.2,-8.57596392400002));
#170870=CARTESIAN_POINT('Ctrl Pts',(6.98469152199994,15.2,-8.57897805400002));
#170871=CARTESIAN_POINT('Ctrl Pts',(6.98568750699994,15.2,-8.58199788300002));
#170872=CARTESIAN_POINT('Ctrl Pts',(6.98668266799994,15.2,-8.58502340600002));
#170873=CARTESIAN_POINT('Ctrl Pts',(6.98767699599994,15.2,-8.58805461600002));
#170874=CARTESIAN_POINT('Ctrl Pts',(6.98867048099994,15.2,-8.59109150800002));
#170875=CARTESIAN_POINT('Ctrl Pts',(6.98966311399994,15.2,-8.59413407600002));
#170876=CARTESIAN_POINT('Ctrl Pts',(6.99065488599994,15.2,-8.59718231200001));
#170877=CARTESIAN_POINT('Ctrl Pts',(6.99164578499994,15.2,-8.60023621100002));
#170878=CARTESIAN_POINT('Ctrl Pts',(6.99263580599994,15.2,-8.60329576700002));
#170879=CARTESIAN_POINT('Ctrl Pts',(6.99362493699994,15.2,-8.60636097400001));
#170880=CARTESIAN_POINT('Ctrl Pts',(6.99461316799994,15.2,-8.60943182400002));
#170881=CARTESIAN_POINT('Ctrl Pts',(6.99560049199994,15.2,-8.61250831300002));
#170882=CARTESIAN_POINT('Ctrl Pts',(6.99658689799994,15.2,-8.61559043400002));
#170883=CARTESIAN_POINT('Ctrl Pts',(6.99757237899994,15.2,-8.61867818100002));
#170884=CARTESIAN_POINT('Ctrl Pts',(6.99855692199994,15.2,-8.62177154700002));
#170885=CARTESIAN_POINT('Ctrl Pts',(6.99954052099995,15.2,-8.62487052700001));
#170886=CARTESIAN_POINT('Ctrl Pts',(7.00052316699994,15.2,-8.62797511400002));
#170887=CARTESIAN_POINT('Ctrl Pts',(7.00150484899994,15.2,-8.63108530300002));
#170888=CARTESIAN_POINT('Ctrl Pts',(7.00248555899995,15.2,-8.63420108600002));
#170889=CARTESIAN_POINT('Ctrl Pts',(7.00346528799995,15.2,-8.63732245800002));
#170890=CARTESIAN_POINT('Ctrl Pts',(7.00444402699994,15.2,-8.64044941300002));
#170891=CARTESIAN_POINT('Ctrl Pts',(7.00542176599994,15.2,-8.64358194500002));
#170892=CARTESIAN_POINT('Ctrl Pts',(7.00639849599995,15.2,-8.64672004800001));
#170893=CARTESIAN_POINT('Ctrl Pts',(7.00737420899994,15.2,-8.64986371400001));
#170894=CARTESIAN_POINT('Ctrl Pts',(7.00834889699994,15.2,-8.65301294000002));
#170895=CARTESIAN_POINT('Ctrl Pts',(7.00932254799994,15.2,-8.65616771800001));
#170896=CARTESIAN_POINT('Ctrl Pts',(7.01029515599994,15.2,-8.65932804100002));
#170897=CARTESIAN_POINT('Ctrl Pts',(7.01126671099995,15.2,-8.66249390500002));
#170898=CARTESIAN_POINT('Ctrl Pts',(7.01223720399994,15.2,-8.66566530400002));
#170899=CARTESIAN_POINT('Ctrl Pts',(7.01320662599994,15.2,-8.66884222900002));
#170900=CARTESIAN_POINT('Ctrl Pts',(7.01417496999994,15.2,-8.67202467700002));
#170901=CARTESIAN_POINT('Ctrl Pts',(7.01514222399994,15.2,-8.67521264000001));
#170902=CARTESIAN_POINT('Ctrl Pts',(7.01610838099994,15.2,-8.67840611400002));
#170903=CARTESIAN_POINT('Ctrl Pts',(7.01707343299995,15.2,-8.68160509100001));
#170904=CARTESIAN_POINT('Ctrl Pts',(7.01803736899994,15.2,-8.68480956600001));
#170905=CARTESIAN_POINT('Ctrl Pts',(7.01900018299995,15.2,-8.68801953100002));
#170906=CARTESIAN_POINT('Ctrl Pts',(7.01996186499994,15.2,-8.69123498300001));
#170907=CARTESIAN_POINT('Ctrl Pts',(7.02092240599994,15.2,-8.69445591400002));
#170908=CARTESIAN_POINT('Ctrl Pts',(7.02188179799994,15.2,-8.69768231900002));
#170909=CARTESIAN_POINT('Ctrl Pts',(7.02284003299994,15.2,-8.70091419100002));
#170910=CARTESIAN_POINT('Ctrl Pts',(7.02379709999994,15.2,-8.70415152400002));
#170911=CARTESIAN_POINT('Ctrl Pts',(7.02475299199994,15.2,-8.70739431300001));
#170912=CARTESIAN_POINT('Ctrl Pts',(7.02570770099994,15.2,-8.71064255100002));
#170913=CARTESIAN_POINT('Ctrl Pts',(7.02666121799994,15.2,-8.71389623300002));
#170914=CARTESIAN_POINT('Ctrl Pts',(7.02761353399994,15.2,-8.71715535200002));
#170915=CARTESIAN_POINT('Ctrl Pts',(7.02856464099994,15.2,-8.72041990300002));
#170916=CARTESIAN_POINT('Ctrl Pts',(7.02951453099994,15.2,-8.72368987800002));
#170917=CARTESIAN_POINT('Ctrl Pts',(7.03046319299995,15.2,-8.72696527400001));
#170918=CARTESIAN_POINT('Ctrl Pts',(7.03141062299995,15.2,-8.73024608200001));
#170919=CARTESIAN_POINT('Ctrl Pts',(7.03235680899994,15.2,-8.73353229700001));
#170920=CARTESIAN_POINT('Ctrl Pts',(7.03330174299994,15.2,-8.73682391500001));
#170921=CARTESIAN_POINT('Ctrl Pts',(7.03424541799994,15.2,-8.74012092800001));
#170922=CARTESIAN_POINT('Ctrl Pts',(7.03518782499994,15.2,-8.74342333000002));
#170923=CARTESIAN_POINT('Ctrl Pts',(7.03612895599995,15.2,-8.74673111600002));
#170924=CARTESIAN_POINT('Ctrl Pts',(7.03706880199994,15.2,-8.75004428000001));
#170925=CARTESIAN_POINT('Ctrl Pts',(7.03800735599994,15.2,-8.75336281500001));
#170926=CARTESIAN_POINT('Ctrl Pts',(7.03894460699994,15.2,-8.75668671600002));
#170927=CARTESIAN_POINT('Ctrl Pts',(7.03988054999994,15.2,-8.76001597500002));
#170928=CARTESIAN_POINT('Ctrl Pts',(7.04081517499994,15.2,-8.76335058900001));
#170929=CARTESIAN_POINT('Ctrl Pts',(7.04174847399995,15.2,-8.76669055200002));
#170930=CARTESIAN_POINT('Ctrl Pts',(7.04268043899994,15.2,-8.77003585600002));
#170931=CARTESIAN_POINT('Ctrl Pts',(7.04361106199995,15.2,-8.77338649600001));
#170932=CARTESIAN_POINT('Ctrl Pts',(7.04454033599994,15.2,-8.77674246600002));
#170933=CARTESIAN_POINT('Ctrl Pts',(7.04546824999994,15.2,-8.78010376100002));
#170934=CARTESIAN_POINT('Ctrl Pts',(7.04639479699994,15.2,-8.78347037400001));
#170935=CARTESIAN_POINT('Ctrl Pts',(7.04731997099994,15.2,-8.78684229900001));
#170936=CARTESIAN_POINT('Ctrl Pts',(7.04824376099995,15.2,-8.79021953000001));
#170937=CARTESIAN_POINT('Ctrl Pts',(7.04916616099994,15.2,-8.79360206200002));
#170938=CARTESIAN_POINT('Ctrl Pts',(7.05008716199995,15.2,-8.79698988800002));
#170939=CARTESIAN_POINT('Ctrl Pts',(7.05100675599994,15.2,-8.80038300300001));
#170940=CARTESIAN_POINT('Ctrl Pts',(7.05192493599994,15.2,-8.80378140200002));
#170941=CARTESIAN_POINT('Ctrl Pts',(7.05284169299994,15.2,-8.80718507700001));
#170942=CARTESIAN_POINT('Ctrl Pts',(7.05375701899994,15.2,-8.81059402400002));
#170943=CARTESIAN_POINT('Ctrl Pts',(7.05467090599995,15.2,-8.81400823500002));
#170944=CARTESIAN_POINT('Ctrl Pts',(7.05558334699995,15.2,-8.81742770600002));
#170945=CARTESIAN_POINT('Ctrl Pts',(7.05649433399994,15.2,-8.82085243000001));
#170946=CARTESIAN_POINT('Ctrl Pts',(7.05740385899994,15.2,-8.82428240200002));
#170947=CARTESIAN_POINT('Ctrl Pts',(7.05831191399994,15.2,-8.82771761700001));
#170948=CARTESIAN_POINT('Ctrl Pts',(7.05921848999994,15.2,-8.83115806600001));
#170949=CARTESIAN_POINT('Ctrl Pts',(7.06012358099994,15.2,-8.83460374700002));
#170950=CARTESIAN_POINT('Ctrl Pts',(7.06102717799994,15.2,-8.83805465100002));
#170951=CARTESIAN_POINT('Ctrl Pts',(7.06192927499995,15.2,-8.84151077400002));
#170952=CARTESIAN_POINT('Ctrl Pts',(7.06282986099994,15.2,-8.84497210900001));
#170953=CARTESIAN_POINT('Ctrl Pts',(7.06372893199994,15.2,-8.84843865100001));
#170954=CARTESIAN_POINT('Ctrl Pts',(7.06462647799994,15.2,-8.85191039400001));
#170955=CARTESIAN_POINT('Ctrl Pts',(7.06552248999994,15.2,-8.85538733200002));
#170956=CARTESIAN_POINT('Ctrl Pts',(7.06641696399994,15.2,-8.85886945800002));
#170957=CARTESIAN_POINT('Ctrl Pts',(7.06730988999994,15.2,-8.86235676900002));
#170958=CARTESIAN_POINT('Ctrl Pts',(7.06820126099994,15.2,-8.86584925900002));
#170959=CARTESIAN_POINT('Ctrl Pts',(7.06909106899994,15.2,-8.86934691900001));
#170960=CARTESIAN_POINT('Ctrl Pts',(7.06997930699995,15.2,-8.87284974500002));
#170961=CARTESIAN_POINT('Ctrl Pts',(7.07086596699994,15.2,-8.87635773100002));
#170962=CARTESIAN_POINT('Ctrl Pts',(7.07175103999995,15.2,-8.87987087200001));
#170963=CARTESIAN_POINT('Ctrl Pts',(7.07263452099994,15.2,-8.88338916200002));
#170964=CARTESIAN_POINT('Ctrl Pts',(7.07351640099994,15.2,-8.88691259500002));
#170965=CARTESIAN_POINT('Ctrl Pts',(7.07439667399994,15.2,-8.89044116400001));
#170966=CARTESIAN_POINT('Ctrl Pts',(7.07527532899995,15.2,-8.89397486500001));
#170967=CARTESIAN_POINT('Ctrl Pts',(7.07615236299994,15.2,-8.89751369100001));
#170968=CARTESIAN_POINT('Ctrl Pts',(7.07702776499994,15.2,-8.90105763700002));
#170969=CARTESIAN_POINT('Ctrl Pts',(7.07790152999995,15.2,-8.90460669800002));
#170970=CARTESIAN_POINT('Ctrl Pts',(7.07877364899994,15.2,-8.90816086600001));
#170971=CARTESIAN_POINT('Ctrl Pts',(7.07964411499994,15.2,-8.91172013700002));
#170972=CARTESIAN_POINT('Ctrl Pts',(7.08051291999994,15.2,-8.91528450500001));
#170973=CARTESIAN_POINT('Ctrl Pts',(7.08138005899994,15.2,-8.91885396400001));
#170974=CARTESIAN_POINT('Ctrl Pts',(7.08224552099994,15.2,-8.92242850800002));
#170975=CARTESIAN_POINT('Ctrl Pts',(7.08310930199994,15.2,-8.92600813100002));
#170976=CARTESIAN_POINT('Ctrl Pts',(7.08397139199994,15.2,-8.92959282900001));
#170977=CARTESIAN_POINT('Ctrl Pts',(7.08483178599994,15.2,-8.93318259300001));
#170978=CARTESIAN_POINT('Ctrl Pts',(7.08569047499994,15.2,-8.93677742100002));
#170979=CARTESIAN_POINT('Ctrl Pts',(7.08654745099994,15.2,-8.94037730400001));
#170980=CARTESIAN_POINT('Ctrl Pts',(7.08740270999995,15.2,-8.94398223900001));
#170981=CARTESIAN_POINT('Ctrl Pts',(7.08825624299994,15.2,-8.94759221800001));
#170982=CARTESIAN_POINT('Ctrl Pts',(7.08910804199994,15.2,-8.95120723800002));
#170983=CARTESIAN_POINT('Ctrl Pts',(7.08995810299994,15.2,-8.95482729200002));
#170984=CARTESIAN_POINT('Ctrl Pts',(7.09080641499994,15.2,-8.95845237400002));
#170985=CARTESIAN_POINT('Ctrl Pts',(7.09165297099994,15.2,-8.96208247700002));
#170986=CARTESIAN_POINT('Ctrl Pts',(7.09249776599994,15.2,-8.96571759800001));
#170987=CARTESIAN_POINT('Ctrl Pts',(7.09334079199994,15.2,-8.96935772800001));
#170988=CARTESIAN_POINT('Ctrl Pts',(7.09418203899994,15.2,-8.97300286300002));
#170989=CARTESIAN_POINT('Ctrl Pts',(7.09502150299994,15.2,-8.97665299700002));
#170990=CARTESIAN_POINT('Ctrl Pts',(7.09585917499994,15.2,-8.98030812400001));
#170991=CARTESIAN_POINT('Ctrl Pts',(7.09669504999995,15.2,-8.98396824000002));
#170992=CARTESIAN_POINT('Ctrl Pts',(7.09752912199995,15.2,-8.98763333900002));
#170993=CARTESIAN_POINT('Ctrl Pts',(7.09836138399995,15.2,-8.99130341500002));
#170994=CARTESIAN_POINT('Ctrl Pts',(7.09919182999994,15.2,-8.99497846600001));
#170995=CARTESIAN_POINT('Ctrl Pts',(7.10002044999994,15.2,-8.99865848200001));
#170996=CARTESIAN_POINT('Ctrl Pts',(7.10084723999994,15.2,-9.00234345900002));
#170997=CARTESIAN_POINT('Ctrl Pts',(7.10167218799994,15.2,-9.00603338900002));
#170998=CARTESIAN_POINT('Ctrl Pts',(7.10249528699994,15.2,-9.00972826500002));
#170999=CARTESIAN_POINT('Ctrl Pts',(7.10331652799994,15.2,-9.01342808000001));
#171000=CARTESIAN_POINT('Ctrl Pts',(7.10413590299994,15.2,-9.01713282900002));
#171001=CARTESIAN_POINT('Ctrl Pts',(7.10495340799994,15.2,-9.02084250500002));
#171002=CARTESIAN_POINT('Ctrl Pts',(7.10576903499994,15.2,-9.02455710700002));
#171003=CARTESIAN_POINT('Ctrl Pts',(7.10658278299994,15.2,-9.02827662900001));
#171004=CARTESIAN_POINT('Ctrl Pts',(7.10739465099994,15.2,-9.03200107200002));
#171005=CARTESIAN_POINT('Ctrl Pts',(7.10804263899995,15.2,-9.03498456100002));
#171006=CARTESIAN_POINT('Ctrl Pts',(7.10852778299994,15.2,-9.03722439200001));
#171007=CARTESIAN_POINT('Ctrl Pts',(7.10885083699995,15.2,-9.03871859500001));
#171008=CARTESIAN_POINT('Ctrl Pts',(7.10901226899994,15.2,-9.03946594400002));
#171009=CARTESIAN_POINT('Origin',(-5.66257110645729E-14,15.2,-1.77635683940025E-14));
#171010=CARTESIAN_POINT('',(7.012168986001,15.2,-7.6465751233345));
#171011=CARTESIAN_POINT('',(7.012168986001,12.2,-7.6465751233345));
#171012=CARTESIAN_POINT('',(7.01216898599994,15.2,-7.64657512300002));
#171013=CARTESIAN_POINT('Origin',(-5.66257110645729E-14,12.2,-1.77635683940025E-14));
#171014=CARTESIAN_POINT('Origin',(-5.66257110645729E-14,15.2,-1.77635683940025E-14));
#171015=CARTESIAN_POINT('Origin',(-5.66257110645729E-14,15.2,-1.77635683940025E-14));
#171016=CARTESIAN_POINT('',(8.05377977099995,15.2,-8.20893607000002));
#171017=CARTESIAN_POINT('',(8.32310290799994,15.2,-7.93573928300002));
#171018=CARTESIAN_POINT('Origin',(-5.66257110645729E-14,15.2,-1.77635683940025E-14));
#171019=CARTESIAN_POINT('',(8.32310290799994,12.2,-7.93573928300002));
#171020=CARTESIAN_POINT('',(8.32310290799994,15.2,-7.93573928300002));
#171021=CARTESIAN_POINT('',(8.05377977099995,12.2,-8.20893607000002));
#171022=CARTESIAN_POINT('Origin',(-5.66257110645729E-14,12.2,-1.77635683940025E-14));
#171023=CARTESIAN_POINT('',(8.05377977099995,15.2,-8.20893607000002));
#171024=CARTESIAN_POINT('Ctrl Pts',(8.32310290799994,15.2,-7.93573928300002));
#171025=CARTESIAN_POINT('Ctrl Pts',(8.32310290799994,11.6,-7.93573928300002));
#171026=CARTESIAN_POINT('Ctrl Pts',(8.32283676099994,15.2,-7.93502251600002));
#171027=CARTESIAN_POINT('Ctrl Pts',(8.32283676099994,11.6,-7.93502251600002));
#171028=CARTESIAN_POINT('Ctrl Pts',(8.32230434799994,15.2,-7.93358949600002));
#171029=CARTESIAN_POINT('Ctrl Pts',(8.32230434799994,11.6,-7.93358949600002));
#171030=CARTESIAN_POINT('Ctrl Pts',(8.32150538099994,15.2,-7.93144150700002));
#171031=CARTESIAN_POINT('Ctrl Pts',(8.32150538099994,11.6,-7.93144150700002));
#171032=CARTESIAN_POINT('Ctrl Pts',(8.32043939299994,15.2,-7.92858060400001));
#171033=CARTESIAN_POINT('Ctrl Pts',(8.32043939299994,11.6,-7.92858060400001));
#171034=CARTESIAN_POINT('Ctrl Pts',(8.31910574599994,15.2,-7.92500961100002));
#171035=CARTESIAN_POINT('Ctrl Pts',(8.31910574599994,11.6,-7.92500961100002));
#171036=CARTESIAN_POINT('Ctrl Pts',(8.31777093699994,15.2,-7.92144375600002));
#171037=CARTESIAN_POINT('Ctrl Pts',(8.31777093699994,11.6,-7.92144375600002));
#171038=CARTESIAN_POINT('Ctrl Pts',(8.31643496899994,15.2,-7.91788304100002));
#171039=CARTESIAN_POINT('Ctrl Pts',(8.31643496899994,11.6,-7.91788304100002));
#171040=CARTESIAN_POINT('Ctrl Pts',(8.31509784399995,15.2,-7.91432746600002));
#171041=CARTESIAN_POINT('Ctrl Pts',(8.31509784399995,11.6,-7.91432746600002));
#171042=CARTESIAN_POINT('Ctrl Pts',(8.31375956699994,15.2,-7.91077703500001));
#171043=CARTESIAN_POINT('Ctrl Pts',(8.31375956699994,11.6,-7.91077703500001));
#171044=CARTESIAN_POINT('Ctrl Pts',(8.31242014699994,15.2,-7.90723175400001));
#171045=CARTESIAN_POINT('Ctrl Pts',(8.31242014699994,11.6,-7.90723175400001));
#171046=CARTESIAN_POINT('Ctrl Pts',(8.31107958999995,15.2,-7.90369162500002));
#171047=CARTESIAN_POINT('Ctrl Pts',(8.31107958999995,11.6,-7.90369162500002));
#171048=CARTESIAN_POINT('Ctrl Pts',(8.30973790699994,15.2,-7.90015665600002));
#171049=CARTESIAN_POINT('Ctrl Pts',(8.30973790699994,11.6,-7.90015665600002));
#171050=CARTESIAN_POINT('Ctrl Pts',(8.30839510599995,15.2,-7.89662685200001));
#171051=CARTESIAN_POINT('Ctrl Pts',(8.30839510599995,11.6,-7.89662685200001));
#171052=CARTESIAN_POINT('Ctrl Pts',(8.30705119799994,15.2,-7.89310221800001));
#171053=CARTESIAN_POINT('Ctrl Pts',(8.30705119799994,11.6,-7.89310221800001));
#171054=CARTESIAN_POINT('Ctrl Pts',(8.30570619199994,15.2,-7.88958275900002));
#171055=CARTESIAN_POINT('Ctrl Pts',(8.30570619199994,11.6,-7.88958275900002));
#171056=CARTESIAN_POINT('Ctrl Pts',(8.30436009499994,15.2,-7.88606848100001));
#171057=CARTESIAN_POINT('Ctrl Pts',(8.30436009499994,11.6,-7.88606848100001));
#171058=CARTESIAN_POINT('Ctrl Pts',(8.30301291399994,15.2,-7.88255938900001));
#171059=CARTESIAN_POINT('Ctrl Pts',(8.30301291399994,11.6,-7.88255938900001));
#171060=CARTESIAN_POINT('Ctrl Pts',(8.30166465799994,15.2,-7.87905548500002));
#171061=CARTESIAN_POINT('Ctrl Pts',(8.30166465799994,11.6,-7.87905548500002));
#171062=CARTESIAN_POINT('Ctrl Pts',(8.30031533299995,15.2,-7.87555677500002));
#171063=CARTESIAN_POINT('Ctrl Pts',(8.30031533299995,11.6,-7.87555677500002));
#171064=CARTESIAN_POINT('Ctrl Pts',(8.29896494599994,15.2,-7.87206326300002));
#171065=CARTESIAN_POINT('Ctrl Pts',(8.29896494599994,11.6,-7.87206326300002));
#171066=CARTESIAN_POINT('Ctrl Pts',(8.29761350399994,15.2,-7.86857495200002));
#171067=CARTESIAN_POINT('Ctrl Pts',(8.29761350399994,11.6,-7.86857495200002));
#171068=CARTESIAN_POINT('Ctrl Pts',(8.29626101599995,15.2,-7.86509184700002));
#171069=CARTESIAN_POINT('Ctrl Pts',(8.29626101599995,11.6,-7.86509184700002));
#171070=CARTESIAN_POINT('Ctrl Pts',(8.29490748799994,15.2,-7.86161395500002));
#171071=CARTESIAN_POINT('Ctrl Pts',(8.29490748799994,11.6,-7.86161395500002));
#171072=CARTESIAN_POINT('Ctrl Pts',(8.29355293099994,15.2,-7.85814127700001));
#171073=CARTESIAN_POINT('Ctrl Pts',(8.29355293099994,11.6,-7.85814127700001));
#171074=CARTESIAN_POINT('Ctrl Pts',(8.29219734999995,15.2,-7.85467382100002));
#171075=CARTESIAN_POINT('Ctrl Pts',(8.29219734999995,11.6,-7.85467382100002));
#171076=CARTESIAN_POINT('Ctrl Pts',(8.29084075499994,15.2,-7.85121159100001));
#171077=CARTESIAN_POINT('Ctrl Pts',(8.29084075499994,11.6,-7.85121159100001));
#171078=CARTESIAN_POINT('Ctrl Pts',(8.28948315499994,15.2,-7.84775459000001));
#171079=CARTESIAN_POINT('Ctrl Pts',(8.28948315499994,11.6,-7.84775459000001));
#171080=CARTESIAN_POINT('Ctrl Pts',(8.28812455599994,15.2,-7.84430282500002));
#171081=CARTESIAN_POINT('Ctrl Pts',(8.28812455599994,11.6,-7.84430282500002));
#171082=CARTESIAN_POINT('Ctrl Pts',(8.28676496699994,15.2,-7.84085630000002));
#171083=CARTESIAN_POINT('Ctrl Pts',(8.28676496699994,11.6,-7.84085630000002));
#171084=CARTESIAN_POINT('Ctrl Pts',(8.28540439599994,15.2,-7.83741501800002));
#171085=CARTESIAN_POINT('Ctrl Pts',(8.28540439599994,11.6,-7.83741501800002));
#171086=CARTESIAN_POINT('Ctrl Pts',(8.28404284999994,15.2,-7.83397898500001));
#171087=CARTESIAN_POINT('Ctrl Pts',(8.28404284999994,11.6,-7.83397898500001));
#171088=CARTESIAN_POINT('Ctrl Pts',(8.28268033699995,15.2,-7.83054820600002));
#171089=CARTESIAN_POINT('Ctrl Pts',(8.28268033699995,11.6,-7.83054820600002));
#171090=CARTESIAN_POINT('Ctrl Pts',(8.28131686599994,15.2,-7.82712268400001));
#171091=CARTESIAN_POINT('Ctrl Pts',(8.28131686599994,11.6,-7.82712268400001));
#171092=CARTESIAN_POINT('Ctrl Pts',(8.27995244399995,15.2,-7.82370242500001));
#171093=CARTESIAN_POINT('Ctrl Pts',(8.27995244399995,11.6,-7.82370242500001));
#171094=CARTESIAN_POINT('Ctrl Pts',(8.27858707899994,15.2,-7.82028743300001));
#171095=CARTESIAN_POINT('Ctrl Pts',(8.27858707899994,11.6,-7.82028743300001));
#171096=CARTESIAN_POINT('Ctrl Pts',(8.27722078099994,15.2,-7.81687771200002));
#171097=CARTESIAN_POINT('Ctrl Pts',(8.27722078099994,11.6,-7.81687771200002));
#171098=CARTESIAN_POINT('Ctrl Pts',(8.27585355599994,15.2,-7.81347326900002));
#171099=CARTESIAN_POINT('Ctrl Pts',(8.27585355599994,11.6,-7.81347326900002));
#171100=CARTESIAN_POINT('Ctrl Pts',(8.27448541299994,15.2,-7.81007410700001));
#171101=CARTESIAN_POINT('Ctrl Pts',(8.27448541299994,11.6,-7.81007410700001));
#171102=CARTESIAN_POINT('Ctrl Pts',(8.27311635999994,15.2,-7.80668023000001));
#171103=CARTESIAN_POINT('Ctrl Pts',(8.27311635999994,11.6,-7.80668023000001));
#171104=CARTESIAN_POINT('Ctrl Pts',(8.27174640499994,15.2,-7.80329164300002));
#171105=CARTESIAN_POINT('Ctrl Pts',(8.27174640499994,11.6,-7.80329164300002));
#171106=CARTESIAN_POINT('Ctrl Pts',(8.27037555599994,15.2,-7.79990835200002));
#171107=CARTESIAN_POINT('Ctrl Pts',(8.27037555599994,11.6,-7.79990835200002));
#171108=CARTESIAN_POINT('Ctrl Pts',(8.26900382399994,15.2,-7.79653036100001));
#171109=CARTESIAN_POINT('Ctrl Pts',(8.26900382399994,11.6,-7.79653036100001));
#171110=CARTESIAN_POINT('Ctrl Pts',(8.26763121199994,15.2,-7.79315767400002));
#171111=CARTESIAN_POINT('Ctrl Pts',(8.26763121199994,11.6,-7.79315767400002));
#171112=CARTESIAN_POINT('Ctrl Pts',(8.26625773199994,15.2,-7.78979029600002));
#171113=CARTESIAN_POINT('Ctrl Pts',(8.26625773199994,11.6,-7.78979029600002));
#171114=CARTESIAN_POINT('Ctrl Pts',(8.26488339199994,15.2,-7.78642823100002));
#171115=CARTESIAN_POINT('Ctrl Pts',(8.26488339199994,11.6,-7.78642823100002));
#171116=CARTESIAN_POINT('Ctrl Pts',(8.26350819799995,15.2,-7.78307148500001));
#171117=CARTESIAN_POINT('Ctrl Pts',(8.26350819799995,11.6,-7.78307148500001));
#171118=CARTESIAN_POINT('Ctrl Pts',(8.26213216099994,15.2,-7.77972006200002));
#171119=CARTESIAN_POINT('Ctrl Pts',(8.26213216099994,11.6,-7.77972006200002));
#171120=CARTESIAN_POINT('Ctrl Pts',(8.26075528799995,15.2,-7.77637396700002));
#171121=CARTESIAN_POINT('Ctrl Pts',(8.26075528799995,11.6,-7.77637396700002));
#171122=CARTESIAN_POINT('Ctrl Pts',(8.25937758699994,15.2,-7.77303320300001));
#171123=CARTESIAN_POINT('Ctrl Pts',(8.25937758699994,11.6,-7.77303320300001));
#171124=CARTESIAN_POINT('Ctrl Pts',(8.25799906799995,15.2,-7.76969777700002));
#171125=CARTESIAN_POINT('Ctrl Pts',(8.25799906799995,11.6,-7.76969777700002));
#171126=CARTESIAN_POINT('Ctrl Pts',(8.25661973699994,15.2,-7.76636769200002));
#171127=CARTESIAN_POINT('Ctrl Pts',(8.25661973699994,11.6,-7.76636769200002));
#171128=CARTESIAN_POINT('Ctrl Pts',(8.25523960299994,15.2,-7.76304295400001));
#171129=CARTESIAN_POINT('Ctrl Pts',(8.25523960299994,11.6,-7.76304295400001));
#171130=CARTESIAN_POINT('Ctrl Pts',(8.25385867499994,15.2,-7.75972356600001));
#171131=CARTESIAN_POINT('Ctrl Pts',(8.25385867499994,11.6,-7.75972356600001));
#171132=CARTESIAN_POINT('Ctrl Pts',(8.25247696199994,15.2,-7.75640953400002));
#171133=CARTESIAN_POINT('Ctrl Pts',(8.25247696199994,11.6,-7.75640953400002));
#171134=CARTESIAN_POINT('Ctrl Pts',(8.25109447199995,15.2,-7.75310086400002));
#171135=CARTESIAN_POINT('Ctrl Pts',(8.25109447199995,11.6,-7.75310086400002));
#171136=CARTESIAN_POINT('Ctrl Pts',(8.24971121199994,15.2,-7.74979755600001));
#171137=CARTESIAN_POINT('Ctrl Pts',(8.24971121199994,11.6,-7.74979755600001));
#171138=CARTESIAN_POINT('Ctrl Pts',(8.24832719199994,15.2,-7.74649962000002));
#171139=CARTESIAN_POINT('Ctrl Pts',(8.24832719199994,11.6,-7.74649962000002));
#171140=CARTESIAN_POINT('Ctrl Pts',(8.24694242099994,15.2,-7.74320705700001));
#171141=CARTESIAN_POINT('Ctrl Pts',(8.24694242099994,11.6,-7.74320705700001));
#171142=CARTESIAN_POINT('Ctrl Pts',(8.24555690699994,15.2,-7.73991987300001));
#171143=CARTESIAN_POINT('Ctrl Pts',(8.24555690699994,11.6,-7.73991987300001));
#171144=CARTESIAN_POINT('Ctrl Pts',(8.24417065699994,15.2,-7.73663807300002));
#171145=CARTESIAN_POINT('Ctrl Pts',(8.24417065699994,11.6,-7.73663807300002));
#171146=CARTESIAN_POINT('Ctrl Pts',(8.24278367999994,15.2,-7.73336166100002));
#171147=CARTESIAN_POINT('Ctrl Pts',(8.24278367999994,11.6,-7.73336166100002));
#171148=CARTESIAN_POINT('Ctrl Pts',(8.24139598699994,15.2,-7.73009064300001));
#171149=CARTESIAN_POINT('Ctrl Pts',(8.24139598699994,11.6,-7.73009064300001));
#171150=CARTESIAN_POINT('Ctrl Pts',(8.24000758299994,15.2,-7.72682502200002));
#171151=CARTESIAN_POINT('Ctrl Pts',(8.24000758299994,11.6,-7.72682502200002));
#171152=CARTESIAN_POINT('Ctrl Pts',(8.23861848099994,15.2,-7.72356480200001));
#171153=CARTESIAN_POINT('Ctrl Pts',(8.23861848099994,11.6,-7.72356480200001));
#171154=CARTESIAN_POINT('Ctrl Pts',(8.23722868599994,15.2,-7.72030999100001));
#171155=CARTESIAN_POINT('Ctrl Pts',(8.23722868599994,11.6,-7.72030999100001));
#171156=CARTESIAN_POINT('Ctrl Pts',(8.23583820599995,15.2,-7.71706059100002));
#171157=CARTESIAN_POINT('Ctrl Pts',(8.23583820599995,11.6,-7.71706059100002));
#171158=CARTESIAN_POINT('Ctrl Pts',(8.23444705399995,15.2,-7.71381660700002));
#171159=CARTESIAN_POINT('Ctrl Pts',(8.23444705399995,11.6,-7.71381660700002));
#171160=CARTESIAN_POINT('Ctrl Pts',(8.23305523399994,15.2,-7.71057804500002));
#171161=CARTESIAN_POINT('Ctrl Pts',(8.23305523399994,11.6,-7.71057804500002));
#171162=CARTESIAN_POINT('Ctrl Pts',(8.23166275799995,15.2,-7.70734490700002));
#171163=CARTESIAN_POINT('Ctrl Pts',(8.23166275799995,11.6,-7.70734490700002));
#171164=CARTESIAN_POINT('Ctrl Pts',(8.23026963299995,15.2,-7.70411720200002));
#171165=CARTESIAN_POINT('Ctrl Pts',(8.23026963299995,11.6,-7.70411720200002));
#171166=CARTESIAN_POINT('Ctrl Pts',(8.22887586899994,15.2,-7.70089492900001));
#171167=CARTESIAN_POINT('Ctrl Pts',(8.22887586899994,11.6,-7.70089492900001));
#171168=CARTESIAN_POINT('Ctrl Pts',(8.22748147299994,15.2,-7.69767809800002));
#171169=CARTESIAN_POINT('Ctrl Pts',(8.22748147299994,11.6,-7.69767809800002));
#171170=CARTESIAN_POINT('Ctrl Pts',(8.22608645599994,15.2,-7.69446671100001));
#171171=CARTESIAN_POINT('Ctrl Pts',(8.22608645599994,11.6,-7.69446671100001));
#171172=CARTESIAN_POINT('Ctrl Pts',(8.22469082399994,15.2,-7.69126077300001));
#171173=CARTESIAN_POINT('Ctrl Pts',(8.22469082399994,11.6,-7.69126077300001));
#171174=CARTESIAN_POINT('Ctrl Pts',(8.22329458799994,15.2,-7.68806029000002));
#171175=CARTESIAN_POINT('Ctrl Pts',(8.22329458799994,11.6,-7.68806029000002));
#171176=CARTESIAN_POINT('Ctrl Pts',(8.22189775699995,15.2,-7.68486526400002));
#171177=CARTESIAN_POINT('Ctrl Pts',(8.22189775699995,11.6,-7.68486526400002));
#171178=CARTESIAN_POINT('Ctrl Pts',(8.22050033799994,15.2,-7.68167570200001));
#171179=CARTESIAN_POINT('Ctrl Pts',(8.22050033799994,11.6,-7.68167570200001));
#171180=CARTESIAN_POINT('Ctrl Pts',(8.21910234199994,15.2,-7.67849160900001));
#171181=CARTESIAN_POINT('Ctrl Pts',(8.21910234199994,11.6,-7.67849160900001));
#171182=CARTESIAN_POINT('Ctrl Pts',(8.21770377699995,15.2,-7.67531298700002));
#171183=CARTESIAN_POINT('Ctrl Pts',(8.21770377699995,11.6,-7.67531298700002));
#171184=CARTESIAN_POINT('Ctrl Pts',(8.21630465099994,15.2,-7.67213984300002));
#171185=CARTESIAN_POINT('Ctrl Pts',(8.21630465099994,11.6,-7.67213984300002));
#171186=CARTESIAN_POINT('Ctrl Pts',(8.21490497299994,15.2,-7.66897218200001));
#171187=CARTESIAN_POINT('Ctrl Pts',(8.21490497299994,11.6,-7.66897218200001));
#171188=CARTESIAN_POINT('Ctrl Pts',(8.21350475399995,15.2,-7.66581000700001));
#171189=CARTESIAN_POINT('Ctrl Pts',(8.21350475399995,11.6,-7.66581000700001));
#171190=CARTESIAN_POINT('Ctrl Pts',(8.21210400199995,15.2,-7.66265332400001));
#171191=CARTESIAN_POINT('Ctrl Pts',(8.21210400199995,11.6,-7.66265332400001));
#171192=CARTESIAN_POINT('Ctrl Pts',(8.21070272499994,15.2,-7.65950213700001));
#171193=CARTESIAN_POINT('Ctrl Pts',(8.21070272499994,11.6,-7.65950213700001));
#171194=CARTESIAN_POINT('Ctrl Pts',(8.20930093299994,15.2,-7.65635645100001));
#171195=CARTESIAN_POINT('Ctrl Pts',(8.20930093299994,11.6,-7.65635645100001));
#171196=CARTESIAN_POINT('Ctrl Pts',(8.20789863399994,15.2,-7.65321627000001));
#171197=CARTESIAN_POINT('Ctrl Pts',(8.20789863399994,11.6,-7.65321627000001));
#171198=CARTESIAN_POINT('Ctrl Pts',(8.20649583899994,15.2,-7.65008160000002));
#171199=CARTESIAN_POINT('Ctrl Pts',(8.20649583899994,11.6,-7.65008160000002));
#171200=CARTESIAN_POINT('Ctrl Pts',(8.20509255499994,15.2,-7.64695244500002));
#171201=CARTESIAN_POINT('Ctrl Pts',(8.20509255499994,11.6,-7.64695244500002));
#171202=CARTESIAN_POINT('Ctrl Pts',(8.20368879299994,15.2,-7.64382880900002));
#171203=CARTESIAN_POINT('Ctrl Pts',(8.20368879299994,11.6,-7.64382880900002));
#171204=CARTESIAN_POINT('Ctrl Pts',(8.20228455999995,15.2,-7.64071069900002));
#171205=CARTESIAN_POINT('Ctrl Pts',(8.20228455999995,11.6,-7.64071069900002));
#171206=CARTESIAN_POINT('Ctrl Pts',(8.20087986699994,15.2,-7.63759811700002));
#171207=CARTESIAN_POINT('Ctrl Pts',(8.20087986699994,11.6,-7.63759811700002));
#171208=CARTESIAN_POINT('Ctrl Pts',(8.19947472199994,15.2,-7.63449107000002));
#171209=CARTESIAN_POINT('Ctrl Pts',(8.19947472199994,11.6,-7.63449107000002));
#171210=CARTESIAN_POINT('Ctrl Pts',(8.19806913599994,15.2,-7.63138956100001));
#171211=CARTESIAN_POINT('Ctrl Pts',(8.19806913599994,11.6,-7.63138956100001));
#171212=CARTESIAN_POINT('Ctrl Pts',(8.19666311599994,15.2,-7.62829359600002));
#171213=CARTESIAN_POINT('Ctrl Pts',(8.19666311599994,11.6,-7.62829359600002));
#171214=CARTESIAN_POINT('Ctrl Pts',(8.19525667099994,15.2,-7.62520317900002));
#171215=CARTESIAN_POINT('Ctrl Pts',(8.19525667099994,11.6,-7.62520317900002));
#171216=CARTESIAN_POINT('Ctrl Pts',(8.19384981299994,15.2,-7.62211831500001));
#171217=CARTESIAN_POINT('Ctrl Pts',(8.19384981299994,11.6,-7.62211831500001));
#171218=CARTESIAN_POINT('Ctrl Pts',(8.19244254899994,15.2,-7.61903900800001));
#171219=CARTESIAN_POINT('Ctrl Pts',(8.19244254899994,11.6,-7.61903900800001));
#171220=CARTESIAN_POINT('Ctrl Pts',(8.19103488899994,15.2,-7.61596526400002));
#171221=CARTESIAN_POINT('Ctrl Pts',(8.19103488899994,11.6,-7.61596526400002));
#171222=CARTESIAN_POINT('Ctrl Pts',(8.18962684199994,15.2,-7.61289708700001));
#171223=CARTESIAN_POINT('Ctrl Pts',(8.18962684199994,11.6,-7.61289708700001));
#171224=CARTESIAN_POINT('Ctrl Pts',(8.18821841799994,15.2,-7.60983448100002));
#171225=CARTESIAN_POINT('Ctrl Pts',(8.18821841799994,11.6,-7.60983448100002));
#171226=CARTESIAN_POINT('Ctrl Pts',(8.18680962599995,15.2,-7.60677745200002));
#171227=CARTESIAN_POINT('Ctrl Pts',(8.18680962599995,11.6,-7.60677745200002));
#171228=CARTESIAN_POINT('Ctrl Pts',(8.18540047699994,15.2,-7.60372600500002));
#171229=CARTESIAN_POINT('Ctrl Pts',(8.18540047699994,11.6,-7.60372600500002));
#171230=CARTESIAN_POINT('Ctrl Pts',(8.18399097599994,15.2,-7.60068014400002));
#171231=CARTESIAN_POINT('Ctrl Pts',(8.18399097599994,11.6,-7.60068014400002));
#171232=CARTESIAN_POINT('Ctrl Pts',(8.18258113699994,15.2,-7.59763987300002));
#171233=CARTESIAN_POINT('Ctrl Pts',(8.18258113699994,11.6,-7.59763987300002));
#171234=CARTESIAN_POINT('Ctrl Pts',(8.18117096699994,15.2,-7.59460519700002));
#171235=CARTESIAN_POINT('Ctrl Pts',(8.18117096699994,11.6,-7.59460519700002));
#171236=CARTESIAN_POINT('Ctrl Pts',(8.17976047699995,15.2,-7.59157612300001));
#171237=CARTESIAN_POINT('Ctrl Pts',(8.17976047699995,11.6,-7.59157612300001));
#171238=CARTESIAN_POINT('Ctrl Pts',(8.17834967399994,15.2,-7.58855265300002));
#171239=CARTESIAN_POINT('Ctrl Pts',(8.17834967399994,11.6,-7.58855265300002));
#171240=CARTESIAN_POINT('Ctrl Pts',(8.17693857099994,15.2,-7.58553479300001));
#171241=CARTESIAN_POINT('Ctrl Pts',(8.17693857099994,11.6,-7.58553479300001));
#171242=CARTESIAN_POINT('Ctrl Pts',(8.17552717499994,15.2,-7.58252254800002));
#171243=CARTESIAN_POINT('Ctrl Pts',(8.17552717499994,11.6,-7.58252254800002));
#171244=CARTESIAN_POINT('Ctrl Pts',(8.17411549699994,15.2,-7.57951592200002));
#171245=CARTESIAN_POINT('Ctrl Pts',(8.17411549699994,11.6,-7.57951592200002));
#171246=CARTESIAN_POINT('Ctrl Pts',(8.17270354399994,15.2,-7.57651491900001));
#171247=CARTESIAN_POINT('Ctrl Pts',(8.17270354399994,11.6,-7.57651491900001));
#171248=CARTESIAN_POINT('Ctrl Pts',(8.17129132899994,15.2,-7.57351954600002));
#171249=CARTESIAN_POINT('Ctrl Pts',(8.17129132899994,11.6,-7.57351954600002));
#171250=CARTESIAN_POINT('Ctrl Pts',(8.16987885999995,15.2,-7.57052980700001));
#171251=CARTESIAN_POINT('Ctrl Pts',(8.16987885999995,11.6,-7.57052980700001));
#171252=CARTESIAN_POINT('Ctrl Pts',(8.16846614699994,15.2,-7.56754570500001));
#171253=CARTESIAN_POINT('Ctrl Pts',(8.16846614699994,11.6,-7.56754570500001));
#171254=CARTESIAN_POINT('Ctrl Pts',(8.16705319899994,15.2,-7.56456724700002));
#171255=CARTESIAN_POINT('Ctrl Pts',(8.16705319899994,11.6,-7.56456724700002));
#171256=CARTESIAN_POINT('Ctrl Pts',(8.16564002699995,15.2,-7.56159443600002));
#171257=CARTESIAN_POINT('Ctrl Pts',(8.16564002699995,11.6,-7.56159443600002));
#171258=CARTESIAN_POINT('Ctrl Pts',(8.16422663899995,15.2,-7.55862727900002));
#171259=CARTESIAN_POINT('Ctrl Pts',(8.16422663899995,11.6,-7.55862727900002));
#171260=CARTESIAN_POINT('Ctrl Pts',(8.16281304699995,15.2,-7.55566577800002));
#171261=CARTESIAN_POINT('Ctrl Pts',(8.16281304699995,11.6,-7.55566577800002));
#171262=CARTESIAN_POINT('Ctrl Pts',(8.16139925799994,15.2,-7.55270994000002));
#171263=CARTESIAN_POINT('Ctrl Pts',(8.16139925799994,11.6,-7.55270994000002));
#171264=CARTESIAN_POINT('Ctrl Pts',(8.15998528399994,15.2,-7.54975976900001));
#171265=CARTESIAN_POINT('Ctrl Pts',(8.15998528399994,11.6,-7.54975976900001));
#171266=CARTESIAN_POINT('Ctrl Pts',(8.15857113399994,15.2,-7.54681526900002));
#171267=CARTESIAN_POINT('Ctrl Pts',(8.15857113399994,11.6,-7.54681526900002));
#171268=CARTESIAN_POINT('Ctrl Pts',(8.15715681899994,15.2,-7.54387644600002));
#171269=CARTESIAN_POINT('Ctrl Pts',(8.15715681899994,11.6,-7.54387644600002));
#171270=CARTESIAN_POINT('Ctrl Pts',(8.15574234599995,15.2,-7.54094330400001));
#171271=CARTESIAN_POINT('Ctrl Pts',(8.15574234599995,11.6,-7.54094330400001));
#171272=CARTESIAN_POINT('Ctrl Pts',(8.15432772699995,15.2,-7.53801584800001));
#171273=CARTESIAN_POINT('Ctrl Pts',(8.15432772699995,11.6,-7.53801584800001));
#171274=CARTESIAN_POINT('Ctrl Pts',(8.15291297199994,15.2,-7.53509408200002));
#171275=CARTESIAN_POINT('Ctrl Pts',(8.15291297199994,11.6,-7.53509408200002));
#171276=CARTESIAN_POINT('Ctrl Pts',(8.15149809099994,15.2,-7.53217801400002));
#171277=CARTESIAN_POINT('Ctrl Pts',(8.15149809099994,11.6,-7.53217801400002));
#171278=CARTESIAN_POINT('Ctrl Pts',(8.15008309399994,15.2,-7.52926764500002));
#171279=CARTESIAN_POINT('Ctrl Pts',(8.15008309399994,11.6,-7.52926764500002));
#171280=CARTESIAN_POINT('Ctrl Pts',(8.14866798999994,15.2,-7.52636298000001));
#171281=CARTESIAN_POINT('Ctrl Pts',(8.14866798999994,11.6,-7.52636298000001));
#171282=CARTESIAN_POINT('Ctrl Pts',(8.14725278899994,15.2,-7.52346402700002));
#171283=CARTESIAN_POINT('Ctrl Pts',(8.14725278899994,11.6,-7.52346402700002));
#171284=CARTESIAN_POINT('Ctrl Pts',(8.14583750199994,15.2,-7.52057078700001));
#171285=CARTESIAN_POINT('Ctrl Pts',(8.14583750199994,11.6,-7.52057078700001));
#171286=CARTESIAN_POINT('Ctrl Pts',(8.14442213799994,15.2,-7.51768326800001));
#171287=CARTESIAN_POINT('Ctrl Pts',(8.14442213799994,11.6,-7.51768326800001));
#171288=CARTESIAN_POINT('Ctrl Pts',(8.14300670799994,15.2,-7.51480147300001));
#171289=CARTESIAN_POINT('Ctrl Pts',(8.14300670799994,11.6,-7.51480147300001));
#171290=CARTESIAN_POINT('Ctrl Pts',(8.14159122299994,15.2,-7.51192540700002));
#171291=CARTESIAN_POINT('Ctrl Pts',(8.14159122299994,11.6,-7.51192540700002));
#171292=CARTESIAN_POINT('Ctrl Pts',(8.14017569099994,15.2,-7.50905507500002));
#171293=CARTESIAN_POINT('Ctrl Pts',(8.14017569099994,11.6,-7.50905507500002));
#171294=CARTESIAN_POINT('Ctrl Pts',(8.13876012299995,15.2,-7.50619048100001));
#171295=CARTESIAN_POINT('Ctrl Pts',(8.13876012299995,11.6,-7.50619048100001));
#171296=CARTESIAN_POINT('Ctrl Pts',(8.13734453099995,15.2,-7.50333163200001));
#171297=CARTESIAN_POINT('Ctrl Pts',(8.13734453099995,11.6,-7.50333163200001));
#171298=CARTESIAN_POINT('Ctrl Pts',(8.13592892199994,15.2,-7.50047853100002));
#171299=CARTESIAN_POINT('Ctrl Pts',(8.13592892199994,11.6,-7.50047853100002));
#171300=CARTESIAN_POINT('Ctrl Pts',(8.13451330699994,15.2,-7.49763118200002));
#171301=CARTESIAN_POINT('Ctrl Pts',(8.13451330699994,11.6,-7.49763118200002));
#171302=CARTESIAN_POINT('Ctrl Pts',(8.13309769899995,15.2,-7.49478959200002));
#171303=CARTESIAN_POINT('Ctrl Pts',(8.13309769899995,11.6,-7.49478959200002));
#171304=CARTESIAN_POINT('Ctrl Pts',(8.13168210599994,15.2,-7.49195376500002));
#171305=CARTESIAN_POINT('Ctrl Pts',(8.13168210599994,11.6,-7.49195376500002));
#171306=CARTESIAN_POINT('Ctrl Pts',(8.13026653799995,15.2,-7.48912370500002));
#171307=CARTESIAN_POINT('Ctrl Pts',(8.13026653799995,11.6,-7.48912370500002));
#171308=CARTESIAN_POINT('Ctrl Pts',(8.12885100599994,15.2,-7.48629941700001));
#171309=CARTESIAN_POINT('Ctrl Pts',(8.12885100599994,11.6,-7.48629941700001));
#171310=CARTESIAN_POINT('Ctrl Pts',(8.12743552099995,15.2,-7.48348090800001));
#171311=CARTESIAN_POINT('Ctrl Pts',(8.12743552099995,11.6,-7.48348090800001));
#171312=CARTESIAN_POINT('Ctrl Pts',(8.12602009199994,15.2,-7.48066818000002));
#171313=CARTESIAN_POINT('Ctrl Pts',(8.12602009199994,11.6,-7.48066818000002));
#171314=CARTESIAN_POINT('Ctrl Pts',(8.12460473099994,15.2,-7.47786123800001));
#171315=CARTESIAN_POINT('Ctrl Pts',(8.12460473099994,11.6,-7.47786123800001));
#171316=CARTESIAN_POINT('Ctrl Pts',(8.12318944699994,15.2,-7.47506008900002));
#171317=CARTESIAN_POINT('Ctrl Pts',(8.12318944699994,11.6,-7.47506008900002));
#171318=CARTESIAN_POINT('Ctrl Pts',(8.12177425199994,15.2,-7.47226473600002));
#171319=CARTESIAN_POINT('Ctrl Pts',(8.12177425199994,11.6,-7.47226473600002));
#171320=CARTESIAN_POINT('Ctrl Pts',(8.12035915499994,15.2,-7.46947518500002));
#171321=CARTESIAN_POINT('Ctrl Pts',(8.12035915499994,11.6,-7.46947518500002));
#171322=CARTESIAN_POINT('Ctrl Pts',(8.11894416699994,15.2,-7.46669144000002));
#171323=CARTESIAN_POINT('Ctrl Pts',(8.11894416699994,11.6,-7.46669144000002));
#171324=CARTESIAN_POINT('Ctrl Pts',(8.11752929899994,15.2,-7.46391350600002));
#171325=CARTESIAN_POINT('Ctrl Pts',(8.11752929899994,11.6,-7.46391350600002));
#171326=CARTESIAN_POINT('Ctrl Pts',(8.11611456099994,15.2,-7.46114138700002));
#171327=CARTESIAN_POINT('Ctrl Pts',(8.11611456099994,11.6,-7.46114138700002));
#171328=CARTESIAN_POINT('Ctrl Pts',(8.11469996399994,15.2,-7.45837509000002));
#171329=CARTESIAN_POINT('Ctrl Pts',(8.11469996399994,11.6,-7.45837509000002));
#171330=CARTESIAN_POINT('Ctrl Pts',(8.11328551799994,15.2,-7.45561461800002));
#171331=CARTESIAN_POINT('Ctrl Pts',(8.11328551799994,11.6,-7.45561461800002));
#171332=CARTESIAN_POINT('Ctrl Pts',(8.11187123599994,15.2,-7.45285997600002));
#171333=CARTESIAN_POINT('Ctrl Pts',(8.11187123599994,11.6,-7.45285997600002));
#171334=CARTESIAN_POINT('Ctrl Pts',(8.11045712499994,15.2,-7.45011117000002));
#171335=CARTESIAN_POINT('Ctrl Pts',(8.11045712499994,11.6,-7.45011117000002));
#171336=CARTESIAN_POINT('Ctrl Pts',(8.10904319799995,15.2,-7.44736820300002));
#171337=CARTESIAN_POINT('Ctrl Pts',(8.10904319799995,11.6,-7.44736820300002));
#171338=CARTESIAN_POINT('Ctrl Pts',(8.10762946499995,15.2,-7.44463108200001));
#171339=CARTESIAN_POINT('Ctrl Pts',(8.10762946499995,11.6,-7.44463108200001));
#171340=CARTESIAN_POINT('Ctrl Pts',(8.10621593799994,15.2,-7.44189981000002));
#171341=CARTESIAN_POINT('Ctrl Pts',(8.10621593799994,11.6,-7.44189981000002));
#171342=CARTESIAN_POINT('Ctrl Pts',(8.10480262699994,15.2,-7.43917439400001));
#171343=CARTESIAN_POINT('Ctrl Pts',(8.10480262699994,11.6,-7.43917439400001));
#171344=CARTESIAN_POINT('Ctrl Pts',(8.10338954199995,15.2,-7.43645483600002));
#171345=CARTESIAN_POINT('Ctrl Pts',(8.10338954199995,11.6,-7.43645483600002));
#171346=CARTESIAN_POINT('Ctrl Pts',(8.10197669399994,15.2,-7.43374114300002));
#171347=CARTESIAN_POINT('Ctrl Pts',(8.10197669399994,11.6,-7.43374114300002));
#171348=CARTESIAN_POINT('Ctrl Pts',(8.10056409499994,15.2,-7.43103331900001));
#171349=CARTESIAN_POINT('Ctrl Pts',(8.10056409499994,11.6,-7.43103331900001));
#171350=CARTESIAN_POINT('Ctrl Pts',(8.09915175599994,15.2,-7.42833136900002));
#171351=CARTESIAN_POINT('Ctrl Pts',(8.09915175599994,11.6,-7.42833136900002));
#171352=CARTESIAN_POINT('Ctrl Pts',(8.09773968599995,15.2,-7.42563529800002));
#171353=CARTESIAN_POINT('Ctrl Pts',(8.09773968599995,11.6,-7.42563529800002));
#171354=CARTESIAN_POINT('Ctrl Pts',(8.09632789799995,15.2,-7.42294511100001));
#171355=CARTESIAN_POINT('Ctrl Pts',(8.09632789799995,11.6,-7.42294511100001));
#171356=CARTESIAN_POINT('Ctrl Pts',(8.09491640099994,15.2,-7.42026081400001));
#171357=CARTESIAN_POINT('Ctrl Pts',(8.09491640099994,11.6,-7.42026081400001));
#171358=CARTESIAN_POINT('Ctrl Pts',(8.09350520799994,15.2,-7.41758240800002));
#171359=CARTESIAN_POINT('Ctrl Pts',(8.09350520799994,11.6,-7.41758240800002));
#171360=CARTESIAN_POINT('Ctrl Pts',(8.09209432999995,15.2,-7.41490990200001));
#171361=CARTESIAN_POINT('Ctrl Pts',(8.09209432999995,11.6,-7.41490990200001));
#171362=CARTESIAN_POINT('Ctrl Pts',(8.09068377599995,15.2,-7.41224329900002));
#171363=CARTESIAN_POINT('Ctrl Pts',(8.09068377599995,11.6,-7.41224329900002));
#171364=CARTESIAN_POINT('Ctrl Pts',(8.08927355799994,15.2,-7.40958260500002));
#171365=CARTESIAN_POINT('Ctrl Pts',(8.08927355799994,11.6,-7.40958260500002));
#171366=CARTESIAN_POINT('Ctrl Pts',(8.08786368899994,15.2,-7.40692782200002));
#171367=CARTESIAN_POINT('Ctrl Pts',(8.08786368899994,11.6,-7.40692782200002));
#171368=CARTESIAN_POINT('Ctrl Pts',(8.08645417899994,15.2,-7.40427895900002));
#171369=CARTESIAN_POINT('Ctrl Pts',(8.08645417899994,11.6,-7.40427895900002));
#171370=CARTESIAN_POINT('Ctrl Pts',(8.08504503799995,15.2,-7.40163601800001));
#171371=CARTESIAN_POINT('Ctrl Pts',(8.08504503799995,11.6,-7.40163601800001));
#171372=CARTESIAN_POINT('Ctrl Pts',(8.08363627799995,15.2,-7.39899900500002));
#171373=CARTESIAN_POINT('Ctrl Pts',(8.08363627799995,11.6,-7.39899900500002));
#171374=CARTESIAN_POINT('Ctrl Pts',(8.08222790999995,15.2,-7.39636792500002));
#171375=CARTESIAN_POINT('Ctrl Pts',(8.08222790999995,11.6,-7.39636792500002));
#171376=CARTESIAN_POINT('Ctrl Pts',(8.08081994599995,15.2,-7.39374278100002));
#171377=CARTESIAN_POINT('Ctrl Pts',(8.08081994599995,11.6,-7.39374278100002));
#171378=CARTESIAN_POINT('Ctrl Pts',(8.07941239799994,15.2,-7.39112358100002));
#171379=CARTESIAN_POINT('Ctrl Pts',(8.07941239799994,11.6,-7.39112358100002));
#171380=CARTESIAN_POINT('Ctrl Pts',(8.07800527499994,15.2,-7.38851032800002));
#171381=CARTESIAN_POINT('Ctrl Pts',(8.07800527499994,11.6,-7.38851032800002));
#171382=CARTESIAN_POINT('Ctrl Pts',(8.07659858999994,15.2,-7.38590302700001));
#171383=CARTESIAN_POINT('Ctrl Pts',(8.07659858999994,11.6,-7.38590302700001));
#171384=CARTESIAN_POINT('Ctrl Pts',(8.07519235299995,15.2,-7.38330168300001));
#171385=CARTESIAN_POINT('Ctrl Pts',(8.07519235299995,11.6,-7.38330168300001));
#171386=CARTESIAN_POINT('Ctrl Pts',(8.07378657799994,15.2,-7.38070630100002));
#171387=CARTESIAN_POINT('Ctrl Pts',(8.07378657799994,11.6,-7.38070630100002));
#171388=CARTESIAN_POINT('Ctrl Pts',(8.07238127399994,15.2,-7.37811688600001));
#171389=CARTESIAN_POINT('Ctrl Pts',(8.07238127399994,11.6,-7.37811688600001));
#171390=CARTESIAN_POINT('Ctrl Pts',(8.07097645399995,15.2,-7.37553344300002));
#171391=CARTESIAN_POINT('Ctrl Pts',(8.07097645399995,11.6,-7.37553344300002));
#171392=CARTESIAN_POINT('Ctrl Pts',(8.06957212799994,15.2,-7.37295597700002));
#171393=CARTESIAN_POINT('Ctrl Pts',(8.06957212799994,11.6,-7.37295597700002));
#171394=CARTESIAN_POINT('Ctrl Pts',(8.06816830899994,15.2,-7.37038449300002));
#171395=CARTESIAN_POINT('Ctrl Pts',(8.06816830899994,11.6,-7.37038449300002));
#171396=CARTESIAN_POINT('Ctrl Pts',(8.06676500799994,15.2,-7.36781899400002));
#171397=CARTESIAN_POINT('Ctrl Pts',(8.06676500799994,11.6,-7.36781899400002));
#171398=CARTESIAN_POINT('Ctrl Pts',(8.06536223699995,15.2,-7.36525948800002));
#171399=CARTESIAN_POINT('Ctrl Pts',(8.06536223699995,11.6,-7.36525948800002));
#171400=CARTESIAN_POINT('Ctrl Pts',(8.06396000599995,15.2,-7.36270597800001));
#171401=CARTESIAN_POINT('Ctrl Pts',(8.06396000599995,11.6,-7.36270597800001));
#171402=CARTESIAN_POINT('Ctrl Pts',(8.06255832899994,15.2,-7.36015847000001));
#171403=CARTESIAN_POINT('Ctrl Pts',(8.06255832899994,11.6,-7.36015847000001));
#171404=CARTESIAN_POINT('Ctrl Pts',(8.06115721599994,15.2,-7.35761696800001));
#171405=CARTESIAN_POINT('Ctrl Pts',(8.06115721599994,11.6,-7.35761696800001));
#171406=CARTESIAN_POINT('Ctrl Pts',(8.05975667999994,15.2,-7.35508147600001));
#171407=CARTESIAN_POINT('Ctrl Pts',(8.05975667999994,11.6,-7.35508147600001));
#171408=CARTESIAN_POINT('Ctrl Pts',(8.05835673199994,15.2,-7.35255200200001));
#171409=CARTESIAN_POINT('Ctrl Pts',(8.05835673199994,11.6,-7.35255200200001));
#171410=CARTESIAN_POINT('Ctrl Pts',(8.05695738399994,15.2,-7.35002854800002));
#171411=CARTESIAN_POINT('Ctrl Pts',(8.05695738399994,11.6,-7.35002854800002));
#171412=CARTESIAN_POINT('Ctrl Pts',(8.05555864699994,15.2,-7.34751112100002));
#171413=CARTESIAN_POINT('Ctrl Pts',(8.05555864699994,11.6,-7.34751112100002));
#171414=CARTESIAN_POINT('Ctrl Pts',(8.05416053399994,15.2,-7.34499972400001));
#171415=CARTESIAN_POINT('Ctrl Pts',(8.05416053399994,11.6,-7.34499972400001));
#171416=CARTESIAN_POINT('Ctrl Pts',(8.05276305599994,15.2,-7.34249436400002));
#171417=CARTESIAN_POINT('Ctrl Pts',(8.05276305599994,11.6,-7.34249436400002));
#171418=CARTESIAN_POINT('Ctrl Pts',(8.05136622599994,15.2,-7.33999504400002));
#171419=CARTESIAN_POINT('Ctrl Pts',(8.05136622599994,11.6,-7.33999504400002));
#171420=CARTESIAN_POINT('Ctrl Pts',(8.04997005499994,15.2,-7.33750177000001));
#171421=CARTESIAN_POINT('Ctrl Pts',(8.04997005499994,11.6,-7.33750177000001));
#171422=CARTESIAN_POINT('Ctrl Pts',(8.04857455599995,15.2,-7.33501454700002));
#171423=CARTESIAN_POINT('Ctrl Pts',(8.04857455599995,11.6,-7.33501454700002));
#171424=CARTESIAN_POINT('Ctrl Pts',(8.04717973999994,15.2,-7.33253338100001));
#171425=CARTESIAN_POINT('Ctrl Pts',(8.04717973999994,11.6,-7.33253338100001));
#171426=CARTESIAN_POINT('Ctrl Pts',(8.04578561899995,15.2,-7.33005827400002));
#171427=CARTESIAN_POINT('Ctrl Pts',(8.04578561899995,11.6,-7.33005827400002));
#171428=CARTESIAN_POINT('Ctrl Pts',(8.04439220499994,15.2,-7.32758923400001));
#171429=CARTESIAN_POINT('Ctrl Pts',(8.04439220499994,11.6,-7.32758923400001));
#171430=CARTESIAN_POINT('Ctrl Pts',(8.04299951199994,15.2,-7.32512626400001));
#171431=CARTESIAN_POINT('Ctrl Pts',(8.04299951199994,11.6,-7.32512626400001));
#171432=CARTESIAN_POINT('Ctrl Pts',(8.04160754999995,15.2,-7.32266936900002));
#171433=CARTESIAN_POINT('Ctrl Pts',(8.04160754999995,11.6,-7.32266936900002));
#171434=CARTESIAN_POINT('Ctrl Pts',(8.04021633199994,15.2,-7.32021855600002));
#171435=CARTESIAN_POINT('Ctrl Pts',(8.04021633199994,11.6,-7.32021855600002));
#171436=CARTESIAN_POINT('Ctrl Pts',(8.03882586899995,15.2,-7.31777382800002));
#171437=CARTESIAN_POINT('Ctrl Pts',(8.03882586899995,11.6,-7.31777382800002));
#171438=CARTESIAN_POINT('Ctrl Pts',(8.03743617699994,15.2,-7.31533519100001));
#171439=CARTESIAN_POINT('Ctrl Pts',(8.03743617699994,11.6,-7.31533519100001));
#171440=CARTESIAN_POINT('Ctrl Pts',(8.03604726399995,15.2,-7.31290264900001));
#171441=CARTESIAN_POINT('Ctrl Pts',(8.03604726399995,11.6,-7.31290264900001));
#171442=CARTESIAN_POINT('Ctrl Pts',(8.03465914399995,15.2,-7.31047620700001));
#171443=CARTESIAN_POINT('Ctrl Pts',(8.03465914399995,11.6,-7.31047620700001));
#171444=CARTESIAN_POINT('Ctrl Pts',(8.03327182899995,15.2,-7.30805587200001));
#171445=CARTESIAN_POINT('Ctrl Pts',(8.03327182899995,11.6,-7.30805587200001));
#171446=CARTESIAN_POINT('Ctrl Pts',(8.03188533199994,15.2,-7.30564164600001));
#171447=CARTESIAN_POINT('Ctrl Pts',(8.03188533199994,11.6,-7.30564164600001));
#171448=CARTESIAN_POINT('Ctrl Pts',(8.03049966599995,15.2,-7.30323353700002));
#171449=CARTESIAN_POINT('Ctrl Pts',(8.03049966599995,11.6,-7.30323353700002));
#171450=CARTESIAN_POINT('Ctrl Pts',(8.02911484199995,15.2,-7.30083154700001));
#171451=CARTESIAN_POINT('Ctrl Pts',(8.02911484199995,11.6,-7.30083154700001));
#171452=CARTESIAN_POINT('Ctrl Pts',(8.02773087299994,15.2,-7.29843568400002));
#171453=CARTESIAN_POINT('Ctrl Pts',(8.02773087299994,11.6,-7.29843568400002));
#171454=CARTESIAN_POINT('Ctrl Pts',(8.02634777099994,15.2,-7.29604595200002));
#171455=CARTESIAN_POINT('Ctrl Pts',(8.02634777099994,11.6,-7.29604595200002));
#171456=CARTESIAN_POINT('Ctrl Pts',(8.02496554899994,15.2,-7.29366235400001));
#171457=CARTESIAN_POINT('Ctrl Pts',(8.02496554899994,11.6,-7.29366235400001));
#171458=CARTESIAN_POINT('Ctrl Pts',(8.02358422099994,15.2,-7.29128489700001));
#171459=CARTESIAN_POINT('Ctrl Pts',(8.02358422099994,11.6,-7.29128489700001));
#171460=CARTESIAN_POINT('Ctrl Pts',(8.02220379799994,15.2,-7.28891358600002));
#171461=CARTESIAN_POINT('Ctrl Pts',(8.02220379799994,11.6,-7.28891358600002));
#171462=CARTESIAN_POINT('Ctrl Pts',(8.02082429299994,15.2,-7.28654842400001));
#171463=CARTESIAN_POINT('Ctrl Pts',(8.02082429299994,11.6,-7.28654842400001));
#171464=CARTESIAN_POINT('Ctrl Pts',(8.01944571799994,15.2,-7.28418941900002));
#171465=CARTESIAN_POINT('Ctrl Pts',(8.01944571799994,11.6,-7.28418941900002));
#171466=CARTESIAN_POINT('Ctrl Pts',(8.01806808699994,15.2,-7.28183657500002));
#171467=CARTESIAN_POINT('Ctrl Pts',(8.01806808699994,11.6,-7.28183657500002));
#171468=CARTESIAN_POINT('Ctrl Pts',(8.01669141199995,15.2,-7.27948989700002));
#171469=CARTESIAN_POINT('Ctrl Pts',(8.01669141199995,11.6,-7.27948989700002));
#171470=CARTESIAN_POINT('Ctrl Pts',(8.01531570699994,15.2,-7.27714938900001));
#171471=CARTESIAN_POINT('Ctrl Pts',(8.01531570699994,11.6,-7.27714938900001));
#171472=CARTESIAN_POINT('Ctrl Pts',(8.01394098199994,15.2,-7.27481505600001));
#171473=CARTESIAN_POINT('Ctrl Pts',(8.01394098199994,11.6,-7.27481505600001));
#171474=CARTESIAN_POINT('Ctrl Pts',(8.01256725299995,15.2,-7.27248690400002));
#171475=CARTESIAN_POINT('Ctrl Pts',(8.01256725299995,11.6,-7.27248690400002));
#171476=CARTESIAN_POINT('Ctrl Pts',(8.01119453199994,15.2,-7.27016493800001));
#171477=CARTESIAN_POINT('Ctrl Pts',(8.01119453199994,11.6,-7.27016493800001));
#171478=CARTESIAN_POINT('Ctrl Pts',(8.00982282999994,15.2,-7.26784916400002));
#171479=CARTESIAN_POINT('Ctrl Pts',(8.00982282999994,11.6,-7.26784916400002));
#171480=CARTESIAN_POINT('Ctrl Pts',(8.00845216399994,15.2,-7.26553958500002));
#171481=CARTESIAN_POINT('Ctrl Pts',(8.00845216399994,11.6,-7.26553958500002));
#171482=CARTESIAN_POINT('Ctrl Pts',(8.00708254199994,15.2,-7.26323620600001));
#171483=CARTESIAN_POINT('Ctrl Pts',(8.00708254199994,11.6,-7.26323620600001));
#171484=CARTESIAN_POINT('Ctrl Pts',(8.00571398099994,15.2,-7.26093903400002));
#171485=CARTESIAN_POINT('Ctrl Pts',(8.00571398099994,11.6,-7.26093903400002));
#171486=CARTESIAN_POINT('Ctrl Pts',(8.00434649299994,15.2,-7.25864807300002));
#171487=CARTESIAN_POINT('Ctrl Pts',(8.00434649299994,11.6,-7.25864807300002));
#171488=CARTESIAN_POINT('Ctrl Pts',(8.00298009099994,15.2,-7.25636332800002));
#171489=CARTESIAN_POINT('Ctrl Pts',(8.00298009099994,11.6,-7.25636332800002));
#171490=CARTESIAN_POINT('Ctrl Pts',(8.00161478799994,15.2,-7.25408480400001));
#171491=CARTESIAN_POINT('Ctrl Pts',(8.00161478799994,11.6,-7.25408480400001));
#171492=CARTESIAN_POINT('Ctrl Pts',(8.00025059599994,15.2,-7.25181250700001));
#171493=CARTESIAN_POINT('Ctrl Pts',(8.00025059599994,11.6,-7.25181250700001));
#171494=CARTESIAN_POINT('Ctrl Pts',(7.99888753099995,15.2,-7.24954644100002));
#171495=CARTESIAN_POINT('Ctrl Pts',(7.99888753099995,11.6,-7.24954644100002));
#171496=CARTESIAN_POINT('Ctrl Pts',(7.99752560499994,15.2,-7.24728661100002));
#171497=CARTESIAN_POINT('Ctrl Pts',(7.99752560499994,11.6,-7.24728661100002));
#171498=CARTESIAN_POINT('Ctrl Pts',(7.99616483099994,15.2,-7.24503302300001));
#171499=CARTESIAN_POINT('Ctrl Pts',(7.99616483099994,11.6,-7.24503302300001));
#171500=CARTESIAN_POINT('Ctrl Pts',(7.99480522199994,15.2,-7.24278568000001));
#171501=CARTESIAN_POINT('Ctrl Pts',(7.99480522199994,11.6,-7.24278568000001));
#171502=CARTESIAN_POINT('Ctrl Pts',(7.99344679099995,15.2,-7.24054459100002));
#171503=CARTESIAN_POINT('Ctrl Pts',(7.99344679099995,11.6,-7.24054459100002));
#171504=CARTESIAN_POINT('Ctrl Pts',(7.99208955399994,15.2,-7.23830975700002));
#171505=CARTESIAN_POINT('Ctrl Pts',(7.99208955399994,11.6,-7.23830975700002));
#171506=CARTESIAN_POINT('Ctrl Pts',(7.99073352199994,15.2,-7.23608118600002));
#171507=CARTESIAN_POINT('Ctrl Pts',(7.99073352199994,11.6,-7.23608118600002));
#171508=CARTESIAN_POINT('Ctrl Pts',(7.98937870999994,15.2,-7.23385888200001));
#171509=CARTESIAN_POINT('Ctrl Pts',(7.98937870999994,11.6,-7.23385888200001));
#171510=CARTESIAN_POINT('Ctrl Pts',(7.98802512999995,15.2,-7.23164284900002));
#171511=CARTESIAN_POINT('Ctrl Pts',(7.98802512999995,11.6,-7.23164284900002));
#171512=CARTESIAN_POINT('Ctrl Pts',(7.98667279799994,15.2,-7.22943309400002));
#171513=CARTESIAN_POINT('Ctrl Pts',(7.98667279799994,11.6,-7.22943309400002));
#171514=CARTESIAN_POINT('Ctrl Pts',(7.98532172499994,15.2,-7.22722962000002));
#171515=CARTESIAN_POINT('Ctrl Pts',(7.98532172499994,11.6,-7.22722962000002));
#171516=CARTESIAN_POINT('Ctrl Pts',(7.98397192599994,15.2,-7.22503243400002));
#171517=CARTESIAN_POINT('Ctrl Pts',(7.98397192599994,11.6,-7.22503243400002));
#171518=CARTESIAN_POINT('Ctrl Pts',(7.98262341399994,15.2,-7.22284154100001));
#171519=CARTESIAN_POINT('Ctrl Pts',(7.98262341399994,11.6,-7.22284154100001));
#171520=CARTESIAN_POINT('Ctrl Pts',(7.98127620499994,15.2,-7.22065694600002));
#171521=CARTESIAN_POINT('Ctrl Pts',(7.98127620499994,11.6,-7.22065694600002));
#171522=CARTESIAN_POINT('Ctrl Pts',(7.97993030999994,15.2,-7.21847865300001));
#171523=CARTESIAN_POINT('Ctrl Pts',(7.97993030999994,11.6,-7.21847865300001));
#171524=CARTESIAN_POINT('Ctrl Pts',(7.97858574299994,15.2,-7.21630666700002));
#171525=CARTESIAN_POINT('Ctrl Pts',(7.97858574299994,11.6,-7.21630666700002));
#171526=CARTESIAN_POINT('Ctrl Pts',(7.97724252099994,15.2,-7.21414099500001));
#171527=CARTESIAN_POINT('Ctrl Pts',(7.97724252099994,11.6,-7.21414099500001));
#171528=CARTESIAN_POINT('Ctrl Pts',(7.97590065499994,15.2,-7.21198164000001));
#171529=CARTESIAN_POINT('Ctrl Pts',(7.97590065499994,11.6,-7.21198164000001));
#171530=CARTESIAN_POINT('Ctrl Pts',(7.97456015899995,15.2,-7.20982861000002));
#171531=CARTESIAN_POINT('Ctrl Pts',(7.97456015899995,11.6,-7.20982861000002));
#171532=CARTESIAN_POINT('Ctrl Pts',(7.97322104799994,15.2,-7.20768190700002));
#171533=CARTESIAN_POINT('Ctrl Pts',(7.97322104799994,11.6,-7.20768190700002));
#171534=CARTESIAN_POINT('Ctrl Pts',(7.97188333599994,15.2,-7.20554153800002));
#171535=CARTESIAN_POINT('Ctrl Pts',(7.97188333599994,11.6,-7.20554153800002));
#171536=CARTESIAN_POINT('Ctrl Pts',(7.97054703699994,15.2,-7.20340750800001));
#171537=CARTESIAN_POINT('Ctrl Pts',(7.97054703699994,11.6,-7.20340750800001));
#171538=CARTESIAN_POINT('Ctrl Pts',(7.96921216599995,15.2,-7.20127982100002));
#171539=CARTESIAN_POINT('Ctrl Pts',(7.96921216599995,11.6,-7.20127982100002));
#171540=CARTESIAN_POINT('Ctrl Pts',(7.96787873499994,15.2,-7.19915848400002));
#171541=CARTESIAN_POINT('Ctrl Pts',(7.96787873499994,11.6,-7.19915848400002));
#171542=CARTESIAN_POINT('Ctrl Pts',(7.96654675899994,15.2,-7.19704350100002));
#171543=CARTESIAN_POINT('Ctrl Pts',(7.96654675899994,11.6,-7.19704350100002));
#171544=CARTESIAN_POINT('Ctrl Pts',(7.96521625299994,15.2,-7.19493487700002));
#171545=CARTESIAN_POINT('Ctrl Pts',(7.96521625299994,11.6,-7.19493487700002));
#171546=CARTESIAN_POINT('Ctrl Pts',(7.96388723099994,15.2,-7.19283261800002));
#171547=CARTESIAN_POINT('Ctrl Pts',(7.96388723099994,11.6,-7.19283261800002));
#171548=CARTESIAN_POINT('Ctrl Pts',(7.96255970799994,15.2,-7.19073672800001));
#171549=CARTESIAN_POINT('Ctrl Pts',(7.96255970799994,11.6,-7.19073672800001));
#171550=CARTESIAN_POINT('Ctrl Pts',(7.96123369799994,15.2,-7.18864721300001));
#171551=CARTESIAN_POINT('Ctrl Pts',(7.96123369799994,11.6,-7.18864721300001));
#171552=CARTESIAN_POINT('Ctrl Pts',(7.95990921399994,15.2,-7.18656407900002));
#171553=CARTESIAN_POINT('Ctrl Pts',(7.95990921399994,11.6,-7.18656407900002));
#171554=CARTESIAN_POINT('Ctrl Pts',(7.95858627199994,15.2,-7.18448732900002));
#171555=CARTESIAN_POINT('Ctrl Pts',(7.95858627199994,11.6,-7.18448732900002));
#171556=CARTESIAN_POINT('Ctrl Pts',(7.95726488599994,15.2,-7.18241697000002));
#171557=CARTESIAN_POINT('Ctrl Pts',(7.95726488599994,11.6,-7.18241697000002));
#171558=CARTESIAN_POINT('Ctrl Pts',(7.95594507099994,15.2,-7.18035300600001));
#171559=CARTESIAN_POINT('Ctrl Pts',(7.95594507099994,11.6,-7.18035300600001));
#171560=CARTESIAN_POINT('Ctrl Pts',(7.95462684099994,15.2,-7.17829544400002));
#171561=CARTESIAN_POINT('Ctrl Pts',(7.95462684099994,11.6,-7.17829544400002));
#171562=CARTESIAN_POINT('Ctrl Pts',(7.95331021099994,15.2,-7.17624428700002));
#171563=CARTESIAN_POINT('Ctrl Pts',(7.95331021099994,11.6,-7.17624428700002));
#171564=CARTESIAN_POINT('Ctrl Pts',(7.95199519599994,15.2,-7.17419954200002));
#171565=CARTESIAN_POINT('Ctrl Pts',(7.95199519599994,11.6,-7.17419954200002));
#171566=CARTESIAN_POINT('Ctrl Pts',(7.95068181099994,15.2,-7.17216121300002));
#171567=CARTESIAN_POINT('Ctrl Pts',(7.95068181099994,11.6,-7.17216121300002));
#171568=CARTESIAN_POINT('Ctrl Pts',(7.94937006899994,15.2,-7.17012930500001));
#171569=CARTESIAN_POINT('Ctrl Pts',(7.94937006899994,11.6,-7.17012930500001));
#171570=CARTESIAN_POINT('Ctrl Pts',(7.94805998699994,15.2,-7.16810382500002));
#171571=CARTESIAN_POINT('Ctrl Pts',(7.94805998699994,11.6,-7.16810382500002));
#171572=CARTESIAN_POINT('Ctrl Pts',(7.94675157799994,15.2,-7.16608477700002));
#171573=CARTESIAN_POINT('Ctrl Pts',(7.94675157799994,11.6,-7.16608477700002));
#171574=CARTESIAN_POINT('Ctrl Pts',(7.94544485899995,15.2,-7.16407216700001));
#171575=CARTESIAN_POINT('Ctrl Pts',(7.94544485899995,11.6,-7.16407216700001));
#171576=CARTESIAN_POINT('Ctrl Pts',(7.94413984299994,15.2,-7.16206599900002));
#171577=CARTESIAN_POINT('Ctrl Pts',(7.94413984299994,11.6,-7.16206599900002));
#171578=CARTESIAN_POINT('Ctrl Pts',(7.94283654599995,15.2,-7.16006627800001));
#171579=CARTESIAN_POINT('Ctrl Pts',(7.94283654599995,11.6,-7.16006627800001));
#171580=CARTESIAN_POINT('Ctrl Pts',(7.94153498399995,15.2,-7.15807301100002));
#171581=CARTESIAN_POINT('Ctrl Pts',(7.94153498399995,11.6,-7.15807301100002));
#171582=CARTESIAN_POINT('Ctrl Pts',(7.94023516999995,15.2,-7.15608620200002));
#171583=CARTESIAN_POINT('Ctrl Pts',(7.94023516999995,11.6,-7.15608620200002));
#171584=CARTESIAN_POINT('Ctrl Pts',(7.93893712099995,15.2,-7.15410585600001));
#171585=CARTESIAN_POINT('Ctrl Pts',(7.93893712099995,11.6,-7.15410585600001));
#171586=CARTESIAN_POINT('Ctrl Pts',(7.93764085099995,15.2,-7.15213198100002));
#171587=CARTESIAN_POINT('Ctrl Pts',(7.93764085099995,11.6,-7.15213198100002));
#171588=CARTESIAN_POINT('Ctrl Pts',(7.93634637499995,15.2,-7.15016457800001));
#171589=CARTESIAN_POINT('Ctrl Pts',(7.93634637499995,11.6,-7.15016457800001));
#171590=CARTESIAN_POINT('Ctrl Pts',(7.93505370999994,15.2,-7.14820365600002));
#171591=CARTESIAN_POINT('Ctrl Pts',(7.93505370999994,11.6,-7.14820365600002));
#171592=CARTESIAN_POINT('Ctrl Pts',(7.93376286999995,15.2,-7.14624921800001));
#171593=CARTESIAN_POINT('Ctrl Pts',(7.93376286999995,11.6,-7.14624921800001));
#171594=CARTESIAN_POINT('Ctrl Pts',(7.93247387099994,15.2,-7.14430127000002));
#171595=CARTESIAN_POINT('Ctrl Pts',(7.93247387099994,11.6,-7.14430127000002));
#171596=CARTESIAN_POINT('Ctrl Pts',(7.93118672799995,15.2,-7.14235981700002));
#171597=CARTESIAN_POINT('Ctrl Pts',(7.93118672799995,11.6,-7.14235981700002));
#171598=CARTESIAN_POINT('Ctrl Pts',(7.92990145699994,15.2,-7.14042486500002));
#171599=CARTESIAN_POINT('Ctrl Pts',(7.92990145699994,11.6,-7.14042486500002));
#171600=CARTESIAN_POINT('Ctrl Pts',(7.92861807299994,15.2,-7.13849641800002));
#171601=CARTESIAN_POINT('Ctrl Pts',(7.92861807299994,11.6,-7.13849641800002));
#171602=CARTESIAN_POINT('Ctrl Pts',(7.92733659099994,15.2,-7.13657448300002));
#171603=CARTESIAN_POINT('Ctrl Pts',(7.92733659099994,11.6,-7.13657448300002));
#171604=CARTESIAN_POINT('Ctrl Pts',(7.92605702899994,15.2,-7.13465906400002));
#171605=CARTESIAN_POINT('Ctrl Pts',(7.92605702899994,11.6,-7.13465906400002));
#171606=CARTESIAN_POINT('Ctrl Pts',(7.92477940099995,15.2,-7.13275016800001));
#171607=CARTESIAN_POINT('Ctrl Pts',(7.92477940099995,11.6,-7.13275016800001));
#171608=CARTESIAN_POINT('Ctrl Pts',(7.92350372299994,15.2,-7.13084779800001));
#171609=CARTESIAN_POINT('Ctrl Pts',(7.92350372299994,11.6,-7.13084779800001));
#171610=CARTESIAN_POINT('Ctrl Pts',(7.92223000999994,15.2,-7.12895196000002));
#171611=CARTESIAN_POINT('Ctrl Pts',(7.92223000999994,11.6,-7.12895196000002));
#171612=CARTESIAN_POINT('Ctrl Pts',(7.92095827899994,15.2,-7.12706266100002));
#171613=CARTESIAN_POINT('Ctrl Pts',(7.92095827899994,11.6,-7.12706266100002));
#171614=CARTESIAN_POINT('Ctrl Pts',(7.91968854599994,15.2,-7.12517990400002));
#171615=CARTESIAN_POINT('Ctrl Pts',(7.91968854599994,11.6,-7.12517990400002));
#171616=CARTESIAN_POINT('Ctrl Pts',(7.91842082599994,15.2,-7.12330369600001));
#171617=CARTESIAN_POINT('Ctrl Pts',(7.91842082599994,11.6,-7.12330369600001));
#171618=CARTESIAN_POINT('Ctrl Pts',(7.91715513599994,15.2,-7.12143404200001));
#171619=CARTESIAN_POINT('Ctrl Pts',(7.91715513599994,11.6,-7.12143404200001));
#171620=CARTESIAN_POINT('Ctrl Pts',(7.91589149199995,15.2,-7.11957094700002));
#171621=CARTESIAN_POINT('Ctrl Pts',(7.91589149199995,11.6,-7.11957094700002));
#171622=CARTESIAN_POINT('Ctrl Pts',(7.91462990899995,15.2,-7.11771441600002));
#171623=CARTESIAN_POINT('Ctrl Pts',(7.91462990899995,11.6,-7.11771441600002));
#171624=CARTESIAN_POINT('Ctrl Pts',(7.91337040399994,15.2,-7.11586445500001));
#171625=CARTESIAN_POINT('Ctrl Pts',(7.91337040399994,11.6,-7.11586445500001));
#171626=CARTESIAN_POINT('Ctrl Pts',(7.91211299299994,15.2,-7.11402106900002));
#171627=CARTESIAN_POINT('Ctrl Pts',(7.91211299299994,11.6,-7.11402106900002));
#171628=CARTESIAN_POINT('Ctrl Pts',(7.91085769199994,15.2,-7.11218426400002));
#171629=CARTESIAN_POINT('Ctrl Pts',(7.91085769199994,11.6,-7.11218426400002));
#171630=CARTESIAN_POINT('Ctrl Pts',(7.90960451799994,15.2,-7.11035404400001));
#171631=CARTESIAN_POINT('Ctrl Pts',(7.90960451799994,11.6,-7.11035404400001));
#171632=CARTESIAN_POINT('Ctrl Pts',(7.90835348799995,15.2,-7.10853041700001));
#171633=CARTESIAN_POINT('Ctrl Pts',(7.90835348799995,11.6,-7.10853041700001));
#171634=CARTESIAN_POINT('Ctrl Pts',(7.90710461699994,15.2,-7.10671338500001));
#171635=CARTESIAN_POINT('Ctrl Pts',(7.90710461699994,11.6,-7.10671338500001));
#171636=CARTESIAN_POINT('Ctrl Pts',(7.90585792199994,15.2,-7.10490295600002));
#171637=CARTESIAN_POINT('Ctrl Pts',(7.90585792199994,11.6,-7.10490295600002));
#171638=CARTESIAN_POINT('Ctrl Pts',(7.90461341899995,15.2,-7.10309913500001));
#171639=CARTESIAN_POINT('Ctrl Pts',(7.90461341899995,11.6,-7.10309913500001));
#171640=CARTESIAN_POINT('Ctrl Pts',(7.90337112499994,15.2,-7.10130192600002));
#171641=CARTESIAN_POINT('Ctrl Pts',(7.90337112499994,11.6,-7.10130192600002));
#171642=CARTESIAN_POINT('Ctrl Pts',(7.90213105799995,15.2,-7.09951133600002));
#171643=CARTESIAN_POINT('Ctrl Pts',(7.90213105799995,11.6,-7.09951133600002));
#171644=CARTESIAN_POINT('Ctrl Pts',(7.90089323199994,15.2,-7.09772736900002));
#171645=CARTESIAN_POINT('Ctrl Pts',(7.90089323199994,11.6,-7.09772736900002));
#171646=CARTESIAN_POINT('Ctrl Pts',(7.89965766699994,15.2,-7.09595003100001));
#171647=CARTESIAN_POINT('Ctrl Pts',(7.89965766699994,11.6,-7.09595003100001));
#171648=CARTESIAN_POINT('Ctrl Pts',(7.89842437699994,15.2,-7.09417932900001));
#171649=CARTESIAN_POINT('Ctrl Pts',(7.89842437699994,11.6,-7.09417932900001));
#171650=CARTESIAN_POINT('Ctrl Pts',(7.89719338099995,15.2,-7.09241526600002));
#171651=CARTESIAN_POINT('Ctrl Pts',(7.89719338099995,11.6,-7.09241526600002));
#171652=CARTESIAN_POINT('Ctrl Pts',(7.89596469399994,15.2,-7.09065784900002));
#171653=CARTESIAN_POINT('Ctrl Pts',(7.89596469399994,11.6,-7.09065784900002));
#171654=CARTESIAN_POINT('Ctrl Pts',(7.89473833399994,15.2,-7.08890708300002));
#171655=CARTESIAN_POINT('Ctrl Pts',(7.89473833399994,11.6,-7.08890708300002));
#171656=CARTESIAN_POINT('Ctrl Pts',(7.89351431799994,15.2,-7.08716297200001));
#171657=CARTESIAN_POINT('Ctrl Pts',(7.89351431799994,11.6,-7.08716297200001));
#171658=CARTESIAN_POINT('Ctrl Pts',(7.89229266299994,15.2,-7.08542552500001));
#171659=CARTESIAN_POINT('Ctrl Pts',(7.89229266299994,11.6,-7.08542552500001));
#171660=CARTESIAN_POINT('Ctrl Pts',(7.89107338599995,15.2,-7.08369474300002));
#171661=CARTESIAN_POINT('Ctrl Pts',(7.89107338599995,11.6,-7.08369474300002));
#171662=CARTESIAN_POINT('Ctrl Pts',(7.88985650599995,15.2,-7.08197063500001));
#171663=CARTESIAN_POINT('Ctrl Pts',(7.88985650599995,11.6,-7.08197063500001));
#171664=CARTESIAN_POINT('Ctrl Pts',(7.88864203699994,15.2,-7.08025320500001));
#171665=CARTESIAN_POINT('Ctrl Pts',(7.88864203699994,11.6,-7.08025320500001));
#171666=CARTESIAN_POINT('Ctrl Pts',(7.88742999899994,15.2,-7.07854245900001));
#171667=CARTESIAN_POINT('Ctrl Pts',(7.88742999899994,11.6,-7.07854245900001));
#171668=CARTESIAN_POINT('Ctrl Pts',(7.88622040799994,15.2,-7.07683840200002));
#171669=CARTESIAN_POINT('Ctrl Pts',(7.88622040799994,11.6,-7.07683840200002));
#171670=CARTESIAN_POINT('Ctrl Pts',(7.88501328299994,15.2,-7.07514104000002));
#171671=CARTESIAN_POINT('Ctrl Pts',(7.88501328299994,11.6,-7.07514104000002));
#171672=CARTESIAN_POINT('Ctrl Pts',(7.88380863899994,15.2,-7.07345037800001));
#171673=CARTESIAN_POINT('Ctrl Pts',(7.88380863899994,11.6,-7.07345037800001));
#171674=CARTESIAN_POINT('Ctrl Pts',(7.88260649599994,15.2,-7.07176642200002));
#171675=CARTESIAN_POINT('Ctrl Pts',(7.88260649599994,11.6,-7.07176642200002));
#171676=CARTESIAN_POINT('Ctrl Pts',(7.88140687099995,15.2,-7.07008917700002));
#171677=CARTESIAN_POINT('Ctrl Pts',(7.88140687099995,11.6,-7.07008917700002));
#171678=CARTESIAN_POINT('Ctrl Pts',(7.88020978099994,15.2,-7.06841865000002));
#171679=CARTESIAN_POINT('Ctrl Pts',(7.88020978099994,11.6,-7.06841865000002));
#171680=CARTESIAN_POINT('Ctrl Pts',(7.87901524399994,15.2,-7.06675484400002));
#171681=CARTESIAN_POINT('Ctrl Pts',(7.87901524399994,11.6,-7.06675484400002));
#171682=CARTESIAN_POINT('Ctrl Pts',(7.87782327799994,15.2,-7.06509776600001));
#171683=CARTESIAN_POINT('Ctrl Pts',(7.87782327799994,11.6,-7.06509776600001));
#171684=CARTESIAN_POINT('Ctrl Pts',(7.87663390099994,15.2,-7.06344742200002));
#171685=CARTESIAN_POINT('Ctrl Pts',(7.87663390099994,11.6,-7.06344742200002));
#171686=CARTESIAN_POINT('Ctrl Pts',(7.87544713199994,15.2,-7.06180381500002));
#171687=CARTESIAN_POINT('Ctrl Pts',(7.87544713199994,11.6,-7.06180381500002));
#171688=CARTESIAN_POINT('Ctrl Pts',(7.87426298699994,15.2,-7.06016695500002));
#171689=CARTESIAN_POINT('Ctrl Pts',(7.87426298699994,11.6,-7.06016695500002));
#171690=CARTESIAN_POINT('Ctrl Pts',(7.87308148499994,15.2,-7.05853684400001));
#171691=CARTESIAN_POINT('Ctrl Pts',(7.87308148499994,11.6,-7.05853684400001));
#171692=CARTESIAN_POINT('Ctrl Pts',(7.87190264399995,15.2,-7.05691348900002));
#171693=CARTESIAN_POINT('Ctrl Pts',(7.87190264399995,11.6,-7.05691348900002));
#171694=CARTESIAN_POINT('Ctrl Pts',(7.87072648199994,15.2,-7.05529689500001));
#171695=CARTESIAN_POINT('Ctrl Pts',(7.87072648199994,11.6,-7.05529689500001));
#171696=CARTESIAN_POINT('Ctrl Pts',(7.86955301799994,15.2,-7.05368706700002));
#171697=CARTESIAN_POINT('Ctrl Pts',(7.86955301799994,11.6,-7.05368706700002));
#171698=CARTESIAN_POINT('Ctrl Pts',(7.86838226999994,15.2,-7.05208401300002));
#171699=CARTESIAN_POINT('Ctrl Pts',(7.86838226999994,11.6,-7.05208401300002));
#171700=CARTESIAN_POINT('Ctrl Pts',(7.86721425699994,15.2,-7.05048773600002));
#171701=CARTESIAN_POINT('Ctrl Pts',(7.86721425699994,11.6,-7.05048773600002));
#171702=CARTESIAN_POINT('Ctrl Pts',(7.86604899599994,15.2,-7.04889824300002));
#171703=CARTESIAN_POINT('Ctrl Pts',(7.86604899599994,11.6,-7.04889824300002));
#171704=CARTESIAN_POINT('Ctrl Pts',(7.86488650699994,15.2,-7.04731553900002));
#171705=CARTESIAN_POINT('Ctrl Pts',(7.86488650699994,11.6,-7.04731553900002));
#171706=CARTESIAN_POINT('Ctrl Pts',(7.86372680699994,15.2,-7.04573963100002));
#171707=CARTESIAN_POINT('Ctrl Pts',(7.86372680699994,11.6,-7.04573963100002));
#171708=CARTESIAN_POINT('Ctrl Pts',(7.86256991599994,15.2,-7.04417052200002));
#171709=CARTESIAN_POINT('Ctrl Pts',(7.86256991599994,11.6,-7.04417052200002));
#171710=CARTESIAN_POINT('Ctrl Pts',(7.86141585299994,15.2,-7.04260821900001));
#171711=CARTESIAN_POINT('Ctrl Pts',(7.86141585299994,11.6,-7.04260821900001));
#171712=CARTESIAN_POINT('Ctrl Pts',(7.86026463599995,15.2,-7.04105272900001));
#171713=CARTESIAN_POINT('Ctrl Pts',(7.86026463599995,11.6,-7.04105272900001));
#171714=CARTESIAN_POINT('Ctrl Pts',(7.85911628399995,15.2,-7.03950405600001));
#171715=CARTESIAN_POINT('Ctrl Pts',(7.85911628399995,11.6,-7.03950405600001));
#171716=CARTESIAN_POINT('Ctrl Pts',(7.85797081499994,15.2,-7.03796220700001));
#171717=CARTESIAN_POINT('Ctrl Pts',(7.85797081499994,11.6,-7.03796220700001));
#171718=CARTESIAN_POINT('Ctrl Pts',(7.85682825099994,15.2,-7.03642718500002));
#171719=CARTESIAN_POINT('Ctrl Pts',(7.85682825099994,11.6,-7.03642718500002));
#171720=CARTESIAN_POINT('Ctrl Pts',(7.85568860799994,15.2,-7.03489899900001));
#171721=CARTESIAN_POINT('Ctrl Pts',(7.85568860799994,11.6,-7.03489899900001));
#171722=CARTESIAN_POINT('Ctrl Pts',(7.85455190599994,15.2,-7.03337765200001));
#171723=CARTESIAN_POINT('Ctrl Pts',(7.85455190599994,11.6,-7.03337765200001));
#171724=CARTESIAN_POINT('Ctrl Pts',(7.85341816499994,15.2,-7.03186315100002));
#171725=CARTESIAN_POINT('Ctrl Pts',(7.85341816499994,11.6,-7.03186315100002));
#171726=CARTESIAN_POINT('Ctrl Pts',(7.85228740299994,15.2,-7.03035550200001));
#171727=CARTESIAN_POINT('Ctrl Pts',(7.85228740299994,11.6,-7.03035550200001));
#171728=CARTESIAN_POINT('Ctrl Pts',(7.85115964099995,15.2,-7.02885471000001));
#171729=CARTESIAN_POINT('Ctrl Pts',(7.85115964099995,11.6,-7.02885471000001));
#171730=CARTESIAN_POINT('Ctrl Pts',(7.85003489699994,15.2,-7.02736078100001));
#171731=CARTESIAN_POINT('Ctrl Pts',(7.85003489699994,11.6,-7.02736078100001));
#171732=CARTESIAN_POINT('Ctrl Pts',(7.84891319099994,15.2,-7.02587372100002));
#171733=CARTESIAN_POINT('Ctrl Pts',(7.84891319099994,11.6,-7.02587372100002));
#171734=CARTESIAN_POINT('Ctrl Pts',(7.84779454299994,15.2,-7.02439353600001));
#171735=CARTESIAN_POINT('Ctrl Pts',(7.84779454299994,11.6,-7.02439353600001));
#171736=CARTESIAN_POINT('Ctrl Pts',(7.84667897299994,15.2,-7.02292023000001));
#171737=CARTESIAN_POINT('Ctrl Pts',(7.84667897299994,11.6,-7.02292023000001));
#171738=CARTESIAN_POINT('Ctrl Pts',(7.84556649899995,15.2,-7.02145381000002));
#171739=CARTESIAN_POINT('Ctrl Pts',(7.84556649899995,11.6,-7.02145381000002));
#171740=CARTESIAN_POINT('Ctrl Pts',(7.84445714199994,15.2,-7.01999428200001));
#171741=CARTESIAN_POINT('Ctrl Pts',(7.84445714199994,11.6,-7.01999428200001));
#171742=CARTESIAN_POINT('Ctrl Pts',(7.84335092199994,15.2,-7.01854165200002));
#171743=CARTESIAN_POINT('Ctrl Pts',(7.84335092199994,11.6,-7.01854165200002));
#171744=CARTESIAN_POINT('Ctrl Pts',(7.84224785899994,15.2,-7.01709592400002));
#171745=CARTESIAN_POINT('Ctrl Pts',(7.84224785899994,11.6,-7.01709592400002));
#171746=CARTESIAN_POINT('Ctrl Pts',(7.84114797199994,15.2,-7.01565710600002));
#171747=CARTESIAN_POINT('Ctrl Pts',(7.84114797199994,11.6,-7.01565710600002));
#171748=CARTESIAN_POINT('Ctrl Pts',(7.84005128199994,15.2,-7.01422520300002));
#171749=CARTESIAN_POINT('Ctrl Pts',(7.84005128199994,11.6,-7.01422520300002));
#171750=CARTESIAN_POINT('Ctrl Pts',(7.83895780899994,15.2,-7.01280021900001));
#171751=CARTESIAN_POINT('Ctrl Pts',(7.83895780899994,11.6,-7.01280021900001));
#171752=CARTESIAN_POINT('Ctrl Pts',(7.83786757299994,15.2,-7.01138216400001));
#171753=CARTESIAN_POINT('Ctrl Pts',(7.83786757299994,11.6,-7.01138216400001));
#171754=CARTESIAN_POINT('Ctrl Pts',(7.83678059499994,15.2,-7.00997103900002));
#171755=CARTESIAN_POINT('Ctrl Pts',(7.83678059499994,11.6,-7.00997103900002));
#171756=CARTESIAN_POINT('Ctrl Pts',(7.83569689499994,15.2,-7.00856685400002));
#171757=CARTESIAN_POINT('Ctrl Pts',(7.83569689499994,11.6,-7.00856685400002));
#171758=CARTESIAN_POINT('Ctrl Pts',(7.83461649299994,15.2,-7.00716961200002));
#171759=CARTESIAN_POINT('Ctrl Pts',(7.83461649299994,11.6,-7.00716961200002));
#171760=CARTESIAN_POINT('Ctrl Pts',(7.83353940999994,15.2,-7.00577931900002));
#171761=CARTESIAN_POINT('Ctrl Pts',(7.83353940999994,11.6,-7.00577931900002));
#171762=CARTESIAN_POINT('Ctrl Pts',(7.83246566699995,15.2,-7.00439598200001));
#171763=CARTESIAN_POINT('Ctrl Pts',(7.83246566699995,11.6,-7.00439598200001));
#171764=CARTESIAN_POINT('Ctrl Pts',(7.83139528399994,15.2,-7.00301960700001));
#171765=CARTESIAN_POINT('Ctrl Pts',(7.83139528399994,11.6,-7.00301960700001));
#171766=CARTESIAN_POINT('Ctrl Pts',(7.83032828199994,15.2,-7.00165020000002));
#171767=CARTESIAN_POINT('Ctrl Pts',(7.83032828199994,11.6,-7.00165020000002));
#171768=CARTESIAN_POINT('Ctrl Pts',(7.82926468199994,15.2,-7.00028776600002));
#171769=CARTESIAN_POINT('Ctrl Pts',(7.82926468199994,11.6,-7.00028776600002));
#171770=CARTESIAN_POINT('Ctrl Pts',(7.82820450599995,15.2,-6.99893231100001));
#171771=CARTESIAN_POINT('Ctrl Pts',(7.82820450599995,11.6,-6.99893231100001));
#171772=CARTESIAN_POINT('Ctrl Pts',(7.82714777299995,15.2,-6.99758384000001));
#171773=CARTESIAN_POINT('Ctrl Pts',(7.82714777299995,11.6,-6.99758384000001));
#171774=CARTESIAN_POINT('Ctrl Pts',(7.82609450599994,15.2,-6.99624236100002));
#171775=CARTESIAN_POINT('Ctrl Pts',(7.82609450599994,11.6,-6.99624236100002));
#171776=CARTESIAN_POINT('Ctrl Pts',(7.82504472499994,15.2,-6.99490787800002));
#171777=CARTESIAN_POINT('Ctrl Pts',(7.82504472499994,11.6,-6.99490787800002));
#171778=CARTESIAN_POINT('Ctrl Pts',(7.82399845099994,15.2,-6.99358039900002));
#171779=CARTESIAN_POINT('Ctrl Pts',(7.82399845099994,11.6,-6.99358039900002));
#171780=CARTESIAN_POINT('Ctrl Pts',(7.82295570699994,15.2,-6.99225992800002));
#171781=CARTESIAN_POINT('Ctrl Pts',(7.82295570699994,11.6,-6.99225992800002));
#171782=CARTESIAN_POINT('Ctrl Pts',(7.82191651399994,15.2,-6.99094647200001));
#171783=CARTESIAN_POINT('Ctrl Pts',(7.82191651399994,11.6,-6.99094647200001));
#171784=CARTESIAN_POINT('Ctrl Pts',(7.82088089199994,15.2,-6.98964003700001));
#171785=CARTESIAN_POINT('Ctrl Pts',(7.82088089199994,11.6,-6.98964003700001));
#171786=CARTESIAN_POINT('Ctrl Pts',(7.81984886499994,15.2,-6.98834063000002));
#171787=CARTESIAN_POINT('Ctrl Pts',(7.81984886499994,11.6,-6.98834063000002));
#171788=CARTESIAN_POINT('Ctrl Pts',(7.81882045199994,15.2,-6.98704825400001));
#171789=CARTESIAN_POINT('Ctrl Pts',(7.81882045199994,11.6,-6.98704825400001));
#171790=CARTESIAN_POINT('Ctrl Pts',(7.81779567699994,15.2,-6.98576291700002));
#171791=CARTESIAN_POINT('Ctrl Pts',(7.81779567699994,11.6,-6.98576291700002));
#171792=CARTESIAN_POINT('Ctrl Pts',(7.81677456099994,15.2,-6.98448462500001));
#171793=CARTESIAN_POINT('Ctrl Pts',(7.81677456099994,11.6,-6.98448462500001));
#171794=CARTESIAN_POINT('Ctrl Pts',(7.81575712599994,15.2,-6.98321338300002));
#171795=CARTESIAN_POINT('Ctrl Pts',(7.81575712599994,11.6,-6.98321338300002));
#171796=CARTESIAN_POINT('Ctrl Pts',(7.81474339499994,15.2,-6.98194919900001));
#171797=CARTESIAN_POINT('Ctrl Pts',(7.81474339499994,11.6,-6.98194919900001));
#171798=CARTESIAN_POINT('Ctrl Pts',(7.81373338799995,15.2,-6.98069207700001));
#171799=CARTESIAN_POINT('Ctrl Pts',(7.81373338799995,11.6,-6.98069207700001));
#171800=CARTESIAN_POINT('Ctrl Pts',(7.81272712999994,15.2,-6.97944202400001));
#171801=CARTESIAN_POINT('Ctrl Pts',(7.81272712999994,11.6,-6.97944202400001));
#171802=CARTESIAN_POINT('Ctrl Pts',(7.81172464099994,15.2,-6.97819904500002));
#171803=CARTESIAN_POINT('Ctrl Pts',(7.81172464099994,11.6,-6.97819904500002));
#171804=CARTESIAN_POINT('Ctrl Pts',(7.81072594399994,15.2,-6.97696314800002));
#171805=CARTESIAN_POINT('Ctrl Pts',(7.81072594399994,11.6,-6.97696314800002));
#171806=CARTESIAN_POINT('Ctrl Pts',(7.80973106299995,15.2,-6.97573433800001));
#171807=CARTESIAN_POINT('Ctrl Pts',(7.80973106299995,11.6,-6.97573433800001));
#171808=CARTESIAN_POINT('Ctrl Pts',(7.80874001999995,15.2,-6.97451262100002));
#171809=CARTESIAN_POINT('Ctrl Pts',(7.80874001999995,11.6,-6.97451262100002));
#171810=CARTESIAN_POINT('Ctrl Pts',(7.80775283599994,15.2,-6.97329800400002));
#171811=CARTESIAN_POINT('Ctrl Pts',(7.80775283599994,11.6,-6.97329800400002));
#171812=CARTESIAN_POINT('Ctrl Pts',(7.80676953599994,15.2,-6.97209049100002));
#171813=CARTESIAN_POINT('Ctrl Pts',(7.80676953599994,11.6,-6.97209049100002));
#171814=CARTESIAN_POINT('Ctrl Pts',(7.80579014099994,15.2,-6.97089009000001));
#171815=CARTESIAN_POINT('Ctrl Pts',(7.80579014099994,11.6,-6.97089009000001));
#171816=CARTESIAN_POINT('Ctrl Pts',(7.80481467499994,15.2,-6.96969680700001));
#171817=CARTESIAN_POINT('Ctrl Pts',(7.80481467499994,11.6,-6.96969680700001));
#171818=CARTESIAN_POINT('Ctrl Pts',(7.80384316099994,15.2,-6.96851064800001));
#171819=CARTESIAN_POINT('Ctrl Pts',(7.80384316099994,11.6,-6.96851064800001));
#171820=CARTESIAN_POINT('Ctrl Pts',(7.80287562299995,15.2,-6.96733161900001));
#171821=CARTESIAN_POINT('Ctrl Pts',(7.80287562299995,11.6,-6.96733161900001));
#171822=CARTESIAN_POINT('Ctrl Pts',(7.80191208299994,15.2,-6.96615972600001));
#171823=CARTESIAN_POINT('Ctrl Pts',(7.80191208299994,11.6,-6.96615972600001));
#171824=CARTESIAN_POINT('Ctrl Pts',(7.80095256499994,15.2,-6.96499497500002));
#171825=CARTESIAN_POINT('Ctrl Pts',(7.80095256499994,11.6,-6.96499497500002));
#171826=CARTESIAN_POINT('Ctrl Pts',(7.79999709199994,15.2,-6.96383737300001));
#171827=CARTESIAN_POINT('Ctrl Pts',(7.79999709199994,11.6,-6.96383737300001));
#171828=CARTESIAN_POINT('Ctrl Pts',(7.79904568799994,15.2,-6.96268692600002));
#171829=CARTESIAN_POINT('Ctrl Pts',(7.79904568799994,11.6,-6.96268692600002));
#171830=CARTESIAN_POINT('Ctrl Pts',(7.79809837699994,15.2,-6.96154364000002));
#171831=CARTESIAN_POINT('Ctrl Pts',(7.79809837699994,11.6,-6.96154364000002));
#171832=CARTESIAN_POINT('Ctrl Pts',(7.79715518199994,15.2,-6.96040752000001));
#171833=CARTESIAN_POINT('Ctrl Pts',(7.79715518199994,11.6,-6.96040752000001));
#171834=CARTESIAN_POINT('Ctrl Pts',(7.79621612699994,15.2,-6.95927857500001));
#171835=CARTESIAN_POINT('Ctrl Pts',(7.79621612699994,11.6,-6.95927857500001));
#171836=CARTESIAN_POINT('Ctrl Pts',(7.79528123699994,15.2,-6.95815681000001));
#171837=CARTESIAN_POINT('Ctrl Pts',(7.79528123699994,11.6,-6.95815681000001));
#171838=CARTESIAN_POINT('Ctrl Pts',(7.79435053399994,15.2,-6.95704223000002));
#171839=CARTESIAN_POINT('Ctrl Pts',(7.79435053399994,11.6,-6.95704223000002));
#171840=CARTESIAN_POINT('Ctrl Pts',(7.79342404399994,15.2,-6.95593484200002));
#171841=CARTESIAN_POINT('Ctrl Pts',(7.79342404399994,11.6,-6.95593484200002));
#171842=CARTESIAN_POINT('Ctrl Pts',(7.79250179099995,15.2,-6.95483465400001));
#171843=CARTESIAN_POINT('Ctrl Pts',(7.79250179099995,11.6,-6.95483465400001));
#171844=CARTESIAN_POINT('Ctrl Pts',(7.79158379899994,15.2,-6.95374167100002));
#171845=CARTESIAN_POINT('Ctrl Pts',(7.79158379899994,11.6,-6.95374167100002));
#171846=CARTESIAN_POINT('Ctrl Pts',(7.79067009299995,15.2,-6.95265589900002));
#171847=CARTESIAN_POINT('Ctrl Pts',(7.79067009299995,11.6,-6.95265589900002));
#171848=CARTESIAN_POINT('Ctrl Pts',(7.78976069699994,15.2,-6.95157734400001));
#171849=CARTESIAN_POINT('Ctrl Pts',(7.78976069699994,11.6,-6.95157734400001));
#171850=CARTESIAN_POINT('Ctrl Pts',(7.78885563499994,15.2,-6.95050601300002));
#171851=CARTESIAN_POINT('Ctrl Pts',(7.78885563499994,11.6,-6.95050601300002));
#171852=CARTESIAN_POINT('Ctrl Pts',(7.78795493299994,15.2,-6.94944191300002));
#171853=CARTESIAN_POINT('Ctrl Pts',(7.78795493299994,11.6,-6.94944191300002));
#171854=CARTESIAN_POINT('Ctrl Pts',(7.78705861699994,15.2,-6.94838504900002));
#171855=CARTESIAN_POINT('Ctrl Pts',(7.78705861699994,11.6,-6.94838504900002));
#171856=CARTESIAN_POINT('Ctrl Pts',(7.78616670899994,15.2,-6.94733542900002));
#171857=CARTESIAN_POINT('Ctrl Pts',(7.78616670899994,11.6,-6.94733542900002));
#171858=CARTESIAN_POINT('Ctrl Pts',(7.78527923799994,15.2,-6.94629305800002));
#171859=CARTESIAN_POINT('Ctrl Pts',(7.78527923799994,11.6,-6.94629305800002));
#171860=CARTESIAN_POINT('Ctrl Pts',(7.78439622499994,15.2,-6.94525794300001));
#171861=CARTESIAN_POINT('Ctrl Pts',(7.78439622499994,11.6,-6.94525794300001));
#171862=CARTESIAN_POINT('Ctrl Pts',(7.78351769799994,15.2,-6.94423009100002));
#171863=CARTESIAN_POINT('Ctrl Pts',(7.78351769799994,11.6,-6.94423009100002));
#171864=CARTESIAN_POINT('Ctrl Pts',(7.78264368299994,15.2,-6.94320950700002));
#171865=CARTESIAN_POINT('Ctrl Pts',(7.78264368299994,11.6,-6.94320950700002));
#171866=CARTESIAN_POINT('Ctrl Pts',(7.78177420299994,15.2,-6.94219620000001));
#171867=CARTESIAN_POINT('Ctrl Pts',(7.78177420299994,11.6,-6.94219620000001));
#171868=CARTESIAN_POINT('Ctrl Pts',(7.78090928599994,15.2,-6.94119017400002));
#171869=CARTESIAN_POINT('Ctrl Pts',(7.78090928599994,11.6,-6.94119017400002));
#171870=CARTESIAN_POINT('Ctrl Pts',(7.78004895599994,15.2,-6.94019143600002));
#171871=CARTESIAN_POINT('Ctrl Pts',(7.78004895599994,11.6,-6.94019143600002));
#171872=CARTESIAN_POINT('Ctrl Pts',(7.77919324199994,15.2,-6.93919999300002));
#171873=CARTESIAN_POINT('Ctrl Pts',(7.77919324199994,11.6,-6.93919999300002));
#171874=CARTESIAN_POINT('Ctrl Pts',(7.77834216699994,15.2,-6.93821585200002));
#171875=CARTESIAN_POINT('Ctrl Pts',(7.77834216699994,11.6,-6.93821585200002));
#171876=CARTESIAN_POINT('Ctrl Pts',(7.77749575799994,15.2,-6.93723901900002));
#171877=CARTESIAN_POINT('Ctrl Pts',(7.77749575799994,11.6,-6.93723901900002));
#171878=CARTESIAN_POINT('Ctrl Pts',(7.77665404199994,15.2,-6.93626950100001));
#171879=CARTESIAN_POINT('Ctrl Pts',(7.77665404199994,11.6,-6.93626950100001));
#171880=CARTESIAN_POINT('Ctrl Pts',(7.77581704399994,15.2,-6.93530730300001));
#171881=CARTESIAN_POINT('Ctrl Pts',(7.77581704399994,11.6,-6.93530730300001));
#171882=CARTESIAN_POINT('Ctrl Pts',(7.77498479199994,15.2,-6.93435243300002));
#171883=CARTESIAN_POINT('Ctrl Pts',(7.77498479199994,11.6,-6.93435243300002));
#171884=CARTESIAN_POINT('Ctrl Pts',(7.77415731199994,15.2,-6.93340489800002));
#171885=CARTESIAN_POINT('Ctrl Pts',(7.77415731199994,11.6,-6.93340489800002));
#171886=CARTESIAN_POINT('Ctrl Pts',(7.77333463099994,15.2,-6.93246470300001));
#171887=CARTESIAN_POINT('Ctrl Pts',(7.77333463099994,11.6,-6.93246470300001));
#171888=CARTESIAN_POINT('Ctrl Pts',(7.77251677499994,15.2,-6.93153185600002));
#171889=CARTESIAN_POINT('Ctrl Pts',(7.77251677499994,11.6,-6.93153185600002));
#171890=CARTESIAN_POINT('Ctrl Pts',(7.77170377299995,15.2,-6.93060636300002));
#171891=CARTESIAN_POINT('Ctrl Pts',(7.77170377299995,11.6,-6.93060636300002));
#171892=CARTESIAN_POINT('Ctrl Pts',(7.77089564999994,15.2,-6.92968823200002));
#171893=CARTESIAN_POINT('Ctrl Pts',(7.77089564999994,11.6,-6.92968823200002));
#171894=CARTESIAN_POINT('Ctrl Pts',(7.77009243399994,15.2,-6.92877746800002));
#171895=CARTESIAN_POINT('Ctrl Pts',(7.77009243399994,11.6,-6.92877746800002));
#171896=CARTESIAN_POINT('Ctrl Pts',(7.76929415399994,15.2,-6.92787407800001));
#171897=CARTESIAN_POINT('Ctrl Pts',(7.76929415399994,11.6,-6.92787407800001));
#171898=CARTESIAN_POINT('Ctrl Pts',(7.76850083499995,15.2,-6.92697807000001));
#171899=CARTESIAN_POINT('Ctrl Pts',(7.76850083499995,11.6,-6.92697807000001));
#171900=CARTESIAN_POINT('Ctrl Pts',(7.76771250599994,15.2,-6.92608944900002));
#171901=CARTESIAN_POINT('Ctrl Pts',(7.76771250599994,11.6,-6.92608944900002));
#171902=CARTESIAN_POINT('Ctrl Pts',(7.76692919399995,15.2,-6.92520822300001));
#171903=CARTESIAN_POINT('Ctrl Pts',(7.76692919399995,11.6,-6.92520822300001));
#171904=CARTESIAN_POINT('Ctrl Pts',(7.76615092799994,15.2,-6.92433439700002));
#171905=CARTESIAN_POINT('Ctrl Pts',(7.76615092799994,11.6,-6.92433439700002));
#171906=CARTESIAN_POINT('Ctrl Pts',(7.76537773499994,15.2,-6.92346798200001));
#171907=CARTESIAN_POINT('Ctrl Pts',(7.76537773499994,11.6,-6.92346798200001));
#171908=CARTESIAN_POINT('Ctrl Pts',(7.76460964399995,15.2,-6.92260898000002));
#171909=CARTESIAN_POINT('Ctrl Pts',(7.76460964399995,11.6,-6.92260898000002));
#171910=CARTESIAN_POINT('Ctrl Pts',(7.76384668299994,15.2,-6.92175740000001));
#171911=CARTESIAN_POINT('Ctrl Pts',(7.76384668299994,11.6,-6.92175740000001));
#171912=CARTESIAN_POINT('Ctrl Pts',(7.76308887999994,15.2,-6.92091324900002));
#171913=CARTESIAN_POINT('Ctrl Pts',(7.76308887999994,11.6,-6.92091324900002));
#171914=CARTESIAN_POINT('Ctrl Pts',(7.76233626399994,15.2,-6.92007653400001));
#171915=CARTESIAN_POINT('Ctrl Pts',(7.76233626399994,11.6,-6.92007653400001));
#171916=CARTESIAN_POINT('Ctrl Pts',(7.76158886399994,15.2,-6.91924726000002));
#171917=CARTESIAN_POINT('Ctrl Pts',(7.76158886399994,11.6,-6.91924726000002));
#171918=CARTESIAN_POINT('Ctrl Pts',(7.76084670899994,15.2,-6.91842543600002));
#171919=CARTESIAN_POINT('Ctrl Pts',(7.76084670899994,11.6,-6.91842543600002));
#171920=CARTESIAN_POINT('Ctrl Pts',(7.76010982699994,15.2,-6.91761106900002));
#171921=CARTESIAN_POINT('Ctrl Pts',(7.76010982699994,11.6,-6.91761106900002));
#171922=CARTESIAN_POINT('Ctrl Pts',(7.75937824799994,15.2,-6.91680416500001));
#171923=CARTESIAN_POINT('Ctrl Pts',(7.75937824799994,11.6,-6.91680416500001));
#171924=CARTESIAN_POINT('Ctrl Pts',(7.75865200099994,15.2,-6.91600473000002));
#171925=CARTESIAN_POINT('Ctrl Pts',(7.75865200099994,11.6,-6.91600473000002));
#171926=CARTESIAN_POINT('Ctrl Pts',(7.75793111599994,15.2,-6.91521277400001));
#171927=CARTESIAN_POINT('Ctrl Pts',(7.75793111599994,11.6,-6.91521277400001));
#171928=CARTESIAN_POINT('Ctrl Pts',(7.75721561999994,15.2,-6.91442830100002));
#171929=CARTESIAN_POINT('Ctrl Pts',(7.75721561999994,11.6,-6.91442830100002));
#171930=CARTESIAN_POINT('Ctrl Pts',(7.75650554599994,15.2,-6.91365131900002));
#171931=CARTESIAN_POINT('Ctrl Pts',(7.75650554599994,11.6,-6.91365131900002));
#171932=CARTESIAN_POINT('Ctrl Pts',(7.75580092299994,15.2,-6.91288183500002));
#171933=CARTESIAN_POINT('Ctrl Pts',(7.75580092299994,11.6,-6.91288183500002));
#171934=CARTESIAN_POINT('Ctrl Pts',(7.75510177999994,15.2,-6.91211985800001));
#171935=CARTESIAN_POINT('Ctrl Pts',(7.75510177999994,11.6,-6.91211985800001));
#171936=CARTESIAN_POINT('Ctrl Pts',(7.75440814899994,15.2,-6.91136539200001));
#171937=CARTESIAN_POINT('Ctrl Pts',(7.75440814899994,11.6,-6.91136539200001));
#171938=CARTESIAN_POINT('Ctrl Pts',(7.75372005699994,15.2,-6.91061844600001));
#171939=CARTESIAN_POINT('Ctrl Pts',(7.75372005699994,11.6,-6.91061844600001));
#171940=CARTESIAN_POINT('Ctrl Pts',(7.75303753799994,15.2,-6.90987902600002));
#171941=CARTESIAN_POINT('Ctrl Pts',(7.75303753799994,11.6,-6.90987902600002));
#171942=CARTESIAN_POINT('Ctrl Pts',(7.75236061999995,15.2,-6.90914714000002));
#171943=CARTESIAN_POINT('Ctrl Pts',(7.75236061999995,11.6,-6.90914714000002));
#171944=CARTESIAN_POINT('Ctrl Pts',(7.75168933499994,15.2,-6.90842279600002));
#171945=CARTESIAN_POINT('Ctrl Pts',(7.75168933499994,11.6,-6.90842279600002));
#171946=CARTESIAN_POINT('Ctrl Pts',(7.75102371399995,15.2,-6.90770599900001));
#171947=CARTESIAN_POINT('Ctrl Pts',(7.75102371399995,11.6,-6.90770599900001));
#171948=CARTESIAN_POINT('Ctrl Pts',(7.75036378799994,15.2,-6.90699675800002));
#171949=CARTESIAN_POINT('Ctrl Pts',(7.75036378799994,11.6,-6.90699675800002));
#171950=CARTESIAN_POINT('Ctrl Pts',(7.74970958799994,15.2,-6.90629507900002));
#171951=CARTESIAN_POINT('Ctrl Pts',(7.74970958799994,11.6,-6.90629507900002));
#171952=CARTESIAN_POINT('Ctrl Pts',(7.74906114399994,15.2,-6.90560097000001));
#171953=CARTESIAN_POINT('Ctrl Pts',(7.74906114399994,11.6,-6.90560097000001));
#171954=CARTESIAN_POINT('Ctrl Pts',(7.74841849099994,15.2,-6.90491443800001));
#171955=CARTESIAN_POINT('Ctrl Pts',(7.74841849099994,11.6,-6.90491443800001));
#171956=CARTESIAN_POINT('Ctrl Pts',(7.74778165799995,15.2,-6.90423549000001));
#171957=CARTESIAN_POINT('Ctrl Pts',(7.74778165799995,11.6,-6.90423549000001));
#171958=CARTESIAN_POINT('Ctrl Pts',(7.74715431199994,15.2,-6.90356800200002));
#171959=CARTESIAN_POINT('Ctrl Pts',(7.74715431199994,11.6,-6.90356800200002));
#171960=CARTESIAN_POINT('Ctrl Pts',(7.74665780199994,15.2,-6.90304077600001));
#171961=CARTESIAN_POINT('Ctrl Pts',(7.74665780199994,11.6,-6.90304077600001));
#171962=CARTESIAN_POINT('Ctrl Pts',(7.74628892999995,15.2,-6.90264967000001));
#171963=CARTESIAN_POINT('Ctrl Pts',(7.74628892999995,11.6,-6.90264967000001));
#171964=CARTESIAN_POINT('Ctrl Pts',(7.74604536199995,15.2,-6.90239167400001));
#171965=CARTESIAN_POINT('Ctrl Pts',(7.74604536199995,11.6,-6.90239167400001));
#171966=CARTESIAN_POINT('Ctrl Pts',(7.74592563699994,15.2,-6.90226492000001));
#171967=CARTESIAN_POINT('Ctrl Pts',(7.74592563699994,11.6,-6.90226492000001));
#171968=CARTESIAN_POINT('',(7.74592563699994,12.2,-6.90226492000001));
#171969=CARTESIAN_POINT('',(7.74592563699994,15.2,-6.90226492000001));
#171970=CARTESIAN_POINT('',(7.74592563699994,12.2,-6.90226492000001));
#171971=CARTESIAN_POINT('Ctrl Pts',(8.32310290799994,12.2,-7.93573928300002));
#171972=CARTESIAN_POINT('Ctrl Pts',(8.32283676099994,12.2,-7.93502251600002));
#171973=CARTESIAN_POINT('Ctrl Pts',(8.32230434799994,12.2,-7.93358949600002));
#171974=CARTESIAN_POINT('Ctrl Pts',(8.32150538099994,12.2,-7.93144150700002));
#171975=CARTESIAN_POINT('Ctrl Pts',(8.32043939299994,12.2,-7.92858060400001));
#171976=CARTESIAN_POINT('Ctrl Pts',(8.31910574599994,12.2,-7.92500961100002));
#171977=CARTESIAN_POINT('Ctrl Pts',(8.31777093699994,12.2,-7.92144375600002));
#171978=CARTESIAN_POINT('Ctrl Pts',(8.31643496899994,12.2,-7.91788304100002));
#171979=CARTESIAN_POINT('Ctrl Pts',(8.31509784399995,12.2,-7.91432746600002));
#171980=CARTESIAN_POINT('Ctrl Pts',(8.31375956699994,12.2,-7.91077703500001));
#171981=CARTESIAN_POINT('Ctrl Pts',(8.31242014699994,12.2,-7.90723175400001));
#171982=CARTESIAN_POINT('Ctrl Pts',(8.31107958999995,12.2,-7.90369162500002));
#171983=CARTESIAN_POINT('Ctrl Pts',(8.30973790699994,12.2,-7.90015665600002));
#171984=CARTESIAN_POINT('Ctrl Pts',(8.30812654585849,12.2,-7.89592089135391));
#171985=CARTESIAN_POINT('Ctrl Pts',(8.30651352407067,12.2,-7.89169288132307));
#171986=CARTESIAN_POINT('Ctrl Pts',(8.30489885992922,12.2,-7.88747263667696));
#171987=CARTESIAN_POINT('Ctrl Pts',(8.3032825651414,12.2,-7.88326016964612));
#171988=CARTESIAN_POINT('Ctrl Pts',(8.30166465799994,12.2,-7.87905548500002));
#171989=CARTESIAN_POINT('Ctrl Pts',(8.30031533299995,12.2,-7.87555677500002));
#171990=CARTESIAN_POINT('Ctrl Pts',(8.29896494599994,12.2,-7.87206326300002));
#171991=CARTESIAN_POINT('Ctrl Pts',(8.29761350399994,12.2,-7.86857495200002));
#171992=CARTESIAN_POINT('Ctrl Pts',(8.29626101599995,12.2,-7.86509184700002));
#171993=CARTESIAN_POINT('Ctrl Pts',(8.29490748799994,12.2,-7.86161395500002));
#171994=CARTESIAN_POINT('Ctrl Pts',(8.29355293099994,12.2,-7.85814127700001));
#171995=CARTESIAN_POINT('Ctrl Pts',(8.29219734999995,12.2,-7.85467382100002));
#171996=CARTESIAN_POINT('Ctrl Pts',(8.29084075499994,12.2,-7.85121159100001));
#171997=CARTESIAN_POINT('Ctrl Pts',(8.28948315499994,12.2,-7.84775459000001));
#171998=CARTESIAN_POINT('Ctrl Pts',(8.28812455599994,12.2,-7.84430282500002));
#171999=CARTESIAN_POINT('Ctrl Pts',(8.28676496699994,12.2,-7.84085630000002));
#172000=CARTESIAN_POINT('Ctrl Pts',(8.28540439599994,12.2,-7.83741501800002));
#172001=CARTESIAN_POINT('Ctrl Pts',(8.28404284999994,12.2,-7.83397898500001));
#172002=CARTESIAN_POINT('Ctrl Pts',(8.28268033699995,12.2,-7.83054820600002));
#172003=CARTESIAN_POINT('Ctrl Pts',(8.28131686599994,12.2,-7.82712268400001));
#172004=CARTESIAN_POINT('Ctrl Pts',(8.27995244399995,12.2,-7.82370242500001));
#172005=CARTESIAN_POINT('Ctrl Pts',(8.27858707899994,12.2,-7.82028743300001));
#172006=CARTESIAN_POINT('Ctrl Pts',(8.27722078099994,12.2,-7.81687771200002));
#172007=CARTESIAN_POINT('Ctrl Pts',(8.27585355599994,12.2,-7.81347326900002));
#172008=CARTESIAN_POINT('Ctrl Pts',(8.27448541299994,12.2,-7.81007410700001));
#172009=CARTESIAN_POINT('Ctrl Pts',(8.27311635999994,12.2,-7.80668023000001));
#172010=CARTESIAN_POINT('Ctrl Pts',(8.27174640499994,12.2,-7.80329164300002));
#172011=CARTESIAN_POINT('Ctrl Pts',(8.27037555599994,12.2,-7.79990835200002));
#172012=CARTESIAN_POINT('Ctrl Pts',(8.26900382399994,12.2,-7.79653036100001));
#172013=CARTESIAN_POINT('Ctrl Pts',(8.26763121199994,12.2,-7.79315767400002));
#172014=CARTESIAN_POINT('Ctrl Pts',(8.26625773199994,12.2,-7.78979029600002));
#172015=CARTESIAN_POINT('Ctrl Pts',(8.26488339199994,12.2,-7.78642823100002));
#172016=CARTESIAN_POINT('Ctrl Pts',(8.26350819799995,12.2,-7.78307148500001));
#172017=CARTESIAN_POINT('Ctrl Pts',(8.26213216099994,12.2,-7.77972006200002));
#172018=CARTESIAN_POINT('Ctrl Pts',(8.26075528799995,12.2,-7.77637396700002));
#172019=CARTESIAN_POINT('Ctrl Pts',(8.25937758699994,12.2,-7.77303320300001));
#172020=CARTESIAN_POINT('Ctrl Pts',(8.25799906799995,12.2,-7.76969777700002));
#172021=CARTESIAN_POINT('Ctrl Pts',(8.25661973699994,12.2,-7.76636769200002));
#172022=CARTESIAN_POINT('Ctrl Pts',(8.25523960299994,12.2,-7.76304295400001));
#172023=CARTESIAN_POINT('Ctrl Pts',(8.25385867499994,12.2,-7.75972356600001));
#172024=CARTESIAN_POINT('Ctrl Pts',(8.25247696199994,12.2,-7.75640953400002));
#172025=CARTESIAN_POINT('Ctrl Pts',(8.25109447199995,12.2,-7.75310086400002));
#172026=CARTESIAN_POINT('Ctrl Pts',(8.24971121199994,12.2,-7.74979755600001));
#172027=CARTESIAN_POINT('Ctrl Pts',(8.24832719199994,12.2,-7.74649962000002));
#172028=CARTESIAN_POINT('Ctrl Pts',(8.24694242099994,12.2,-7.74320705700001));
#172029=CARTESIAN_POINT('Ctrl Pts',(8.24555690699994,12.2,-7.73991987300001));
#172030=CARTESIAN_POINT('Ctrl Pts',(8.24417065699994,12.2,-7.73663807300002));
#172031=CARTESIAN_POINT('Ctrl Pts',(8.24278367999994,12.2,-7.73336166100002));
#172032=CARTESIAN_POINT('Ctrl Pts',(8.24139598699994,12.2,-7.73009064300001));
#172033=CARTESIAN_POINT('Ctrl Pts',(8.24000758299994,12.2,-7.72682502200002));
#172034=CARTESIAN_POINT('Ctrl Pts',(8.23861848099994,12.2,-7.72356480200001));
#172035=CARTESIAN_POINT('Ctrl Pts',(8.23722868599994,12.2,-7.72030999100001));
#172036=CARTESIAN_POINT('Ctrl Pts',(8.23583820599995,12.2,-7.71706059100002));
#172037=CARTESIAN_POINT('Ctrl Pts',(8.23444705399995,12.2,-7.71381660700002));
#172038=CARTESIAN_POINT('Ctrl Pts',(8.23305523399994,12.2,-7.71057804500002));
#172039=CARTESIAN_POINT('Ctrl Pts',(8.23166275799995,12.2,-7.70734490700002));
#172040=CARTESIAN_POINT('Ctrl Pts',(8.23026963299995,12.2,-7.70411720200002));
#172041=CARTESIAN_POINT('Ctrl Pts',(8.22887586899994,12.2,-7.70089492900001));
#172042=CARTESIAN_POINT('Ctrl Pts',(8.22748147299994,12.2,-7.69767809800002));
#172043=CARTESIAN_POINT('Ctrl Pts',(8.22608645599994,12.2,-7.69446671100001));
#172044=CARTESIAN_POINT('Ctrl Pts',(8.22469082399994,12.2,-7.69126077300001));
#172045=CARTESIAN_POINT('Ctrl Pts',(8.22329458799994,12.2,-7.68806029000002));
#172046=CARTESIAN_POINT('Ctrl Pts',(8.22189775699995,12.2,-7.68486526400002));
#172047=CARTESIAN_POINT('Ctrl Pts',(8.22050033799994,12.2,-7.68167570200001));
#172048=CARTESIAN_POINT('Ctrl Pts',(8.21910234199994,12.2,-7.67849160900001));
#172049=CARTESIAN_POINT('Ctrl Pts',(8.21770377699995,12.2,-7.67531298700002));
#172050=CARTESIAN_POINT('Ctrl Pts',(8.21630465099994,12.2,-7.67213984300002));
#172051=CARTESIAN_POINT('Ctrl Pts',(8.21490497299994,12.2,-7.66897218200001));
#172052=CARTESIAN_POINT('Ctrl Pts',(8.21350475399995,12.2,-7.66581000700001));
#172053=CARTESIAN_POINT('Ctrl Pts',(8.21210400199995,12.2,-7.66265332400001));
#172054=CARTESIAN_POINT('Ctrl Pts',(8.21070272499994,12.2,-7.65950213700001));
#172055=CARTESIAN_POINT('Ctrl Pts',(8.20930093299994,12.2,-7.65635645100001));
#172056=CARTESIAN_POINT('Ctrl Pts',(8.20789863399994,12.2,-7.65321627000001));
#172057=CARTESIAN_POINT('Ctrl Pts',(8.20649583899994,12.2,-7.65008160000002));
#172058=CARTESIAN_POINT('Ctrl Pts',(8.20509255499994,12.2,-7.64695244500002));
#172059=CARTESIAN_POINT('Ctrl Pts',(8.20368879299994,12.2,-7.64382880900002));
#172060=CARTESIAN_POINT('Ctrl Pts',(8.20228455999995,12.2,-7.64071069900002));
#172061=CARTESIAN_POINT('Ctrl Pts',(8.20087986699994,12.2,-7.63759811700002));
#172062=CARTESIAN_POINT('Ctrl Pts',(8.19947472199994,12.2,-7.63449107000002));
#172063=CARTESIAN_POINT('Ctrl Pts',(8.19806913599994,12.2,-7.63138956100001));
#172064=CARTESIAN_POINT('Ctrl Pts',(8.19666311599994,12.2,-7.62829359600002));
#172065=CARTESIAN_POINT('Ctrl Pts',(8.19525667099994,12.2,-7.62520317900002));
#172066=CARTESIAN_POINT('Ctrl Pts',(8.19384981299994,12.2,-7.62211831500001));
#172067=CARTESIAN_POINT('Ctrl Pts',(8.19244254899994,12.2,-7.61903900800001));
#172068=CARTESIAN_POINT('Ctrl Pts',(8.19103488899994,12.2,-7.61596526400002));
#172069=CARTESIAN_POINT('Ctrl Pts',(8.18962684199994,12.2,-7.61289708700001));
#172070=CARTESIAN_POINT('Ctrl Pts',(8.18821841799994,12.2,-7.60983448100002));
#172071=CARTESIAN_POINT('Ctrl Pts',(8.18680962599995,12.2,-7.60677745200002));
#172072=CARTESIAN_POINT('Ctrl Pts',(8.18540047699994,12.2,-7.60372600500002));
#172073=CARTESIAN_POINT('Ctrl Pts',(8.18399097599994,12.2,-7.60068014400002));
#172074=CARTESIAN_POINT('Ctrl Pts',(8.18258113699994,12.2,-7.59763987300002));
#172075=CARTESIAN_POINT('Ctrl Pts',(8.18117096699994,12.2,-7.59460519700002));
#172076=CARTESIAN_POINT('Ctrl Pts',(8.17976047699995,12.2,-7.59157612300001));
#172077=CARTESIAN_POINT('Ctrl Pts',(8.17834967399994,12.2,-7.58855265300002));
#172078=CARTESIAN_POINT('Ctrl Pts',(8.17693857099994,12.2,-7.58553479300001));
#172079=CARTESIAN_POINT('Ctrl Pts',(8.17552717499994,12.2,-7.58252254800002));
#172080=CARTESIAN_POINT('Ctrl Pts',(8.17411549699994,12.2,-7.57951592200002));
#172081=CARTESIAN_POINT('Ctrl Pts',(8.17270354399994,12.2,-7.57651491900001));
#172082=CARTESIAN_POINT('Ctrl Pts',(8.17129132899994,12.2,-7.57351954600002));
#172083=CARTESIAN_POINT('Ctrl Pts',(8.16987885999995,12.2,-7.57052980700001));
#172084=CARTESIAN_POINT('Ctrl Pts',(8.16846614699994,12.2,-7.56754570500001));
#172085=CARTESIAN_POINT('Ctrl Pts',(8.16705319899994,12.2,-7.56456724700002));
#172086=CARTESIAN_POINT('Ctrl Pts',(8.16564002699995,12.2,-7.56159443600002));
#172087=CARTESIAN_POINT('Ctrl Pts',(8.16422663899995,12.2,-7.55862727900002));
#172088=CARTESIAN_POINT('Ctrl Pts',(8.16281304699995,12.2,-7.55566577800002));
#172089=CARTESIAN_POINT('Ctrl Pts',(8.16139925799994,12.2,-7.55270994000002));
#172090=CARTESIAN_POINT('Ctrl Pts',(8.15998528399994,12.2,-7.54975976900001));
#172091=CARTESIAN_POINT('Ctrl Pts',(8.15857113399994,12.2,-7.54681526900002));
#172092=CARTESIAN_POINT('Ctrl Pts',(8.15715681899994,12.2,-7.54387644600002));
#172093=CARTESIAN_POINT('Ctrl Pts',(8.15574234599995,12.2,-7.54094330400001));
#172094=CARTESIAN_POINT('Ctrl Pts',(8.15432772699995,12.2,-7.53801584800001));
#172095=CARTESIAN_POINT('Ctrl Pts',(8.15291297199994,12.2,-7.53509408200002));
#172096=CARTESIAN_POINT('Ctrl Pts',(8.15149809099994,12.2,-7.53217801400002));
#172097=CARTESIAN_POINT('Ctrl Pts',(8.15008309399994,12.2,-7.52926764500002));
#172098=CARTESIAN_POINT('Ctrl Pts',(8.14866798999994,12.2,-7.52636298000001));
#172099=CARTESIAN_POINT('Ctrl Pts',(8.14725278899994,12.2,-7.52346402700002));
#172100=CARTESIAN_POINT('Ctrl Pts',(8.14583750199994,12.2,-7.52057078700001));
#172101=CARTESIAN_POINT('Ctrl Pts',(8.14442213799994,12.2,-7.51768326800001));
#172102=CARTESIAN_POINT('Ctrl Pts',(8.14300670799994,12.2,-7.51480147300001));
#172103=CARTESIAN_POINT('Ctrl Pts',(8.14159122299994,12.2,-7.51192540700002));
#172104=CARTESIAN_POINT('Ctrl Pts',(8.14017569099994,12.2,-7.50905507500002));
#172105=CARTESIAN_POINT('Ctrl Pts',(8.13876012299995,12.2,-7.50619048100001));
#172106=CARTESIAN_POINT('Ctrl Pts',(8.13734453099995,12.2,-7.50333163200001));
#172107=CARTESIAN_POINT('Ctrl Pts',(8.13592892199994,12.2,-7.50047853100002));
#172108=CARTESIAN_POINT('Ctrl Pts',(8.13423018390736,12.2,-7.4970617120138));
#172109=CARTESIAN_POINT('Ctrl Pts',(8.13253145646908,12.2,-7.49365353183833));
#172110=CARTESIAN_POINT('Ctrl Pts',(8.1308327555308,12.2,-7.4902539981617));
#172111=CARTESIAN_POINT('Ctrl Pts',(8.12913410293822,12.2,-7.48686311867665));
#172112=CARTESIAN_POINT('Ctrl Pts',(8.12743552099995,12.2,-7.48348090800001));
#172113=CARTESIAN_POINT('Ctrl Pts',(8.12602009199994,12.2,-7.48066818000002));
#172114=CARTESIAN_POINT('Ctrl Pts',(8.12460473099994,12.2,-7.47786123800001));
#172115=CARTESIAN_POINT('Ctrl Pts',(8.12318944699994,12.2,-7.47506008900002));
#172116=CARTESIAN_POINT('Ctrl Pts',(8.12177425199994,12.2,-7.47226473600002));
#172117=CARTESIAN_POINT('Ctrl Pts',(8.12035915499994,12.2,-7.46947518500002));
#172118=CARTESIAN_POINT('Ctrl Pts',(8.11894416699994,12.2,-7.46669144000002));
#172119=CARTESIAN_POINT('Ctrl Pts',(8.11752929899994,12.2,-7.46391350600002));
#172120=CARTESIAN_POINT('Ctrl Pts',(8.11611456099994,12.2,-7.46114138700002));
#172121=CARTESIAN_POINT('Ctrl Pts',(8.11469996399994,12.2,-7.45837509000002));
#172122=CARTESIAN_POINT('Ctrl Pts',(8.11328551799994,12.2,-7.45561461800002));
#172123=CARTESIAN_POINT('Ctrl Pts',(8.11187123599994,12.2,-7.45285997600002));
#172124=CARTESIAN_POINT('Ctrl Pts',(8.11045712499994,12.2,-7.45011117000002));
#172125=CARTESIAN_POINT('Ctrl Pts',(8.10904319799995,12.2,-7.44736820300002));
#172126=CARTESIAN_POINT('Ctrl Pts',(8.10762946499995,12.2,-7.44463108200001));
#172127=CARTESIAN_POINT('Ctrl Pts',(8.10621593799994,12.2,-7.44189981000002));
#172128=CARTESIAN_POINT('Ctrl Pts',(8.10480262699994,12.2,-7.43917439400001));
#172129=CARTESIAN_POINT('Ctrl Pts',(8.10338954199995,12.2,-7.43645483600002));
#172130=CARTESIAN_POINT('Ctrl Pts',(8.10197669399994,12.2,-7.43374114300002));
#172131=CARTESIAN_POINT('Ctrl Pts',(8.10056409499994,12.2,-7.43103331900001));
#172132=CARTESIAN_POINT('Ctrl Pts',(8.09915175599994,12.2,-7.42833136900002));
#172133=CARTESIAN_POINT('Ctrl Pts',(8.09773968599995,12.2,-7.42563529800002));
#172134=CARTESIAN_POINT('Ctrl Pts',(8.09632789799995,12.2,-7.42294511100001));
#172135=CARTESIAN_POINT('Ctrl Pts',(8.09491640099994,12.2,-7.42026081400001));
#172136=CARTESIAN_POINT('Ctrl Pts',(8.09350520799994,12.2,-7.41758240800002));
#172137=CARTESIAN_POINT('Ctrl Pts',(8.09209432999995,12.2,-7.41490990200001));
#172138=CARTESIAN_POINT('Ctrl Pts',(8.09068377599995,12.2,-7.41224329900002));
#172139=CARTESIAN_POINT('Ctrl Pts',(8.08927355799994,12.2,-7.40958260500002));
#172140=CARTESIAN_POINT('Ctrl Pts',(8.08786368899994,12.2,-7.40692782200002));
#172141=CARTESIAN_POINT('Ctrl Pts',(8.08645417899994,12.2,-7.40427895900002));
#172142=CARTESIAN_POINT('Ctrl Pts',(8.08504503799995,12.2,-7.40163601800001));
#172143=CARTESIAN_POINT('Ctrl Pts',(8.08363627799995,12.2,-7.39899900500002));
#172144=CARTESIAN_POINT('Ctrl Pts',(8.08222790999995,12.2,-7.39636792500002));
#172145=CARTESIAN_POINT('Ctrl Pts',(8.08081994599995,12.2,-7.39374278100002));
#172146=CARTESIAN_POINT('Ctrl Pts',(8.07941239799994,12.2,-7.39112358100002));
#172147=CARTESIAN_POINT('Ctrl Pts',(8.07800527499994,12.2,-7.38851032800002));
#172148=CARTESIAN_POINT('Ctrl Pts',(8.07659858999994,12.2,-7.38590302700001));
#172149=CARTESIAN_POINT('Ctrl Pts',(8.07519235299995,12.2,-7.38330168300001));
#172150=CARTESIAN_POINT('Ctrl Pts',(8.07378657799994,12.2,-7.38070630100002));
#172151=CARTESIAN_POINT('Ctrl Pts',(8.07238127399994,12.2,-7.37811688600001));
#172152=CARTESIAN_POINT('Ctrl Pts',(8.07097645399995,12.2,-7.37553344300002));
#172153=CARTESIAN_POINT('Ctrl Pts',(8.06957212799994,12.2,-7.37295597700002));
#172154=CARTESIAN_POINT('Ctrl Pts',(8.06816830899994,12.2,-7.37038449300002));
#172155=CARTESIAN_POINT('Ctrl Pts',(8.06676500799994,12.2,-7.36781899400002));
#172156=CARTESIAN_POINT('Ctrl Pts',(8.06536223699995,12.2,-7.36525948800002));
#172157=CARTESIAN_POINT('Ctrl Pts',(8.06396000599995,12.2,-7.36270597800001));
#172158=CARTESIAN_POINT('Ctrl Pts',(8.06255832899994,12.2,-7.36015847000001));
#172159=CARTESIAN_POINT('Ctrl Pts',(8.06115721599994,12.2,-7.35761696800001));
#172160=CARTESIAN_POINT('Ctrl Pts',(8.05975667999994,12.2,-7.35508147600001));
#172161=CARTESIAN_POINT('Ctrl Pts',(8.05835673199994,12.2,-7.35255200200001));
#172162=CARTESIAN_POINT('Ctrl Pts',(8.05695738399994,12.2,-7.35002854800002));
#172163=CARTESIAN_POINT('Ctrl Pts',(8.05555864699994,12.2,-7.34751112100002));
#172164=CARTESIAN_POINT('Ctrl Pts',(8.05416053399994,12.2,-7.34499972400001));
#172165=CARTESIAN_POINT('Ctrl Pts',(8.05276305599994,12.2,-7.34249436400002));
#172166=CARTESIAN_POINT('Ctrl Pts',(8.05136622599994,12.2,-7.33999504400002));
#172167=CARTESIAN_POINT('Ctrl Pts',(8.04997005499994,12.2,-7.33750177000001));
#172168=CARTESIAN_POINT('Ctrl Pts',(8.04857455599995,12.2,-7.33501454700002));
#172169=CARTESIAN_POINT('Ctrl Pts',(8.04717973999994,12.2,-7.33253338100001));
#172170=CARTESIAN_POINT('Ctrl Pts',(8.04578561899995,12.2,-7.33005827400002));
#172171=CARTESIAN_POINT('Ctrl Pts',(8.04439220499994,12.2,-7.32758923400001));
#172172=CARTESIAN_POINT('Ctrl Pts',(8.04299951199994,12.2,-7.32512626400001));
#172173=CARTESIAN_POINT('Ctrl Pts',(8.04160754999995,12.2,-7.32266936900002));
#172174=CARTESIAN_POINT('Ctrl Pts',(8.04021633199994,12.2,-7.32021855600002));
#172175=CARTESIAN_POINT('Ctrl Pts',(8.03882586899995,12.2,-7.31777382800002));
#172176=CARTESIAN_POINT('Ctrl Pts',(8.03743617699994,12.2,-7.31533519100001));
#172177=CARTESIAN_POINT('Ctrl Pts',(8.03604726399995,12.2,-7.31290264900001));
#172178=CARTESIAN_POINT('Ctrl Pts',(8.03465914399995,12.2,-7.31047620700001));
#172179=CARTESIAN_POINT('Ctrl Pts',(8.03327182899995,12.2,-7.30805587200001));
#172180=CARTESIAN_POINT('Ctrl Pts',(8.03188533199994,12.2,-7.30564164600001));
#172181=CARTESIAN_POINT('Ctrl Pts',(8.03049966599995,12.2,-7.30323353700002));
#172182=CARTESIAN_POINT('Ctrl Pts',(8.02911484199995,12.2,-7.30083154700001));
#172183=CARTESIAN_POINT('Ctrl Pts',(8.02773087299994,12.2,-7.29843568400002));
#172184=CARTESIAN_POINT('Ctrl Pts',(8.02634777099994,12.2,-7.29604595200002));
#172185=CARTESIAN_POINT('Ctrl Pts',(8.02496554899994,12.2,-7.29366235400001));
#172186=CARTESIAN_POINT('Ctrl Pts',(8.02358422099994,12.2,-7.29128489700001));
#172187=CARTESIAN_POINT('Ctrl Pts',(8.02220379799994,12.2,-7.28891358600002));
#172188=CARTESIAN_POINT('Ctrl Pts',(8.02082429299994,12.2,-7.28654842400001));
#172189=CARTESIAN_POINT('Ctrl Pts',(8.01944571799994,12.2,-7.28418941900002));
#172190=CARTESIAN_POINT('Ctrl Pts',(8.01806808699994,12.2,-7.28183657500002));
#172191=CARTESIAN_POINT('Ctrl Pts',(8.01669141199995,12.2,-7.27948989700002));
#172192=CARTESIAN_POINT('Ctrl Pts',(8.01531570699994,12.2,-7.27714938900001));
#172193=CARTESIAN_POINT('Ctrl Pts',(8.01394098199994,12.2,-7.27481505600001));
#172194=CARTESIAN_POINT('Ctrl Pts',(8.01256725299995,12.2,-7.27248690400002));
#172195=CARTESIAN_POINT('Ctrl Pts',(8.01119453199994,12.2,-7.27016493800001));
#172196=CARTESIAN_POINT('Ctrl Pts',(8.00982282999994,12.2,-7.26784916400002));
#172197=CARTESIAN_POINT('Ctrl Pts',(8.00845216399994,12.2,-7.26553958500002));
#172198=CARTESIAN_POINT('Ctrl Pts',(8.00708254199994,12.2,-7.26323620600001));
#172199=CARTESIAN_POINT('Ctrl Pts',(8.00571398099994,12.2,-7.26093903400002));
#172200=CARTESIAN_POINT('Ctrl Pts',(8.00434649299994,12.2,-7.25864807300002));
#172201=CARTESIAN_POINT('Ctrl Pts',(8.00298009099994,12.2,-7.25636332800002));
#172202=CARTESIAN_POINT('Ctrl Pts',(8.00161478799994,12.2,-7.25408480400001));
#172203=CARTESIAN_POINT('Ctrl Pts',(8.00025059599994,12.2,-7.25181250700001));
#172204=CARTESIAN_POINT('Ctrl Pts',(7.99888753099995,12.2,-7.24954644100002));
#172205=CARTESIAN_POINT('Ctrl Pts',(7.99752560499994,12.2,-7.24728661100002));
#172206=CARTESIAN_POINT('Ctrl Pts',(7.99616483099994,12.2,-7.24503302300001));
#172207=CARTESIAN_POINT('Ctrl Pts',(7.99480522199994,12.2,-7.24278568000001));
#172208=CARTESIAN_POINT('Ctrl Pts',(7.99344679099995,12.2,-7.24054459100002));
#172209=CARTESIAN_POINT('Ctrl Pts',(7.99208955399994,12.2,-7.23830975700002));
#172210=CARTESIAN_POINT('Ctrl Pts',(7.99073352199994,12.2,-7.23608118600002));
#172211=CARTESIAN_POINT('Ctrl Pts',(7.98937870999994,12.2,-7.23385888200001));
#172212=CARTESIAN_POINT('Ctrl Pts',(7.98802512999995,12.2,-7.23164284900002));
#172213=CARTESIAN_POINT('Ctrl Pts',(7.98667279799994,12.2,-7.22943309400002));
#172214=CARTESIAN_POINT('Ctrl Pts',(7.98532172499994,12.2,-7.22722962000002));
#172215=CARTESIAN_POINT('Ctrl Pts',(7.98397192599994,12.2,-7.22503243400002));
#172216=CARTESIAN_POINT('Ctrl Pts',(7.98262341399994,12.2,-7.22284154100001));
#172217=CARTESIAN_POINT('Ctrl Pts',(7.98127620499994,12.2,-7.22065694600002));
#172218=CARTESIAN_POINT('Ctrl Pts',(7.97993030999994,12.2,-7.21847865300001));
#172219=CARTESIAN_POINT('Ctrl Pts',(7.97858574299994,12.2,-7.21630666700002));
#172220=CARTESIAN_POINT('Ctrl Pts',(7.97724252099994,12.2,-7.21414099500001));
#172221=CARTESIAN_POINT('Ctrl Pts',(7.97590065499994,12.2,-7.21198164000001));
#172222=CARTESIAN_POINT('Ctrl Pts',(7.97456015899995,12.2,-7.20982861000002));
#172223=CARTESIAN_POINT('Ctrl Pts',(7.97322104799994,12.2,-7.20768190700002));
#172224=CARTESIAN_POINT('Ctrl Pts',(7.97188333599994,12.2,-7.20554153800002));
#172225=CARTESIAN_POINT('Ctrl Pts',(7.97054703699994,12.2,-7.20340750800001));
#172226=CARTESIAN_POINT('Ctrl Pts',(7.96921216599995,12.2,-7.20127982100002));
#172227=CARTESIAN_POINT('Ctrl Pts',(7.96787873499994,12.2,-7.19915848400002));
#172228=CARTESIAN_POINT('Ctrl Pts',(7.96654675899994,12.2,-7.19704350100002));
#172229=CARTESIAN_POINT('Ctrl Pts',(7.96521625299994,12.2,-7.19493487700002));
#172230=CARTESIAN_POINT('Ctrl Pts',(7.96388723099994,12.2,-7.19283261800002));
#172231=CARTESIAN_POINT('Ctrl Pts',(7.96255970799994,12.2,-7.19073672800001));
#172232=CARTESIAN_POINT('Ctrl Pts',(7.96123369799994,12.2,-7.18864721300001));
#172233=CARTESIAN_POINT('Ctrl Pts',(7.95990921399994,12.2,-7.18656407900002));
#172234=CARTESIAN_POINT('Ctrl Pts',(7.95858627199994,12.2,-7.18448732900002));
#172235=CARTESIAN_POINT('Ctrl Pts',(7.95726488599994,12.2,-7.18241697000002));
#172236=CARTESIAN_POINT('Ctrl Pts',(7.95594507099994,12.2,-7.18035300600001));
#172237=CARTESIAN_POINT('Ctrl Pts',(7.95462684099994,12.2,-7.17829544400002));
#172238=CARTESIAN_POINT('Ctrl Pts',(7.95331021099994,12.2,-7.17624428700002));
#172239=CARTESIAN_POINT('Ctrl Pts',(7.95199519599994,12.2,-7.17419954200002));
#172240=CARTESIAN_POINT('Ctrl Pts',(7.95068181099994,12.2,-7.17216121300002));
#172241=CARTESIAN_POINT('Ctrl Pts',(7.94937006899994,12.2,-7.17012930500001));
#172242=CARTESIAN_POINT('Ctrl Pts',(7.94805998699994,12.2,-7.16810382500002));
#172243=CARTESIAN_POINT('Ctrl Pts',(7.94675157799994,12.2,-7.16608477700002));
#172244=CARTESIAN_POINT('Ctrl Pts',(7.94544485899995,12.2,-7.16407216700001));
#172245=CARTESIAN_POINT('Ctrl Pts',(7.94413984299994,12.2,-7.16206599900002));
#172246=CARTESIAN_POINT('Ctrl Pts',(7.94283654599995,12.2,-7.16006627800001));
#172247=CARTESIAN_POINT('Ctrl Pts',(7.94153498399995,12.2,-7.15807301100002));
#172248=CARTESIAN_POINT('Ctrl Pts',(7.94023516999995,12.2,-7.15608620200002));
#172249=CARTESIAN_POINT('Ctrl Pts',(7.93893712099995,12.2,-7.15410585600001));
#172250=CARTESIAN_POINT('Ctrl Pts',(7.93764085099995,12.2,-7.15213198100002));
#172251=CARTESIAN_POINT('Ctrl Pts',(7.93634637499995,12.2,-7.15016457800001));
#172252=CARTESIAN_POINT('Ctrl Pts',(7.93505370999994,12.2,-7.14820365600002));
#172253=CARTESIAN_POINT('Ctrl Pts',(7.93376286999995,12.2,-7.14624921800001));
#172254=CARTESIAN_POINT('Ctrl Pts',(7.93247387099994,12.2,-7.14430127000002));
#172255=CARTESIAN_POINT('Ctrl Pts',(7.93118672799995,12.2,-7.14235981700002));
#172256=CARTESIAN_POINT('Ctrl Pts',(7.92990145699994,12.2,-7.14042486500002));
#172257=CARTESIAN_POINT('Ctrl Pts',(7.92861807299994,12.2,-7.13849641800002));
#172258=CARTESIAN_POINT('Ctrl Pts',(7.92733659099994,12.2,-7.13657448300002));
#172259=CARTESIAN_POINT('Ctrl Pts',(7.92605702899994,12.2,-7.13465906400002));
#172260=CARTESIAN_POINT('Ctrl Pts',(7.92477940099995,12.2,-7.13275016800001));
#172261=CARTESIAN_POINT('Ctrl Pts',(7.92350372299994,12.2,-7.13084779800001));
#172262=CARTESIAN_POINT('Ctrl Pts',(7.92223000999994,12.2,-7.12895196000002));
#172263=CARTESIAN_POINT('Ctrl Pts',(7.92095827899994,12.2,-7.12706266100002));
#172264=CARTESIAN_POINT('Ctrl Pts',(7.91968854599994,12.2,-7.12517990400002));
#172265=CARTESIAN_POINT('Ctrl Pts',(7.91842082599994,12.2,-7.12330369600001));
#172266=CARTESIAN_POINT('Ctrl Pts',(7.91715513599994,12.2,-7.12143404200001));
#172267=CARTESIAN_POINT('Ctrl Pts',(7.91589149199995,12.2,-7.11957094700002));
#172268=CARTESIAN_POINT('Ctrl Pts',(7.91462990899995,12.2,-7.11771441600002));
#172269=CARTESIAN_POINT('Ctrl Pts',(7.91337040399994,12.2,-7.11586445500001));
#172270=CARTESIAN_POINT('Ctrl Pts',(7.91211299299994,12.2,-7.11402106900002));
#172271=CARTESIAN_POINT('Ctrl Pts',(7.91085769199994,12.2,-7.11218426400002));
#172272=CARTESIAN_POINT('Ctrl Pts',(7.90960451799994,12.2,-7.11035404400001));
#172273=CARTESIAN_POINT('Ctrl Pts',(7.90835348799995,12.2,-7.10853041700001));
#172274=CARTESIAN_POINT('Ctrl Pts',(7.90710461699994,12.2,-7.10671338500001));
#172275=CARTESIAN_POINT('Ctrl Pts',(7.90585792199994,12.2,-7.10490295600002));
#172276=CARTESIAN_POINT('Ctrl Pts',(7.90461341899995,12.2,-7.10309913500001));
#172277=CARTESIAN_POINT('Ctrl Pts',(7.90337112499994,12.2,-7.10130192600002));
#172278=CARTESIAN_POINT('Ctrl Pts',(7.90213105799995,12.2,-7.09951133600002));
#172279=CARTESIAN_POINT('Ctrl Pts',(7.90089323199994,12.2,-7.09772736900002));
#172280=CARTESIAN_POINT('Ctrl Pts',(7.89965766699994,12.2,-7.09595003100001));
#172281=CARTESIAN_POINT('Ctrl Pts',(7.89842437699994,12.2,-7.09417932900001));
#172282=CARTESIAN_POINT('Ctrl Pts',(7.89719338099995,12.2,-7.09241526600002));
#172283=CARTESIAN_POINT('Ctrl Pts',(7.89596469399994,12.2,-7.09065784900002));
#172284=CARTESIAN_POINT('Ctrl Pts',(7.89473833399994,12.2,-7.08890708300002));
#172285=CARTESIAN_POINT('Ctrl Pts',(7.89351431799994,12.2,-7.08716297200001));
#172286=CARTESIAN_POINT('Ctrl Pts',(7.89229266299994,12.2,-7.08542552500001));
#172287=CARTESIAN_POINT('Ctrl Pts',(7.89107338599995,12.2,-7.08369474300002));
#172288=CARTESIAN_POINT('Ctrl Pts',(7.88985650599995,12.2,-7.08197063500001));
#172289=CARTESIAN_POINT('Ctrl Pts',(7.88864203699994,12.2,-7.08025320500001));
#172290=CARTESIAN_POINT('Ctrl Pts',(7.88742999899994,12.2,-7.07854245900001));
#172291=CARTESIAN_POINT('Ctrl Pts',(7.88622040799994,12.2,-7.07683840200002));
#172292=CARTESIAN_POINT('Ctrl Pts',(7.88501328299994,12.2,-7.07514104000002));
#172293=CARTESIAN_POINT('Ctrl Pts',(7.88380863899994,12.2,-7.07345037800001));
#172294=CARTESIAN_POINT('Ctrl Pts',(7.88260649599994,12.2,-7.07176642200002));
#172295=CARTESIAN_POINT('Ctrl Pts',(7.88140687099995,12.2,-7.07008917700002));
#172296=CARTESIAN_POINT('Ctrl Pts',(7.88020978099994,12.2,-7.06841865000002));
#172297=CARTESIAN_POINT('Ctrl Pts',(7.87901524399994,12.2,-7.06675484400002));
#172298=CARTESIAN_POINT('Ctrl Pts',(7.87782327799994,12.2,-7.06509776600001));
#172299=CARTESIAN_POINT('Ctrl Pts',(7.87663390099994,12.2,-7.06344742200002));
#172300=CARTESIAN_POINT('Ctrl Pts',(7.87544713199994,12.2,-7.06180381500002));
#172301=CARTESIAN_POINT('Ctrl Pts',(7.87426298699994,12.2,-7.06016695500002));
#172302=CARTESIAN_POINT('Ctrl Pts',(7.87308148499994,12.2,-7.05853684400001));
#172303=CARTESIAN_POINT('Ctrl Pts',(7.87190264399995,12.2,-7.05691348900002));
#172304=CARTESIAN_POINT('Ctrl Pts',(7.87072648199994,12.2,-7.05529689500001));
#172305=CARTESIAN_POINT('Ctrl Pts',(7.86955301799994,12.2,-7.05368706700002));
#172306=CARTESIAN_POINT('Ctrl Pts',(7.86838226999994,12.2,-7.05208401300002));
#172307=CARTESIAN_POINT('Ctrl Pts',(7.86721425699994,12.2,-7.05048773600002));
#172308=CARTESIAN_POINT('Ctrl Pts',(7.86604899599994,12.2,-7.04889824300002));
#172309=CARTESIAN_POINT('Ctrl Pts',(7.86488650699994,12.2,-7.04731553900002));
#172310=CARTESIAN_POINT('Ctrl Pts',(7.86372680699994,12.2,-7.04573963100002));
#172311=CARTESIAN_POINT('Ctrl Pts',(7.86256991599994,12.2,-7.04417052200002));
#172312=CARTESIAN_POINT('Ctrl Pts',(7.86141585299994,12.2,-7.04260821900001));
#172313=CARTESIAN_POINT('Ctrl Pts',(7.86026463599995,12.2,-7.04105272900001));
#172314=CARTESIAN_POINT('Ctrl Pts',(7.85911628399995,12.2,-7.03950405600001));
#172315=CARTESIAN_POINT('Ctrl Pts',(7.85797081499994,12.2,-7.03796220700001));
#172316=CARTESIAN_POINT('Ctrl Pts',(7.85682825099994,12.2,-7.03642718500002));
#172317=CARTESIAN_POINT('Ctrl Pts',(7.85568860799994,12.2,-7.03489899900001));
#172318=CARTESIAN_POINT('Ctrl Pts',(7.85455190599994,12.2,-7.03337765200001));
#172319=CARTESIAN_POINT('Ctrl Pts',(7.85341816499994,12.2,-7.03186315100002));
#172320=CARTESIAN_POINT('Ctrl Pts',(7.85228740299994,12.2,-7.03035550200001));
#172321=CARTESIAN_POINT('Ctrl Pts',(7.85115964099995,12.2,-7.02885471000001));
#172322=CARTESIAN_POINT('Ctrl Pts',(7.85003489699994,12.2,-7.02736078100001));
#172323=CARTESIAN_POINT('Ctrl Pts',(7.84891319099994,12.2,-7.02587372100002));
#172324=CARTESIAN_POINT('Ctrl Pts',(7.84779454299994,12.2,-7.02439353600001));
#172325=CARTESIAN_POINT('Ctrl Pts',(7.84667897299994,12.2,-7.02292023000001));
#172326=CARTESIAN_POINT('Ctrl Pts',(7.84556649899995,12.2,-7.02145381000002));
#172327=CARTESIAN_POINT('Ctrl Pts',(7.84445714199994,12.2,-7.01999428200001));
#172328=CARTESIAN_POINT('Ctrl Pts',(7.84335092199994,12.2,-7.01854165200002));
#172329=CARTESIAN_POINT('Ctrl Pts',(7.84224785899994,12.2,-7.01709592400002));
#172330=CARTESIAN_POINT('Ctrl Pts',(7.84114797199994,12.2,-7.01565710600002));
#172331=CARTESIAN_POINT('Ctrl Pts',(7.84005128199994,12.2,-7.01422520300002));
#172332=CARTESIAN_POINT('Ctrl Pts',(7.83895780899994,12.2,-7.01280021900001));
#172333=CARTESIAN_POINT('Ctrl Pts',(7.83786757299994,12.2,-7.01138216400001));
#172334=CARTESIAN_POINT('Ctrl Pts',(7.83656319944734,12.2,-7.00968881406154));
#172335=CARTESIAN_POINT('Ctrl Pts',(7.83526374289428,12.2,-7.00800587412212));
#172336=CARTESIAN_POINT('Ctrl Pts',(7.83396924322319,12.2,-7.00633335002984));
#172337=CARTESIAN_POINT('Ctrl Pts',(7.83267974367058,12.2,-7.00467125709134));
#172338=CARTESIAN_POINT('Ctrl Pts',(7.83139528399994,12.2,-7.00301960700001));
#172339=CARTESIAN_POINT('Ctrl Pts',(7.83032828199994,12.2,-7.00165020000002));
#172340=CARTESIAN_POINT('Ctrl Pts',(7.82926468199994,12.2,-7.00028776600002));
#172341=CARTESIAN_POINT('Ctrl Pts',(7.82820450599995,12.2,-6.99893231100001));
#172342=CARTESIAN_POINT('Ctrl Pts',(7.82714777299995,12.2,-6.99758384000001));
#172343=CARTESIAN_POINT('Ctrl Pts',(7.82609450599994,12.2,-6.99624236100002));
#172344=CARTESIAN_POINT('Ctrl Pts',(7.82504472499994,12.2,-6.99490787800002));
#172345=CARTESIAN_POINT('Ctrl Pts',(7.82399845099994,12.2,-6.99358039900002));
#172346=CARTESIAN_POINT('Ctrl Pts',(7.82295570699994,12.2,-6.99225992800002));
#172347=CARTESIAN_POINT('Ctrl Pts',(7.82191651399994,12.2,-6.99094647200001));
#172348=CARTESIAN_POINT('Ctrl Pts',(7.82088089199994,12.2,-6.98964003700001));
#172349=CARTESIAN_POINT('Ctrl Pts',(7.81984886499994,12.2,-6.98834063000002));
#172350=CARTESIAN_POINT('Ctrl Pts',(7.81882045199994,12.2,-6.98704825400001));
#172351=CARTESIAN_POINT('Ctrl Pts',(7.81779567699994,12.2,-6.98576291700002));
#172352=CARTESIAN_POINT('Ctrl Pts',(7.81677456099994,12.2,-6.98448462500001));
#172353=CARTESIAN_POINT('Ctrl Pts',(7.81575712599994,12.2,-6.98321338300002));
#172354=CARTESIAN_POINT('Ctrl Pts',(7.81474339499994,12.2,-6.98194919900001));
#172355=CARTESIAN_POINT('Ctrl Pts',(7.81373338799995,12.2,-6.98069207700001));
#172356=CARTESIAN_POINT('Ctrl Pts',(7.81272712999994,12.2,-6.97944202400001));
#172357=CARTESIAN_POINT('Ctrl Pts',(7.81172464099994,12.2,-6.97819904500002));
#172358=CARTESIAN_POINT('Ctrl Pts',(7.81072594399994,12.2,-6.97696314800002));
#172359=CARTESIAN_POINT('Ctrl Pts',(7.80973106299995,12.2,-6.97573433800001));
#172360=CARTESIAN_POINT('Ctrl Pts',(7.80874001999995,12.2,-6.97451262100002));
#172361=CARTESIAN_POINT('Ctrl Pts',(7.80775283599994,12.2,-6.97329800400002));
#172362=CARTESIAN_POINT('Ctrl Pts',(7.80676953599994,12.2,-6.97209049100002));
#172363=CARTESIAN_POINT('Ctrl Pts',(7.80579014099994,12.2,-6.97089009000001));
#172364=CARTESIAN_POINT('Ctrl Pts',(7.80481467499994,12.2,-6.96969680700001));
#172365=CARTESIAN_POINT('Ctrl Pts',(7.80384316099994,12.2,-6.96851064800001));
#172366=CARTESIAN_POINT('Ctrl Pts',(7.80287562299995,12.2,-6.96733161900001));
#172367=CARTESIAN_POINT('Ctrl Pts',(7.80191208299994,12.2,-6.96615972600001));
#172368=CARTESIAN_POINT('Ctrl Pts',(7.80095256499994,12.2,-6.96499497500002));
#172369=CARTESIAN_POINT('Ctrl Pts',(7.79999709199994,12.2,-6.96383737300001));
#172370=CARTESIAN_POINT('Ctrl Pts',(7.79904568799994,12.2,-6.96268692600002));
#172371=CARTESIAN_POINT('Ctrl Pts',(7.79809837699994,12.2,-6.96154364000002));
#172372=CARTESIAN_POINT('Ctrl Pts',(7.79715518199994,12.2,-6.96040752000001));
#172373=CARTESIAN_POINT('Ctrl Pts',(7.79621612699994,12.2,-6.95927857500001));
#172374=CARTESIAN_POINT('Ctrl Pts',(7.79528123699994,12.2,-6.95815681000001));
#172375=CARTESIAN_POINT('Ctrl Pts',(7.79435053399994,12.2,-6.95704223000002));
#172376=CARTESIAN_POINT('Ctrl Pts',(7.79342404399994,12.2,-6.95593484200002));
#172377=CARTESIAN_POINT('Ctrl Pts',(7.79250179099995,12.2,-6.95483465400001));
#172378=CARTESIAN_POINT('Ctrl Pts',(7.79158379899994,12.2,-6.95374167100002));
#172379=CARTESIAN_POINT('Ctrl Pts',(7.79067009299995,12.2,-6.95265589900002));
#172380=CARTESIAN_POINT('Ctrl Pts',(7.78976069699994,12.2,-6.95157734400001));
#172381=CARTESIAN_POINT('Ctrl Pts',(7.78885563499994,12.2,-6.95050601300002));
#172382=CARTESIAN_POINT('Ctrl Pts',(7.78795493299994,12.2,-6.94944191300002));
#172383=CARTESIAN_POINT('Ctrl Pts',(7.78705861699994,12.2,-6.94838504900002));
#172384=CARTESIAN_POINT('Ctrl Pts',(7.78616670899994,12.2,-6.94733542900002));
#172385=CARTESIAN_POINT('Ctrl Pts',(7.78527923799994,12.2,-6.94629305800002));
#172386=CARTESIAN_POINT('Ctrl Pts',(7.78439622499994,12.2,-6.94525794300001));
#172387=CARTESIAN_POINT('Ctrl Pts',(7.78351769799994,12.2,-6.94423009100002));
#172388=CARTESIAN_POINT('Ctrl Pts',(7.78264368299994,12.2,-6.94320950700002));
#172389=CARTESIAN_POINT('Ctrl Pts',(7.78177420299994,12.2,-6.94219620000001));
#172390=CARTESIAN_POINT('Ctrl Pts',(7.78090928599994,12.2,-6.94119017400002));
#172391=CARTESIAN_POINT('Ctrl Pts',(7.78004895599994,12.2,-6.94019143600002));
#172392=CARTESIAN_POINT('Ctrl Pts',(7.77919324199994,12.2,-6.93919999300002));
#172393=CARTESIAN_POINT('Ctrl Pts',(7.77834216699994,12.2,-6.93821585200002));
#172394=CARTESIAN_POINT('Ctrl Pts',(7.77749575799994,12.2,-6.93723901900002));
#172395=CARTESIAN_POINT('Ctrl Pts',(7.77665404199994,12.2,-6.93626950100001));
#172396=CARTESIAN_POINT('Ctrl Pts',(7.77581704399994,12.2,-6.93530730300001));
#172397=CARTESIAN_POINT('Ctrl Pts',(7.77498479199994,12.2,-6.93435243300002));
#172398=CARTESIAN_POINT('Ctrl Pts',(7.77415731199994,12.2,-6.93340489800002));
#172399=CARTESIAN_POINT('Ctrl Pts',(7.77333463099994,12.2,-6.93246470300001));
#172400=CARTESIAN_POINT('Ctrl Pts',(7.77251677499994,12.2,-6.93153185600002));
#172401=CARTESIAN_POINT('Ctrl Pts',(7.77170377299995,12.2,-6.93060636300002));
#172402=CARTESIAN_POINT('Ctrl Pts',(7.77089564999994,12.2,-6.92968823200002));
#172403=CARTESIAN_POINT('Ctrl Pts',(7.77009243399994,12.2,-6.92877746800002));
#172404=CARTESIAN_POINT('Ctrl Pts',(7.76929415399994,12.2,-6.92787407800001));
#172405=CARTESIAN_POINT('Ctrl Pts',(7.76850083499995,12.2,-6.92697807000001));
#172406=CARTESIAN_POINT('Ctrl Pts',(7.76771250599994,12.2,-6.92608944900002));
#172407=CARTESIAN_POINT('Ctrl Pts',(7.76692919399995,12.2,-6.92520822300001));
#172408=CARTESIAN_POINT('Ctrl Pts',(7.76615092799994,12.2,-6.92433439700002));
#172409=CARTESIAN_POINT('Ctrl Pts',(7.76537773499994,12.2,-6.92346798200001));
#172410=CARTESIAN_POINT('Ctrl Pts',(7.76460964399995,12.2,-6.92260898000002));
#172411=CARTESIAN_POINT('Ctrl Pts',(7.76384668299994,12.2,-6.92175740000001));
#172412=CARTESIAN_POINT('Ctrl Pts',(7.76308887999994,12.2,-6.92091324900002));
#172413=CARTESIAN_POINT('Ctrl Pts',(7.76233626399994,12.2,-6.92007653400001));
#172414=CARTESIAN_POINT('Ctrl Pts',(7.76158886399994,12.2,-6.91924726000002));
#172415=CARTESIAN_POINT('Ctrl Pts',(7.76084670899994,12.2,-6.91842543600002));
#172416=CARTESIAN_POINT('Ctrl Pts',(7.76010982699994,12.2,-6.91761106900002));
#172417=CARTESIAN_POINT('Ctrl Pts',(7.75937824799994,12.2,-6.91680416500001));
#172418=CARTESIAN_POINT('Ctrl Pts',(7.75865200099994,12.2,-6.91600473000002));
#172419=CARTESIAN_POINT('Ctrl Pts',(7.75793111599994,12.2,-6.91521277400001));
#172420=CARTESIAN_POINT('Ctrl Pts',(7.75721561999994,12.2,-6.91442830100002));
#172421=CARTESIAN_POINT('Ctrl Pts',(7.75650554599994,12.2,-6.91365131900002));
#172422=CARTESIAN_POINT('Ctrl Pts',(7.75580092299994,12.2,-6.91288183500002));
#172423=CARTESIAN_POINT('Ctrl Pts',(7.75510177999994,12.2,-6.91211985800001));
#172424=CARTESIAN_POINT('Ctrl Pts',(7.75440814899994,12.2,-6.91136539200001));
#172425=CARTESIAN_POINT('Ctrl Pts',(7.75372005699994,12.2,-6.91061844600001));
#172426=CARTESIAN_POINT('Ctrl Pts',(7.75303753799994,12.2,-6.90987902600002));
#172427=CARTESIAN_POINT('Ctrl Pts',(7.75236061999995,12.2,-6.90914714000002));
#172428=CARTESIAN_POINT('Ctrl Pts',(7.75168933499994,12.2,-6.90842279600002));
#172429=CARTESIAN_POINT('Ctrl Pts',(7.75102371399995,12.2,-6.90770599900001));
#172430=CARTESIAN_POINT('Ctrl Pts',(7.75036378799994,12.2,-6.90699675800002));
#172431=CARTESIAN_POINT('Ctrl Pts',(7.74970958799994,12.2,-6.90629507900002));
#172432=CARTESIAN_POINT('Ctrl Pts',(7.74906114399994,12.2,-6.90560097000001));
#172433=CARTESIAN_POINT('Ctrl Pts',(7.74841849099994,12.2,-6.90491443800001));
#172434=CARTESIAN_POINT('Ctrl Pts',(7.74778165799995,12.2,-6.90423549000001));
#172435=CARTESIAN_POINT('Ctrl Pts',(7.74715431199994,12.2,-6.90356800200002));
#172436=CARTESIAN_POINT('Ctrl Pts',(7.74665780099994,12.2,-6.90304077600001));
#172437=CARTESIAN_POINT('Ctrl Pts',(7.74628892999995,12.2,-6.90264967000001));
#172438=CARTESIAN_POINT('Ctrl Pts',(7.74604536199995,12.2,-6.90239167400001));
#172439=CARTESIAN_POINT('Ctrl Pts',(7.74592563699994,12.2,-6.90226492000001));
#172440=CARTESIAN_POINT('Ctrl Pts',(7.74592563699994,15.2,-6.90226492000001));
#172441=CARTESIAN_POINT('Ctrl Pts',(7.74604536199995,15.2,-6.90239167400001));
#172442=CARTESIAN_POINT('Ctrl Pts',(7.74628892999995,15.2,-6.90264967000001));
#172443=CARTESIAN_POINT('Ctrl Pts',(7.74665780099994,15.2,-6.90304077600001));
#172444=CARTESIAN_POINT('Ctrl Pts',(7.74715431199994,15.2,-6.90356800200002));
#172445=CARTESIAN_POINT('Ctrl Pts',(7.74778165799995,15.2,-6.90423549000001));
#172446=CARTESIAN_POINT('Ctrl Pts',(7.74841849099994,15.2,-6.90491443800001));
#172447=CARTESIAN_POINT('Ctrl Pts',(7.74906114399994,15.2,-6.90560097000001));
#172448=CARTESIAN_POINT('Ctrl Pts',(7.74970958799994,15.2,-6.90629507900002));
#172449=CARTESIAN_POINT('Ctrl Pts',(7.75036378799994,15.2,-6.90699675800002));
#172450=CARTESIAN_POINT('Ctrl Pts',(7.75102371399995,15.2,-6.90770599900001));
#172451=CARTESIAN_POINT('Ctrl Pts',(7.75168933499994,15.2,-6.90842279600002));
#172452=CARTESIAN_POINT('Ctrl Pts',(7.75236061999995,15.2,-6.90914714000002));
#172453=CARTESIAN_POINT('Ctrl Pts',(7.75303753799994,15.2,-6.90987902600002));
#172454=CARTESIAN_POINT('Ctrl Pts',(7.75372005699994,15.2,-6.91061844600001));
#172455=CARTESIAN_POINT('Ctrl Pts',(7.75440814899994,15.2,-6.91136539200001));
#172456=CARTESIAN_POINT('Ctrl Pts',(7.75510177999994,15.2,-6.91211985800001));
#172457=CARTESIAN_POINT('Ctrl Pts',(7.75580092299994,15.2,-6.91288183500002));
#172458=CARTESIAN_POINT('Ctrl Pts',(7.75650554599994,15.2,-6.91365131900002));
#172459=CARTESIAN_POINT('Ctrl Pts',(7.75721561999994,15.2,-6.91442830100002));
#172460=CARTESIAN_POINT('Ctrl Pts',(7.75793111599994,15.2,-6.91521277400001));
#172461=CARTESIAN_POINT('Ctrl Pts',(7.75865200099994,15.2,-6.91600473000002));
#172462=CARTESIAN_POINT('Ctrl Pts',(7.75937824799994,15.2,-6.91680416500001));
#172463=CARTESIAN_POINT('Ctrl Pts',(7.76010982699994,15.2,-6.91761106900002));
#172464=CARTESIAN_POINT('Ctrl Pts',(7.76084670899994,15.2,-6.91842543600002));
#172465=CARTESIAN_POINT('Ctrl Pts',(7.76158886399994,15.2,-6.91924726000002));
#172466=CARTESIAN_POINT('Ctrl Pts',(7.76233626399994,15.2,-6.92007653400001));
#172467=CARTESIAN_POINT('Ctrl Pts',(7.76308887999994,15.2,-6.92091324900002));
#172468=CARTESIAN_POINT('Ctrl Pts',(7.76384668299994,15.2,-6.92175740000001));
#172469=CARTESIAN_POINT('Ctrl Pts',(7.76460964399995,15.2,-6.92260898000002));
#172470=CARTESIAN_POINT('Ctrl Pts',(7.76537773499994,15.2,-6.92346798200001));
#172471=CARTESIAN_POINT('Ctrl Pts',(7.76615092799994,15.2,-6.92433439700002));
#172472=CARTESIAN_POINT('Ctrl Pts',(7.76692919399995,15.2,-6.92520822300001));
#172473=CARTESIAN_POINT('Ctrl Pts',(7.76771250599994,15.2,-6.92608944900002));
#172474=CARTESIAN_POINT('Ctrl Pts',(7.76850083499995,15.2,-6.92697807000001));
#172475=CARTESIAN_POINT('Ctrl Pts',(7.76929415399994,15.2,-6.92787407800001));
#172476=CARTESIAN_POINT('Ctrl Pts',(7.77009243399994,15.2,-6.92877746800002));
#172477=CARTESIAN_POINT('Ctrl Pts',(7.77089564999994,15.2,-6.92968823200002));
#172478=CARTESIAN_POINT('Ctrl Pts',(7.77170377299995,15.2,-6.93060636300002));
#172479=CARTESIAN_POINT('Ctrl Pts',(7.77251677499994,15.2,-6.93153185600002));
#172480=CARTESIAN_POINT('Ctrl Pts',(7.77333463099994,15.2,-6.93246470300001));
#172481=CARTESIAN_POINT('Ctrl Pts',(7.77415731199994,15.2,-6.93340489800002));
#172482=CARTESIAN_POINT('Ctrl Pts',(7.77498479199994,15.2,-6.93435243300002));
#172483=CARTESIAN_POINT('Ctrl Pts',(7.77581704399994,15.2,-6.93530730300001));
#172484=CARTESIAN_POINT('Ctrl Pts',(7.77665404199994,15.2,-6.93626950100001));
#172485=CARTESIAN_POINT('Ctrl Pts',(7.77749575799994,15.2,-6.93723901900002));
#172486=CARTESIAN_POINT('Ctrl Pts',(7.77834216699994,15.2,-6.93821585200002));
#172487=CARTESIAN_POINT('Ctrl Pts',(7.77919324199994,15.2,-6.93919999300002));
#172488=CARTESIAN_POINT('Ctrl Pts',(7.78004895599994,15.2,-6.94019143600002));
#172489=CARTESIAN_POINT('Ctrl Pts',(7.78090928599994,15.2,-6.94119017400002));
#172490=CARTESIAN_POINT('Ctrl Pts',(7.78177420299994,15.2,-6.94219620000001));
#172491=CARTESIAN_POINT('Ctrl Pts',(7.78264368299994,15.2,-6.94320950700002));
#172492=CARTESIAN_POINT('Ctrl Pts',(7.78351769799994,15.2,-6.94423009100002));
#172493=CARTESIAN_POINT('Ctrl Pts',(7.78439622499994,15.2,-6.94525794300001));
#172494=CARTESIAN_POINT('Ctrl Pts',(7.78527923799994,15.2,-6.94629305800002));
#172495=CARTESIAN_POINT('Ctrl Pts',(7.78616670899994,15.2,-6.94733542900002));
#172496=CARTESIAN_POINT('Ctrl Pts',(7.78705861699994,15.2,-6.94838504900002));
#172497=CARTESIAN_POINT('Ctrl Pts',(7.78795493299994,15.2,-6.94944191300002));
#172498=CARTESIAN_POINT('Ctrl Pts',(7.78885563499994,15.2,-6.95050601300002));
#172499=CARTESIAN_POINT('Ctrl Pts',(7.78976069699994,15.2,-6.95157734400001));
#172500=CARTESIAN_POINT('Ctrl Pts',(7.79067009299995,15.2,-6.95265589900002));
#172501=CARTESIAN_POINT('Ctrl Pts',(7.79158379899994,15.2,-6.95374167100002));
#172502=CARTESIAN_POINT('Ctrl Pts',(7.79250179099995,15.2,-6.95483465400001));
#172503=CARTESIAN_POINT('Ctrl Pts',(7.79342404399994,15.2,-6.95593484200002));
#172504=CARTESIAN_POINT('Ctrl Pts',(7.79435053399994,15.2,-6.95704223000002));
#172505=CARTESIAN_POINT('Ctrl Pts',(7.79528123699994,15.2,-6.95815681000001));
#172506=CARTESIAN_POINT('Ctrl Pts',(7.79621612699994,15.2,-6.95927857500001));
#172507=CARTESIAN_POINT('Ctrl Pts',(7.79715518199994,15.2,-6.96040752000001));
#172508=CARTESIAN_POINT('Ctrl Pts',(7.79809837699994,15.2,-6.96154364000002));
#172509=CARTESIAN_POINT('Ctrl Pts',(7.79904568799994,15.2,-6.96268692600002));
#172510=CARTESIAN_POINT('Ctrl Pts',(7.79999709199994,15.2,-6.96383737300001));
#172511=CARTESIAN_POINT('Ctrl Pts',(7.80095256499994,15.2,-6.96499497500002));
#172512=CARTESIAN_POINT('Ctrl Pts',(7.80191208299994,15.2,-6.96615972600001));
#172513=CARTESIAN_POINT('Ctrl Pts',(7.80287562299995,15.2,-6.96733161900001));
#172514=CARTESIAN_POINT('Ctrl Pts',(7.80384316099994,15.2,-6.96851064800001));
#172515=CARTESIAN_POINT('Ctrl Pts',(7.80481467499994,15.2,-6.96969680700001));
#172516=CARTESIAN_POINT('Ctrl Pts',(7.80579014099994,15.2,-6.97089009000001));
#172517=CARTESIAN_POINT('Ctrl Pts',(7.80676953599994,15.2,-6.97209049100002));
#172518=CARTESIAN_POINT('Ctrl Pts',(7.80775283599994,15.2,-6.97329800400002));
#172519=CARTESIAN_POINT('Ctrl Pts',(7.80874001999995,15.2,-6.97451262100002));
#172520=CARTESIAN_POINT('Ctrl Pts',(7.80973106299995,15.2,-6.97573433800001));
#172521=CARTESIAN_POINT('Ctrl Pts',(7.81072594399994,15.2,-6.97696314800002));
#172522=CARTESIAN_POINT('Ctrl Pts',(7.81172464099994,15.2,-6.97819904500002));
#172523=CARTESIAN_POINT('Ctrl Pts',(7.81272712999994,15.2,-6.97944202400001));
#172524=CARTESIAN_POINT('Ctrl Pts',(7.81373338799995,15.2,-6.98069207700001));
#172525=CARTESIAN_POINT('Ctrl Pts',(7.81474339499994,15.2,-6.98194919900001));
#172526=CARTESIAN_POINT('Ctrl Pts',(7.81575712599994,15.2,-6.98321338300002));
#172527=CARTESIAN_POINT('Ctrl Pts',(7.81677456099994,15.2,-6.98448462500001));
#172528=CARTESIAN_POINT('Ctrl Pts',(7.81779567699994,15.2,-6.98576291700002));
#172529=CARTESIAN_POINT('Ctrl Pts',(7.81882045199994,15.2,-6.98704825400001));
#172530=CARTESIAN_POINT('Ctrl Pts',(7.81984886499994,15.2,-6.98834063000002));
#172531=CARTESIAN_POINT('Ctrl Pts',(7.82088089199994,15.2,-6.98964003700001));
#172532=CARTESIAN_POINT('Ctrl Pts',(7.82191651399994,15.2,-6.99094647200001));
#172533=CARTESIAN_POINT('Ctrl Pts',(7.82295570699994,15.2,-6.99225992800002));
#172534=CARTESIAN_POINT('Ctrl Pts',(7.82399845099994,15.2,-6.99358039900002));
#172535=CARTESIAN_POINT('Ctrl Pts',(7.82504472499994,15.2,-6.99490787800002));
#172536=CARTESIAN_POINT('Ctrl Pts',(7.82609450599994,15.2,-6.99624236100002));
#172537=CARTESIAN_POINT('Ctrl Pts',(7.82714777299995,15.2,-6.99758384000001));
#172538=CARTESIAN_POINT('Ctrl Pts',(7.82820450599995,15.2,-6.99893231100001));
#172539=CARTESIAN_POINT('Ctrl Pts',(7.82926468199994,15.2,-7.00028776600002));
#172540=CARTESIAN_POINT('Ctrl Pts',(7.83032828199994,15.2,-7.00165020000002));
#172541=CARTESIAN_POINT('Ctrl Pts',(7.83139528399994,15.2,-7.00301960700001));
#172542=CARTESIAN_POINT('Ctrl Pts',(7.83267974366995,15.2,-7.00467125709003));
#172543=CARTESIAN_POINT('Ctrl Pts',(7.83396924322351,15.2,-7.0063333500305));
#172544=CARTESIAN_POINT('Ctrl Pts',(7.83526374289397,15.2,-7.00800587412146));
#172545=CARTESIAN_POINT('Ctrl Pts',(7.83656319944797,15.2,-7.00968881406286));
#172546=CARTESIAN_POINT('Ctrl Pts',(7.83786757299994,15.2,-7.01138216400001));
#172547=CARTESIAN_POINT('Ctrl Pts',(7.83895780899994,15.2,-7.01280021900001));
#172548=CARTESIAN_POINT('Ctrl Pts',(7.84005128199994,15.2,-7.01422520300002));
#172549=CARTESIAN_POINT('Ctrl Pts',(7.84114797199994,15.2,-7.01565710600002));
#172550=CARTESIAN_POINT('Ctrl Pts',(7.84224785899994,15.2,-7.01709592400002));
#172551=CARTESIAN_POINT('Ctrl Pts',(7.84335092199994,15.2,-7.01854165200002));
#172552=CARTESIAN_POINT('Ctrl Pts',(7.84445714199994,15.2,-7.01999428200001));
#172553=CARTESIAN_POINT('Ctrl Pts',(7.84556649899995,15.2,-7.02145381000002));
#172554=CARTESIAN_POINT('Ctrl Pts',(7.84667897299994,15.2,-7.02292023000001));
#172555=CARTESIAN_POINT('Ctrl Pts',(7.84779454299994,15.2,-7.02439353600001));
#172556=CARTESIAN_POINT('Ctrl Pts',(7.84891319099994,15.2,-7.02587372100002));
#172557=CARTESIAN_POINT('Ctrl Pts',(7.85003489699994,15.2,-7.02736078100001));
#172558=CARTESIAN_POINT('Ctrl Pts',(7.85115964099995,15.2,-7.02885471000001));
#172559=CARTESIAN_POINT('Ctrl Pts',(7.85228740299994,15.2,-7.03035550200001));
#172560=CARTESIAN_POINT('Ctrl Pts',(7.85341816499994,15.2,-7.03186315100002));
#172561=CARTESIAN_POINT('Ctrl Pts',(7.85455190599994,15.2,-7.03337765200001));
#172562=CARTESIAN_POINT('Ctrl Pts',(7.85568860799994,15.2,-7.03489899900001));
#172563=CARTESIAN_POINT('Ctrl Pts',(7.85682825099994,15.2,-7.03642718500002));
#172564=CARTESIAN_POINT('Ctrl Pts',(7.85797081499994,15.2,-7.03796220700001));
#172565=CARTESIAN_POINT('Ctrl Pts',(7.85911628399995,15.2,-7.03950405600001));
#172566=CARTESIAN_POINT('Ctrl Pts',(7.86026463599995,15.2,-7.04105272900001));
#172567=CARTESIAN_POINT('Ctrl Pts',(7.86141585299994,15.2,-7.04260821900001));
#172568=CARTESIAN_POINT('Ctrl Pts',(7.86256991599994,15.2,-7.04417052200002));
#172569=CARTESIAN_POINT('Ctrl Pts',(7.86372680699994,15.2,-7.04573963100002));
#172570=CARTESIAN_POINT('Ctrl Pts',(7.86488650699994,15.2,-7.04731553900002));
#172571=CARTESIAN_POINT('Ctrl Pts',(7.86604899599994,15.2,-7.04889824300002));
#172572=CARTESIAN_POINT('Ctrl Pts',(7.86721425699994,15.2,-7.05048773600002));
#172573=CARTESIAN_POINT('Ctrl Pts',(7.86838226999994,15.2,-7.05208401300002));
#172574=CARTESIAN_POINT('Ctrl Pts',(7.86955301799994,15.2,-7.05368706700002));
#172575=CARTESIAN_POINT('Ctrl Pts',(7.87072648199994,15.2,-7.05529689500001));
#172576=CARTESIAN_POINT('Ctrl Pts',(7.87190264399995,15.2,-7.05691348900002));
#172577=CARTESIAN_POINT('Ctrl Pts',(7.87308148499994,15.2,-7.05853684400001));
#172578=CARTESIAN_POINT('Ctrl Pts',(7.87426298699994,15.2,-7.06016695500002));
#172579=CARTESIAN_POINT('Ctrl Pts',(7.87544713199994,15.2,-7.06180381500002));
#172580=CARTESIAN_POINT('Ctrl Pts',(7.87663390099994,15.2,-7.06344742200002));
#172581=CARTESIAN_POINT('Ctrl Pts',(7.87782327799994,15.2,-7.06509776600001));
#172582=CARTESIAN_POINT('Ctrl Pts',(7.87901524399994,15.2,-7.06675484400002));
#172583=CARTESIAN_POINT('Ctrl Pts',(7.88020978099994,15.2,-7.06841865000002));
#172584=CARTESIAN_POINT('Ctrl Pts',(7.88140687099995,15.2,-7.07008917700002));
#172585=CARTESIAN_POINT('Ctrl Pts',(7.88260649599994,15.2,-7.07176642200002));
#172586=CARTESIAN_POINT('Ctrl Pts',(7.88380863899994,15.2,-7.07345037800001));
#172587=CARTESIAN_POINT('Ctrl Pts',(7.88501328299994,15.2,-7.07514104000002));
#172588=CARTESIAN_POINT('Ctrl Pts',(7.88622040799994,15.2,-7.07683840200002));
#172589=CARTESIAN_POINT('Ctrl Pts',(7.88742999899994,15.2,-7.07854245900001));
#172590=CARTESIAN_POINT('Ctrl Pts',(7.88864203699994,15.2,-7.08025320500001));
#172591=CARTESIAN_POINT('Ctrl Pts',(7.88985650599995,15.2,-7.08197063500001));
#172592=CARTESIAN_POINT('Ctrl Pts',(7.89107338599995,15.2,-7.08369474300002));
#172593=CARTESIAN_POINT('Ctrl Pts',(7.89229266299994,15.2,-7.08542552500001));
#172594=CARTESIAN_POINT('Ctrl Pts',(7.89351431799994,15.2,-7.08716297200001));
#172595=CARTESIAN_POINT('Ctrl Pts',(7.89473833399994,15.2,-7.08890708300002));
#172596=CARTESIAN_POINT('Ctrl Pts',(7.89596469399994,15.2,-7.09065784900002));
#172597=CARTESIAN_POINT('Ctrl Pts',(7.89719338099995,15.2,-7.09241526600002));
#172598=CARTESIAN_POINT('Ctrl Pts',(7.89842437699994,15.2,-7.09417932900001));
#172599=CARTESIAN_POINT('Ctrl Pts',(7.89965766699994,15.2,-7.09595003100001));
#172600=CARTESIAN_POINT('Ctrl Pts',(7.90089323199994,15.2,-7.09772736900002));
#172601=CARTESIAN_POINT('Ctrl Pts',(7.90213105799995,15.2,-7.09951133600002));
#172602=CARTESIAN_POINT('Ctrl Pts',(7.90337112499994,15.2,-7.10130192600002));
#172603=CARTESIAN_POINT('Ctrl Pts',(7.90461341899995,15.2,-7.10309913500001));
#172604=CARTESIAN_POINT('Ctrl Pts',(7.90585792199994,15.2,-7.10490295600002));
#172605=CARTESIAN_POINT('Ctrl Pts',(7.90710461699994,15.2,-7.10671338500001));
#172606=CARTESIAN_POINT('Ctrl Pts',(7.90835348799995,15.2,-7.10853041700001));
#172607=CARTESIAN_POINT('Ctrl Pts',(7.90960451799994,15.2,-7.11035404400001));
#172608=CARTESIAN_POINT('Ctrl Pts',(7.91085769199994,15.2,-7.11218426400002));
#172609=CARTESIAN_POINT('Ctrl Pts',(7.91211299299994,15.2,-7.11402106900002));
#172610=CARTESIAN_POINT('Ctrl Pts',(7.91337040399994,15.2,-7.11586445500001));
#172611=CARTESIAN_POINT('Ctrl Pts',(7.91462990899995,15.2,-7.11771441600002));
#172612=CARTESIAN_POINT('Ctrl Pts',(7.91589149199995,15.2,-7.11957094700002));
#172613=CARTESIAN_POINT('Ctrl Pts',(7.91715513599994,15.2,-7.12143404200001));
#172614=CARTESIAN_POINT('Ctrl Pts',(7.91842082599994,15.2,-7.12330369600001));
#172615=CARTESIAN_POINT('Ctrl Pts',(7.91968854599994,15.2,-7.12517990400002));
#172616=CARTESIAN_POINT('Ctrl Pts',(7.92095827899994,15.2,-7.12706266100002));
#172617=CARTESIAN_POINT('Ctrl Pts',(7.92223000999994,15.2,-7.12895196000002));
#172618=CARTESIAN_POINT('Ctrl Pts',(7.92350372299994,15.2,-7.13084779800001));
#172619=CARTESIAN_POINT('Ctrl Pts',(7.92477940099995,15.2,-7.13275016800001));
#172620=CARTESIAN_POINT('Ctrl Pts',(7.92605702899994,15.2,-7.13465906400002));
#172621=CARTESIAN_POINT('Ctrl Pts',(7.92733659099994,15.2,-7.13657448300002));
#172622=CARTESIAN_POINT('Ctrl Pts',(7.92861807299994,15.2,-7.13849641800002));
#172623=CARTESIAN_POINT('Ctrl Pts',(7.92990145699994,15.2,-7.14042486500002));
#172624=CARTESIAN_POINT('Ctrl Pts',(7.93118672799995,15.2,-7.14235981700002));
#172625=CARTESIAN_POINT('Ctrl Pts',(7.93247387099994,15.2,-7.14430127000002));
#172626=CARTESIAN_POINT('Ctrl Pts',(7.93376286999995,15.2,-7.14624921800001));
#172627=CARTESIAN_POINT('Ctrl Pts',(7.93505370999994,15.2,-7.14820365600002));
#172628=CARTESIAN_POINT('Ctrl Pts',(7.93634637499995,15.2,-7.15016457800001));
#172629=CARTESIAN_POINT('Ctrl Pts',(7.93764085099995,15.2,-7.15213198100002));
#172630=CARTESIAN_POINT('Ctrl Pts',(7.93893712099995,15.2,-7.15410585600001));
#172631=CARTESIAN_POINT('Ctrl Pts',(7.94023516999995,15.2,-7.15608620200002));
#172632=CARTESIAN_POINT('Ctrl Pts',(7.94153498399995,15.2,-7.15807301100002));
#172633=CARTESIAN_POINT('Ctrl Pts',(7.94283654599995,15.2,-7.16006627800001));
#172634=CARTESIAN_POINT('Ctrl Pts',(7.94413984299994,15.2,-7.16206599900002));
#172635=CARTESIAN_POINT('Ctrl Pts',(7.94544485899995,15.2,-7.16407216700001));
#172636=CARTESIAN_POINT('Ctrl Pts',(7.94675157799994,15.2,-7.16608477700002));
#172637=CARTESIAN_POINT('Ctrl Pts',(7.94805998699994,15.2,-7.16810382500002));
#172638=CARTESIAN_POINT('Ctrl Pts',(7.94937006899994,15.2,-7.17012930500001));
#172639=CARTESIAN_POINT('Ctrl Pts',(7.95068181099994,15.2,-7.17216121300002));
#172640=CARTESIAN_POINT('Ctrl Pts',(7.95199519599994,15.2,-7.17419954200002));
#172641=CARTESIAN_POINT('Ctrl Pts',(7.95331021099994,15.2,-7.17624428700002));
#172642=CARTESIAN_POINT('Ctrl Pts',(7.95462684099994,15.2,-7.17829544400002));
#172643=CARTESIAN_POINT('Ctrl Pts',(7.95594507099994,15.2,-7.18035300600001));
#172644=CARTESIAN_POINT('Ctrl Pts',(7.95726488599994,15.2,-7.18241697000002));
#172645=CARTESIAN_POINT('Ctrl Pts',(7.95858627199994,15.2,-7.18448732900002));
#172646=CARTESIAN_POINT('Ctrl Pts',(7.95990921399994,15.2,-7.18656407900002));
#172647=CARTESIAN_POINT('Ctrl Pts',(7.96123369799994,15.2,-7.18864721300001));
#172648=CARTESIAN_POINT('Ctrl Pts',(7.96255970799994,15.2,-7.19073672800001));
#172649=CARTESIAN_POINT('Ctrl Pts',(7.96388723099994,15.2,-7.19283261800002));
#172650=CARTESIAN_POINT('Ctrl Pts',(7.96521625299994,15.2,-7.19493487700002));
#172651=CARTESIAN_POINT('Ctrl Pts',(7.96654675899994,15.2,-7.19704350100002));
#172652=CARTESIAN_POINT('Ctrl Pts',(7.96787873499994,15.2,-7.19915848400002));
#172653=CARTESIAN_POINT('Ctrl Pts',(7.96921216599995,15.2,-7.20127982100002));
#172654=CARTESIAN_POINT('Ctrl Pts',(7.97054703699994,15.2,-7.20340750800001));
#172655=CARTESIAN_POINT('Ctrl Pts',(7.97188333599994,15.2,-7.20554153800002));
#172656=CARTESIAN_POINT('Ctrl Pts',(7.97322104799994,15.2,-7.20768190700002));
#172657=CARTESIAN_POINT('Ctrl Pts',(7.97456015899995,15.2,-7.20982861000002));
#172658=CARTESIAN_POINT('Ctrl Pts',(7.97590065499994,15.2,-7.21198164000001));
#172659=CARTESIAN_POINT('Ctrl Pts',(7.97724252099994,15.2,-7.21414099500001));
#172660=CARTESIAN_POINT('Ctrl Pts',(7.97858574299994,15.2,-7.21630666700002));
#172661=CARTESIAN_POINT('Ctrl Pts',(7.97993030999994,15.2,-7.21847865300001));
#172662=CARTESIAN_POINT('Ctrl Pts',(7.98127620499994,15.2,-7.22065694600002));
#172663=CARTESIAN_POINT('Ctrl Pts',(7.98262341399994,15.2,-7.22284154100001));
#172664=CARTESIAN_POINT('Ctrl Pts',(7.98397192599994,15.2,-7.22503243400002));
#172665=CARTESIAN_POINT('Ctrl Pts',(7.98532172499994,15.2,-7.22722962000002));
#172666=CARTESIAN_POINT('Ctrl Pts',(7.98667279799994,15.2,-7.22943309400002));
#172667=CARTESIAN_POINT('Ctrl Pts',(7.98802512999995,15.2,-7.23164284900002));
#172668=CARTESIAN_POINT('Ctrl Pts',(7.98937870999994,15.2,-7.23385888200001));
#172669=CARTESIAN_POINT('Ctrl Pts',(7.99073352199994,15.2,-7.23608118600002));
#172670=CARTESIAN_POINT('Ctrl Pts',(7.99208955399994,15.2,-7.23830975700002));
#172671=CARTESIAN_POINT('Ctrl Pts',(7.99344679099995,15.2,-7.24054459100002));
#172672=CARTESIAN_POINT('Ctrl Pts',(7.99480522199994,15.2,-7.24278568000001));
#172673=CARTESIAN_POINT('Ctrl Pts',(7.99616483099994,15.2,-7.24503302300001));
#172674=CARTESIAN_POINT('Ctrl Pts',(7.99752560499994,15.2,-7.24728661100002));
#172675=CARTESIAN_POINT('Ctrl Pts',(7.99888753099995,15.2,-7.24954644100002));
#172676=CARTESIAN_POINT('Ctrl Pts',(8.00025059599994,15.2,-7.25181250700001));
#172677=CARTESIAN_POINT('Ctrl Pts',(8.00161478799994,15.2,-7.25408480400001));
#172678=CARTESIAN_POINT('Ctrl Pts',(8.00298009099994,15.2,-7.25636332800002));
#172679=CARTESIAN_POINT('Ctrl Pts',(8.00434649299994,15.2,-7.25864807300002));
#172680=CARTESIAN_POINT('Ctrl Pts',(8.00571398099994,15.2,-7.26093903400002));
#172681=CARTESIAN_POINT('Ctrl Pts',(8.00708254199994,15.2,-7.26323620600001));
#172682=CARTESIAN_POINT('Ctrl Pts',(8.00845216399994,15.2,-7.26553958500002));
#172683=CARTESIAN_POINT('Ctrl Pts',(8.00982282999994,15.2,-7.26784916400002));
#172684=CARTESIAN_POINT('Ctrl Pts',(8.01119453199994,15.2,-7.27016493800001));
#172685=CARTESIAN_POINT('Ctrl Pts',(8.01256725299995,15.2,-7.27248690400002));
#172686=CARTESIAN_POINT('Ctrl Pts',(8.01394098199994,15.2,-7.27481505600001));
#172687=CARTESIAN_POINT('Ctrl Pts',(8.01531570699994,15.2,-7.27714938900001));
#172688=CARTESIAN_POINT('Ctrl Pts',(8.01669141199995,15.2,-7.27948989700002));
#172689=CARTESIAN_POINT('Ctrl Pts',(8.01806808699994,15.2,-7.28183657500002));
#172690=CARTESIAN_POINT('Ctrl Pts',(8.01944571799994,15.2,-7.28418941900002));
#172691=CARTESIAN_POINT('Ctrl Pts',(8.02082429299994,15.2,-7.28654842400001));
#172692=CARTESIAN_POINT('Ctrl Pts',(8.02220379799994,15.2,-7.28891358600002));
#172693=CARTESIAN_POINT('Ctrl Pts',(8.02358422099994,15.2,-7.29128489700001));
#172694=CARTESIAN_POINT('Ctrl Pts',(8.02496554899994,15.2,-7.29366235400001));
#172695=CARTESIAN_POINT('Ctrl Pts',(8.02634777099994,15.2,-7.29604595200002));
#172696=CARTESIAN_POINT('Ctrl Pts',(8.02773087299994,15.2,-7.29843568400002));
#172697=CARTESIAN_POINT('Ctrl Pts',(8.02911484199995,15.2,-7.30083154700001));
#172698=CARTESIAN_POINT('Ctrl Pts',(8.03049966599995,15.2,-7.30323353700002));
#172699=CARTESIAN_POINT('Ctrl Pts',(8.03188533199994,15.2,-7.30564164600001));
#172700=CARTESIAN_POINT('Ctrl Pts',(8.03327182899995,15.2,-7.30805587200001));
#172701=CARTESIAN_POINT('Ctrl Pts',(8.03465914399995,15.2,-7.31047620700001));
#172702=CARTESIAN_POINT('Ctrl Pts',(8.03604726399995,15.2,-7.31290264900001));
#172703=CARTESIAN_POINT('Ctrl Pts',(8.03743617699994,15.2,-7.31533519100001));
#172704=CARTESIAN_POINT('Ctrl Pts',(8.03882586899995,15.2,-7.31777382800002));
#172705=CARTESIAN_POINT('Ctrl Pts',(8.04021633199994,15.2,-7.32021855600002));
#172706=CARTESIAN_POINT('Ctrl Pts',(8.04160754999995,15.2,-7.32266936900002));
#172707=CARTESIAN_POINT('Ctrl Pts',(8.04299951199994,15.2,-7.32512626400001));
#172708=CARTESIAN_POINT('Ctrl Pts',(8.04439220499994,15.2,-7.32758923400001));
#172709=CARTESIAN_POINT('Ctrl Pts',(8.04578561899995,15.2,-7.33005827400002));
#172710=CARTESIAN_POINT('Ctrl Pts',(8.04717973999994,15.2,-7.33253338100001));
#172711=CARTESIAN_POINT('Ctrl Pts',(8.04857455599995,15.2,-7.33501454700002));
#172712=CARTESIAN_POINT('Ctrl Pts',(8.04997005499994,15.2,-7.33750177000001));
#172713=CARTESIAN_POINT('Ctrl Pts',(8.05136622599994,15.2,-7.33999504400002));
#172714=CARTESIAN_POINT('Ctrl Pts',(8.05276305599994,15.2,-7.34249436400002));
#172715=CARTESIAN_POINT('Ctrl Pts',(8.05416053399994,15.2,-7.34499972400001));
#172716=CARTESIAN_POINT('Ctrl Pts',(8.05555864699994,15.2,-7.34751112100002));
#172717=CARTESIAN_POINT('Ctrl Pts',(8.05695738399994,15.2,-7.35002854800002));
#172718=CARTESIAN_POINT('Ctrl Pts',(8.05835673199994,15.2,-7.35255200200001));
#172719=CARTESIAN_POINT('Ctrl Pts',(8.05975667999994,15.2,-7.35508147600001));
#172720=CARTESIAN_POINT('Ctrl Pts',(8.06115721599994,15.2,-7.35761696800001));
#172721=CARTESIAN_POINT('Ctrl Pts',(8.06255832899994,15.2,-7.36015847000001));
#172722=CARTESIAN_POINT('Ctrl Pts',(8.06396000599995,15.2,-7.36270597800001));
#172723=CARTESIAN_POINT('Ctrl Pts',(8.06536223699995,15.2,-7.36525948800002));
#172724=CARTESIAN_POINT('Ctrl Pts',(8.06676500799994,15.2,-7.36781899400002));
#172725=CARTESIAN_POINT('Ctrl Pts',(8.06816830899994,15.2,-7.37038449300002));
#172726=CARTESIAN_POINT('Ctrl Pts',(8.06957212799994,15.2,-7.37295597700002));
#172727=CARTESIAN_POINT('Ctrl Pts',(8.07097645399995,15.2,-7.37553344300002));
#172728=CARTESIAN_POINT('Ctrl Pts',(8.07238127399994,15.2,-7.37811688600001));
#172729=CARTESIAN_POINT('Ctrl Pts',(8.07378657799994,15.2,-7.38070630100002));
#172730=CARTESIAN_POINT('Ctrl Pts',(8.07519235299995,15.2,-7.38330168300001));
#172731=CARTESIAN_POINT('Ctrl Pts',(8.07659858999994,15.2,-7.38590302700001));
#172732=CARTESIAN_POINT('Ctrl Pts',(8.07800527499994,15.2,-7.38851032800002));
#172733=CARTESIAN_POINT('Ctrl Pts',(8.07941239799994,15.2,-7.39112358100002));
#172734=CARTESIAN_POINT('Ctrl Pts',(8.08081994599995,15.2,-7.39374278100002));
#172735=CARTESIAN_POINT('Ctrl Pts',(8.08222790999995,15.2,-7.39636792500002));
#172736=CARTESIAN_POINT('Ctrl Pts',(8.08363627799995,15.2,-7.39899900500002));
#172737=CARTESIAN_POINT('Ctrl Pts',(8.08504503799995,15.2,-7.40163601800001));
#172738=CARTESIAN_POINT('Ctrl Pts',(8.08645417899994,15.2,-7.40427895900002));
#172739=CARTESIAN_POINT('Ctrl Pts',(8.08786368899994,15.2,-7.40692782200002));
#172740=CARTESIAN_POINT('Ctrl Pts',(8.08927355799994,15.2,-7.40958260500002));
#172741=CARTESIAN_POINT('Ctrl Pts',(8.09068377599995,15.2,-7.41224329900002));
#172742=CARTESIAN_POINT('Ctrl Pts',(8.09209432999995,15.2,-7.41490990200001));
#172743=CARTESIAN_POINT('Ctrl Pts',(8.09350520799994,15.2,-7.41758240800002));
#172744=CARTESIAN_POINT('Ctrl Pts',(8.09491640099994,15.2,-7.42026081400001));
#172745=CARTESIAN_POINT('Ctrl Pts',(8.09632789799995,15.2,-7.42294511100001));
#172746=CARTESIAN_POINT('Ctrl Pts',(8.09773968599995,15.2,-7.42563529800002));
#172747=CARTESIAN_POINT('Ctrl Pts',(8.09915175599994,15.2,-7.42833136900002));
#172748=CARTESIAN_POINT('Ctrl Pts',(8.10056409499994,15.2,-7.43103331900001));
#172749=CARTESIAN_POINT('Ctrl Pts',(8.10197669399994,15.2,-7.43374114300002));
#172750=CARTESIAN_POINT('Ctrl Pts',(8.10338954199995,15.2,-7.43645483600002));
#172751=CARTESIAN_POINT('Ctrl Pts',(8.10480262699994,15.2,-7.43917439400001));
#172752=CARTESIAN_POINT('Ctrl Pts',(8.10621593799994,15.2,-7.44189981000002));
#172753=CARTESIAN_POINT('Ctrl Pts',(8.10762946499995,15.2,-7.44463108200001));
#172754=CARTESIAN_POINT('Ctrl Pts',(8.10904319799995,15.2,-7.44736820300002));
#172755=CARTESIAN_POINT('Ctrl Pts',(8.11045712499994,15.2,-7.45011117000002));
#172756=CARTESIAN_POINT('Ctrl Pts',(8.11187123599994,15.2,-7.45285997600002));
#172757=CARTESIAN_POINT('Ctrl Pts',(8.11328551799994,15.2,-7.45561461800002));
#172758=CARTESIAN_POINT('Ctrl Pts',(8.11469996399994,15.2,-7.45837509000002));
#172759=CARTESIAN_POINT('Ctrl Pts',(8.11611456099994,15.2,-7.46114138700002));
#172760=CARTESIAN_POINT('Ctrl Pts',(8.11752929899994,15.2,-7.46391350600002));
#172761=CARTESIAN_POINT('Ctrl Pts',(8.11894416699994,15.2,-7.46669144000002));
#172762=CARTESIAN_POINT('Ctrl Pts',(8.12035915499994,15.2,-7.46947518500002));
#172763=CARTESIAN_POINT('Ctrl Pts',(8.12177425199994,15.2,-7.47226473600002));
#172764=CARTESIAN_POINT('Ctrl Pts',(8.12318944699994,15.2,-7.47506008900002));
#172765=CARTESIAN_POINT('Ctrl Pts',(8.12460473099994,15.2,-7.47786123800001));
#172766=CARTESIAN_POINT('Ctrl Pts',(8.12602009199994,15.2,-7.48066818000002));
#172767=CARTESIAN_POINT('Ctrl Pts',(8.12743552099995,15.2,-7.48348090800001));
#172768=CARTESIAN_POINT('Ctrl Pts',(8.12913410293823,15.2,-7.48686311867713));
#172769=CARTESIAN_POINT('Ctrl Pts',(8.1308327555308,15.2,-7.49025399816146));
#172770=CARTESIAN_POINT('Ctrl Pts',(8.13253145646909,15.2,-7.49365353183857));
#172771=CARTESIAN_POINT('Ctrl Pts',(8.13423018390736,15.2,-7.49706171201332));
#172772=CARTESIAN_POINT('Ctrl Pts',(8.13592892199994,15.2,-7.50047853100002));
#172773=CARTESIAN_POINT('Ctrl Pts',(8.13734453099995,15.2,-7.50333163200001));
#172774=CARTESIAN_POINT('Ctrl Pts',(8.13876012299995,15.2,-7.50619048100001));
#172775=CARTESIAN_POINT('Ctrl Pts',(8.14017569099994,15.2,-7.50905507500002));
#172776=CARTESIAN_POINT('Ctrl Pts',(8.14159122299994,15.2,-7.51192540700002));
#172777=CARTESIAN_POINT('Ctrl Pts',(8.14300670799994,15.2,-7.51480147300001));
#172778=CARTESIAN_POINT('Ctrl Pts',(8.14442213799994,15.2,-7.51768326800001));
#172779=CARTESIAN_POINT('Ctrl Pts',(8.14583750199994,15.2,-7.52057078700001));
#172780=CARTESIAN_POINT('Ctrl Pts',(8.14725278899994,15.2,-7.52346402700002));
#172781=CARTESIAN_POINT('Ctrl Pts',(8.14866798999994,15.2,-7.52636298000001));
#172782=CARTESIAN_POINT('Ctrl Pts',(8.15008309399994,15.2,-7.52926764500002));
#172783=CARTESIAN_POINT('Ctrl Pts',(8.15149809099994,15.2,-7.53217801400002));
#172784=CARTESIAN_POINT('Ctrl Pts',(8.15291297199994,15.2,-7.53509408200002));
#172785=CARTESIAN_POINT('Ctrl Pts',(8.15432772699995,15.2,-7.53801584800001));
#172786=CARTESIAN_POINT('Ctrl Pts',(8.15574234599995,15.2,-7.54094330400001));
#172787=CARTESIAN_POINT('Ctrl Pts',(8.15715681899994,15.2,-7.54387644600002));
#172788=CARTESIAN_POINT('Ctrl Pts',(8.15857113399994,15.2,-7.54681526900002));
#172789=CARTESIAN_POINT('Ctrl Pts',(8.15998528399994,15.2,-7.54975976900001));
#172790=CARTESIAN_POINT('Ctrl Pts',(8.16139925799994,15.2,-7.55270994000002));
#172791=CARTESIAN_POINT('Ctrl Pts',(8.16281304699995,15.2,-7.55566577800002));
#172792=CARTESIAN_POINT('Ctrl Pts',(8.16422663899995,15.2,-7.55862727900002));
#172793=CARTESIAN_POINT('Ctrl Pts',(8.16564002699995,15.2,-7.56159443600002));
#172794=CARTESIAN_POINT('Ctrl Pts',(8.16705319899994,15.2,-7.56456724700002));
#172795=CARTESIAN_POINT('Ctrl Pts',(8.16846614699994,15.2,-7.56754570500001));
#172796=CARTESIAN_POINT('Ctrl Pts',(8.16987885999995,15.2,-7.57052980700001));
#172797=CARTESIAN_POINT('Ctrl Pts',(8.17129132899994,15.2,-7.57351954600002));
#172798=CARTESIAN_POINT('Ctrl Pts',(8.17270354399994,15.2,-7.57651491900001));
#172799=CARTESIAN_POINT('Ctrl Pts',(8.17411549699994,15.2,-7.57951592200002));
#172800=CARTESIAN_POINT('Ctrl Pts',(8.17552717499994,15.2,-7.58252254800002));
#172801=CARTESIAN_POINT('Ctrl Pts',(8.17693857099994,15.2,-7.58553479300001));
#172802=CARTESIAN_POINT('Ctrl Pts',(8.17834967399994,15.2,-7.58855265300002));
#172803=CARTESIAN_POINT('Ctrl Pts',(8.17976047699995,15.2,-7.59157612300001));
#172804=CARTESIAN_POINT('Ctrl Pts',(8.18117096699994,15.2,-7.59460519700002));
#172805=CARTESIAN_POINT('Ctrl Pts',(8.18258113699994,15.2,-7.59763987300002));
#172806=CARTESIAN_POINT('Ctrl Pts',(8.18399097599994,15.2,-7.60068014400002));
#172807=CARTESIAN_POINT('Ctrl Pts',(8.18540047699994,15.2,-7.60372600500002));
#172808=CARTESIAN_POINT('Ctrl Pts',(8.18680962599995,15.2,-7.60677745200002));
#172809=CARTESIAN_POINT('Ctrl Pts',(8.18821841799994,15.2,-7.60983448100002));
#172810=CARTESIAN_POINT('Ctrl Pts',(8.18962684199994,15.2,-7.61289708700001));
#172811=CARTESIAN_POINT('Ctrl Pts',(8.19103488899994,15.2,-7.61596526400002));
#172812=CARTESIAN_POINT('Ctrl Pts',(8.19244254899994,15.2,-7.61903900800001));
#172813=CARTESIAN_POINT('Ctrl Pts',(8.19384981299994,15.2,-7.62211831500001));
#172814=CARTESIAN_POINT('Ctrl Pts',(8.19525667099994,15.2,-7.62520317900002));
#172815=CARTESIAN_POINT('Ctrl Pts',(8.19666311599994,15.2,-7.62829359600002));
#172816=CARTESIAN_POINT('Ctrl Pts',(8.19806913599994,15.2,-7.63138956100001));
#172817=CARTESIAN_POINT('Ctrl Pts',(8.19947472199994,15.2,-7.63449107000002));
#172818=CARTESIAN_POINT('Ctrl Pts',(8.20087986699994,15.2,-7.63759811700002));
#172819=CARTESIAN_POINT('Ctrl Pts',(8.20228455999995,15.2,-7.64071069900002));
#172820=CARTESIAN_POINT('Ctrl Pts',(8.20368879299994,15.2,-7.64382880900002));
#172821=CARTESIAN_POINT('Ctrl Pts',(8.20509255499994,15.2,-7.64695244500002));
#172822=CARTESIAN_POINT('Ctrl Pts',(8.20649583899994,15.2,-7.65008160000002));
#172823=CARTESIAN_POINT('Ctrl Pts',(8.20789863399994,15.2,-7.65321627000001));
#172824=CARTESIAN_POINT('Ctrl Pts',(8.20930093299994,15.2,-7.65635645100001));
#172825=CARTESIAN_POINT('Ctrl Pts',(8.21070272499994,15.2,-7.65950213700001));
#172826=CARTESIAN_POINT('Ctrl Pts',(8.21210400199995,15.2,-7.66265332400001));
#172827=CARTESIAN_POINT('Ctrl Pts',(8.21350475399995,15.2,-7.66581000700001));
#172828=CARTESIAN_POINT('Ctrl Pts',(8.21490497299994,15.2,-7.66897218200001));
#172829=CARTESIAN_POINT('Ctrl Pts',(8.21630465099994,15.2,-7.67213984300002));
#172830=CARTESIAN_POINT('Ctrl Pts',(8.21770377699995,15.2,-7.67531298700002));
#172831=CARTESIAN_POINT('Ctrl Pts',(8.21910234199994,15.2,-7.67849160900001));
#172832=CARTESIAN_POINT('Ctrl Pts',(8.22050033799994,15.2,-7.68167570200001));
#172833=CARTESIAN_POINT('Ctrl Pts',(8.22189775699995,15.2,-7.68486526400002));
#172834=CARTESIAN_POINT('Ctrl Pts',(8.22329458799994,15.2,-7.68806029000002));
#172835=CARTESIAN_POINT('Ctrl Pts',(8.22469082399994,15.2,-7.69126077300001));
#172836=CARTESIAN_POINT('Ctrl Pts',(8.22608645599994,15.2,-7.69446671100001));
#172837=CARTESIAN_POINT('Ctrl Pts',(8.22748147299994,15.2,-7.69767809800002));
#172838=CARTESIAN_POINT('Ctrl Pts',(8.22887586899994,15.2,-7.70089492900001));
#172839=CARTESIAN_POINT('Ctrl Pts',(8.23026963299995,15.2,-7.70411720200002));
#172840=CARTESIAN_POINT('Ctrl Pts',(8.23166275799995,15.2,-7.70734490700002));
#172841=CARTESIAN_POINT('Ctrl Pts',(8.23305523399994,15.2,-7.71057804500002));
#172842=CARTESIAN_POINT('Ctrl Pts',(8.23444705399995,15.2,-7.71381660700002));
#172843=CARTESIAN_POINT('Ctrl Pts',(8.23583820599995,15.2,-7.71706059100002));
#172844=CARTESIAN_POINT('Ctrl Pts',(8.23722868599994,15.2,-7.72030999100001));
#172845=CARTESIAN_POINT('Ctrl Pts',(8.23861848099994,15.2,-7.72356480200001));
#172846=CARTESIAN_POINT('Ctrl Pts',(8.24000758299994,15.2,-7.72682502200002));
#172847=CARTESIAN_POINT('Ctrl Pts',(8.24139598699994,15.2,-7.73009064300001));
#172848=CARTESIAN_POINT('Ctrl Pts',(8.24278367999994,15.2,-7.73336166100002));
#172849=CARTESIAN_POINT('Ctrl Pts',(8.24417065699994,15.2,-7.73663807300002));
#172850=CARTESIAN_POINT('Ctrl Pts',(8.24555690699994,15.2,-7.73991987300001));
#172851=CARTESIAN_POINT('Ctrl Pts',(8.24694242099994,15.2,-7.74320705700001));
#172852=CARTESIAN_POINT('Ctrl Pts',(8.24832719199994,15.2,-7.74649962000002));
#172853=CARTESIAN_POINT('Ctrl Pts',(8.24971121199994,15.2,-7.74979755600001));
#172854=CARTESIAN_POINT('Ctrl Pts',(8.25109447199995,15.2,-7.75310086400002));
#172855=CARTESIAN_POINT('Ctrl Pts',(8.25247696199994,15.2,-7.75640953400002));
#172856=CARTESIAN_POINT('Ctrl Pts',(8.25385867499994,15.2,-7.75972356600001));
#172857=CARTESIAN_POINT('Ctrl Pts',(8.25523960299994,15.2,-7.76304295400001));
#172858=CARTESIAN_POINT('Ctrl Pts',(8.25661973699994,15.2,-7.76636769200002));
#172859=CARTESIAN_POINT('Ctrl Pts',(8.25799906799995,15.2,-7.76969777700002));
#172860=CARTESIAN_POINT('Ctrl Pts',(8.25937758699994,15.2,-7.77303320300001));
#172861=CARTESIAN_POINT('Ctrl Pts',(8.26075528799995,15.2,-7.77637396700002));
#172862=CARTESIAN_POINT('Ctrl Pts',(8.26213216099994,15.2,-7.77972006200002));
#172863=CARTESIAN_POINT('Ctrl Pts',(8.26350819799995,15.2,-7.78307148500001));
#172864=CARTESIAN_POINT('Ctrl Pts',(8.26488339199994,15.2,-7.78642823100002));
#172865=CARTESIAN_POINT('Ctrl Pts',(8.26625773199994,15.2,-7.78979029600002));
#172866=CARTESIAN_POINT('Ctrl Pts',(8.26763121199994,15.2,-7.79315767400002));
#172867=CARTESIAN_POINT('Ctrl Pts',(8.26900382399994,15.2,-7.79653036100001));
#172868=CARTESIAN_POINT('Ctrl Pts',(8.27037555599994,15.2,-7.79990835200002));
#172869=CARTESIAN_POINT('Ctrl Pts',(8.27174640499994,15.2,-7.80329164300002));
#172870=CARTESIAN_POINT('Ctrl Pts',(8.27311635999994,15.2,-7.80668023000001));
#172871=CARTESIAN_POINT('Ctrl Pts',(8.27448541299994,15.2,-7.81007410700001));
#172872=CARTESIAN_POINT('Ctrl Pts',(8.27585355599994,15.2,-7.81347326900002));
#172873=CARTESIAN_POINT('Ctrl Pts',(8.27722078099994,15.2,-7.81687771200002));
#172874=CARTESIAN_POINT('Ctrl Pts',(8.27858707899994,15.2,-7.82028743300001));
#172875=CARTESIAN_POINT('Ctrl Pts',(8.27995244399995,15.2,-7.82370242500001));
#172876=CARTESIAN_POINT('Ctrl Pts',(8.28131686599994,15.2,-7.82712268400001));
#172877=CARTESIAN_POINT('Ctrl Pts',(8.28268033699995,15.2,-7.83054820600002));
#172878=CARTESIAN_POINT('Ctrl Pts',(8.28404284999994,15.2,-7.83397898500001));
#172879=CARTESIAN_POINT('Ctrl Pts',(8.28540439599994,15.2,-7.83741501800002));
#172880=CARTESIAN_POINT('Ctrl Pts',(8.28676496699994,15.2,-7.84085630000002));
#172881=CARTESIAN_POINT('Ctrl Pts',(8.28812455599994,15.2,-7.84430282500002));
#172882=CARTESIAN_POINT('Ctrl Pts',(8.28948315499994,15.2,-7.84775459000001));
#172883=CARTESIAN_POINT('Ctrl Pts',(8.29084075499994,15.2,-7.85121159100001));
#172884=CARTESIAN_POINT('Ctrl Pts',(8.29219734999995,15.2,-7.85467382100002));
#172885=CARTESIAN_POINT('Ctrl Pts',(8.29355293099994,15.2,-7.85814127700001));
#172886=CARTESIAN_POINT('Ctrl Pts',(8.29490748799994,15.2,-7.86161395500002));
#172887=CARTESIAN_POINT('Ctrl Pts',(8.29626101599995,15.2,-7.86509184700002));
#172888=CARTESIAN_POINT('Ctrl Pts',(8.29761350399994,15.2,-7.86857495200002));
#172889=CARTESIAN_POINT('Ctrl Pts',(8.29896494599994,15.2,-7.87206326300002));
#172890=CARTESIAN_POINT('Ctrl Pts',(8.30031533299995,15.2,-7.87555677500002));
#172891=CARTESIAN_POINT('Ctrl Pts',(8.30166465799994,15.2,-7.87905548500002));
#172892=CARTESIAN_POINT('Ctrl Pts',(8.30328256514116,15.2,-7.88326016964724));
#172893=CARTESIAN_POINT('Ctrl Pts',(8.30489885992934,15.2,-7.8874726366764));
#172894=CARTESIAN_POINT('Ctrl Pts',(8.30651352407055,15.2,-7.89169288132363));
#172895=CARTESIAN_POINT('Ctrl Pts',(8.30812654585873,15.2,-7.89592089135279));
#172896=CARTESIAN_POINT('Ctrl Pts',(8.30973790699994,15.2,-7.90015665600002));
#172897=CARTESIAN_POINT('Ctrl Pts',(8.31107958999995,15.2,-7.90369162500002));
#172898=CARTESIAN_POINT('Ctrl Pts',(8.31242014699994,15.2,-7.90723175400001));
#172899=CARTESIAN_POINT('Ctrl Pts',(8.31375956699994,15.2,-7.91077703500001));
#172900=CARTESIAN_POINT('Ctrl Pts',(8.31509784399995,15.2,-7.91432746600002));
#172901=CARTESIAN_POINT('Ctrl Pts',(8.31643496899994,15.2,-7.91788304100002));
#172902=CARTESIAN_POINT('Ctrl Pts',(8.31777093699994,15.2,-7.92144375600002));
#172903=CARTESIAN_POINT('Ctrl Pts',(8.31910574599994,15.2,-7.92500961100002));
#172904=CARTESIAN_POINT('Ctrl Pts',(8.32043939299994,15.2,-7.92858060400001));
#172905=CARTESIAN_POINT('Ctrl Pts',(8.32150538099994,15.2,-7.93144150700002));
#172906=CARTESIAN_POINT('Ctrl Pts',(8.32230434799994,15.2,-7.93358949600002));
#172907=CARTESIAN_POINT('Ctrl Pts',(8.32283676099994,15.2,-7.93502251600002));
#172908=CARTESIAN_POINT('Ctrl Pts',(8.32310290799994,15.2,-7.93573928300002));
#172909=CARTESIAN_POINT('Ctrl Pts',(7.01216898599994,15.2,-7.64657512400002));
#172910=CARTESIAN_POINT('Ctrl Pts',(7.01216898599994,11.6,-7.64657512400002));
#172911=CARTESIAN_POINT('Ctrl Pts',(7.01229743599994,15.2,-7.64669302600002));
#172912=CARTESIAN_POINT('Ctrl Pts',(7.01229743599994,11.6,-7.64669302600002));
#172913=CARTESIAN_POINT('Ctrl Pts',(7.01255888299994,15.2,-7.64693288600002));
#172914=CARTESIAN_POINT('Ctrl Pts',(7.01255888299994,11.6,-7.64693288600002));
#172915=CARTESIAN_POINT('Ctrl Pts',(7.01295521699994,15.2,-7.64729613400001));
#172916=CARTESIAN_POINT('Ctrl Pts',(7.01295521699994,11.6,-7.64729613400001));
#172917=CARTESIAN_POINT('Ctrl Pts',(7.01348947999994,15.2,-7.64778506600001));
#172918=CARTESIAN_POINT('Ctrl Pts',(7.01348947999994,11.6,-7.64778506600001));
#172919=CARTESIAN_POINT('Ctrl Pts',(7.01416585899994,15.2,-7.64840281600002));
#172920=CARTESIAN_POINT('Ctrl Pts',(7.01416585899994,11.6,-7.64840281600002));
#172921=CARTESIAN_POINT('Ctrl Pts',(7.01485382999994,15.2,-7.64902988900002));
#172922=CARTESIAN_POINT('Ctrl Pts',(7.01485382999994,11.6,-7.64902988900002));
#172923=CARTESIAN_POINT('Ctrl Pts',(7.01554946899994,15.2,-7.64966267400002));
#172924=CARTESIAN_POINT('Ctrl Pts',(7.01554946899994,11.6,-7.64966267400002));
#172925=CARTESIAN_POINT('Ctrl Pts',(7.01625276599994,15.2,-7.65030114000002));
#172926=CARTESIAN_POINT('Ctrl Pts',(7.01625276599994,11.6,-7.65030114000002));
#172927=CARTESIAN_POINT('Ctrl Pts',(7.01696371599994,15.2,-7.65094525300002));
#172928=CARTESIAN_POINT('Ctrl Pts',(7.01696371599994,11.6,-7.65094525300002));
#172929=CARTESIAN_POINT('Ctrl Pts',(7.01768230799994,15.2,-7.65159498400001));
#172930=CARTESIAN_POINT('Ctrl Pts',(7.01768230799994,11.6,-7.65159498400001));
#172931=CARTESIAN_POINT('Ctrl Pts',(7.01840853599994,15.2,-7.65225030200002));
#172932=CARTESIAN_POINT('Ctrl Pts',(7.01840853599994,11.6,-7.65225030200002));
#172933=CARTESIAN_POINT('Ctrl Pts',(7.01914239299994,15.2,-7.65291117500002));
#172934=CARTESIAN_POINT('Ctrl Pts',(7.01914239299994,11.6,-7.65291117500002));
#172935=CARTESIAN_POINT('Ctrl Pts',(7.01988386999994,15.2,-7.65357757300002));
#172936=CARTESIAN_POINT('Ctrl Pts',(7.01988386999994,11.6,-7.65357757300002));
#172937=CARTESIAN_POINT('Ctrl Pts',(7.02063295999994,15.2,-7.65424946400002));
#172938=CARTESIAN_POINT('Ctrl Pts',(7.02063295999994,11.6,-7.65424946400002));
#172939=CARTESIAN_POINT('Ctrl Pts',(7.02138965599994,15.2,-7.65492682000002));
#172940=CARTESIAN_POINT('Ctrl Pts',(7.02138965599994,11.6,-7.65492682000002));
#172941=CARTESIAN_POINT('Ctrl Pts',(7.02215394899994,15.2,-7.65560960700002));
#172942=CARTESIAN_POINT('Ctrl Pts',(7.02215394899994,11.6,-7.65560960700002));
#172943=CARTESIAN_POINT('Ctrl Pts',(7.02292583299994,15.2,-7.65629779800002));
#172944=CARTESIAN_POINT('Ctrl Pts',(7.02292583299994,11.6,-7.65629779800002));
#172945=CARTESIAN_POINT('Ctrl Pts',(7.02370529899994,15.2,-7.65699136200002));
#172946=CARTESIAN_POINT('Ctrl Pts',(7.02370529899994,11.6,-7.65699136200002));
#172947=CARTESIAN_POINT('Ctrl Pts',(7.02449234199994,15.2,-7.65769026900001));
#172948=CARTESIAN_POINT('Ctrl Pts',(7.02449234199994,11.6,-7.65769026900001));
#172949=CARTESIAN_POINT('Ctrl Pts',(7.02528695099994,15.2,-7.65839448900002));
#172950=CARTESIAN_POINT('Ctrl Pts',(7.02528695099994,11.6,-7.65839448900002));
#172951=CARTESIAN_POINT('Ctrl Pts',(7.02608912099994,15.2,-7.65910399200001));
#172952=CARTESIAN_POINT('Ctrl Pts',(7.02608912099994,11.6,-7.65910399200001));
#172953=CARTESIAN_POINT('Ctrl Pts',(7.02689884399994,15.2,-7.65981875000002));
#172954=CARTESIAN_POINT('Ctrl Pts',(7.02689884399994,11.6,-7.65981875000002));
#172955=CARTESIAN_POINT('Ctrl Pts',(7.02771611299994,15.2,-7.66053873300002));
#172956=CARTESIAN_POINT('Ctrl Pts',(7.02771611299994,11.6,-7.66053873300002));
#172957=CARTESIAN_POINT('Ctrl Pts',(7.02854091899995,15.2,-7.66126391100002));
#172958=CARTESIAN_POINT('Ctrl Pts',(7.02854091899995,11.6,-7.66126391100002));
#172959=CARTESIAN_POINT('Ctrl Pts',(7.02937325699994,15.2,-7.66199425500002));
#172960=CARTESIAN_POINT('Ctrl Pts',(7.02937325699994,11.6,-7.66199425500002));
#172961=CARTESIAN_POINT('Ctrl Pts',(7.03021311799994,15.2,-7.66272973700002));
#172962=CARTESIAN_POINT('Ctrl Pts',(7.03021311799994,11.6,-7.66272973700002));
#172963=CARTESIAN_POINT('Ctrl Pts',(7.03106049599994,15.2,-7.66347032800001));
#172964=CARTESIAN_POINT('Ctrl Pts',(7.03106049599994,11.6,-7.66347032800001));
#172965=CARTESIAN_POINT('Ctrl Pts',(7.03191538199994,15.2,-7.66421599900001));
#172966=CARTESIAN_POINT('Ctrl Pts',(7.03191538199994,11.6,-7.66421599900001));
#172967=CARTESIAN_POINT('Ctrl Pts',(7.03277776899994,15.2,-7.66496672300002));
#172968=CARTESIAN_POINT('Ctrl Pts',(7.03277776899994,11.6,-7.66496672300002));
#172969=CARTESIAN_POINT('Ctrl Pts',(7.03364765099994,15.2,-7.66572247000001));
#172970=CARTESIAN_POINT('Ctrl Pts',(7.03364765099994,11.6,-7.66572247000001));
#172971=CARTESIAN_POINT('Ctrl Pts',(7.03452502099994,15.2,-7.66648321100002));
#172972=CARTESIAN_POINT('Ctrl Pts',(7.03452502099994,11.6,-7.66648321100002));
#172973=CARTESIAN_POINT('Ctrl Pts',(7.03540986899994,15.2,-7.66724892000001));
#172974=CARTESIAN_POINT('Ctrl Pts',(7.03540986899994,11.6,-7.66724892000001));
#172975=CARTESIAN_POINT('Ctrl Pts',(7.03630218999994,15.2,-7.66801956900002));
#172976=CARTESIAN_POINT('Ctrl Pts',(7.03630218999994,11.6,-7.66801956900002));
#172977=CARTESIAN_POINT('Ctrl Pts',(7.03720197799995,15.2,-7.66879512800001));
#172978=CARTESIAN_POINT('Ctrl Pts',(7.03720197799995,11.6,-7.66879512800001));
#172979=CARTESIAN_POINT('Ctrl Pts',(7.03810922299994,15.2,-7.66957557200002));
#172980=CARTESIAN_POINT('Ctrl Pts',(7.03810922299994,11.6,-7.66957557200002));
#172981=CARTESIAN_POINT('Ctrl Pts',(7.03902391899994,15.2,-7.67036087200001));
#172982=CARTESIAN_POINT('Ctrl Pts',(7.03902391899994,11.6,-7.67036087200001));
#172983=CARTESIAN_POINT('Ctrl Pts',(7.03994605999994,15.2,-7.67115100000002));
#172984=CARTESIAN_POINT('Ctrl Pts',(7.03994605999994,11.6,-7.67115100000002));
#172985=CARTESIAN_POINT('Ctrl Pts',(7.04087563899994,15.2,-7.67194593000001));
#172986=CARTESIAN_POINT('Ctrl Pts',(7.04087563899994,11.6,-7.67194593000001));
#172987=CARTESIAN_POINT('Ctrl Pts',(7.04181264599994,15.2,-7.67274563400001));
#172988=CARTESIAN_POINT('Ctrl Pts',(7.04181264599994,11.6,-7.67274563400001));
#172989=CARTESIAN_POINT('Ctrl Pts',(7.04275707599994,15.2,-7.67355008500001));
#172990=CARTESIAN_POINT('Ctrl Pts',(7.04275707599994,11.6,-7.67355008500001));
#172991=CARTESIAN_POINT('Ctrl Pts',(7.04370892199995,15.2,-7.67435925700001));
#172992=CARTESIAN_POINT('Ctrl Pts',(7.04370892199995,11.6,-7.67435925700001));
#172993=CARTESIAN_POINT('Ctrl Pts',(7.04466817699994,15.2,-7.67517312200001));
#172994=CARTESIAN_POINT('Ctrl Pts',(7.04466817699994,11.6,-7.67517312200001));
#172995=CARTESIAN_POINT('Ctrl Pts',(7.04563483299994,15.2,-7.67599165500001));
#172996=CARTESIAN_POINT('Ctrl Pts',(7.04563483299994,11.6,-7.67599165500001));
#172997=CARTESIAN_POINT('Ctrl Pts',(7.04660888399994,15.2,-7.67681482700001));
#172998=CARTESIAN_POINT('Ctrl Pts',(7.04660888399994,11.6,-7.67681482700001));
#172999=CARTESIAN_POINT('Ctrl Pts',(7.04759032399994,15.2,-7.67764261300002));
#173000=CARTESIAN_POINT('Ctrl Pts',(7.04759032399994,11.6,-7.67764261300002));
#173001=CARTESIAN_POINT('Ctrl Pts',(7.04857914399994,15.2,-7.67847498700001));
#173002=CARTESIAN_POINT('Ctrl Pts',(7.04857914399994,11.6,-7.67847498700001));
#173003=CARTESIAN_POINT('Ctrl Pts',(7.04957533699995,15.2,-7.67931192200002));
#173004=CARTESIAN_POINT('Ctrl Pts',(7.04957533699995,11.6,-7.67931192200002));
#173005=CARTESIAN_POINT('Ctrl Pts',(7.05057889899994,15.2,-7.68015339300002));
#173006=CARTESIAN_POINT('Ctrl Pts',(7.05057889899994,11.6,-7.68015339300002));
#173007=CARTESIAN_POINT('Ctrl Pts',(7.05158981999995,15.2,-7.68099937300001));
#173008=CARTESIAN_POINT('Ctrl Pts',(7.05158981999995,11.6,-7.68099937300001));
#173009=CARTESIAN_POINT('Ctrl Pts',(7.05260809399994,15.2,-7.68184983700002));
#173010=CARTESIAN_POINT('Ctrl Pts',(7.05260809399994,11.6,-7.68184983700002));
#173011=CARTESIAN_POINT('Ctrl Pts',(7.05363371299994,15.2,-7.68270475700002));
#173012=CARTESIAN_POINT('Ctrl Pts',(7.05363371299994,11.6,-7.68270475700002));
#173013=CARTESIAN_POINT('Ctrl Pts',(7.05466667299994,15.2,-7.68356411000001));
#173014=CARTESIAN_POINT('Ctrl Pts',(7.05466667299994,11.6,-7.68356411000001));
#173015=CARTESIAN_POINT('Ctrl Pts',(7.05570696599994,15.2,-7.68442787000001));
#173016=CARTESIAN_POINT('Ctrl Pts',(7.05570696599994,11.6,-7.68442787000001));
#173017=CARTESIAN_POINT('Ctrl Pts',(7.05675458399995,15.2,-7.68529601200001));
#173018=CARTESIAN_POINT('Ctrl Pts',(7.05675458399995,11.6,-7.68529601200001));
#173019=CARTESIAN_POINT('Ctrl Pts',(7.05780952099994,15.2,-7.68616850900001));
#173020=CARTESIAN_POINT('Ctrl Pts',(7.05780952099994,11.6,-7.68616850900001));
#173021=CARTESIAN_POINT('Ctrl Pts',(7.05887177099994,15.2,-7.68704533700002));
#173022=CARTESIAN_POINT('Ctrl Pts',(7.05887177099994,11.6,-7.68704533700002));
#173023=CARTESIAN_POINT('Ctrl Pts',(7.05994132499994,15.2,-7.68792647200002));
#173024=CARTESIAN_POINT('Ctrl Pts',(7.05994132499994,11.6,-7.68792647200002));
#173025=CARTESIAN_POINT('Ctrl Pts',(7.06101817799994,15.2,-7.68881188600002));
#173026=CARTESIAN_POINT('Ctrl Pts',(7.06101817799994,11.6,-7.68881188600002));
#173027=CARTESIAN_POINT('Ctrl Pts',(7.06210232399994,15.2,-7.68970155800002));
#173028=CARTESIAN_POINT('Ctrl Pts',(7.06210232399994,11.6,-7.68970155800002));
#173029=CARTESIAN_POINT('Ctrl Pts',(7.06319375299994,15.2,-7.69059545900002));
#173030=CARTESIAN_POINT('Ctrl Pts',(7.06319375299994,11.6,-7.69059545900002));
#173031=CARTESIAN_POINT('Ctrl Pts',(7.06429246299995,15.2,-7.69149356800002));
#173032=CARTESIAN_POINT('Ctrl Pts',(7.06429246299995,11.6,-7.69149356800002));
#173033=CARTESIAN_POINT('Ctrl Pts',(7.06539844399994,15.2,-7.69239585900002));
#173034=CARTESIAN_POINT('Ctrl Pts',(7.06539844399994,11.6,-7.69239585900002));
#173035=CARTESIAN_POINT('Ctrl Pts',(7.06651168899994,15.2,-7.69330230800002));
#173036=CARTESIAN_POINT('Ctrl Pts',(7.06651168899994,11.6,-7.69330230800002));
#173037=CARTESIAN_POINT('Ctrl Pts',(7.06763219399994,15.2,-7.69421289100002));
#173038=CARTESIAN_POINT('Ctrl Pts',(7.06763219399994,11.6,-7.69421289100002));
#173039=CARTESIAN_POINT('Ctrl Pts',(7.06875994999994,15.2,-7.69512758300002));
#173040=CARTESIAN_POINT('Ctrl Pts',(7.06875994999994,11.6,-7.69512758300002));
#173041=CARTESIAN_POINT('Ctrl Pts',(7.06989495099994,15.2,-7.69604636000001));
#173042=CARTESIAN_POINT('Ctrl Pts',(7.06989495099994,11.6,-7.69604636000001));
#173043=CARTESIAN_POINT('Ctrl Pts',(7.07103718999995,15.2,-7.69696919900002));
#173044=CARTESIAN_POINT('Ctrl Pts',(7.07103718999995,11.6,-7.69696919900002));
#173045=CARTESIAN_POINT('Ctrl Pts',(7.07218666199994,15.2,-7.69789607500002));
#173046=CARTESIAN_POINT('Ctrl Pts',(7.07218666199994,11.6,-7.69789607500002));
#173047=CARTESIAN_POINT('Ctrl Pts',(7.07334335899994,15.2,-7.69882696300002));
#173048=CARTESIAN_POINT('Ctrl Pts',(7.07334335899994,11.6,-7.69882696300002));
#173049=CARTESIAN_POINT('Ctrl Pts',(7.07450727399995,15.2,-7.69976184200001));
#173050=CARTESIAN_POINT('Ctrl Pts',(7.07450727399995,11.6,-7.69976184200001));
#173051=CARTESIAN_POINT('Ctrl Pts',(7.07567840199994,15.2,-7.70070068800001));
#173052=CARTESIAN_POINT('Ctrl Pts',(7.07567840199994,11.6,-7.70070068800001));
#173053=CARTESIAN_POINT('Ctrl Pts',(7.07685673499994,15.2,-7.70164347600002));
#173054=CARTESIAN_POINT('Ctrl Pts',(7.07685673499994,11.6,-7.70164347600002));
#173055=CARTESIAN_POINT('Ctrl Pts',(7.07804226699994,15.2,-7.70259018400001));
#173056=CARTESIAN_POINT('Ctrl Pts',(7.07804226699994,11.6,-7.70259018400001));
#173057=CARTESIAN_POINT('Ctrl Pts',(7.07923499199994,15.2,-7.70354078700001));
#173058=CARTESIAN_POINT('Ctrl Pts',(7.07923499199994,11.6,-7.70354078700001));
#173059=CARTESIAN_POINT('Ctrl Pts',(7.08043490299994,15.2,-7.70449526500002));
#173060=CARTESIAN_POINT('Ctrl Pts',(7.08043490299994,11.6,-7.70449526500002));
#173061=CARTESIAN_POINT('Ctrl Pts',(7.08164199399994,15.2,-7.70545359200002));
#173062=CARTESIAN_POINT('Ctrl Pts',(7.08164199399994,11.6,-7.70545359200002));
#173063=CARTESIAN_POINT('Ctrl Pts',(7.08285625699994,15.2,-7.70641574500001));
#173064=CARTESIAN_POINT('Ctrl Pts',(7.08285625699994,11.6,-7.70641574500001));
#173065=CARTESIAN_POINT('Ctrl Pts',(7.08407768699994,15.2,-7.70738170300002));
#173066=CARTESIAN_POINT('Ctrl Pts',(7.08407768699994,11.6,-7.70738170300002));
#173067=CARTESIAN_POINT('Ctrl Pts',(7.08530627699994,15.2,-7.70835144200002));
#173068=CARTESIAN_POINT('Ctrl Pts',(7.08530627699994,11.6,-7.70835144200002));
#173069=CARTESIAN_POINT('Ctrl Pts',(7.08654202199994,15.2,-7.70932493900002));
#173070=CARTESIAN_POINT('Ctrl Pts',(7.08654202199994,11.6,-7.70932493900002));
#173071=CARTESIAN_POINT('Ctrl Pts',(7.08778491199994,15.2,-7.71030217200002));
#173072=CARTESIAN_POINT('Ctrl Pts',(7.08778491199994,11.6,-7.71030217200002));
#173073=CARTESIAN_POINT('Ctrl Pts',(7.08903494499994,15.2,-7.71128311800001));
#173074=CARTESIAN_POINT('Ctrl Pts',(7.08903494499994,11.6,-7.71128311800001));
#173075=CARTESIAN_POINT('Ctrl Pts',(7.09029211099995,15.2,-7.71226775600002));
#173076=CARTESIAN_POINT('Ctrl Pts',(7.09029211099995,11.6,-7.71226775600002));
#173077=CARTESIAN_POINT('Ctrl Pts',(7.09155640599994,15.2,-7.71325606100002));
#173078=CARTESIAN_POINT('Ctrl Pts',(7.09155640599994,11.6,-7.71325606100002));
#173079=CARTESIAN_POINT('Ctrl Pts',(7.09282782099995,15.2,-7.71424801400002));
#173080=CARTESIAN_POINT('Ctrl Pts',(7.09282782099995,11.6,-7.71424801400002));
#173081=CARTESIAN_POINT('Ctrl Pts',(7.09410635299994,15.2,-7.71524359000002));
#173082=CARTESIAN_POINT('Ctrl Pts',(7.09410635299994,11.6,-7.71524359000002));
#173083=CARTESIAN_POINT('Ctrl Pts',(7.09539199299994,15.2,-7.71624276900001));
#173084=CARTESIAN_POINT('Ctrl Pts',(7.09539199299994,11.6,-7.71624276900001));
#173085=CARTESIAN_POINT('Ctrl Pts',(7.09668473699994,15.2,-7.71724552700002));
#173086=CARTESIAN_POINT('Ctrl Pts',(7.09668473699994,11.6,-7.71724552700002));
#173087=CARTESIAN_POINT('Ctrl Pts',(7.09798457499994,15.2,-7.71825184400001));
#173088=CARTESIAN_POINT('Ctrl Pts',(7.09798457499994,11.6,-7.71825184400001));
#173089=CARTESIAN_POINT('Ctrl Pts',(7.09929150499994,15.2,-7.71926169700001));
#173090=CARTESIAN_POINT('Ctrl Pts',(7.09929150499994,11.6,-7.71926169700001));
#173091=CARTESIAN_POINT('Ctrl Pts',(7.10060551799994,15.2,-7.72027506500002));
#173092=CARTESIAN_POINT('Ctrl Pts',(7.10060551799994,11.6,-7.72027506500002));
#173093=CARTESIAN_POINT('Ctrl Pts',(7.10192660699994,15.2,-7.72129192600002));
#173094=CARTESIAN_POINT('Ctrl Pts',(7.10192660699994,11.6,-7.72129192600002));
#173095=CARTESIAN_POINT('Ctrl Pts',(7.10325476799994,15.2,-7.72231225700001));
#173096=CARTESIAN_POINT('Ctrl Pts',(7.10325476799994,11.6,-7.72231225700001));
#173097=CARTESIAN_POINT('Ctrl Pts',(7.10458999399994,15.2,-7.72333604000002));
#173098=CARTESIAN_POINT('Ctrl Pts',(7.10458999399994,11.6,-7.72333604000002));
#173099=CARTESIAN_POINT('Ctrl Pts',(7.10593227899994,15.2,-7.72436325100001));
#173100=CARTESIAN_POINT('Ctrl Pts',(7.10593227899994,11.6,-7.72436325100001));
#173101=CARTESIAN_POINT('Ctrl Pts',(7.10728161499994,15.2,-7.72539386900001));
#173102=CARTESIAN_POINT('Ctrl Pts',(7.10728161499994,11.6,-7.72539386900001));
#173103=CARTESIAN_POINT('Ctrl Pts',(7.10863799699994,15.2,-7.72642787400001));
#173104=CARTESIAN_POINT('Ctrl Pts',(7.10863799699994,11.6,-7.72642787400001));
#173105=CARTESIAN_POINT('Ctrl Pts',(7.11000141999994,15.2,-7.72746524300001));
#173106=CARTESIAN_POINT('Ctrl Pts',(7.11000141999994,11.6,-7.72746524300001));
#173107=CARTESIAN_POINT('Ctrl Pts',(7.11137187499994,15.2,-7.72850595600002));
#173108=CARTESIAN_POINT('Ctrl Pts',(7.11137187499994,11.6,-7.72850595600002));
#173109=CARTESIAN_POINT('Ctrl Pts',(7.11274935899994,15.2,-7.72954999200002));
#173110=CARTESIAN_POINT('Ctrl Pts',(7.11274935899994,11.6,-7.72954999200002));
#173111=CARTESIAN_POINT('Ctrl Pts',(7.11413386299995,15.2,-7.73059733100002));
#173112=CARTESIAN_POINT('Ctrl Pts',(7.11413386299995,11.6,-7.73059733100002));
#173113=CARTESIAN_POINT('Ctrl Pts',(7.11552538199994,15.2,-7.73164795100002));
#173114=CARTESIAN_POINT('Ctrl Pts',(7.11552538199994,11.6,-7.73164795100002));
#173115=CARTESIAN_POINT('Ctrl Pts',(7.11692391099994,15.2,-7.73270183100002));
#173116=CARTESIAN_POINT('Ctrl Pts',(7.11692391099994,11.6,-7.73270183100002));
#173117=CARTESIAN_POINT('Ctrl Pts',(7.11832944099994,15.2,-7.73375895200001));
#173118=CARTESIAN_POINT('Ctrl Pts',(7.11832944099994,11.6,-7.73375895200001));
#173119=CARTESIAN_POINT('Ctrl Pts',(7.11974196799994,15.2,-7.73481929100001));
#173120=CARTESIAN_POINT('Ctrl Pts',(7.11974196799994,11.6,-7.73481929100001));
#173121=CARTESIAN_POINT('Ctrl Pts',(7.12116148499994,15.2,-7.73588283000001));
#173122=CARTESIAN_POINT('Ctrl Pts',(7.12116148499994,11.6,-7.73588283000001));
#173123=CARTESIAN_POINT('Ctrl Pts',(7.12258798699994,15.2,-7.73694954800002));
#173124=CARTESIAN_POINT('Ctrl Pts',(7.12258798699994,11.6,-7.73694954800002));
#173125=CARTESIAN_POINT('Ctrl Pts',(7.12402146699994,15.2,-7.73801942300001));
#173126=CARTESIAN_POINT('Ctrl Pts',(7.12402146699994,11.6,-7.73801942300001));
#173127=CARTESIAN_POINT('Ctrl Pts',(7.12546191799994,15.2,-7.73909243600002));
#173128=CARTESIAN_POINT('Ctrl Pts',(7.12546191799994,11.6,-7.73909243600002));
#173129=CARTESIAN_POINT('Ctrl Pts',(7.12690933599994,15.2,-7.74016856800002));
#173130=CARTESIAN_POINT('Ctrl Pts',(7.12690933599994,11.6,-7.74016856800002));
#173131=CARTESIAN_POINT('Ctrl Pts',(7.12836371399994,15.2,-7.74124779700001));
#173132=CARTESIAN_POINT('Ctrl Pts',(7.12836371399994,11.6,-7.74124779700001));
#173133=CARTESIAN_POINT('Ctrl Pts',(7.12982504399994,15.2,-7.74233010400001));
#173134=CARTESIAN_POINT('Ctrl Pts',(7.12982504399994,11.6,-7.74233010400001));
#173135=CARTESIAN_POINT('Ctrl Pts',(7.13129332299994,15.2,-7.74341546800001));
#173136=CARTESIAN_POINT('Ctrl Pts',(7.13129332299994,11.6,-7.74341546800001));
#173137=CARTESIAN_POINT('Ctrl Pts',(7.13276854299994,15.2,-7.74450387100002));
#173138=CARTESIAN_POINT('Ctrl Pts',(7.13276854299994,11.6,-7.74450387100002));
#173139=CARTESIAN_POINT('Ctrl Pts',(7.13425069899994,15.2,-7.74559529100002));
#173140=CARTESIAN_POINT('Ctrl Pts',(7.13425069899994,11.6,-7.74559529100002));
#173141=CARTESIAN_POINT('Ctrl Pts',(7.13573978399995,15.2,-7.74668971000001));
#173142=CARTESIAN_POINT('Ctrl Pts',(7.13573978399995,11.6,-7.74668971000001));
#173143=CARTESIAN_POINT('Ctrl Pts',(7.13723579299994,15.2,-7.74778710800001));
#173144=CARTESIAN_POINT('Ctrl Pts',(7.13723579299994,11.6,-7.74778710800001));
#173145=CARTESIAN_POINT('Ctrl Pts',(7.13873871899994,15.2,-7.74888746400002));
#173146=CARTESIAN_POINT('Ctrl Pts',(7.13873871899994,11.6,-7.74888746400002));
#173147=CARTESIAN_POINT('Ctrl Pts',(7.14024855599994,15.2,-7.74999076200002));
#173148=CARTESIAN_POINT('Ctrl Pts',(7.14024855599994,11.6,-7.74999076200002));
#173149=CARTESIAN_POINT('Ctrl Pts',(7.14176529899994,15.2,-7.75109697800002));
#173150=CARTESIAN_POINT('Ctrl Pts',(7.14176529899994,11.6,-7.75109697800002));
#173151=CARTESIAN_POINT('Ctrl Pts',(7.14328894099994,15.2,-7.75220609600002));
#173152=CARTESIAN_POINT('Ctrl Pts',(7.14328894099994,11.6,-7.75220609600002));
#173153=CARTESIAN_POINT('Ctrl Pts',(7.14481947699994,15.2,-7.75331809500001));
#173154=CARTESIAN_POINT('Ctrl Pts',(7.14481947699994,11.6,-7.75331809500001));
#173155=CARTESIAN_POINT('Ctrl Pts',(7.14635689999994,15.2,-7.75443295600001));
#173156=CARTESIAN_POINT('Ctrl Pts',(7.14635689999994,11.6,-7.75443295600001));
#173157=CARTESIAN_POINT('Ctrl Pts',(7.14790120399994,15.2,-7.75555066200001));
#173158=CARTESIAN_POINT('Ctrl Pts',(7.14790120399994,11.6,-7.75555066200001));
#173159=CARTESIAN_POINT('Ctrl Pts',(7.14945238399994,15.2,-7.75667119200002));
#173160=CARTESIAN_POINT('Ctrl Pts',(7.14945238399994,11.6,-7.75667119200002));
#173161=CARTESIAN_POINT('Ctrl Pts',(7.15101043299994,15.2,-7.75779452500001));
#173162=CARTESIAN_POINT('Ctrl Pts',(7.15101043299994,11.6,-7.75779452500001));
#173163=CARTESIAN_POINT('Ctrl Pts',(7.15257534599994,15.2,-7.75892064600002));
#173164=CARTESIAN_POINT('Ctrl Pts',(7.15257534599994,11.6,-7.75892064600002));
#173165=CARTESIAN_POINT('Ctrl Pts',(7.15414711699994,15.2,-7.76004953400002));
#173166=CARTESIAN_POINT('Ctrl Pts',(7.15414711699994,11.6,-7.76004953400002));
#173167=CARTESIAN_POINT('Ctrl Pts',(7.15572573899995,15.2,-7.76118117200002));
#173168=CARTESIAN_POINT('Ctrl Pts',(7.15572573899995,11.6,-7.76118117200002));
#173169=CARTESIAN_POINT('Ctrl Pts',(7.15731120799994,15.2,-7.76231553800002));
#173170=CARTESIAN_POINT('Ctrl Pts',(7.15731120799994,11.6,-7.76231553800002));
#173171=CARTESIAN_POINT('Ctrl Pts',(7.15890351499994,15.2,-7.76345261600002));
#173172=CARTESIAN_POINT('Ctrl Pts',(7.15890351499994,11.6,-7.76345261600002));
#173173=CARTESIAN_POINT('Ctrl Pts',(7.16050265799994,15.2,-7.76459238700002));
#173174=CARTESIAN_POINT('Ctrl Pts',(7.16050265799994,11.6,-7.76459238700002));
#173175=CARTESIAN_POINT('Ctrl Pts',(7.16210862799994,15.2,-7.76573483100002));
#173176=CARTESIAN_POINT('Ctrl Pts',(7.16210862799994,11.6,-7.76573483100002));
#173177=CARTESIAN_POINT('Ctrl Pts',(7.16372142099994,15.2,-7.76687993200002));
#173178=CARTESIAN_POINT('Ctrl Pts',(7.16372142099994,11.6,-7.76687993200002));
#173179=CARTESIAN_POINT('Ctrl Pts',(7.16534102999994,15.2,-7.76802767000002));
#173180=CARTESIAN_POINT('Ctrl Pts',(7.16534102999994,11.6,-7.76802767000002));
#173181=CARTESIAN_POINT('Ctrl Pts',(7.16696744899994,15.2,-7.76917802700002));
#173182=CARTESIAN_POINT('Ctrl Pts',(7.16696744899994,11.6,-7.76917802700002));
#173183=CARTESIAN_POINT('Ctrl Pts',(7.16860067299994,15.2,-7.77033098400001));
#173184=CARTESIAN_POINT('Ctrl Pts',(7.16860067299994,11.6,-7.77033098400001));
#173185=CARTESIAN_POINT('Ctrl Pts',(7.17024069599994,15.2,-7.77148652400002));
#173186=CARTESIAN_POINT('Ctrl Pts',(7.17024069599994,11.6,-7.77148652400002));
#173187=CARTESIAN_POINT('Ctrl Pts',(7.17188751299994,15.2,-7.77264462900002));
#173188=CARTESIAN_POINT('Ctrl Pts',(7.17188751299994,11.6,-7.77264462900002));
#173189=CARTESIAN_POINT('Ctrl Pts',(7.17354111499994,15.2,-7.77380527900001));
#173190=CARTESIAN_POINT('Ctrl Pts',(7.17354111499994,11.6,-7.77380527900001));
#173191=CARTESIAN_POINT('Ctrl Pts',(7.17520149999994,15.2,-7.77496845800002));
#173192=CARTESIAN_POINT('Ctrl Pts',(7.17520149999994,11.6,-7.77496845800002));
#173193=CARTESIAN_POINT('Ctrl Pts',(7.17686865999994,15.2,-7.77613414800002));
#173194=CARTESIAN_POINT('Ctrl Pts',(7.17686865999994,11.6,-7.77613414800002));
#173195=CARTESIAN_POINT('Ctrl Pts',(7.17854258999994,15.2,-7.77730233000002));
#173196=CARTESIAN_POINT('Ctrl Pts',(7.17854258999994,11.6,-7.77730233000002));
#173197=CARTESIAN_POINT('Ctrl Pts',(7.18022328299995,15.2,-7.77847298600002));
#173198=CARTESIAN_POINT('Ctrl Pts',(7.18022328299995,11.6,-7.77847298600002));
#173199=CARTESIAN_POINT('Ctrl Pts',(7.18191073399994,15.2,-7.77964610000001));
#173200=CARTESIAN_POINT('Ctrl Pts',(7.18191073399994,11.6,-7.77964610000001));
#173201=CARTESIAN_POINT('Ctrl Pts',(7.18360493799994,15.2,-7.78082165300002));
#173202=CARTESIAN_POINT('Ctrl Pts',(7.18360493799994,11.6,-7.78082165300002));
#173203=CARTESIAN_POINT('Ctrl Pts',(7.18530588899994,15.2,-7.78199962700001));
#173204=CARTESIAN_POINT('Ctrl Pts',(7.18530588899994,11.6,-7.78199962700001));
#173205=CARTESIAN_POINT('Ctrl Pts',(7.18701357999994,15.2,-7.78318000600001));
#173206=CARTESIAN_POINT('Ctrl Pts',(7.18701357999994,11.6,-7.78318000600001));
#173207=CARTESIAN_POINT('Ctrl Pts',(7.18872800599994,15.2,-7.78436277100001));
#173208=CARTESIAN_POINT('Ctrl Pts',(7.18872800599994,11.6,-7.78436277100001));
#173209=CARTESIAN_POINT('Ctrl Pts',(7.19044916199994,15.2,-7.78554790600002));
#173210=CARTESIAN_POINT('Ctrl Pts',(7.19044916199994,11.6,-7.78554790600002));
#173211=CARTESIAN_POINT('Ctrl Pts',(7.19217703999994,15.2,-7.78673539200001));
#173212=CARTESIAN_POINT('Ctrl Pts',(7.19217703999994,11.6,-7.78673539200001));
#173213=CARTESIAN_POINT('Ctrl Pts',(7.19391163699994,15.2,-7.78792521200002));
#173214=CARTESIAN_POINT('Ctrl Pts',(7.19391163699994,11.6,-7.78792521200002));
#173215=CARTESIAN_POINT('Ctrl Pts',(7.19565294499994,15.2,-7.78911735100002));
#173216=CARTESIAN_POINT('Ctrl Pts',(7.19565294499994,11.6,-7.78911735100002));
#173217=CARTESIAN_POINT('Ctrl Pts',(7.19740096099994,15.2,-7.79031178700002));
#173218=CARTESIAN_POINT('Ctrl Pts',(7.19740096099994,11.6,-7.79031178700002));
#173219=CARTESIAN_POINT('Ctrl Pts',(7.19915567599994,15.2,-7.79150850900002));
#173220=CARTESIAN_POINT('Ctrl Pts',(7.19915567599994,11.6,-7.79150850900002));
#173221=CARTESIAN_POINT('Ctrl Pts',(7.20091708699995,15.2,-7.79270749500002));
#173222=CARTESIAN_POINT('Ctrl Pts',(7.20091708699995,11.6,-7.79270749500002));
#173223=CARTESIAN_POINT('Ctrl Pts',(7.20268518599994,15.2,-7.79390872900001));
#173224=CARTESIAN_POINT('Ctrl Pts',(7.20268518599994,11.6,-7.79390872900001));
#173225=CARTESIAN_POINT('Ctrl Pts',(7.20445996999994,15.2,-7.79511219500002));
#173226=CARTESIAN_POINT('Ctrl Pts',(7.20445996999994,11.6,-7.79511219500002));
#173227=CARTESIAN_POINT('Ctrl Pts',(7.20624142999994,15.2,-7.79631787700002));
#173228=CARTESIAN_POINT('Ctrl Pts',(7.20624142999994,11.6,-7.79631787700002));
#173229=CARTESIAN_POINT('Ctrl Pts',(7.20802956399995,15.2,-7.79752575600002));
#173230=CARTESIAN_POINT('Ctrl Pts',(7.20802956399995,11.6,-7.79752575600002));
#173231=CARTESIAN_POINT('Ctrl Pts',(7.20982436399995,15.2,-7.79873581700001));
#173232=CARTESIAN_POINT('Ctrl Pts',(7.20982436399995,11.6,-7.79873581700001));
#173233=CARTESIAN_POINT('Ctrl Pts',(7.21162582299994,15.2,-7.79994804100002));
#173234=CARTESIAN_POINT('Ctrl Pts',(7.21162582299994,11.6,-7.79994804100002));
#173235=CARTESIAN_POINT('Ctrl Pts',(7.21343393899994,15.2,-7.80116241400002));
#173236=CARTESIAN_POINT('Ctrl Pts',(7.21343393899994,11.6,-7.80116241400002));
#173237=CARTESIAN_POINT('Ctrl Pts',(7.21524870299994,15.2,-7.80237891700001));
#173238=CARTESIAN_POINT('Ctrl Pts',(7.21524870299994,11.6,-7.80237891700001));
#173239=CARTESIAN_POINT('Ctrl Pts',(7.21707011099994,15.2,-7.80359753500001));
#173240=CARTESIAN_POINT('Ctrl Pts',(7.21707011099994,11.6,-7.80359753500001));
#173241=CARTESIAN_POINT('Ctrl Pts',(7.21889815899995,15.2,-7.80481825200001));
#173242=CARTESIAN_POINT('Ctrl Pts',(7.21889815899995,11.6,-7.80481825200001));
#173243=CARTESIAN_POINT('Ctrl Pts',(7.22073283799994,15.2,-7.80604104900001));
#173244=CARTESIAN_POINT('Ctrl Pts',(7.22073283799994,11.6,-7.80604104900001));
#173245=CARTESIAN_POINT('Ctrl Pts',(7.22257414399994,15.2,-7.80726591200001));
#173246=CARTESIAN_POINT('Ctrl Pts',(7.22257414399994,11.6,-7.80726591200001));
#173247=CARTESIAN_POINT('Ctrl Pts',(7.22442207099995,15.2,-7.80849282300002));
#173248=CARTESIAN_POINT('Ctrl Pts',(7.22442207099995,11.6,-7.80849282300002));
#173249=CARTESIAN_POINT('Ctrl Pts',(7.22627661399994,15.2,-7.80972176700002));
#173250=CARTESIAN_POINT('Ctrl Pts',(7.22627661399994,11.6,-7.80972176700002));
#173251=CARTESIAN_POINT('Ctrl Pts',(7.22813776799994,15.2,-7.81095272700002));
#173252=CARTESIAN_POINT('Ctrl Pts',(7.22813776799994,11.6,-7.81095272700002));
#173253=CARTESIAN_POINT('Ctrl Pts',(7.23000552399995,15.2,-7.81218568800002));
#173254=CARTESIAN_POINT('Ctrl Pts',(7.23000552399995,11.6,-7.81218568800002));
#173255=CARTESIAN_POINT('Ctrl Pts',(7.23187987999995,15.2,-7.81342063100002));
#173256=CARTESIAN_POINT('Ctrl Pts',(7.23187987999995,11.6,-7.81342063100002));
#173257=CARTESIAN_POINT('Ctrl Pts',(7.23376082999994,15.2,-7.81465754200001));
#173258=CARTESIAN_POINT('Ctrl Pts',(7.23376082999994,11.6,-7.81465754200001));
#173259=CARTESIAN_POINT('Ctrl Pts',(7.23564836799994,15.2,-7.81589640600002));
#173260=CARTESIAN_POINT('Ctrl Pts',(7.23564836799994,11.6,-7.81589640600002));
#173261=CARTESIAN_POINT('Ctrl Pts',(7.23754248699994,15.2,-7.81713720600001));
#173262=CARTESIAN_POINT('Ctrl Pts',(7.23754248699994,11.6,-7.81713720600001));
#173263=CARTESIAN_POINT('Ctrl Pts',(7.23944318299995,15.2,-7.81837992500002));
#173264=CARTESIAN_POINT('Ctrl Pts',(7.23944318299995,11.6,-7.81837992500002));
#173265=CARTESIAN_POINT('Ctrl Pts',(7.24135044899994,15.2,-7.81962454700002));
#173266=CARTESIAN_POINT('Ctrl Pts',(7.24135044899994,11.6,-7.81962454700002));
#173267=CARTESIAN_POINT('Ctrl Pts',(7.24326428099995,15.2,-7.82087105900001));
#173268=CARTESIAN_POINT('Ctrl Pts',(7.24326428099995,11.6,-7.82087105900001));
#173269=CARTESIAN_POINT('Ctrl Pts',(7.24518467299994,15.2,-7.82211944200002));
#173270=CARTESIAN_POINT('Ctrl Pts',(7.24518467299994,11.6,-7.82211944200002));
#173271=CARTESIAN_POINT('Ctrl Pts',(7.24711161899994,15.2,-7.82336968200001));
#173272=CARTESIAN_POINT('Ctrl Pts',(7.24711161899994,11.6,-7.82336968200001));
#173273=CARTESIAN_POINT('Ctrl Pts',(7.24904511399994,15.2,-7.82462176200001));
#173274=CARTESIAN_POINT('Ctrl Pts',(7.24904511399994,11.6,-7.82462176200001));
#173275=CARTESIAN_POINT('Ctrl Pts',(7.25098515199995,15.2,-7.82587566800002));
#173276=CARTESIAN_POINT('Ctrl Pts',(7.25098515199995,11.6,-7.82587566800002));
#173277=CARTESIAN_POINT('Ctrl Pts',(7.25293172799995,15.2,-7.82713138500001));
#173278=CARTESIAN_POINT('Ctrl Pts',(7.25293172799995,11.6,-7.82713138500001));
#173279=CARTESIAN_POINT('Ctrl Pts',(7.25488483599994,15.2,-7.82838889500002));
#173280=CARTESIAN_POINT('Ctrl Pts',(7.25488483599994,11.6,-7.82838889500002));
#173281=CARTESIAN_POINT('Ctrl Pts',(7.25684446999994,15.2,-7.82964818400002));
#173282=CARTESIAN_POINT('Ctrl Pts',(7.25684446999994,11.6,-7.82964818400002));
#173283=CARTESIAN_POINT('Ctrl Pts',(7.25881062599994,15.2,-7.83090923600002));
#173284=CARTESIAN_POINT('Ctrl Pts',(7.25881062599994,11.6,-7.83090923600002));
#173285=CARTESIAN_POINT('Ctrl Pts',(7.26078329799994,15.2,-7.83217203500002));
#173286=CARTESIAN_POINT('Ctrl Pts',(7.26078329799994,11.6,-7.83217203500002));
#173287=CARTESIAN_POINT('Ctrl Pts',(7.26276247899994,15.2,-7.83343656800002));
#173288=CARTESIAN_POINT('Ctrl Pts',(7.26276247899994,11.6,-7.83343656800002));
#173289=CARTESIAN_POINT('Ctrl Pts',(7.26474816499994,15.2,-7.83470281800002));
#173290=CARTESIAN_POINT('Ctrl Pts',(7.26474816499994,11.6,-7.83470281800002));
#173291=CARTESIAN_POINT('Ctrl Pts',(7.26674034999995,15.2,-7.83597077000002));
#173292=CARTESIAN_POINT('Ctrl Pts',(7.26674034999995,11.6,-7.83597077000002));
#173293=CARTESIAN_POINT('Ctrl Pts',(7.26873902899994,15.2,-7.83724040800001));
#173294=CARTESIAN_POINT('Ctrl Pts',(7.26873902899994,11.6,-7.83724040800001));
#173295=CARTESIAN_POINT('Ctrl Pts',(7.27074419499994,15.2,-7.83851172000002));
#173296=CARTESIAN_POINT('Ctrl Pts',(7.27074419499994,11.6,-7.83851172000002));
#173297=CARTESIAN_POINT('Ctrl Pts',(7.27275584499994,15.2,-7.83978468700001));
#173298=CARTESIAN_POINT('Ctrl Pts',(7.27275584499994,11.6,-7.83978468700001));
#173299=CARTESIAN_POINT('Ctrl Pts',(7.27477397199995,15.2,-7.84105929500001));
#173300=CARTESIAN_POINT('Ctrl Pts',(7.27477397199995,11.6,-7.84105929500001));
#173301=CARTESIAN_POINT('Ctrl Pts',(7.27679856999995,15.2,-7.84233553100002));
#173302=CARTESIAN_POINT('Ctrl Pts',(7.27679856999995,11.6,-7.84233553100002));
#173303=CARTESIAN_POINT('Ctrl Pts',(7.27882963499995,15.2,-7.84361337900001));
#173304=CARTESIAN_POINT('Ctrl Pts',(7.27882963499995,11.6,-7.84361337900001));
#173305=CARTESIAN_POINT('Ctrl Pts',(7.28086715999994,15.2,-7.84489282200001));
#173306=CARTESIAN_POINT('Ctrl Pts',(7.28086715999994,11.6,-7.84489282200001));
#173307=CARTESIAN_POINT('Ctrl Pts',(7.28291114199994,15.2,-7.84617384900002));
#173308=CARTESIAN_POINT('Ctrl Pts',(7.28291114199994,11.6,-7.84617384900002));
#173309=CARTESIAN_POINT('Ctrl Pts',(7.28496157299994,15.2,-7.84745644200001));
#173310=CARTESIAN_POINT('Ctrl Pts',(7.28496157299994,11.6,-7.84745644200001));
#173311=CARTESIAN_POINT('Ctrl Pts',(7.28701844799994,15.2,-7.84874058700002));
#173312=CARTESIAN_POINT('Ctrl Pts',(7.28701844799994,11.6,-7.84874058700002));
#173313=CARTESIAN_POINT('Ctrl Pts',(7.28908176299995,15.2,-7.85002627000001));
#173314=CARTESIAN_POINT('Ctrl Pts',(7.28908176299995,11.6,-7.85002627000001));
#173315=CARTESIAN_POINT('Ctrl Pts',(7.29115151099994,15.2,-7.85131347600001));
#173316=CARTESIAN_POINT('Ctrl Pts',(7.29115151099994,11.6,-7.85131347600001));
#173317=CARTESIAN_POINT('Ctrl Pts',(7.29322768799994,15.2,-7.85260219100002));
#173318=CARTESIAN_POINT('Ctrl Pts',(7.29322768799994,11.6,-7.85260219100002));
#173319=CARTESIAN_POINT('Ctrl Pts',(7.29531028699994,15.2,-7.85389239900002));
#173320=CARTESIAN_POINT('Ctrl Pts',(7.29531028699994,11.6,-7.85389239900002));
#173321=CARTESIAN_POINT('Ctrl Pts',(7.29739930399994,15.2,-7.85518408600002));
#173322=CARTESIAN_POINT('Ctrl Pts',(7.29739930399994,11.6,-7.85518408600002));
#173323=CARTESIAN_POINT('Ctrl Pts',(7.29949473199994,15.2,-7.85647723800002));
#173324=CARTESIAN_POINT('Ctrl Pts',(7.29949473199994,11.6,-7.85647723800002));
#173325=CARTESIAN_POINT('Ctrl Pts',(7.30159656799994,15.2,-7.85777184100001));
#173326=CARTESIAN_POINT('Ctrl Pts',(7.30159656799994,11.6,-7.85777184100001));
#173327=CARTESIAN_POINT('Ctrl Pts',(7.30370480499994,15.2,-7.85906787900001));
#173328=CARTESIAN_POINT('Ctrl Pts',(7.30370480499994,11.6,-7.85906787900001));
#173329=CARTESIAN_POINT('Ctrl Pts',(7.30581943699994,15.2,-7.86036533900001));
#173330=CARTESIAN_POINT('Ctrl Pts',(7.30581943699994,11.6,-7.86036533900001));
#173331=CARTESIAN_POINT('Ctrl Pts',(7.30794045899994,15.2,-7.86166420600001));
#173332=CARTESIAN_POINT('Ctrl Pts',(7.30794045899994,11.6,-7.86166420600001));
#173333=CARTESIAN_POINT('Ctrl Pts',(7.31006786699994,15.2,-7.86296446600002));
#173334=CARTESIAN_POINT('Ctrl Pts',(7.31006786699994,11.6,-7.86296446600002));
#173335=CARTESIAN_POINT('Ctrl Pts',(7.31220165399994,15.2,-7.86426610500002));
#173336=CARTESIAN_POINT('Ctrl Pts',(7.31220165399994,11.6,-7.86426610500002));
#173337=CARTESIAN_POINT('Ctrl Pts',(7.31434181599995,15.2,-7.86556910800002));
#173338=CARTESIAN_POINT('Ctrl Pts',(7.31434181599995,11.6,-7.86556910800002));
#173339=CARTESIAN_POINT('Ctrl Pts',(7.31648834699994,15.2,-7.86687346200001));
#173340=CARTESIAN_POINT('Ctrl Pts',(7.31648834699994,11.6,-7.86687346200001));
#173341=CARTESIAN_POINT('Ctrl Pts',(7.31864124199994,15.2,-7.86817915200002));
#173342=CARTESIAN_POINT('Ctrl Pts',(7.31864124199994,11.6,-7.86817915200002));
#173343=CARTESIAN_POINT('Ctrl Pts',(7.32080049399995,15.2,-7.86948616400001));
#173344=CARTESIAN_POINT('Ctrl Pts',(7.32080049399995,11.6,-7.86948616400001));
#173345=CARTESIAN_POINT('Ctrl Pts',(7.32296609999994,15.2,-7.87079448400001));
#173346=CARTESIAN_POINT('Ctrl Pts',(7.32296609999994,11.6,-7.87079448400001));
#173347=CARTESIAN_POINT('Ctrl Pts',(7.32513805299994,15.2,-7.87210409900001));
#173348=CARTESIAN_POINT('Ctrl Pts',(7.32513805299994,11.6,-7.87210409900001));
#173349=CARTESIAN_POINT('Ctrl Pts',(7.32731634799995,15.2,-7.87341499400001));
#173350=CARTESIAN_POINT('Ctrl Pts',(7.32731634799995,11.6,-7.87341499400001));
#173351=CARTESIAN_POINT('Ctrl Pts',(7.32950097899994,15.2,-7.87472715600002));
#173352=CARTESIAN_POINT('Ctrl Pts',(7.32950097899994,11.6,-7.87472715600002));
#173353=CARTESIAN_POINT('Ctrl Pts',(7.33169194399995,15.2,-7.87604056900002));
#173354=CARTESIAN_POINT('Ctrl Pts',(7.33169194399995,11.6,-7.87604056900002));
#173355=CARTESIAN_POINT('Ctrl Pts',(7.33388923299994,15.2,-7.87735522200002));
#173356=CARTESIAN_POINT('Ctrl Pts',(7.33388923299994,11.6,-7.87735522200002));
#173357=CARTESIAN_POINT('Ctrl Pts',(7.33609284399994,15.2,-7.87867109900001));
#173358=CARTESIAN_POINT('Ctrl Pts',(7.33609284399994,11.6,-7.87867109900001));
#173359=CARTESIAN_POINT('Ctrl Pts',(7.33830276899995,15.2,-7.87998818800002));
#173360=CARTESIAN_POINT('Ctrl Pts',(7.33830276899995,11.6,-7.87998818800002));
#173361=CARTESIAN_POINT('Ctrl Pts',(7.34051900599995,15.2,-7.88130647500001));
#173362=CARTESIAN_POINT('Ctrl Pts',(7.34051900599995,11.6,-7.88130647500001));
#173363=CARTESIAN_POINT('Ctrl Pts',(7.34274154699994,15.2,-7.88262594500001));
#173364=CARTESIAN_POINT('Ctrl Pts',(7.34274154699994,11.6,-7.88262594500001));
#173365=CARTESIAN_POINT('Ctrl Pts',(7.34497038799995,15.2,-7.88394658600001));
#173366=CARTESIAN_POINT('Ctrl Pts',(7.34497038799995,11.6,-7.88394658600001));
#173367=CARTESIAN_POINT('Ctrl Pts',(7.34720552299994,15.2,-7.88526838400001));
#173368=CARTESIAN_POINT('Ctrl Pts',(7.34720552299994,11.6,-7.88526838400001));
#173369=CARTESIAN_POINT('Ctrl Pts',(7.34944694599994,15.2,-7.88659132500002));
#173370=CARTESIAN_POINT('Ctrl Pts',(7.34944694599994,11.6,-7.88659132500002));
#173371=CARTESIAN_POINT('Ctrl Pts',(7.35169465499995,15.2,-7.88791539600001));
#173372=CARTESIAN_POINT('Ctrl Pts',(7.35169465499995,11.6,-7.88791539600001));
#173373=CARTESIAN_POINT('Ctrl Pts',(7.35394863999994,15.2,-7.88924058300001));
#173374=CARTESIAN_POINT('Ctrl Pts',(7.35394863999994,11.6,-7.88924058300001));
#173375=CARTESIAN_POINT('Ctrl Pts',(7.35620889899994,15.2,-7.89056687300001));
#173376=CARTESIAN_POINT('Ctrl Pts',(7.35620889899994,11.6,-7.89056687300001));
#173377=CARTESIAN_POINT('Ctrl Pts',(7.35847542699994,15.2,-7.89189425200002));
#173378=CARTESIAN_POINT('Ctrl Pts',(7.35847542699994,11.6,-7.89189425200002));
#173379=CARTESIAN_POINT('Ctrl Pts',(7.36074821699994,15.2,-7.89322270800002));
#173380=CARTESIAN_POINT('Ctrl Pts',(7.36074821699994,11.6,-7.89322270800002));
#173381=CARTESIAN_POINT('Ctrl Pts',(7.36302726299995,15.2,-7.89455222600001));
#173382=CARTESIAN_POINT('Ctrl Pts',(7.36302726299995,11.6,-7.89455222600001));
#173383=CARTESIAN_POINT('Ctrl Pts',(7.36531256299994,15.2,-7.89588279400002));
#173384=CARTESIAN_POINT('Ctrl Pts',(7.36531256299994,11.6,-7.89588279400002));
#173385=CARTESIAN_POINT('Ctrl Pts',(7.36760410799994,15.2,-7.89721439900001));
#173386=CARTESIAN_POINT('Ctrl Pts',(7.36760410799994,11.6,-7.89721439900001));
#173387=CARTESIAN_POINT('Ctrl Pts',(7.36990189499994,15.2,-7.89854702700002));
#173388=CARTESIAN_POINT('Ctrl Pts',(7.36990189499994,11.6,-7.89854702700002));
#173389=CARTESIAN_POINT('Ctrl Pts',(7.37220591899994,15.2,-7.89988066400002));
#173390=CARTESIAN_POINT('Ctrl Pts',(7.37220591899994,11.6,-7.89988066400002));
#173391=CARTESIAN_POINT('Ctrl Pts',(7.37451617399994,15.2,-7.90121530000001));
#173392=CARTESIAN_POINT('Ctrl Pts',(7.37451617399994,11.6,-7.90121530000001));
#173393=CARTESIAN_POINT('Ctrl Pts',(7.37683265399995,15.2,-7.90255091900002));
#173394=CARTESIAN_POINT('Ctrl Pts',(7.37683265399995,11.6,-7.90255091900002));
#173395=CARTESIAN_POINT('Ctrl Pts',(7.37915535499994,15.2,-7.90388750900001));
#173396=CARTESIAN_POINT('Ctrl Pts',(7.37915535499994,11.6,-7.90388750900001));
#173397=CARTESIAN_POINT('Ctrl Pts',(7.38148426999994,15.2,-7.90522505700002));
#173398=CARTESIAN_POINT('Ctrl Pts',(7.38148426999994,11.6,-7.90522505700002));
#173399=CARTESIAN_POINT('Ctrl Pts',(7.38381939699994,15.2,-7.90656355000002));
#173400=CARTESIAN_POINT('Ctrl Pts',(7.38381939699994,11.6,-7.90656355000002));
#173401=CARTESIAN_POINT('Ctrl Pts',(7.38616072799994,15.2,-7.90790297500001));
#173402=CARTESIAN_POINT('Ctrl Pts',(7.38616072799994,11.6,-7.90790297500001));
#173403=CARTESIAN_POINT('Ctrl Pts',(7.38850825799994,15.2,-7.90924331900002));
#173404=CARTESIAN_POINT('Ctrl Pts',(7.38850825799994,11.6,-7.90924331900002));
#173405=CARTESIAN_POINT('Ctrl Pts',(7.39086198299994,15.2,-7.91058457000001));
#173406=CARTESIAN_POINT('Ctrl Pts',(7.39086198299994,11.6,-7.91058457000001));
#173407=CARTESIAN_POINT('Ctrl Pts',(7.39322189599994,15.2,-7.91192671500001));
#173408=CARTESIAN_POINT('Ctrl Pts',(7.39322189599994,11.6,-7.91192671500001));
#173409=CARTESIAN_POINT('Ctrl Pts',(7.39558799399994,15.2,-7.91326974000001));
#173410=CARTESIAN_POINT('Ctrl Pts',(7.39558799399994,11.6,-7.91326974000001));
#173411=CARTESIAN_POINT('Ctrl Pts',(7.39796027099994,15.2,-7.91461363300002));
#173412=CARTESIAN_POINT('Ctrl Pts',(7.39796027099994,11.6,-7.91461363300002));
#173413=CARTESIAN_POINT('Ctrl Pts',(7.40033872099994,15.2,-7.91595838200001));
#173414=CARTESIAN_POINT('Ctrl Pts',(7.40033872099994,11.6,-7.91595838200001));
#173415=CARTESIAN_POINT('Ctrl Pts',(7.40272333899994,15.2,-7.91730397200002));
#173416=CARTESIAN_POINT('Ctrl Pts',(7.40272333899994,11.6,-7.91730397200002));
#173417=CARTESIAN_POINT('Ctrl Pts',(7.40511411999995,15.2,-7.91865039400002));
#173418=CARTESIAN_POINT('Ctrl Pts',(7.40511411999995,11.6,-7.91865039400002));
#173419=CARTESIAN_POINT('Ctrl Pts',(7.40751105899994,15.2,-7.91999763300002));
#173420=CARTESIAN_POINT('Ctrl Pts',(7.40751105899994,11.6,-7.91999763300002));
#173421=CARTESIAN_POINT('Ctrl Pts',(7.40991415099994,15.2,-7.92134567700002));
#173422=CARTESIAN_POINT('Ctrl Pts',(7.40991415099994,11.6,-7.92134567700002));
#173423=CARTESIAN_POINT('Ctrl Pts',(7.41232339099994,15.2,-7.92269451400001));
#173424=CARTESIAN_POINT('Ctrl Pts',(7.41232339099994,11.6,-7.92269451400001));
#173425=CARTESIAN_POINT('Ctrl Pts',(7.41473877199994,15.2,-7.92404412900002));
#173426=CARTESIAN_POINT('Ctrl Pts',(7.41473877199994,11.6,-7.92404412900002));
#173427=CARTESIAN_POINT('Ctrl Pts',(7.41716029099995,15.2,-7.92539451300001));
#173428=CARTESIAN_POINT('Ctrl Pts',(7.41716029099995,11.6,-7.92539451300001));
#173429=CARTESIAN_POINT('Ctrl Pts',(7.41958794199994,15.2,-7.92674565200001));
#173430=CARTESIAN_POINT('Ctrl Pts',(7.41958794199994,11.6,-7.92674565200001));
#173431=CARTESIAN_POINT('Ctrl Pts',(7.42202171899994,15.2,-7.92809753400002));
#173432=CARTESIAN_POINT('Ctrl Pts',(7.42202171899994,11.6,-7.92809753400002));
#173433=CARTESIAN_POINT('Ctrl Pts',(7.42446161799994,15.2,-7.92945014600001));
#173434=CARTESIAN_POINT('Ctrl Pts',(7.42446161799994,11.6,-7.92945014600001));
#173435=CARTESIAN_POINT('Ctrl Pts',(7.42690763399994,15.2,-7.93080347600001));
#173436=CARTESIAN_POINT('Ctrl Pts',(7.42690763399994,11.6,-7.93080347600001));
#173437=CARTESIAN_POINT('Ctrl Pts',(7.42935975999995,15.2,-7.93215751200002));
#173438=CARTESIAN_POINT('Ctrl Pts',(7.42935975999995,11.6,-7.93215751200002));
#173439=CARTESIAN_POINT('Ctrl Pts',(7.43181799299995,15.2,-7.93351224200002));
#173440=CARTESIAN_POINT('Ctrl Pts',(7.43181799299995,11.6,-7.93351224200002));
#173441=CARTESIAN_POINT('Ctrl Pts',(7.43428232699994,15.2,-7.93486765200001));
#173442=CARTESIAN_POINT('Ctrl Pts',(7.43428232699994,11.6,-7.93486765200001));
#173443=CARTESIAN_POINT('Ctrl Pts',(7.43675275699994,15.2,-7.93622373200002));
#173444=CARTESIAN_POINT('Ctrl Pts',(7.43675275699994,11.6,-7.93622373200002));
#173445=CARTESIAN_POINT('Ctrl Pts',(7.43922927599994,15.2,-7.93758046900002));
#173446=CARTESIAN_POINT('Ctrl Pts',(7.43922927599994,11.6,-7.93758046900002));
#173447=CARTESIAN_POINT('Ctrl Pts',(7.44171188299994,15.2,-7.93893785000002));
#173448=CARTESIAN_POINT('Ctrl Pts',(7.44171188299994,11.6,-7.93893785000002));
#173449=CARTESIAN_POINT('Ctrl Pts',(7.44420056799994,15.2,-7.94029586500002));
#173450=CARTESIAN_POINT('Ctrl Pts',(7.44420056799994,11.6,-7.94029586500002));
#173451=CARTESIAN_POINT('Ctrl Pts',(7.44669532899994,15.2,-7.94165450000002));
#173452=CARTESIAN_POINT('Ctrl Pts',(7.44669532899994,11.6,-7.94165450000002));
#173453=CARTESIAN_POINT('Ctrl Pts',(7.44919616099994,15.2,-7.94301374500002));
#173454=CARTESIAN_POINT('Ctrl Pts',(7.44919616099994,11.6,-7.94301374500002));
#173455=CARTESIAN_POINT('Ctrl Pts',(7.45170305699994,15.2,-7.94437358500002));
#173456=CARTESIAN_POINT('Ctrl Pts',(7.45170305699994,11.6,-7.94437358500002));
#173457=CARTESIAN_POINT('Ctrl Pts',(7.45421601299994,15.2,-7.94573401100001));
#173458=CARTESIAN_POINT('Ctrl Pts',(7.45421601299994,11.6,-7.94573401100001));
#173459=CARTESIAN_POINT('Ctrl Pts',(7.45673502399994,15.2,-7.94709501000002));
#173460=CARTESIAN_POINT('Ctrl Pts',(7.45673502399994,11.6,-7.94709501000002));
#173461=CARTESIAN_POINT('Ctrl Pts',(7.45926008499994,15.2,-7.94845657000002));
#173462=CARTESIAN_POINT('Ctrl Pts',(7.45926008499994,11.6,-7.94845657000002));
#173463=CARTESIAN_POINT('Ctrl Pts',(7.46179118999994,15.2,-7.94981867900002));
#173464=CARTESIAN_POINT('Ctrl Pts',(7.46179118999994,11.6,-7.94981867900002));
#173465=CARTESIAN_POINT('Ctrl Pts',(7.46432833399994,15.2,-7.95118132500002));
#173466=CARTESIAN_POINT('Ctrl Pts',(7.46432833399994,11.6,-7.95118132500002));
#173467=CARTESIAN_POINT('Ctrl Pts',(7.46687151199994,15.2,-7.95254449800002));
#173468=CARTESIAN_POINT('Ctrl Pts',(7.46687151199994,11.6,-7.95254449800002));
#173469=CARTESIAN_POINT('Ctrl Pts',(7.46942071999994,15.2,-7.95390818300002));
#173470=CARTESIAN_POINT('Ctrl Pts',(7.46942071999994,11.6,-7.95390818300002));
#173471=CARTESIAN_POINT('Ctrl Pts',(7.47197595099995,15.2,-7.95527237200002));
#173472=CARTESIAN_POINT('Ctrl Pts',(7.47197595099995,11.6,-7.95527237200002));
#173473=CARTESIAN_POINT('Ctrl Pts',(7.47453719999994,15.2,-7.95663705000001));
#173474=CARTESIAN_POINT('Ctrl Pts',(7.47453719999994,11.6,-7.95663705000001));
#173475=CARTESIAN_POINT('Ctrl Pts',(7.47710446499994,15.2,-7.95800220700002));
#173476=CARTESIAN_POINT('Ctrl Pts',(7.47710446499994,11.6,-7.95800220700002));
#173477=CARTESIAN_POINT('Ctrl Pts',(7.47967773699994,15.2,-7.95936783200001));
#173478=CARTESIAN_POINT('Ctrl Pts',(7.47967773699994,11.6,-7.95936783200001));
#173479=CARTESIAN_POINT('Ctrl Pts',(7.48225701299994,15.2,-7.96073391100002));
#173480=CARTESIAN_POINT('Ctrl Pts',(7.48225701299994,11.6,-7.96073391100002));
#173481=CARTESIAN_POINT('Ctrl Pts',(7.48484228799994,15.2,-7.96210043600002));
#173482=CARTESIAN_POINT('Ctrl Pts',(7.48484228799994,11.6,-7.96210043600002));
#173483=CARTESIAN_POINT('Ctrl Pts',(7.48743355699995,15.2,-7.96346739200001));
#173484=CARTESIAN_POINT('Ctrl Pts',(7.48743355699995,11.6,-7.96346739200001));
#173485=CARTESIAN_POINT('Ctrl Pts',(7.49003081299994,15.2,-7.96483476900002));
#173486=CARTESIAN_POINT('Ctrl Pts',(7.49003081299994,11.6,-7.96483476900002));
#173487=CARTESIAN_POINT('Ctrl Pts',(7.49263405299994,15.2,-7.96620255600001));
#173488=CARTESIAN_POINT('Ctrl Pts',(7.49263405299994,11.6,-7.96620255600001));
#173489=CARTESIAN_POINT('Ctrl Pts',(7.49524327099994,15.2,-7.96757074100002));
#173490=CARTESIAN_POINT('Ctrl Pts',(7.49524327099994,11.6,-7.96757074100002));
#173491=CARTESIAN_POINT('Ctrl Pts',(7.49785846099994,15.2,-7.96893931300002));
#173492=CARTESIAN_POINT('Ctrl Pts',(7.49785846099994,11.6,-7.96893931300002));
#173493=CARTESIAN_POINT('Ctrl Pts',(7.50047961999995,15.2,-7.97030826000002));
#173494=CARTESIAN_POINT('Ctrl Pts',(7.50047961999995,11.6,-7.97030826000002));
#173495=CARTESIAN_POINT('Ctrl Pts',(7.50310674299994,15.2,-7.97167757000001));
#173496=CARTESIAN_POINT('Ctrl Pts',(7.50310674299994,11.6,-7.97167757000001));
#173497=CARTESIAN_POINT('Ctrl Pts',(7.50573982199994,15.2,-7.97304723400002));
#173498=CARTESIAN_POINT('Ctrl Pts',(7.50573982199994,11.6,-7.97304723400002));
#173499=CARTESIAN_POINT('Ctrl Pts',(7.50837885499994,15.2,-7.97441723900001));
#173500=CARTESIAN_POINT('Ctrl Pts',(7.50837885499994,11.6,-7.97441723900001));
#173501=CARTESIAN_POINT('Ctrl Pts',(7.51102383599994,15.2,-7.97578757300001));
#173502=CARTESIAN_POINT('Ctrl Pts',(7.51102383599994,11.6,-7.97578757300001));
#173503=CARTESIAN_POINT('Ctrl Pts',(7.51367475799994,15.2,-7.97715822700001));
#173504=CARTESIAN_POINT('Ctrl Pts',(7.51367475799994,11.6,-7.97715822700001));
#173505=CARTESIAN_POINT('Ctrl Pts',(7.51633161799995,15.2,-7.97852918700002));
#173506=CARTESIAN_POINT('Ctrl Pts',(7.51633161799995,11.6,-7.97852918700002));
#173507=CARTESIAN_POINT('Ctrl Pts',(7.51899441199994,15.2,-7.97990044500001));
#173508=CARTESIAN_POINT('Ctrl Pts',(7.51899441199994,11.6,-7.97990044500001));
#173509=CARTESIAN_POINT('Ctrl Pts',(7.52166313299995,15.2,-7.98127198800002));
#173510=CARTESIAN_POINT('Ctrl Pts',(7.52166313299995,11.6,-7.98127198800002));
#173511=CARTESIAN_POINT('Ctrl Pts',(7.52433777599994,15.2,-7.98264380500001));
#173512=CARTESIAN_POINT('Ctrl Pts',(7.52433777599994,11.6,-7.98264380500001));
#173513=CARTESIAN_POINT('Ctrl Pts',(7.52701833599994,15.2,-7.98401588500001));
#173514=CARTESIAN_POINT('Ctrl Pts',(7.52701833599994,11.6,-7.98401588500001));
#173515=CARTESIAN_POINT('Ctrl Pts',(7.52970480999994,15.2,-7.98538821700002));
#173516=CARTESIAN_POINT('Ctrl Pts',(7.52970480999994,11.6,-7.98538821700002));
#173517=CARTESIAN_POINT('Ctrl Pts',(7.53239718999994,15.2,-7.98676079000002));
#173518=CARTESIAN_POINT('Ctrl Pts',(7.53239718999994,11.6,-7.98676079000002));
#173519=CARTESIAN_POINT('Ctrl Pts',(7.53509547299994,15.2,-7.98813359300001));
#173520=CARTESIAN_POINT('Ctrl Pts',(7.53509547299994,11.6,-7.98813359300001));
#173521=CARTESIAN_POINT('Ctrl Pts',(7.53779965199994,15.2,-7.98950661400001));
#173522=CARTESIAN_POINT('Ctrl Pts',(7.53779965199994,11.6,-7.98950661400001));
#173523=CARTESIAN_POINT('Ctrl Pts',(7.54050972499994,15.2,-7.99087984500002));
#173524=CARTESIAN_POINT('Ctrl Pts',(7.54050972499994,11.6,-7.99087984500002));
#173525=CARTESIAN_POINT('Ctrl Pts',(7.54322568399994,15.2,-7.99225327200002));
#173526=CARTESIAN_POINT('Ctrl Pts',(7.54322568399994,11.6,-7.99225327200002));
#173527=CARTESIAN_POINT('Ctrl Pts',(7.54594752699994,15.2,-7.99362688500001));
#173528=CARTESIAN_POINT('Ctrl Pts',(7.54594752699994,11.6,-7.99362688500001));
#173529=CARTESIAN_POINT('Ctrl Pts',(7.54867524599995,15.2,-7.99500067300002));
#173530=CARTESIAN_POINT('Ctrl Pts',(7.54867524599995,11.6,-7.99500067300002));
#173531=CARTESIAN_POINT('Ctrl Pts',(7.55140883599994,15.2,-7.99637462700002));
#173532=CARTESIAN_POINT('Ctrl Pts',(7.55140883599994,11.6,-7.99637462700002));
#173533=CARTESIAN_POINT('Ctrl Pts',(7.55414829499995,15.2,-7.99774873400001));
#173534=CARTESIAN_POINT('Ctrl Pts',(7.55414829499995,11.6,-7.99774873400001));
#173535=CARTESIAN_POINT('Ctrl Pts',(7.55689361499994,15.2,-7.99912298400002));
#173536=CARTESIAN_POINT('Ctrl Pts',(7.55689361499994,11.6,-7.99912298400002));
#173537=CARTESIAN_POINT('Ctrl Pts',(7.55964479299994,15.2,-8.00049736600002));
#173538=CARTESIAN_POINT('Ctrl Pts',(7.55964479299994,11.6,-8.00049736600002));
#173539=CARTESIAN_POINT('Ctrl Pts',(7.56240182199994,15.2,-8.00187187000001));
#173540=CARTESIAN_POINT('Ctrl Pts',(7.56240182199994,11.6,-8.00187187000001));
#173541=CARTESIAN_POINT('Ctrl Pts',(7.56516469899994,15.2,-8.00324648500002));
#173542=CARTESIAN_POINT('Ctrl Pts',(7.56516469899994,11.6,-8.00324648500002));
#173543=CARTESIAN_POINT('Ctrl Pts',(7.56793341799994,15.2,-8.00462119900001));
#173544=CARTESIAN_POINT('Ctrl Pts',(7.56793341799994,11.6,-8.00462119900001));
#173545=CARTESIAN_POINT('Ctrl Pts',(7.57070797399995,15.2,-8.00599600300002));
#173546=CARTESIAN_POINT('Ctrl Pts',(7.57070797399995,11.6,-8.00599600300002));
#173547=CARTESIAN_POINT('Ctrl Pts',(7.57348836199994,15.2,-8.00737088600001));
#173548=CARTESIAN_POINT('Ctrl Pts',(7.57348836199994,11.6,-8.00737088600001));
#173549=CARTESIAN_POINT('Ctrl Pts',(7.57627457699994,15.2,-8.00874583800002));
#173550=CARTESIAN_POINT('Ctrl Pts',(7.57627457699994,11.6,-8.00874583800002));
#173551=CARTESIAN_POINT('Ctrl Pts',(7.57906661499994,15.2,-8.01012084700002));
#173552=CARTESIAN_POINT('Ctrl Pts',(7.57906661499994,11.6,-8.01012084700002));
#173553=CARTESIAN_POINT('Ctrl Pts',(7.58186446999995,15.2,-8.01149590300002));
#173554=CARTESIAN_POINT('Ctrl Pts',(7.58186446999995,11.6,-8.01149590300002));
#173555=CARTESIAN_POINT('Ctrl Pts',(7.58466813599994,15.2,-8.01287099600002));
#173556=CARTESIAN_POINT('Ctrl Pts',(7.58466813599994,11.6,-8.01287099600002));
#173557=CARTESIAN_POINT('Ctrl Pts',(7.58747760999994,15.2,-8.01424611600002));
#173558=CARTESIAN_POINT('Ctrl Pts',(7.58747760999994,11.6,-8.01424611600002));
#173559=CARTESIAN_POINT('Ctrl Pts',(7.59029288699994,15.2,-8.01562125100002));
#173560=CARTESIAN_POINT('Ctrl Pts',(7.59029288699994,11.6,-8.01562125100002));
#173561=CARTESIAN_POINT('Ctrl Pts',(7.59311395999994,15.2,-8.01699639100002));
#173562=CARTESIAN_POINT('Ctrl Pts',(7.59311395999994,11.6,-8.01699639100002));
#173563=CARTESIAN_POINT('Ctrl Pts',(7.59594082499994,15.2,-8.01837152600001));
#173564=CARTESIAN_POINT('Ctrl Pts',(7.59594082499994,11.6,-8.01837152600001));
#173565=CARTESIAN_POINT('Ctrl Pts',(7.59877347799994,15.2,-8.01974664700002));
#173566=CARTESIAN_POINT('Ctrl Pts',(7.59877347799994,11.6,-8.01974664700002));
#173567=CARTESIAN_POINT('Ctrl Pts',(7.60161191199995,15.2,-8.02112174000002));
#173568=CARTESIAN_POINT('Ctrl Pts',(7.60161191199995,11.6,-8.02112174000002));
#173569=CARTESIAN_POINT('Ctrl Pts',(7.60445612499994,15.2,-8.02249679800001));
#173570=CARTESIAN_POINT('Ctrl Pts',(7.60445612499994,11.6,-8.02249679800001));
#173571=CARTESIAN_POINT('Ctrl Pts',(7.60730610999994,15.2,-8.02387181100002));
#173572=CARTESIAN_POINT('Ctrl Pts',(7.60730610999994,11.6,-8.02387181100002));
#173573=CARTESIAN_POINT('Ctrl Pts',(7.61016186199994,15.2,-8.02524676500001));
#173574=CARTESIAN_POINT('Ctrl Pts',(7.61016186199994,11.6,-8.02524676500001));
#173575=CARTESIAN_POINT('Ctrl Pts',(7.61302337699994,15.2,-8.02662165300001));
#173576=CARTESIAN_POINT('Ctrl Pts',(7.61302337699994,11.6,-8.02662165300001));
#173577=CARTESIAN_POINT('Ctrl Pts',(7.61589064899994,15.2,-8.02799646400001));
#173578=CARTESIAN_POINT('Ctrl Pts',(7.61589064899994,11.6,-8.02799646400001));
#173579=CARTESIAN_POINT('Ctrl Pts',(7.61876367299994,15.2,-8.02937118700001));
#173580=CARTESIAN_POINT('Ctrl Pts',(7.61876367299994,11.6,-8.02937118700001));
#173581=CARTESIAN_POINT('Ctrl Pts',(7.62164244499994,15.2,-8.03074581300002));
#173582=CARTESIAN_POINT('Ctrl Pts',(7.62164244499994,11.6,-8.03074581300002));
#173583=CARTESIAN_POINT('Ctrl Pts',(7.62452696099994,15.2,-8.03212033100002));
#173584=CARTESIAN_POINT('Ctrl Pts',(7.62452696099994,11.6,-8.03212033100002));
#173585=CARTESIAN_POINT('Ctrl Pts',(7.62741721299995,15.2,-8.03349473200001));
#173586=CARTESIAN_POINT('Ctrl Pts',(7.62741721299995,11.6,-8.03349473200001));
#173587=CARTESIAN_POINT('Ctrl Pts',(7.63031319799994,15.2,-8.03486900500002));
#173588=CARTESIAN_POINT('Ctrl Pts',(7.63031319799994,11.6,-8.03486900500002));
#173589=CARTESIAN_POINT('Ctrl Pts',(7.63321491099994,15.2,-8.03624314000002));
#173590=CARTESIAN_POINT('Ctrl Pts',(7.63321491099994,11.6,-8.03624314000002));
#173591=CARTESIAN_POINT('Ctrl Pts',(7.63612234699995,15.2,-8.03761712700001));
#173592=CARTESIAN_POINT('Ctrl Pts',(7.63612234699995,11.6,-8.03761712700001));
#173593=CARTESIAN_POINT('Ctrl Pts',(7.63903550099994,15.2,-8.03899095600002));
#173594=CARTESIAN_POINT('Ctrl Pts',(7.63903550099994,11.6,-8.03899095600002));
#173595=CARTESIAN_POINT('Ctrl Pts',(7.64195436699994,15.2,-8.04036461600001));
#173596=CARTESIAN_POINT('Ctrl Pts',(7.64195436699994,11.6,-8.04036461600001));
#173597=CARTESIAN_POINT('Ctrl Pts',(7.64487894199994,15.2,-8.04173809900002));
#173598=CARTESIAN_POINT('Ctrl Pts',(7.64487894199994,11.6,-8.04173809900002));
#173599=CARTESIAN_POINT('Ctrl Pts',(7.64780921899994,15.2,-8.04311139400001));
#173600=CARTESIAN_POINT('Ctrl Pts',(7.64780921899994,11.6,-8.04311139400001));
#173601=CARTESIAN_POINT('Ctrl Pts',(7.65074519499994,15.2,-8.04448449100001));
#173602=CARTESIAN_POINT('Ctrl Pts',(7.65074519499994,11.6,-8.04448449100001));
#173603=CARTESIAN_POINT('Ctrl Pts',(7.65368686399994,15.2,-8.04585738000002));
#173604=CARTESIAN_POINT('Ctrl Pts',(7.65368686399994,11.6,-8.04585738000002));
#173605=CARTESIAN_POINT('Ctrl Pts',(7.65663422099994,15.2,-8.04723005200002));
#173606=CARTESIAN_POINT('Ctrl Pts',(7.65663422099994,11.6,-8.04723005200002));
#173607=CARTESIAN_POINT('Ctrl Pts',(7.65958726299995,15.2,-8.04860249700001));
#173608=CARTESIAN_POINT('Ctrl Pts',(7.65958726299995,11.6,-8.04860249700001));
#173609=CARTESIAN_POINT('Ctrl Pts',(7.66254598199994,15.2,-8.04997470400002));
#173610=CARTESIAN_POINT('Ctrl Pts',(7.66254598199994,11.6,-8.04997470400002));
#173611=CARTESIAN_POINT('Ctrl Pts',(7.66551037499994,15.2,-8.05134666300001));
#173612=CARTESIAN_POINT('Ctrl Pts',(7.66551037499994,11.6,-8.05134666300001));
#173613=CARTESIAN_POINT('Ctrl Pts',(7.66848043599994,15.2,-8.05271836600001));
#173614=CARTESIAN_POINT('Ctrl Pts',(7.66848043599994,11.6,-8.05271836600001));
#173615=CARTESIAN_POINT('Ctrl Pts',(7.67145616099994,15.2,-8.05408980300001));
#173616=CARTESIAN_POINT('Ctrl Pts',(7.67145616099994,11.6,-8.05408980300001));
#173617=CARTESIAN_POINT('Ctrl Pts',(7.67443754499994,15.2,-8.05546096200001));
#173618=CARTESIAN_POINT('Ctrl Pts',(7.67443754499994,11.6,-8.05546096200001));
#173619=CARTESIAN_POINT('Ctrl Pts',(7.67742458199994,15.2,-8.05683183700001));
#173620=CARTESIAN_POINT('Ctrl Pts',(7.67742458199994,11.6,-8.05683183700001));
#173621=CARTESIAN_POINT('Ctrl Pts',(7.68041726999994,15.2,-8.05820241500001));
#173622=CARTESIAN_POINT('Ctrl Pts',(7.68041726999994,11.6,-8.05820241500001));
#173623=CARTESIAN_POINT('Ctrl Pts',(7.68341559999994,15.2,-8.05957268800002));
#173624=CARTESIAN_POINT('Ctrl Pts',(7.68341559999994,11.6,-8.05957268800002));
#173625=CARTESIAN_POINT('Ctrl Pts',(7.68641956999994,15.2,-8.06094264600001));
#173626=CARTESIAN_POINT('Ctrl Pts',(7.68641956999994,11.6,-8.06094264600001));
#173627=CARTESIAN_POINT('Ctrl Pts',(7.68942917399994,15.2,-8.06231227900001));
#173628=CARTESIAN_POINT('Ctrl Pts',(7.68942917399994,11.6,-8.06231227900001));
#173629=CARTESIAN_POINT('Ctrl Pts',(7.69244440799994,15.2,-8.06368157700001));
#173630=CARTESIAN_POINT('Ctrl Pts',(7.69244440799994,11.6,-8.06368157700001));
#173631=CARTESIAN_POINT('Ctrl Pts',(7.69546526599994,15.2,-8.06505053200001));
#173632=CARTESIAN_POINT('Ctrl Pts',(7.69546526599994,11.6,-8.06505053200001));
#173633=CARTESIAN_POINT('Ctrl Pts',(7.69849174399994,15.2,-8.06641913400002));
#173634=CARTESIAN_POINT('Ctrl Pts',(7.69849174399994,11.6,-8.06641913400002));
#173635=CARTESIAN_POINT('Ctrl Pts',(7.70152383599994,15.2,-8.06778737300002));
#173636=CARTESIAN_POINT('Ctrl Pts',(7.70152383599994,11.6,-8.06778737300002));
#173637=CARTESIAN_POINT('Ctrl Pts',(7.70456153899994,15.2,-8.06915523900001));
#173638=CARTESIAN_POINT('Ctrl Pts',(7.70456153899994,11.6,-8.06915523900001));
#173639=CARTESIAN_POINT('Ctrl Pts',(7.70760484499994,15.2,-8.07052272400002));
#173640=CARTESIAN_POINT('Ctrl Pts',(7.70760484499994,11.6,-8.07052272400002));
#173641=CARTESIAN_POINT('Ctrl Pts',(7.71065375199995,15.2,-8.07188981700002));
#173642=CARTESIAN_POINT('Ctrl Pts',(7.71065375199995,11.6,-8.07188981700002));
#173643=CARTESIAN_POINT('Ctrl Pts',(7.71370825399995,15.2,-8.07325651000001));
#173644=CARTESIAN_POINT('Ctrl Pts',(7.71370825399995,11.6,-8.07325651000001));
#173645=CARTESIAN_POINT('Ctrl Pts',(7.71676834699995,15.2,-8.07462279100001));
#173646=CARTESIAN_POINT('Ctrl Pts',(7.71676834699995,11.6,-8.07462279100001));
#173647=CARTESIAN_POINT('Ctrl Pts',(7.71983402499994,15.2,-8.07598865400001));
#173648=CARTESIAN_POINT('Ctrl Pts',(7.71983402499994,11.6,-8.07598865400001));
#173649=CARTESIAN_POINT('Ctrl Pts',(7.72290528299994,15.2,-8.07735408800001));
#173650=CARTESIAN_POINT('Ctrl Pts',(7.72290528299994,11.6,-8.07735408800001));
#173651=CARTESIAN_POINT('Ctrl Pts',(7.72598211699994,15.2,-8.07871908400001));
#173652=CARTESIAN_POINT('Ctrl Pts',(7.72598211699994,11.6,-8.07871908400001));
#173653=CARTESIAN_POINT('Ctrl Pts',(7.72906452199994,15.2,-8.08008363200001));
#173654=CARTESIAN_POINT('Ctrl Pts',(7.72906452199994,11.6,-8.08008363200001));
#173655=CARTESIAN_POINT('Ctrl Pts',(7.73215249199994,15.2,-8.08144772300002));
#173656=CARTESIAN_POINT('Ctrl Pts',(7.73215249199994,11.6,-8.08144772300002));
#173657=CARTESIAN_POINT('Ctrl Pts',(7.73524602399994,15.2,-8.08281134700002));
#173658=CARTESIAN_POINT('Ctrl Pts',(7.73524602399994,11.6,-8.08281134700002));
#173659=CARTESIAN_POINT('Ctrl Pts',(7.73834511099994,15.2,-8.08417449700002));
#173660=CARTESIAN_POINT('Ctrl Pts',(7.73834511099994,11.6,-8.08417449700002));
#173661=CARTESIAN_POINT('Ctrl Pts',(7.74144975099994,15.2,-8.08553716200001));
#173662=CARTESIAN_POINT('Ctrl Pts',(7.74144975099994,11.6,-8.08553716200001));
#173663=CARTESIAN_POINT('Ctrl Pts',(7.74455993599994,15.2,-8.08689933300002));
#173664=CARTESIAN_POINT('Ctrl Pts',(7.74455993599994,11.6,-8.08689933300002));
#173665=CARTESIAN_POINT('Ctrl Pts',(7.74767566299994,15.2,-8.08826100000001));
#173666=CARTESIAN_POINT('Ctrl Pts',(7.74767566299994,11.6,-8.08826100000001));
#173667=CARTESIAN_POINT('Ctrl Pts',(7.75079692599994,15.2,-8.08962215600001));
#173668=CARTESIAN_POINT('Ctrl Pts',(7.75079692599994,11.6,-8.08962215600001));
#173669=CARTESIAN_POINT('Ctrl Pts',(7.75392372099994,15.2,-8.09098279100001));
#173670=CARTESIAN_POINT('Ctrl Pts',(7.75392372099994,11.6,-8.09098279100001));
#173671=CARTESIAN_POINT('Ctrl Pts',(7.75705604399994,15.2,-8.09234289400001));
#173672=CARTESIAN_POINT('Ctrl Pts',(7.75705604399994,11.6,-8.09234289400001));
#173673=CARTESIAN_POINT('Ctrl Pts',(7.76019388899994,15.2,-8.09370245900002));
#173674=CARTESIAN_POINT('Ctrl Pts',(7.76019388899994,11.6,-8.09370245900002));
#173675=CARTESIAN_POINT('Ctrl Pts',(7.76333724999994,15.2,-8.09506147500001));
#173676=CARTESIAN_POINT('Ctrl Pts',(7.76333724999994,11.6,-8.09506147500001));
#173677=CARTESIAN_POINT('Ctrl Pts',(7.76648612399994,15.2,-8.09641993200002));
#173678=CARTESIAN_POINT('Ctrl Pts',(7.76648612399994,11.6,-8.09641993200002));
#173679=CARTESIAN_POINT('Ctrl Pts',(7.76964050599994,15.2,-8.09777782300002));
#173680=CARTESIAN_POINT('Ctrl Pts',(7.76964050599994,11.6,-8.09777782300002));
#173681=CARTESIAN_POINT('Ctrl Pts',(7.77280038999994,15.2,-8.09913513800002));
#173682=CARTESIAN_POINT('Ctrl Pts',(7.77280038999994,11.6,-8.09913513800002));
#173683=CARTESIAN_POINT('Ctrl Pts',(7.77596577299994,15.2,-8.10049186900001));
#173684=CARTESIAN_POINT('Ctrl Pts',(7.77596577299994,11.6,-8.10049186900001));
#173685=CARTESIAN_POINT('Ctrl Pts',(7.77913664799994,15.2,-8.10184800500002));
#173686=CARTESIAN_POINT('Ctrl Pts',(7.77913664799994,11.6,-8.10184800500002));
#173687=CARTESIAN_POINT('Ctrl Pts',(7.78231301099995,15.2,-8.10320354000002));
#173688=CARTESIAN_POINT('Ctrl Pts',(7.78231301099995,11.6,-8.10320354000002));
#173689=CARTESIAN_POINT('Ctrl Pts',(7.78549485799994,15.2,-8.10455846200002));
#173690=CARTESIAN_POINT('Ctrl Pts',(7.78549485799994,11.6,-8.10455846200002));
#173691=CARTESIAN_POINT('Ctrl Pts',(7.78868218299994,15.2,-8.10591276400002));
#173692=CARTESIAN_POINT('Ctrl Pts',(7.78868218299994,11.6,-8.10591276400002));
#173693=CARTESIAN_POINT('Ctrl Pts',(7.79187498299994,15.2,-8.10726643600002));
#173694=CARTESIAN_POINT('Ctrl Pts',(7.79187498299994,11.6,-8.10726643600002));
#173695=CARTESIAN_POINT('Ctrl Pts',(7.79507325099994,15.2,-8.10861947000001));
#173696=CARTESIAN_POINT('Ctrl Pts',(7.79507325099994,11.6,-8.10861947000001));
#173697=CARTESIAN_POINT('Ctrl Pts',(7.79827698299994,15.2,-8.10997185600002));
#173698=CARTESIAN_POINT('Ctrl Pts',(7.79827698299994,11.6,-8.10997185600002));
#173699=CARTESIAN_POINT('Ctrl Pts',(7.80148617399994,15.2,-8.11132358800002));
#173700=CARTESIAN_POINT('Ctrl Pts',(7.80148617399994,11.6,-8.11132358800002));
#173701=CARTESIAN_POINT('Ctrl Pts',(7.80470081999994,15.2,-8.11267465300002));
#173702=CARTESIAN_POINT('Ctrl Pts',(7.80470081999994,11.6,-8.11267465300002));
#173703=CARTESIAN_POINT('Ctrl Pts',(7.80792091399995,15.2,-8.11402504600002));
#173704=CARTESIAN_POINT('Ctrl Pts',(7.80792091399995,11.6,-8.11402504600002));
#173705=CARTESIAN_POINT('Ctrl Pts',(7.81114645399994,15.2,-8.11537475600002));
#173706=CARTESIAN_POINT('Ctrl Pts',(7.81114645399994,11.6,-8.11537475600002));
#173707=CARTESIAN_POINT('Ctrl Pts',(7.81437743299994,15.2,-8.11672377300001));
#173708=CARTESIAN_POINT('Ctrl Pts',(7.81437743299994,11.6,-8.11672377300001));
#173709=CARTESIAN_POINT('Ctrl Pts',(7.81761384899994,15.2,-8.11807209300002));
#173710=CARTESIAN_POINT('Ctrl Pts',(7.81761384899994,11.6,-8.11807209300002));
#173711=CARTESIAN_POINT('Ctrl Pts',(7.82085569299995,15.2,-8.11941970200002));
#173712=CARTESIAN_POINT('Ctrl Pts',(7.82085569299995,11.6,-8.11941970200002));
#173713=CARTESIAN_POINT('Ctrl Pts',(7.82410296399994,15.2,-8.12076659500002));
#173714=CARTESIAN_POINT('Ctrl Pts',(7.82410296399994,11.6,-8.12076659500002));
#173715=CARTESIAN_POINT('Ctrl Pts',(7.82735565499994,15.2,-8.12211276200001));
#173716=CARTESIAN_POINT('Ctrl Pts',(7.82735565499994,11.6,-8.12211276200001));
#173717=CARTESIAN_POINT('Ctrl Pts',(7.83061376199995,15.2,-8.12345819400001));
#173718=CARTESIAN_POINT('Ctrl Pts',(7.83061376199995,11.6,-8.12345819400001));
#173719=CARTESIAN_POINT('Ctrl Pts',(7.83387727999994,15.2,-8.12480288300002));
#173720=CARTESIAN_POINT('Ctrl Pts',(7.83387727999994,11.6,-8.12480288300002));
#173721=CARTESIAN_POINT('Ctrl Pts',(7.83714620399994,15.2,-8.12614682000002));
#173722=CARTESIAN_POINT('Ctrl Pts',(7.83714620399994,11.6,-8.12614682000002));
#173723=CARTESIAN_POINT('Ctrl Pts',(7.84042052999995,15.2,-8.12748999700002));
#173724=CARTESIAN_POINT('Ctrl Pts',(7.84042052999995,11.6,-8.12748999700002));
#173725=CARTESIAN_POINT('Ctrl Pts',(7.84370025199994,15.2,-8.12883240500001));
#173726=CARTESIAN_POINT('Ctrl Pts',(7.84370025199994,11.6,-8.12883240500001));
#173727=CARTESIAN_POINT('Ctrl Pts',(7.84698536499994,15.2,-8.13017403400002));
#173728=CARTESIAN_POINT('Ctrl Pts',(7.84698536499994,11.6,-8.13017403400002));
#173729=CARTESIAN_POINT('Ctrl Pts',(7.85027586699995,15.2,-8.13151487800001));
#173730=CARTESIAN_POINT('Ctrl Pts',(7.85027586699995,11.6,-8.13151487800001));
#173731=CARTESIAN_POINT('Ctrl Pts',(7.85357174999994,15.2,-8.13285492700001));
#173732=CARTESIAN_POINT('Ctrl Pts',(7.85357174999994,11.6,-8.13285492700001));
#173733=CARTESIAN_POINT('Ctrl Pts',(7.85687300999995,15.2,-8.13419417300001));
#173734=CARTESIAN_POINT('Ctrl Pts',(7.85687300999995,11.6,-8.13419417300001));
#173735=CARTESIAN_POINT('Ctrl Pts',(7.86017964299995,15.2,-8.13553260800001));
#173736=CARTESIAN_POINT('Ctrl Pts',(7.86017964299995,11.6,-8.13553260800001));
#173737=CARTESIAN_POINT('Ctrl Pts',(7.86349164399994,15.2,-8.13687022200002));
#173738=CARTESIAN_POINT('Ctrl Pts',(7.86349164399994,11.6,-8.13687022200002));
#173739=CARTESIAN_POINT('Ctrl Pts',(7.86680900699994,15.2,-8.13820700800001));
#173740=CARTESIAN_POINT('Ctrl Pts',(7.86680900699994,11.6,-8.13820700800001));
#173741=CARTESIAN_POINT('Ctrl Pts',(7.87013172899995,15.2,-8.13954295600002));
#173742=CARTESIAN_POINT('Ctrl Pts',(7.87013172899995,11.6,-8.13954295600002));
#173743=CARTESIAN_POINT('Ctrl Pts',(7.87345980499994,15.2,-8.14087806000002));
#173744=CARTESIAN_POINT('Ctrl Pts',(7.87345980499994,11.6,-8.14087806000002));
#173745=CARTESIAN_POINT('Ctrl Pts',(7.87679322899994,15.2,-8.14221230900002));
#173746=CARTESIAN_POINT('Ctrl Pts',(7.87679322899994,11.6,-8.14221230900002));
#173747=CARTESIAN_POINT('Ctrl Pts',(7.88013199699995,15.2,-8.14354569700001));
#173748=CARTESIAN_POINT('Ctrl Pts',(7.88013199699995,11.6,-8.14354569700001));
#173749=CARTESIAN_POINT('Ctrl Pts',(7.88347610399994,15.2,-8.14487821400002));
#173750=CARTESIAN_POINT('Ctrl Pts',(7.88347610399994,11.6,-8.14487821400002));
#173751=CARTESIAN_POINT('Ctrl Pts',(7.88682554499994,15.2,-8.14620985200002));
#173752=CARTESIAN_POINT('Ctrl Pts',(7.88682554499994,11.6,-8.14620985200002));
#173753=CARTESIAN_POINT('Ctrl Pts',(7.89018031499995,15.2,-8.14754060400002));
#173754=CARTESIAN_POINT('Ctrl Pts',(7.89018031499995,11.6,-8.14754060400002));
#173755=CARTESIAN_POINT('Ctrl Pts',(7.89354040999994,15.2,-8.14887046000001));
#173756=CARTESIAN_POINT('Ctrl Pts',(7.89354040999994,11.6,-8.14887046000001));
#173757=CARTESIAN_POINT('Ctrl Pts',(7.89690582599994,15.2,-8.15019941300001));
#173758=CARTESIAN_POINT('Ctrl Pts',(7.89690582599994,11.6,-8.15019941300001));
#173759=CARTESIAN_POINT('Ctrl Pts',(7.90027655699994,15.2,-8.15152745300002));
#173760=CARTESIAN_POINT('Ctrl Pts',(7.90027655699994,11.6,-8.15152745300002));
#173761=CARTESIAN_POINT('Ctrl Pts',(7.90365259799994,15.2,-8.15285457300002));
#173762=CARTESIAN_POINT('Ctrl Pts',(7.90365259799994,11.6,-8.15285457300002));
#173763=CARTESIAN_POINT('Ctrl Pts',(7.90703394399995,15.2,-8.15418076500002));
#173764=CARTESIAN_POINT('Ctrl Pts',(7.90703394399995,11.6,-8.15418076500002));
#173765=CARTESIAN_POINT('Ctrl Pts',(7.91042059099994,15.2,-8.15550602000001));
#173766=CARTESIAN_POINT('Ctrl Pts',(7.91042059099994,11.6,-8.15550602000001));
#173767=CARTESIAN_POINT('Ctrl Pts',(7.91381253499994,15.2,-8.15683033100001));
#173768=CARTESIAN_POINT('Ctrl Pts',(7.91381253499994,11.6,-8.15683033100001));
#173769=CARTESIAN_POINT('Ctrl Pts',(7.91720976999994,15.2,-8.15815368900001));
#173770=CARTESIAN_POINT('Ctrl Pts',(7.91720976999994,11.6,-8.15815368900001));
#173771=CARTESIAN_POINT('Ctrl Pts',(7.92061229099994,15.2,-8.15947608600002));
#173772=CARTESIAN_POINT('Ctrl Pts',(7.92061229099994,11.6,-8.15947608600002));
#173773=CARTESIAN_POINT('Ctrl Pts',(7.92402009399995,15.2,-8.16079751400002));
#173774=CARTESIAN_POINT('Ctrl Pts',(7.92402009399995,11.6,-8.16079751400002));
#173775=CARTESIAN_POINT('Ctrl Pts',(7.92743317499994,15.2,-8.16211796400001));
#173776=CARTESIAN_POINT('Ctrl Pts',(7.92743317499994,11.6,-8.16211796400001));
#173777=CARTESIAN_POINT('Ctrl Pts',(7.93085152599994,15.2,-8.16343743000001));
#173778=CARTESIAN_POINT('Ctrl Pts',(7.93085152599994,11.6,-8.16343743000001));
#173779=CARTESIAN_POINT('Ctrl Pts',(7.93427514599994,15.2,-8.16475590100002));
#173780=CARTESIAN_POINT('Ctrl Pts',(7.93427514599994,11.6,-8.16475590100002));
#173781=CARTESIAN_POINT('Ctrl Pts',(7.93770402899994,15.2,-8.16607337100002));
#173782=CARTESIAN_POINT('Ctrl Pts',(7.93770402899994,11.6,-8.16607337100002));
#173783=CARTESIAN_POINT('Ctrl Pts',(7.94113816999995,15.2,-8.16738983200001));
#173784=CARTESIAN_POINT('Ctrl Pts',(7.94113816999995,11.6,-8.16738983200001));
#173785=CARTESIAN_POINT('Ctrl Pts',(7.94457756299995,15.2,-8.16870527600001));
#173786=CARTESIAN_POINT('Ctrl Pts',(7.94457756299995,11.6,-8.16870527600001));
#173787=CARTESIAN_POINT('Ctrl Pts',(7.94802220599995,15.2,-8.17001969300001));
#173788=CARTESIAN_POINT('Ctrl Pts',(7.94802220599995,11.6,-8.17001969300001));
#173789=CARTESIAN_POINT('Ctrl Pts',(7.95147209099994,15.2,-8.17133307700002));
#173790=CARTESIAN_POINT('Ctrl Pts',(7.95147209099994,11.6,-8.17133307700002));
#173791=CARTESIAN_POINT('Ctrl Pts',(7.95492721599994,15.2,-8.17264542000002));
#173792=CARTESIAN_POINT('Ctrl Pts',(7.95492721599994,11.6,-8.17264542000002));
#173793=CARTESIAN_POINT('Ctrl Pts',(7.95838757499994,15.2,-8.17395671300002));
#173794=CARTESIAN_POINT('Ctrl Pts',(7.95838757499994,11.6,-8.17395671300002));
#173795=CARTESIAN_POINT('Ctrl Pts',(7.96185316299994,15.2,-8.17526694900002));
#173796=CARTESIAN_POINT('Ctrl Pts',(7.96185316299994,11.6,-8.17526694900002));
#173797=CARTESIAN_POINT('Ctrl Pts',(7.96532397699995,15.2,-8.17657611900002));
#173798=CARTESIAN_POINT('Ctrl Pts',(7.96532397699995,11.6,-8.17657611900002));
#173799=CARTESIAN_POINT('Ctrl Pts',(7.96880000999994,15.2,-8.17788421800002));
#173800=CARTESIAN_POINT('Ctrl Pts',(7.96880000999994,11.6,-8.17788421800002));
#173801=CARTESIAN_POINT('Ctrl Pts',(7.97228125899994,15.2,-8.17919123400002));
#173802=CARTESIAN_POINT('Ctrl Pts',(7.97228125899994,11.6,-8.17919123400002));
#173803=CARTESIAN_POINT('Ctrl Pts',(7.97576771799994,15.2,-8.18049716300001));
#173804=CARTESIAN_POINT('Ctrl Pts',(7.97576771799994,11.6,-8.18049716300001));
#173805=CARTESIAN_POINT('Ctrl Pts',(7.97925938299994,15.2,-8.18180199500001));
#173806=CARTESIAN_POINT('Ctrl Pts',(7.97925938299994,11.6,-8.18180199500001));
#173807=CARTESIAN_POINT('Ctrl Pts',(7.98275624999994,15.2,-8.18310572200001));
#173808=CARTESIAN_POINT('Ctrl Pts',(7.98275624999994,11.6,-8.18310572200001));
#173809=CARTESIAN_POINT('Ctrl Pts',(7.98625831199994,15.2,-8.18440833600001));
#173810=CARTESIAN_POINT('Ctrl Pts',(7.98625831199994,11.6,-8.18440833600001));
#173811=CARTESIAN_POINT('Ctrl Pts',(7.98976556499994,15.2,-8.18570982900001));
#173812=CARTESIAN_POINT('Ctrl Pts',(7.98976556499994,11.6,-8.18570982900001));
#173813=CARTESIAN_POINT('Ctrl Pts',(7.99327800399994,15.2,-8.18701019200001));
#173814=CARTESIAN_POINT('Ctrl Pts',(7.99327800399994,11.6,-8.18701019200001));
#173815=CARTESIAN_POINT('Ctrl Pts',(7.99679562499994,15.2,-8.18830942000002));
#173816=CARTESIAN_POINT('Ctrl Pts',(7.99679562499994,11.6,-8.18830942000002));
#173817=CARTESIAN_POINT('Ctrl Pts',(8.00031842399994,15.2,-8.18960750500001));
#173818=CARTESIAN_POINT('Ctrl Pts',(8.00031842399994,11.6,-8.18960750500001));
#173819=CARTESIAN_POINT('Ctrl Pts',(8.00384639599995,15.2,-8.19090444000001));
#173820=CARTESIAN_POINT('Ctrl Pts',(8.00384639599995,11.6,-8.19090444000001));
#173821=CARTESIAN_POINT('Ctrl Pts',(8.00737953699995,15.2,-8.19220021800002));
#173822=CARTESIAN_POINT('Ctrl Pts',(8.00737953699995,11.6,-8.19220021800002));
#173823=CARTESIAN_POINT('Ctrl Pts',(8.01091784199994,15.2,-8.19349483100002));
#173824=CARTESIAN_POINT('Ctrl Pts',(8.01091784199994,11.6,-8.19349483100002));
#173825=CARTESIAN_POINT('Ctrl Pts',(8.01446130799994,15.2,-8.19478827200001));
#173826=CARTESIAN_POINT('Ctrl Pts',(8.01446130799994,11.6,-8.19478827200001));
#173827=CARTESIAN_POINT('Ctrl Pts',(8.01800992599994,15.2,-8.19608053200002));
#173828=CARTESIAN_POINT('Ctrl Pts',(8.01800992599994,11.6,-8.19608053200002));
#173829=CARTESIAN_POINT('Ctrl Pts',(8.02156369399994,15.2,-8.19737160100001));
#173830=CARTESIAN_POINT('Ctrl Pts',(8.02156369399994,11.6,-8.19737160100001));
#173831=CARTESIAN_POINT('Ctrl Pts',(8.02512260399994,15.2,-8.19866147000001));
#173832=CARTESIAN_POINT('Ctrl Pts',(8.02512260399994,11.6,-8.19866147000001));
#173833=CARTESIAN_POINT('Ctrl Pts',(8.02868665099994,15.2,-8.19995012900002));
#173834=CARTESIAN_POINT('Ctrl Pts',(8.02868665099994,11.6,-8.19995012900002));
#173835=CARTESIAN_POINT('Ctrl Pts',(8.03225582899995,15.2,-8.20123757100001));
#173836=CARTESIAN_POINT('Ctrl Pts',(8.03225582899995,11.6,-8.20123757100001));
#173837=CARTESIAN_POINT('Ctrl Pts',(8.03583013499994,15.2,-8.20252378800001));
#173838=CARTESIAN_POINT('Ctrl Pts',(8.03583013499994,11.6,-8.20252378800001));
#173839=CARTESIAN_POINT('Ctrl Pts',(8.03940956399994,15.2,-8.20380877500002));
#173840=CARTESIAN_POINT('Ctrl Pts',(8.03940956399994,11.6,-8.20380877500002));
#173841=CARTESIAN_POINT('Ctrl Pts',(8.04299411599994,15.2,-8.20509252900001));
#173842=CARTESIAN_POINT('Ctrl Pts',(8.04299411599994,11.6,-8.20509252900001));
#173843=CARTESIAN_POINT('Ctrl Pts',(8.04658378799994,15.2,-8.20637504800001));
#173844=CARTESIAN_POINT('Ctrl Pts',(8.04658378799994,11.6,-8.20637504800001));
#173845=CARTESIAN_POINT('Ctrl Pts',(8.04945962199995,15.2,-8.20740007500002));
#173846=CARTESIAN_POINT('Ctrl Pts',(8.04945962199995,11.6,-8.20740007500002));
#173847=CARTESIAN_POINT('Ctrl Pts',(8.05161880099994,15.2,-8.20816828800002));
#173848=CARTESIAN_POINT('Ctrl Pts',(8.05161880099994,11.6,-8.20816828800002));
#173849=CARTESIAN_POINT('Ctrl Pts',(8.05305927699994,15.2,-8.20868018400001));
#173850=CARTESIAN_POINT('Ctrl Pts',(8.05305927699994,11.6,-8.20868018400001));
#173851=CARTESIAN_POINT('Ctrl Pts',(8.05377977099995,15.2,-8.20893607000002));
#173852=CARTESIAN_POINT('Ctrl Pts',(8.05377977099995,11.6,-8.20893607000002));
#173853=CARTESIAN_POINT('Ctrl Pts',(7.01216898599994,15.2,-7.64657512400002));
#173854=CARTESIAN_POINT('Ctrl Pts',(7.01348522039998,15.2,-7.64778327244868));
#173855=CARTESIAN_POINT('Ctrl Pts',(7.0148472207803,15.2,-7.64902613336841));
#173856=CARTESIAN_POINT('Ctrl Pts',(7.01625467904572,15.2,-7.65030255165183));
#173857=CARTESIAN_POINT('Ctrl Pts',(7.01766892478633,15.2,-7.65158512546942));
#173858=CARTESIAN_POINT('Ctrl Pts',(7.01912907680239,15.2,-7.6529015883544));
#173859=CARTESIAN_POINT('Ctrl Pts',(7.02063486162897,15.2,-7.65425083033056));
#173860=CARTESIAN_POINT('Ctrl Pts',(7.0221406463188,15.2,-7.65560007218416));
#173861=CARTESIAN_POINT('Ctrl Pts',(7.0236920633662,15.2,-7.65698209165132));
#173862=CARTESIAN_POINT('Ctrl Pts',(7.02528884122486,15.2,-7.65839580976662));
#173863=CARTESIAN_POINT('Ctrl Pts',(7.02688561908352,15.2,-7.65980952788194));
#173864=CARTESIAN_POINT('Ctrl Pts',(7.02852775929139,15.1999999999999,-7.66125494592225));
#173865=CARTESIAN_POINT('Ctrl Pts',(7.03021499706176,15.2,-7.66273101410725));
#173866=CARTESIAN_POINT('Ctrl Pts',(7.03190223498539,15.2,-7.66420708242633));
#173867=CARTESIAN_POINT('Ctrl Pts',(7.03363456925201,15.2,-7.66571380189834));
#173868=CARTESIAN_POINT('Ctrl Pts',(7.03541173743525,15.2,-7.66725015515077));
#173869=CARTESIAN_POINT('Ctrl Pts',(7.03718890545706,15.2,-7.66878650826362));
#173870=CARTESIAN_POINT('Ctrl Pts',(7.03901091135163,15.2,-7.67035249414299));
#173871=CARTESIAN_POINT('Ctrl Pts',(7.04087749604239,15.2,-7.67194712350903));
#173872=CARTESIAN_POINT('Ctrl Pts',(7.04274408073314,15.2,-7.67354175287507));
#173873=CARTESIAN_POINT('Ctrl Pts',(7.04465524144143,15.2,-7.67516502671293));
#173874=CARTESIAN_POINT('Ctrl Pts',(7.04661073111848,15.2,-7.67681598040177));
#173875=CARTESIAN_POINT('Ctrl Pts',(7.04856622097314,15.2,-7.67846693424055));
#173876=CARTESIAN_POINT('Ctrl Pts',(7.0505660383916,15.2,-7.68014557138276));
#173877=CARTESIAN_POINT('Ctrl Pts',(7.052609930506,15.2,-7.68185095122753));
#173878=CARTESIAN_POINT('Ctrl Pts',(7.05465382243473,15.2,-7.68355633091739));
#173879=CARTESIAN_POINT('Ctrl Pts',(7.0567417943918,15.2,-7.68528845520865));
#173880=CARTESIAN_POINT('Ctrl Pts',(7.05887359714957,15.2,-7.68704641381255));
#173881=CARTESIAN_POINT('Ctrl Pts',(7.06100539990735,15.2,-7.68880437241647));
#173882=CARTESIAN_POINT('Ctrl Pts',(7.06318103490329,15.2,-7.69058816246829));
#173883=CARTESIAN_POINT('Ctrl Pts',(7.06540025990411,15.2,-7.6923968984015));
#173884=CARTESIAN_POINT('Ctrl Pts',(7.06761948490493,15.2,-7.69420563433471));
#173885=CARTESIAN_POINT('Ctrl Pts',(7.0698823003436,15.2,-7.69603931773329));
#173886=CARTESIAN_POINT('Ctrl Pts',(7.07218846800684,15.2,-7.69789707783082));
#173887=CARTESIAN_POINT('Ctrl Pts',(7.07449463587956,15.2,-7.69975483809708));
#173888=CARTESIAN_POINT('Ctrl Pts',(7.07684415358985,15.2,-7.70163667853241));
#173889=CARTESIAN_POINT('Ctrl Pts',(7.07923678863878,15.2,-7.70354175580389));
#173890=CARTESIAN_POINT('Ctrl Pts',(7.08162942347036,15.2,-7.70544683290233));
#173891=CARTESIAN_POINT('Ctrl Pts',(7.08406517439433,15.2,-7.70737514680284));
#173892=CARTESIAN_POINT('Ctrl Pts',(7.08654380831541,15.2,-7.70932587299076));
#173893=CARTESIAN_POINT('Ctrl Pts',(7.0890224422365,15.2,-7.71127659917867));
#173894=CARTESIAN_POINT('Ctrl Pts',(7.09154395894146,15.2,-7.71324973923985));
#173895=CARTESIAN_POINT('Ctrl Pts',(7.09410812976205,15.2,-7.71524449049922));
#173896=CARTESIAN_POINT('Ctrl Pts',(7.09667230081556,15.2,-7.7172392419398));
#173897=CARTESIAN_POINT('Ctrl Pts',(7.09927912588989,15.2,-7.71925560495751));
#173898=CARTESIAN_POINT('Ctrl Pts',(7.10192837511943,15.2,-7.72129279365276));
#173899=CARTESIAN_POINT('Ctrl Pts',(7.10457762410833,15.2,-7.72332998216297));
#173900=CARTESIAN_POINT('Ctrl Pts',(7.10726930113564,15.2,-7.72538800047348));
#173901=CARTESIAN_POINT('Ctrl Pts',(7.11000317804863,15.2,-7.72746607899071));
#173902=CARTESIAN_POINT('Ctrl Pts',(7.11273705496164,15.2,-7.72954415750794));
#173903=CARTESIAN_POINT('Ctrl Pts',(7.11551313393964,15.2,-7.73164229980578));
#173904=CARTESIAN_POINT('Ctrl Pts',(7.11833118991771,15.2,-7.73375975631085));
#173905=CARTESIAN_POINT('Ctrl Pts',(7.12114924615177,15.2,-7.73587721300827));
#173906=CARTESIAN_POINT('Ctrl Pts',(7.12400928121682,15.2,-7.73801398467397));
#173907=CARTESIAN_POINT('Ctrl Pts',(7.12691107627235,15.2,-7.74016934248353));
#173908=CARTESIAN_POINT('Ctrl Pts',(7.12981287106431,15.2,-7.7423247000973));
#173909=CARTESIAN_POINT('Ctrl Pts',(7.13275642209166,15.2,-7.74449864123796));
#173910=CARTESIAN_POINT('Ctrl Pts',(7.1357415149832,15.2,-7.74669045474165));
#173911=CARTESIAN_POINT('Ctrl Pts',(7.13922412353743,15.2,-7.74924757062868));
#173912=CARTESIAN_POINT('Ctrl Pts',(7.14276327322082,15.2,-7.75182900945527));
#173913=CARTESIAN_POINT('Ctrl Pts',(7.14635862055642,15.2,-7.75443366743267));
#173914=CARTESIAN_POINT('Ctrl Pts',(7.14944034668413,15.2,-7.75666623129739));
#173915=CARTESIAN_POINT('Ctrl Pts',(7.15256336090648,15.2,-7.75891585329897));
#173916=CARTESIAN_POINT('Ctrl Pts',(7.1557274507082,15.2,-7.76118185404998));
#173917=CARTESIAN_POINT('Ctrl Pts',(7.15889154050992,15.2,-7.763447854801));
#173918=CARTESIAN_POINT('Ctrl Pts',(7.16209670506911,15.2,-7.76573023257232));
#173919=CARTESIAN_POINT('Ctrl Pts',(7.16534273219429,15.2,-7.76802832451938));
#173920=CARTESIAN_POINT('Ctrl Pts',(7.16804775489691,15.2,-7.76994340121152));
#173921=CARTESIAN_POINT('Ctrl Pts',(7.17078115538202,15.2,-7.77186938930173));
#173922=CARTESIAN_POINT('Ctrl Pts',(7.17354281051943,15.2,-7.77380591110674));
#173923=CARTESIAN_POINT('Ctrl Pts',(7.17630446565684,15.2,-7.77574243291174));
#173924=CARTESIAN_POINT('Ctrl Pts',(7.17909437698944,15.2,-7.77768948970035));
#173925=CARTESIAN_POINT('Ctrl Pts',(7.18191242205741,15.2,-7.77964670963038));
#173926=CARTESIAN_POINT('Ctrl Pts',(7.18473046712538,15.2,-7.7816039295604));
#173927=CARTESIAN_POINT('Ctrl Pts',(7.18757664829089,15.2,-7.78357131208995));
#173928=CARTESIAN_POINT('Ctrl Pts',(7.19045084253998,15.2,-7.78554849376558));
#173929=CARTESIAN_POINT('Ctrl Pts',(7.19332503678907,15.2,-7.78752567544121));
#173930=CARTESIAN_POINT('Ctrl Pts',(7.19622724572209,15.2,-7.78951265435554));
#173931=CARTESIAN_POINT('Ctrl Pts',(7.1991573499582,15.2,-7.79150907504999));
#173932=CARTESIAN_POINT('Ctrl Pts',(7.20208745419431,15.2,-7.79350549574444));
#173933=CARTESIAN_POINT('Ctrl Pts',(7.20504545320452,15.2,-7.79551135381969));
#173934=CARTESIAN_POINT('Ctrl Pts',(7.20803123050984,15.2,-7.79752630146776));
#173935=CARTESIAN_POINT('Ctrl Pts',(7.21101700781514,15.2,-7.79954124911583));
#173936=CARTESIAN_POINT('Ctrl Pts',(7.21403055872527,15.2,-7.80156528312143));
#173937=CARTESIAN_POINT('Ctrl Pts',(7.21707177115727,15.2,-7.80359805985799));
#173938=CARTESIAN_POINT('Ctrl Pts',(7.22011298358927,15.2,-7.80563083659455));
#173939=CARTESIAN_POINT('Ctrl Pts',(7.22318185372334,15.2,-7.80767235337257));
#173940=CARTESIAN_POINT('Ctrl Pts',(7.22627826691921,15.2,-7.80972227115078));
#173941=CARTESIAN_POINT('Ctrl Pts',(7.22937468011509,15.2,-7.81177218892899));
#173942=CARTESIAN_POINT('Ctrl Pts',(7.232498633412,15.2,-7.81383050583054));
#173943=CARTESIAN_POINT('Ctrl Pts',(7.2356500136408,15.2,-7.8158968902399));
#173944=CARTESIAN_POINT('Ctrl Pts',(7.2388013938696,15.2,-7.81796327464925));
#173945=CARTESIAN_POINT('Ctrl Pts',(7.24198019768924,15.2,-7.82003772281617));
#173946=CARTESIAN_POINT('Ctrl Pts',(7.24518631192758,15.2,-7.82211990649735));
#173947=CARTESIAN_POINT('Ctrl Pts',(7.24839242616592,15.2,-7.82420209017854));
#173948=CARTESIAN_POINT('Ctrl Pts',(7.25162585030193,15.2,-7.8262920095904));
#173949=CARTESIAN_POINT('Ctrl Pts',(7.25488646794304,15.2,-7.82838934000766));
#173950=CARTESIAN_POINT('Ctrl Pts',(7.25814708522875,15.2,-7.83048667019634));
#173951=CARTESIAN_POINT('Ctrl Pts',(7.26143489795205,15.2,-7.83259141059899));
#173952=CARTESIAN_POINT('Ctrl Pts',(7.26474978932463,15.2,-7.83470324321544));
#173953=CARTESIAN_POINT('Ctrl Pts',(7.26806468105854,15.2,-7.83681507606209));
#173954=CARTESIAN_POINT('Ctrl Pts',(7.27140665252256,15.2,-7.83893400037807));
#173955=CARTESIAN_POINT('Ctrl Pts',(7.27477558932589,15.2,-7.84105970169696));
#173956=CARTESIAN_POINT('Ctrl Pts',(7.27881831371023,15.2,-7.84361054341864));
#173957=CARTESIAN_POINT('Ctrl Pts',(7.28289986889003,15.2,-7.84617114590798));
#173958=CARTESIAN_POINT('Ctrl Pts',(7.28702005819959,15.2,-7.84874097163176));
#173959=CARTESIAN_POINT('Ctrl Pts',(7.29045354910377,15.2,-7.85088249295154));
#173960=CARTESIAN_POINT('Ctrl Pts',(7.29391387020648,15.2,-7.85303042183648));
#173961=CARTESIAN_POINT('Ctrl Pts',(7.2974009071881,15.2,-7.85518445250007));
#173962=CARTESIAN_POINT('Ctrl Pts',(7.30088794416971,15.2,-7.85733848316366));
